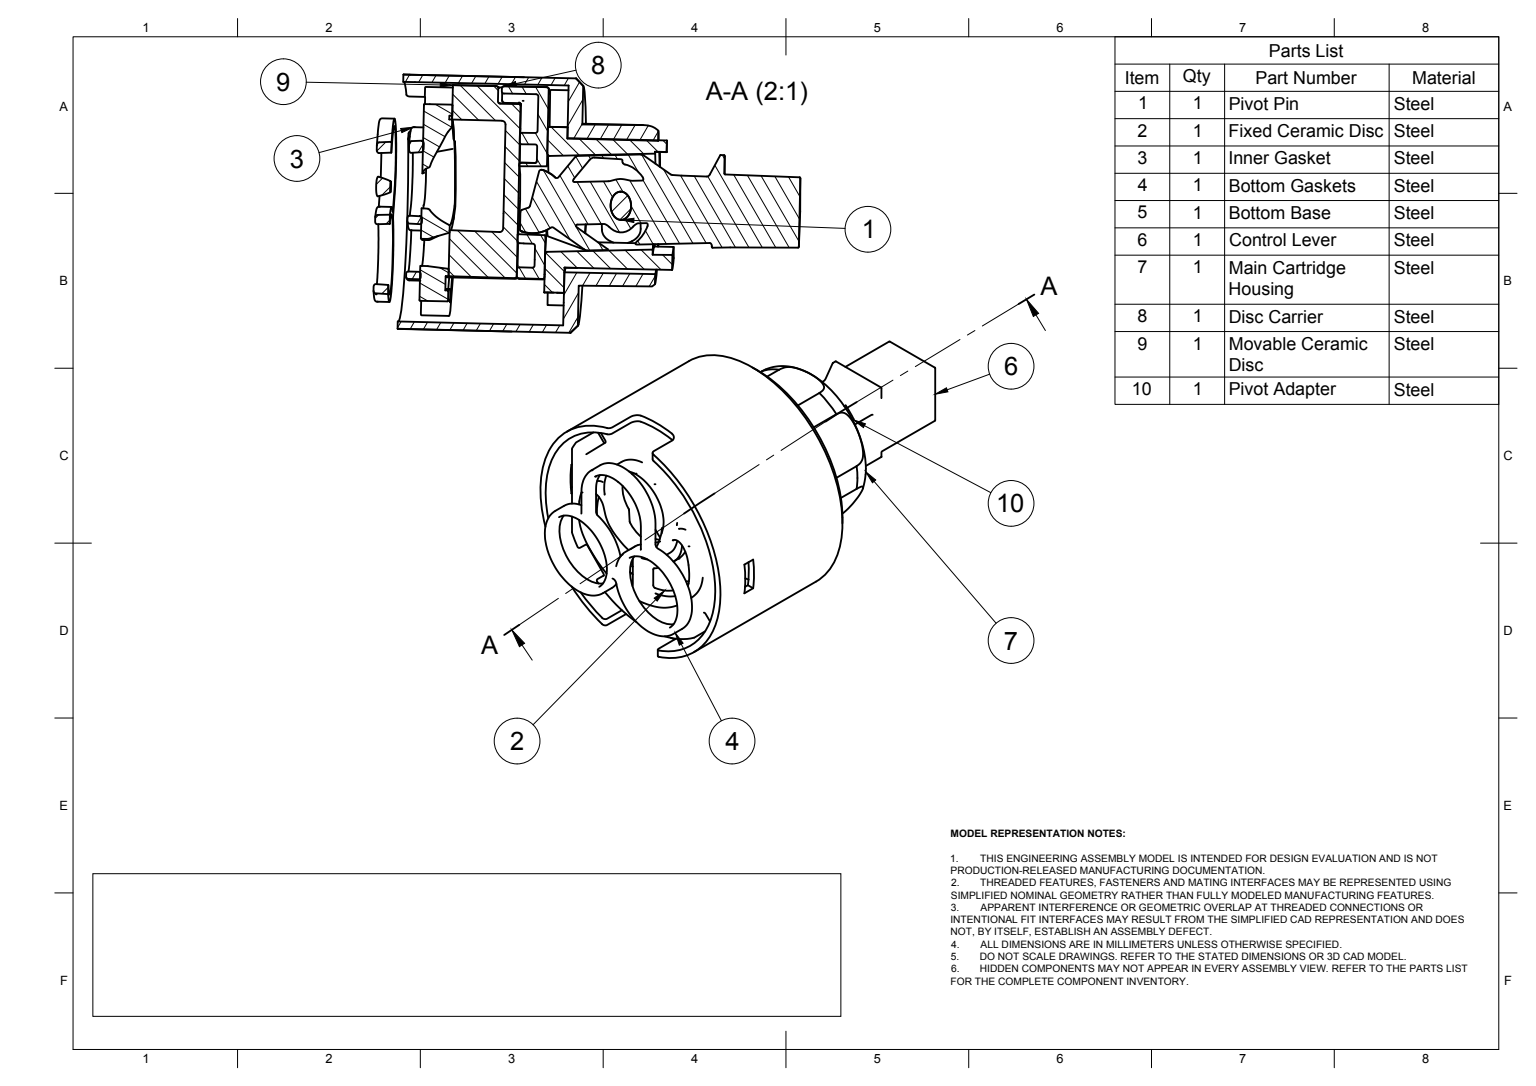
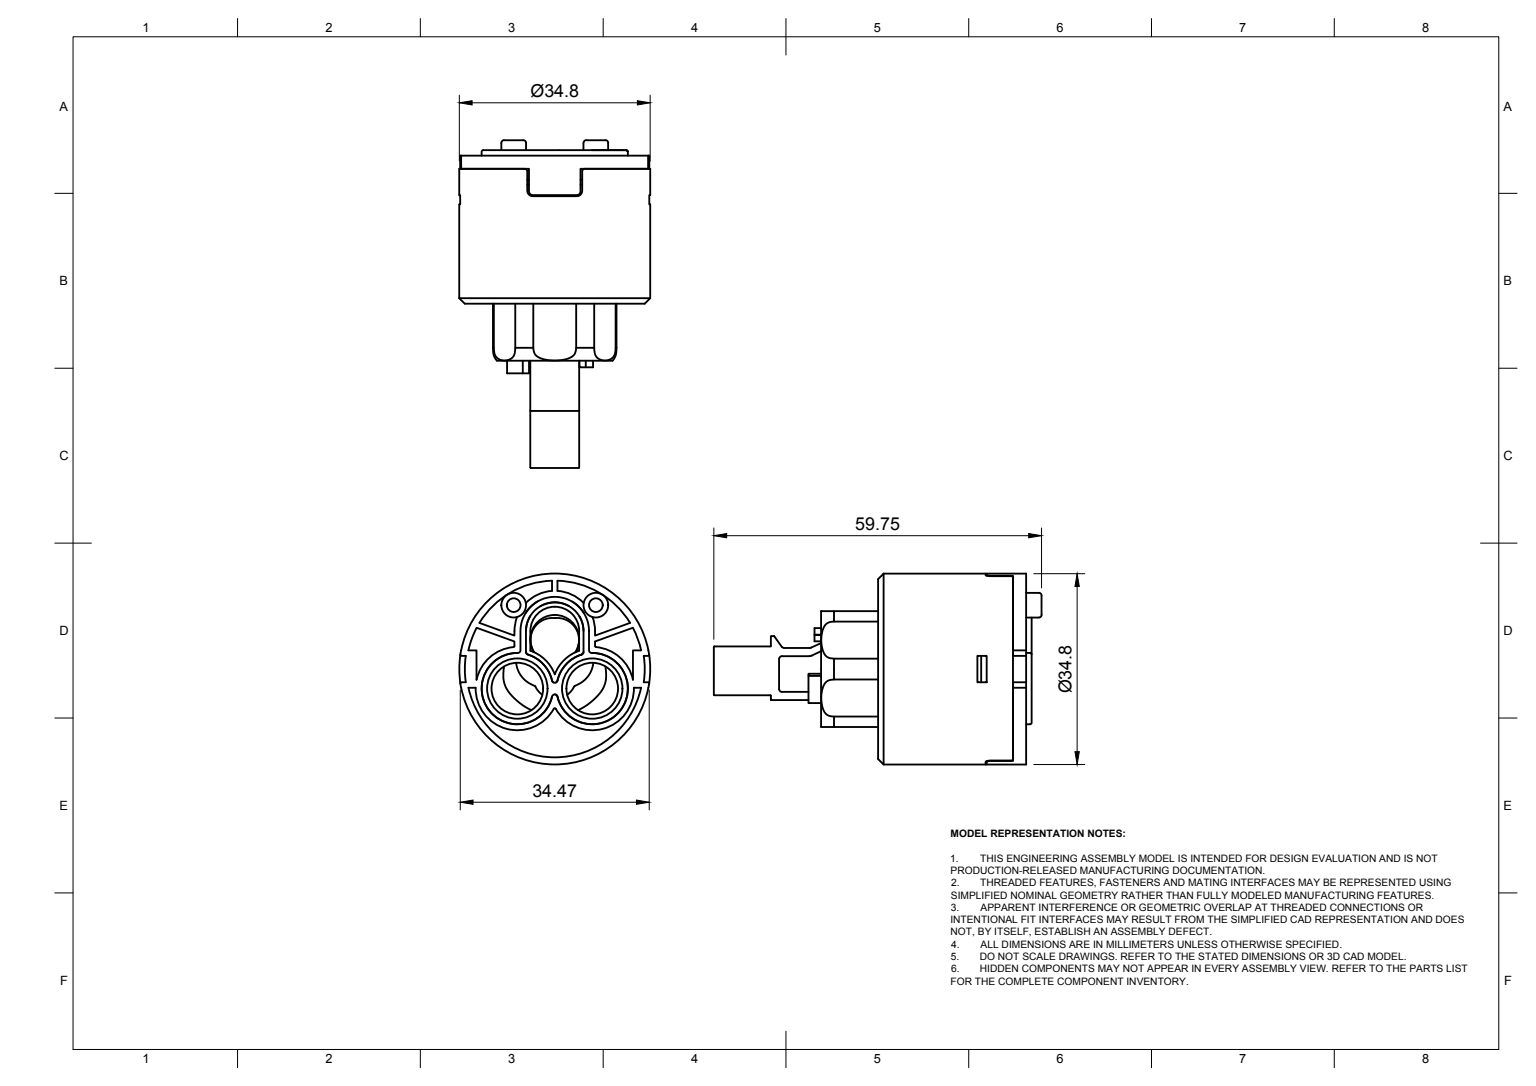
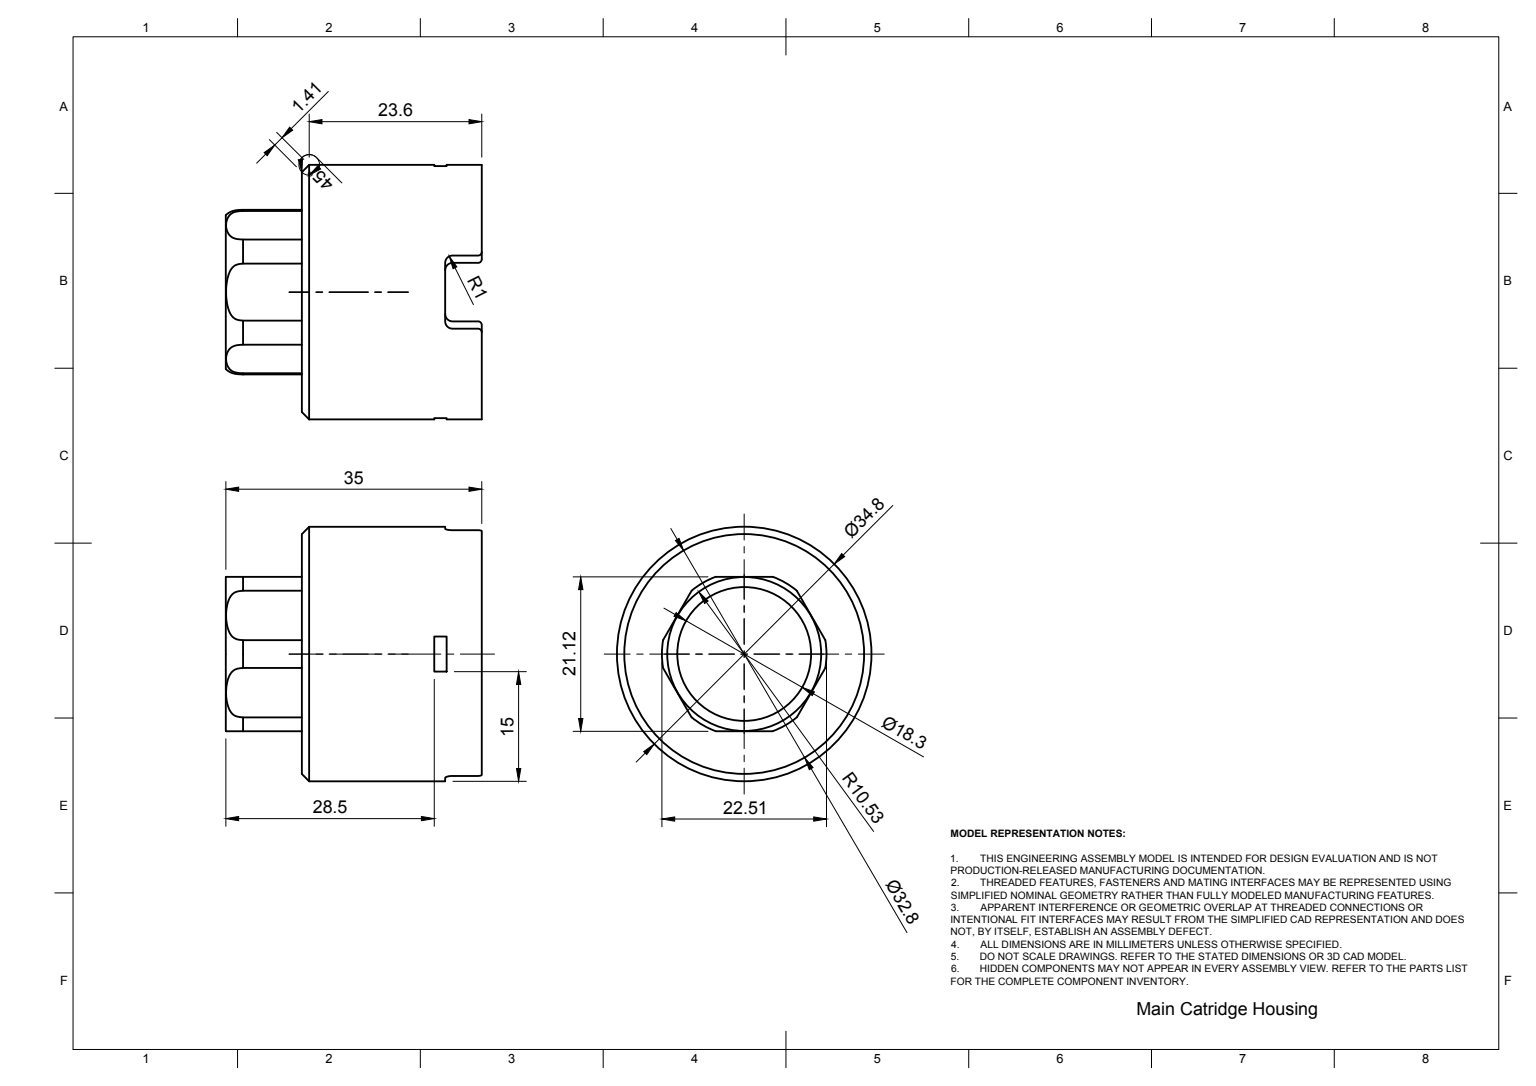
ISO-10303-21;
HEADER;
/* Generated by software containing ST-Developer
 * from STEP Tools, Inc. (www.steptools.com) 
 */

FILE_DESCRIPTION(
/* description */ ('STEP AP214'),
/* implementation_level */ '2;1');

FILE_NAME(
/* name */ 'MAS-608',
/* time_stamp */ '2026-10-06T00:19:40-07:00',
/* author */ (''),
/* organization */ (''),
/* preprocessor_version */ 'ST-DEVELOPER v20.2',
/* originating_system */ 'Autodesk Translation Framework v15.15.0.0',
/* authorisation */ '');

FILE_SCHEMA (('AUTOMOTIVE_DESIGN { 1 0 10303 214 3 1 1 }'));
ENDSEC;

DATA;
#10=MECHANICAL_DESIGN_GEOMETRIC_PRESENTATION_REPRESENTATION('',(#2063,#2064,
#2065,#2066,#2067,#2068,#2069,#2070,#2071,#2072),#98302);
#11=ITEM_DEFINED_TRANSFORMATION($,$,#34291,#38606);
#12=ITEM_DEFINED_TRANSFORMATION($,$,#34303,#38607);
#13=ITEM_DEFINED_TRANSFORMATION($,$,#34823,#38608);
#14=ITEM_DEFINED_TRANSFORMATION($,$,#34920,#38609);
#15=ITEM_DEFINED_TRANSFORMATION($,$,#34962,#38610);
#16=ITEM_DEFINED_TRANSFORMATION($,$,#35726,#38611);
#17=ITEM_DEFINED_TRANSFORMATION($,$,#36369,#38612);
#18=ITEM_DEFINED_TRANSFORMATION($,$,#36602,#38613);
#19=ITEM_DEFINED_TRANSFORMATION($,$,#38088,#38614);
#20=ITEM_DEFINED_TRANSFORMATION($,$,#38347,#38615);
#21=(
REPRESENTATION_RELATIONSHIP($,$,#98340,#98339)
REPRESENTATION_RELATIONSHIP_WITH_TRANSFORMATION(#11)
SHAPE_REPRESENTATION_RELATIONSHIP()
);
#22=(
REPRESENTATION_RELATIONSHIP($,$,#98341,#98339)
REPRESENTATION_RELATIONSHIP_WITH_TRANSFORMATION(#12)
SHAPE_REPRESENTATION_RELATIONSHIP()
);
#23=(
REPRESENTATION_RELATIONSHIP($,$,#98342,#98339)
REPRESENTATION_RELATIONSHIP_WITH_TRANSFORMATION(#13)
SHAPE_REPRESENTATION_RELATIONSHIP()
);
#24=(
REPRESENTATION_RELATIONSHIP($,$,#98343,#98339)
REPRESENTATION_RELATIONSHIP_WITH_TRANSFORMATION(#14)
SHAPE_REPRESENTATION_RELATIONSHIP()
);
#25=(
REPRESENTATION_RELATIONSHIP($,$,#98344,#98339)
REPRESENTATION_RELATIONSHIP_WITH_TRANSFORMATION(#15)
SHAPE_REPRESENTATION_RELATIONSHIP()
);
#26=(
REPRESENTATION_RELATIONSHIP($,$,#98345,#98339)
REPRESENTATION_RELATIONSHIP_WITH_TRANSFORMATION(#16)
SHAPE_REPRESENTATION_RELATIONSHIP()
);
#27=(
REPRESENTATION_RELATIONSHIP($,$,#98346,#98339)
REPRESENTATION_RELATIONSHIP_WITH_TRANSFORMATION(#17)
SHAPE_REPRESENTATION_RELATIONSHIP()
);
#28=(
REPRESENTATION_RELATIONSHIP($,$,#98347,#98339)
REPRESENTATION_RELATIONSHIP_WITH_TRANSFORMATION(#18)
SHAPE_REPRESENTATION_RELATIONSHIP()
);
#29=(
REPRESENTATION_RELATIONSHIP($,$,#98348,#98339)
REPRESENTATION_RELATIONSHIP_WITH_TRANSFORMATION(#19)
SHAPE_REPRESENTATION_RELATIONSHIP()
);
#30=(
REPRESENTATION_RELATIONSHIP($,$,#98349,#98339)
REPRESENTATION_RELATIONSHIP_WITH_TRANSFORMATION(#20)
SHAPE_REPRESENTATION_RELATIONSHIP()
);
#31=CONTEXT_DEPENDENT_SHAPE_REPRESENTATION(#21,#98329);
#32=CONTEXT_DEPENDENT_SHAPE_REPRESENTATION(#22,#98330);
#33=CONTEXT_DEPENDENT_SHAPE_REPRESENTATION(#23,#98331);
#34=CONTEXT_DEPENDENT_SHAPE_REPRESENTATION(#24,#98332);
#35=CONTEXT_DEPENDENT_SHAPE_REPRESENTATION(#25,#98333);
#36=CONTEXT_DEPENDENT_SHAPE_REPRESENTATION(#26,#98334);
#37=CONTEXT_DEPENDENT_SHAPE_REPRESENTATION(#27,#98335);
#38=CONTEXT_DEPENDENT_SHAPE_REPRESENTATION(#28,#98336);
#39=CONTEXT_DEPENDENT_SHAPE_REPRESENTATION(#29,#98337);
#40=CONTEXT_DEPENDENT_SHAPE_REPRESENTATION(#30,#98338);
#41=NEXT_ASSEMBLY_USAGE_OCCURRENCE('Pivot Pin:1','Pivot Pin:1',
'Pivot Pin:1',#98351,#98352,'Pivot Pin:1');
#42=NEXT_ASSEMBLY_USAGE_OCCURRENCE('Fixed Ceramic Disc:1',
'Fixed Ceramic Disc:1','Fixed Ceramic Disc:1',#98351,#98353,
'Fixed Ceramic Disc:1');
#43=NEXT_ASSEMBLY_USAGE_OCCURRENCE('Inner Gasket:1','Inner Gasket:1',
'Inner Gasket:1',#98351,#98354,'Inner Gasket:1');
#44=NEXT_ASSEMBLY_USAGE_OCCURRENCE('Bottom Gaskets:1',
'Bottom Gaskets:1','Bottom Gaskets:1',#98351,#98355,'Bottom Gaskets:1');
#45=NEXT_ASSEMBLY_USAGE_OCCURRENCE('Bottom Base:1','Bottom Base:1',
'Bottom Base:1',#98351,#98356,'Bottom Base:1');
#46=NEXT_ASSEMBLY_USAGE_OCCURRENCE('Control Lever:1','Control Lever:1',
'Control Lever:1',#98351,#98357,'Control Lever:1');
#47=NEXT_ASSEMBLY_USAGE_OCCURRENCE('Main Cartridge Housing:1',
'Main Cartridge Housing:1','Main Cartridge Housing:1',#98351,#98358,
'Main Cartridge Housing:1');
#48=NEXT_ASSEMBLY_USAGE_OCCURRENCE('Disc Carrier:1','Disc Carrier:1',
'Disc Carrier:1',#98351,#98359,'Disc Carrier:1');
#49=NEXT_ASSEMBLY_USAGE_OCCURRENCE('Movable Ceramic Disc:1',
'Movable Ceramic Disc:1','Movable Ceramic Disc:1',#98351,#98360,
'Movable Ceramic Disc:1');
#50=NEXT_ASSEMBLY_USAGE_OCCURRENCE('Pivot Adapter:1','Pivot Adapter:1',
'Pivot Adapter:1',#98351,#98361,'Pivot Adapter:1');
#51=(
BOUNDED_SURFACE()
B_SPLINE_SURFACE(2,2,((#79789,#79790,#79791),(#79792,#79793,#79794),(#79795,
#79796,#79797)),.UNSPECIFIED.,.F.,.F.,.F.)
B_SPLINE_SURFACE_WITH_KNOTS((3,3),(3,3),(-1.5707963267949,0.),(2.16840434497101E-15,
1.5707963267949),.UNSPECIFIED.)
GEOMETRIC_REPRESENTATION_ITEM()
RATIONAL_B_SPLINE_SURFACE(((1.,0.707106781186548,1.),(0.707106781186552,
0.500000000000004,0.707106781186552),(1.,0.707106781186548,1.)))
REPRESENTATION_ITEM('')
SURFACE()
);
#52=(
BOUNDED_SURFACE()
B_SPLINE_SURFACE(2,2,((#79805,#79806,#79807),(#79808,#79809,#79810),(#79811,
#79812,#79813)),.UNSPECIFIED.,.F.,.F.,.F.)
B_SPLINE_SURFACE_WITH_KNOTS((3,3),(3,3),(-1.5707963267949,0.),(-2.60208521396521E-15,
1.57079632679489),.UNSPECIFIED.)
GEOMETRIC_REPRESENTATION_ITEM()
RATIONAL_B_SPLINE_SURFACE(((1.,0.707106781186547,1.),(0.707106781186549,
0.500000000000001,0.707106781186549),(1.,0.707106781186547,1.)))
REPRESENTATION_ITEM('')
SURFACE()
);
#53=(
BOUNDED_SURFACE()
B_SPLINE_SURFACE(2,2,((#80188,#80189,#80190),(#80191,#80192,#80193),(#80194,
#80195,#80196)),.UNSPECIFIED.,.F.,.F.,.F.)
B_SPLINE_SURFACE_WITH_KNOTS((3,3),(3,3),(0.,1.4106605988315),(0.376263560334167,
1.46306115470143),.UNSPECIFIED.)
GEOMETRIC_REPRESENTATION_ITEM()
RATIONAL_B_SPLINE_SURFACE(((1.,0.855956286723383,1.),(0.761397465025631,
0.651722946883935,0.761397465025631),(1.,0.855956286723383,1.)))
REPRESENTATION_ITEM('')
SURFACE()
);
#54=(
BOUNDED_SURFACE()
B_SPLINE_SURFACE(2,2,((#80214,#80215,#80216),(#80217,#80218,#80219),(#80220,
#80221,#80222)),.UNSPECIFIED.,.F.,.F.,.F.)
B_SPLINE_SURFACE_WITH_KNOTS((3,3),(3,3),(0.,1.4106586369982),(-1.77013213181166E-11,
1.08679759433717),.UNSPECIFIED.)
GEOMETRIC_REPRESENTATION_ITEM()
RATIONAL_B_SPLINE_SURFACE(((1.,0.855956286726587,1.),(0.761398100939168,
0.651723491200565,0.761398100939168),(1.,0.855956286726587,1.)))
REPRESENTATION_ITEM('')
SURFACE()
);
#55=(
BOUNDED_SURFACE()
B_SPLINE_SURFACE(2,2,((#82289,#82290,#82291),(#82292,#82293,#82294),(#82295,
#82296,#82297)),.UNSPECIFIED.,.F.,.F.,.F.)
B_SPLINE_SURFACE_WITH_KNOTS((3,3),(3,3),(-1.5707963267949,0.),(-1.5707963267949,
-2.16840434497101E-15),.UNSPECIFIED.)
GEOMETRIC_REPRESENTATION_ITEM()
RATIONAL_B_SPLINE_SURFACE(((1.,0.707106781186548,1.),(0.707106781186552,
0.500000000000004,0.707106781186552),(1.,0.707106781186548,1.)))
REPRESENTATION_ITEM('')
SURFACE()
);
#56=(
BOUNDED_SURFACE()
B_SPLINE_SURFACE(2,2,((#82717,#82718,#82719),(#82720,#82721,#82722),(#82723,
#82724,#82725)),.UNSPECIFIED.,.F.,.F.,.F.)
B_SPLINE_SURFACE_WITH_KNOTS((3,3),(3,3),(-1.5707963267949,0.),(-1.57079632679489,
2.60208521396521E-15),.UNSPECIFIED.)
GEOMETRIC_REPRESENTATION_ITEM()
RATIONAL_B_SPLINE_SURFACE(((1.,0.707106781186547,1.),(0.707106781186549,
0.500000000000001,0.707106781186549),(1.,0.707106781186547,1.)))
REPRESENTATION_ITEM('')
SURFACE()
);
#57=(
BOUNDED_SURFACE()
B_SPLINE_SURFACE(2,2,((#82902,#82903,#82904),(#82905,#82906,#82907),(#82908,
#82909,#82910)),.UNSPECIFIED.,.F.,.F.,.F.)
B_SPLINE_SURFACE_WITH_KNOTS((3,3),(3,3),(0.,1.41065863634176),(-1.08679758944487,
1.77019687584094E-11),.UNSPECIFIED.)
GEOMETRIC_REPRESENTATION_ITEM()
RATIONAL_B_SPLINE_SURFACE(((1.,0.855956287991364,1.),(0.761398101151941,
0.651723492345688,0.761398101151941),(1.,0.855956287991364,1.)))
REPRESENTATION_ITEM('')
SURFACE()
);
#58=(
BOUNDED_SURFACE()
B_SPLINE_SURFACE(2,2,((#83156,#83157,#83158),(#83159,#83160,#83161),(#83162,
#83163,#83164)),.UNSPECIFIED.,.F.,.F.,.F.)
B_SPLINE_SURFACE_WITH_KNOTS((3,3),(3,3),(0.,1.41066059181116),(-1.46306115470144,
-0.376263565240401),.UNSPECIFIED.)
GEOMETRIC_REPRESENTATION_ITEM()
RATIONAL_B_SPLINE_SURFACE(((1.,0.855956287991761,1.),(0.761397467301222,
0.651722949797482,0.761397467301222),(1.,0.855956287991761,1.)))
REPRESENTATION_ITEM('')
SURFACE()
);
#59=(
BOUNDED_SURFACE()
B_SPLINE_SURFACE(3,3,((#83282,#83283,#83284,#83285),(#83286,#83287,#83288,
#83289),(#83290,#83291,#83292,#83293),(#83294,#83295,#83296,#83297),(#83298,
#83299,#83300,#83301),(#83302,#83303,#83304,#83305),(#83306,#83307,#83308,
#83309)),.UNSPECIFIED.,.F.,.F.,.F.)
B_SPLINE_SURFACE_WITH_KNOTS((4,3,4),(4,4),(0.,1.,1.00725260737196),(0.,
1.),.UNSPECIFIED.)
GEOMETRIC_REPRESENTATION_ITEM()
RATIONAL_B_SPLINE_SURFACE(((1.,0.333333333333333,0.333333333333333,1.),
(1.,0.333333333333333,0.333333333333333,1.),(1.,0.333333333333333,0.333333333333333,
1.),(1.,0.333333333333333,0.333333333333333,1.),(1.,0.333333333333333,0.333333333333333,
1.),(1.,0.333333333333333,0.333333333333333,1.),(1.,0.333333333333333,0.333333333333333,
1.)))
REPRESENTATION_ITEM('')
SURFACE()
);
#60=(
BOUNDED_SURFACE()
B_SPLINE_SURFACE(2,2,((#83938,#83939,#83940,#83941,#83942),(#83943,#83944,
#83945,#83946,#83947),(#83948,#83949,#83950,#83951,#83952),(#83953,#83954,
#83955,#83956,#83957),(#83958,#83959,#83960,#83961,#83962)),
 .UNSPECIFIED.,.F.,.F.,.F.)
B_SPLINE_SURFACE_WITH_KNOTS((3,2,3),(3,2,3),(0.,0.785398163496265,1.57079632699253),
(-2.06718528792769,-1.03359264376751,3.92659169068388E-10),
 .UNSPECIFIED.)
GEOMETRIC_REPRESENTATION_ITEM()
RATIONAL_B_SPLINE_SURFACE(((1.,0.869406567431186,1.,0.869406567431186,1.),
(0.923879532492386,0.803226933064135,0.923879532492386,0.803226933064135,
0.923879532492386),(1.,0.869406567431186,1.,0.869406567431186,1.),(0.92387953249249,
0.803226933064225,0.92387953249249,0.803226933064225,0.92387953249249),
(1.,0.869406567431186,1.,0.869406567431186,1.)))
REPRESENTATION_ITEM('')
SURFACE()
);
#61=(
BOUNDED_SURFACE()
B_SPLINE_SURFACE(2,2,((#84445,#84446,#84447,#84448,#84449),(#84450,#84451,
#84452,#84453,#84454),(#84455,#84456,#84457,#84458,#84459),(#84460,#84461,
#84462,#84463,#84464),(#84465,#84466,#84467,#84468,#84469)),
 .UNSPECIFIED.,.F.,.F.,.F.)
B_SPLINE_SURFACE_WITH_KNOTS((3,2,3),(3,2,3),(0.,0.785398163496265,1.57079632699253),
(-3.92659169068388E-10,1.03359264376751,2.06718528792769),.UNSPECIFIED.)
GEOMETRIC_REPRESENTATION_ITEM()
RATIONAL_B_SPLINE_SURFACE(((1.,0.869406567431186,1.,0.869406567431186,1.),
(0.923879532492386,0.803226933064135,0.923879532492386,0.803226933064135,
0.923879532492386),(1.,0.869406567431186,1.,0.869406567431186,1.),(0.92387953249249,
0.803226933064225,0.92387953249249,0.803226933064225,0.92387953249249),
(1.,0.869406567431186,1.,0.869406567431186,1.)))
REPRESENTATION_ITEM('')
SURFACE()
);
#62=(
BOUNDED_SURFACE()
B_SPLINE_SURFACE(3,3,((#85159,#85160,#85161,#85162),(#85163,#85164,#85165,
#85166),(#85167,#85168,#85169,#85170),(#85171,#85172,#85173,#85174),(#85175,
#85176,#85177,#85178),(#85179,#85180,#85181,#85182),(#85183,#85184,#85185,
#85186)),.UNSPECIFIED.,.F.,.F.,.F.)
B_SPLINE_SURFACE_WITH_KNOTS((4,3,4),(4,4),(0.,1.,1.00725260737198),(0.,
1.),.UNSPECIFIED.)
GEOMETRIC_REPRESENTATION_ITEM()
RATIONAL_B_SPLINE_SURFACE(((1.,0.333333333333333,0.333333333333333,1.),
(1.,0.333333333333333,0.333333333333333,1.),(1.,0.333333333333333,0.333333333333333,
1.),(1.,0.333333333333333,0.333333333333333,1.),(1.,0.333333333333333,0.333333333333333,
1.),(1.,0.333333333333333,0.333333333333333,1.),(1.,0.333333333333333,0.333333333333333,
1.)))
REPRESENTATION_ITEM('')
SURFACE()
);
#63=ORIENTED_CLOSED_SHELL('',*,#34171,.F.);
#64=ORIENTED_CLOSED_SHELL('',*,#34172,.F.);
#65=BREP_WITH_VOIDS('Body1',#34173,(#63,#64));
#66=TOROIDAL_SURFACE('',#34375,15.8,0.1);
#67=TOROIDAL_SURFACE('',#34378,0.2,0.1);
#68=TOROIDAL_SURFACE('',#34386,0.4,0.1);
#69=TOROIDAL_SURFACE('',#34394,0.4,0.1);
#70=TOROIDAL_SURFACE('',#34402,0.2,0.1);
#71=TOROIDAL_SURFACE('',#34407,15.8,0.1);
#72=TOROIDAL_SURFACE('',#34412,0.4,0.1);
#73=TOROIDAL_SURFACE('',#34420,0.4,0.1);
#74=TOROIDAL_SURFACE('',#34425,15.8,0.1);
#75=TOROIDAL_SURFACE('',#34430,0.2,0.1);
#76=TOROIDAL_SURFACE('',#34438,0.4,0.1);
#77=TOROIDAL_SURFACE('',#34446,0.4,0.1);
#78=TOROIDAL_SURFACE('',#34454,0.2,0.1);
#79=TOROIDAL_SURFACE('',#34462,15.8,0.1);
#80=TOROIDAL_SURFACE('',#34464,0.2,0.1);
#81=TOROIDAL_SURFACE('',#34472,0.4,0.1);
#82=TOROIDAL_SURFACE('',#34480,0.4,0.1);
#83=TOROIDAL_SURFACE('',#34488,0.2,0.1);
#84=TOROIDAL_SURFACE('',#34493,15.8,0.1);
#85=TOROIDAL_SURFACE('',#34498,0.4,0.1);
#86=TOROIDAL_SURFACE('',#34506,0.4,0.1);
#87=TOROIDAL_SURFACE('',#34511,15.8,0.1);
#88=TOROIDAL_SURFACE('',#34516,0.2,0.1);
#89=TOROIDAL_SURFACE('',#34524,0.4,0.1);
#90=TOROIDAL_SURFACE('',#34532,0.2,0.1);
#91=TOROIDAL_SURFACE('',#34537,0.4,0.1);
#92=TOROIDAL_SURFACE('',#34602,15.8,0.1);
#93=TOROIDAL_SURFACE('',#34606,0.2,0.1);
#94=TOROIDAL_SURFACE('',#34611,0.4,0.1);
#95=TOROIDAL_SURFACE('',#34616,0.4,0.1);
#96=TOROIDAL_SURFACE('',#34621,0.2,0.1);
#97=TOROIDAL_SURFACE('',#34624,15.8,0.1);
#98=TOROIDAL_SURFACE('',#34627,0.4,0.1);
#99=TOROIDAL_SURFACE('',#34632,0.4,0.1);
#100=TOROIDAL_SURFACE('',#34635,15.8,0.1);
#101=TOROIDAL_SURFACE('',#34638,0.2,0.1);
#102=TOROIDAL_SURFACE('',#34643,0.4,0.1);
#103=TOROIDAL_SURFACE('',#34648,0.4,0.1);
#104=TOROIDAL_SURFACE('',#34653,0.2,0.1);
#105=TOROIDAL_SURFACE('',#34656,15.8,0.1);
#106=TOROIDAL_SURFACE('',#34659,0.2,0.1);
#107=TOROIDAL_SURFACE('',#34664,0.4,0.1);
#108=TOROIDAL_SURFACE('',#34669,0.4,0.1);
#109=TOROIDAL_SURFACE('',#34674,0.2,0.1);
#110=TOROIDAL_SURFACE('',#34677,15.8,0.1);
#111=TOROIDAL_SURFACE('',#34680,0.4,0.1);
#112=TOROIDAL_SURFACE('',#34685,0.4,0.1);
#113=TOROIDAL_SURFACE('',#34688,15.8,0.1);
#114=TOROIDAL_SURFACE('',#34691,0.2,0.1);
#115=TOROIDAL_SURFACE('',#34696,0.4,0.1);
#116=TOROIDAL_SURFACE('',#34701,0.2,0.1);
#117=TOROIDAL_SURFACE('',#34704,0.4,0.1);
#118=TOROIDAL_SURFACE('',#34927,5.8,0.3);
#119=TOROIDAL_SURFACE('',#34931,5.8,0.3);
#120=TOROIDAL_SURFACE('',#35179,1.75,0.5);
#121=TOROIDAL_SURFACE('',#35197,1.75,0.5);
#122=TOROIDAL_SURFACE('',#35509,16.1,0.3);
#123=TOROIDAL_SURFACE('',#35537,0.6,0.3);
#124=TOROIDAL_SURFACE('',#35540,15.7,0.3);
#125=TOROIDAL_SURFACE('',#35542,0.6,0.3);
#126=TOROIDAL_SURFACE('',#35565,16.1,0.3);
#127=TOROIDAL_SURFACE('',#35593,0.6,0.3);
#128=TOROIDAL_SURFACE('',#35596,15.7,0.3);
#129=TOROIDAL_SURFACE('',#35598,0.6,0.3);
#130=TOROIDAL_SURFACE('',#35623,16.1,0.3);
#131=TOROIDAL_SURFACE('',#35651,0.6,0.3);
#132=TOROIDAL_SURFACE('',#35654,15.7,0.3);
#133=TOROIDAL_SURFACE('',#35656,0.6,0.3);
#134=TOROIDAL_SURFACE('',#35689,16.1,0.3);
#135=TOROIDAL_SURFACE('',#35706,0.6,0.3);
#136=TOROIDAL_SURFACE('',#35709,15.7,0.3);
#137=TOROIDAL_SURFACE('',#35711,0.6,0.3);
#138=TOROIDAL_SURFACE('',#35727,4.25458972174,0.3);
#139=TOROIDAL_SURFACE('',#35732,4.40145759978,0.3);
#140=TOROIDAL_SURFACE('',#35739,4.72461821943,0.3);
#141=TOROIDAL_SURFACE('',#35746,4.40145759978,0.3);
#142=TOROIDAL_SURFACE('',#35752,4.25458972174,0.3);
#143=TOROIDAL_SURFACE('',#35757,4.1423251838,0.3);
#144=TOROIDAL_SURFACE('',#35772,4.00032353732,0.3);
#145=TOROIDAL_SURFACE('',#35791,4.00032353732,0.3);
#146=TOROIDAL_SURFACE('',#35793,3.93623398426,0.3);
#147=TOROIDAL_SURFACE('',#35806,1.3,0.3);
#148=TOROIDAL_SURFACE('',#35819,4.45,0.3);
#149=TOROIDAL_SURFACE('',#35846,0.9,0.1);
#150=TOROIDAL_SURFACE('',#35851,0.6,0.1);
#151=TOROIDAL_SURFACE('',#35856,0.6,0.1);
#152=TOROIDAL_SURFACE('',#35874,3.85,0.3);
#153=TOROIDAL_SURFACE('',#35880,1.1,0.1);
#154=TOROIDAL_SURFACE('',#35901,4.15601973046,0.3);
#155=TOROIDAL_SURFACE('',#35912,0.7,0.3);
#156=TOROIDAL_SURFACE('',#35915,1.1,0.1);
#157=TOROIDAL_SURFACE('',#35927,0.8,0.3);
#158=TOROIDAL_SURFACE('',#35929,0.8,0.3);
#159=TOROIDAL_SURFACE('',#35933,0.9,0.1);
#160=TOROIDAL_SURFACE('',#35938,0.2,0.1);
#161=TOROIDAL_SURFACE('',#35941,3.05,0.1);
#162=TOROIDAL_SURFACE('',#35947,0.4,0.1);
#163=TOROIDAL_SURFACE('',#35951,1.1,0.1);
#164=TOROIDAL_SURFACE('',#35955,0.4,0.1);
#165=TOROIDAL_SURFACE('',#35960,3.05,0.1);
#166=TOROIDAL_SURFACE('',#35964,0.2,0.1);
#167=TOROIDAL_SURFACE('',#35969,0.9,0.1);
#168=TOROIDAL_SURFACE('',#35974,0.4,0.1);
#169=TOROIDAL_SURFACE('',#35979,0.6,0.1);
#170=TOROIDAL_SURFACE('',#35984,0.6,0.1);
#171=TOROIDAL_SURFACE('',#35995,0.2,0.1);
#172=TOROIDAL_SURFACE('',#36006,0.2,0.1);
#173=TOROIDAL_SURFACE('',#36010,2.95,0.3);
#174=TOROIDAL_SURFACE('',#36014,0.7,0.3);
#175=TOROIDAL_SURFACE('',#36016,2.65,0.3);
#176=TOROIDAL_SURFACE('',#36021,2.65,0.3);
#177=TOROIDAL_SURFACE('',#36027,2.65,0.3);
#178=TOROIDAL_SURFACE('',#36031,2.65,0.3);
#179=TOROIDAL_SURFACE('',#36042,0.8,0.3);
#180=TOROIDAL_SURFACE('',#36048,3.98150447852,0.3);
#181=TOROIDAL_SURFACE('',#36055,4.46095497424,0.3);
#182=TOROIDAL_SURFACE('',#36106,3.05,0.1);
#183=TOROIDAL_SURFACE('',#36112,4.15601973046,0.3);
#184=TOROIDAL_SURFACE('',#36135,0.9,0.1);
#185=TOROIDAL_SURFACE('',#36140,0.2,0.1);
#186=TOROIDAL_SURFACE('',#36143,0.2,0.1);
#187=TOROIDAL_SURFACE('',#36148,0.9,0.1);
#188=TOROIDAL_SURFACE('',#36153,0.4,0.1);
#189=TOROIDAL_SURFACE('',#36158,0.6,0.1);
#190=TOROIDAL_SURFACE('',#36163,0.6,0.1);
#191=TOROIDAL_SURFACE('',#36178,0.2,0.1);
#192=TOROIDAL_SURFACE('',#36193,0.2,0.1);
#193=TOROIDAL_SURFACE('',#36206,2.95,0.3);
#194=TOROIDAL_SURFACE('',#36212,0.7,0.3);
#195=TOROIDAL_SURFACE('',#36215,0.7,0.3);
#196=TOROIDAL_SURFACE('',#36220,0.8,0.3);
#197=TOROIDAL_SURFACE('',#36229,0.8,0.3);
#198=TOROIDAL_SURFACE('',#36233,0.8,0.3);
#199=TOROIDAL_SURFACE('',#36237,3.85,0.3);
#200=TOROIDAL_SURFACE('',#36240,2.36684105319,0.1);
#201=TOROIDAL_SURFACE('',#36253,0.4,0.1);
#202=TOROIDAL_SURFACE('',#36259,1.1,0.1);
#203=TOROIDAL_SURFACE('',#36268,3.98150447852,0.3);
#204=TOROIDAL_SURFACE('',#36272,2.55,0.1);
#205=TOROIDAL_SURFACE('',#36276,1.3,0.3);
#206=TOROIDAL_SURFACE('',#36292,1.1,0.1);
#207=TOROIDAL_SURFACE('',#36306,3.05,0.1);
#208=TOROIDAL_SURFACE('',#36312,0.4,0.1);
#209=TOROIDAL_SURFACE('',#36320,0.6,0.1);
#210=TOROIDAL_SURFACE('',#36325,0.6,0.1);
#211=TOROIDAL_SURFACE('',#36330,0.9,0.1);
#212=TOROIDAL_SURFACE('',#36335,1.1,0.1);
#213=TOROIDAL_SURFACE('',#36363,4.45,0.3);
#214=TOROIDAL_SURFACE('',#36474,0.8,0.3);
#215=TOROIDAL_SURFACE('',#36514,11.3,0.3);
#216=TOROIDAL_SURFACE('',#36520,0.8,0.3);
#217=TOROIDAL_SURFACE('',#36633,13.816744254,0.3);
#218=TOROIDAL_SURFACE('',#36640,0.6,0.3);
#219=TOROIDAL_SURFACE('',#36644,14.9875296363,0.3);
#220=TOROIDAL_SURFACE('',#36648,0.6,0.3);
#221=TOROIDAL_SURFACE('',#36651,14.9875296363,0.3);
#222=TOROIDAL_SURFACE('',#36655,0.6,0.3);
#223=TOROIDAL_SURFACE('',#36662,13.816744254,0.3);
#224=TOROIDAL_SURFACE('',#36692,13.9462109523,0.3);
#225=TOROIDAL_SURFACE('',#36699,0.6,0.3);
#226=TOROIDAL_SURFACE('',#36702,14.9875296363,0.3);
#227=TOROIDAL_SURFACE('',#36707,15.8875296363,0.3);
#228=TOROIDAL_SURFACE('',#36711,8.14541841273,0.3);
#229=TOROIDAL_SURFACE('',#36717,14.3875296363,0.3);
#230=TOROIDAL_SURFACE('',#36742,7.54541841273,0.3);
#231=TOROIDAL_SURFACE('',#36753,14.9875296363,0.3);
#232=TOROIDAL_SURFACE('',#36757,0.6,0.3);
#233=TOROIDAL_SURFACE('',#36763,0.6,0.3);
#234=TOROIDAL_SURFACE('',#36765,0.6,0.3);
#235=TOROIDAL_SURFACE('',#36767,0.6,0.3);
#236=TOROIDAL_SURFACE('',#36769,12.2256279976,0.3);
#237=TOROIDAL_SURFACE('',#36775,14.9875296363,0.3);
#238=TOROIDAL_SURFACE('',#36803,15.3875296363,0.3);
#239=TOROIDAL_SURFACE('',#36831,4.89295371933,0.3);
#240=TOROIDAL_SURFACE('',#36836,0.6,0.3);
#241=TOROIDAL_SURFACE('',#36842,0.6,0.3);
#242=TOROIDAL_SURFACE('',#36846,6.64541841273,0.3);
#243=TOROIDAL_SURFACE('',#36850,0.6,0.3);
#244=TOROIDAL_SURFACE('',#36854,0.6,0.3);
#245=TOROIDAL_SURFACE('',#36859,6.64541841273,0.3);
#246=TOROIDAL_SURFACE('',#36866,0.6,0.3);
#247=TOROIDAL_SURFACE('',#36875,4.89295371933,0.3);
#248=TOROIDAL_SURFACE('',#36879,0.6,0.3);
#249=TOROIDAL_SURFACE('',#36883,0.6,0.3);
#250=TOROIDAL_SURFACE('',#36894,4.89295371933,0.3);
#251=TOROIDAL_SURFACE('',#36900,0.6,0.3);
#252=TOROIDAL_SURFACE('',#36906,0.6,0.3);
#253=TOROIDAL_SURFACE('',#36910,6.64541841273,0.3);
#254=TOROIDAL_SURFACE('',#36914,0.6,0.3);
#255=TOROIDAL_SURFACE('',#36918,0.6,0.3);
#256=TOROIDAL_SURFACE('',#36926,6.04541841273,0.3);
#257=TOROIDAL_SURFACE('',#36933,5.49295371933,0.3);
#258=TOROIDAL_SURFACE('',#36946,5.49295371933,0.3);
#259=TOROIDAL_SURFACE('',#36950,0.6,0.3);
#260=TOROIDAL_SURFACE('',#36954,7.54541841273,0.3);
#261=TOROIDAL_SURFACE('',#36958,0.6,0.3);
#262=TOROIDAL_SURFACE('',#36962,0.6,0.3);
#263=TOROIDAL_SURFACE('',#36973,12.8256279976,0.3);
#264=TOROIDAL_SURFACE('',#36978,5.49295371933,0.3);
#265=TOROIDAL_SURFACE('',#36984,15.8875296363,0.3);
#266=TOROIDAL_SURFACE('',#36988,15.3875296363,0.3);
#267=TOROIDAL_SURFACE('',#36993,15.8875296363,0.3);
#268=TOROIDAL_SURFACE('',#36996,0.985778366608,0.3);
#269=TOROIDAL_SURFACE('',#37005,2.7,0.3);
#270=TOROIDAL_SURFACE('',#37007,2.7,0.3);
#271=TOROIDAL_SURFACE('',#37013,15.8875296363,0.3);
#272=TOROIDAL_SURFACE('',#37039,8.14541841273,0.3);
#273=TOROIDAL_SURFACE('',#37053,14.3875296363,0.3);
#274=TOROIDAL_SURFACE('',#37091,6.04541841273,0.3);
#275=TOROIDAL_SURFACE('',#37112,6.04541841273,0.3);
#276=TOROIDAL_SURFACE('',#37118,0.385778366608,0.3);
#277=TOROIDAL_SURFACE('',#37119,0.6,0.3);
#278=TOROIDAL_SURFACE('',#37129,8.14541841273,0.3);
#279=TOROIDAL_SURFACE('',#37134,0.6,0.3);
#280=TOROIDAL_SURFACE('',#37137,13.3462109523,0.3);
#281=TOROIDAL_SURFACE('',#37140,0.6,0.3);
#282=TOROIDAL_SURFACE('',#37149,14.3875296363,0.3);
#283=TOROIDAL_SURFACE('',#37154,14.3875296363,0.3);
#284=TOROIDAL_SURFACE('',#37170,0.6,0.3);
#285=TOROIDAL_SURFACE('',#37173,7.54541841273,0.3);
#286=TOROIDAL_SURFACE('',#37176,0.6,0.3);
#287=TOROIDAL_SURFACE('',#37182,0.6,0.3);
#288=TOROIDAL_SURFACE('',#37185,0.6,0.3);
#289=TOROIDAL_SURFACE('',#37188,14.9875296363,0.3);
#290=TOROIDAL_SURFACE('',#37190,0.6,0.3);
#291=TOROIDAL_SURFACE('',#37193,13.216744254,0.3);
#292=TOROIDAL_SURFACE('',#37205,15.8875296363,0.3);
#293=TOROIDAL_SURFACE('',#37207,1.3,0.3);
#294=TOROIDAL_SURFACE('',#37211,14.9875296363,0.3);
#295=TOROIDAL_SURFACE('',#37215,0.6,0.3);
#296=TOROIDAL_SURFACE('',#37221,0.6,0.3);
#297=TOROIDAL_SURFACE('',#37225,7.54541841273,0.3);
#298=TOROIDAL_SURFACE('',#37229,0.6,0.3);
#299=TOROIDAL_SURFACE('',#37261,14.3875296363,0.3);
#300=TOROIDAL_SURFACE('',#37264,0.7,0.3);
#301=TOROIDAL_SURFACE('',#37270,14.3875296363,0.3);
#302=TOROIDAL_SURFACE('',#37275,14.3875296363,0.3);
#303=TOROIDAL_SURFACE('',#37282,8.14541841273,0.3);
#304=TOROIDAL_SURFACE('',#37289,0.6,0.3);
#305=TOROIDAL_SURFACE('',#37292,13.216744254,0.3);
#306=TOROIDAL_SURFACE('',#37295,0.6,0.3);
#307=TOROIDAL_SURFACE('',#37328,13.816744254,0.3);
#308=TOROIDAL_SURFACE('',#37335,0.6,0.3);
#309=TOROIDAL_SURFACE('',#37339,14.9875296363,0.3);
#310=TOROIDAL_SURFACE('',#37343,0.6,0.3);
#311=TOROIDAL_SURFACE('',#37346,14.9875296363,0.3);
#312=TOROIDAL_SURFACE('',#37350,0.6,0.3);
#313=TOROIDAL_SURFACE('',#37357,13.816744254,0.3);
#314=TOROIDAL_SURFACE('',#37389,13.9462109523,0.3);
#315=TOROIDAL_SURFACE('',#37396,0.6,0.3);
#316=TOROIDAL_SURFACE('',#37400,14.9875296363,0.3);
#317=TOROIDAL_SURFACE('',#37406,15.8875296363,0.3);
#318=TOROIDAL_SURFACE('',#37412,8.14541841273,0.3);
#319=TOROIDAL_SURFACE('',#37417,14.3875296363,0.3);
#320=TOROIDAL_SURFACE('',#37442,7.54541841273,0.3);
#321=TOROIDAL_SURFACE('',#37453,14.9875296363,0.3);
#322=TOROIDAL_SURFACE('',#37457,0.6,0.3);
#323=TOROIDAL_SURFACE('',#37463,0.6,0.3);
#324=TOROIDAL_SURFACE('',#37465,0.6,0.3);
#325=TOROIDAL_SURFACE('',#37467,0.6,0.3);
#326=TOROIDAL_SURFACE('',#37470,12.2256279976,0.3);
#327=TOROIDAL_SURFACE('',#37476,14.9875296363,0.3);
#328=TOROIDAL_SURFACE('',#37511,15.3875296363,0.3);
#329=TOROIDAL_SURFACE('',#37543,4.89295371933,0.3);
#330=TOROIDAL_SURFACE('',#37548,0.6,0.3);
#331=TOROIDAL_SURFACE('',#37554,0.6,0.3);
#332=TOROIDAL_SURFACE('',#37558,6.64541841273,0.3);
#333=TOROIDAL_SURFACE('',#37562,0.6,0.3);
#334=TOROIDAL_SURFACE('',#37566,0.6,0.3);
#335=TOROIDAL_SURFACE('',#37571,6.64541841273,0.3);
#336=TOROIDAL_SURFACE('',#37578,0.6,0.3);
#337=TOROIDAL_SURFACE('',#37586,4.89295371933,0.3);
#338=TOROIDAL_SURFACE('',#37590,0.6,0.3);
#339=TOROIDAL_SURFACE('',#37594,0.6,0.3);
#340=TOROIDAL_SURFACE('',#37605,4.89295371933,0.3);
#341=TOROIDAL_SURFACE('',#37611,0.6,0.3);
#342=TOROIDAL_SURFACE('',#37617,0.6,0.3);
#343=TOROIDAL_SURFACE('',#37621,6.64541841273,0.3);
#344=TOROIDAL_SURFACE('',#37625,0.6,0.3);
#345=TOROIDAL_SURFACE('',#37629,0.6,0.3);
#346=TOROIDAL_SURFACE('',#37637,6.04541841273,0.3);
#347=TOROIDAL_SURFACE('',#37643,5.49295371933,0.3);
#348=TOROIDAL_SURFACE('',#37656,5.49295371933,0.3);
#349=TOROIDAL_SURFACE('',#37659,0.6,0.3);
#350=TOROIDAL_SURFACE('',#37663,7.54541841273,0.3);
#351=TOROIDAL_SURFACE('',#37667,0.6,0.3);
#352=TOROIDAL_SURFACE('',#37671,0.6,0.3);
#353=TOROIDAL_SURFACE('',#37684,12.8256279976,0.3);
#354=TOROIDAL_SURFACE('',#37689,5.49295371933,0.3);
#355=TOROIDAL_SURFACE('',#37696,15.8875296363,0.3);
#356=TOROIDAL_SURFACE('',#37700,15.3875296363,0.3);
#357=TOROIDAL_SURFACE('',#37710,0.4,0.1);
#358=TOROIDAL_SURFACE('',#37715,0.4,0.1);
#359=TOROIDAL_SURFACE('',#37720,0.4,0.1);
#360=TOROIDAL_SURFACE('',#37722,0.4,0.1);
#361=TOROIDAL_SURFACE('',#37727,0.4,0.1);
#362=TOROIDAL_SURFACE('',#37732,0.4,0.1);
#363=TOROIDAL_SURFACE('',#37737,0.4,0.1);
#364=TOROIDAL_SURFACE('',#37742,0.4,0.1);
#365=TOROIDAL_SURFACE('',#37749,15.8875296363,0.3);
#366=TOROIDAL_SURFACE('',#37750,0.985778366608,0.3);
#367=TOROIDAL_SURFACE('',#37759,2.7,0.3);
#368=TOROIDAL_SURFACE('',#37761,2.7,0.3);
#369=TOROIDAL_SURFACE('',#37766,15.8875296363,0.3);
#370=TOROIDAL_SURFACE('',#37779,15.3875296363,0.3);
#371=TOROIDAL_SURFACE('',#37803,8.14541841273,0.3);
#372=TOROIDAL_SURFACE('',#37814,14.3875296363,0.3);
#373=TOROIDAL_SURFACE('',#37850,6.04541841273,0.3);
#374=TOROIDAL_SURFACE('',#37871,6.04541841273,0.3);
#375=TOROIDAL_SURFACE('',#37877,0.385778366608,0.3);
#376=TOROIDAL_SURFACE('',#37878,0.6,0.3);
#377=TOROIDAL_SURFACE('',#37886,8.14541841273,0.3);
#378=TOROIDAL_SURFACE('',#37891,0.6,0.3);
#379=TOROIDAL_SURFACE('',#37894,13.3462109523,0.3);
#380=TOROIDAL_SURFACE('',#37897,0.6,0.3);
#381=TOROIDAL_SURFACE('',#37909,14.3875296363,0.3);
#382=TOROIDAL_SURFACE('',#37914,14.3875296363,0.3);
#383=TOROIDAL_SURFACE('',#37930,0.6,0.3);
#384=TOROIDAL_SURFACE('',#37933,7.54541841273,0.3);
#385=TOROIDAL_SURFACE('',#37936,0.6,0.3);
#386=TOROIDAL_SURFACE('',#37942,0.6,0.3);
#387=TOROIDAL_SURFACE('',#37945,0.6,0.3);
#388=TOROIDAL_SURFACE('',#37948,14.9875296363,0.3);
#389=TOROIDAL_SURFACE('',#37950,0.6,0.3);
#390=TOROIDAL_SURFACE('',#37953,13.216744254,0.3);
#391=TOROIDAL_SURFACE('',#37965,15.8875296363,0.3);
#392=TOROIDAL_SURFACE('',#37967,15.3875296363,0.3);
#393=TOROIDAL_SURFACE('',#37977,0.4,0.1);
#394=TOROIDAL_SURFACE('',#37979,0.4,0.1);
#395=TOROIDAL_SURFACE('',#37984,0.4,0.1);
#396=TOROIDAL_SURFACE('',#37991,0.4,0.1);
#397=TOROIDAL_SURFACE('',#37999,1.3,0.3);
#398=TOROIDAL_SURFACE('',#38003,14.9875296363,0.3);
#399=TOROIDAL_SURFACE('',#38006,0.6,0.3);
#400=TOROIDAL_SURFACE('',#38011,0.6,0.3);
#401=TOROIDAL_SURFACE('',#38014,7.54541841273,0.3);
#402=TOROIDAL_SURFACE('',#38017,0.6,0.3);
#403=TOROIDAL_SURFACE('',#38048,14.3875296363,0.3);
#404=TOROIDAL_SURFACE('',#38051,0.7,0.3);
#405=TOROIDAL_SURFACE('',#38057,14.3875296363,0.3);
#406=TOROIDAL_SURFACE('',#38062,14.3875296363,0.3);
#407=TOROIDAL_SURFACE('',#38071,8.14541841273,0.3);
#408=TOROIDAL_SURFACE('',#38079,0.6,0.3);
#409=TOROIDAL_SURFACE('',#38082,13.216744254,0.3);
#410=TOROIDAL_SURFACE('',#38085,0.6,0.3);
#411=TOROIDAL_SURFACE('',#38089,13.016744254,0.3);
#412=TOROIDAL_SURFACE('',#38103,25.2066723663,0.5);
#413=TOROIDAL_SURFACE('',#38106,11.7773059952,0.5);
#414=TOROIDAL_SURFACE('',#38114,4.5,0.5);
#415=TOROIDAL_SURFACE('',#38119,25.2066723663,0.5);
#416=TOROIDAL_SURFACE('',#38123,4.5,0.5);
#417=TOROIDAL_SURFACE('',#38131,11.7773059952,0.5);
#418=TOROIDAL_SURFACE('',#38142,13.616744254,0.3);
#419=TOROIDAL_SURFACE('',#38173,13.616744254,0.3);
#420=TOROIDAL_SURFACE('',#38197,13.7462109523,0.3);
#421=TOROIDAL_SURFACE('',#38202,2.8,0.3);
#422=TOROIDAL_SURFACE('',#38207,13.7462109523,0.3);
#423=TOROIDAL_SURFACE('',#38229,0.6,0.3);
#424=TOROIDAL_SURFACE('',#38232,13.016744254,0.3);
#425=TOROIDAL_SURFACE('',#38235,0.6,0.3);
#426=TOROIDAL_SURFACE('',#38243,0.6,0.3);
#427=TOROIDAL_SURFACE('',#38245,0.6,0.3);
#428=TOROIDAL_SURFACE('',#38253,0.6,0.3);
#429=TOROIDAL_SURFACE('',#38256,13.1462109523,0.3);
#430=TOROIDAL_SURFACE('',#38259,2.2,0.3);
#431=TOROIDAL_SURFACE('',#38262,13.1462109523,0.3);
#432=TOROIDAL_SURFACE('',#38265,0.6,0.3);
#433=TOROIDAL_SURFACE('',#38283,15.8875296363,0.3);
#434=TOROIDAL_SURFACE('',#38290,15.8875296363,0.3);
#435=TOROIDAL_SURFACE('',#38294,2.7,0.3);
#436=TOROIDAL_SURFACE('',#38307,15.8875296363,0.3);
#437=TOROIDAL_SURFACE('',#38312,15.8875296363,0.3);
#438=TOROIDAL_SURFACE('',#38317,2.7,0.3);
#439=TOROIDAL_SURFACE('',#38322,2.7,0.3);
#440=TOROIDAL_SURFACE('',#38336,15.3875296363,0.3);
#441=TOROIDAL_SURFACE('',#38338,15.3875296363,0.3);
#442=TOROIDAL_SURFACE('',#38342,15.3875296363,0.3);
#443=TOROIDAL_SURFACE('',#38348,4.64715395326,0.3);
#444=TOROIDAL_SURFACE('',#38570,0.6,0.3);
#445=TOROIDAL_SURFACE('',#38577,0.6,0.3);
#446=TOROIDAL_SURFACE('',#38588,0.6,0.3);
#447=TOROIDAL_SURFACE('',#38591,4.47840533247,0.3);
#448=TOROIDAL_SURFACE('',#38598,0.6,0.3);
#449=ELLIPSE('',#34351,0.0975089533003066,0.0318233698452749);
#450=ELLIPSE('',#34354,0.210203962458616,0.0684164528781414);
#451=ELLIPSE('',#34355,4.51181641557726,0.330426027279306);
#452=ELLIPSE('',#34356,0.371777616681055,0.0636641381433054);
#453=ELLIPSE('',#34358,1.12077531771054,0.208207940858736);
#454=ELLIPSE('',#34360,7.044836022966,0.27423437971207);
#455=ELLIPSE('',#34362,0.0975089533003066,0.0318233698452749);
#456=ELLIPSE('',#34364,7.044836022966,0.27423437971207);
#457=ELLIPSE('',#34365,1.12077531771054,0.208207940858736);
#458=ELLIPSE('',#34367,0.371777616681055,0.0636641381433054);
#459=ELLIPSE('',#34369,4.51181641557726,0.330426027279306);
#460=ELLIPSE('',#34370,0.210203962458616,0.0684164528781414);
#461=ELLIPSE('',#34546,4.64326105948723,1.41336611178093);
#462=ELLIPSE('',#34562,4.51762701288,1.39428357264109);
#463=ELLIPSE('',#34573,0.257803751558044,0.175002130709107);
#464=ELLIPSE('',#34575,0.1975438935833,0.117585941695249);
#465=ELLIPSE('',#34583,0.249924507512202,0.163903784221422);
#466=ELLIPSE('',#34586,0.1975438935833,0.117585941695249);
#467=ELLIPSE('',#34754,0.0363695267596646,0.0157585247759226);
#468=ELLIPSE('',#34757,0.0363695267596646,0.0157585247759226);
#469=ELLIPSE('',#34761,0.0439364458692703,0.0199986358668788);
#470=ELLIPSE('',#34763,0.751422058778054,0.147149952825287);
#471=ELLIPSE('',#34765,20.1759483174618,1.96800786553162);
#472=ELLIPSE('',#34766,20.1759483174618,1.96800786553162);
#473=ELLIPSE('',#34768,0.751422058778054,0.147149952825287);
#474=ELLIPSE('',#34770,0.0439364458692703,0.0199986358668788);
#475=ELLIPSE('',#34772,0.299969315421473,0.299941755102118);
#476=ELLIPSE('',#34773,0.299972264763754,0.299945275725425);
#477=ELLIPSE('',#34774,0.0990009013291418,0.0878823615802462);
#478=ELLIPSE('',#34780,0.299972288094039,0.299945322652049);
#479=ELLIPSE('',#34781,0.299969314787288,0.299941753885528);
#480=ELLIPSE('',#34782,0.0990009013291418,0.0878823615802462);
#481=ELLIPSE('',#34793,0.7851617239929,0.0246669925758606);
#482=ELLIPSE('',#34796,0.7851617239929,0.0246669925758606);
#483=ELLIPSE('',#34825,8.3799208131191,7.21545183497513);
#484=ELLIPSE('',#34826,4.63750951971154,3.97939150633538);
#485=ELLIPSE('',#34827,0.279111750317682,0.0287889222318791);
#486=ELLIPSE('',#34828,0.279155849620574,0.0287979766923596);
#487=ELLIPSE('',#34829,4.63750644581462,3.97938959050038);
#488=ELLIPSE('',#34830,2.90419978119635,2.54008245675797);
#489=ELLIPSE('',#34832,8.37996203818539,7.2155054701837);
#490=ELLIPSE('',#34833,4.6362036535388,3.97712799641558);
#491=ELLIPSE('',#34834,4.63620357301174,3.97712785757339);
#492=ELLIPSE('',#34835,2.90476620332758,2.54108275826229);
#493=ELLIPSE('',#34836,0.298848921430035,0.296905429574988);
#494=ELLIPSE('',#34837,0.298848915091874,0.296905425010623);
#495=ELLIPSE('',#34838,2.60097379562585,2.25500631930886);
#496=ELLIPSE('',#34839,0.298848922240667,0.296905431566661);
#497=ELLIPSE('',#34840,2.60096854257791,2.25499721056391);
#498=ELLIPSE('',#34841,0.298849077415496,0.296905613510738);
#499=ELLIPSE('',#34843,0.298848945791595,0.296905486595381);
#500=ELLIPSE('',#34844,0.298848920821335,0.296905428111335);
#501=ELLIPSE('',#34845,0.298848930247292,0.29690545026939);
#502=ELLIPSE('',#34846,0.29884892225185,0.296905431603897);
#503=ELLIPSE('',#34847,0.298848926446922,0.296905441346893);
#504=ELLIPSE('',#34848,0.298848931059905,0.296905452258441);
#505=ELLIPSE('',#34849,0.298848921910928,0.296905430717524);
#506=ELLIPSE('',#34850,0.298848923110476,0.2969054336145);
#507=ELLIPSE('',#34851,0.298848920968869,0.296905428505602);
#508=ELLIPSE('',#34852,4.93548202851956,4.27020424069084);
#509=ELLIPSE('',#34853,4.93548202854622,4.27020424073721);
#510=ELLIPSE('',#34854,0.298848930560778,0.296905451093701);
#511=ELLIPSE('',#34855,0.298848867142046,0.29690533520481);
#512=ELLIPSE('',#34856,0.29884889306055,0.296905361405062);
#513=ELLIPSE('',#34860,0.298848921989232,0.296905430886302);
#514=ELLIPSE('',#34861,0.298848931849281,0.29690545410484);
#515=ELLIPSE('',#34862,0.298848907172553,0.296905413572369);
#516=ELLIPSE('',#34863,0.298848917642298,0.296905420688533);
#517=ELLIPSE('',#34864,0.298848921443323,0.296905430437503);
#518=ELLIPSE('',#34865,0.298848921699928,0.296905431123917);
#519=ELLIPSE('',#34866,0.298848934453035,0.296905460108951);
#520=ELLIPSE('',#34867,0.298848929099766,0.296905447642822);
#521=ELLIPSE('',#34868,0.298848923421217,0.296905434233442);
#522=ELLIPSE('',#34869,2.60895186279743,2.25339178646564);
#523=ELLIPSE('',#34870,2.60895186279368,2.25339178645907);
#524=ELLIPSE('',#34871,0.298848908378948,0.296905399041772);
#525=ELLIPSE('',#34872,0.298848920956384,0.296905429882047);
#526=ELLIPSE('',#34873,0.298848920542523,0.29690542750572);
#527=ELLIPSE('',#34874,0.298848922234712,0.296905431547994);
#528=ELLIPSE('',#34875,0.298848922247508,0.296905431596198);
#529=ELLIPSE('',#34876,0.298848920242847,0.296905428747462);
#530=ELLIPSE('',#34877,0.298848966327266,0.296905496668989);
#531=ELLIPSE('',#34878,0.298849039002102,0.296905705367311);
#532=ELLIPSE('',#34879,0.29884891584007,0.296905416549116);
#533=ELLIPSE('',#34880,0.29884892201266,0.296905430947192);
#534=ELLIPSE('',#34881,2.60146235146488,2.25585351865204);
#535=ELLIPSE('',#34882,2.60146235146488,2.25585351865204);
#536=ELLIPSE('',#34883,0.298848922283708,0.296905431682282);
#537=ELLIPSE('',#34886,0.298848921993761,0.296905430900167);
#538=ELLIPSE('',#34888,0.298848922246914,0.296905431583466);
#539=ELLIPSE('',#34890,0.298848844698996,0.29690524961801);
#540=ELLIPSE('',#34891,0.298848922270607,0.296905431629623);
#541=ELLIPSE('',#34892,0.298848920959998,0.296905428481053);
#542=ELLIPSE('',#34893,4.93548202854677,4.27020424073817);
#543=ELLIPSE('',#34894,4.93548202854677,4.27020424073817);
#544=ELLIPSE('',#34895,0.298848930553665,0.29690545107324);
#545=ELLIPSE('',#34896,0.298848903185399,0.296905386777569);
#546=ELLIPSE('',#34897,0.298848895686848,0.296905369235784);
#547=ELLIPSE('',#34898,0.298848888559201,0.296905352560715);
#548=ELLIPSE('',#34899,0.298848922192621,0.296905431506102);
#549=ELLIPSE('',#34900,0.298848921998645,0.296905430922456);
#550=ELLIPSE('',#34901,0.298848922257891,0.296905431618786);
#551=ELLIPSE('',#34902,0.298848922085066,0.296905431050029);
#552=ELLIPSE('',#34903,0.298848921299427,0.296905430686572);
#553=ELLIPSE('',#34904,0.298848903202731,0.296905386834583);
#554=ELLIPSE('',#34905,0.298848888580021,0.296905352625924);
#555=ELLIPSE('',#34906,0.298848921981868,0.296905430864804);
#556=ELLIPSE('',#34907,0.298848909286409,0.296905401179665);
#557=ELLIPSE('',#34908,0.298848920591055,0.296905427635518);
#558=ELLIPSE('',#34909,0.298848922344033,0.296905431832649);
#559=ELLIPSE('',#34910,0.298848921961888,0.296905430820688);
#560=ELLIPSE('',#34911,0.298848922215141,0.296905431504259);
#561=ELLIPSE('',#34912,0.298848922001989,0.296905430644444);
#562=ELLIPSE('',#34913,0.298848941683903,0.296905477135918);
#563=ELLIPSE('',#34914,0.29884892196829,0.296905430801925);
#564=ELLIPSE('',#34915,8.67731949920772,7.50537904899086);
#565=ELLIPSE('',#34916,0.298848909045585,0.29690540101209);
#566=ELLIPSE('',#34917,8.67731949917931,7.50537904894157);
#567=ELLIPSE('',#34918,0.298848902335981,0.296905383066002);
#568=ELLIPSE('',#34919,0.298848920767452,0.296905427460604);
#569=ELLIPSE('',#34935,0.298848919318477,0.296905424707719);
#570=ELLIPSE('',#34936,0.298848892580485,0.296905360939291);
#571=ELLIPSE('',#34940,0.298848920090728,0.296905426638253);
#572=ELLIPSE('',#34941,0.29884889341624,0.296905361759044);
#573=ELLIPSE('',#34943,0.298848922260772,0.296905431625149);
#574=ELLIPSE('',#34945,0.298848920759339,0.296905428089205);
#575=ELLIPSE('',#34946,0.29884891933117,0.296905424743563);
#576=ELLIPSE('',#34947,0.298848915871755,0.296905416638318);
#577=ELLIPSE('',#34948,0.298848919843559,0.296905425953451);
#578=ELLIPSE('',#34949,0.298848891288725,0.296905359078035);
#579=ELLIPSE('',#34950,0.298848918410882,0.296905426718576);
#580=ELLIPSE('',#34951,0.298848922900226,0.296905433124464);
#581=ELLIPSE('',#34952,0.298848913927389,0.296905412076352);
#582=ELLIPSE('',#34953,0.298848922234263,0.296905431565699);
#583=ELLIPSE('',#34954,0.298848922236084,0.296905431557407);
#584=ELLIPSE('',#34956,0.298848891608559,0.296905359578392);
#585=ELLIPSE('',#34958,0.298848942238611,0.296905478386828);
#586=ELLIPSE('',#34959,0.298848922236084,0.296905431557407);
#587=ELLIPSE('',#35016,13.361638124116,11.5578357668316);
#588=ELLIPSE('',#35018,0.952789221356583,0.825051280209737);
#589=ELLIPSE('',#35164,8.5034308409691,7.3551645679647);
#590=ELLIPSE('',#35170,0.95278921998829,0.825051277838727);
#591=ELLIPSE('',#35172,13.3616381240247,11.5578357666725);
#592=ELLIPSE('',#35175,13.3641581201969,11.5586227277888);
#593=ELLIPSE('',#35177,13.3735436793885,11.5615411739172);
#594=ELLIPSE('',#35193,13.3735436794947,11.5615411741025);
#595=ELLIPSE('',#35195,13.3641581202021,11.5586227277978);
#596=ELLIPSE('',#35373,5.47251735374185,5.45746583056251);
#597=ELLIPSE('',#35374,5.47484463449433,5.45859738058976);
#598=ELLIPSE('',#35383,1586.78234781094,77.5099567232996);
#599=ELLIPSE('',#35385,1.14101622851481,0.979516364167449);
#600=ELLIPSE('',#35388,3.21318791213204,0.733552647206039);
#601=ELLIPSE('',#35393,9.5906032530047,5.82945480771065);
#602=ELLIPSE('',#35396,9.59060325044611,5.82945480684165);
#603=ELLIPSE('',#35401,1586.78234781094,77.5099567232996);
#604=ELLIPSE('',#35402,1.14101622838842,0.979516363971379);
#605=ELLIPSE('',#35405,3.21319255571472,0.733554698090194);
#606=ELLIPSE('',#35728,0.35400824521659,0.325120639664921);
#607=ELLIPSE('',#35730,0.26079295230188,0.225428549013028);
#608=ELLIPSE('',#35733,0.298959427554072,0.296143919662364);
#609=ELLIPSE('',#35753,0.260785485861866,0.225415709617204);
#610=ELLIPSE('',#35755,0.354058541716697,0.325144371990916);
#611=ELLIPSE('',#35805,0.298848922732419,0.296905432652653);
#612=ELLIPSE('',#35824,0.298891660055286,0.297093982021653);
#613=ELLIPSE('',#35833,0.298979043963965,0.297433001748831);
#614=ELLIPSE('',#35835,0.298894659298114,0.297106043484314);
#615=ELLIPSE('',#35836,0.298977328382314,0.297429112568373);
#616=ELLIPSE('',#35932,0.14142135623731,0.1);
#617=ELLIPSE('',#36133,0.14142135623731,0.1);
#618=ELLIPSE('',#36348,0.298848922836507,0.296905432909967);
#619=ELLIPSE('',#36349,0.298979123737475,0.29743317011586);
#620=ELLIPSE('',#36360,0.298979307954305,0.297433587262778);
#621=ELLIPSE('',#36361,0.298894247034695,0.297105377501926);
#622=ELLIPSE('',#36365,0.298891932661897,0.29709461276469);
#623=ELLIPSE('',#36366,0.298848892860348,0.296905360884096);
#624=ELLIPSE('',#36463,0.633386697976725,0.600234218712226);
#625=ELLIPSE('',#36470,0.298848745481257,0.296905215937904);
#626=ELLIPSE('',#36481,0.298864249839058,0.2969781551131);
#627=ELLIPSE('',#36482,0.635896586711713,0.60270133395858);
#628=ELLIPSE('',#36483,0.298848747221063,0.29690521700943);
#629=ELLIPSE('',#36505,0.633386697976725,0.600234218712226);
#630=ELLIPSE('',#36515,0.361788189515145,0.300001798267345);
#631=ELLIPSE('',#36516,0.298848773865698,0.296905284176984);
#632=ELLIPSE('',#36519,12.0546709739503,2.90799426775398);
#633=ELLIPSE('',#36527,0.298864504195414,0.296977933551803);
#634=ELLIPSE('',#36528,0.298848775543376,0.296905285050702);
#635=ELLIPSE('',#36529,0.635896586711713,0.60270133395858);
#636=ELLIPSE('',#36609,0.616948377444998,0.596990574629877);
#637=ELLIPSE('',#36774,0.298848892782947,0.2969053606671);
#638=ELLIPSE('',#36784,0.723457342561266,0.612142527579512);
#639=ELLIPSE('',#36787,0.839901750727128,0.325201544662394);
#640=ELLIPSE('',#36791,0.839902765005034,0.32520200920329);
#641=ELLIPSE('',#36792,0.855720879944736,0.334538055133644);
#642=ELLIPSE('',#36796,0.978504400650312,0.43206650732588);
#643=ELLIPSE('',#36807,0.298987522088764,0.297463090341305);
#644=ELLIPSE('',#36864,0.0996163073938246,0.0989684771695573);
#645=ELLIPSE('',#36865,0.0996064607576122,0.098921046723739);
#646=ELLIPSE('',#36870,0.0996019636355457,0.0988979538729398);
#647=ELLIPSE('',#36871,0.83480328877623,0.449020774204173);
#648=ELLIPSE('',#36872,0.0996163010870433,0.0989684579736212);
#649=ELLIPSE('',#36873,0.0996019611035896,0.0988979479073979);
#650=ELLIPSE('',#36874,0.95881614661924,0.545128833125042);
#651=ELLIPSE('',#36888,0.0996019636635876,0.0988979539393061);
#652=ELLIPSE('',#36889,0.834793007766825,0.449012007377356);
#653=ELLIPSE('',#36890,0.0996163011297496,0.0989684580705834);
#654=ELLIPSE('',#36891,0.0996019612880109,0.0988979483606112);
#655=ELLIPSE('',#36892,0.0996163073978892,0.0989684771734698);
#656=ELLIPSE('',#36893,0.842981617008318,0.456043592675208);
#657=ELLIPSE('',#37011,0.298848927783278,0.296905444507015);
#658=ELLIPSE('',#37012,0.299091836143122,0.297812318683333);
#659=ELLIPSE('',#37015,0.299092017159912,0.297812365396506);
#660=ELLIPSE('',#37030,0.298848921977966,0.296905430756493);
#661=ELLIPSE('',#37033,0.358196202460482,0.312309449719818);
#662=ELLIPSE('',#37114,0.299085253265536,0.297791465794382);
#663=ELLIPSE('',#37167,0.298848922572082,0.296905433095193);
#664=ELLIPSE('',#37196,0.48575646188926,0.315209432805966);
#665=ELLIPSE('',#37197,0.298848922223572,0.296905431591445);
#666=ELLIPSE('',#37198,0.298976384440305,0.297423661821599);
#667=ELLIPSE('',#37201,0.298848893179516,0.296905361743558);
#668=ELLIPSE('',#37203,0.298849004322787,0.296905465668005);
#669=ELLIPSE('',#37209,0.299077289129448,0.297765861381808);
#670=ELLIPSE('',#37233,0.2988599234424,0.296955631862372);
#671=ELLIPSE('',#37234,0.311781310291398,0.301461130998388);
#672=ELLIPSE('',#37302,0.616948377444998,0.596990574629877);
#673=ELLIPSE('',#37475,0.298848921980292,0.296905430856554);
#674=ELLIPSE('',#37488,0.723457342561266,0.612142527579512);
#675=ELLIPSE('',#37496,0.855721443648946,0.334538377478706);
#676=ELLIPSE('',#37500,0.839900853126743,0.325201217495182);
#677=ELLIPSE('',#37501,0.855721622372424,0.334538483108095);
#678=ELLIPSE('',#37576,0.0996064588793403,0.0989210426276871);
#679=ELLIPSE('',#37577,0.0996163153029603,0.0989684770999027);
#680=ELLIPSE('',#37582,0.0996163073887366,0.0989684771505584);
#681=ELLIPSE('',#37583,0.842986353714893,0.456047441690848);
#682=ELLIPSE('',#37584,0.0996019612459525,0.0988979482541347);
#683=ELLIPSE('',#37585,0.0996019632515573,0.0988979536268878);
#684=ELLIPSE('',#37599,0.0996163073858426,0.0989684771452112);
#685=ELLIPSE('',#37600,0.84298514231536,0.456046449061635);
#686=ELLIPSE('',#37601,0.0996019612550026,0.0988979482814453);
#687=ELLIPSE('',#37602,0.0996019632510724,0.0988979536158697);
#688=ELLIPSE('',#37603,0.83479393416711,0.449012748427101);
#689=ELLIPSE('',#37604,0.0996163011297535,0.0989684580706061);
#690=ELLIPSE('',#37764,0.299091892234915,0.297812430528943);
#691=ELLIPSE('',#37765,0.298848892822638,0.296905360819338);
#692=ELLIPSE('',#37767,0.298848925852848,0.296905440053724);
#693=ELLIPSE('',#37768,0.299092010660396,0.29781235080905);
#694=ELLIPSE('',#37796,0.358196201537078,0.312309449169694);
#695=ELLIPSE('',#37927,0.298848900003069,0.29690537960284);
#696=ELLIPSE('',#37955,0.298848922307858,0.296905431614744);
#697=ELLIPSE('',#37956,0.298976199239788,0.29742370304314);
#698=ELLIPSE('',#37957,0.298848893194714,0.296905361846251);
#699=ELLIPSE('',#37958,0.48575646188926,0.315209432805966);
#700=ELLIPSE('',#37960,0.298848918312141,0.296905422207127);
#701=ELLIPSE('',#37961,0.298848927446579,0.29690544380809);
#702=ELLIPSE('',#37963,0.298849777080326,0.296906780571315);
#703=ELLIPSE('',#38001,0.299077129594657,0.297765592394515);
#704=ELLIPSE('',#38020,0.311781310291398,0.301461130998388);
#705=ELLIPSE('',#38021,0.2988599234424,0.296955631862372);
#706=ELLIPSE('',#38289,0.298848923957396,0.296905362261884);
#707=ELLIPSE('',#38314,0.2988489185537,0.296905422816142);
#708=ELLIPSE('',#38324,0.298848919017662,0.29690542389071);
#709=ELLIPSE('',#38343,0.298849404757611,0.296905780207238);
#710=SPHERICAL_SURFACE('',#34346,0.3);
#711=SPHERICAL_SURFACE('',#34785,0.3);
#712=SPHERICAL_SURFACE('',#35503,0.3);
#713=SPHERICAL_SURFACE('',#35507,0.3);
#714=SPHERICAL_SURFACE('',#35514,0.3);
#715=SPHERICAL_SURFACE('',#35522,0.3);
#716=SPHERICAL_SURFACE('',#35527,0.3);
#717=SPHERICAL_SURFACE('',#35532,0.3);
#718=SPHERICAL_SURFACE('',#35559,0.3);
#719=SPHERICAL_SURFACE('',#35563,0.3);
#720=SPHERICAL_SURFACE('',#35570,0.3);
#721=SPHERICAL_SURFACE('',#35578,0.3);
#722=SPHERICAL_SURFACE('',#35583,0.3);
#723=SPHERICAL_SURFACE('',#35588,0.3);
#724=SPHERICAL_SURFACE('',#35617,0.3);
#725=SPHERICAL_SURFACE('',#35621,0.3);
#726=SPHERICAL_SURFACE('',#35628,0.3);
#727=SPHERICAL_SURFACE('',#35636,0.3);
#728=SPHERICAL_SURFACE('',#35641,0.3);
#729=SPHERICAL_SURFACE('',#35646,0.3);
#730=SPHERICAL_SURFACE('',#35673,0.3);
#731=SPHERICAL_SURFACE('',#35677,0.3);
#732=SPHERICAL_SURFACE('',#35686,0.3);
#733=SPHERICAL_SURFACE('',#35691,0.3);
#734=SPHERICAL_SURFACE('',#35697,0.3);
#735=SPHERICAL_SURFACE('',#35700,0.3);
#736=SPHERICAL_SURFACE('',#35769,0.3);
#737=SPHERICAL_SURFACE('',#35775,4.45);
#738=SPHERICAL_SURFACE('',#35788,0.3);
#739=SPHERICAL_SURFACE('',#35899,0.3);
#740=SPHERICAL_SURFACE('',#36036,0.3);
#741=SPHERICAL_SURFACE('',#36040,0.3);
#742=SPHERICAL_SURFACE('',#36047,0.3);
#743=SPHERICAL_SURFACE('',#36063,0.1);
#744=SPHERICAL_SURFACE('',#36068,0.1);
#745=SPHERICAL_SURFACE('',#36086,0.1);
#746=SPHERICAL_SURFACE('',#36089,0.1);
#747=SPHERICAL_SURFACE('',#36095,0.1);
#748=SPHERICAL_SURFACE('',#36098,0.1);
#749=SPHERICAL_SURFACE('',#36126,0.3);
#750=SPHERICAL_SURFACE('',#36199,0.1);
#751=SPHERICAL_SURFACE('',#36223,0.3);
#752=SPHERICAL_SURFACE('',#36227,0.3);
#753=SPHERICAL_SURFACE('',#36245,0.1);
#754=SPHERICAL_SURFACE('',#36246,0.1);
#755=SPHERICAL_SURFACE('',#36247,0.1);
#756=SPHERICAL_SURFACE('',#36248,0.1);
#757=SPHERICAL_SURFACE('',#36265,0.3);
#758=SPHERICAL_SURFACE('',#36308,0.1);
#759=SPHERICAL_SURFACE('',#36631,0.3);
#760=SPHERICAL_SURFACE('',#36636,0.3);
#761=SPHERICAL_SURFACE('',#36660,0.3);
#762=SPHERICAL_SURFACE('',#36665,0.3);
#763=SPHERICAL_SURFACE('',#36690,0.3);
#764=SPHERICAL_SURFACE('',#36695,0.3);
#765=SPHERICAL_SURFACE('',#36705,0.3);
#766=SPHERICAL_SURFACE('',#36721,0.3);
#767=SPHERICAL_SURFACE('',#36724,0.3);
#768=SPHERICAL_SURFACE('',#36728,0.3);
#769=SPHERICAL_SURFACE('',#36731,0.3);
#770=SPHERICAL_SURFACE('',#36759,0.3);
#771=SPHERICAL_SURFACE('',#36800,0.3);
#772=SPHERICAL_SURFACE('',#36930,0.3);
#773=SPHERICAL_SURFACE('',#36936,0.3);
#774=SPHERICAL_SURFACE('',#36939,0.3);
#775=SPHERICAL_SURFACE('',#36942,0.3);
#776=SPHERICAL_SURFACE('',#36966,0.3);
#777=SPHERICAL_SURFACE('',#36971,0.3);
#778=SPHERICAL_SURFACE('',#37003,0.3);
#779=SPHERICAL_SURFACE('',#37016,0.3);
#780=SPHERICAL_SURFACE('',#37021,0.3);
#781=SPHERICAL_SURFACE('',#37037,0.3);
#782=SPHERICAL_SURFACE('',#37043,0.3);
#783=SPHERICAL_SURFACE('',#37048,0.3);
#784=SPHERICAL_SURFACE('',#37050,0.3);
#785=SPHERICAL_SURFACE('',#37057,0.3);
#786=SPHERICAL_SURFACE('',#37089,0.3);
#787=SPHERICAL_SURFACE('',#37093,0.3);
#788=SPHERICAL_SURFACE('',#37095,0.3);
#789=SPHERICAL_SURFACE('',#37100,0.3);
#790=SPHERICAL_SURFACE('',#37101,0.3);
#791=SPHERICAL_SURFACE('',#37110,0.3);
#792=SPHERICAL_SURFACE('',#37117,0.3);
#793=SPHERICAL_SURFACE('',#37122,0.3);
#794=SPHERICAL_SURFACE('',#37145,0.3);
#795=SPHERICAL_SURFACE('',#37152,0.3);
#796=SPHERICAL_SURFACE('',#37162,0.3);
#797=SPHERICAL_SURFACE('',#37258,0.3);
#798=SPHERICAL_SURFACE('',#37267,0.3);
#799=SPHERICAL_SURFACE('',#37272,0.3);
#800=SPHERICAL_SURFACE('',#37277,0.3);
#801=SPHERICAL_SURFACE('',#37280,0.3);
#802=SPHERICAL_SURFACE('',#37284,0.3);
#803=SPHERICAL_SURFACE('',#37326,0.3);
#804=SPHERICAL_SURFACE('',#37331,0.3);
#805=SPHERICAL_SURFACE('',#37355,0.3);
#806=SPHERICAL_SURFACE('',#37360,0.3);
#807=SPHERICAL_SURFACE('',#37387,0.3);
#808=SPHERICAL_SURFACE('',#37392,0.3);
#809=SPHERICAL_SURFACE('',#37403,0.3);
#810=SPHERICAL_SURFACE('',#37421,0.3);
#811=SPHERICAL_SURFACE('',#37424,0.3);
#812=SPHERICAL_SURFACE('',#37428,0.3);
#813=SPHERICAL_SURFACE('',#37431,0.3);
#814=SPHERICAL_SURFACE('',#37459,0.3);
#815=SPHERICAL_SURFACE('',#37508,0.3);
#816=SPHERICAL_SURFACE('',#37640,0.3);
#817=SPHERICAL_SURFACE('',#37646,0.3);
#818=SPHERICAL_SURFACE('',#37649,0.3);
#819=SPHERICAL_SURFACE('',#37652,0.3);
#820=SPHERICAL_SURFACE('',#37675,0.3);
#821=SPHERICAL_SURFACE('',#37682,0.3);
#822=SPHERICAL_SURFACE('',#37757,0.3);
#823=SPHERICAL_SURFACE('',#37769,0.3);
#824=SPHERICAL_SURFACE('',#37787,0.3);
#825=SPHERICAL_SURFACE('',#37801,0.3);
#826=SPHERICAL_SURFACE('',#37806,0.3);
#827=SPHERICAL_SURFACE('',#37810,0.3);
#828=SPHERICAL_SURFACE('',#37812,0.3);
#829=SPHERICAL_SURFACE('',#37817,0.3);
#830=SPHERICAL_SURFACE('',#37848,0.3);
#831=SPHERICAL_SURFACE('',#37852,0.3);
#832=SPHERICAL_SURFACE('',#37854,0.3);
#833=SPHERICAL_SURFACE('',#37859,0.3);
#834=SPHERICAL_SURFACE('',#37860,0.3);
#835=SPHERICAL_SURFACE('',#37869,0.3);
#836=SPHERICAL_SURFACE('',#37876,0.3);
#837=SPHERICAL_SURFACE('',#37879,0.3);
#838=SPHERICAL_SURFACE('',#37905,0.3);
#839=SPHERICAL_SURFACE('',#37911,0.3);
#840=SPHERICAL_SURFACE('',#37922,0.3);
#841=SPHERICAL_SURFACE('',#38045,0.3);
#842=SPHERICAL_SURFACE('',#38054,0.3);
#843=SPHERICAL_SURFACE('',#38059,0.3);
#844=SPHERICAL_SURFACE('',#38065,0.3);
#845=SPHERICAL_SURFACE('',#38069,0.3);
#846=SPHERICAL_SURFACE('',#38074,0.3);
#847=SPHERICAL_SURFACE('',#38146,0.3);
#848=SPHERICAL_SURFACE('',#38154,0.3);
#849=SPHERICAL_SURFACE('',#38166,0.3);
#850=SPHERICAL_SURFACE('',#38177,0.3);
#851=SPHERICAL_SURFACE('',#38195,0.3);
#852=SPHERICAL_SURFACE('',#38214,0.3);
#853=SPHERICAL_SURFACE('',#38274,0.3);
#854=SPHERICAL_SURFACE('',#38278,0.3);
#855=SPHERICAL_SURFACE('',#38298,0.3);
#856=SPHERICAL_SURFACE('',#38303,0.3);
#857=SPHERICAL_SURFACE('',#38327,0.3);
#858=SPHERICAL_SURFACE('',#38331,0.3);
#859=SPHERICAL_SURFACE('',#38392,4.49);
#860=SPHERICAL_SURFACE('',#38586,0.3);
#861=SPHERICAL_SURFACE('',#38596,0.3);
#862=B_SPLINE_SURFACE_WITH_KNOTS('',5,1,((#49366,#49367),(#49368,#49369),
(#49370,#49371),(#49372,#49373),(#49374,#49375),(#49376,#49377),(#49378,
#49379),(#49380,#49381),(#49382,#49383)),.UNSPECIFIED.,.F.,.F.,.F.,(6,3,
6),(2,2),(0.,2.10936312981,4.22279623369),(0.,3.10437234689),
 .UNSPECIFIED.);
#863=B_SPLINE_SURFACE_WITH_KNOTS('',5,1,((#49466,#49467),(#49468,#49469),
(#49470,#49471),(#49472,#49473),(#49474,#49475),(#49476,#49477),(#49478,
#49479),(#49480,#49481),(#49482,#49483)),.UNSPECIFIED.,.F.,.F.,.F.,(6,3,
6),(2,2),(0.11111371251,1.22636799075,2.75103476973),(0.,0.108300515181936),
 .UNSPECIFIED.);
#864=B_SPLINE_SURFACE_WITH_KNOTS('',5,1,((#49587,#49588),(#49589,#49590),
(#49591,#49592),(#49593,#49594),(#49595,#49596),(#49597,#49598),(#49599,
#49600),(#49601,#49602),(#49603,#49604),(#49605,#49606),(#49607,#49608),
(#49609,#49610),(#49611,#49612),(#49613,#49614),(#49615,#49616),(#49617,
#49618),(#49619,#49620),(#49621,#49622)),.UNSPECIFIED.,.F.,.F.,.F.,(6,3,
3,3,3,6),(2,2),(0.465128126763,3.42050470566,7.30063973795,10.0042092191,
12.4987596036,13.1731669678),(0.,0.115270049227219),.UNSPECIFIED.);
#865=B_SPLINE_SURFACE_WITH_KNOTS('',5,1,((#49746,#49747),(#49748,#49749),
(#49750,#49751),(#49752,#49753),(#49754,#49755),(#49756,#49757)),
 .UNSPECIFIED.,.F.,.F.,.F.,(6,6),(2,2),(0.,1.62525620495),(0.,0.103685293259447),
 .UNSPECIFIED.);
#866=B_SPLINE_SURFACE_WITH_KNOTS('',5,1,((#49791,#49792),(#49793,#49794),
(#49795,#49796),(#49797,#49798),(#49799,#49800),(#49801,#49802),(#49803,
#49804),(#49805,#49806),(#49807,#49808),(#49809,#49810),(#49811,#49812),
(#49813,#49814),(#49815,#49816),(#49817,#49818),(#49819,#49820)),
 .UNSPECIFIED.,.F.,.F.,.F.,(6,3,3,3,6),(2,2),(0.617889185003,0.915206541473,
1.58780472511,2.42003303229,2.57855093571),(0.,0.109749059692414),
 .UNSPECIFIED.);
#867=B_SPLINE_SURFACE_WITH_KNOTS('',5,1,((#49873,#49874),(#49875,#49876),
(#49877,#49878),(#49879,#49880),(#49881,#49882),(#49883,#49884)),
 .UNSPECIFIED.,.F.,.F.,.F.,(6,6),(2,2),(0.,0.788840280269),(0.,0.12),
 .UNSPECIFIED.);
#868=B_SPLINE_SURFACE_WITH_KNOTS('',5,1,((#49932,#49933),(#49934,#49935),
(#49936,#49937),(#49938,#49939),(#49940,#49941),(#49942,#49943),(#49944,
#49945),(#49946,#49947),(#49948,#49949)),.UNSPECIFIED.,.F.,.F.,.F.,(6,3,
6),(2,2),(0.248824060028,2.99459552346,6.14853595161),(0.,0.120001139724),
 .UNSPECIFIED.);
#869=B_SPLINE_SURFACE_WITH_KNOTS('',5,1,((#50067,#50068),(#50069,#50070),
(#50071,#50072),(#50073,#50074),(#50075,#50076),(#50077,#50078),(#50079,
#50080),(#50081,#50082),(#50083,#50084)),.UNSPECIFIED.,.F.,.F.,.F.,(6,3,
6),(2,2),(0.11111371251,1.22636799075,2.75103476973),(0.,0.108300515181936),
 .UNSPECIFIED.);
#870=B_SPLINE_SURFACE_WITH_KNOTS('',5,1,((#50165,#50166),(#50167,#50168),
(#50169,#50170),(#50171,#50172),(#50173,#50174),(#50175,#50176),(#50177,
#50178),(#50179,#50180),(#50181,#50182)),.UNSPECIFIED.,.F.,.F.,.F.,(6,3,
6),(2,2),(0.248824060028,2.99459552346,6.14853595161),(0.,0.120001139724),
 .UNSPECIFIED.);
#871=B_SPLINE_SURFACE_WITH_KNOTS('',5,1,((#50281,#50282),(#50283,#50284),
(#50285,#50286),(#50287,#50288),(#50289,#50290),(#50291,#50292)),
 .UNSPECIFIED.,.F.,.F.,.F.,(6,6),(2,2),(0.,0.788840280269),(0.,0.12),
 .UNSPECIFIED.);
#872=B_SPLINE_SURFACE_WITH_KNOTS('',5,1,((#50340,#50341),(#50342,#50343),
(#50344,#50345),(#50346,#50347),(#50348,#50349),(#50350,#50351),(#50352,
#50353),(#50354,#50355),(#50356,#50357),(#50358,#50359),(#50360,#50361),
(#50362,#50363),(#50364,#50365),(#50366,#50367),(#50368,#50369)),
 .UNSPECIFIED.,.F.,.F.,.F.,(6,3,3,3,6),(2,2),(0.617889185003,0.915206541473,
1.58780472511,2.42003303229,2.57855093571),(0.,0.109749059692414),
 .UNSPECIFIED.);
#873=B_SPLINE_SURFACE_WITH_KNOTS('',5,1,((#50555,#50556),(#50557,#50558),
(#50559,#50560),(#50561,#50562),(#50563,#50564),(#50565,#50566)),
 .UNSPECIFIED.,.F.,.F.,.F.,(6,6),(2,2),(0.,1.62525620495),(0.,0.103685293259447),
 .UNSPECIFIED.);
#874=B_SPLINE_SURFACE_WITH_KNOTS('',5,1,((#50600,#50601),(#50602,#50603),
(#50604,#50605),(#50606,#50607),(#50608,#50609),(#50610,#50611),(#50612,
#50613),(#50614,#50615),(#50616,#50617),(#50618,#50619),(#50620,#50621),
(#50622,#50623),(#50624,#50625),(#50626,#50627),(#50628,#50629),(#50630,
#50631),(#50632,#50633),(#50634,#50635)),.UNSPECIFIED.,.F.,.F.,.F.,(6,3,
3,3,3,6),(2,2),(0.465128126763,3.42050470566,7.30063973795,10.0042092191,
12.4987596036,13.1731669678),(0.,0.115270054056779),.UNSPECIFIED.);
#875=B_SPLINE_SURFACE_WITH_KNOTS('',5,1,((#51251,#51252),(#51253,#51254),
(#51255,#51256),(#51257,#51258),(#51259,#51260),(#51261,#51262)),
 .UNSPECIFIED.,.F.,.F.,.F.,(6,6),(2,2),(0.,0.600083611309),(0.,3.10437234689),
 .UNSPECIFIED.);
#876=B_SPLINE_SURFACE_WITH_KNOTS('',5,1,((#51336,#51337),(#51338,#51339),
(#51340,#51341),(#51342,#51343),(#51344,#51345),(#51346,#51347)),
 .UNSPECIFIED.,.F.,.F.,.F.,(6,6),(2,2),(0.,0.226010362356),(0.,3.10437234689),
 .UNSPECIFIED.);
#877=B_SPLINE_SURFACE_WITH_KNOTS('',5,1,((#51368,#51369),(#51370,#51371),
(#51372,#51373),(#51374,#51375),(#51376,#51377),(#51378,#51379),(#51380,
#51381),(#51382,#51383),(#51384,#51385),(#51386,#51387),(#51388,#51389),
(#51390,#51391)),.UNSPECIFIED.,.F.,.F.,.F.,(6,3,3,6),(2,2),(0.,2.83532528452,
6.09533201542,9.83397913335),(0.,3.10437234689),.UNSPECIFIED.);
#878=B_SPLINE_SURFACE_WITH_KNOTS('',5,1,((#51471,#51472),(#51473,#51474),
(#51475,#51476),(#51477,#51478),(#51479,#51480),(#51481,#51482)),
 .UNSPECIFIED.,.F.,.F.,.F.,(6,6),(2,2),(0.,0.224378834114),(0.,3.10437234689),
 .UNSPECIFIED.);
#879=B_SPLINE_SURFACE_WITH_KNOTS('',5,1,((#51514,#51515),(#51516,#51517),
(#51518,#51519),(#51520,#51521),(#51522,#51523),(#51524,#51525)),
 .UNSPECIFIED.,.F.,.F.,.F.,(6,6),(2,2),(0.,0.2489231439),(0.,3.10437234689),
 .UNSPECIFIED.);
#880=B_SPLINE_SURFACE_WITH_KNOTS('',5,1,((#51570,#51571),(#51572,#51573),
(#51574,#51575),(#51576,#51577),(#51578,#51579),(#51580,#51581),(#51582,
#51583),(#51584,#51585),(#51586,#51587),(#51588,#51589),(#51590,#51591),
(#51592,#51593)),.UNSPECIFIED.,.F.,.F.,.F.,(6,3,3,6),(2,2),(0.,0.629547398659,
1.2493532974,1.86132516749),(0.,3.10437234689),.UNSPECIFIED.);
#881=B_SPLINE_SURFACE_WITH_KNOTS('',5,1,((#51679,#51680),(#51681,#51682),
(#51683,#51684),(#51685,#51686),(#51687,#51688),(#51689,#51690)),
 .UNSPECIFIED.,.F.,.F.,.F.,(6,6),(2,2),(0.,0.482067685837),(0.,3.10437234689),
 .UNSPECIFIED.);
#882=B_SPLINE_SURFACE_WITH_KNOTS('',5,1,((#51717,#51718),(#51719,#51720),
(#51721,#51722),(#51723,#51724),(#51725,#51726),(#51727,#51728)),
 .UNSPECIFIED.,.F.,.F.,.F.,(6,6),(2,2),(0.,1.84813202664),(0.,3.10437234689),
 .UNSPECIFIED.);
#883=B_SPLINE_SURFACE_WITH_KNOTS('',5,5,((#51829,#51830,#51831,#51832,#51833,
#51834),(#51835,#51836,#51837,#51838,#51839,#51840),(#51841,#51842,#51843,
#51844,#51845,#51846),(#51847,#51848,#51849,#51850,#51851,#51852),(#51853,
#51854,#51855,#51856,#51857,#51858),(#51859,#51860,#51861,#51862,#51863,
#51864)),.UNSPECIFIED.,.F.,.F.,.F.,(6,6),(6,6),(0.840058180513,4.79280767082),
(0.,1.),.UNSPECIFIED.);
#884=B_SPLINE_SURFACE_WITH_KNOTS('',5,5,((#51900,#51901,#51902,#51903,#51904,
#51905),(#51906,#51907,#51908,#51909,#51910,#51911),(#51912,#51913,#51914,
#51915,#51916,#51917),(#51918,#51919,#51920,#51921,#51922,#51923),(#51924,
#51925,#51926,#51927,#51928,#51929),(#51930,#51931,#51932,#51933,#51934,
#51935),(#51936,#51937,#51938,#51939,#51940,#51941),(#51942,#51943,#51944,
#51945,#51946,#51947),(#51948,#51949,#51950,#51951,#51952,#51953)),
 .UNSPECIFIED.,.F.,.F.,.F.,(6,3,6),(6,6),(0.225815728085,0.523709124902,
0.747252061964),(0.,1.),.UNSPECIFIED.);
#885=B_SPLINE_SURFACE_WITH_KNOTS('',5,5,((#51995,#51996,#51997,#51998,#51999,
#52000),(#52001,#52002,#52003,#52004,#52005,#52006),(#52007,#52008,#52009,
#52010,#52011,#52012),(#52013,#52014,#52015,#52016,#52017,#52018),(#52019,
#52020,#52021,#52022,#52023,#52024),(#52025,#52026,#52027,#52028,#52029,
#52030)),.UNSPECIFIED.,.F.,.F.,.F.,(6,6),(6,6),(1.28339894164,1.34350433703),
(0.,1.),.UNSPECIFIED.);
#886=B_SPLINE_SURFACE_WITH_KNOTS('',5,5,((#52045,#52046,#52047,#52048,#52049,
#52050),(#52051,#52052,#52053,#52054,#52055,#52056),(#52057,#52058,#52059,
#52060,#52061,#52062),(#52063,#52064,#52065,#52066,#52067,#52068),(#52069,
#52070,#52071,#52072,#52073,#52074),(#52075,#52076,#52077,#52078,#52079,
#52080)),.UNSPECIFIED.,.F.,.F.,.F.,(6,6),(6,6),(1.036743613,1.10280574369),
(0.,1.),.UNSPECIFIED.);
#887=B_SPLINE_SURFACE_WITH_KNOTS('',5,5,((#52086,#52087,#52088,#52089,#52090,
#52091),(#52092,#52093,#52094,#52095,#52096,#52097),(#52098,#52099,#52100,
#52101,#52102,#52103),(#52104,#52105,#52106,#52107,#52108,#52109),(#52110,
#52111,#52112,#52113,#52114,#52115),(#52116,#52117,#52118,#52119,#52120,
#52121),(#52122,#52123,#52124,#52125,#52126,#52127),(#52128,#52129,#52130,
#52131,#52132,#52133),(#52134,#52135,#52136,#52137,#52138,#52139)),
 .UNSPECIFIED.,.F.,.F.,.F.,(6,3,6),(6,6),(0.342430056326,0.787545489389,
1.14838178471),(0.,1.),.UNSPECIFIED.);
#888=B_SPLINE_SURFACE_WITH_KNOTS('',5,5,((#52179,#52180,#52181,#52182,#52183,
#52184),(#52185,#52186,#52187,#52188,#52189,#52190),(#52191,#52192,#52193,
#52194,#52195,#52196),(#52197,#52198,#52199,#52200,#52201,#52202),(#52203,
#52204,#52205,#52206,#52207,#52208),(#52209,#52210,#52211,#52212,#52213,
#52214)),.UNSPECIFIED.,.F.,.F.,.F.,(6,6),(6,6),(1.40817420416,1.45205022904),
(0.,1.),.UNSPECIFIED.);
#889=B_SPLINE_SURFACE_WITH_KNOTS('',5,5,((#52216,#52217,#52218,#52219,#52220,
#52221),(#52222,#52223,#52224,#52225,#52226,#52227),(#52228,#52229,#52230,
#52231,#52232,#52233),(#52234,#52235,#52236,#52237,#52238,#52239),(#52240,
#52241,#52242,#52243,#52244,#52245),(#52246,#52247,#52248,#52249,#52250,
#52251),(#52252,#52253,#52254,#52255,#52256,#52257),(#52258,#52259,#52260,
#52261,#52262,#52263),(#52264,#52265,#52266,#52267,#52268,#52269),(#52270,
#52271,#52272,#52273,#52274,#52275),(#52276,#52277,#52278,#52279,#52280,
#52281),(#52282,#52283,#52284,#52285,#52286,#52287)),.UNSPECIFIED.,.F.,
 .F.,.F.,(6,3,3,6),(6,6),(4.46364567829,9.98301756848,13.6615164274,17.5757040899),
(0.,1.),.UNSPECIFIED.);
#890=B_SPLINE_SURFACE_WITH_KNOTS('',5,5,((#52425,#52426,#52427,#52428,#52429,
#52430),(#52431,#52432,#52433,#52434,#52435,#52436),(#52437,#52438,#52439,
#52440,#52441,#52442),(#52443,#52444,#52445,#52446,#52447,#52448),(#52449,
#52450,#52451,#52452,#52453,#52454),(#52455,#52456,#52457,#52458,#52459,
#52460),(#52461,#52462,#52463,#52464,#52465,#52466),(#52467,#52468,#52469,
#52470,#52471,#52472),(#52473,#52474,#52475,#52476,#52477,#52478)),
 .UNSPECIFIED.,.F.,.F.,.F.,(6,3,6),(6,6),(1.01054285509,1.23011259501,1.32384910338),
(0.,1.),.UNSPECIFIED.);
#891=B_SPLINE_SURFACE_WITH_KNOTS('',5,5,((#52506,#52507,#52508,#52509,#52510,
#52511),(#52512,#52513,#52514,#52515,#52516,#52517),(#52518,#52519,#52520,
#52521,#52522,#52523),(#52524,#52525,#52526,#52527,#52528,#52529),(#52530,
#52531,#52532,#52533,#52534,#52535),(#52536,#52537,#52538,#52539,#52540,
#52541),(#52542,#52543,#52544,#52545,#52546,#52547),(#52548,#52549,#52550,
#52551,#52552,#52553),(#52554,#52555,#52556,#52557,#52558,#52559)),
 .UNSPECIFIED.,.F.,.F.,.F.,(6,3,6),(6,6),(2.57539738198,5.72432320356,8.12037630607),
(0.,1.),.UNSPECIFIED.);
#892=B_SPLINE_SURFACE_WITH_KNOTS('',5,5,((#52650,#52651,#52652,#52653,#52654,
#52655),(#52656,#52657,#52658,#52659,#52660,#52661),(#52662,#52663,#52664,
#52665,#52666,#52667),(#52668,#52669,#52670,#52671,#52672,#52673),(#52674,
#52675,#52676,#52677,#52678,#52679),(#52680,#52681,#52682,#52683,#52684,
#52685)),.UNSPECIFIED.,.F.,.F.,.F.,(6,6),(6,6),(0.993700418328028,1.22287270565897),
(-0.00157928356897239,1.00011077696173),.UNSPECIFIED.);
#893=B_SPLINE_SURFACE_WITH_KNOTS('',5,5,((#52690,#52691,#52692,#52693,#52694,
#52695),(#52696,#52697,#52698,#52699,#52700,#52701),(#52702,#52703,#52704,
#52705,#52706,#52707),(#52708,#52709,#52710,#52711,#52712,#52713),(#52714,
#52715,#52716,#52717,#52718,#52719),(#52720,#52721,#52722,#52723,#52724,
#52725)),.UNSPECIFIED.,.F.,.F.,.F.,(6,6),(6,6),(2.37851323355,2.46410111513),
(0.,1.),.UNSPECIFIED.);
#894=B_SPLINE_SURFACE_WITH_KNOTS('',5,5,((#52738,#52739,#52740,#52741,#52742,
#52743),(#52744,#52745,#52746,#52747,#52748,#52749),(#52750,#52751,#52752,
#52753,#52754,#52755),(#52756,#52757,#52758,#52759,#52760,#52761),(#52762,
#52763,#52764,#52765,#52766,#52767),(#52768,#52769,#52770,#52771,#52772,
#52773),(#52774,#52775,#52776,#52777,#52778,#52779),(#52780,#52781,#52782,
#52783,#52784,#52785),(#52786,#52787,#52788,#52789,#52790,#52791)),
 .UNSPECIFIED.,.F.,.F.,.F.,(6,3,6),(6,6),(0.586327318555,1.59285457075,
2.96825275179),(0.,1.),.UNSPECIFIED.);
#895=B_SPLINE_SURFACE_WITH_KNOTS('',5,5,((#52906,#52907,#52908,#52909,#52910,
#52911),(#52912,#52913,#52914,#52915,#52916,#52917),(#52918,#52919,#52920,
#52921,#52922,#52923),(#52924,#52925,#52926,#52927,#52928,#52929),(#52930,
#52931,#52932,#52933,#52934,#52935),(#52936,#52937,#52938,#52939,#52940,
#52941)),.UNSPECIFIED.,.F.,.F.,.F.,(6,6),(6,6),(0.881014033286,0.963434555076),
(0.,1.),.UNSPECIFIED.);
#896=B_SPLINE_SURFACE_WITH_KNOTS('',5,5,((#52951,#52952,#52953,#52954,#52955,
#52956),(#52957,#52958,#52959,#52960,#52961,#52962),(#52963,#52964,#52965,
#52966,#52967,#52968),(#52969,#52970,#52971,#52972,#52973,#52974),(#52975,
#52976,#52977,#52978,#52979,#52980),(#52981,#52982,#52983,#52984,#52985,
#52986),(#52987,#52988,#52989,#52990,#52991,#52992),(#52993,#52994,#52995,
#52996,#52997,#52998),(#52999,#53000,#53001,#53002,#53003,#53004)),
 .UNSPECIFIED.,.F.,.F.,.F.,(6,3,6),(6,6),(0.734432475987,1.16119681048,
1.33983380059),(0.,1.),.UNSPECIFIED.);
#897=B_SPLINE_SURFACE_WITH_KNOTS('',5,5,((#53026,#53027,#53028,#53029,#53030,
#53031),(#53032,#53033,#53034,#53035,#53036,#53037),(#53038,#53039,#53040,
#53041,#53042,#53043),(#53044,#53045,#53046,#53047,#53048,#53049),(#53050,
#53051,#53052,#53053,#53054,#53055),(#53056,#53057,#53058,#53059,#53060,
#53061),(#53062,#53063,#53064,#53065,#53066,#53067),(#53068,#53069,#53070,
#53071,#53072,#53073),(#53074,#53075,#53076,#53077,#53078,#53079),(#53080,
#53081,#53082,#53083,#53084,#53085),(#53086,#53087,#53088,#53089,#53090,
#53091),(#53092,#53093,#53094,#53095,#53096,#53097)),.UNSPECIFIED.,.F.,
 .F.,.F.,(6,3,3,6),(6,6),(1.14300114544,1.64244110169,2.30706085766,3.58561463726),
(0.,1.),.UNSPECIFIED.);
#898=B_SPLINE_SURFACE_WITH_KNOTS('',5,5,((#53200,#53201,#53202,#53203,#53204,
#53205),(#53206,#53207,#53208,#53209,#53210,#53211),(#53212,#53213,#53214,
#53215,#53216,#53217),(#53218,#53219,#53220,#53221,#53222,#53223),(#53224,
#53225,#53226,#53227,#53228,#53229),(#53230,#53231,#53232,#53233,#53234,
#53235)),.UNSPECIFIED.,.F.,.F.,.F.,(6,6),(6,6),(1.26425849888,1.32115953697),
(0.,1.),.UNSPECIFIED.);
#899=B_SPLINE_SURFACE_WITH_KNOTS('',5,1,((#53242,#53243),(#53244,#53245),
(#53246,#53247),(#53248,#53249),(#53250,#53251),(#53252,#53253)),
 .UNSPECIFIED.,.F.,.F.,.F.,(6,6),(2,2),(0.,0.898161272296),(0.,3.10437234689),
 .UNSPECIFIED.);
#900=B_SPLINE_SURFACE_WITH_KNOTS('',3,5,((#53286,#53287,#53288,#53289,#53290,
#53291),(#53292,#53293,#53294,#53295,#53296,#53297),(#53298,#53299,#53300,
#53301,#53302,#53303),(#53304,#53305,#53306,#53307,#53308,#53309)),
 .UNSPECIFIED.,.F.,.F.,.F.,(4,4),(6,6),(0.338318706236,0.636935495757),
(0.,1.),.UNSPECIFIED.);
#901=B_SPLINE_SURFACE_WITH_KNOTS('',5,1,((#53310,#53311),(#53312,#53313),
(#53314,#53315),(#53316,#53317),(#53318,#53319),(#53320,#53321),(#53322,
#53323),(#53324,#53325),(#53326,#53327)),.UNSPECIFIED.,.F.,.F.,.F.,(6,3,
6),(2,2),(0.,3.38335932988,6.7689179912),(-4.93438140460603E-6,3.10437234689),
 .UNSPECIFIED.);
#902=B_SPLINE_SURFACE_WITH_KNOTS('',5,5,((#53466,#53467,#53468,#53469,#53470,
#53471),(#53472,#53473,#53474,#53475,#53476,#53477),(#53478,#53479,#53480,
#53481,#53482,#53483),(#53484,#53485,#53486,#53487,#53488,#53489),(#53490,
#53491,#53492,#53493,#53494,#53495),(#53496,#53497,#53498,#53499,#53500,
#53501),(#53502,#53503,#53504,#53505,#53506,#53507),(#53508,#53509,#53510,
#53511,#53512,#53513),(#53514,#53515,#53516,#53517,#53518,#53519),(#53520,
#53521,#53522,#53523,#53524,#53525),(#53526,#53527,#53528,#53529,#53530,
#53531),(#53532,#53533,#53534,#53535,#53536,#53537)),.UNSPECIFIED.,.F.,
 .F.,.F.,(6,3,3,6),(6,6),(0.,2.20713855153,4.85810064575,8.61717037377),
(0.,1.),.UNSPECIFIED.);
#903=B_SPLINE_SURFACE_WITH_KNOTS('',5,5,((#53539,#53540,#53541,#53542,#53543,
#53544),(#53545,#53546,#53547,#53548,#53549,#53550),(#53551,#53552,#53553,
#53554,#53555,#53556),(#53557,#53558,#53559,#53560,#53561,#53562),(#53563,
#53564,#53565,#53566,#53567,#53568),(#53569,#53570,#53571,#53572,#53573,
#53574)),.UNSPECIFIED.,.F.,.F.,.F.,(6,6),(6,6),(2.946262962,2.98811189909),
(0.,1.),.UNSPECIFIED.);
#904=B_SPLINE_SURFACE_WITH_KNOTS('',5,5,((#53578,#53579,#53580,#53581,#53582,
#53583),(#53584,#53585,#53586,#53587,#53588,#53589),(#53590,#53591,#53592,
#53593,#53594,#53595),(#53596,#53597,#53598,#53599,#53600,#53601),(#53602,
#53603,#53604,#53605,#53606,#53607),(#53608,#53609,#53610,#53611,#53612,
#53613),(#53614,#53615,#53616,#53617,#53618,#53619),(#53620,#53621,#53622,
#53623,#53624,#53625),(#53626,#53627,#53628,#53629,#53630,#53631)),
 .UNSPECIFIED.,.F.,.F.,.F.,(6,3,6),(6,6),(0.160705691504905,0.296334742315,
0.49268070055009),(-0.00285589455108982,1.),.UNSPECIFIED.);
#905=B_SPLINE_SURFACE_WITH_KNOTS('',5,5,((#53652,#53653,#53654,#53655,#53656,
#53657),(#53658,#53659,#53660,#53661,#53662,#53663),(#53664,#53665,#53666,
#53667,#53668,#53669),(#53670,#53671,#53672,#53673,#53674,#53675),(#53676,
#53677,#53678,#53679,#53680,#53681),(#53682,#53683,#53684,#53685,#53686,
#53687)),.UNSPECIFIED.,.F.,.F.,.F.,(6,6),(6,6),(1.51692742518,1.55221398826),
(0.,1.),.UNSPECIFIED.);
#906=B_SPLINE_SURFACE_WITH_KNOTS('',5,5,((#53688,#53689,#53690,#53691,#53692,
#53693),(#53694,#53695,#53696,#53697,#53698,#53699),(#53700,#53701,#53702,
#53703,#53704,#53705),(#53706,#53707,#53708,#53709,#53710,#53711),(#53712,
#53713,#53714,#53715,#53716,#53717),(#53718,#53719,#53720,#53721,#53722,
#53723)),.UNSPECIFIED.,.F.,.F.,.F.,(6,6),(6,6),(1.28339894164,1.34350433703),
(0.,1.),.UNSPECIFIED.);
#907=B_SPLINE_SURFACE_WITH_KNOTS('',5,5,((#53738,#53739,#53740,#53741,#53742,
#53743),(#53744,#53745,#53746,#53747,#53748,#53749),(#53750,#53751,#53752,
#53753,#53754,#53755),(#53756,#53757,#53758,#53759,#53760,#53761),(#53762,
#53763,#53764,#53765,#53766,#53767),(#53768,#53769,#53770,#53771,#53772,
#53773),(#53774,#53775,#53776,#53777,#53778,#53779),(#53780,#53781,#53782,
#53783,#53784,#53785),(#53786,#53787,#53788,#53789,#53790,#53791)),
 .UNSPECIFIED.,.F.,.F.,.F.,(6,3,6),(6,6),(0.225815728085,0.523709124902,
0.747252061964),(0.,1.),.UNSPECIFIED.);
#908=B_SPLINE_SURFACE_WITH_KNOTS('',5,5,((#53802,#53803,#53804,#53805,#53806,
#53807),(#53808,#53809,#53810,#53811,#53812,#53813),(#53814,#53815,#53816,
#53817,#53818,#53819),(#53820,#53821,#53822,#53823,#53824,#53825),(#53826,
#53827,#53828,#53829,#53830,#53831),(#53832,#53833,#53834,#53835,#53836,
#53837)),.UNSPECIFIED.,.F.,.F.,.F.,(6,6),(6,6),(0.840058180513,4.79280767082),
(0.,1.),.UNSPECIFIED.);
#909=B_SPLINE_SURFACE_WITH_KNOTS('',5,5,((#53846,#53847,#53848,#53849,#53850,
#53851),(#53852,#53853,#53854,#53855,#53856,#53857),(#53858,#53859,#53860,
#53861,#53862,#53863),(#53864,#53865,#53866,#53867,#53868,#53869),(#53870,
#53871,#53872,#53873,#53874,#53875),(#53876,#53877,#53878,#53879,#53880,
#53881)),.UNSPECIFIED.,.F.,.F.,.F.,(6,6),(6,6),(1.51692742518,1.55221398826),
(0.,1.),.UNSPECIFIED.);
#910=B_SPLINE_SURFACE_WITH_KNOTS('',5,5,((#53886,#53887,#53888,#53889,#53890,
#53891),(#53892,#53893,#53894,#53895,#53896,#53897),(#53898,#53899,#53900,
#53901,#53902,#53903),(#53904,#53905,#53906,#53907,#53908,#53909),(#53910,
#53911,#53912,#53913,#53914,#53915),(#53916,#53917,#53918,#53919,#53920,
#53921),(#53922,#53923,#53924,#53925,#53926,#53927),(#53928,#53929,#53930,
#53931,#53932,#53933),(#53934,#53935,#53936,#53937,#53938,#53939)),
 .UNSPECIFIED.,.F.,.F.,.F.,(6,3,6),(6,6),(0.163561586047,0.296334742315,
0.489824805999),(0.,1.),.UNSPECIFIED.);
#911=B_SPLINE_SURFACE_WITH_KNOTS('',5,5,((#53941,#53942,#53943,#53944,#53945,
#53946),(#53947,#53948,#53949,#53950,#53951,#53952),(#53953,#53954,#53955,
#53956,#53957,#53958),(#53959,#53960,#53961,#53962,#53963,#53964),(#53965,
#53966,#53967,#53968,#53969,#53970),(#53971,#53972,#53973,#53974,#53975,
#53976)),.UNSPECIFIED.,.F.,.F.,.F.,(6,6),(6,6),(2.946262962,2.98811189909),
(0.,1.),.UNSPECIFIED.);
#912=B_SPLINE_SURFACE_WITH_KNOTS('',5,5,((#53978,#53979,#53980,#53981,#53982,
#53983),(#53984,#53985,#53986,#53987,#53988,#53989),(#53990,#53991,#53992,
#53993,#53994,#53995),(#53996,#53997,#53998,#53999,#54000,#54001),(#54002,
#54003,#54004,#54005,#54006,#54007),(#54008,#54009,#54010,#54011,#54012,
#54013),(#54014,#54015,#54016,#54017,#54018,#54019),(#54020,#54021,#54022,
#54023,#54024,#54025),(#54026,#54027,#54028,#54029,#54030,#54031),(#54032,
#54033,#54034,#54035,#54036,#54037),(#54038,#54039,#54040,#54041,#54042,
#54043),(#54044,#54045,#54046,#54047,#54048,#54049)),.UNSPECIFIED.,.F.,
 .F.,.F.,(6,3,3,6),(6,6),(0.,2.20713855153,4.85810064575,8.61717037377),
(0.,1.),.UNSPECIFIED.);
#913=B_SPLINE_SURFACE_WITH_KNOTS('',5,1,((#54062,#54063),(#54064,#54065),
(#54066,#54067),(#54068,#54069),(#54070,#54071),(#54072,#54073),(#54074,
#54075),(#54076,#54077),(#54078,#54079)),.UNSPECIFIED.,.F.,.F.,.F.,(6,3,
6),(2,2),(0.,3.38335932988,6.7689179912),(-1.30243697672538E-5,3.10437234689),
 .UNSPECIFIED.);
#914=B_SPLINE_SURFACE_WITH_KNOTS('',5,1,((#54088,#54089),(#54090,#54091),
(#54092,#54093),(#54094,#54095),(#54096,#54097),(#54098,#54099)),
 .UNSPECIFIED.,.F.,.F.,.F.,(6,6),(2,2),(0.,0.898161272296),(0.,3.10437234689),
 .UNSPECIFIED.);
#915=B_SPLINE_SURFACE_WITH_KNOTS('',3,5,((#54135,#54136,#54137,#54138,#54139,
#54140),(#54141,#54142,#54143,#54144,#54145,#54146),(#54147,#54148,#54149,
#54150,#54151,#54152),(#54153,#54154,#54155,#54156,#54157,#54158)),
 .UNSPECIFIED.,.F.,.F.,.F.,(4,4),(6,6),(0.338318706236,0.636935495757),
(0.,1.),.UNSPECIFIED.);
#916=B_SPLINE_SURFACE_WITH_KNOTS('',5,5,((#54160,#54161,#54162,#54163,#54164,
#54165),(#54166,#54167,#54168,#54169,#54170,#54171),(#54172,#54173,#54174,
#54175,#54176,#54177),(#54178,#54179,#54180,#54181,#54182,#54183),(#54184,
#54185,#54186,#54187,#54188,#54189),(#54190,#54191,#54192,#54193,#54194,
#54195)),.UNSPECIFIED.,.F.,.F.,.F.,(6,6),(6,6),(1.26425849888,1.32115953697),
(0.,1.),.UNSPECIFIED.);
#917=B_SPLINE_SURFACE_WITH_KNOTS('',5,5,((#54197,#54198,#54199,#54200,#54201,
#54202),(#54203,#54204,#54205,#54206,#54207,#54208),(#54209,#54210,#54211,
#54212,#54213,#54214),(#54215,#54216,#54217,#54218,#54219,#54220),(#54221,
#54222,#54223,#54224,#54225,#54226),(#54227,#54228,#54229,#54230,#54231,
#54232),(#54233,#54234,#54235,#54236,#54237,#54238),(#54239,#54240,#54241,
#54242,#54243,#54244),(#54245,#54246,#54247,#54248,#54249,#54250),(#54251,
#54252,#54253,#54254,#54255,#54256),(#54257,#54258,#54259,#54260,#54261,
#54262),(#54263,#54264,#54265,#54266,#54267,#54268)),.UNSPECIFIED.,.F.,
 .F.,.F.,(6,3,3,6),(6,6),(1.14300114544,1.64244110169,2.30706085766,3.58561463726),
(0.,1.),.UNSPECIFIED.);
#918=B_SPLINE_SURFACE_WITH_KNOTS('',5,5,((#54270,#54271,#54272,#54273,#54274,
#54275),(#54276,#54277,#54278,#54279,#54280,#54281),(#54282,#54283,#54284,
#54285,#54286,#54287),(#54288,#54289,#54290,#54291,#54292,#54293),(#54294,
#54295,#54296,#54297,#54298,#54299),(#54300,#54301,#54302,#54303,#54304,
#54305),(#54306,#54307,#54308,#54309,#54310,#54311),(#54312,#54313,#54314,
#54315,#54316,#54317),(#54318,#54319,#54320,#54321,#54322,#54323)),
 .UNSPECIFIED.,.F.,.F.,.F.,(6,3,6),(6,6),(0.734432475987,1.16119681048,
1.33983380059),(0.,1.),.UNSPECIFIED.);
#919=B_SPLINE_SURFACE_WITH_KNOTS('',5,5,((#54325,#54326,#54327,#54328,#54329,
#54330),(#54331,#54332,#54333,#54334,#54335,#54336),(#54337,#54338,#54339,
#54340,#54341,#54342),(#54343,#54344,#54345,#54346,#54347,#54348),(#54349,
#54350,#54351,#54352,#54353,#54354),(#54355,#54356,#54357,#54358,#54359,
#54360)),.UNSPECIFIED.,.F.,.F.,.F.,(6,6),(6,6),(0.881014033286,0.963434555076),
(0.,1.),.UNSPECIFIED.);
#920=B_SPLINE_SURFACE_WITH_KNOTS('',5,5,((#54362,#54363,#54364,#54365,#54366,
#54367),(#54368,#54369,#54370,#54371,#54372,#54373),(#54374,#54375,#54376,
#54377,#54378,#54379),(#54380,#54381,#54382,#54383,#54384,#54385),(#54386,
#54387,#54388,#54389,#54390,#54391),(#54392,#54393,#54394,#54395,#54396,
#54397),(#54398,#54399,#54400,#54401,#54402,#54403),(#54404,#54405,#54406,
#54407,#54408,#54409),(#54410,#54411,#54412,#54413,#54414,#54415)),
 .UNSPECIFIED.,.F.,.F.,.F.,(6,3,6),(6,6),(0.586327318555,1.59285457075,
2.96825275179),(0.,1.),.UNSPECIFIED.);
#921=B_SPLINE_SURFACE_WITH_KNOTS('',5,5,((#54417,#54418,#54419,#54420,#54421,
#54422),(#54423,#54424,#54425,#54426,#54427,#54428),(#54429,#54430,#54431,
#54432,#54433,#54434),(#54435,#54436,#54437,#54438,#54439,#54440),(#54441,
#54442,#54443,#54444,#54445,#54446),(#54447,#54448,#54449,#54450,#54451,
#54452)),.UNSPECIFIED.,.F.,.F.,.F.,(6,6),(6,6),(2.37851323355,2.46410111513),
(0.,1.),.UNSPECIFIED.);
#922=B_SPLINE_SURFACE_WITH_KNOTS('',5,5,((#54454,#54455,#54456,#54457,#54458,
#54459),(#54460,#54461,#54462,#54463,#54464,#54465),(#54466,#54467,#54468,
#54469,#54470,#54471),(#54472,#54473,#54474,#54475,#54476,#54477),(#54478,
#54479,#54480,#54481,#54482,#54483),(#54484,#54485,#54486,#54487,#54488,
#54489),(#54490,#54491,#54492,#54493,#54494,#54495),(#54496,#54497,#54498,
#54499,#54500,#54501),(#54502,#54503,#54504,#54505,#54506,#54507)),
 .UNSPECIFIED.,.F.,.F.,.F.,(6,3,6),(6,6),(2.57539738198,5.72432320356,8.12037630607),
(0.,1.),.UNSPECIFIED.);
#923=B_SPLINE_SURFACE_WITH_KNOTS('',5,5,((#54509,#54510,#54511,#54512,#54513,
#54514),(#54515,#54516,#54517,#54518,#54519,#54520),(#54521,#54522,#54523,
#54524,#54525,#54526),(#54527,#54528,#54529,#54530,#54531,#54532),(#54533,
#54534,#54535,#54536,#54537,#54538),(#54539,#54540,#54541,#54542,#54543,
#54544),(#54545,#54546,#54547,#54548,#54549,#54550),(#54551,#54552,#54553,
#54554,#54555,#54556),(#54557,#54558,#54559,#54560,#54561,#54562)),
 .UNSPECIFIED.,.F.,.F.,.F.,(6,3,6),(6,6),(1.01054285509,1.23011259501,1.32384910338),
(0.,1.),.UNSPECIFIED.);
#924=B_SPLINE_SURFACE_WITH_KNOTS('',5,5,((#54564,#54565,#54566,#54567,#54568,
#54569),(#54570,#54571,#54572,#54573,#54574,#54575),(#54576,#54577,#54578,
#54579,#54580,#54581),(#54582,#54583,#54584,#54585,#54586,#54587),(#54588,
#54589,#54590,#54591,#54592,#54593),(#54594,#54595,#54596,#54597,#54598,
#54599),(#54600,#54601,#54602,#54603,#54604,#54605),(#54606,#54607,#54608,
#54609,#54610,#54611),(#54612,#54613,#54614,#54615,#54616,#54617),(#54618,
#54619,#54620,#54621,#54622,#54623),(#54624,#54625,#54626,#54627,#54628,
#54629),(#54630,#54631,#54632,#54633,#54634,#54635)),.UNSPECIFIED.,.F.,
 .F.,.F.,(6,3,3,6),(6,6),(4.46364567829,9.98301756848,13.6615164274,17.5757040899),
(0.,1.),.UNSPECIFIED.);
#925=B_SPLINE_SURFACE_WITH_KNOTS('',5,5,((#54637,#54638,#54639,#54640,#54641,
#54642),(#54643,#54644,#54645,#54646,#54647,#54648),(#54649,#54650,#54651,
#54652,#54653,#54654),(#54655,#54656,#54657,#54658,#54659,#54660),(#54661,
#54662,#54663,#54664,#54665,#54666),(#54667,#54668,#54669,#54670,#54671,
#54672)),.UNSPECIFIED.,.F.,.F.,.F.,(6,6),(6,6),(0.994217933968,1.222355190019),
(-0.00106176792899955,1.00011077696173),.UNSPECIFIED.);
#926=B_SPLINE_SURFACE_WITH_KNOTS('',5,5,((#54674,#54675,#54676,#54677,#54678,
#54679),(#54680,#54681,#54682,#54683,#54684,#54685),(#54686,#54687,#54688,
#54689,#54690,#54691),(#54692,#54693,#54694,#54695,#54696,#54697),(#54698,
#54699,#54700,#54701,#54702,#54703),(#54704,#54705,#54706,#54707,#54708,
#54709)),.UNSPECIFIED.,.F.,.F.,.F.,(6,6),(6,6),(1.40817420416,1.45205022904),
(0.,1.),.UNSPECIFIED.);
#927=B_SPLINE_SURFACE_WITH_KNOTS('',5,5,((#54712,#54713,#54714,#54715,#54716,
#54717),(#54718,#54719,#54720,#54721,#54722,#54723),(#54724,#54725,#54726,
#54727,#54728,#54729),(#54730,#54731,#54732,#54733,#54734,#54735),(#54736,
#54737,#54738,#54739,#54740,#54741),(#54742,#54743,#54744,#54745,#54746,
#54747),(#54748,#54749,#54750,#54751,#54752,#54753),(#54754,#54755,#54756,
#54757,#54758,#54759),(#54760,#54761,#54762,#54763,#54764,#54765)),
 .UNSPECIFIED.,.F.,.F.,.F.,(6,3,6),(6,6),(0.342430056326,0.787545489389,
1.14838178471),(0.,1.),.UNSPECIFIED.);
#928=B_SPLINE_SURFACE_WITH_KNOTS('',5,5,((#54767,#54768,#54769,#54770,#54771,
#54772),(#54773,#54774,#54775,#54776,#54777,#54778),(#54779,#54780,#54781,
#54782,#54783,#54784),(#54785,#54786,#54787,#54788,#54789,#54790),(#54791,
#54792,#54793,#54794,#54795,#54796),(#54797,#54798,#54799,#54800,#54801,
#54802)),.UNSPECIFIED.,.F.,.F.,.F.,(6,6),(6,6),(1.036743613,1.10280574369),
(0.,1.),.UNSPECIFIED.);
#929=B_SPLINE_SURFACE_WITH_KNOTS('',5,1,((#55071,#55072),(#55073,#55074),
(#55075,#55076),(#55077,#55078),(#55079,#55080),(#55081,#55082)),
 .UNSPECIFIED.,.F.,.F.,.F.,(6,6),(2,2),(0.,3.0373684949),(0.,3.10437234689),
 .UNSPECIFIED.);
#930=B_SPLINE_SURFACE_WITH_KNOTS('',5,1,((#55109,#55110),(#55111,#55112),
(#55113,#55114),(#55115,#55116),(#55117,#55118),(#55119,#55120)),
 .UNSPECIFIED.,.F.,.F.,.F.,(6,6),(2,2),(0.,0.392615054569),(0.,3.10437234689),
 .UNSPECIFIED.);
#931=B_SPLINE_SURFACE_WITH_KNOTS('',5,1,((#55137,#55138),(#55139,#55140),
(#55141,#55142),(#55143,#55144),(#55145,#55146),(#55147,#55148)),
 .UNSPECIFIED.,.F.,.F.,.F.,(6,6),(2,2),(0.,0.226010362356),(0.,3.10437234689),
 .UNSPECIFIED.);
#932=B_SPLINE_SURFACE_WITH_KNOTS('',5,1,((#55159,#55160),(#55161,#55162),
(#55163,#55164),(#55165,#55166),(#55167,#55168),(#55169,#55170)),
 .UNSPECIFIED.,.F.,.F.,.F.,(6,6),(2,2),(0.,0.600083611309),(0.,3.10437234689),
 .UNSPECIFIED.);
#933=B_SPLINE_SURFACE_WITH_KNOTS('',5,1,((#55181,#55182),(#55183,#55184),
(#55185,#55186),(#55187,#55188),(#55189,#55190),(#55191,#55192),(#55193,
#55194),(#55195,#55196),(#55197,#55198),(#55199,#55200),(#55201,#55202),
(#55203,#55204)),.UNSPECIFIED.,.F.,.F.,.F.,(6,3,3,6),(2,2),(0.,2.83532528452,
6.09533201542,9.83397913335),(0.,3.10437234689),.UNSPECIFIED.);
#934=B_SPLINE_SURFACE_WITH_KNOTS('',5,1,((#55271,#55272),(#55273,#55274),
(#55275,#55276),(#55277,#55278),(#55279,#55280),(#55281,#55282)),
 .UNSPECIFIED.,.F.,.F.,.F.,(6,6),(2,2),(0.,0.224378834114),(0.,3.10437234689),
 .UNSPECIFIED.);
#935=B_SPLINE_SURFACE_WITH_KNOTS('',5,1,((#55291,#55292),(#55293,#55294),
(#55295,#55296),(#55297,#55298),(#55299,#55300),(#55301,#55302),(#55303,
#55304),(#55305,#55306),(#55307,#55308)),.UNSPECIFIED.,.F.,.F.,.F.,(6,3,
6),(2,2),(0.,2.10936312981,4.22279623369),(0.,3.10437234689),
 .UNSPECIFIED.);
#936=B_SPLINE_SURFACE_WITH_KNOTS('',5,1,((#55351,#55352),(#55353,#55354),
(#55355,#55356),(#55357,#55358),(#55359,#55360),(#55361,#55362)),
 .UNSPECIFIED.,.F.,.F.,.F.,(6,6),(2,2),(0.,1.84821844080963),(0.,3.10437234689),
 .UNSPECIFIED.);
#937=B_SPLINE_SURFACE_WITH_KNOTS('',5,1,((#55396,#55397),(#55398,#55399),
(#55400,#55401),(#55402,#55403),(#55404,#55405),(#55406,#55407)),
 .UNSPECIFIED.,.F.,.F.,.F.,(6,6),(2,2),(0.,0.482067685837),(0.,3.10437234689),
 .UNSPECIFIED.);
#938=B_SPLINE_SURFACE_WITH_KNOTS('',5,1,((#55411,#55412),(#55413,#55414),
(#55415,#55416),(#55417,#55418),(#55419,#55420),(#55421,#55422),(#55423,
#55424),(#55425,#55426),(#55427,#55428),(#55429,#55430),(#55431,#55432),
(#55433,#55434)),.UNSPECIFIED.,.F.,.F.,.F.,(6,3,3,6),(2,2),(0.,0.629547398659,
1.2493532974,1.86132516749),(0.,3.10437234689),.UNSPECIFIED.);
#939=B_SPLINE_SURFACE_WITH_KNOTS('',5,1,((#55504,#55505),(#55506,#55507),
(#55508,#55509),(#55510,#55511),(#55512,#55513),(#55514,#55515)),
 .UNSPECIFIED.,.F.,.F.,.F.,(6,6),(2,2),(0.,0.2489231439),(0.,3.10437234689),
 .UNSPECIFIED.);
#940=B_SPLINE_SURFACE_WITH_KNOTS('',5,1,((#55517,#55518),(#55519,#55520),
(#55521,#55522),(#55523,#55524),(#55525,#55526),(#55527,#55528)),
 .UNSPECIFIED.,.F.,.F.,.F.,(6,6),(2,2),(0.,3.0373684949),(0.,3.10437234689),
 .UNSPECIFIED.);
#941=B_SPLINE_SURFACE_WITH_KNOTS('',5,1,((#55553,#55554),(#55555,#55556),
(#55557,#55558),(#55559,#55560),(#55561,#55562),(#55563,#55564)),
 .UNSPECIFIED.,.F.,.F.,.F.,(6,6),(2,2),(0.,0.392615054569),(0.,3.10437234689),
 .UNSPECIFIED.);
#942=B_SPLINE_SURFACE_WITH_KNOTS('',5,5,((#55575,#55576,#55577,#55578,#55579,
#55580),(#55581,#55582,#55583,#55584,#55585,#55586),(#55587,#55588,#55589,
#55590,#55591,#55592),(#55593,#55594,#55595,#55596,#55597,#55598),(#55599,
#55600,#55601,#55602,#55603,#55604),(#55605,#55606,#55607,#55608,#55609,
#55610),(#55611,#55612,#55613,#55614,#55615,#55616),(#55617,#55618,#55619,
#55620,#55621,#55622),(#55623,#55624,#55625,#55626,#55627,#55628)),
 .UNSPECIFIED.,.F.,.F.,.F.,(6,3,6),(6,6),(8.63627991204,12.3201261581,17.1386583361),
(0.,0.3),.UNSPECIFIED.);
#943=B_SPLINE_SURFACE_WITH_KNOTS('',5,5,((#55795,#55796,#55797,#55798,#55799,
#55800),(#55801,#55802,#55803,#55804,#55805,#55806),(#55807,#55808,#55809,
#55810,#55811,#55812),(#55813,#55814,#55815,#55816,#55817,#55818),(#55819,
#55820,#55821,#55822,#55823,#55824),(#55825,#55826,#55827,#55828,#55829,
#55830),(#55831,#55832,#55833,#55834,#55835,#55836),(#55837,#55838,#55839,
#55840,#55841,#55842),(#55843,#55844,#55845,#55846,#55847,#55848)),
 .UNSPECIFIED.,.F.,.F.,.F.,(6,3,6),(6,6),(1.56090158029,2.52299916049,2.93530749734),
(0.,0.3),.UNSPECIFIED.);
#944=B_SPLINE_SURFACE_WITH_KNOTS('',5,5,((#55877,#55878,#55879,#55880,#55881,
#55882),(#55883,#55884,#55885,#55886,#55887,#55888),(#55889,#55890,#55891,
#55892,#55893,#55894),(#55895,#55896,#55897,#55898,#55899,#55900),(#55901,
#55902,#55903,#55904,#55905,#55906),(#55907,#55908,#55909,#55910,#55911,
#55912),(#55913,#55914,#55915,#55916,#55917,#55918),(#55919,#55920,#55921,
#55922,#55923,#55924),(#55925,#55926,#55927,#55928,#55929,#55930)),
 .UNSPECIFIED.,.F.,.F.,.F.,(6,3,6),(6,6),(3.22008961045,5.63866638969,8.97249770267),
(0.,0.3),.UNSPECIFIED.);
#945=B_SPLINE_SURFACE_WITH_KNOTS('',5,5,((#55998,#55999,#56000,#56001,#56002,
#56003),(#56004,#56005,#56006,#56007,#56008,#56009),(#56010,#56011,#56012,
#56013,#56014,#56015),(#56016,#56017,#56018,#56019,#56020,#56021),(#56022,
#56023,#56024,#56025,#56026,#56027),(#56028,#56029,#56030,#56031,#56032,
#56033),(#56034,#56035,#56036,#56037,#56038,#56039),(#56040,#56041,#56042,
#56043,#56044,#56045),(#56046,#56047,#56048,#56049,#56050,#56051)),
 .UNSPECIFIED.,.F.,.F.,.F.,(6,3,6),(6,6),(1.72939840805139,1.80499037738,
1.87215083229958),(-2.7802799580615E-5,0.3),.UNSPECIFIED.);
#946=B_SPLINE_SURFACE_WITH_KNOTS('',5,5,((#56388,#56389,#56390,#56391,#56392,
#56393),(#56394,#56395,#56396,#56397,#56398,#56399),(#56400,#56401,#56402,
#56403,#56404,#56405),(#56406,#56407,#56408,#56409,#56410,#56411),(#56412,
#56413,#56414,#56415,#56416,#56417),(#56418,#56419,#56420,#56421,#56422,
#56423)),.UNSPECIFIED.,.F.,.F.,.F.,(6,6),(6,6),(1.03921348145,1.16363378049),
(0.,0.3),.UNSPECIFIED.);
#947=B_SPLINE_SURFACE_WITH_KNOTS('',5,5,((#56432,#56433,#56434,#56435,#56436,
#56437),(#56438,#56439,#56440,#56441,#56442,#56443),(#56444,#56445,#56446,
#56447,#56448,#56449),(#56450,#56451,#56452,#56453,#56454,#56455),(#56456,
#56457,#56458,#56459,#56460,#56461),(#56462,#56463,#56464,#56465,#56466,
#56467)),.UNSPECIFIED.,.F.,.F.,.F.,(6,6),(6,6),(0.594536305137334,3.46674155179467),
(-0.000626841014666089,0.3),.UNSPECIFIED.);
#948=B_SPLINE_SURFACE_WITH_KNOTS('',5,5,((#56486,#56487,#56488,#56489,#56490,
#56491),(#56492,#56493,#56494,#56495,#56496,#56497),(#56498,#56499,#56500,
#56501,#56502,#56503),(#56504,#56505,#56506,#56507,#56508,#56509),(#56510,
#56511,#56512,#56513,#56514,#56515),(#56516,#56517,#56518,#56519,#56520,
#56521)),.UNSPECIFIED.,.F.,.F.,.F.,(6,6),(6,6),(3.1034218264,3.1199806069),
(0.,0.3),.UNSPECIFIED.);
#949=B_SPLINE_SURFACE_WITH_KNOTS('',5,5,((#56525,#56526,#56527,#56528,#56529,
#56530),(#56531,#56532,#56533,#56534,#56535,#56536),(#56537,#56538,#56539,
#56540,#56541,#56542),(#56543,#56544,#56545,#56546,#56547,#56548),(#56549,
#56550,#56551,#56552,#56553,#56554),(#56555,#56556,#56557,#56558,#56559,
#56560),(#56561,#56562,#56563,#56564,#56565,#56566),(#56567,#56568,#56569,
#56570,#56571,#56572),(#56573,#56574,#56575,#56576,#56577,#56578)),
 .UNSPECIFIED.,.F.,.F.,.F.,(6,3,6),(6,6),(0.0737511682725,0.240560274088,
0.36600685554),(0.,0.3),.UNSPECIFIED.);
#950=B_SPLINE_SURFACE_WITH_KNOTS('',4,5,((#56590,#56591,#56592,#56593,#56594,
#56595),(#56596,#56597,#56598,#56599,#56600,#56601),(#56602,#56603,#56604,
#56605,#56606,#56607),(#56608,#56609,#56610,#56611,#56612,#56613),(#56614,
#56615,#56616,#56617,#56618,#56619)),.UNSPECIFIED.,.F.,.F.,.F.,(5,5),(6,
6),(1.03670984253,1.04687754685),(0.,0.3),.UNSPECIFIED.);
#951=B_SPLINE_SURFACE_WITH_KNOTS('',5,5,((#56626,#56627,#56628,#56629,#56630,
#56631),(#56632,#56633,#56634,#56635,#56636,#56637),(#56638,#56639,#56640,
#56641,#56642,#56643),(#56644,#56645,#56646,#56647,#56648,#56649),(#56650,
#56651,#56652,#56653,#56654,#56655),(#56656,#56657,#56658,#56659,#56660,
#56661),(#56662,#56663,#56664,#56665,#56666,#56667),(#56668,#56669,#56670,
#56671,#56672,#56673),(#56674,#56675,#56676,#56677,#56678,#56679)),
 .UNSPECIFIED.,.F.,.F.,.F.,(6,3,6),(6,6),(1.01756015018,3.02586880249,6.44209971341),
(0.,0.3),.UNSPECIFIED.);
#952=B_SPLINE_SURFACE_WITH_KNOTS('',5,5,((#56691,#56692,#56693,#56694,#56695,
#56696),(#56697,#56698,#56699,#56700,#56701,#56702),(#56703,#56704,#56705,
#56706,#56707,#56708),(#56709,#56710,#56711,#56712,#56713,#56714),(#56715,
#56716,#56717,#56718,#56719,#56720),(#56721,#56722,#56723,#56724,#56725,
#56726),(#56727,#56728,#56729,#56730,#56731,#56732),(#56733,#56734,#56735,
#56736,#56737,#56738),(#56739,#56740,#56741,#56742,#56743,#56744)),
 .UNSPECIFIED.,.F.,.F.,.F.,(6,3,6),(6,6),(1.01756015018,3.02586880249,6.44209971341),
(0.,0.3),.UNSPECIFIED.);
#953=B_SPLINE_SURFACE_WITH_KNOTS('',4,5,((#56844,#56845,#56846,#56847,#56848,
#56849),(#56850,#56851,#56852,#56853,#56854,#56855),(#56856,#56857,#56858,
#56859,#56860,#56861),(#56862,#56863,#56864,#56865,#56866,#56867),(#56868,
#56869,#56870,#56871,#56872,#56873)),.UNSPECIFIED.,.F.,.F.,.F.,(5,5),(6,
6),(1.03670984253,1.04687754685),(0.,0.3),.UNSPECIFIED.);
#954=B_SPLINE_SURFACE_WITH_KNOTS('',5,5,((#56880,#56881,#56882,#56883,#56884,
#56885),(#56886,#56887,#56888,#56889,#56890,#56891),(#56892,#56893,#56894,
#56895,#56896,#56897),(#56898,#56899,#56900,#56901,#56902,#56903),(#56904,
#56905,#56906,#56907,#56908,#56909),(#56910,#56911,#56912,#56913,#56914,
#56915),(#56916,#56917,#56918,#56919,#56920,#56921),(#56922,#56923,#56924,
#56925,#56926,#56927),(#56928,#56929,#56930,#56931,#56932,#56933)),
 .UNSPECIFIED.,.F.,.F.,.F.,(6,3,6),(6,6),(0.0737511682725,0.240560274088,
0.36600685554),(0.,0.3),.UNSPECIFIED.);
#955=B_SPLINE_SURFACE_WITH_KNOTS('',5,5,((#56958,#56959,#56960,#56961,#56962,
#56963),(#56964,#56965,#56966,#56967,#56968,#56969),(#56970,#56971,#56972,
#56973,#56974,#56975),(#56976,#56977,#56978,#56979,#56980,#56981),(#56982,
#56983,#56984,#56985,#56986,#56987),(#56988,#56989,#56990,#56991,#56992,
#56993)),.UNSPECIFIED.,.F.,.F.,.F.,(6,6),(6,6),(3.1034218264,3.1199806069),
(0.,0.3),.UNSPECIFIED.);
#956=B_SPLINE_SURFACE_WITH_KNOTS('',5,5,((#56997,#56998,#56999,#57000,#57001,
#57002),(#57003,#57004,#57005,#57006,#57007,#57008),(#57009,#57010,#57011,
#57012,#57013,#57014),(#57015,#57016,#57017,#57018,#57019,#57020),(#57021,
#57022,#57023,#57024,#57025,#57026),(#57027,#57028,#57029,#57030,#57031,
#57032)),.UNSPECIFIED.,.F.,.F.,.F.,(6,6),(6,6),(0.594419717825406,3.46685813910659),
(-0.000743428326593711,0.3),.UNSPECIFIED.);
#957=B_SPLINE_SURFACE_WITH_KNOTS('',5,5,((#57039,#57040,#57041,#57042,#57043,
#57044),(#57045,#57046,#57047,#57048,#57049,#57050),(#57051,#57052,#57053,
#57054,#57055,#57056),(#57057,#57058,#57059,#57060,#57061,#57062),(#57063,
#57064,#57065,#57066,#57067,#57068),(#57069,#57070,#57071,#57072,#57073,
#57074)),.UNSPECIFIED.,.F.,.F.,.F.,(6,6),(6,6),(1.03921348145,1.16363378049),
(0.,0.3),.UNSPECIFIED.);
#958=B_SPLINE_SURFACE_WITH_KNOTS('',5,5,((#57092,#57093,#57094,#57095,#57096,
#57097),(#57098,#57099,#57100,#57101,#57102,#57103),(#57104,#57105,#57106,
#57107,#57108,#57109),(#57110,#57111,#57112,#57113,#57114,#57115),(#57116,
#57117,#57118,#57119,#57120,#57121),(#57122,#57123,#57124,#57125,#57126,
#57127),(#57128,#57129,#57130,#57131,#57132,#57133),(#57134,#57135,#57136,
#57137,#57138,#57139),(#57140,#57141,#57142,#57143,#57144,#57145)),
 .UNSPECIFIED.,.F.,.F.,.F.,(6,3,6),(6,6),(1.72942608575,1.80499037738,1.8721230295),
(0.,0.3),.UNSPECIFIED.);
#959=B_SPLINE_SURFACE_WITH_KNOTS('',5,5,((#57164,#57165,#57166,#57167,#57168,
#57169),(#57170,#57171,#57172,#57173,#57174,#57175),(#57176,#57177,#57178,
#57179,#57180,#57181),(#57182,#57183,#57184,#57185,#57186,#57187),(#57188,
#57189,#57190,#57191,#57192,#57193),(#57194,#57195,#57196,#57197,#57198,
#57199),(#57200,#57201,#57202,#57203,#57204,#57205),(#57206,#57207,#57208,
#57209,#57210,#57211),(#57212,#57213,#57214,#57215,#57216,#57217)),
 .UNSPECIFIED.,.F.,.F.,.F.,(6,3,6),(6,6),(3.22008961045,5.63866638969,8.97249770267),
(0.,0.3),.UNSPECIFIED.);
#960=B_SPLINE_SURFACE_WITH_KNOTS('',5,5,((#57269,#57270,#57271,#57272,#57273,
#57274),(#57275,#57276,#57277,#57278,#57279,#57280),(#57281,#57282,#57283,
#57284,#57285,#57286),(#57287,#57288,#57289,#57290,#57291,#57292),(#57293,
#57294,#57295,#57296,#57297,#57298),(#57299,#57300,#57301,#57302,#57303,
#57304),(#57305,#57306,#57307,#57308,#57309,#57310),(#57311,#57312,#57313,
#57314,#57315,#57316),(#57317,#57318,#57319,#57320,#57321,#57322)),
 .UNSPECIFIED.,.F.,.F.,.F.,(6,3,6),(6,6),(1.56090158029,2.52299916049,2.93530749734),
(0.,0.3),.UNSPECIFIED.);
#961=B_SPLINE_SURFACE_WITH_KNOTS('',5,5,((#57341,#57342,#57343,#57344,#57345,
#57346),(#57347,#57348,#57349,#57350,#57351,#57352),(#57353,#57354,#57355,
#57356,#57357,#57358),(#57359,#57360,#57361,#57362,#57363,#57364),(#57365,
#57366,#57367,#57368,#57369,#57370),(#57371,#57372,#57373,#57374,#57375,
#57376),(#57377,#57378,#57379,#57380,#57381,#57382),(#57383,#57384,#57385,
#57386,#57387,#57388),(#57389,#57390,#57391,#57392,#57393,#57394)),
 .UNSPECIFIED.,.F.,.F.,.F.,(6,3,6),(6,6),(8.63480411392599,12.3201261581,
17.1386583361),(0.,0.301475798114014),.UNSPECIFIED.);
#962=B_SPLINE_SURFACE_WITH_KNOTS('',5,5,((#57528,#57529,#57530,#57531,#57532,
#57533),(#57534,#57535,#57536,#57537,#57538,#57539),(#57540,#57541,#57542,
#57543,#57544,#57545),(#57546,#57547,#57548,#57549,#57550,#57551),(#57552,
#57553,#57554,#57555,#57556,#57557),(#57558,#57559,#57560,#57561,#57562,
#57563),(#57564,#57565,#57566,#57567,#57568,#57569),(#57570,#57571,#57572,
#57573,#57574,#57575),(#57576,#57577,#57578,#57579,#57580,#57581)),
 .UNSPECIFIED.,.F.,.F.,.F.,(6,3,6),(6,6),(-3.25426975736,0.,6.50853951471),
(0.,3.45067933061),.UNSPECIFIED.);
#963=B_SPLINE_SURFACE_WITH_KNOTS('',5,5,((#57612,#57613,#57614,#57615,#57616,
#57617),(#57618,#57619,#57620,#57621,#57622,#57623),(#57624,#57625,#57626,
#57627,#57628,#57629),(#57630,#57631,#57632,#57633,#57634,#57635),(#57636,
#57637,#57638,#57639,#57640,#57641),(#57642,#57643,#57644,#57645,#57646,
#57647),(#57648,#57649,#57650,#57651,#57652,#57653),(#57654,#57655,#57656,
#57657,#57658,#57659),(#57660,#57661,#57662,#57663,#57664,#57665)),
 .UNSPECIFIED.,.F.,.F.,.F.,(6,3,6),(6,6),(-3.25426975736,0.,6.50853951471),
(0.,3.45067933061),.UNSPECIFIED.);
#964=B_SPLINE_SURFACE_WITH_KNOTS('',5,1,((#57674,#57675),(#57676,#57677),
(#57678,#57679),(#57680,#57681),(#57682,#57683),(#57684,#57685)),
 .UNSPECIFIED.,.F.,.F.,.F.,(6,6),(2,2),(0.,1.06471780544),(0.,3.45067933061),
 .UNSPECIFIED.);
#965=B_SPLINE_SURFACE_WITH_KNOTS('',5,1,((#57689,#57690),(#57691,#57692),
(#57693,#57694),(#57695,#57696),(#57697,#57698),(#57699,#57700)),
 .UNSPECIFIED.,.F.,.F.,.F.,(6,6),(2,2),(0.,4.45911142417),(0.,3.45067933061),
 .UNSPECIFIED.);
#966=B_SPLINE_SURFACE_WITH_KNOTS('',5,1,((#57704,#57705),(#57706,#57707),
(#57708,#57709),(#57710,#57711),(#57712,#57713),(#57714,#57715)),
 .UNSPECIFIED.,.F.,.F.,.F.,(6,6),(2,2),(0.,0.261676985017),(0.,3.45067933061),
 .UNSPECIFIED.);
#967=B_SPLINE_SURFACE_WITH_KNOTS('',5,1,((#57719,#57720),(#57721,#57722),
(#57723,#57724),(#57725,#57726),(#57727,#57728),(#57729,#57730)),
 .UNSPECIFIED.,.F.,.F.,.F.,(6,6),(2,2),(0.,2.2409741083),(0.,3.45067933061),
 .UNSPECIFIED.);
#968=B_SPLINE_SURFACE_WITH_KNOTS('',5,1,((#57739,#57740),(#57741,#57742),
(#57743,#57744),(#57745,#57746),(#57747,#57748),(#57749,#57750)),
 .UNSPECIFIED.,.F.,.F.,.F.,(6,6),(2,2),(0.,0.230635297438),(0.,3.45067933061),
 .UNSPECIFIED.);
#969=B_SPLINE_SURFACE_WITH_KNOTS('',5,1,((#57754,#57755),(#57756,#57757),
(#57758,#57759),(#57760,#57761),(#57762,#57763),(#57764,#57765)),
 .UNSPECIFIED.,.F.,.F.,.F.,(6,6),(2,2),(0.,4.13278827108),(0.,3.45067933061),
 .UNSPECIFIED.);
#970=B_SPLINE_SURFACE_WITH_KNOTS('',5,1,((#57769,#57770),(#57771,#57772),
(#57773,#57774),(#57775,#57776),(#57777,#57778),(#57779,#57780)),
 .UNSPECIFIED.,.F.,.F.,.F.,(6,6),(2,2),(0.,4.13278827108),(0.,3.45067933061),
 .UNSPECIFIED.);
#971=B_SPLINE_SURFACE_WITH_KNOTS('',5,1,((#57784,#57785),(#57786,#57787),
(#57788,#57789),(#57790,#57791),(#57792,#57793),(#57794,#57795)),
 .UNSPECIFIED.,.F.,.F.,.F.,(6,6),(2,2),(0.,0.230635297438),(0.,3.45067933061),
 .UNSPECIFIED.);
#972=B_SPLINE_SURFACE_WITH_KNOTS('',5,1,((#57799,#57800),(#57801,#57802),
(#57803,#57804),(#57805,#57806),(#57807,#57808),(#57809,#57810)),
 .UNSPECIFIED.,.F.,.F.,.F.,(6,6),(2,2),(0.,2.2409741083),(0.,3.45067933061),
 .UNSPECIFIED.);
#973=B_SPLINE_SURFACE_WITH_KNOTS('',5,1,((#57819,#57820),(#57821,#57822),
(#57823,#57824),(#57825,#57826),(#57827,#57828),(#57829,#57830)),
 .UNSPECIFIED.,.F.,.F.,.F.,(6,6),(2,2),(0.,0.261676985017),(0.,3.45067933061),
 .UNSPECIFIED.);
#974=B_SPLINE_SURFACE_WITH_KNOTS('',5,1,((#57834,#57835),(#57836,#57837),
(#57838,#57839),(#57840,#57841),(#57842,#57843),(#57844,#57845)),
 .UNSPECIFIED.,.F.,.F.,.F.,(6,6),(2,2),(0.,4.45911142417),(0.,3.45067933061),
 .UNSPECIFIED.);
#975=B_SPLINE_SURFACE_WITH_KNOTS('',5,1,((#57849,#57850),(#57851,#57852),
(#57853,#57854),(#57855,#57856),(#57857,#57858),(#57859,#57860)),
 .UNSPECIFIED.,.F.,.F.,.F.,(6,6),(2,2),(0.,1.06471780544),(0.,3.45067933061),
 .UNSPECIFIED.);
#976=B_SPLINE_SURFACE_WITH_KNOTS('',5,5,((#63396,#63397,#63398,#63399,#63400,
#63401),(#63402,#63403,#63404,#63405,#63406,#63407),(#63408,#63409,#63410,
#63411,#63412,#63413),(#63414,#63415,#63416,#63417,#63418,#63419),(#63420,
#63421,#63422,#63423,#63424,#63425),(#63426,#63427,#63428,#63429,#63430,
#63431),(#63432,#63433,#63434,#63435,#63436,#63437),(#63438,#63439,#63440,
#63441,#63442,#63443),(#63444,#63445,#63446,#63447,#63448,#63449)),
 .UNSPECIFIED.,.F.,.F.,.F.,(6,3,6),(6,6),(0.168109267782,0.19381333378,
0.219517399778),(0.,0.3),.UNSPECIFIED.);
#977=B_SPLINE_SURFACE_WITH_KNOTS('',5,5,((#63455,#63456,#63457,#63458,#63459,
#63460),(#63461,#63462,#63463,#63464,#63465,#63466),(#63467,#63468,#63469,
#63470,#63471,#63472),(#63473,#63474,#63475,#63476,#63477,#63478),(#63479,
#63480,#63481,#63482,#63483,#63484),(#63485,#63486,#63487,#63488,#63489,
#63490)),.UNSPECIFIED.,.F.,.F.,.F.,(6,6),(6,6),(0.167763693398,0.219167536347),
(0.,0.3),.UNSPECIFIED.);
#978=B_SPLINE_SURFACE_WITH_KNOTS('',5,5,((#63499,#63500,#63501,#63502,#63503,
#63504),(#63505,#63506,#63507,#63508,#63509,#63510),(#63511,#63512,#63513,
#63514,#63515,#63516),(#63517,#63518,#63519,#63520,#63521,#63522),(#63523,
#63524,#63525,#63526,#63527,#63528),(#63529,#63530,#63531,#63532,#63533,
#63534),(#63535,#63536,#63537,#63538,#63539,#63540),(#63541,#63542,#63543,
#63544,#63545,#63546),(#63547,#63548,#63549,#63550,#63551,#63552),(#63553,
#63554,#63555,#63556,#63557,#63558),(#63559,#63560,#63561,#63562,#63563,
#63564),(#63565,#63566,#63567,#63568,#63569,#63570),(#63571,#63572,#63573,
#63574,#63575,#63576),(#63577,#63578,#63579,#63580,#63581,#63582),(#63583,
#63584,#63585,#63586,#63587,#63588),(#63589,#63590,#63591,#63592,#63593,
#63594),(#63595,#63596,#63597,#63598,#63599,#63600),(#63601,#63602,#63603,
#63604,#63605,#63606)),.UNSPECIFIED.,.F.,.F.,.F.,(6,3,3,3,3,6),(6,6),(16.6199171728,
22.5384106111,30.5763256225,36.3852909182,40.8836102145,50.0065308028),
(0.,0.3),.UNSPECIFIED.);
#979=B_SPLINE_SURFACE_WITH_KNOTS('',5,5,((#63633,#63634,#63635,#63636,#63637,
#63638),(#63639,#63640,#63641,#63642,#63643,#63644),(#63645,#63646,#63647,
#63648,#63649,#63650),(#63651,#63652,#63653,#63654,#63655,#63656),(#63657,
#63658,#63659,#63660,#63661,#63662),(#63663,#63664,#63665,#63666,#63667,
#63668),(#63669,#63670,#63671,#63672,#63673,#63674),(#63675,#63676,#63677,
#63678,#63679,#63680),(#63681,#63682,#63683,#63684,#63685,#63686),(#63687,
#63688,#63689,#63690,#63691,#63692),(#63693,#63694,#63695,#63696,#63697,
#63698),(#63699,#63700,#63701,#63702,#63703,#63704),(#63705,#63706,#63707,
#63708,#63709,#63710),(#63711,#63712,#63713,#63714,#63715,#63716),(#63717,
#63718,#63719,#63720,#63721,#63722),(#63723,#63724,#63725,#63726,#63727,
#63728),(#63729,#63730,#63731,#63732,#63733,#63734),(#63735,#63736,#63737,
#63738,#63739,#63740)),.UNSPECIFIED.,.F.,.F.,.F.,(6,3,3,3,3,6),(6,6),(12.5665153309,
21.1100928391,29.3112279304,33.9967366188,38.6616814006,45.9550550567),
(0.,0.3),.UNSPECIFIED.);
#980=B_SPLINE_SURFACE_WITH_KNOTS('',5,1,((#63864,#63865),(#63866,#63867),
(#63868,#63869),(#63870,#63871),(#63872,#63873),(#63874,#63875),(#63876,
#63877),(#63878,#63879),(#63880,#63881),(#63882,#63883),(#63884,#63885),
(#63886,#63887),(#63888,#63889),(#63890,#63891),(#63892,#63893),(#63894,
#63895),(#63896,#63897),(#63898,#63899),(#63900,#63901),(#63902,#63903),
(#63904,#63905),(#63906,#63907),(#63908,#63909),(#63910,#63911)),
 .UNSPECIFIED.,.F.,.F.,.F.,(6,3,3,3,3,3,3,6),(2,2),(7.96998083279,14.7982954236,
17.0693303053,21.6304346192,24.5117412112,26.3698077055,28.2289298688,30.7490985197),
(0.,0.168000000000001),.UNSPECIFIED.);
#981=B_SPLINE_SURFACE_WITH_KNOTS('',5,5,((#63913,#63914,#63915,#63916,#63917,
#63918),(#63919,#63920,#63921,#63922,#63923,#63924),(#63925,#63926,#63927,
#63928,#63929,#63930),(#63931,#63932,#63933,#63934,#63935,#63936),(#63937,
#63938,#63939,#63940,#63941,#63942),(#63943,#63944,#63945,#63946,#63947,
#63948),(#63949,#63950,#63951,#63952,#63953,#63954),(#63955,#63956,#63957,
#63958,#63959,#63960),(#63961,#63962,#63963,#63964,#63965,#63966)),
 .UNSPECIFIED.,.F.,.F.,.F.,(6,3,6),(6,6),(2.81282962644,5.03686033438,7.40331879449),
(0.,0.3),.UNSPECIFIED.);
#982=B_SPLINE_SURFACE_WITH_KNOTS('',5,5,((#64024,#64025,#64026,#64027,#64028,
#64029),(#64030,#64031,#64032,#64033,#64034,#64035),(#64036,#64037,#64038,
#64039,#64040,#64041),(#64042,#64043,#64044,#64045,#64046,#64047),(#64048,
#64049,#64050,#64051,#64052,#64053),(#64054,#64055,#64056,#64057,#64058,
#64059),(#64060,#64061,#64062,#64063,#64064,#64065),(#64066,#64067,#64068,
#64069,#64070,#64071),(#64072,#64073,#64074,#64075,#64076,#64077)),
 .UNSPECIFIED.,.F.,.F.,.F.,(6,3,6),(6,6),(2.10740882,4.45303692778,6.6978412202),
(0.,0.3),.UNSPECIFIED.);
#983=B_SPLINE_SURFACE_WITH_KNOTS('',5,1,((#64089,#64090),(#64091,#64092),
(#64093,#64094),(#64095,#64096),(#64097,#64098),(#64099,#64100),(#64101,
#64102),(#64103,#64104),(#64105,#64106),(#64107,#64108),(#64109,#64110),
(#64111,#64112)),.UNSPECIFIED.,.F.,.F.,.F.,(6,3,3,6),(2,2),(1.44955812073,
3.05666068068,3.70866677692,4.6795923245),(0.,0.168000000000001),
 .UNSPECIFIED.);
#984=B_SPLINE_SURFACE_WITH_KNOTS('',5,5,((#64114,#64115,#64116,#64117,#64118,
#64119),(#64120,#64121,#64122,#64123,#64124,#64125),(#64126,#64127,#64128,
#64129,#64130,#64131),(#64132,#64133,#64134,#64135,#64136,#64137),(#64138,
#64139,#64140,#64141,#64142,#64143),(#64144,#64145,#64146,#64147,#64148,
#64149),(#64150,#64151,#64152,#64153,#64154,#64155),(#64156,#64157,#64158,
#64159,#64160,#64161),(#64162,#64163,#64164,#64165,#64166,#64167),(#64168,
#64169,#64170,#64171,#64172,#64173),(#64174,#64175,#64176,#64177,#64178,
#64179),(#64180,#64181,#64182,#64183,#64184,#64185),(#64186,#64187,#64188,
#64189,#64190,#64191),(#64192,#64193,#64194,#64195,#64196,#64197),(#64198,
#64199,#64200,#64201,#64202,#64203)),.UNSPECIFIED.,.F.,.F.,.F.,(6,3,3,3,
6),(6,6),(2.88912209896,5.1429678095,7.13061874999,9.13254225469,11.2103678193),
(0.,0.3),.UNSPECIFIED.);
#985=B_SPLINE_SURFACE_WITH_KNOTS('',5,5,((#64315,#64316,#64317,#64318,#64319,
#64320),(#64321,#64322,#64323,#64324,#64325,#64326),(#64327,#64328,#64329,
#64330,#64331,#64332),(#64333,#64334,#64335,#64336,#64337,#64338),(#64339,
#64340,#64341,#64342,#64343,#64344),(#64345,#64346,#64347,#64348,#64349,
#64350),(#64351,#64352,#64353,#64354,#64355,#64356),(#64357,#64358,#64359,
#64360,#64361,#64362),(#64363,#64364,#64365,#64366,#64367,#64368),(#64369,
#64370,#64371,#64372,#64373,#64374),(#64375,#64376,#64377,#64378,#64379,
#64380),(#64381,#64382,#64383,#64384,#64385,#64386),(#64387,#64388,#64389,
#64390,#64391,#64392),(#64393,#64394,#64395,#64396,#64397,#64398),(#64399,
#64400,#64401,#64402,#64403,#64404)),.UNSPECIFIED.,.F.,.F.,.F.,(6,3,3,3,
6),(6,6),(3.85983652914,5.49553262739,7.77935654812,9.92881869084,12.1812673196),
(0.,0.3),.UNSPECIFIED.);
#986=B_SPLINE_SURFACE_WITH_KNOTS('',5,1,((#64422,#64423),(#64424,#64425),
(#64426,#64427),(#64428,#64429),(#64430,#64431),(#64432,#64433),(#64434,
#64435),(#64436,#64437),(#64438,#64439),(#64440,#64441),(#64442,#64443),
(#64444,#64445),(#64446,#64447),(#64448,#64449),(#64450,#64451),(#64452,
#64453),(#64454,#64455),(#64456,#64457),(#64458,#64459),(#64460,#64461),
(#64462,#64463),(#64464,#64465),(#64466,#64467),(#64468,#64469)),
 .UNSPECIFIED.,.F.,.F.,.F.,(6,3,3,3,3,3,3,6),(2,2),(1.38821963106,1.92901664016,
2.47239764086,3.02881582981,3.59314912291,4.73969819441,5.30964375821,6.97732526363),
(0.,0.168000000000001),.UNSPECIFIED.);
#987=B_SPLINE_SURFACE_WITH_KNOTS('',5,5,((#64471,#64472,#64473,#64474,#64475,
#64476),(#64477,#64478,#64479,#64480,#64481,#64482),(#64483,#64484,#64485,
#64486,#64487,#64488),(#64489,#64490,#64491,#64492,#64493,#64494),(#64495,
#64496,#64497,#64498,#64499,#64500),(#64501,#64502,#64503,#64504,#64505,
#64506),(#64507,#64508,#64509,#64510,#64511,#64512),(#64513,#64514,#64515,
#64516,#64517,#64518),(#64519,#64520,#64521,#64522,#64523,#64524),(#64525,
#64526,#64527,#64528,#64529,#64530),(#64531,#64532,#64533,#64534,#64535,
#64536),(#64537,#64538,#64539,#64540,#64541,#64542),(#64543,#64544,#64545,
#64546,#64547,#64548),(#64549,#64550,#64551,#64552,#64553,#64554),(#64555,
#64556,#64557,#64558,#64559,#64560),(#64561,#64562,#64563,#64564,#64565,
#64566),(#64567,#64568,#64569,#64570,#64571,#64572),(#64573,#64574,#64575,
#64576,#64577,#64578),(#64579,#64580,#64581,#64582,#64583,#64584),(#64585,
#64586,#64587,#64588,#64589,#64590),(#64591,#64592,#64593,#64594,#64595,
#64596),(#64597,#64598,#64599,#64600,#64601,#64602),(#64603,#64604,#64605,
#64606,#64607,#64608),(#64609,#64610,#64611,#64612,#64613,#64614)),
 .UNSPECIFIED.,.F.,.F.,.F.,(6,3,3,3,3,3,3,6),(6,6),(2.49496263694,3.75614411414,
4.32934465344,5.25874047989,6.18762608197,8.03803358836,9.88322107258,15.7678954384),
(0.,0.3),.UNSPECIFIED.);
#988=B_SPLINE_SURFACE_WITH_KNOTS('',5,5,((#64753,#64754,#64755,#64756,#64757,
#64758),(#64759,#64760,#64761,#64762,#64763,#64764),(#64765,#64766,#64767,
#64768,#64769,#64770),(#64771,#64772,#64773,#64774,#64775,#64776),(#64777,
#64778,#64779,#64780,#64781,#64782),(#64783,#64784,#64785,#64786,#64787,
#64788),(#64789,#64790,#64791,#64792,#64793,#64794),(#64795,#64796,#64797,
#64798,#64799,#64800),(#64801,#64802,#64803,#64804,#64805,#64806),(#64807,
#64808,#64809,#64810,#64811,#64812),(#64813,#64814,#64815,#64816,#64817,
#64818),(#64819,#64820,#64821,#64822,#64823,#64824),(#64825,#64826,#64827,
#64828,#64829,#64830),(#64831,#64832,#64833,#64834,#64835,#64836),(#64837,
#64838,#64839,#64840,#64841,#64842),(#64843,#64844,#64845,#64846,#64847,
#64848),(#64849,#64850,#64851,#64852,#64853,#64854),(#64855,#64856,#64857,
#64858,#64859,#64860)),.UNSPECIFIED.,.F.,.F.,.F.,(6,3,3,3,3,6),(6,6),(4.00115394842,
11.4721831186,13.451526058,14.4455167529,15.8981054324,17.2738332784),(0.,
0.3),.UNSPECIFIED.);
#989=B_SPLINE_SURFACE_WITH_KNOTS('',5,1,((#64881,#64882),(#64883,#64884),
(#64885,#64886),(#64887,#64888),(#64889,#64890),(#64891,#64892),(#64893,
#64894),(#64895,#64896),(#64897,#64898),(#64899,#64900),(#64901,#64902),
(#64903,#64904),(#64905,#64906),(#64907,#64908),(#64909,#64910),(#64911,
#64912),(#64913,#64914),(#64915,#64916)),.UNSPECIFIED.,.F.,.F.,.F.,(6,3,
3,3,3,6),(2,2),(2.30144058436,3.21523268549,4.17948834992,7.86941426972,
10.6293166988,11.5241632533),(0.,0.168000000000001),.UNSPECIFIED.);
#990=B_SPLINE_SURFACE_WITH_KNOTS('',5,5,((#64918,#64919,#64920,#64921,#64922,
#64923),(#64924,#64925,#64926,#64927,#64928,#64929),(#64930,#64931,#64932,
#64933,#64934,#64935),(#64936,#64937,#64938,#64939,#64940,#64941),(#64942,
#64943,#64944,#64945,#64946,#64947),(#64948,#64949,#64950,#64951,#64952,
#64953),(#64954,#64955,#64956,#64957,#64958,#64959),(#64960,#64961,#64962,
#64963,#64964,#64965),(#64966,#64967,#64968,#64969,#64970,#64971)),
 .UNSPECIFIED.,.F.,.F.,.F.,(6,3,6),(6,6),(1.35769229991,2.30681875984,3.25594521977),
(0.,0.3),.UNSPECIFIED.);
#991=B_SPLINE_SURFACE_WITH_KNOTS('',5,5,((#64975,#64976,#64977,#64978,#64979,
#64980),(#64981,#64982,#64983,#64984,#64985,#64986),(#64987,#64988,#64989,
#64990,#64991,#64992),(#64993,#64994,#64995,#64996,#64997,#64998),(#64999,
#65000,#65001,#65002,#65003,#65004),(#65005,#65006,#65007,#65008,#65009,
#65010),(#65011,#65012,#65013,#65014,#65015,#65016),(#65017,#65018,#65019,
#65020,#65021,#65022),(#65023,#65024,#65025,#65026,#65027,#65028)),
 .UNSPECIFIED.,.F.,.F.,.F.,(6,3,6),(6,6),(1.35799881012,2.30712712606,3.25625544201),
(0.,0.3),.UNSPECIFIED.);
#992=B_SPLINE_SURFACE_WITH_KNOTS('',5,1,((#65032,#65033),(#65034,#65035),
(#65036,#65037),(#65038,#65039),(#65040,#65041),(#65042,#65043)),
 .UNSPECIFIED.,.F.,.F.,.F.,(6,6),(2,2),(0.96552770951,2.34485300881),(0.,
0.168000000000001),.UNSPECIFIED.);
#993=B_SPLINE_SURFACE_WITH_KNOTS('',5,5,((#65045,#65046,#65047,#65048,#65049,
#65050),(#65051,#65052,#65053,#65054,#65055,#65056),(#65057,#65058,#65059,
#65060,#65061,#65062),(#65063,#65064,#65065,#65066,#65067,#65068),(#65069,
#65070,#65071,#65072,#65073,#65074),(#65075,#65076,#65077,#65078,#65079,
#65080),(#65081,#65082,#65083,#65084,#65085,#65086),(#65087,#65088,#65089,
#65090,#65091,#65092),(#65093,#65094,#65095,#65096,#65097,#65098)),
 .UNSPECIFIED.,.F.,.F.,.F.,(6,3,6),(6,6),(0.591273571839,1.32390886326,
1.88642093473),(0.,0.3),.UNSPECIFIED.);
#994=B_SPLINE_SURFACE_WITH_KNOTS('',5,5,((#65107,#65108,#65109,#65110,#65111,
#65112),(#65113,#65114,#65115,#65116,#65117,#65118),(#65119,#65120,#65121,
#65122,#65123,#65124),(#65125,#65126,#65127,#65128,#65129,#65130),(#65131,
#65132,#65133,#65134,#65135,#65136),(#65137,#65138,#65139,#65140,#65141,
#65142),(#65143,#65144,#65145,#65146,#65147,#65148),(#65149,#65150,#65151,
#65152,#65153,#65154),(#65155,#65156,#65157,#65158,#65159,#65160)),
 .UNSPECIFIED.,.F.,.F.,.F.,(6,3,6),(6,6),(0.591154687012,1.24895024918,
1.88603455695),(0.,0.3),.UNSPECIFIED.);
#995=B_SPLINE_SURFACE_WITH_KNOTS('',5,1,((#65172,#65173),(#65174,#65175),
(#65176,#65177),(#65178,#65179),(#65180,#65181),(#65182,#65183)),
 .UNSPECIFIED.,.F.,.F.,.F.,(6,6),(2,2),(0.493788369863,1.19920032681),(0.,
0.168000000000001),.UNSPECIFIED.);
#996=B_SPLINE_SURFACE_WITH_KNOTS('',5,5,((#65255,#65256,#65257,#65258,#65259,
#65260),(#65261,#65262,#65263,#65264,#65265,#65266),(#65267,#65268,#65269,
#65270,#65271,#65272),(#65273,#65274,#65275,#65276,#65277,#65278),(#65279,
#65280,#65281,#65282,#65283,#65284),(#65285,#65286,#65287,#65288,#65289,
#65290),(#65291,#65292,#65293,#65294,#65295,#65296),(#65297,#65298,#65299,
#65300,#65301,#65302),(#65303,#65304,#65305,#65306,#65307,#65308)),
 .UNSPECIFIED.,.F.,.F.,.F.,(6,3,6),(6,6),(1.56059358548,2.9568323585,4.75555213266),
(0.,0.3),.UNSPECIFIED.);
#997=B_SPLINE_SURFACE_WITH_KNOTS('',5,5,((#65361,#65362,#65363,#65364,#65365,
#65366),(#65367,#65368,#65369,#65370,#65371,#65372),(#65373,#65374,#65375,
#65376,#65377,#65378),(#65379,#65380,#65381,#65382,#65383,#65384),(#65385,
#65386,#65387,#65388,#65389,#65390),(#65391,#65392,#65393,#65394,#65395,
#65396),(#65397,#65398,#65399,#65400,#65401,#65402),(#65403,#65404,#65405,
#65406,#65407,#65408),(#65409,#65410,#65411,#65412,#65413,#65414)),
 .UNSPECIFIED.,.F.,.F.,.F.,(6,3,6),(6,6),(1.62520881516,3.23201031665,4.82017891154),
(0.,0.3),.UNSPECIFIED.);
#998=B_SPLINE_SURFACE_WITH_KNOTS('',5,1,((#65421,#65422),(#65423,#65424),
(#65425,#65426),(#65427,#65428),(#65429,#65430),(#65431,#65432)),
 .UNSPECIFIED.,.F.,.F.,.F.,(6,6),(2,2),(1.41662542015,3.44037602036),(0.,
0.168000000000001),.UNSPECIFIED.);
#999=B_SPLINE_SURFACE_WITH_KNOTS('',5,5,((#65433,#65434,#65435,#65436,#65437,
#65438),(#65439,#65440,#65441,#65442,#65443,#65444),(#65445,#65446,#65447,
#65448,#65449,#65450),(#65451,#65452,#65453,#65454,#65455,#65456),(#65457,
#65458,#65459,#65460,#65461,#65462),(#65463,#65464,#65465,#65466,#65467,
#65468),(#65469,#65470,#65471,#65472,#65473,#65474),(#65475,#65476,#65477,
#65478,#65479,#65480),(#65481,#65482,#65483,#65484,#65485,#65486)),
 .UNSPECIFIED.,.F.,.F.,.F.,(6,3,6),(6,6),(3.6079177031,7.76832519582,12.1678629797),
(0.,0.3),.UNSPECIFIED.);
#1000=B_SPLINE_SURFACE_WITH_KNOTS('',5,5,((#65508,#65509,#65510,#65511,
#65512,#65513),(#65514,#65515,#65516,#65517,#65518,#65519),(#65520,#65521,
#65522,#65523,#65524,#65525),(#65526,#65527,#65528,#65529,#65530,#65531),
(#65532,#65533,#65534,#65535,#65536,#65537),(#65538,#65539,#65540,#65541,
#65542,#65543),(#65544,#65545,#65546,#65547,#65548,#65549),(#65550,#65551,
#65552,#65553,#65554,#65555),(#65556,#65557,#65558,#65559,#65560,#65561)),
 .UNSPECIFIED.,.F.,.F.,.F.,(6,3,6),(6,6),(5.26262328413,9.35737491835,13.8219121669),
(0.,0.3),.UNSPECIFIED.);
#1001=B_SPLINE_SURFACE_WITH_KNOTS('',5,1,((#65583,#65584),(#65585,#65586),
(#65587,#65588),(#65589,#65590),(#65591,#65592),(#65593,#65594),(#65595,
#65596),(#65597,#65598),(#65599,#65600),(#65601,#65602),(#65603,#65604),
(#65605,#65606),(#65607,#65608),(#65609,#65610),(#65611,#65612),(#65613,
#65614),(#65615,#65616)),.UNSPECIFIED.,.F.,.F.,.F.,(6,5,3,3,6),(2,2),(1.81082989417716,
1.81130449228,3.02278054545,4.81654635721,7.83913682071),(0.,0.168000000000001),
 .UNSPECIFIED.);
#1002=B_SPLINE_SURFACE_WITH_KNOTS('',5,5,((#65619,#65620,#65621,#65622,
#65623,#65624),(#65625,#65626,#65627,#65628,#65629,#65630),(#65631,#65632,
#65633,#65634,#65635,#65636),(#65637,#65638,#65639,#65640,#65641,#65642),
(#65643,#65644,#65645,#65646,#65647,#65648),(#65649,#65650,#65651,#65652,
#65653,#65654),(#65655,#65656,#65657,#65658,#65659,#65660),(#65661,#65662,
#65663,#65664,#65665,#65666),(#65667,#65668,#65669,#65670,#65671,#65672)),
 .UNSPECIFIED.,.F.,.F.,.F.,(6,3,6),(6,6),(6.65601718416,11.623259991,18.3853430669),
(0.,0.3),.UNSPECIFIED.);
#1003=B_SPLINE_SURFACE_WITH_KNOTS('',5,5,((#65681,#65682,#65683,#65684,
#65685,#65686),(#65687,#65688,#65689,#65690,#65691,#65692),(#65693,#65694,
#65695,#65696,#65697,#65698),(#65699,#65700,#65701,#65702,#65703,#65704),
(#65705,#65706,#65707,#65708,#65709,#65710),(#65711,#65712,#65713,#65714,
#65715,#65716),(#65717,#65718,#65719,#65720,#65721,#65722),(#65723,#65724,
#65725,#65726,#65727,#65728),(#65729,#65730,#65731,#65732,#65733,#65734)),
 .UNSPECIFIED.,.F.,.F.,.F.,(6,3,6),(6,6),(6.65635355468,12.3414051375,18.3857494183),
(0.,0.3),.UNSPECIFIED.);
#1004=B_SPLINE_SURFACE_WITH_KNOTS('',5,1,((#65748,#65749),(#65750,#65751),
(#65752,#65753),(#65754,#65755),(#65756,#65757),(#65758,#65759)),
 .UNSPECIFIED.,.F.,.F.,.F.,(6,6),(2,2),(5.84195403358,14.187602653),(0.,
0.168000000000001),.UNSPECIFIED.);
#1005=B_SPLINE_SURFACE_WITH_KNOTS('',5,5,((#65761,#65762,#65763,#65764,
#65765,#65766),(#65767,#65768,#65769,#65770,#65771,#65772),(#65773,#65774,
#65775,#65776,#65777,#65778),(#65779,#65780,#65781,#65782,#65783,#65784),
(#65785,#65786,#65787,#65788,#65789,#65790),(#65791,#65792,#65793,#65794,
#65795,#65796),(#65797,#65798,#65799,#65800,#65801,#65802),(#65803,#65804,
#65805,#65806,#65807,#65808),(#65809,#65810,#65811,#65812,#65813,#65814)),
 .UNSPECIFIED.,.F.,.F.,.F.,(6,3,6),(6,6),(6.656059514,12.5206580023,18.3855563608),
(0.,0.3),.UNSPECIFIED.);
#1006=B_SPLINE_SURFACE_WITH_KNOTS('',5,5,((#65872,#65873,#65874,#65875,
#65876,#65877),(#65878,#65879,#65880,#65881,#65882,#65883),(#65884,#65885,
#65886,#65887,#65888,#65889),(#65890,#65891,#65892,#65893,#65894,#65895),
(#65896,#65897,#65898,#65899,#65900,#65901),(#65902,#65903,#65904,#65905,
#65906,#65907),(#65908,#65909,#65910,#65911,#65912,#65913),(#65914,#65915,
#65916,#65917,#65918,#65919),(#65920,#65921,#65922,#65923,#65924,#65925)),
 .UNSPECIFIED.,.F.,.F.,.F.,(6,3,6),(6,6),(6.65611545055,12.5207139017,18.3856123466),
(0.,0.3),.UNSPECIFIED.);
#1007=B_SPLINE_SURFACE_WITH_KNOTS('',5,1,((#65983,#65984),(#65985,#65986),
(#65987,#65988),(#65989,#65990),(#65991,#65992),(#65993,#65994)),
 .UNSPECIFIED.,.F.,.F.,.F.,(6,6),(2,2),(5.84195403358,14.187602653),(0.,
0.168000000000001),.UNSPECIFIED.);
#1008=B_SPLINE_SURFACE_WITH_KNOTS('',5,5,((#65996,#65997,#65998,#65999,
#66000,#66001),(#66002,#66003,#66004,#66005,#66006,#66007),(#66008,#66009,
#66010,#66011,#66012,#66013),(#66014,#66015,#66016,#66017,#66018,#66019),
(#66020,#66021,#66022,#66023,#66024,#66025),(#66026,#66027,#66028,#66029,
#66030,#66031),(#66032,#66033,#66034,#66035,#66036,#66037),(#66038,#66039,
#66040,#66041,#66042,#66043),(#66044,#66045,#66046,#66047,#66048,#66049),
(#66050,#66051,#66052,#66053,#66054,#66055),(#66056,#66057,#66058,#66059,
#66060,#66061),(#66062,#66063,#66064,#66065,#66066,#66067),(#66068,#66069,
#66070,#66071,#66072,#66073),(#66074,#66075,#66076,#66077,#66078,#66079)),
 .UNSPECIFIED.,.F.,.F.,.F.,(6,3,5,6),(6,6),(5.26516274934,9.50401785273,
13.8254388584,13.9110416194906),(0.,0.3),.UNSPECIFIED.);
#1009=B_SPLINE_SURFACE_WITH_KNOTS('',5,5,((#66094,#66095,#66096,#66097,
#66098,#66099),(#66100,#66101,#66102,#66103,#66104,#66105),(#66106,#66107,
#66108,#66109,#66110,#66111),(#66112,#66113,#66114,#66115,#66116,#66117),
(#66118,#66119,#66120,#66121,#66122,#66123),(#66124,#66125,#66126,#66127,
#66128,#66129),(#66130,#66131,#66132,#66133,#66134,#66135),(#66136,#66137,
#66138,#66139,#66140,#66141),(#66142,#66143,#66144,#66145,#66146,#66147)),
 .UNSPECIFIED.,.F.,.F.,.F.,(6,3,6),(6,6),(3.60712399577,7.99998279071,12.1666998724),
(0.,0.3),.UNSPECIFIED.);
#1010=B_SPLINE_SURFACE_WITH_KNOTS('',5,1,((#66225,#66226),(#66227,#66228),
(#66229,#66230),(#66231,#66232),(#66233,#66234),(#66235,#66236),(#66237,
#66238),(#66239,#66240),(#66241,#66242),(#66243,#66244),(#66245,#66246),
(#66247,#66248)),.UNSPECIFIED.,.F.,.F.,.F.,(6,3,3,6),(2,2),(2.71670313018,
5.73911718302,7.53277830329,8.74418364899),(0.,0.168000000000001),
 .UNSPECIFIED.);
#1011=B_SPLINE_SURFACE_WITH_KNOTS('',5,5,((#66250,#66251,#66252,#66253,
#66254,#66255),(#66256,#66257,#66258,#66259,#66260,#66261),(#66262,#66263,
#66264,#66265,#66266,#66267),(#66268,#66269,#66270,#66271,#66272,#66273),
(#66274,#66275,#66276,#66277,#66278,#66279),(#66280,#66281,#66282,#66283,
#66284,#66285),(#66286,#66287,#66288,#66289,#66290,#66291),(#66292,#66293,
#66294,#66295,#66296,#66297),(#66298,#66299,#66300,#66301,#66302,#66303),
(#66304,#66305,#66306,#66307,#66308,#66309),(#66310,#66311,#66312,#66313,
#66314,#66315),(#66316,#66317,#66318,#66319,#66320,#66321),(#66322,#66323,
#66324,#66325,#66326,#66327),(#66328,#66329,#66330,#66331,#66332,#66333),
(#66334,#66335,#66336,#66337,#66338,#66339)),.UNSPECIFIED.,.F.,.F.,.F.,
(6,3,3,3,6),(6,6),(5.22957298235,8.73373254507,11.36693316,14.9187174958,
17.8070761317),(0.,0.3),.UNSPECIFIED.);
#1012=B_SPLINE_SURFACE_WITH_KNOTS('',5,5,((#66427,#66428,#66429,#66430,
#66431,#66432),(#66433,#66434,#66435,#66436,#66437,#66438),(#66439,#66440,
#66441,#66442,#66443,#66444),(#66445,#66446,#66447,#66448,#66449,#66450),
(#66451,#66452,#66453,#66454,#66455,#66456),(#66457,#66458,#66459,#66460,
#66461,#66462),(#66463,#66464,#66465,#66466,#66467,#66468),(#66469,#66470,
#66471,#66472,#66473,#66474),(#66475,#66476,#66477,#66478,#66479,#66480),
(#66481,#66482,#66483,#66484,#66485,#66486),(#66487,#66488,#66489,#66490,
#66491,#66492),(#66493,#66494,#66495,#66496,#66497,#66498),(#66499,#66500,
#66501,#66502,#66503,#66504),(#66505,#66506,#66507,#66508,#66509,#66510),
(#66511,#66512,#66513,#66514,#66515,#66516)),.UNSPECIFIED.,.F.,.F.,.F.,
(6,3,3,3,6),(6,6),(5.19541482867,8.7224443269,11.7666783733,14.769293572,
17.772416875),(0.,0.3),.UNSPECIFIED.);
#1013=B_SPLINE_SURFACE_WITH_KNOTS('',5,1,((#66537,#66538),(#66539,#66540),
(#66541,#66542),(#66543,#66544),(#66545,#66546),(#66547,#66548),(#66549,
#66550),(#66551,#66552),(#66553,#66554),(#66555,#66556),(#66557,#66558),
(#66559,#66560),(#66561,#66562),(#66563,#66564),(#66565,#66566),(#66567,
#66568),(#66569,#66570),(#66571,#66572)),.UNSPECIFIED.,.F.,.F.,.F.,(6,3,
3,3,3,6),(2,2),(2.56814442563,4.26587753681,5.98143772792,6.84529958826,
9.44079904688,11.1645337758),(0.,0.168000000000001),.UNSPECIFIED.);
#1014=B_SPLINE_SURFACE_WITH_KNOTS('',5,5,((#66574,#66575,#66576,#66577,
#66578,#66579),(#66580,#66581,#66582,#66583,#66584,#66585),(#66586,#66587,
#66588,#66589,#66590,#66591),(#66592,#66593,#66594,#66595,#66596,#66597),
(#66598,#66599,#66600,#66601,#66602,#66603),(#66604,#66605,#66606,#66607,
#66608,#66609),(#66610,#66611,#66612,#66613,#66614,#66615),(#66616,#66617,
#66618,#66619,#66620,#66621),(#66622,#66623,#66624,#66625,#66626,#66627)),
 .UNSPECIFIED.,.F.,.F.,.F.,(6,3,6),(6,6),(1.00648613473,1.91246268912,2.81843924351),
(0.,0.3),.UNSPECIFIED.);
#1015=B_SPLINE_SURFACE_WITH_KNOTS('',5,5,((#66631,#66632,#66633,#66634,
#66635,#66636),(#66637,#66638,#66639,#66640,#66641,#66642),(#66643,#66644,
#66645,#66646,#66647,#66648),(#66649,#66650,#66651,#66652,#66653,#66654),
(#66655,#66656,#66657,#66658,#66659,#66660),(#66661,#66662,#66663,#66664,
#66665,#66666),(#66667,#66668,#66669,#66670,#66671,#66672),(#66673,#66674,
#66675,#66676,#66677,#66678),(#66679,#66680,#66681,#66682,#66683,#66684)),
 .UNSPECIFIED.,.F.,.F.,.F.,(6,3,6),(6,6),(1.00636935115,1.91235557727,2.81834180338),
(0.,0.3),.UNSPECIFIED.);
#1016=B_SPLINE_SURFACE_WITH_KNOTS('',5,1,((#66688,#66689),(#66690,#66691),
(#66692,#66693),(#66694,#66695),(#66696,#66697),(#66698,#66699)),
 .UNSPECIFIED.,.F.,.F.,.F.,(6,6),(2,2),(0.855391128886,2.07737845587),(0.,
0.168000000000001),.UNSPECIFIED.);
#1017=B_SPLINE_SURFACE_WITH_KNOTS('',5,5,((#66701,#66702,#66703,#66704,
#66705,#66706),(#66707,#66708,#66709,#66710,#66711,#66712),(#66713,#66714,
#66715,#66716,#66717,#66718),(#66719,#66720,#66721,#66722,#66723,#66724),
(#66725,#66726,#66727,#66728,#66729,#66730),(#66731,#66732,#66733,#66734,
#66735,#66736),(#66737,#66738,#66739,#66740,#66741,#66742),(#66743,#66744,
#66745,#66746,#66747,#66748),(#66749,#66750,#66751,#66752,#66753,#66754),
(#66755,#66756,#66757,#66758,#66759,#66760),(#66761,#66762,#66763,#66764,
#66765,#66766),(#66767,#66768,#66769,#66770,#66771,#66772),(#66773,#66774,
#66775,#66776,#66777,#66778),(#66779,#66780,#66781,#66782,#66783,#66784),
(#66785,#66786,#66787,#66788,#66789,#66790)),.UNSPECIFIED.,.F.,.F.,.F.,
(6,3,3,3,6),(6,6),(5.25334327713,8.78087326212,11.4506730327,14.9857329729,
17.830940375),(0.,0.3),.UNSPECIFIED.);
#1018=B_SPLINE_SURFACE_WITH_KNOTS('',5,5,((#66809,#66810,#66811,#66812,
#66813,#66814),(#66815,#66816,#66817,#66818,#66819,#66820),(#66821,#66822,
#66823,#66824,#66825,#66826),(#66827,#66828,#66829,#66830,#66831,#66832),
(#66833,#66834,#66835,#66836,#66837,#66838),(#66839,#66840,#66841,#66842,
#66843,#66844),(#66845,#66846,#66847,#66848,#66849,#66850),(#66851,#66852,
#66853,#66854,#66855,#66856),(#66857,#66858,#66859,#66860,#66861,#66862),
(#66863,#66864,#66865,#66866,#66867,#66868),(#66869,#66870,#66871,#66872,
#66873,#66874),(#66875,#66876,#66877,#66878,#66879,#66880),(#66881,#66882,
#66883,#66884,#66885,#66886),(#66887,#66888,#66889,#66890,#66891,#66892),
(#66893,#66894,#66895,#66896,#66897,#66898)),.UNSPECIFIED.,.F.,.F.,.F.,
(6,3,3,3,6),(6,6),(5.18156607379,7.64878179687,11.6904556298,14.7384492068,
17.7593366521),(0.,0.3),.UNSPECIFIED.);
#1019=B_SPLINE_SURFACE_WITH_KNOTS('',5,1,((#66917,#66918),(#66919,#66920),
(#66921,#66922),(#66923,#66924),(#66925,#66926),(#66927,#66928),(#66929,
#66930),(#66931,#66932),(#66933,#66934),(#66935,#66936),(#66937,#66938),
(#66939,#66940),(#66941,#66942),(#66943,#66944),(#66945,#66946),(#66947,
#66948),(#66949,#66950),(#66951,#66952)),.UNSPECIFIED.,.F.,.F.,.F.,(6,3,
3,3,3,6),(2,2),(2.58143959,4.30538111878,6.90119302094,7.76515862896,9.48090785315,
11.1787837181),(0.,0.168000000000001),.UNSPECIFIED.);
#1020=B_SPLINE_SURFACE_WITH_KNOTS('',5,5,((#66953,#66954,#66955,#66956,
#66957,#66958),(#66959,#66960,#66961,#66962,#66963,#66964),(#66965,#66966,
#66967,#66968,#66969,#66970),(#66971,#66972,#66973,#66974,#66975,#66976),
(#66977,#66978,#66979,#66980,#66981,#66982),(#66983,#66984,#66985,#66986,
#66987,#66988),(#66989,#66990,#66991,#66992,#66993,#66994),(#66995,#66996,
#66997,#66998,#66999,#67000),(#67001,#67002,#67003,#67004,#67005,#67006),
(#67007,#67008,#67009,#67010,#67011,#67012),(#67013,#67014,#67015,#67016,
#67017,#67018),(#67019,#67020,#67021,#67022,#67023,#67024),(#67025,#67026,
#67027,#67028,#67029,#67030),(#67031,#67032,#67033,#67034,#67035,#67036),
(#67037,#67038,#67039,#67040,#67041,#67042)),.UNSPECIFIED.,.F.,.F.,.F.,
(6,3,3,3,6),(6,6),(3.85962234114,6.1874356314,8.16908321302,10.1785749125,
12.1808522654),(0.,0.3),.UNSPECIFIED.);
#1021=B_SPLINE_SURFACE_WITH_KNOTS('',5,5,((#67071,#67072,#67073,#67074,
#67075,#67076),(#67077,#67078,#67079,#67080,#67081,#67082),(#67083,#67084,
#67085,#67086,#67087,#67088),(#67089,#67090,#67091,#67092,#67093,#67094),
(#67095,#67096,#67097,#67098,#67099,#67100),(#67101,#67102,#67103,#67104,
#67105,#67106),(#67107,#67108,#67109,#67110,#67111,#67112),(#67113,#67114,
#67115,#67116,#67117,#67118),(#67119,#67120,#67121,#67122,#67123,#67124),
(#67125,#67126,#67127,#67128,#67129,#67130),(#67131,#67132,#67133,#67134,
#67135,#67136),(#67137,#67138,#67139,#67140,#67141,#67142)),
 .UNSPECIFIED.,.F.,.F.,.F.,(6,3,3,6),(6,6),(2.76827068394,6.61192064383,
8.76054366777,11.0890194561),(0.,0.3),.UNSPECIFIED.);
#1022=B_SPLINE_SURFACE_WITH_KNOTS('',5,1,((#67159,#67160),(#67161,#67162),
(#67163,#67164),(#67165,#67166),(#67167,#67168),(#67169,#67170),(#67171,
#67172),(#67173,#67174),(#67175,#67176),(#67177,#67178),(#67179,#67180),
(#67181,#67182),(#67183,#67184),(#67185,#67186),(#67187,#67188),(#67189,
#67190),(#67191,#67192),(#67193,#67194),(#67195,#67196),(#67197,#67198),
(#67199,#67200),(#67201,#67202),(#67203,#67204),(#67205,#67206)),
 .UNSPECIFIED.,.F.,.F.,.F.,(6,3,3,3,3,3,3,6),(2,2),(1.95166187923,3.61934338467,
4.18928894847,5.33583801997,5.90017131307,6.45658950203,6.99997050268,7.54076751178),
(0.,0.168000000000001),.UNSPECIFIED.);
#1023=B_SPLINE_SURFACE_WITH_KNOTS('',5,5,((#67209,#67210,#67211,#67212,
#67213,#67214),(#67215,#67216,#67217,#67218,#67219,#67220),(#67221,#67222,
#67223,#67224,#67225,#67226),(#67227,#67228,#67229,#67230,#67231,#67232),
(#67233,#67234,#67235,#67236,#67237,#67238),(#67239,#67240,#67241,#67242,
#67243,#67244),(#67245,#67246,#67247,#67248,#67249,#67250),(#67251,#67252,
#67253,#67254,#67255,#67256),(#67257,#67258,#67259,#67260,#67261,#67262)),
 .UNSPECIFIED.,.F.,.F.,.F.,(6,3,6),(6,6),(2.24719882413,4.51381221186,6.83969663211),
(0.,0.3),.UNSPECIFIED.);
#1024=B_SPLINE_SURFACE_WITH_KNOTS('',5,5,((#67317,#67318,#67319,#67320,
#67321,#67322),(#67323,#67324,#67325,#67326,#67327,#67328),(#67329,#67330,
#67331,#67332,#67333,#67334),(#67335,#67336,#67337,#67338,#67339,#67340),
(#67341,#67342,#67343,#67344,#67345,#67346),(#67347,#67348,#67349,#67350,
#67351,#67352),(#67353,#67354,#67355,#67356,#67357,#67358),(#67359,#67360,
#67361,#67362,#67363,#67364),(#67365,#67366,#67367,#67368,#67369,#67370)),
 .UNSPECIFIED.,.F.,.F.,.F.,(6,3,6),(6,6),(2.81287993679,5.11582036754,7.40337618611),
(0.,0.3),.UNSPECIFIED.);
#1025=B_SPLINE_SURFACE_WITH_KNOTS('',5,1,((#67382,#67383),(#67384,#67385),
(#67386,#67387),(#67388,#67389),(#67390,#67391),(#67392,#67393),(#67394,
#67395),(#67396,#67397),(#67398,#67399),(#67400,#67401),(#67402,#67403),
(#67404,#67405)),.UNSPECIFIED.,.F.,.F.,.F.,(6,3,3,6),(2,2),(1.13146961455,
2.10239516213,2.75440125835,4.36150381835),(0.,0.168000000000001),
 .UNSPECIFIED.);
#1026=B_SPLINE_SURFACE_WITH_KNOTS('',5,5,((#67407,#67408,#67409,#67410,
#67411,#67412),(#67413,#67414,#67415,#67416,#67417,#67418),(#67419,#67420,
#67421,#67422,#67423,#67424),(#67425,#67426,#67427,#67428,#67429,#67430),
(#67431,#67432,#67433,#67434,#67435,#67436),(#67437,#67438,#67439,#67440,
#67441,#67442),(#67443,#67444,#67445,#67446,#67447,#67448),(#67449,#67450,
#67451,#67452,#67453,#67454),(#67455,#67456,#67457,#67458,#67459,#67460),
(#67461,#67462,#67463,#67464,#67465,#67466),(#67467,#67468,#67469,#67470,
#67471,#67472),(#67473,#67474,#67475,#67476,#67477,#67478),(#67479,#67480,
#67481,#67482,#67483,#67484),(#67485,#67486,#67487,#67488,#67489,#67490),
(#67491,#67492,#67493,#67494,#67495,#67496),(#67497,#67498,#67499,#67500,
#67501,#67502),(#67503,#67504,#67505,#67506,#67507,#67508),(#67509,#67510,
#67511,#67512,#67513,#67514)),.UNSPECIFIED.,.F.,.F.,.F.,(6,3,3,3,3,6),(6,
6),(12.5665153092,21.1100928175,29.3112276523,33.9967363407,38.6616811225,
45.9550547113),(0.,0.3),.UNSPECIFIED.);
#1027=B_SPLINE_SURFACE_WITH_KNOTS('',5,5,((#67647,#67648,#67649,#67650,
#67651,#67652),(#67653,#67654,#67655,#67656,#67657,#67658),(#67659,#67660,
#67661,#67662,#67663,#67664),(#67665,#67666,#67667,#67668,#67669,#67670),
(#67671,#67672,#67673,#67674,#67675,#67676),(#67677,#67678,#67679,#67680,
#67681,#67682),(#67683,#67684,#67685,#67686,#67687,#67688),(#67689,#67690,
#67691,#67692,#67693,#67694),(#67695,#67696,#67697,#67698,#67699,#67700),
(#67701,#67702,#67703,#67704,#67705,#67706),(#67707,#67708,#67709,#67710,
#67711,#67712),(#67713,#67714,#67715,#67716,#67717,#67718),(#67719,#67720,
#67721,#67722,#67723,#67724),(#67725,#67726,#67727,#67728,#67729,#67730),
(#67731,#67732,#67733,#67734,#67735,#67736),(#67737,#67738,#67739,#67740,
#67741,#67742),(#67743,#67744,#67745,#67746,#67747,#67748),(#67749,#67750,
#67751,#67752,#67753,#67754)),.UNSPECIFIED.,.F.,.F.,.F.,(6,3,3,3,3,6),(6,
6),(16.6199171729,22.5384104949,30.5763255063,36.3852905632,40.8836098595,
50.0065304478),(0.,0.3),.UNSPECIFIED.);
#1028=B_SPLINE_SURFACE_WITH_KNOTS('',5,1,((#67775,#67776),(#67777,#67778),
(#67779,#67780),(#67781,#67782),(#67783,#67784),(#67785,#67786),(#67787,
#67788),(#67789,#67790),(#67791,#67792),(#67793,#67794),(#67795,#67796),
(#67797,#67798),(#67799,#67800),(#67801,#67802),(#67803,#67804),(#67805,
#67806),(#67807,#67808),(#67809,#67810),(#67811,#67812),(#67813,#67814),
(#67815,#67816),(#67817,#67818),(#67819,#67820),(#67821,#67822)),
 .UNSPECIFIED.,.F.,.F.,.F.,(6,3,3,3,3,3,3,6),(2,2),(5.81590786279,8.33607651362,
10.1951986769,12.0532651712,14.9345717632,19.4956760771,21.7667109588,28.5950255496),
(0.,0.168000000000001),.UNSPECIFIED.);
#1029=B_SPLINE_SURFACE_WITH_KNOTS('',5,5,((#67824,#67825,#67826,#67827,
#67828,#67829),(#67830,#67831,#67832,#67833,#67834,#67835),(#67836,#67837,
#67838,#67839,#67840,#67841),(#67842,#67843,#67844,#67845,#67846,#67847),
(#67848,#67849,#67850,#67851,#67852,#67853),(#67854,#67855,#67856,#67857,
#67858,#67859),(#67860,#67861,#67862,#67863,#67864,#67865),(#67866,#67867,
#67868,#67869,#67870,#67871),(#67872,#67873,#67874,#67875,#67876,#67877)),
 .UNSPECIFIED.,.F.,.F.,.F.,(6,3,6),(6,6),(0.168109267782,0.193813333781,
0.219517399779),(0.,0.3),.UNSPECIFIED.);
#1030=B_SPLINE_SURFACE_WITH_KNOTS('',5,5,((#67881,#67882,#67883,#67884,
#67885,#67886),(#67887,#67888,#67889,#67890,#67891,#67892),(#67893,#67894,
#67895,#67896,#67897,#67898),(#67899,#67900,#67901,#67902,#67903,#67904),
(#67905,#67906,#67907,#67908,#67909,#67910),(#67911,#67912,#67913,#67914,
#67915,#67916)),.UNSPECIFIED.,.F.,.F.,.F.,(6,6),(6,6),(0.167763693388,0.219167536337),
(0.,0.3),.UNSPECIFIED.);
#1031=B_SPLINE_SURFACE_WITH_KNOTS('',5,5,((#67922,#67923,#67924,#67925,
#67926,#67927),(#67928,#67929,#67930,#67931,#67932,#67933),(#67934,#67935,
#67936,#67937,#67938,#67939),(#67940,#67941,#67942,#67943,#67944,#67945),
(#67946,#67947,#67948,#67949,#67950,#67951),(#67952,#67953,#67954,#67955,
#67956,#67957),(#67958,#67959,#67960,#67961,#67962,#67963),(#67964,#67965,
#67966,#67967,#67968,#67969),(#67970,#67971,#67972,#67973,#67974,#67975)),
 .UNSPECIFIED.,.F.,.F.,.F.,(6,3,6),(6,6),(1.62532205434,2.95680207855,4.76574024567),
(0.,0.3),.UNSPECIFIED.);
#1032=B_SPLINE_SURFACE_WITH_KNOTS('',5,5,((#68014,#68015,#68016,#68017,
#68018,#68019),(#68020,#68021,#68022,#68023,#68024,#68025),(#68026,#68027,
#68028,#68029,#68030,#68031),(#68032,#68033,#68034,#68035,#68036,#68037),
(#68038,#68039,#68040,#68041,#68042,#68043),(#68044,#68045,#68046,#68047,
#68048,#68049),(#68050,#68051,#68052,#68053,#68054,#68055),(#68056,#68057,
#68058,#68059,#68060,#68061),(#68062,#68063,#68064,#68065,#68066,#68067)),
 .UNSPECIFIED.,.F.,.F.,.F.,(6,3,6),(6,6),(1.62047643556,3.23201205664,4.75541642643),
(0.,0.3),.UNSPECIFIED.);
#1033=B_SPLINE_SURFACE_WITH_KNOTS('',5,1,((#68106,#68107),(#68108,#68109),
(#68110,#68111),(#68112,#68113),(#68114,#68115),(#68116,#68117)),
 .UNSPECIFIED.,.F.,.F.,.F.,(6,6),(2,2),(1.41662542015,3.44037602036),(0.,
0.168000000000001),.UNSPECIFIED.);
#1034=B_SPLINE_SURFACE_WITH_KNOTS('',5,5,((#68129,#68130,#68131,#68132,
#68133,#68134),(#68135,#68136,#68137,#68138,#68139,#68140),(#68141,#68142,
#68143,#68144,#68145,#68146),(#68147,#68148,#68149,#68150,#68151,#68152),
(#68153,#68154,#68155,#68156,#68157,#68158),(#68159,#68160,#68161,#68162,
#68163,#68164),(#68165,#68166,#68167,#68168,#68169,#68170),(#68171,#68172,
#68173,#68174,#68175,#68176),(#68177,#68178,#68179,#68180,#68181,#68182)),
 .UNSPECIFIED.,.F.,.F.,.F.,(6,3,6),(6,6),(0.591274134056,1.32390942548,
1.88642149695),(0.,0.3),.UNSPECIFIED.);
#1035=B_SPLINE_SURFACE_WITH_KNOTS('',5,5,((#68191,#68192,#68193,#68194,
#68195,#68196),(#68197,#68198,#68199,#68200,#68201,#68202),(#68203,#68204,
#68205,#68206,#68207,#68208),(#68209,#68210,#68211,#68212,#68213,#68214),
(#68215,#68216,#68217,#68218,#68219,#68220),(#68221,#68222,#68223,#68224,
#68225,#68226),(#68227,#68228,#68229,#68230,#68231,#68232),(#68233,#68234,
#68235,#68236,#68237,#68238),(#68239,#68240,#68241,#68242,#68243,#68244)),
 .UNSPECIFIED.,.F.,.F.,.F.,(6,3,6),(6,6),(0.591155709264,1.24895127143,
1.8860355782),(0.,0.3),.UNSPECIFIED.);
#1036=B_SPLINE_SURFACE_WITH_KNOTS('',5,1,((#68256,#68257),(#68258,#68259),
(#68260,#68261),(#68262,#68263),(#68264,#68265),(#68266,#68267)),
 .UNSPECIFIED.,.F.,.F.,.F.,(6,6),(2,2),(0.493788369863,1.19920032681),(0.,
0.168000000000001),.UNSPECIFIED.);
#1037=B_SPLINE_SURFACE_WITH_KNOTS('',5,5,((#68269,#68270,#68271,#68272,
#68273,#68274),(#68275,#68276,#68277,#68278,#68279,#68280),(#68281,#68282,
#68283,#68284,#68285,#68286),(#68287,#68288,#68289,#68290,#68291,#68292),
(#68293,#68294,#68295,#68296,#68297,#68298),(#68299,#68300,#68301,#68302,
#68303,#68304),(#68305,#68306,#68307,#68308,#68309,#68310),(#68311,#68312,
#68313,#68314,#68315,#68316),(#68317,#68318,#68319,#68320,#68321,#68322)),
 .UNSPECIFIED.,.F.,.F.,.F.,(6,3,6),(6,6),(1.35769229991,2.30681875985,3.25594521979),
(0.,0.3),.UNSPECIFIED.);
#1038=B_SPLINE_SURFACE_WITH_KNOTS('',5,5,((#68326,#68327,#68328,#68329,
#68330,#68331),(#68332,#68333,#68334,#68335,#68336,#68337),(#68338,#68339,
#68340,#68341,#68342,#68343),(#68344,#68345,#68346,#68347,#68348,#68349),
(#68350,#68351,#68352,#68353,#68354,#68355),(#68356,#68357,#68358,#68359,
#68360,#68361),(#68362,#68363,#68364,#68365,#68366,#68367),(#68368,#68369,
#68370,#68371,#68372,#68373),(#68374,#68375,#68376,#68377,#68378,#68379)),
 .UNSPECIFIED.,.F.,.F.,.F.,(6,3,6),(6,6),(1.35799881012,2.30712712606,3.25625544201),
(0.,0.3),.UNSPECIFIED.);
#1039=B_SPLINE_SURFACE_WITH_KNOTS('',5,1,((#68383,#68384),(#68385,#68386),
(#68387,#68388),(#68389,#68390),(#68391,#68392),(#68393,#68394)),
 .UNSPECIFIED.,.F.,.F.,.F.,(6,6),(2,2),(0.96552770951,2.34485300881),(0.,
0.168000000000001),.UNSPECIFIED.);
#1040=B_SPLINE_SURFACE_WITH_KNOTS('',5,5,((#68396,#68397,#68398,#68399,
#68400,#68401),(#68402,#68403,#68404,#68405,#68406,#68407),(#68408,#68409,
#68410,#68411,#68412,#68413),(#68414,#68415,#68416,#68417,#68418,#68419),
(#68420,#68421,#68422,#68423,#68424,#68425),(#68426,#68427,#68428,#68429,
#68430,#68431),(#68432,#68433,#68434,#68435,#68436,#68437),(#68438,#68439,
#68440,#68441,#68442,#68443),(#68444,#68445,#68446,#68447,#68448,#68449),
(#68450,#68451,#68452,#68453,#68454,#68455),(#68456,#68457,#68458,#68459,
#68460,#68461),(#68462,#68463,#68464,#68465,#68466,#68467),(#68468,#68469,
#68470,#68471,#68472,#68473),(#68474,#68475,#68476,#68477,#68478,#68479),
(#68480,#68481,#68482,#68483,#68484,#68485),(#68486,#68487,#68488,#68489,
#68490,#68491),(#68492,#68493,#68494,#68495,#68496,#68497),(#68498,#68499,
#68500,#68501,#68502,#68503),(#68504,#68505,#68506,#68507,#68508,#68509),
(#68510,#68511,#68512,#68513,#68514,#68515),(#68516,#68517,#68518,#68519,
#68520,#68521)),.UNSPECIFIED.,.F.,.F.,.F.,(6,3,3,3,3,3,6),(6,6),(4.50366397293,
11.9396101613,13.7854271296,14.9414943029,15.6351526747,16.3253424406,17.7760995894),
(0.,0.3),.UNSPECIFIED.);
#1041=B_SPLINE_SURFACE_WITH_KNOTS('',5,5,((#68540,#68541,#68542,#68543,
#68544,#68545),(#68546,#68547,#68548,#68549,#68550,#68551),(#68552,#68553,
#68554,#68555,#68556,#68557),(#68558,#68559,#68560,#68561,#68562,#68563),
(#68564,#68565,#68566,#68567,#68568,#68569),(#68570,#68571,#68572,#68573,
#68574,#68575),(#68576,#68577,#68578,#68579,#68580,#68581),(#68582,#68583,
#68584,#68585,#68586,#68587),(#68588,#68589,#68590,#68591,#68592,#68593),
(#68594,#68595,#68596,#68597,#68598,#68599),(#68600,#68601,#68602,#68603,
#68604,#68605),(#68606,#68607,#68608,#68609,#68610,#68611),(#68612,#68613,
#68614,#68615,#68616,#68617),(#68618,#68619,#68620,#68621,#68622,#68623),
(#68624,#68625,#68626,#68627,#68628,#68629),(#68630,#68631,#68632,#68633,
#68634,#68635),(#68636,#68637,#68638,#68639,#68640,#68641),(#68642,#68643,
#68644,#68645,#68646,#68647),(#68648,#68649,#68650,#68651,#68652,#68653),
(#68654,#68655,#68656,#68657,#68658,#68659),(#68660,#68661,#68662,#68663,
#68664,#68665)),.UNSPECIFIED.,.F.,.F.,.F.,(6,3,3,3,3,3,6),(6,6),(4.57396017214,
5.92885717573,7.41888220249,8.65504128479,9.89120036709,11.8754981945,17.8472140382),
(0.,0.3),.UNSPECIFIED.);
#1042=B_SPLINE_SURFACE_WITH_KNOTS('',5,1,((#68687,#68688),(#68689,#68690),
(#68691,#68692),(#68693,#68694),(#68695,#68696),(#68697,#68698),(#68699,
#68700),(#68701,#68702),(#68703,#68704),(#68705,#68706),(#68707,#68708),
(#68709,#68710),(#68711,#68712),(#68713,#68714),(#68715,#68716),(#68717,
#68718),(#68719,#68720),(#68721,#68722)),.UNSPECIFIED.,.F.,.F.,.F.,(6,3,
3,3,3,6),(2,2),(2.29196781189,3.18681436572,5.94671679294,9.63664271035,
10.6008983863,11.5146904868),(0.,0.168000000000001),.UNSPECIFIED.);
#1043=B_SPLINE_SURFACE_WITH_KNOTS('',5,5,((#68723,#68724,#68725,#68726,
#68727,#68728),(#68729,#68730,#68731,#68732,#68733,#68734),(#68735,#68736,
#68737,#68738,#68739,#68740),(#68741,#68742,#68743,#68744,#68745,#68746),
(#68747,#68748,#68749,#68750,#68751,#68752),(#68753,#68754,#68755,#68756,
#68757,#68758),(#68759,#68760,#68761,#68762,#68763,#68764),(#68765,#68766,
#68767,#68768,#68769,#68770),(#68771,#68772,#68773,#68774,#68775,#68776),
(#68777,#68778,#68779,#68780,#68781,#68782),(#68783,#68784,#68785,#68786,
#68787,#68788),(#68789,#68790,#68791,#68792,#68793,#68794)),
 .UNSPECIFIED.,.F.,.F.,.F.,(6,3,3,6),(6,6),(3.96957835788,8.52280966994,
10.8013830785,13.2112648606),(0.,0.3),.UNSPECIFIED.);
#1044=B_SPLINE_SURFACE_WITH_KNOTS('',5,5,((#68811,#68812,#68813,#68814,
#68815,#68816),(#68817,#68818,#68819,#68820,#68821,#68822),(#68823,#68824,
#68825,#68826,#68827,#68828),(#68829,#68830,#68831,#68832,#68833,#68834),
(#68835,#68836,#68837,#68838,#68839,#68840),(#68841,#68842,#68843,#68844,
#68845,#68846),(#68847,#68848,#68849,#68850,#68851,#68852),(#68853,#68854,
#68855,#68856,#68857,#68858),(#68859,#68860,#68861,#68862,#68863,#68864),
(#68865,#68866,#68867,#68868,#68869,#68870),(#68871,#68872,#68873,#68874,
#68875,#68876),(#68877,#68878,#68879,#68880,#68881,#68882)),
 .UNSPECIFIED.,.F.,.F.,.F.,(6,3,3,6),(6,6),(3.98723768815,6.53884477084,
8.77115009928,13.2289036984),(0.,0.3),.UNSPECIFIED.);
#1045=B_SPLINE_SURFACE_WITH_KNOTS('',5,1,((#68908,#68909),(#68910,#68911),
(#68912,#68913),(#68914,#68915),(#68916,#68917),(#68918,#68919),(#68920,
#68921),(#68922,#68923),(#68924,#68925),(#68926,#68927),(#68928,#68929),
(#68930,#68931),(#68932,#68933),(#68934,#68935),(#68936,#68937),(#68938,
#68939),(#68940,#68941),(#68942,#68943),(#68944,#68945),(#68946,#68947),
(#68948,#68949)),.UNSPECIFIED.,.F.,.F.,.F.,(6,3,3,3,3,3,6),(2,2),(1.95811472427,
3.23566574513,3.88589710876,5.21424414623,6.55599923652,7.22663415565,8.5548107935),
(0.,0.168000000000001),.UNSPECIFIED.);
#1046=B_SPLINE_SURFACE_WITH_KNOTS('',5,5,((#68952,#68953,#68954,#68955,
#68956,#68957),(#68958,#68959,#68960,#68961,#68962,#68963),(#68964,#68965,
#68966,#68967,#68968,#68969),(#68970,#68971,#68972,#68973,#68974,#68975),
(#68976,#68977,#68978,#68979,#68980,#68981),(#68982,#68983,#68984,#68985,
#68986,#68987),(#68988,#68989,#68990,#68991,#68992,#68993),(#68994,#68995,
#68996,#68997,#68998,#68999),(#69000,#69001,#69002,#69003,#69004,#69005)),
 .UNSPECIFIED.,.F.,.F.,.F.,(6,3,6),(6,6),(0.620886007027,1.29421436741,
2.17771162296),(0.,0.3),.UNSPECIFIED.);
#1047=B_SPLINE_SURFACE_WITH_KNOTS('',5,5,((#69014,#69015,#69016,#69017,
#69018,#69019),(#69020,#69021,#69022,#69023,#69024,#69025),(#69026,#69027,
#69028,#69029,#69030,#69031),(#69032,#69033,#69034,#69035,#69036,#69037),
(#69038,#69039,#69040,#69041,#69042,#69043),(#69044,#69045,#69046,#69047,
#69048,#69049),(#69050,#69051,#69052,#69053,#69054,#69055),(#69056,#69057,
#69058,#69059,#69060,#69061),(#69062,#69063,#69064,#69065,#69066,#69067)),
 .UNSPECIFIED.,.F.,.F.,.F.,(6,3,6),(6,6),(0.620875478398,1.40616268126,
2.17764450768),(0.,0.3),.UNSPECIFIED.);
#1048=B_SPLINE_SURFACE_WITH_KNOTS('',5,1,((#69113,#69114),(#69115,#69116),
(#69117,#69118),(#69119,#69120),(#69121,#69122),(#69123,#69124)),
 .UNSPECIFIED.,.F.,.F.,.F.,(6,6),(2,2),(0.52702168644,1.27990980993),(0.,
0.168000000000001),.UNSPECIFIED.);
#1049=B_SPLINE_SURFACE_WITH_KNOTS('',5,5,((#69126,#69127,#69128,#69129,
#69130,#69131),(#69132,#69133,#69134,#69135,#69136,#69137),(#69138,#69139,
#69140,#69141,#69142,#69143),(#69144,#69145,#69146,#69147,#69148,#69149),
(#69150,#69151,#69152,#69153,#69154,#69155),(#69156,#69157,#69158,#69159,
#69160,#69161),(#69162,#69163,#69164,#69165,#69166,#69167),(#69168,#69169,
#69170,#69171,#69172,#69173),(#69174,#69175,#69176,#69177,#69178,#69179)),
 .UNSPECIFIED.,.F.,.F.,.F.,(6,3,6),(6,6),(8.8689446919,17.3139944292,23.7989023215),
(0.,0.3),.UNSPECIFIED.);
#1050=B_SPLINE_SURFACE_WITH_KNOTS('',5,5,((#69191,#69192,#69193,#69194,
#69195,#69196),(#69197,#69198,#69199,#69200,#69201,#69202),(#69203,#69204,
#69205,#69206,#69207,#69208),(#69209,#69210,#69211,#69212,#69213,#69214),
(#69215,#69216,#69217,#69218,#69219,#69220),(#69221,#69222,#69223,#69224,
#69225,#69226),(#69227,#69228,#69229,#69230,#69231,#69232),(#69233,#69234,
#69235,#69236,#69237,#69238),(#69239,#69240,#69241,#69242,#69243,#69244)),
 .UNSPECIFIED.,.F.,.F.,.F.,(6,3,6),(6,6),(8.86843301073,15.565351162,23.7990765439),
(0.,0.3),.UNSPECIFIED.);
#1051=B_SPLINE_SURFACE_WITH_KNOTS('',5,1,((#69253,#69254),(#69255,#69256),
(#69257,#69258),(#69259,#69260),(#69261,#69262),(#69263,#69264)),
 .UNSPECIFIED.,.F.,.F.,.F.,(6,6),(2,2),(7.91037074022,19.2109003691),(0.,
0.168000000000001),.UNSPECIFIED.);
#1052=B_SPLINE_SURFACE_WITH_KNOTS('',5,5,((#69266,#69267,#69268,#69269,
#69270,#69271),(#69272,#69273,#69274,#69275,#69276,#69277),(#69278,#69279,
#69280,#69281,#69282,#69283),(#69284,#69285,#69286,#69287,#69288,#69289),
(#69290,#69291,#69292,#69293,#69294,#69295),(#69296,#69297,#69298,#69299,
#69300,#69301),(#69302,#69303,#69304,#69305,#69306,#69307),(#69308,#69309,
#69310,#69311,#69312,#69313),(#69314,#69315,#69316,#69317,#69318,#69319)),
 .UNSPECIFIED.,.F.,.F.,.F.,(6,3,6),(6,6),(8.86873667877,17.3137864161,23.7986943084),
(0.,0.3),.UNSPECIFIED.);
#1053=B_SPLINE_SURFACE_WITH_KNOTS('',5,5,((#69331,#69332,#69333,#69334,
#69335,#69336),(#69337,#69338,#69339,#69340,#69341,#69342),(#69343,#69344,
#69345,#69346,#69347,#69348),(#69349,#69350,#69351,#69352,#69353,#69354),
(#69355,#69356,#69357,#69358,#69359,#69360),(#69361,#69362,#69363,#69364,
#69365,#69366),(#69367,#69368,#69369,#69370,#69371,#69372),(#69373,#69374,
#69375,#69376,#69377,#69378),(#69379,#69380,#69381,#69382,#69383,#69384)),
 .UNSPECIFIED.,.F.,.F.,.F.,(6,3,6),(6,6),(8.86829015303,15.5652083044,23.7989336863),
(0.,0.3),.UNSPECIFIED.);
#1054=B_SPLINE_SURFACE_WITH_KNOTS('',5,1,((#69393,#69394),(#69395,#69396),
(#69397,#69398),(#69399,#69400),(#69401,#69402),(#69403,#69404)),
 .UNSPECIFIED.,.F.,.F.,.F.,(6,6),(2,2),(7.91037074022,19.2109003691),(0.,
0.168000000000001),.UNSPECIFIED.);
#1055=B_SPLINE_SURFACE_WITH_KNOTS('',5,5,((#69406,#69407,#69408,#69409,
#69410,#69411),(#69412,#69413,#69414,#69415,#69416,#69417),(#69418,#69419,
#69420,#69421,#69422,#69423),(#69424,#69425,#69426,#69427,#69428,#69429),
(#69430,#69431,#69432,#69433,#69434,#69435),(#69436,#69437,#69438,#69439,
#69440,#69441),(#69442,#69443,#69444,#69445,#69446,#69447),(#69448,#69449,
#69450,#69451,#69452,#69453),(#69454,#69455,#69456,#69457,#69458,#69459)),
 .UNSPECIFIED.,.F.,.F.,.F.,(6,3,6),(6,6),(0.620884089829,1.29421245021,
2.17770970576),(0.,0.3),.UNSPECIFIED.);
#1056=B_SPLINE_SURFACE_WITH_KNOTS('',5,5,((#69468,#69469,#69470,#69471,
#69472,#69473),(#69474,#69475,#69476,#69477,#69478,#69479),(#69480,#69481,
#69482,#69483,#69484,#69485),(#69486,#69487,#69488,#69489,#69490,#69491),
(#69492,#69493,#69494,#69495,#69496,#69497),(#69498,#69499,#69500,#69501,
#69502,#69503),(#69504,#69505,#69506,#69507,#69508,#69509),(#69510,#69511,
#69512,#69513,#69514,#69515),(#69516,#69517,#69518,#69519,#69520,#69521)),
 .UNSPECIFIED.,.F.,.F.,.F.,(6,3,6),(6,6),(0.620866600281,1.40615380315,
2.1776356295),(0.,0.3),.UNSPECIFIED.);
#1057=B_SPLINE_SURFACE_WITH_KNOTS('',5,1,((#69567,#69568),(#69569,#69570),
(#69571,#69572),(#69573,#69574),(#69575,#69576),(#69577,#69578)),
 .UNSPECIFIED.,.F.,.F.,.F.,(6,6),(2,2),(0.52702168644,1.27990980993),(0.,
0.168000000000001),.UNSPECIFIED.);
#1058=B_SPLINE_SURFACE_WITH_KNOTS('',5,5,((#69580,#69581,#69582,#69583,
#69584,#69585),(#69586,#69587,#69588,#69589,#69590,#69591),(#69592,#69593,
#69594,#69595,#69596,#69597),(#69598,#69599,#69600,#69601,#69602,#69603),
(#69604,#69605,#69606,#69607,#69608,#69609),(#69610,#69611,#69612,#69613,
#69614,#69615),(#69616,#69617,#69618,#69619,#69620,#69621),(#69622,#69623,
#69624,#69625,#69626,#69627),(#69628,#69629,#69630,#69631,#69632,#69633),
(#69634,#69635,#69636,#69637,#69638,#69639),(#69640,#69641,#69642,#69643,
#69644,#69645),(#69646,#69647,#69648,#69649,#69650,#69651)),
 .UNSPECIFIED.,.F.,.F.,.F.,(6,3,3,6),(6,6),(3.98757792105,6.5613910649,
8.51083290938,13.2292989355),(0.,0.3),.UNSPECIFIED.);
#1059=B_SPLINE_SURFACE_WITH_KNOTS('',5,5,((#69675,#69676,#69677,#69678,
#69679,#69680),(#69681,#69682,#69683,#69684,#69685,#69686),(#69687,#69688,
#69689,#69690,#69691,#69692),(#69693,#69694,#69695,#69696,#69697,#69698),
(#69699,#69700,#69701,#69702,#69703,#69704),(#69705,#69706,#69707,#69708,
#69709,#69710),(#69711,#69712,#69713,#69714,#69715,#69716),(#69717,#69718,
#69719,#69720,#69721,#69722),(#69723,#69724,#69725,#69726,#69727,#69728),
(#69729,#69730,#69731,#69732,#69733,#69734),(#69735,#69736,#69737,#69738,
#69739,#69740),(#69741,#69742,#69743,#69744,#69745,#69746)),
 .UNSPECIFIED.,.F.,.F.,.F.,(6,3,3,6),(6,6),(3.96959709723,8.41545051994,
10.641451928,13.2113291298),(0.,0.3),.UNSPECIFIED.);
#1060=B_SPLINE_SURFACE_WITH_KNOTS('',5,1,((#69770,#69771),(#69772,#69773),
(#69774,#69775),(#69776,#69777),(#69778,#69779),(#69780,#69781),(#69782,
#69783),(#69784,#69785),(#69786,#69787),(#69788,#69789),(#69790,#69791),
(#69792,#69793),(#69794,#69795),(#69796,#69797),(#69798,#69799),(#69800,
#69801),(#69802,#69803),(#69804,#69805),(#69806,#69807),(#69808,#69809),
(#69810,#69811)),.UNSPECIFIED.,.F.,.F.,.F.,(6,3,3,3,3,3,6),(2,2),(1.98342753277,
3.31160417062,3.98223908975,5.32399418003,6.6523412175,7.30257258114,8.58012360199),
(0.,0.168000000000001),.UNSPECIFIED.);
#1061=B_SPLINE_SURFACE_WITH_KNOTS('',5,5,((#69813,#69814,#69815,#69816,
#69817,#69818),(#69819,#69820,#69821,#69822,#69823,#69824),(#69825,#69826,
#69827,#69828,#69829,#69830),(#69831,#69832,#69833,#69834,#69835,#69836),
(#69837,#69838,#69839,#69840,#69841,#69842),(#69843,#69844,#69845,#69846,
#69847,#69848),(#69849,#69850,#69851,#69852,#69853,#69854),(#69855,#69856,
#69857,#69858,#69859,#69860),(#69861,#69862,#69863,#69864,#69865,#69866),
(#69867,#69868,#69869,#69870,#69871,#69872),(#69873,#69874,#69875,#69876,
#69877,#69878),(#69879,#69880,#69881,#69882,#69883,#69884),(#69885,#69886,
#69887,#69888,#69889,#69890),(#69891,#69892,#69893,#69894,#69895,#69896),
(#69897,#69898,#69899,#69900,#69901,#69902)),.UNSPECIFIED.,.F.,.F.,.F.,
(6,3,3,3,6),(6,6),(1.97579103232,2.74141165766,3.51110670868,5.05016737922,
7.48619339243),(0.,0.3),.UNSPECIFIED.);
#1062=B_SPLINE_SURFACE_WITH_KNOTS('',5,5,((#69920,#69921,#69922,#69923,
#69924,#69925),(#69926,#69927,#69928,#69929,#69930,#69931),(#69932,#69933,
#69934,#69935,#69936,#69937),(#69938,#69939,#69940,#69941,#69942,#69943),
(#69944,#69945,#69946,#69947,#69948,#69949),(#69950,#69951,#69952,#69953,
#69954,#69955),(#69956,#69957,#69958,#69959,#69960,#69961),(#69962,#69963,
#69964,#69965,#69966,#69967),(#69968,#69969,#69970,#69971,#69972,#69973),
(#69974,#69975,#69976,#69977,#69978,#69979),(#69980,#69981,#69982,#69983,
#69984,#69985),(#69986,#69987,#69988,#69989,#69990,#69991),(#69992,#69993,
#69994,#69995,#69996,#69997),(#69998,#69999,#70000,#70001,#70002,#70003),
(#70004,#70005,#70006,#70007,#70008,#70009)),.UNSPECIFIED.,.F.,.F.,.F.,
(6,3,3,3,6),(6,6),(2.79838908821,5.60075527683,6.50571033408,7.18248685409,
8.30480917216),(0.,0.3),.UNSPECIFIED.);
#1063=B_SPLINE_SURFACE_WITH_KNOTS('',5,1,((#70103,#70104),(#70105,#70106),
(#70107,#70108),(#70109,#70110),(#70111,#70112),(#70113,#70114),(#70115,
#70116),(#70117,#70118),(#70119,#70120),(#70121,#70122),(#70123,#70124),
(#70125,#70126),(#70127,#70128),(#70129,#70130),(#70131,#70132)),
 .UNSPECIFIED.,.F.,.F.,.F.,(6,3,3,3,6),(2,2),(1.35736905211,2.5282953222,
3.70557211292,4.48067762876,5.21689863741),(0.,0.168000000000001),
 .UNSPECIFIED.);
#1064=B_SPLINE_SURFACE_WITH_KNOTS('',5,5,((#70134,#70135,#70136,#70137,
#70138,#70139),(#70140,#70141,#70142,#70143,#70144,#70145),(#70146,#70147,
#70148,#70149,#70150,#70151),(#70152,#70153,#70154,#70155,#70156,#70157),
(#70158,#70159,#70160,#70161,#70162,#70163),(#70164,#70165,#70166,#70167,
#70168,#70169),(#70170,#70171,#70172,#70173,#70174,#70175),(#70176,#70177,
#70178,#70179,#70180,#70181),(#70182,#70183,#70184,#70185,#70186,#70187),
(#70188,#70189,#70190,#70191,#70192,#70193),(#70194,#70195,#70196,#70197,
#70198,#70199),(#70200,#70201,#70202,#70203,#70204,#70205),(#70206,#70207,
#70208,#70209,#70210,#70211),(#70212,#70213,#70214,#70215,#70216,#70217),
(#70218,#70219,#70220,#70221,#70222,#70223),(#70224,#70225,#70226,#70227,
#70228,#70229),(#70230,#70231,#70232,#70233,#70234,#70235),(#70236,#70237,
#70238,#70239,#70240,#70241),(#70242,#70243,#70244,#70245,#70246,#70247),
(#70248,#70249,#70250,#70251,#70252,#70253),(#70254,#70255,#70256,#70257,
#70258,#70259),(#70260,#70261,#70262,#70263,#70264,#70265),(#70266,#70267,
#70268,#70269,#70270,#70271),(#70272,#70273,#70274,#70275,#70276,#70277),
(#70278,#70279,#70280,#70281,#70282,#70283),(#70284,#70285,#70286,#70287,
#70288,#70289),(#70290,#70291,#70292,#70293,#70294,#70295),(#70296,#70297,
#70298,#70299,#70300,#70301),(#70302,#70303,#70304,#70305,#70306,#70307),
(#70308,#70309,#70310,#70311,#70312,#70313)),.UNSPECIFIED.,.F.,.F.,.F.,
(6,3,3,3,3,3,3,3,3,6),(6,6),(13.0484209298,14.3771824271,15.7058202332,
19.4329797586,22.2257607493,27.8279202183,33.4574539385,41.6679674559,47.6452295392,
53.2420797137),(0.,0.3),.UNSPECIFIED.);
#1065=B_SPLINE_SURFACE_WITH_KNOTS('',5,5,((#70355,#70356,#70357,#70358,
#70359,#70360),(#70361,#70362,#70363,#70364,#70365,#70366),(#70367,#70368,
#70369,#70370,#70371,#70372),(#70373,#70374,#70375,#70376,#70377,#70378),
(#70379,#70380,#70381,#70382,#70383,#70384),(#70385,#70386,#70387,#70388,
#70389,#70390),(#70391,#70392,#70393,#70394,#70395,#70396),(#70397,#70398,
#70399,#70400,#70401,#70402),(#70403,#70404,#70405,#70406,#70407,#70408),
(#70409,#70410,#70411,#70412,#70413,#70414),(#70415,#70416,#70417,#70418,
#70419,#70420),(#70421,#70422,#70423,#70424,#70425,#70426),(#70427,#70428,
#70429,#70430,#70431,#70432),(#70433,#70434,#70435,#70436,#70437,#70438),
(#70439,#70440,#70441,#70442,#70443,#70444),(#70445,#70446,#70447,#70448,
#70449,#70450),(#70451,#70452,#70453,#70454,#70455,#70456),(#70457,#70458,
#70459,#70460,#70461,#70462),(#70463,#70464,#70465,#70466,#70467,#70468),
(#70469,#70470,#70471,#70472,#70473,#70474),(#70475,#70476,#70477,#70478,
#70479,#70480),(#70481,#70482,#70483,#70484,#70485,#70486),(#70487,#70488,
#70489,#70490,#70491,#70492),(#70493,#70494,#70495,#70496,#70497,#70498),
(#70499,#70500,#70501,#70502,#70503,#70504),(#70505,#70506,#70507,#70508,
#70509,#70510),(#70511,#70512,#70513,#70514,#70515,#70516),(#70517,#70518,
#70519,#70520,#70521,#70522),(#70523,#70524,#70525,#70526,#70527,#70528),
(#70529,#70530,#70531,#70532,#70533,#70534)),.UNSPECIFIED.,.F.,.F.,.F.,
(6,3,3,3,3,3,3,3,3,6),(6,6),(13.30850513,22.9473682995,26.1445609307,32.8906058289,
38.6549810462,44.3241190945,47.1169000853,50.8440596107,52.1726974168,53.5008998895),
(0.,0.3),.UNSPECIFIED.);
#1066=B_SPLINE_SURFACE_WITH_KNOTS('',5,1,((#70576,#70577),(#70578,#70579),
(#70580,#70581),(#70582,#70583),(#70584,#70585),(#70586,#70587),(#70588,
#70589),(#70590,#70591),(#70592,#70593),(#70594,#70595),(#70596,#70597),
(#70598,#70599),(#70600,#70601),(#70602,#70603),(#70604,#70605),(#70606,
#70607),(#70608,#70609),(#70610,#70611),(#70612,#70613),(#70614,#70615),
(#70616,#70617),(#70618,#70619),(#70620,#70621),(#70622,#70623),(#70624,
#70625),(#70626,#70627),(#70628,#70629),(#70630,#70631),(#70632,#70633),
(#70634,#70635),(#70636,#70637),(#70638,#70639),(#70640,#70641),(#70642,
#70643),(#70644,#70645),(#70646,#70647),(#70648,#70649),(#70650,#70651),
(#70652,#70653)),.UNSPECIFIED.,.F.,.F.,.F.,(6,3,3,3,3,3,3,3,3,3,3,3,6),
(2,2),(5.58814360433,6.30725257391,8.49590865562,13.7853920845,17.0993514659,
21.0213468886,22.3238009285,24.9287160587,27.5338438134,29.43694187,30.0730233774,
30.7075742798,31.7310892021),(0.,0.168000000000001),.UNSPECIFIED.);
#1067=B_SPLINE_SURFACE_WITH_KNOTS('',5,5,((#70655,#70656,#70657,#70658,
#70659,#70660),(#70661,#70662,#70663,#70664,#70665,#70666),(#70667,#70668,
#70669,#70670,#70671,#70672),(#70673,#70674,#70675,#70676,#70677,#70678),
(#70679,#70680,#70681,#70682,#70683,#70684),(#70685,#70686,#70687,#70688,
#70689,#70690),(#70691,#70692,#70693,#70694,#70695,#70696),(#70697,#70698,
#70699,#70700,#70701,#70702),(#70703,#70704,#70705,#70706,#70707,#70708)),
 .UNSPECIFIED.,.F.,.F.,.F.,(6,3,6),(6,6),(2.27369288769,4.21221438122,6.15073587476),
(0.,0.3),.UNSPECIFIED.);
#1068=B_SPLINE_SURFACE_WITH_KNOTS('',5,5,((#70712,#70713,#70714,#70715,
#70716,#70717),(#70718,#70719,#70720,#70721,#70722,#70723),(#70724,#70725,
#70726,#70727,#70728,#70729),(#70730,#70731,#70732,#70733,#70734,#70735),
(#70736,#70737,#70738,#70739,#70740,#70741),(#70742,#70743,#70744,#70745,
#70746,#70747),(#70748,#70749,#70750,#70751,#70752,#70753),(#70754,#70755,
#70756,#70757,#70758,#70759),(#70760,#70761,#70762,#70763,#70764,#70765)),
 .UNSPECIFIED.,.F.,.F.,.F.,(6,3,6),(6,6),(2.27401419165,4.2125468931,6.15107959455),
(0.,0.3),.UNSPECIFIED.);
#1069=B_SPLINE_SURFACE_WITH_KNOTS('',5,1,((#70769,#70770),(#70771,#70772),
(#70773,#70774),(#70775,#70776),(#70777,#70778),(#70779,#70780)),
 .UNSPECIFIED.,.F.,.F.,.F.,(6,6),(2,2),(1.9503302649,4.73651635762),(0.,
0.168000000000001),.UNSPECIFIED.);
#1070=B_SPLINE_SURFACE_WITH_KNOTS('',5,5,((#70782,#70783,#70784,#70785,
#70786,#70787),(#70788,#70789,#70790,#70791,#70792,#70793),(#70794,#70795,
#70796,#70797,#70798,#70799),(#70800,#70801,#70802,#70803,#70804,#70805),
(#70806,#70807,#70808,#70809,#70810,#70811),(#70812,#70813,#70814,#70815,
#70816,#70817),(#70818,#70819,#70820,#70821,#70822,#70823),(#70824,#70825,
#70826,#70827,#70828,#70829),(#70830,#70831,#70832,#70833,#70834,#70835),
(#70836,#70837,#70838,#70839,#70840,#70841),(#70842,#70843,#70844,#70845,
#70846,#70847),(#70848,#70849,#70850,#70851,#70852,#70853),(#70854,#70855,
#70856,#70857,#70858,#70859),(#70860,#70861,#70862,#70863,#70864,#70865),
(#70866,#70867,#70868,#70869,#70870,#70871),(#70872,#70873,#70874,#70875,
#70876,#70877),(#70878,#70879,#70880,#70881,#70882,#70883),(#70884,#70885,
#70886,#70887,#70888,#70889),(#70890,#70891,#70892,#70893,#70894,#70895),
(#70896,#70897,#70898,#70899,#70900,#70901),(#70902,#70903,#70904,#70905,
#70906,#70907),(#70908,#70909,#70910,#70911,#70912,#70913),(#70914,#70915,
#70916,#70917,#70918,#70919),(#70920,#70921,#70922,#70923,#70924,#70925),
(#70926,#70927,#70928,#70929,#70930,#70931),(#70932,#70933,#70934,#70935,
#70936,#70937),(#70938,#70939,#70940,#70941,#70942,#70943),(#70944,#70945,
#70946,#70947,#70948,#70949),(#70950,#70951,#70952,#70953,#70954,#70955),
(#70956,#70957,#70958,#70959,#70960,#70961)),.UNSPECIFIED.,.F.,.F.,.F.,
(6,3,3,3,3,3,3,3,3,6),(6,6),(13.309352184,22.6115369711,27.6548280379,33.4130337529,
39.0575237739,44.6786014526,47.4881463874,50.2976913221,51.8585343078,53.4991626515),
(0.,0.3),.UNSPECIFIED.);
#1071=B_SPLINE_SURFACE_WITH_KNOTS('',5,5,((#71003,#71004,#71005,#71006,
#71007,#71008),(#71009,#71010,#71011,#71012,#71013,#71014),(#71015,#71016,
#71017,#71018,#71019,#71020),(#71021,#71022,#71023,#71024,#71025,#71026),
(#71027,#71028,#71029,#71030,#71031,#71032),(#71033,#71034,#71035,#71036,
#71037,#71038),(#71039,#71040,#71041,#71042,#71043,#71044),(#71045,#71046,
#71047,#71048,#71049,#71050),(#71051,#71052,#71053,#71054,#71055,#71056),
(#71057,#71058,#71059,#71060,#71061,#71062),(#71063,#71064,#71065,#71066,
#71067,#71068),(#71069,#71070,#71071,#71072,#71073,#71074),(#71075,#71076,
#71077,#71078,#71079,#71080),(#71081,#71082,#71083,#71084,#71085,#71086),
(#71087,#71088,#71089,#71090,#71091,#71092),(#71093,#71094,#71095,#71096,
#71097,#71098),(#71099,#71100,#71101,#71102,#71103,#71104),(#71105,#71106,
#71107,#71108,#71109,#71110),(#71111,#71112,#71113,#71114,#71115,#71116),
(#71117,#71118,#71119,#71120,#71121,#71122),(#71123,#71124,#71125,#71126,
#71127,#71128),(#71129,#71130,#71131,#71132,#71133,#71134),(#71135,#71136,
#71137,#71138,#71139,#71140),(#71141,#71142,#71143,#71144,#71145,#71146),
(#71147,#71148,#71149,#71150,#71151,#71152),(#71153,#71154,#71155,#71156,
#71157,#71158),(#71159,#71160,#71161,#71162,#71163,#71164)),
 .UNSPECIFIED.,.F.,.F.,.F.,(6,3,3,3,3,3,3,3,6),(6,6),(13.1529830415,14.6756170516,
15.9546703779,18.8316459182,24.5861173859,33.242662653,37.0047521746,43.9231881457,
53.3460404053),(0.,0.3),.UNSPECIFIED.);
#1072=B_SPLINE_SURFACE_WITH_KNOTS('',5,1,((#71372,#71373),(#71374,#71375),
(#71376,#71377),(#71378,#71379),(#71380,#71381),(#71382,#71383),(#71384,
#71385),(#71386,#71387),(#71388,#71389),(#71390,#71391),(#71392,#71393),
(#71394,#71395),(#71396,#71397),(#71398,#71399),(#71400,#71401),(#71402,
#71403),(#71404,#71405),(#71406,#71407),(#71408,#71409),(#71410,#71411),
(#71412,#71413),(#71414,#71415),(#71416,#71417),(#71418,#71419),(#71420,
#71421),(#71422,#71423),(#71424,#71425),(#71426,#71427),(#71428,#71429),
(#71430,#71431),(#71432,#71433),(#71434,#71435),(#71436,#71437),(#71438,
#71439),(#71440,#71441),(#71442,#71443),(#71444,#71445),(#71446,#71447),
(#71448,#71449)),.UNSPECIFIED.,.F.,.F.,.F.,(6,3,3,3,3,3,3,3,3,3,3,3,6),
(2,2),(5.7403465807,6.76386150304,7.39841240531,8.03449391269,9.9375919693,
12.5427197241,15.1476348542,16.4500888941,20.3720843168,23.6860436982,28.9755271271,
31.1641832088,31.8832921784),(0.,0.168000000000001),.UNSPECIFIED.);
#1073=B_SPLINE_SURFACE_WITH_KNOTS('',5,5,((#71451,#71452,#71453,#71454,
#71455,#71456),(#71457,#71458,#71459,#71460,#71461,#71462),(#71463,#71464,
#71465,#71466,#71467,#71468),(#71469,#71470,#71471,#71472,#71473,#71474),
(#71475,#71476,#71477,#71478,#71479,#71480),(#71481,#71482,#71483,#71484,
#71485,#71486),(#71487,#71488,#71489,#71490,#71491,#71492),(#71493,#71494,
#71495,#71496,#71497,#71498),(#71499,#71500,#71501,#71502,#71503,#71504),
(#71505,#71506,#71507,#71508,#71509,#71510),(#71511,#71512,#71513,#71514,
#71515,#71516),(#71517,#71518,#71519,#71520,#71521,#71522),(#71523,#71524,
#71525,#71526,#71527,#71528),(#71529,#71530,#71531,#71532,#71533,#71534),
(#71535,#71536,#71537,#71538,#71539,#71540)),.UNSPECIFIED.,.F.,.F.,.F.,
(6,3,3,3,6),(6,6),(2.79870510475,4.34415602331,5.89253492006,7.24045509522,
8.30631830913),(0.,0.3),.UNSPECIFIED.);
#1074=B_SPLINE_SURFACE_WITH_KNOTS('',5,5,((#71556,#71557,#71558,#71559,
#71560,#71561),(#71562,#71563,#71564,#71565,#71566,#71567),(#71568,#71569,
#71570,#71571,#71572,#71573),(#71574,#71575,#71576,#71577,#71578,#71579),
(#71580,#71581,#71582,#71583,#71584,#71585),(#71586,#71587,#71588,#71589,
#71590,#71591),(#71592,#71593,#71594,#71595,#71596,#71597),(#71598,#71599,
#71600,#71601,#71602,#71603),(#71604,#71605,#71606,#71607,#71608,#71609),
(#71610,#71611,#71612,#71613,#71614,#71615),(#71616,#71617,#71618,#71619,
#71620,#71621),(#71622,#71623,#71624,#71625,#71626,#71627)),
 .UNSPECIFIED.,.F.,.F.,.F.,(6,3,3,6),(6,6),(2.28525111063,3.36176031805,
5.06337143522,7.79281869645),(0.,0.3),.UNSPECIFIED.);
#1075=B_SPLINE_SURFACE_WITH_KNOTS('',5,1,((#71710,#71711),(#71712,#71713),
(#71714,#71715),(#71716,#71717),(#71718,#71719),(#71720,#71721),(#71722,
#71723),(#71724,#71725),(#71726,#71727),(#71728,#71729),(#71730,#71731),
(#71732,#71733),(#71734,#71735),(#71736,#71737),(#71738,#71739)),
 .UNSPECIFIED.,.F.,.F.,.F.,(6,3,3,3,6),(2,2),(1.14001641713,1.87623741919,
2.65134293549,3.82861972691,4.99954599766),(0.,0.168000000000001),
 .UNSPECIFIED.);
#1076=B_SPLINE_SURFACE_WITH_KNOTS('',5,5,((#72928,#72929,#72930,#72931,
#72932,#72933),(#72934,#72935,#72936,#72937,#72938,#72939),(#72940,#72941,
#72942,#72943,#72944,#72945),(#72946,#72947,#72948,#72949,#72950,#72951),
(#72952,#72953,#72954,#72955,#72956,#72957),(#72958,#72959,#72960,#72961,
#72962,#72963),(#72964,#72965,#72966,#72967,#72968,#72969),(#72970,#72971,
#72972,#72973,#72974,#72975),(#72976,#72977,#72978,#72979,#72980,#72981)),
 .UNSPECIFIED.,.F.,.F.,.F.,(6,3,6),(6,6),(0.546404786097,1.22269549144,
1.74380556781),(0.,0.3),.UNSPECIFIED.);
#1077=B_SPLINE_SURFACE_WITH_KNOTS('',5,1,((#72992,#72993),(#72994,#72995),
(#72996,#72997),(#72998,#72999),(#73000,#73001),(#73002,#73003)),
 .UNSPECIFIED.,.F.,.F.,.F.,(6,6),(2,2),(0.454732309483,1.10434989446),(0.,
0.204),.UNSPECIFIED.);
#1078=B_SPLINE_SURFACE_WITH_KNOTS('',5,5,((#73012,#73013,#73014,#73015,
#73016,#73017),(#73018,#73019,#73020,#73021,#73022,#73023),(#73024,#73025,
#73026,#73027,#73028,#73029),(#73030,#73031,#73032,#73033,#73034,#73035),
(#73036,#73037,#73038,#73039,#73040,#73041),(#73042,#73043,#73044,#73045,
#73046,#73047),(#73048,#73049,#73050,#73051,#73052,#73053),(#73054,#73055,
#73056,#73057,#73058,#73059),(#73060,#73061,#73062,#73063,#73064,#73065)),
 .UNSPECIFIED.,.F.,.F.,.F.,(6,3,6),(6,6),(6.80309055586,12.796423133,18.7900427979),
(0.,0.3),.UNSPECIFIED.);
#1079=B_SPLINE_SURFACE_WITH_KNOTS('',5,1,((#73074,#73075),(#73076,#73077),
(#73078,#73079),(#73080,#73081),(#73082,#73083),(#73084,#73085)),
 .UNSPECIFIED.,.F.,.F.,.F.,(6,6),(2,2),(5.9795921157,14.5218665667),(0.,
0.203999999999999),.UNSPECIFIED.);
#1080=B_SPLINE_SURFACE_WITH_KNOTS('',5,5,((#73087,#73088,#73089,#73090,
#73091,#73092),(#73093,#73094,#73095,#73096,#73097,#73098),(#73099,#73100,
#73101,#73102,#73103,#73104),(#73105,#73106,#73107,#73108,#73109,#73110),
(#73111,#73112,#73113,#73114,#73115,#73116),(#73117,#73118,#73119,#73120,
#73121,#73122),(#73123,#73124,#73125,#73126,#73127,#73128),(#73129,#73130,
#73131,#73132,#73133,#73134),(#73135,#73136,#73137,#73138,#73139,#73140)),
 .UNSPECIFIED.,.F.,.F.,.F.,(6,3,6),(6,6),(6.80400424079,13.5782854139,18.7904488943),
(0.,0.3),.UNSPECIFIED.);
#1081=B_SPLINE_SURFACE_WITH_KNOTS('',5,1,((#73201,#73202),(#73203,#73204),
(#73205,#73206),(#73207,#73208),(#73209,#73210),(#73211,#73212)),
 .UNSPECIFIED.,.F.,.F.,.F.,(6,6),(2,2),(5.9795921157,14.5218665667),(0.,
0.204),.UNSPECIFIED.);
#1082=B_SPLINE_SURFACE_WITH_KNOTS('',5,5,((#73220,#73221,#73222,#73223,
#73224,#73225),(#73226,#73227,#73228,#73229,#73230,#73231),(#73232,#73233,
#73234,#73235,#73236,#73237),(#73238,#73239,#73240,#73241,#73242,#73243),
(#73244,#73245,#73246,#73247,#73248,#73249),(#73250,#73251,#73252,#73253,
#73254,#73255),(#73256,#73257,#73258,#73259,#73260,#73261),(#73262,#73263,
#73264,#73265,#73266,#73267),(#73268,#73269,#73270,#73271,#73272,#73273)),
 .UNSPECIFIED.,.F.,.F.,.F.,(6,3,6),(6,6),(0.54640511867,1.22269582402,1.74380590038),
(0.,0.3),.UNSPECIFIED.);
#1083=B_SPLINE_SURFACE_WITH_KNOTS('',5,1,((#73282,#73283),(#73284,#73285),
(#73286,#73287),(#73288,#73289),(#73290,#73291),(#73292,#73293)),
 .UNSPECIFIED.,.F.,.F.,.F.,(6,6),(2,2),(0.454732309483,1.10434989446),(0.,
0.203999999999999),.UNSPECIFIED.);
#1084=B_SPLINE_SURFACE_WITH_KNOTS('',5,5,((#73295,#73296,#73297,#73298,
#73299,#73300),(#73301,#73302,#73303,#73304,#73305,#73306),(#73307,#73308,
#73309,#73310,#73311,#73312),(#73313,#73314,#73315,#73316,#73317,#73318),
(#73319,#73320,#73321,#73322,#73323,#73324),(#73325,#73326,#73327,#73328,
#73329,#73330),(#73331,#73332,#73333,#73334,#73335,#73336),(#73337,#73338,
#73339,#73340,#73341,#73342),(#73343,#73344,#73345,#73346,#73347,#73348)),
 .UNSPECIFIED.,.F.,.F.,.F.,(6,3,6),(6,6),(5.54615686267,10.8163068596,14.9229845471),
(0.,0.3),.UNSPECIFIED.);
#1085=B_SPLINE_SURFACE_WITH_KNOTS('',5,1,((#73357,#73358),(#73359,#73360),
(#73361,#73362),(#73363,#73364),(#73365,#73366),(#73367,#73368)),
 .UNSPECIFIED.,.F.,.F.,.F.,(6,6),(2,2),(4.82544286935,11.7189326827),(0.,
0.203999999999999),.UNSPECIFIED.);
#1086=B_SPLINE_SURFACE_WITH_KNOTS('',5,5,((#73370,#73371,#73372,#73373,
#73374,#73375),(#73376,#73377,#73378,#73379,#73380,#73381),(#73382,#73383,
#73384,#73385,#73386,#73387),(#73388,#73389,#73390,#73391,#73392,#73393),
(#73394,#73395,#73396,#73397,#73398,#73399),(#73400,#73401,#73402,#73403,
#73404,#73405),(#73406,#73407,#73408,#73409,#73410,#73411),(#73412,#73413,
#73414,#73415,#73416,#73417),(#73418,#73419,#73420,#73421,#73422,#73423)),
 .UNSPECIFIED.,.F.,.F.,.F.,(6,3,6),(6,6),(1.16471317114,2.5069575699,3.70327394785),
(0.,0.3),.UNSPECIFIED.);
#1087=B_SPLINE_SURFACE_WITH_KNOTS('',5,1,((#73478,#73479),(#73480,#73481),
(#73482,#73483),(#73484,#73485),(#73486,#73487),(#73488,#73489)),
 .UNSPECIFIED.,.F.,.F.,.F.,(6,6),(2,2),(1.04539060089,2.53880574503),(0.,
0.204),.UNSPECIFIED.);
#1088=B_SPLINE_SURFACE_WITH_KNOTS('',5,5,((#73491,#73492,#73493,#73494,
#73495,#73496),(#73497,#73498,#73499,#73500,#73501,#73502),(#73503,#73504,
#73505,#73506,#73507,#73508),(#73509,#73510,#73511,#73512,#73513,#73514),
(#73515,#73516,#73517,#73518,#73519,#73520),(#73521,#73522,#73523,#73524,
#73525,#73526),(#73527,#73528,#73529,#73530,#73531,#73532),(#73533,#73534,
#73535,#73536,#73537,#73538),(#73539,#73540,#73541,#73542,#73543,#73544)),
 .UNSPECIFIED.,.F.,.F.,.F.,(6,3,6),(6,6),(5.54628902772,10.8164390246,14.9231167121),
(0.,0.3),.UNSPECIFIED.);
#1089=B_SPLINE_SURFACE_WITH_KNOTS('',5,1,((#73551,#73552),(#73553,#73554),
(#73555,#73556),(#73557,#73558),(#73559,#73560),(#73561,#73562)),
 .UNSPECIFIED.,.F.,.F.,.F.,(6,6),(2,2),(4.82544286935,11.7189326827),(0.,
0.204),.UNSPECIFIED.);
#1090=B_SPLINE_SURFACE_WITH_KNOTS('',5,5,((#73563,#73564,#73565,#73566,
#73567,#73568),(#73569,#73570,#73571,#73572,#73573,#73574),(#73575,#73576,
#73577,#73578,#73579,#73580),(#73581,#73582,#73583,#73584,#73585,#73586),
(#73587,#73588,#73589,#73590,#73591,#73592),(#73593,#73594,#73595,#73596,
#73597,#73598),(#73599,#73600,#73601,#73602,#73603,#73604),(#73605,#73606,
#73607,#73608,#73609,#73610),(#73611,#73612,#73613,#73614,#73615,#73616)),
 .UNSPECIFIED.,.F.,.F.,.F.,(6,3,6),(6,6),(0.68208121853,1.52935115459,2.17454139046),
(0.,0.3),.UNSPECIFIED.);
#1091=B_SPLINE_SURFACE_WITH_KNOTS('',5,1,((#73627,#73628),(#73629,#73630),
(#73631,#73632),(#73633,#73634),(#73635,#73636),(#73637,#73638)),
 .UNSPECIFIED.,.F.,.F.,.F.,(6,6),(2,2),(0.574089330078,1.39421694447),(0.,
0.203999999999999),.UNSPECIFIED.);
#1092=B_SPLINE_SURFACE_WITH_KNOTS('',5,5,((#73641,#73642,#73643,#73644,
#73645,#73646),(#73647,#73648,#73649,#73650,#73651,#73652),(#73653,#73654,
#73655,#73656,#73657,#73658),(#73659,#73660,#73661,#73662,#73663,#73664),
(#73665,#73666,#73667,#73668,#73669,#73670),(#73671,#73672,#73673,#73674,
#73675,#73676),(#73677,#73678,#73679,#73680,#73681,#73682),(#73683,#73684,
#73685,#73686,#73687,#73688),(#73689,#73690,#73691,#73692,#73693,#73694),
(#73695,#73696,#73697,#73698,#73699,#73700),(#73701,#73702,#73703,#73704,
#73705,#73706),(#73707,#73708,#73709,#73710,#73711,#73712),(#73713,#73714,
#73715,#73716,#73717,#73718),(#73719,#73720,#73721,#73722,#73723,#73724),
(#73725,#73726,#73727,#73728,#73729,#73730)),.UNSPECIFIED.,.F.,.F.,.F.,
(6,3,3,3,6),(6,6),(13.4402611449,23.5689081291,33.6443676545,43.7196576595,
53.84849829),(0.,0.3),.UNSPECIFIED.);
#1093=B_SPLINE_SURFACE_WITH_KNOTS('',5,1,((#73748,#73749),(#73750,#73751),
(#73752,#73753),(#73754,#73755),(#73756,#73757),(#73758,#73759),(#73760,
#73761),(#73762,#73763),(#73764,#73765),(#73766,#73767),(#73768,#73769),
(#73770,#73771),(#73772,#73773),(#73774,#73775),(#73776,#73777)),
 .UNSPECIFIED.,.F.,.F.,.F.,(6,3,3,3,6),(2,2),(9.75975111992,17.2672519814,
24.7747528429,32.2822537043,39.7897545658),(0.,0.203999999999999),
 .UNSPECIFIED.);
#1094=B_SPLINE_SURFACE_WITH_KNOTS('',5,5,((#73779,#73780,#73781,#73782,
#73783,#73784),(#73785,#73786,#73787,#73788,#73789,#73790),(#73791,#73792,
#73793,#73794,#73795,#73796),(#73797,#73798,#73799,#73800,#73801,#73802),
(#73803,#73804,#73805,#73806,#73807,#73808),(#73809,#73810,#73811,#73812,
#73813,#73814),(#73815,#73816,#73817,#73818,#73819,#73820),(#73821,#73822,
#73823,#73824,#73825,#73826),(#73827,#73828,#73829,#73830,#73831,#73832)),
 .UNSPECIFIED.,.F.,.F.,.F.,(6,3,6),(6,6),(0.578957415869,1.29652194364,
1.84813902128),(0.,0.3),.UNSPECIFIED.);
#1095=B_SPLINE_SURFACE_WITH_KNOTS('',5,1,((#73841,#73842),(#73843,#73844),
(#73845,#73846),(#73847,#73848),(#73849,#73850),(#73851,#73852)),
 .UNSPECIFIED.,.F.,.F.,.F.,(6,6),(2,2),(0.48312294093,1.17329857083),(0.,
0.203999999999999),.UNSPECIFIED.);
#1096=B_SPLINE_SURFACE_WITH_KNOTS('',5,5,((#73854,#73855,#73856,#73857,
#73858,#73859),(#73860,#73861,#73862,#73863,#73864,#73865),(#73866,#73867,
#73868,#73869,#73870,#73871),(#73872,#73873,#73874,#73875,#73876,#73877),
(#73878,#73879,#73880,#73881,#73882,#73883),(#73884,#73885,#73886,#73887,
#73888,#73889),(#73890,#73891,#73892,#73893,#73894,#73895),(#73896,#73897,
#73898,#73899,#73900,#73901),(#73902,#73903,#73904,#73905,#73906,#73907)),
 .UNSPECIFIED.,.F.,.F.,.F.,(6,3,6),(6,6),(0.579418789984,1.29713059772,
1.84860050261),(0.,0.3),.UNSPECIFIED.);
#1097=B_SPLINE_SURFACE_WITH_KNOTS('',5,1,((#73916,#73917),(#73918,#73919),
(#73920,#73921),(#73922,#73923),(#73924,#73925),(#73926,#73927)),
 .UNSPECIFIED.,.F.,.F.,.F.,(6,6),(2,2),(0.48312294093,1.17329857083),(0.,
0.204),.UNSPECIFIED.);
#1098=B_SPLINE_SURFACE_WITH_KNOTS('',5,5,((#73929,#73930,#73931,#73932,
#73933,#73934),(#73935,#73936,#73937,#73938,#73939,#73940),(#73941,#73942,
#73943,#73944,#73945,#73946),(#73947,#73948,#73949,#73950,#73951,#73952),
(#73953,#73954,#73955,#73956,#73957,#73958),(#73959,#73960,#73961,#73962,
#73963,#73964),(#73965,#73966,#73967,#73968,#73969,#73970),(#73971,#73972,
#73973,#73974,#73975,#73976),(#73977,#73978,#73979,#73980,#73981,#73982),
(#73983,#73984,#73985,#73986,#73987,#73988),(#73989,#73990,#73991,#73992,
#73993,#73994),(#73995,#73996,#73997,#73998,#73999,#74000),(#74001,#74002,
#74003,#74004,#74005,#74006),(#74007,#74008,#74009,#74010,#74011,#74012),
(#74013,#74014,#74015,#74016,#74017,#74018)),.UNSPECIFIED.,.F.,.F.,.F.,
(6,3,3,3,6),(6,6),(13.4404181035,23.5157081046,33.5961540362,43.6766373031,
53.8487877185),(0.,0.3),.UNSPECIFIED.);
#1099=B_SPLINE_SURFACE_WITH_KNOTS('',5,1,((#74036,#74037),(#74038,#74039),
(#74040,#74041),(#74042,#74043),(#74044,#74045),(#74046,#74047),(#74048,
#74049),(#74050,#74051),(#74052,#74053),(#74054,#74055),(#74056,#74057),
(#74058,#74059),(#74060,#74061),(#74062,#74063),(#74064,#74065)),
 .UNSPECIFIED.,.F.,.F.,.F.,(6,3,3,3,6),(2,2),(9.75975111992,17.2672519814,
24.7747528429,32.2822537043,39.7897545658),(0.,0.203999999999999),
 .UNSPECIFIED.);
#1100=B_SPLINE_SURFACE_WITH_KNOTS('',5,5,((#74067,#74068,#74069,#74070,
#74071,#74072),(#74073,#74074,#74075,#74076,#74077,#74078),(#74079,#74080,
#74081,#74082,#74083,#74084),(#74085,#74086,#74087,#74088,#74089,#74090),
(#74091,#74092,#74093,#74094,#74095,#74096),(#74097,#74098,#74099,#74100,
#74101,#74102),(#74103,#74104,#74105,#74106,#74107,#74108),(#74109,#74110,
#74111,#74112,#74113,#74114),(#74115,#74116,#74117,#74118,#74119,#74120)),
 .UNSPECIFIED.,.F.,.F.,.F.,(6,3,6),(6,6),(0.682080632107,1.52935056816,
2.17454080403),(0.,0.3),.UNSPECIFIED.);
#1101=B_SPLINE_SURFACE_WITH_KNOTS('',5,1,((#74129,#74130),(#74131,#74132),
(#74133,#74134),(#74135,#74136),(#74137,#74138),(#74139,#74140)),
 .UNSPECIFIED.,.F.,.F.,.F.,(6,6),(2,2),(0.574089330078,1.39421694447),(0.,
0.203999999999999),.UNSPECIFIED.);
#1102=B_SPLINE_SURFACE_WITH_KNOTS('',5,5,((#74148,#74149,#74150,#74151,
#74152,#74153),(#74154,#74155,#74156,#74157,#74158,#74159),(#74160,#74161,
#74162,#74163,#74164,#74165),(#74166,#74167,#74168,#74169,#74170,#74171),
(#74172,#74173,#74174,#74175,#74176,#74177),(#74178,#74179,#74180,#74181,
#74182,#74183),(#74184,#74185,#74186,#74187,#74188,#74189),(#74190,#74191,
#74192,#74193,#74194,#74195),(#74196,#74197,#74198,#74199,#74200,#74201)),
 .UNSPECIFIED.,.F.,.F.,.F.,(6,3,6),(6,6),(8.03777014773,13.7697600959,21.5792812917),
(0.,0.3),.UNSPECIFIED.);
#1103=B_SPLINE_SURFACE_WITH_KNOTS('',5,1,((#74210,#74211),(#74212,#74213),
(#74214,#74215),(#74216,#74217),(#74218,#74219),(#74220,#74221)),
 .UNSPECIFIED.,.F.,.F.,.F.,(6,6),(2,2),(7.11986732816,17.2911063684),(0.,
0.204),.UNSPECIFIED.);
#1104=B_SPLINE_SURFACE_WITH_KNOTS('',5,5,((#74223,#74224,#74225,#74226,
#74227,#74228),(#74229,#74230,#74231,#74232,#74233,#74234),(#74235,#74236,
#74237,#74238,#74239,#74240),(#74241,#74242,#74243,#74244,#74245,#74246),
(#74247,#74248,#74249,#74250,#74251,#74252),(#74253,#74254,#74255,#74256,
#74257,#74258),(#74259,#74260,#74261,#74262,#74263,#74264),(#74265,#74266,
#74267,#74268,#74269,#74270),(#74271,#74272,#74273,#74274,#74275,#74276)),
 .UNSPECIFIED.,.F.,.F.,.F.,(6,3,6),(6,6),(8.03689290773,13.768506892,21.5784150656),
(0.,0.3),.UNSPECIFIED.);
#1105=B_SPLINE_SURFACE_WITH_KNOTS('',5,1,((#74285,#74286),(#74287,#74288),
(#74289,#74290),(#74291,#74292),(#74293,#74294),(#74295,#74296)),
 .UNSPECIFIED.,.F.,.F.,.F.,(6,6),(2,2),(7.11986732816,17.2911063684),(0.,
0.204000000000001),.UNSPECIFIED.);
#1106=B_SPLINE_SURFACE_WITH_KNOTS('',3,1,((#74322,#74323),(#74324,#74325),
(#74326,#74327),(#74328,#74329)),.UNSPECIFIED.,.F.,.F.,.F.,(4,4),(2,2),
(1.93787056397,2.72108189072),(0.,0.18),.UNSPECIFIED.);
#1107=B_SPLINE_SURFACE_WITH_KNOTS('',3,1,((#74355,#74356),(#74357,#74358),
(#74359,#74360),(#74361,#74362)),.UNSPECIFIED.,.F.,.F.,.F.,(4,4),(2,2),
(1.93787056397,2.72108189072),(0.,0.18),.UNSPECIFIED.);
#1108=B_SPLINE_SURFACE_WITH_KNOTS('',4,1,((#74601,#74602),(#74603,#74604),
(#74605,#74606),(#74607,#74608),(#74609,#74610)),.UNSPECIFIED.,.F.,.F.,
 .F.,(5,5),(2,2),(13.4220086236,14.3963748612),(0.,0.288),.UNSPECIFIED.);
#1109=B_SPLINE_SURFACE_WITH_KNOTS('',4,1,((#74660,#74661),(#74662,#74663),
(#74664,#74665),(#74666,#74667),(#74668,#74669)),.UNSPECIFIED.,.F.,.F.,
 .F.,(5,5),(2,2),(13.4220086236,14.3963748612),(0.,0.288),.UNSPECIFIED.);
#1110=B_SPLINE_SURFACE_WITH_KNOTS('',4,1,((#74721,#74722),(#74723,#74724),
(#74725,#74726),(#74727,#74728),(#74729,#74730)),.UNSPECIFIED.,.F.,.F.,
 .F.,(5,5),(2,2),(7.90893025972,8.88329649724),(0.,0.288),.UNSPECIFIED.);
#1111=B_SPLINE_SURFACE_WITH_KNOTS('',4,1,((#74780,#74781),(#74782,#74783),
(#74784,#74785),(#74786,#74787),(#74788,#74789)),.UNSPECIFIED.,.F.,.F.,
 .F.,(5,5),(2,2),(7.90893025972,8.88329649724),(0.,0.288),.UNSPECIFIED.);
#1112=B_SPLINE_SURFACE_WITH_KNOTS('',5,1,((#75672,#75673),(#75674,#75675),
(#75676,#75677),(#75678,#75679),(#75680,#75681),(#75682,#75683),(#75684,
#75685),(#75686,#75687),(#75688,#75689),(#75690,#75691),(#75692,#75693),
(#75694,#75695)),.UNSPECIFIED.,.F.,.F.,.F.,(6,3,3,6),(2,2),(0.,3.06410506181,
5.01303018899,6.53082821197),(0.,0.180000000000001),.UNSPECIFIED.);
#1113=B_SPLINE_SURFACE_WITH_KNOTS('',5,1,((#75710,#75711),(#75712,#75713),
(#75714,#75715),(#75716,#75717),(#75718,#75719),(#75720,#75721),(#75722,
#75723),(#75724,#75725),(#75726,#75727),(#75728,#75729),(#75730,#75731),
(#75732,#75733)),.UNSPECIFIED.,.F.,.F.,.F.,(6,3,3,6),(2,2),(0.,1.23981126536,
4.14117682427,4.7101423031),(0.,0.180000000000001),.UNSPECIFIED.);
#1114=B_SPLINE_SURFACE_WITH_KNOTS('',5,1,((#75748,#75749),(#75750,#75751),
(#75752,#75753),(#75754,#75755),(#75756,#75757),(#75758,#75759),(#75760,
#75761),(#75762,#75763),(#75764,#75765),(#75766,#75767),(#75768,#75769),
(#75770,#75771)),.UNSPECIFIED.,.F.,.F.,.F.,(6,3,3,6),(2,2),(17.5092154859,
21.7374875265,29.3008927769,31.9433833551),(0.,0.180000000000001),
 .UNSPECIFIED.);
#1115=B_SPLINE_SURFACE_WITH_KNOTS('',5,1,((#75786,#75787),(#75788,#75789),
(#75790,#75791),(#75792,#75793),(#75794,#75795),(#75796,#75797),(#75798,
#75799),(#75800,#75801),(#75802,#75803)),.UNSPECIFIED.,.F.,.F.,.F.,(6,3,
6),(2,2),(10.4583103224,10.8525207074,15.6953714763),(0.,0.180000000000001),
 .UNSPECIFIED.);
#1116=B_SPLINE_SURFACE_WITH_KNOTS('',5,1,((#75836,#75837),(#75838,#75839),
(#75840,#75841),(#75842,#75843),(#75844,#75845),(#75846,#75847),(#75848,
#75849),(#75850,#75851),(#75852,#75853)),.UNSPECIFIED.,.F.,.F.,.F.,(6,3,
6),(2,2),(-1.52206773895,0.,8.40229743882),(0.,0.180000000000003),
 .UNSPECIFIED.);
#1117=B_SPLINE_SURFACE_WITH_KNOTS('',5,1,((#75877,#75878),(#75879,#75880),
(#75881,#75882),(#75883,#75884),(#75885,#75886),(#75887,#75888),(#75889,
#75890),(#75891,#75892),(#75893,#75894)),.UNSPECIFIED.,.F.,.F.,.F.,(6,3,
6),(2,2),(-1.52206773895,0.,8.40229791516),(0.,0.180000000000001),
 .UNSPECIFIED.);
#1118=B_SPLINE_SURFACE_WITH_KNOTS('',5,1,((#75906,#75907),(#75908,#75909),
(#75910,#75911),(#75912,#75913),(#75914,#75915),(#75916,#75917),(#75918,
#75919),(#75920,#75921),(#75922,#75923)),.UNSPECIFIED.,.F.,.F.,.F.,(6,3,
6),(2,2),(10.4583103224,10.8525207074,15.6953714763),(0.,0.180000000000001),
 .UNSPECIFIED.);
#1119=B_SPLINE_SURFACE_WITH_KNOTS('',5,1,((#75956,#75957),(#75958,#75959),
(#75960,#75961),(#75962,#75963),(#75964,#75965),(#75966,#75967),(#75968,
#75969),(#75970,#75971),(#75972,#75973),(#75974,#75975),(#75976,#75977),
(#75978,#75979)),.UNSPECIFIED.,.F.,.F.,.F.,(6,3,3,6),(2,2),(17.5092154859,
21.7374875265,29.3008927769,31.9433833551),(0.,0.180000000000001),
 .UNSPECIFIED.);
#1120=B_SPLINE_SURFACE_WITH_KNOTS('',5,1,((#75996,#75997),(#75998,#75999),
(#76000,#76001),(#76002,#76003),(#76004,#76005),(#76006,#76007),(#76008,
#76009),(#76010,#76011),(#76012,#76013),(#76014,#76015),(#76016,#76017),
(#76018,#76019)),.UNSPECIFIED.,.F.,.F.,.F.,(6,3,3,6),(2,2),(0.,1.23981126536,
4.14117682427,4.7101423031),(0.,0.180000000000001),.UNSPECIFIED.);
#1121=B_SPLINE_SURFACE_WITH_KNOTS('',5,1,((#76034,#76035),(#76036,#76037),
(#76038,#76039),(#76040,#76041),(#76042,#76043),(#76044,#76045),(#76046,
#76047),(#76048,#76049),(#76050,#76051),(#76052,#76053),(#76054,#76055),
(#76056,#76057)),.UNSPECIFIED.,.F.,.F.,.F.,(6,3,3,6),(2,2),(0.,3.06410506181,
5.01303018899,6.53082821197),(0.,0.180000000000001),.UNSPECIFIED.);
#1122=B_SPLINE_SURFACE_WITH_KNOTS('',5,1,((#76190,#76191),(#76192,#76193),
(#76194,#76195),(#76196,#76197),(#76198,#76199),(#76200,#76201),(#76202,
#76203),(#76204,#76205),(#76206,#76207),(#76208,#76209),(#76210,#76211),
(#76212,#76213),(#76214,#76215),(#76216,#76217),(#76218,#76219)),
 .UNSPECIFIED.,.F.,.F.,.F.,(6,3,3,3,6),(2,2),(0.,2.13949651284,3.65547289001,
4.94562974894,5.62440522293),(0.,0.120000000000001),.UNSPECIFIED.);
#1123=B_SPLINE_SURFACE_WITH_KNOTS('',5,1,((#76253,#76254),(#76255,#76256),
(#76257,#76258),(#76259,#76260),(#76261,#76262),(#76263,#76264),(#76265,
#76266),(#76267,#76268),(#76269,#76270)),.UNSPECIFIED.,.F.,.F.,.F.,(6,3,
6),(2,2),(0.,1.07297825382,3.85154891337),(0.,0.120000000000002),
 .UNSPECIFIED.);
#1124=B_SPLINE_SURFACE_WITH_KNOTS('',5,1,((#76292,#76293),(#76294,#76295),
(#76296,#76297),(#76298,#76299),(#76300,#76301),(#76302,#76303),(#76304,
#76305),(#76306,#76307),(#76308,#76309),(#76310,#76311),(#76312,#76313),
(#76314,#76315),(#76316,#76317),(#76318,#76319),(#76320,#76321),(#76322,
#76323),(#76324,#76325),(#76326,#76327)),.UNSPECIFIED.,.F.,.F.,.F.,(6,3,
3,3,3,6),(2,2),(-1.28529178055,0.,8.34825709363,17.7305069581,25.102843518,
27.4630296434),(0.,0.120000000000001),.UNSPECIFIED.);
#1125=B_SPLINE_SURFACE_WITH_KNOTS('',5,1,((#76373,#76374),(#76375,#76376),
(#76377,#76378),(#76379,#76380),(#76381,#76382),(#76383,#76384),(#76385,
#76386),(#76387,#76388),(#76389,#76390),(#76391,#76392),(#76393,#76394),
(#76395,#76396),(#76397,#76398),(#76399,#76400),(#76401,#76402),(#76403,
#76404),(#76405,#76406),(#76407,#76408)),.UNSPECIFIED.,.F.,.F.,.F.,(6,3,
3,3,3,6),(2,2),(-1.28529178055,0.,8.34825709363,17.7305069581,25.102843518,
27.4630296434),(0.,0.120000000000001),.UNSPECIFIED.);
#1126=B_SPLINE_SURFACE_WITH_KNOTS('',5,1,((#76448,#76449),(#76450,#76451),
(#76452,#76453),(#76454,#76455),(#76456,#76457),(#76458,#76459),(#76460,
#76461),(#76462,#76463),(#76464,#76465)),.UNSPECIFIED.,.F.,.F.,.F.,(6,3,
6),(2,2),(0.,1.07297825382,3.85154891337),(0.,0.120000000000001),
 .UNSPECIFIED.);
#1127=B_SPLINE_SURFACE_WITH_KNOTS('',5,1,((#76487,#76488),(#76489,#76490),
(#76491,#76492),(#76493,#76494),(#76495,#76496),(#76497,#76498),(#76499,
#76500),(#76501,#76502),(#76503,#76504),(#76505,#76506),(#76507,#76508),
(#76509,#76510),(#76511,#76512),(#76513,#76514),(#76515,#76516)),
 .UNSPECIFIED.,.F.,.F.,.F.,(6,3,3,3,6),(2,2),(0.,2.13949651284,3.65547289001,
4.94562974894,5.62440522293),(0.,0.120000000000001),.UNSPECIFIED.);
#1128=B_SPLINE_SURFACE_WITH_KNOTS('',5,1,((#76588,#76589),(#76590,#76591),
(#76592,#76593),(#76594,#76595),(#76596,#76597),(#76598,#76599)),
 .UNSPECIFIED.,.F.,.F.,.F.,(6,6),(2,2),(0.,3.5713550833),(0.,0.300000000000001),
 .UNSPECIFIED.);
#1129=B_SPLINE_SURFACE_WITH_KNOTS('',5,1,((#76666,#76667),(#76668,#76669),
(#76670,#76671),(#76672,#76673),(#76674,#76675),(#76676,#76677)),
 .UNSPECIFIED.,.F.,.F.,.F.,(6,6),(2,2),(0.,3.5713550833),(0.,0.300000000000001),
 .UNSPECIFIED.);
#1130=B_SPLINE_SURFACE_WITH_KNOTS('',5,1,((#77077,#77078),(#77079,#77080),
(#77081,#77082),(#77083,#77084),(#77085,#77086),(#77087,#77088),(#77089,
#77090),(#77091,#77092),(#77093,#77094),(#77095,#77096),(#77097,#77098),
(#77099,#77100),(#77101,#77102),(#77103,#77104),(#77105,#77106),(#77107,
#77108),(#77109,#77110),(#77111,#77112)),.UNSPECIFIED.,.F.,.F.,.F.,(6,3,
3,3,3,6),(2,2),(2.04066423734,2.62011481805,3.50908168923,4.52495007124,
5.25002578886,6.51367347233),(0.,0.300000000000002),.UNSPECIFIED.);
#1131=B_SPLINE_SURFACE_WITH_KNOTS('',5,1,((#77218,#77219),(#77220,#77221),
(#77222,#77223),(#77224,#77225),(#77226,#77227),(#77228,#77229),(#77230,
#77231),(#77232,#77233),(#77234,#77235),(#77236,#77237),(#77238,#77239),
(#77240,#77241),(#77242,#77243),(#77244,#77245),(#77246,#77247),(#77248,
#77249),(#77250,#77251),(#77252,#77253)),.UNSPECIFIED.,.F.,.F.,.F.,(6,3,
3,3,3,6),(2,2),(2.04066423734,2.62011481805,3.50908168923,4.52495007124,
5.25002578886,6.51367347233),(0.,0.300000000000002),.UNSPECIFIED.);
#1132=B_SPLINE_SURFACE_WITH_KNOTS('',5,1,((#77254,#77255),(#77256,#77257),
(#77258,#77259),(#77260,#77261),(#77262,#77263),(#77264,#77265),(#77266,
#77267),(#77268,#77269),(#77270,#77271),(#77272,#77273),(#77274,#77275),
(#77276,#77277)),.UNSPECIFIED.,.F.,.F.,.F.,(6,3,3,6),(2,2),(0.,3.39713474113,
6.68643994484,8.37826425912),(0.,0.300000000000001),.UNSPECIFIED.);
#1133=B_SPLINE_SURFACE_WITH_KNOTS('',5,1,((#77298,#77299),(#77300,#77301),
(#77302,#77303),(#77304,#77305),(#77306,#77307),(#77308,#77309),(#77310,
#77311),(#77312,#77313),(#77314,#77315)),.UNSPECIFIED.,.F.,.F.,.F.,(6,3,
6),(2,2),(0.,2.6134611976,3.73613338933),(0.,0.300000000000001),
 .UNSPECIFIED.);
#1134=B_SPLINE_SURFACE_WITH_KNOTS('',5,1,((#77327,#77328),(#77329,#77330),
(#77331,#77332),(#77333,#77334),(#77335,#77336),(#77337,#77338)),
 .UNSPECIFIED.,.F.,.F.,.F.,(6,6),(2,2),(0.,1.1155886229),(0.,0.300000000000001),
 .UNSPECIFIED.);
#1135=B_SPLINE_SURFACE_WITH_KNOTS('',5,1,((#77347,#77348),(#77349,#77350),
(#77351,#77352),(#77353,#77354),(#77355,#77356),(#77357,#77358),(#77359,
#77360),(#77361,#77362),(#77363,#77364),(#77365,#77366),(#77367,#77368),
(#77369,#77370),(#77371,#77372),(#77373,#77374),(#77375,#77376)),
 .UNSPECIFIED.,.F.,.F.,.F.,(6,3,3,3,6),(2,2),(0.,1.14196741734,1.69664449439,
2.26600465298,2.82383165251),(0.,0.300000000000001),.UNSPECIFIED.);
#1136=B_SPLINE_SURFACE_WITH_KNOTS('',5,1,((#77394,#77395),(#77396,#77397),
(#77398,#77399),(#77400,#77401),(#77402,#77403),(#77404,#77405)),
 .UNSPECIFIED.,.F.,.F.,.F.,(6,6),(2,2),(0.,2.29845936737),(0.,0.300000000000001),
 .UNSPECIFIED.);
#1137=B_SPLINE_SURFACE_WITH_KNOTS('',5,1,((#77414,#77415),(#77416,#77417),
(#77418,#77419),(#77420,#77421),(#77422,#77423),(#77424,#77425),(#77426,
#77427),(#77428,#77429),(#77430,#77431),(#77432,#77433),(#77434,#77435),
(#77436,#77437),(#77438,#77439),(#77440,#77441),(#77442,#77443)),
 .UNSPECIFIED.,.F.,.F.,.F.,(6,3,3,3,6),(2,2),(0.,6.696077534,12.6191089245,
16.7682744334,17.9215041098),(0.,0.300000000000001),.UNSPECIFIED.);
#1138=B_SPLINE_SURFACE_WITH_KNOTS('',5,1,((#77471,#77472),(#77473,#77474),
(#77475,#77476),(#77477,#77478),(#77479,#77480),(#77481,#77482),(#77483,
#77484),(#77485,#77486),(#77487,#77488),(#77489,#77490),(#77491,#77492),
(#77493,#77494),(#77495,#77496),(#77497,#77498),(#77499,#77500)),
 .UNSPECIFIED.,.F.,.F.,.F.,(6,3,3,3,6),(2,2),(0.,6.696077534,12.6191089245,
16.7682744334,17.9215041098),(0.,0.300000000000001),.UNSPECIFIED.);
#1139=B_SPLINE_SURFACE_WITH_KNOTS('',5,1,((#77520,#77521),(#77522,#77523),
(#77524,#77525),(#77526,#77527),(#77528,#77529),(#77530,#77531),(#77532,
#77533),(#77534,#77535),(#77536,#77537)),.UNSPECIFIED.,.F.,.F.,.F.,(6,3,
6),(2,2),(0.,2.6134611976,3.73613338933),(0.,0.300000000000001),
 .UNSPECIFIED.);
#1140=B_SPLINE_SURFACE_WITH_KNOTS('',5,1,((#77565,#77566),(#77567,#77568),
(#77569,#77570),(#77571,#77572),(#77573,#77574),(#77575,#77576),(#77577,
#77578),(#77579,#77580),(#77581,#77582),(#77583,#77584),(#77585,#77586),
(#77587,#77588)),.UNSPECIFIED.,.F.,.F.,.F.,(6,3,3,6),(2,2),(0.,3.39713474113,
6.68643994484,8.37826425912),(0.,0.300000000000001),.UNSPECIFIED.);
#1141=B_SPLINE_SURFACE_WITH_KNOTS('',5,1,((#77603,#77604),(#77605,#77606),
(#77607,#77608),(#77609,#77610),(#77611,#77612),(#77613,#77614)),
 .UNSPECIFIED.,.F.,.F.,.F.,(6,6),(2,2),(0.,2.29845936737),(0.,0.300000000000001),
 .UNSPECIFIED.);
#1142=B_SPLINE_SURFACE_WITH_KNOTS('',5,1,((#77623,#77624),(#77625,#77626),
(#77627,#77628),(#77629,#77630),(#77631,#77632),(#77633,#77634),(#77635,
#77636),(#77637,#77638),(#77639,#77640),(#77641,#77642),(#77643,#77644),
(#77645,#77646),(#77647,#77648),(#77649,#77650),(#77651,#77652)),
 .UNSPECIFIED.,.F.,.F.,.F.,(6,3,3,3,6),(2,2),(0.,1.14196741734,1.69664449439,
2.26600465298,2.82383165251),(0.,0.300000000000001),.UNSPECIFIED.);
#1143=B_SPLINE_SURFACE_WITH_KNOTS('',5,1,((#77670,#77671),(#77672,#77673),
(#77674,#77675),(#77676,#77677),(#77678,#77679),(#77680,#77681)),
 .UNSPECIFIED.,.F.,.F.,.F.,(6,6),(2,2),(0.,1.1155886229),(0.,0.300000000000001),
 .UNSPECIFIED.);
#1144=B_SPLINE_SURFACE_WITH_KNOTS('',5,1,((#77688,#77689),(#77690,#77691),
(#77692,#77693),(#77694,#77695),(#77696,#77697),(#77698,#77699),(#77700,
#77701),(#77702,#77703),(#77704,#77705),(#77706,#77707),(#77708,#77709),
(#77710,#77711),(#77712,#77713),(#77714,#77715),(#77716,#77717)),
 .UNSPECIFIED.,.F.,.F.,.F.,(6,3,3,3,6),(2,2),(0.,1.06902836413,2.19771269917,
3.2241260379,4.7004853448),(0.,0.120000000000001),.UNSPECIFIED.);
#1145=B_SPLINE_SURFACE_WITH_KNOTS('',5,1,((#77737,#77738),(#77739,#77740),
(#77741,#77742),(#77743,#77744),(#77745,#77746),(#77747,#77748)),
 .UNSPECIFIED.,.F.,.F.,.F.,(6,6),(2,2),(0.,6.43612007405),(0.,0.120000000000001),
 .UNSPECIFIED.);
#1146=B_SPLINE_SURFACE_WITH_KNOTS('',5,1,((#77777,#77778),(#77779,#77780),
(#77781,#77782),(#77783,#77784),(#77785,#77786),(#77787,#77788),(#77789,
#77790),(#77791,#77792),(#77793,#77794),(#77795,#77796),(#77797,#77798),
(#77799,#77800),(#77801,#77802),(#77803,#77804),(#77805,#77806)),
 .UNSPECIFIED.,.F.,.F.,.F.,(6,3,3,3,6),(2,2),(0.039515807079,7.53253625942,
14.2747183071,18.8083875826,22.71906151),(0.,0.120000000000001),
 .UNSPECIFIED.);
#1147=B_SPLINE_SURFACE_WITH_KNOTS('',5,1,((#77824,#77825),(#77826,#77827),
(#77828,#77829),(#77830,#77831),(#77832,#77833),(#77834,#77835),(#77836,
#77837),(#77838,#77839),(#77840,#77841)),.UNSPECIFIED.,.F.,.F.,.F.,(6,3,
6),(2,2),(1.18944404077E-12,1.10170421198,3.01229896543),(0.,0.120000000000001),
 .UNSPECIFIED.);
#1148=B_SPLINE_SURFACE_WITH_KNOTS('',5,1,((#77851,#77852),(#77853,#77854),
(#77855,#77856),(#77857,#77858),(#77859,#77860),(#77861,#77862),(#77863,
#77864),(#77865,#77866),(#77867,#77868)),.UNSPECIFIED.,.F.,.F.,.F.,(6,3,
6),(2,2),(0.,2.92723336323,3.88093368919),(0.,0.120000000000002),
 .UNSPECIFIED.);
#1149=B_SPLINE_SURFACE_WITH_KNOTS('',5,1,((#77871,#77872),(#77873,#77874),
(#77875,#77876),(#77877,#77878),(#77879,#77880),(#77881,#77882),(#77883,
#77884),(#77885,#77886),(#77887,#77888),(#77889,#77890),(#77891,#77892),
(#77893,#77894),(#77895,#77896),(#77897,#77898),(#77899,#77900),(#77901,
#77902),(#77903,#77904)),.UNSPECIFIED.,.F.,.F.,.F.,(6,3,3,5,6),(2,2),(3.11522256756,
4.13897763214,6.99130562041,9.89933117719,9.89969814681689),(0.,0.120000000000001),
 .UNSPECIFIED.);
#1150=B_SPLINE_SURFACE_WITH_KNOTS('',5,1,((#77908,#77909),(#77910,#77911),
(#77912,#77913),(#77914,#77915),(#77916,#77917),(#77918,#77919),(#77920,
#77921),(#77922,#77923),(#77924,#77925),(#77926,#77927),(#77928,#77929),
(#77930,#77931)),.UNSPECIFIED.,.F.,.F.,.F.,(6,3,3,6),(2,2),(3.11522256756,
4.13897763214,6.99130562041,9.89912618426),(0.,0.120000000000001),
 .UNSPECIFIED.);
#1151=B_SPLINE_SURFACE_WITH_KNOTS('',5,1,((#77933,#77934),(#77935,#77936),
(#77937,#77938),(#77939,#77940),(#77941,#77942),(#77943,#77944),(#77945,
#77946),(#77947,#77948),(#77949,#77950),(#77951,#77952),(#77953,#77954),
(#77955,#77956),(#77957,#77958),(#77959,#77960)),.UNSPECIFIED.,.F.,.F.,
 .F.,(6,3,5,6),(2,2),(0.,2.92723336323,3.88093368919,3.88140412218319),
(0.,0.120000000000005),.UNSPECIFIED.);
#1152=B_SPLINE_SURFACE_WITH_KNOTS('',5,1,((#77987,#77988),(#77989,#77990),
(#77991,#77992),(#77993,#77994),(#77995,#77996),(#77997,#77998)),
 .UNSPECIFIED.,.F.,.F.,.F.,(6,6),(2,2),(0.,6.43612007405),(0.,0.120000000000003),
 .UNSPECIFIED.);
#1153=B_SPLINE_SURFACE_WITH_KNOTS('',5,1,((#78007,#78008),(#78009,#78010),
(#78011,#78012),(#78013,#78014),(#78015,#78016),(#78017,#78018),(#78019,
#78020),(#78021,#78022),(#78023,#78024),(#78025,#78026),(#78027,#78028),
(#78029,#78030),(#78031,#78032),(#78033,#78034),(#78035,#78036)),
 .UNSPECIFIED.,.F.,.F.,.F.,(6,3,3,3,6),(2,2),(0.,1.06902836413,2.19771269917,
3.2241260379,4.7004853448),(0.,0.120000000000001),.UNSPECIFIED.);
#1154=B_SPLINE_SURFACE_WITH_KNOTS('',5,1,((#78054,#78055),(#78056,#78057),
(#78058,#78059),(#78060,#78061),(#78062,#78063),(#78064,#78065),(#78066,
#78067),(#78068,#78069),(#78070,#78071)),.UNSPECIFIED.,.F.,.F.,.F.,(6,3,
6),(2,2),(1.18944404077E-12,1.10170421198,3.01229896543),(0.,0.120000000000001),
 .UNSPECIFIED.);
#1155=B_SPLINE_SURFACE_WITH_KNOTS('',5,1,((#78083,#78084),(#78085,#78086),
(#78087,#78088),(#78089,#78090),(#78091,#78092),(#78093,#78094),(#78095,
#78096),(#78097,#78098),(#78099,#78100),(#78101,#78102),(#78103,#78104),
(#78105,#78106),(#78107,#78108),(#78109,#78110),(#78111,#78112)),
 .UNSPECIFIED.,.F.,.F.,.F.,(6,3,3,3,6),(2,2),(0.0395158070789,7.53253625942,
14.2747183071,18.8083875826,22.71906151),(0.,0.120000000000001),
 .UNSPECIFIED.);
#1156=B_SPLINE_SURFACE_WITH_KNOTS('',5,5,((#79194,#79195,#79196,#79197,
#79198,#79199),(#79200,#79201,#79202,#79203,#79204,#79205),(#79206,#79207,
#79208,#79209,#79210,#79211),(#79212,#79213,#79214,#79215,#79216,#79217),
(#79218,#79219,#79220,#79221,#79222,#79223),(#79224,#79225,#79226,#79227,
#79228,#79229)),.UNSPECIFIED.,.F.,.F.,.F.,(6,6),(6,6),(1.91917304179,2.64214133457),
(0.,0.3),.UNSPECIFIED.);
#1157=B_SPLINE_SURFACE_WITH_KNOTS('',5,5,((#79714,#79715,#79716,#79717,
#79718,#79719),(#79720,#79721,#79722,#79723,#79724,#79725),(#79726,#79727,
#79728,#79729,#79730,#79731),(#79732,#79733,#79734,#79735,#79736,#79737),
(#79738,#79739,#79740,#79741,#79742,#79743),(#79744,#79745,#79746,#79747,
#79748,#79749)),.UNSPECIFIED.,.F.,.F.,.F.,(6,6),(6,6),(1.95117092983,2.67415250918),
(0.,0.3),.UNSPECIFIED.);
#1158=B_SPLINE_SURFACE_WITH_KNOTS('',5,5,((#79924,#79925,#79926,#79927,
#79928,#79929),(#79930,#79931,#79932,#79933,#79934,#79935),(#79936,#79937,
#79938,#79939,#79940,#79941),(#79942,#79943,#79944,#79945,#79946,#79947),
(#79948,#79949,#79950,#79951,#79952,#79953),(#79954,#79955,#79956,#79957,
#79958,#79959)),.UNSPECIFIED.,.F.,.F.,.F.,(6,6),(6,6),(1.62679171178,4.14575432942),
(0.,0.3),.UNSPECIFIED.);
#1159=B_SPLINE_SURFACE_WITH_KNOTS('',5,5,((#79981,#79982,#79983,#79984,
#79985,#79986),(#79987,#79988,#79989,#79990,#79991,#79992),(#79993,#79994,
#79995,#79996,#79997,#79998),(#79999,#80000,#80001,#80002,#80003,#80004),
(#80005,#80006,#80007,#80008,#80009,#80010),(#80011,#80012,#80013,#80014,
#80015,#80016)),.UNSPECIFIED.,.F.,.F.,.F.,(6,6),(6,6),(5.20521075808,6.00042817873),
(0.,0.3),.UNSPECIFIED.);
#1160=B_SPLINE_SURFACE_WITH_KNOTS('',5,5,((#80093,#80094,#80095,#80096,
#80097,#80098),(#80099,#80100,#80101,#80102,#80103,#80104),(#80105,#80106,
#80107,#80108,#80109,#80110),(#80111,#80112,#80113,#80114,#80115,#80116),
(#80117,#80118,#80119,#80120,#80121,#80122),(#80123,#80124,#80125,#80126,
#80127,#80128)),.UNSPECIFIED.,.F.,.F.,.F.,(6,6),(6,6),(5.20484021909,5.76063633602),
(0.,0.3),.UNSPECIFIED.);
#1161=B_SPLINE_SURFACE_WITH_KNOTS('',5,5,((#80139,#80140,#80141,#80142,
#80143,#80144),(#80145,#80146,#80147,#80148,#80149,#80150),(#80151,#80152,
#80153,#80154,#80155,#80156),(#80157,#80158,#80159,#80160,#80161,#80162),
(#80163,#80164,#80165,#80166,#80167,#80168),(#80169,#80170,#80171,#80172,
#80173,#80174)),.UNSPECIFIED.,.F.,.F.,.F.,(6,6),(6,6),(1.9878298196,2.53578324996),
(0.,0.3),.UNSPECIFIED.);
#1162=B_SPLINE_SURFACE_WITH_KNOTS('',5,5,((#80264,#80265,#80266,#80267,
#80268,#80269),(#80270,#80271,#80272,#80273,#80274,#80275),(#80276,#80277,
#80278,#80279,#80280,#80281),(#80282,#80283,#80284,#80285,#80286,#80287),
(#80288,#80289,#80290,#80291,#80292,#80293),(#80294,#80295,#80296,#80297,
#80298,#80299),(#80300,#80301,#80302,#80303,#80304,#80305),(#80306,#80307,
#80308,#80309,#80310,#80311),(#80312,#80313,#80314,#80315,#80316,#80317)),
 .UNSPECIFIED.,.F.,.F.,.F.,(6,3,6),(6,6),(3.54900880514,4.18701109461,4.71575303852),
(0.,0.3),.UNSPECIFIED.);
#1163=B_SPLINE_SURFACE_WITH_KNOTS('',5,5,((#80403,#80404,#80405,#80406,
#80407,#80408),(#80409,#80410,#80411,#80412,#80413,#80414),(#80415,#80416,
#80417,#80418,#80419,#80420),(#80421,#80422,#80423,#80424,#80425,#80426),
(#80427,#80428,#80429,#80430,#80431,#80432),(#80433,#80434,#80435,#80436,
#80437,#80438),(#80439,#80440,#80441,#80442,#80443,#80444),(#80445,#80446,
#80447,#80448,#80449,#80450),(#80451,#80452,#80453,#80454,#80455,#80456)),
 .UNSPECIFIED.,.F.,.F.,.F.,(6,3,6),(6,6),(3.54900880515,4.18701109461,4.71575303852),
(0.,0.3),.UNSPECIFIED.);
#1164=B_SPLINE_SURFACE_WITH_KNOTS('',5,5,((#80828,#80829,#80830,#80831,
#80832,#80833),(#80834,#80835,#80836,#80837,#80838,#80839),(#80840,#80841,
#80842,#80843,#80844,#80845),(#80846,#80847,#80848,#80849,#80850,#80851),
(#80852,#80853,#80854,#80855,#80856,#80857),(#80858,#80859,#80860,#80861,
#80862,#80863)),.UNSPECIFIED.,.F.,.F.,.F.,(6,6),(6,6),(3.53583307557,4.36798756241),
(0.,0.3),.UNSPECIFIED.);
#1165=B_SPLINE_SURFACE_WITH_KNOTS('',5,5,((#80907,#80908,#80909,#80910,
#80911,#80912,#80913,#80914,#80915),(#80916,#80917,#80918,#80919,#80920,
#80921,#80922,#80923,#80924),(#80925,#80926,#80927,#80928,#80929,#80930,
#80931,#80932,#80933),(#80934,#80935,#80936,#80937,#80938,#80939,#80940,
#80941,#80942),(#80943,#80944,#80945,#80946,#80947,#80948,#80949,#80950,
#80951),(#80952,#80953,#80954,#80955,#80956,#80957,#80958,#80959,#80960),
(#80961,#80962,#80963,#80964,#80965,#80966,#80967,#80968,#80969),(#80970,
#80971,#80972,#80973,#80974,#80975,#80976,#80977,#80978),(#80979,#80980,
#80981,#80982,#80983,#80984,#80985,#80986,#80987)),.UNSPECIFIED.,.F.,.F.,
 .F.,(6,3,6),(6,3,6),(1.97024157714,2.85861157082,3.64197819698),(0.,0.15,
0.3),.UNSPECIFIED.);
#1166=B_SPLINE_SURFACE_WITH_KNOTS('',5,5,((#81069,#81070,#81071,#81072,
#81073,#81074,#81075,#81076,#81077),(#81078,#81079,#81080,#81081,#81082,
#81083,#81084,#81085,#81086),(#81087,#81088,#81089,#81090,#81091,#81092,
#81093,#81094,#81095),(#81096,#81097,#81098,#81099,#81100,#81101,#81102,
#81103,#81104),(#81105,#81106,#81107,#81108,#81109,#81110,#81111,#81112,
#81113),(#81114,#81115,#81116,#81117,#81118,#81119,#81120,#81121,#81122),
(#81123,#81124,#81125,#81126,#81127,#81128,#81129,#81130,#81131),(#81132,
#81133,#81134,#81135,#81136,#81137,#81138,#81139,#81140),(#81141,#81142,
#81143,#81144,#81145,#81146,#81147,#81148,#81149)),.UNSPECIFIED.,.F.,.F.,
 .F.,(6,3,6),(6,3,6),(1.91124469448,2.8398573808,3.58302582769),(0.,0.15,
0.3),.UNSPECIFIED.);
#1167=B_SPLINE_SURFACE_WITH_KNOTS('',5,5,((#81243,#81244,#81245,#81246,
#81247,#81248),(#81249,#81250,#81251,#81252,#81253,#81254),(#81255,#81256,
#81257,#81258,#81259,#81260),(#81261,#81262,#81263,#81264,#81265,#81266),
(#81267,#81268,#81269,#81270,#81271,#81272),(#81273,#81274,#81275,#81276,
#81277,#81278),(#81279,#81280,#81281,#81282,#81283,#81284),(#81285,#81286,
#81287,#81288,#81289,#81290),(#81291,#81292,#81293,#81294,#81295,#81296)),
 .UNSPECIFIED.,.F.,.F.,.F.,(6,3,6),(6,6),(0.109166698395,1.13023412606,
2.1197288877),(0.,0.3),.UNSPECIFIED.);
#1168=B_SPLINE_SURFACE_WITH_KNOTS('',5,5,((#81385,#81386,#81387,#81388,
#81389,#81390,#81391,#81392,#81393),(#81394,#81395,#81396,#81397,#81398,
#81399,#81400,#81401,#81402),(#81403,#81404,#81405,#81406,#81407,#81408,
#81409,#81410,#81411),(#81412,#81413,#81414,#81415,#81416,#81417,#81418,
#81419,#81420),(#81421,#81422,#81423,#81424,#81425,#81426,#81427,#81428,
#81429),(#81430,#81431,#81432,#81433,#81434,#81435,#81436,#81437,#81438),
(#81439,#81440,#81441,#81442,#81443,#81444,#81445,#81446,#81447),(#81448,
#81449,#81450,#81451,#81452,#81453,#81454,#81455,#81456),(#81457,#81458,
#81459,#81460,#81461,#81462,#81463,#81464,#81465)),.UNSPECIFIED.,.F.,.F.,
 .F.,(6,3,6),(6,3,6),(2.21471914028,2.64235434316,3.16496476901),(0.,0.15,
0.3),.UNSPECIFIED.);
#1169=B_SPLINE_SURFACE_WITH_KNOTS('',5,5,((#81523,#81524,#81525,#81526,
#81527,#81528,#81529,#81530,#81531),(#81532,#81533,#81534,#81535,#81536,
#81537,#81538,#81539,#81540),(#81541,#81542,#81543,#81544,#81545,#81546,
#81547,#81548,#81549),(#81550,#81551,#81552,#81553,#81554,#81555,#81556,
#81557,#81558),(#81559,#81560,#81561,#81562,#81563,#81564,#81565,#81566,
#81567),(#81568,#81569,#81570,#81571,#81572,#81573,#81574,#81575,#81576),
(#81577,#81578,#81579,#81580,#81581,#81582,#81583,#81584,#81585),(#81586,
#81587,#81588,#81589,#81590,#81591,#81592,#81593,#81594),(#81595,#81596,
#81597,#81598,#81599,#81600,#81601,#81602,#81603)),.UNSPECIFIED.,.F.,.F.,
 .F.,(6,3,6),(6,3,6),(2.20468600976,2.64437519712,3.15494946669),(0.,0.15,
0.3),.UNSPECIFIED.);
#1170=B_SPLINE_SURFACE_WITH_KNOTS('',5,5,((#81743,#81744,#81745,#81746,
#81747,#81748,#81749,#81750,#81751),(#81752,#81753,#81754,#81755,#81756,
#81757,#81758,#81759,#81760),(#81761,#81762,#81763,#81764,#81765,#81766,
#81767,#81768,#81769),(#81770,#81771,#81772,#81773,#81774,#81775,#81776,
#81777,#81778),(#81779,#81780,#81781,#81782,#81783,#81784,#81785,#81786,
#81787),(#81788,#81789,#81790,#81791,#81792,#81793,#81794,#81795,#81796)),
 .UNSPECIFIED.,.F.,.F.,.F.,(6,6),(6,3,6),(1.4421658125425,1.77233951315641),
(-0.000123951336412412,0.15,0.3),.UNSPECIFIED.);
#1171=B_SPLINE_SURFACE_WITH_KNOTS('',5,5,((#81842,#81843,#81844,#81845,
#81846,#81847),(#81848,#81849,#81850,#81851,#81852,#81853),(#81854,#81855,
#81856,#81857,#81858,#81859),(#81860,#81861,#81862,#81863,#81864,#81865),
(#81866,#81867,#81868,#81869,#81870,#81871),(#81872,#81873,#81874,#81875,
#81876,#81877)),.UNSPECIFIED.,.F.,.F.,.F.,(6,6),(6,6),(1.49467475321184,
1.75483909752735),(-4.40481773546895E-5,0.3),.UNSPECIFIED.);
#1172=B_SPLINE_SURFACE_WITH_KNOTS('',5,5,((#81898,#81899,#81900,#81901,
#81902,#81903,#81904,#81905,#81906),(#81907,#81908,#81909,#81910,#81911,
#81912,#81913,#81914,#81915),(#81916,#81917,#81918,#81919,#81920,#81921,
#81922,#81923,#81924),(#81925,#81926,#81927,#81928,#81929,#81930,#81931,
#81932,#81933),(#81934,#81935,#81936,#81937,#81938,#81939,#81940,#81941,
#81942),(#81943,#81944,#81945,#81946,#81947,#81948,#81949,#81950,#81951)),
 .UNSPECIFIED.,.F.,.F.,.F.,(6,6),(6,3,6),(1.40783636987619,1.73804585327402),
(-0.000127187184019683,0.15,0.3),.UNSPECIFIED.);
#1173=B_SPLINE_SURFACE_WITH_KNOTS('',5,5,((#81966,#81967,#81968,#81969,
#81970,#81971),(#81972,#81973,#81974,#81975,#81976,#81977),(#81978,#81979,
#81980,#81981,#81982,#81983),(#81984,#81985,#81986,#81987,#81988,#81989),
(#81990,#81991,#81992,#81993,#81994,#81995),(#81996,#81997,#81998,#81999,
#82000,#82001)),.UNSPECIFIED.,.F.,.F.,.F.,(6,6),(6,6),(1.54690812238987,
1.80703488607013),(-4.43625301270991E-5,0.3),.UNSPECIFIED.);
#1174=B_SPLINE_SURFACE_WITH_KNOTS('',5,5,((#82309,#82310,#82311,#82312,
#82313,#82314),(#82315,#82316,#82317,#82318,#82319,#82320),(#82321,#82322,
#82323,#82324,#82325,#82326),(#82327,#82328,#82329,#82330,#82331,#82332),
(#82333,#82334,#82335,#82336,#82337,#82338),(#82339,#82340,#82341,#82342,
#82343,#82344),(#82345,#82346,#82347,#82348,#82349,#82350),(#82351,#82352,
#82353,#82354,#82355,#82356),(#82357,#82358,#82359,#82360,#82361,#82362)),
 .UNSPECIFIED.,.F.,.F.,.F.,(6,3,6),(6,6),(3.01269951131,3.90600477275,5.02326603963),
(0.,0.3),.UNSPECIFIED.);
#1175=B_SPLINE_SURFACE_WITH_KNOTS('',5,5,((#82489,#82490,#82491,#82492,
#82493,#82494),(#82495,#82496,#82497,#82498,#82499,#82500),(#82501,#82502,
#82503,#82504,#82505,#82506),(#82507,#82508,#82509,#82510,#82511,#82512),
(#82513,#82514,#82515,#82516,#82517,#82518),(#82519,#82520,#82521,#82522,
#82523,#82524)),.UNSPECIFIED.,.F.,.F.,.F.,(6,6),(6,6),(6.50394744106137,
7.33762762903),(-0.00162956260388768,0.301629563228629),.UNSPECIFIED.);
#1176=B_SPLINE_SURFACE_WITH_KNOTS('',5,5,((#82733,#82734,#82735,#82736,
#82737,#82738),(#82739,#82740,#82741,#82742,#82743,#82744),(#82745,#82746,
#82747,#82748,#82749,#82750),(#82751,#82752,#82753,#82754,#82755,#82756),
(#82757,#82758,#82759,#82760,#82761,#82762),(#82763,#82764,#82765,#82766,
#82767,#82768)),.UNSPECIFIED.,.F.,.F.,.F.,(6,6),(6,6),(5.20521075808,6.00042817873),
(0.,0.3),.UNSPECIFIED.);
#1177=B_SPLINE_SURFACE_WITH_KNOTS('',5,5,((#82781,#82782,#82783,#82784,
#82785,#82786),(#82787,#82788,#82789,#82790,#82791,#82792),(#82793,#82794,
#82795,#82796,#82797,#82798),(#82799,#82800,#82801,#82802,#82803,#82804),
(#82805,#82806,#82807,#82808,#82809,#82810),(#82811,#82812,#82813,#82814,
#82815,#82816),(#82817,#82818,#82819,#82820,#82821,#82822),(#82823,#82824,
#82825,#82826,#82827,#82828),(#82829,#82830,#82831,#82832,#82833,#82834)),
 .UNSPECIFIED.,.F.,.F.,.F.,(6,3,6),(6,6),(3.54900880514,4.18701109461,4.71575303852),
(0.,0.3),.UNSPECIFIED.);
#1178=B_SPLINE_SURFACE_WITH_KNOTS('',5,5,((#82991,#82992,#82993,#82994,
#82995,#82996),(#82997,#82998,#82999,#83000,#83001,#83002),(#83003,#83004,
#83005,#83006,#83007,#83008),(#83009,#83010,#83011,#83012,#83013,#83014),
(#83015,#83016,#83017,#83018,#83019,#83020),(#83021,#83022,#83023,#83024,
#83025,#83026)),.UNSPECIFIED.,.F.,.F.,.F.,(6,6),(6,6),(5.20484021909,5.76063633602),
(0.,0.3),.UNSPECIFIED.);
#1179=B_SPLINE_SURFACE_WITH_KNOTS('',5,5,((#83038,#83039,#83040,#83041,
#83042,#83043),(#83044,#83045,#83046,#83047,#83048,#83049),(#83050,#83051,
#83052,#83053,#83054,#83055),(#83056,#83057,#83058,#83059,#83060,#83061),
(#83062,#83063,#83064,#83065,#83066,#83067),(#83068,#83069,#83070,#83071,
#83072,#83073),(#83074,#83075,#83076,#83077,#83078,#83079),(#83080,#83081,
#83082,#83083,#83084,#83085),(#83086,#83087,#83088,#83089,#83090,#83091)),
 .UNSPECIFIED.,.F.,.F.,.F.,(6,3,6),(6,6),(3.54900880515,4.18701109461,4.71575303852),
(0.,0.3),.UNSPECIFIED.);
#1180=B_SPLINE_SURFACE_WITH_KNOTS('',5,5,((#83204,#83205,#83206,#83207,
#83208,#83209),(#83210,#83211,#83212,#83213,#83214,#83215),(#83216,#83217,
#83218,#83219,#83220,#83221),(#83222,#83223,#83224,#83225,#83226,#83227),
(#83228,#83229,#83230,#83231,#83232,#83233),(#83234,#83235,#83236,#83237,
#83238,#83239)),.UNSPECIFIED.,.F.,.F.,.F.,(6,6),(6,6),(1.9878298196,2.53578324996),
(0.,0.3),.UNSPECIFIED.);
#1181=B_SPLINE_SURFACE_WITH_KNOTS('',5,5,((#83241,#83242,#83243,#83244,
#83245,#83246),(#83247,#83248,#83249,#83250,#83251,#83252),(#83253,#83254,
#83255,#83256,#83257,#83258),(#83259,#83260,#83261,#83262,#83263,#83264),
(#83265,#83266,#83267,#83268,#83269,#83270),(#83271,#83272,#83273,#83274,
#83275,#83276)),.UNSPECIFIED.,.F.,.F.,.F.,(6,6),(6,6),(1.62679171178,4.14575432942),
(0.,0.3),.UNSPECIFIED.);
#1182=B_SPLINE_SURFACE_WITH_KNOTS('',5,5,((#83999,#84000,#84001,#84002,
#84003,#84004),(#84005,#84006,#84007,#84008,#84009,#84010),(#84011,#84012,
#84013,#84014,#84015,#84016),(#84017,#84018,#84019,#84020,#84021,#84022),
(#84023,#84024,#84025,#84026,#84027,#84028),(#84029,#84030,#84031,#84032,
#84033,#84034),(#84035,#84036,#84037,#84038,#84039,#84040),(#84041,#84042,
#84043,#84044,#84045,#84046),(#84047,#84048,#84049,#84050,#84051,#84052)),
 .UNSPECIFIED.,.F.,.F.,.F.,(6,3,6),(6,6),(1.66473273091,2.15120270837,2.76480988669),
(0.,0.3),.UNSPECIFIED.);
#1183=B_SPLINE_SURFACE_WITH_KNOTS('',2,5,((#84112,#84113,#84114,#84115,
#84116,#84117),(#84118,#84119,#84120,#84121,#84122,#84123),(#84124,#84125,
#84126,#84127,#84128,#84129)),.UNSPECIFIED.,.F.,.F.,.F.,(3,3),(6,6),(0.,
0.253192357174),(0.,0.3),.UNSPECIFIED.);
#1184=B_SPLINE_SURFACE_WITH_KNOTS('',5,5,((#84188,#84189,#84190,#84191,
#84192,#84193),(#84194,#84195,#84196,#84197,#84198,#84199),(#84200,#84201,
#84202,#84203,#84204,#84205),(#84206,#84207,#84208,#84209,#84210,#84211),
(#84212,#84213,#84214,#84215,#84216,#84217),(#84218,#84219,#84220,#84221,
#84222,#84223),(#84224,#84225,#84226,#84227,#84228,#84229),(#84230,#84231,
#84232,#84233,#84234,#84235),(#84236,#84237,#84238,#84239,#84240,#84241)),
 .UNSPECIFIED.,.F.,.F.,.F.,(6,3,6),(6,6),(1.53218389395,1.91811675676,2.24943434875),
(0.,0.3),.UNSPECIFIED.);
#1185=B_SPLINE_SURFACE_WITH_KNOTS('',5,5,((#84279,#84280,#84281,#84282,
#84283,#84284),(#84285,#84286,#84287,#84288,#84289,#84290),(#84291,#84292,
#84293,#84294,#84295,#84296),(#84297,#84298,#84299,#84300,#84301,#84302),
(#84303,#84304,#84305,#84306,#84307,#84308),(#84309,#84310,#84311,#84312,
#84313,#84314),(#84315,#84316,#84317,#84318,#84319,#84320),(#84321,#84322,
#84323,#84324,#84325,#84326),(#84327,#84328,#84329,#84330,#84331,#84332)),
 .UNSPECIFIED.,.F.,.F.,.F.,(6,3,6),(6,6),(2.14863240656,2.81847755741,3.42099781868),
(0.,0.3),.UNSPECIFIED.);
#1186=B_SPLINE_SURFACE_WITH_KNOTS('',4,5,((#84384,#84385,#84386,#84387,
#84388,#84389),(#84390,#84391,#84392,#84393,#84394,#84395),(#84396,#84397,
#84398,#84399,#84400,#84401),(#84402,#84403,#84404,#84405,#84406,#84407),
(#84408,#84409,#84410,#84411,#84412,#84413)),.UNSPECIFIED.,.F.,.F.,.F.,
(5,5),(6,6),(1.5664121072,1.61647585835),(0.,0.3),.UNSPECIFIED.);
#1187=B_SPLINE_SURFACE_WITH_KNOTS('',5,5,((#84507,#84508,#84509,#84510,
#84511,#84512),(#84513,#84514,#84515,#84516,#84517,#84518),(#84519,#84520,
#84521,#84522,#84523,#84524),(#84525,#84526,#84527,#84528,#84529,#84530),
(#84531,#84532,#84533,#84534,#84535,#84536),(#84537,#84538,#84539,#84540,
#84541,#84542),(#84543,#84544,#84545,#84546,#84547,#84548),(#84549,#84550,
#84551,#84552,#84553,#84554),(#84555,#84556,#84557,#84558,#84559,#84560)),
 .UNSPECIFIED.,.F.,.F.,.F.,(6,3,6),(6,6),(1.66473273091,2.15120270837,2.76480988669),
(0.,0.3),.UNSPECIFIED.);
#1188=B_SPLINE_SURFACE_WITH_KNOTS('',2,5,((#84566,#84567,#84568,#84569,
#84570,#84571),(#84572,#84573,#84574,#84575,#84576,#84577),(#84578,#84579,
#84580,#84581,#84582,#84583)),.UNSPECIFIED.,.F.,.F.,.F.,(3,3),(6,6),(0.,
0.253192357174),(0.,0.3),.UNSPECIFIED.);
#1189=B_SPLINE_SURFACE_WITH_KNOTS('',5,5,((#84679,#84680,#84681,#84682,
#84683,#84684),(#84685,#84686,#84687,#84688,#84689,#84690),(#84691,#84692,
#84693,#84694,#84695,#84696),(#84697,#84698,#84699,#84700,#84701,#84702),
(#84703,#84704,#84705,#84706,#84707,#84708),(#84709,#84710,#84711,#84712,
#84713,#84714),(#84715,#84716,#84717,#84718,#84719,#84720),(#84721,#84722,
#84723,#84724,#84725,#84726),(#84727,#84728,#84729,#84730,#84731,#84732)),
 .UNSPECIFIED.,.F.,.F.,.F.,(6,3,6),(6,6),(1.53218389395,1.91811675676,2.24943434875),
(0.,0.3),.UNSPECIFIED.);
#1190=B_SPLINE_SURFACE_WITH_KNOTS('',5,5,((#84767,#84768,#84769,#84770,
#84771,#84772),(#84773,#84774,#84775,#84776,#84777,#84778),(#84779,#84780,
#84781,#84782,#84783,#84784),(#84785,#84786,#84787,#84788,#84789,#84790),
(#84791,#84792,#84793,#84794,#84795,#84796),(#84797,#84798,#84799,#84800,
#84801,#84802),(#84803,#84804,#84805,#84806,#84807,#84808),(#84809,#84810,
#84811,#84812,#84813,#84814),(#84815,#84816,#84817,#84818,#84819,#84820)),
 .UNSPECIFIED.,.F.,.F.,.F.,(6,3,6),(6,6),(2.14863240656,2.81847755741,3.42099781868),
(0.,0.3),.UNSPECIFIED.);
#1191=B_SPLINE_SURFACE_WITH_KNOTS('',4,5,((#84872,#84873,#84874,#84875,
#84876,#84877),(#84878,#84879,#84880,#84881,#84882,#84883),(#84884,#84885,
#84886,#84887,#84888,#84889),(#84890,#84891,#84892,#84893,#84894,#84895),
(#84896,#84897,#84898,#84899,#84900,#84901)),.UNSPECIFIED.,.F.,.F.,.F.,
(5,5),(6,6),(1.5664121072,1.61647585835),(0.,0.3),.UNSPECIFIED.);
#1192=B_SPLINE_SURFACE_WITH_KNOTS('',5,5,((#86287,#86288,#86289,#86290,
#86291,#86292),(#86293,#86294,#86295,#86296,#86297,#86298),(#86299,#86300,
#86301,#86302,#86303,#86304),(#86305,#86306,#86307,#86308,#86309,#86310),
(#86311,#86312,#86313,#86314,#86315,#86316),(#86317,#86318,#86319,#86320,
#86321,#86322),(#86323,#86324,#86325,#86326,#86327,#86328),(#86329,#86330,
#86331,#86332,#86333,#86334),(#86335,#86336,#86337,#86338,#86339,#86340)),
 .UNSPECIFIED.,.F.,.F.,.F.,(6,3,6),(6,6),(1.75158458902,2.2812742412,2.90384942405),
(0.,0.3),.UNSPECIFIED.);
#1193=B_SPLINE_SURFACE_WITH_KNOTS('',5,5,((#86882,#86883,#86884,#86885,
#86886,#86887),(#86888,#86889,#86890,#86891,#86892,#86893),(#86894,#86895,
#86896,#86897,#86898,#86899),(#86900,#86901,#86902,#86903,#86904,#86905),
(#86906,#86907,#86908,#86909,#86910,#86911),(#86912,#86913,#86914,#86915,
#86916,#86917)),.UNSPECIFIED.,.F.,.F.,.F.,(6,6),(6,6),(1.0735101225,1.1089775272),
(0.,0.1),.UNSPECIFIED.);
#1194=B_SPLINE_SURFACE_WITH_KNOTS('',5,5,((#86931,#86932,#86933,#86934,
#86935,#86936),(#86937,#86938,#86939,#86940,#86941,#86942),(#86943,#86944,
#86945,#86946,#86947,#86948),(#86949,#86950,#86951,#86952,#86953,#86954),
(#86955,#86956,#86957,#86958,#86959,#86960),(#86961,#86962,#86963,#86964,
#86965,#86966)),.UNSPECIFIED.,.F.,.F.,.F.,(6,6),(6,6),(1.62703155549,1.68203627825),
(0.,0.1),.UNSPECIFIED.);
#1195=B_SPLINE_SURFACE_WITH_KNOTS('',5,5,((#86972,#86973,#86974,#86975,
#86976,#86977),(#86978,#86979,#86980,#86981,#86982,#86983),(#86984,#86985,
#86986,#86987,#86988,#86989),(#86990,#86991,#86992,#86993,#86994,#86995),
(#86996,#86997,#86998,#86999,#87000,#87001),(#87002,#87003,#87004,#87005,
#87006,#87007)),.UNSPECIFIED.,.F.,.F.,.F.,(6,6),(6,6),(0.205332243373231,
0.603435556801337),(-5.32516463369809E-5,0.1),.UNSPECIFIED.);
#1196=B_SPLINE_SURFACE_WITH_KNOTS('',4,5,((#87038,#87039,#87040,#87041,
#87042,#87043),(#87044,#87045,#87046,#87047,#87048,#87049),(#87050,#87051,
#87052,#87053,#87054,#87055),(#87056,#87057,#87058,#87059,#87060,#87061),
(#87062,#87063,#87064,#87065,#87066,#87067)),.UNSPECIFIED.,.F.,.F.,.F.,
(5,5),(6,6),(2.44731088148,2.46511887948),(0.,0.1),.UNSPECIFIED.);
#1197=B_SPLINE_SURFACE_WITH_KNOTS('',5,5,((#87090,#87091,#87092,#87093,
#87094,#87095),(#87096,#87097,#87098,#87099,#87100,#87101),(#87102,#87103,
#87104,#87105,#87106,#87107),(#87108,#87109,#87110,#87111,#87112,#87113),
(#87114,#87115,#87116,#87117,#87118,#87119),(#87120,#87121,#87122,#87123,
#87124,#87125)),.UNSPECIFIED.,.F.,.F.,.F.,(6,6),(6,6),(1.62703155549,1.68203627825),
(0.,0.1),.UNSPECIFIED.);
#1198=B_SPLINE_SURFACE_WITH_KNOTS('',5,5,((#87131,#87132,#87133,#87134,
#87135,#87136),(#87137,#87138,#87139,#87140,#87141,#87142),(#87143,#87144,
#87145,#87146,#87147,#87148),(#87149,#87150,#87151,#87152,#87153,#87154),
(#87155,#87156,#87157,#87158,#87159,#87160),(#87161,#87162,#87163,#87164,
#87165,#87166)),.UNSPECIFIED.,.F.,.F.,.F.,(6,6),(6,6),(0.205332100976151,
0.60343837439054),(-5.32318455396895E-5,0.1),.UNSPECIFIED.);
#1199=B_SPLINE_SURFACE_WITH_KNOTS('',5,5,((#87197,#87198,#87199,#87200,
#87201,#87202),(#87203,#87204,#87205,#87206,#87207,#87208),(#87209,#87210,
#87211,#87212,#87213,#87214),(#87215,#87216,#87217,#87218,#87219,#87220),
(#87221,#87222,#87223,#87224,#87225,#87226),(#87227,#87228,#87229,#87230,
#87231,#87232)),.UNSPECIFIED.,.F.,.F.,.F.,(6,6),(6,6),(2.44531347319,2.50031756413),
(0.,0.1),.UNSPECIFIED.);
#1200=B_SPLINE_SURFACE_WITH_KNOTS('',5,5,((#88026,#88027,#88028,#88029,
#88030,#88031),(#88032,#88033,#88034,#88035,#88036,#88037),(#88038,#88039,
#88040,#88041,#88042,#88043),(#88044,#88045,#88046,#88047,#88048,#88049),
(#88050,#88051,#88052,#88053,#88054,#88055),(#88056,#88057,#88058,#88059,
#88060,#88061),(#88062,#88063,#88064,#88065,#88066,#88067),(#88068,#88069,
#88070,#88071,#88072,#88073),(#88074,#88075,#88076,#88077,#88078,#88079)),
 .UNSPECIFIED.,.F.,.F.,.F.,(6,3,6),(6,6),(2.86241645295004,3.3764526533,
4.04046842116996),(0.,0.300992369259961),.UNSPECIFIED.);
#1201=B_SPLINE_SURFACE_WITH_KNOTS('',5,5,((#88128,#88129,#88130,#88131,
#88132,#88133),(#88134,#88135,#88136,#88137,#88138,#88139),(#88140,#88141,
#88142,#88143,#88144,#88145),(#88146,#88147,#88148,#88149,#88150,#88151),
(#88152,#88153,#88154,#88155,#88156,#88157),(#88158,#88159,#88160,#88161,
#88162,#88163),(#88164,#88165,#88166,#88167,#88168,#88169),(#88170,#88171,
#88172,#88173,#88174,#88175),(#88176,#88177,#88178,#88179,#88180,#88181)),
 .UNSPECIFIED.,.F.,.F.,.F.,(6,3,6),(6,6),(4.76185240083,5.31344541544,5.93786871511),
(0.,0.3),.UNSPECIFIED.);
#1202=B_SPLINE_SURFACE_WITH_KNOTS('',5,5,((#88250,#88251,#88252,#88253,
#88254,#88255),(#88256,#88257,#88258,#88259,#88260,#88261),(#88262,#88263,
#88264,#88265,#88266,#88267),(#88268,#88269,#88270,#88271,#88272,#88273),
(#88274,#88275,#88276,#88277,#88278,#88279),(#88280,#88281,#88282,#88283,
#88284,#88285),(#88286,#88287,#88288,#88289,#88290,#88291),(#88292,#88293,
#88294,#88295,#88296,#88297),(#88298,#88299,#88300,#88301,#88302,#88303)),
 .UNSPECIFIED.,.F.,.F.,.F.,(6,3,6),(6,6),(1.64208556101,2.12883652195,2.73162696034),
(0.,0.3),.UNSPECIFIED.);
#1203=B_SPLINE_SURFACE_WITH_KNOTS('',5,5,((#88685,#88686,#88687,#88688,
#88689,#88690),(#88691,#88692,#88693,#88694,#88695,#88696),(#88697,#88698,
#88699,#88700,#88701,#88702),(#88703,#88704,#88705,#88706,#88707,#88708),
(#88709,#88710,#88711,#88712,#88713,#88714),(#88715,#88716,#88717,#88718,
#88719,#88720)),.UNSPECIFIED.,.F.,.F.,.F.,(6,6),(6,6),(0.138174465866154,
1.09237668281),(-0.000329517642285316,0.3),.UNSPECIFIED.);
#1204=B_SPLINE_SURFACE_WITH_KNOTS('',5,5,((#88985,#88986,#88987,#88988,
#88989,#88990),(#88991,#88992,#88993,#88994,#88995,#88996),(#88997,#88998,
#88999,#89000,#89001,#89002),(#89003,#89004,#89005,#89006,#89007,#89008),
(#89009,#89010,#89011,#89012,#89013,#89014),(#89015,#89016,#89017,#89018,
#89019,#89020),(#89021,#89022,#89023,#89024,#89025,#89026),(#89027,#89028,
#89029,#89030,#89031,#89032),(#89033,#89034,#89035,#89036,#89037,#89038),
(#89039,#89040,#89041,#89042,#89043,#89044),(#89045,#89046,#89047,#89048,
#89049,#89050),(#89051,#89052,#89053,#89054,#89055,#89056),(#89057,#89058,
#89059,#89060,#89061,#89062),(#89063,#89064,#89065,#89066,#89067,#89068),
(#89069,#89070,#89071,#89072,#89073,#89074),(#89075,#89076,#89077,#89078,
#89079,#89080),(#89081,#89082,#89083,#89084,#89085,#89086),(#89087,#89088,
#89089,#89090,#89091,#89092)),.UNSPECIFIED.,.F.,.F.,.F.,(6,3,3,3,3,6),(6,
6),(0.,0.630653457813,0.794370029612,0.931886828419,1.04715733204,1.10981746796917),
(0.,0.300159997979174),.UNSPECIFIED.);
#1205=B_SPLINE_SURFACE_WITH_KNOTS('',5,5,((#89179,#89180,#89181,#89182,
#89183,#89184),(#89185,#89186,#89187,#89188,#89189,#89190),(#89191,#89192,
#89193,#89194,#89195,#89196),(#89197,#89198,#89199,#89200,#89201,#89202),
(#89203,#89204,#89205,#89206,#89207,#89208),(#89209,#89210,#89211,#89212,
#89213,#89214),(#89215,#89216,#89217,#89218,#89219,#89220),(#89221,#89222,
#89223,#89224,#89225,#89226),(#89227,#89228,#89229,#89230,#89231,#89232)),
 .UNSPECIFIED.,.F.,.F.,.F.,(6,3,6),(6,6),(0.,0.323534265941,0.647068531882),
(0.,0.538062533561),.UNSPECIFIED.);
#1206=B_SPLINE_SURFACE_WITH_KNOTS('',5,5,((#89332,#89333,#89334,#89335,
#89336,#89337),(#89338,#89339,#89340,#89341,#89342,#89343),(#89344,#89345,
#89346,#89347,#89348,#89349),(#89350,#89351,#89352,#89353,#89354,#89355),
(#89356,#89357,#89358,#89359,#89360,#89361),(#89362,#89363,#89364,#89365,
#89366,#89367)),.UNSPECIFIED.,.F.,.F.,.F.,(6,6),(6,6),(2.77894816417,3.04318822375),
(0.,0.3),.UNSPECIFIED.);
#1207=B_SPLINE_SURFACE_WITH_KNOTS('',5,5,((#89373,#89374,#89375,#89376,
#89377,#89378),(#89379,#89380,#89381,#89382,#89383,#89384),(#89385,#89386,
#89387,#89388,#89389,#89390),(#89391,#89392,#89393,#89394,#89395,#89396),
(#89397,#89398,#89399,#89400,#89401,#89402),(#89403,#89404,#89405,#89406,
#89407,#89408),(#89409,#89410,#89411,#89412,#89413,#89414),(#89415,#89416,
#89417,#89418,#89419,#89420),(#89421,#89422,#89423,#89424,#89425,#89426)),
 .UNSPECIFIED.,.F.,.F.,.F.,(6,3,6),(6,6),(1.25405163269,1.6430233414,2.19239180857),
(0.,0.3),.UNSPECIFIED.);
#1208=B_SPLINE_SURFACE_WITH_KNOTS('',5,5,((#89440,#89441,#89442,#89443,
#89444,#89445),(#89446,#89447,#89448,#89449,#89450,#89451),(#89452,#89453,
#89454,#89455,#89456,#89457),(#89458,#89459,#89460,#89461,#89462,#89463),
(#89464,#89465,#89466,#89467,#89468,#89469),(#89470,#89471,#89472,#89473,
#89474,#89475),(#89476,#89477,#89478,#89479,#89480,#89481),(#89482,#89483,
#89484,#89485,#89486,#89487),(#89488,#89489,#89490,#89491,#89492,#89493)),
 .UNSPECIFIED.,.F.,.F.,.F.,(6,3,6),(6,6),(1.69812247662,2.37608580106,2.83469359842),
(0.,0.3),.UNSPECIFIED.);
#1209=B_SPLINE_SURFACE_WITH_KNOTS('',5,5,((#89507,#89508,#89509,#89510,
#89511,#89512),(#89513,#89514,#89515,#89516,#89517,#89518),(#89519,#89520,
#89521,#89522,#89523,#89524),(#89525,#89526,#89527,#89528,#89529,#89530),
(#89531,#89532,#89533,#89534,#89535,#89536),(#89537,#89538,#89539,#89540,
#89541,#89542)),.UNSPECIFIED.,.F.,.F.,.F.,(6,6),(6,6),(1.6338579571,2.7257140478),
(0.,0.3),.UNSPECIFIED.);
#1210=B_SPLINE_SURFACE_WITH_KNOTS('',5,5,((#89651,#89652,#89653,#89654,
#89655,#89656),(#89657,#89658,#89659,#89660,#89661,#89662),(#89663,#89664,
#89665,#89666,#89667,#89668),(#89669,#89670,#89671,#89672,#89673,#89674),
(#89675,#89676,#89677,#89678,#89679,#89680),(#89681,#89682,#89683,#89684,
#89685,#89686),(#89687,#89688,#89689,#89690,#89691,#89692),(#89693,#89694,
#89695,#89696,#89697,#89698),(#89699,#89700,#89701,#89702,#89703,#89704)),
 .UNSPECIFIED.,.F.,.F.,.F.,(6,3,6),(6,6),(1.37442826527,1.83079344184,2.19966814328),
(0.,0.3),.UNSPECIFIED.);
#1211=B_SPLINE_SURFACE_WITH_KNOTS('',5,5,((#89748,#89749,#89750,#89751,
#89752,#89753),(#89754,#89755,#89756,#89757,#89758,#89759),(#89760,#89761,
#89762,#89763,#89764,#89765),(#89766,#89767,#89768,#89769,#89770,#89771),
(#89772,#89773,#89774,#89775,#89776,#89777),(#89778,#89779,#89780,#89781,
#89782,#89783)),.UNSPECIFIED.,.F.,.F.,.F.,(6,6),(6,6),(1.66778051169,1.825176882),
(0.,0.3),.UNSPECIFIED.);
#1212=B_SPLINE_SURFACE_WITH_KNOTS('',5,5,((#89821,#89822,#89823,#89824,
#89825,#89826),(#89827,#89828,#89829,#89830,#89831,#89832),(#89833,#89834,
#89835,#89836,#89837,#89838),(#89839,#89840,#89841,#89842,#89843,#89844),
(#89845,#89846,#89847,#89848,#89849,#89850),(#89851,#89852,#89853,#89854,
#89855,#89856)),.UNSPECIFIED.,.F.,.F.,.F.,(6,6),(6,6),(1.19509008928,1.27929234824),
(0.,0.3),.UNSPECIFIED.);
#1213=B_SPLINE_SURFACE_WITH_KNOTS('',5,5,((#89860,#89861,#89862,#89863,
#89864,#89865),(#89866,#89867,#89868,#89869,#89870,#89871),(#89872,#89873,
#89874,#89875,#89876,#89877),(#89878,#89879,#89880,#89881,#89882,#89883),
(#89884,#89885,#89886,#89887,#89888,#89889),(#89890,#89891,#89892,#89893,
#89894,#89895)),.UNSPECIFIED.,.F.,.F.,.F.,(6,6),(6,6),(0.176101352323,1.24191828283),
(0.,0.3),.UNSPECIFIED.);
#1214=B_SPLINE_SURFACE_WITH_KNOTS('',5,5,((#90678,#90679,#90680,#90681,
#90682,#90683),(#90684,#90685,#90686,#90687,#90688,#90689),(#90690,#90691,
#90692,#90693,#90694,#90695),(#90696,#90697,#90698,#90699,#90700,#90701),
(#90702,#90703,#90704,#90705,#90706,#90707),(#90708,#90709,#90710,#90711,
#90712,#90713)),.UNSPECIFIED.,.F.,.F.,.F.,(6,6),(6,6),(0.,0.788174979856),
(0.,1.),.UNSPECIFIED.);
#1215=B_SPLINE_SURFACE_WITH_KNOTS('',5,5,((#90776,#90777,#90778,#90779,
#90780,#90781),(#90782,#90783,#90784,#90785,#90786,#90787),(#90788,#90789,
#90790,#90791,#90792,#90793),(#90794,#90795,#90796,#90797,#90798,#90799),
(#90800,#90801,#90802,#90803,#90804,#90805),(#90806,#90807,#90808,#90809,
#90810,#90811),(#90812,#90813,#90814,#90815,#90816,#90817),(#90818,#90819,
#90820,#90821,#90822,#90823),(#90824,#90825,#90826,#90827,#90828,#90829),
(#90830,#90831,#90832,#90833,#90834,#90835),(#90836,#90837,#90838,#90839,
#90840,#90841),(#90842,#90843,#90844,#90845,#90846,#90847)),
 .UNSPECIFIED.,.F.,.F.,.F.,(6,3,3,6),(6,6),(0.144241926362,0.436612428829,
0.752300010655,1.24832448076),(0.,3.),.UNSPECIFIED.);
#1216=B_SPLINE_SURFACE_WITH_KNOTS('',5,5,((#91395,#91396,#91397,#91398,
#91399,#91400),(#91401,#91402,#91403,#91404,#91405,#91406),(#91407,#91408,
#91409,#91410,#91411,#91412),(#91413,#91414,#91415,#91416,#91417,#91418),
(#91419,#91420,#91421,#91422,#91423,#91424),(#91425,#91426,#91427,#91428,
#91429,#91430)),.UNSPECIFIED.,.F.,.F.,.F.,(6,6),(6,6),(5.32377368294E-13,
0.720782737349),(0.,1.),.UNSPECIFIED.);
#1217=B_SPLINE_SURFACE_WITH_KNOTS('',5,5,((#91495,#91496,#91497,#91498,
#91499,#91500),(#91501,#91502,#91503,#91504,#91505,#91506),(#91507,#91508,
#91509,#91510,#91511,#91512),(#91513,#91514,#91515,#91516,#91517,#91518),
(#91519,#91520,#91521,#91522,#91523,#91524),(#91525,#91526,#91527,#91528,
#91529,#91530),(#91531,#91532,#91533,#91534,#91535,#91536),(#91537,#91538,
#91539,#91540,#91541,#91542),(#91543,#91544,#91545,#91546,#91547,#91548)),
 .UNSPECIFIED.,.F.,.F.,.F.,(6,3,6),(6,6),(1.75158458902,2.2812742412,2.90384942405),
(0.,0.3),.UNSPECIFIED.);
#1218=B_SPLINE_SURFACE_WITH_KNOTS('',4,5,((#92139,#92140,#92141,#92142,
#92143,#92144),(#92145,#92146,#92147,#92148,#92149,#92150),(#92151,#92152,
#92153,#92154,#92155,#92156),(#92157,#92158,#92159,#92160,#92161,#92162),
(#92163,#92164,#92165,#92166,#92167,#92168)),.UNSPECIFIED.,.F.,.F.,.F.,
(5,5),(6,6),(1.00826496187,1.04373195388),(0.,0.1),.UNSPECIFIED.);
#1219=B_SPLINE_SURFACE_WITH_KNOTS('',5,5,((#92182,#92183,#92184,#92185,
#92186,#92187),(#92188,#92189,#92190,#92191,#92192,#92193),(#92194,#92195,
#92196,#92197,#92198,#92199),(#92200,#92201,#92202,#92203,#92204,#92205),
(#92206,#92207,#92208,#92209,#92210,#92211),(#92212,#92213,#92214,#92215,
#92216,#92217)),.UNSPECIFIED.,.F.,.F.,.F.,(6,6),(6,6),(2.44531347353,2.50031756447),
(0.,0.1),.UNSPECIFIED.);
#1220=B_SPLINE_SURFACE_WITH_KNOTS('',5,5,((#92223,#92224,#92225,#92226,
#92227,#92228),(#92229,#92230,#92231,#92232,#92233,#92234),(#92235,#92236,
#92237,#92238,#92239,#92240),(#92241,#92242,#92243,#92244,#92245,#92246),
(#92247,#92248,#92249,#92250,#92251,#92252),(#92253,#92254,#92255,#92256,
#92257,#92258)),.UNSPECIFIED.,.F.,.F.,.F.,(6,6),(6,6),(0.205331513734207,
0.603439035907376),(-5.33254607926776E-5,0.1),.UNSPECIFIED.);
#1221=B_SPLINE_SURFACE_WITH_KNOTS('',3,5,((#92289,#92290,#92291,#92292,
#92293,#92294),(#92295,#92296,#92297,#92298,#92299,#92300),(#92301,#92302,
#92303,#92304,#92305,#92306),(#92307,#92308,#92309,#92310,#92311,#92312)),
 .UNSPECIFIED.,.F.,.F.,.F.,(4,4),(6,6),(1.66422823568,1.68203627824),(0.,
0.1),.UNSPECIFIED.);
#1222=B_SPLINE_SURFACE_WITH_KNOTS('',5,5,((#92338,#92339,#92340,#92341,
#92342,#92343),(#92344,#92345,#92346,#92347,#92348,#92349),(#92350,#92351,
#92352,#92353,#92354,#92355),(#92356,#92357,#92358,#92359,#92360,#92361),
(#92362,#92363,#92364,#92365,#92366,#92367),(#92368,#92369,#92370,#92371,
#92372,#92373)),.UNSPECIFIED.,.F.,.F.,.F.,(6,6),(6,6),(2.4453134732,2.50031756414),
(0.,0.1),.UNSPECIFIED.);
#1223=B_SPLINE_SURFACE_WITH_KNOTS('',5,5,((#92379,#92380,#92381,#92382,
#92383,#92384),(#92385,#92386,#92387,#92388,#92389,#92390),(#92391,#92392,
#92393,#92394,#92395,#92396),(#92397,#92398,#92399,#92400,#92401,#92402),
(#92403,#92404,#92405,#92406,#92407,#92408),(#92409,#92410,#92411,#92412,
#92413,#92414)),.UNSPECIFIED.,.F.,.F.,.F.,(6,6),(6,6),(0.205331513735948,
0.603439035886987),(-5.3325460052425E-5,0.1),.UNSPECIFIED.);
#1224=B_SPLINE_SURFACE_WITH_KNOTS('',5,5,((#92445,#92446,#92447,#92448,
#92449,#92450),(#92451,#92452,#92453,#92454,#92455,#92456),(#92457,#92458,
#92459,#92460,#92461,#92462),(#92463,#92464,#92465,#92466,#92467,#92468),
(#92469,#92470,#92471,#92472,#92473,#92474),(#92475,#92476,#92477,#92478,
#92479,#92480)),.UNSPECIFIED.,.F.,.F.,.F.,(6,6),(6,6),(1.6270315555,1.68203627826),
(0.,0.1),.UNSPECIFIED.);
#1225=B_SPLINE_SURFACE_WITH_KNOTS('',5,5,((#93064,#93065,#93066,#93067,
#93068,#93069),(#93070,#93071,#93072,#93073,#93074,#93075),(#93076,#93077,
#93078,#93079,#93080,#93081),(#93082,#93083,#93084,#93085,#93086,#93087),
(#93088,#93089,#93090,#93091,#93092,#93093),(#93094,#93095,#93096,#93097,
#93098,#93099)),.UNSPECIFIED.,.F.,.F.,.F.,(6,6),(6,6),(0.,0.833577451733),
(0.,1.),.UNSPECIFIED.);
#1226=B_SPLINE_SURFACE_WITH_KNOTS('',5,5,((#93322,#93323,#93324,#93325,
#93326,#93327),(#93328,#93329,#93330,#93331,#93332,#93333),(#93334,#93335,
#93336,#93337,#93338,#93339),(#93340,#93341,#93342,#93343,#93344,#93345),
(#93346,#93347,#93348,#93349,#93350,#93351),(#93352,#93353,#93354,#93355,
#93356,#93357),(#93358,#93359,#93360,#93361,#93362,#93363),(#93364,#93365,
#93366,#93367,#93368,#93369),(#93370,#93371,#93372,#93373,#93374,#93375),
(#93376,#93377,#93378,#93379,#93380,#93381),(#93382,#93383,#93384,#93385,
#93386,#93387),(#93388,#93389,#93390,#93391,#93392,#93393),(#93394,#93395,
#93396,#93397,#93398,#93399),(#93400,#93401,#93402,#93403,#93404,#93405),
(#93406,#93407,#93408,#93409,#93410,#93411)),.UNSPECIFIED.,.F.,.F.,.F.,
(6,3,3,3,6),(6,6),(0.,0.314441419907,0.663953725274,0.811338767061,1.10181448416),
(0.,3.),.UNSPECIFIED.);
#1227=B_SPLINE_SURFACE_WITH_KNOTS('',5,5,((#93576,#93577,#93578,#93579,
#93580,#93581),(#93582,#93583,#93584,#93585,#93586,#93587),(#93588,#93589,
#93590,#93591,#93592,#93593),(#93594,#93595,#93596,#93597,#93598,#93599),
(#93600,#93601,#93602,#93603,#93604,#93605),(#93606,#93607,#93608,#93609,
#93610,#93611),(#93612,#93613,#93614,#93615,#93616,#93617),(#93618,#93619,
#93620,#93621,#93622,#93623),(#93624,#93625,#93626,#93627,#93628,#93629)),
 .UNSPECIFIED.,.F.,.F.,.F.,(6,3,6),(6,6),(2.86340882221,3.3764526533,4.03947605191),
(0.,0.3),.UNSPECIFIED.);
#1228=B_SPLINE_SURFACE_WITH_KNOTS('',5,5,((#93696,#93697,#93698,#93699,
#93700,#93701),(#93702,#93703,#93704,#93705,#93706,#93707),(#93708,#93709,
#93710,#93711,#93712,#93713),(#93714,#93715,#93716,#93717,#93718,#93719),
(#93720,#93721,#93722,#93723,#93724,#93725),(#93726,#93727,#93728,#93729,
#93730,#93731),(#93732,#93733,#93734,#93735,#93736,#93737),(#93738,#93739,
#93740,#93741,#93742,#93743),(#93744,#93745,#93746,#93747,#93748,#93749)),
 .UNSPECIFIED.,.F.,.F.,.F.,(6,3,6),(6,6),(4.76185240083,5.31344541544,5.93786871511),
(0.,0.3),.UNSPECIFIED.);
#1229=B_SPLINE_SURFACE_WITH_KNOTS('',5,5,((#93875,#93876,#93877,#93878,
#93879,#93880),(#93881,#93882,#93883,#93884,#93885,#93886),(#93887,#93888,
#93889,#93890,#93891,#93892),(#93893,#93894,#93895,#93896,#93897,#93898),
(#93899,#93900,#93901,#93902,#93903,#93904),(#93905,#93906,#93907,#93908,
#93909,#93910),(#93911,#93912,#93913,#93914,#93915,#93916),(#93917,#93918,
#93919,#93920,#93921,#93922),(#93923,#93924,#93925,#93926,#93927,#93928)),
 .UNSPECIFIED.,.F.,.F.,.F.,(6,3,6),(6,6),(1.64208556101,2.12883652195,2.73162696034),
(0.,0.3),.UNSPECIFIED.);
#1230=B_SPLINE_SURFACE_WITH_KNOTS('',5,5,((#94274,#94275,#94276,#94277,
#94278,#94279),(#94280,#94281,#94282,#94283,#94284,#94285),(#94286,#94287,
#94288,#94289,#94290,#94291),(#94292,#94293,#94294,#94295,#94296,#94297),
(#94298,#94299,#94300,#94301,#94302,#94303),(#94304,#94305,#94306,#94307,
#94308,#94309)),.UNSPECIFIED.,.F.,.F.,.F.,(6,6),(6,6),(0.138284020234617,
1.09237668281),(0.,0.300010819481383),.UNSPECIFIED.);
#1231=B_SPLINE_SURFACE_WITH_KNOTS('',4,5,((#94593,#94594,#94595,#94596,
#94597,#94598),(#94599,#94600,#94601,#94602,#94603,#94604),(#94605,#94606,
#94607,#94608,#94609,#94610),(#94611,#94612,#94613,#94614,#94615,#94616),
(#94617,#94618,#94619,#94620,#94621,#94622)),.UNSPECIFIED.,.F.,.F.,.F.,
(5,5),(6,6),(8.31692747129E-16,0.70510501139),(0.,1.),.UNSPECIFIED.);
#1232=B_SPLINE_SURFACE_WITH_KNOTS('',5,5,((#94701,#94702,#94703,#94704,
#94705,#94706),(#94707,#94708,#94709,#94710,#94711,#94712),(#94713,#94714,
#94715,#94716,#94717,#94718),(#94719,#94720,#94721,#94722,#94723,#94724),
(#94725,#94726,#94727,#94728,#94729,#94730),(#94731,#94732,#94733,#94734,
#94735,#94736),(#94737,#94738,#94739,#94740,#94741,#94742),(#94743,#94744,
#94745,#94746,#94747,#94748),(#94749,#94750,#94751,#94752,#94753,#94754),
(#94755,#94756,#94757,#94758,#94759,#94760),(#94761,#94762,#94763,#94764,
#94765,#94766),(#94767,#94768,#94769,#94770,#94771,#94772),(#94773,#94774,
#94775,#94776,#94777,#94778),(#94779,#94780,#94781,#94782,#94783,#94784),
(#94785,#94786,#94787,#94788,#94789,#94790),(#94791,#94792,#94793,#94794,
#94795,#94796),(#94797,#94798,#94799,#94800,#94801,#94802),(#94803,#94804,
#94805,#94806,#94807,#94808)),.UNSPECIFIED.,.F.,.F.,.F.,(6,3,3,3,3,6),(6,
6),(0.,0.630653457813,0.794370029612,0.931886828419,1.04715733204,1.10965746999),
(0.,0.3),.UNSPECIFIED.);
#1233=B_SPLINE_SURFACE_WITH_KNOTS('',5,5,((#94849,#94850,#94851,#94852,
#94853,#94854),(#94855,#94856,#94857,#94858,#94859,#94860),(#94861,#94862,
#94863,#94864,#94865,#94866),(#94867,#94868,#94869,#94870,#94871,#94872),
(#94873,#94874,#94875,#94876,#94877,#94878),(#94879,#94880,#94881,#94882,
#94883,#94884),(#94885,#94886,#94887,#94888,#94889,#94890),(#94891,#94892,
#94893,#94894,#94895,#94896),(#94897,#94898,#94899,#94900,#94901,#94902)),
 .UNSPECIFIED.,.F.,.F.,.F.,(6,3,6),(6,6),(0.,0.323534265941,0.647068531882),
(0.,0.538062533561),.UNSPECIFIED.);
#1234=B_SPLINE_SURFACE_WITH_KNOTS('',5,5,((#94932,#94933,#94934,#94935,
#94936,#94937),(#94938,#94939,#94940,#94941,#94942,#94943),(#94944,#94945,
#94946,#94947,#94948,#94949),(#94950,#94951,#94952,#94953,#94954,#94955),
(#94956,#94957,#94958,#94959,#94960,#94961),(#94962,#94963,#94964,#94965,
#94966,#94967)),.UNSPECIFIED.,.F.,.F.,.F.,(6,6),(6,6),(2.77894816417,3.04318822375),
(0.,0.3),.UNSPECIFIED.);
#1235=B_SPLINE_SURFACE_WITH_KNOTS('',5,5,((#94973,#94974,#94975,#94976,
#94977,#94978),(#94979,#94980,#94981,#94982,#94983,#94984),(#94985,#94986,
#94987,#94988,#94989,#94990),(#94991,#94992,#94993,#94994,#94995,#94996),
(#94997,#94998,#94999,#95000,#95001,#95002),(#95003,#95004,#95005,#95006,
#95007,#95008),(#95009,#95010,#95011,#95012,#95013,#95014),(#95015,#95016,
#95017,#95018,#95019,#95020),(#95021,#95022,#95023,#95024,#95025,#95026)),
 .UNSPECIFIED.,.F.,.F.,.F.,(6,3,6),(6,6),(1.25405163269,1.6430233414,2.19239180857),
(0.,0.3),.UNSPECIFIED.);
#1236=B_SPLINE_SURFACE_WITH_KNOTS('',5,5,((#95059,#95060,#95061,#95062,
#95063,#95064),(#95065,#95066,#95067,#95068,#95069,#95070),(#95071,#95072,
#95073,#95074,#95075,#95076),(#95077,#95078,#95079,#95080,#95081,#95082),
(#95083,#95084,#95085,#95086,#95087,#95088),(#95089,#95090,#95091,#95092,
#95093,#95094),(#95095,#95096,#95097,#95098,#95099,#95100),(#95101,#95102,
#95103,#95104,#95105,#95106),(#95107,#95108,#95109,#95110,#95111,#95112)),
 .UNSPECIFIED.,.F.,.F.,.F.,(6,3,6),(6,6),(1.69812247662,2.37608580106,2.83469359842),
(0.,0.3),.UNSPECIFIED.);
#1237=B_SPLINE_SURFACE_WITH_KNOTS('',5,5,((#95160,#95161,#95162,#95163,
#95164,#95165),(#95166,#95167,#95168,#95169,#95170,#95171),(#95172,#95173,
#95174,#95175,#95176,#95177),(#95178,#95179,#95180,#95181,#95182,#95183),
(#95184,#95185,#95186,#95187,#95188,#95189),(#95190,#95191,#95192,#95193,
#95194,#95195)),.UNSPECIFIED.,.F.,.F.,.F.,(6,6),(6,6),(1.6338579571,2.7257140478),
(0.,0.3),.UNSPECIFIED.);
#1238=B_SPLINE_SURFACE_WITH_KNOTS('',5,5,((#95325,#95326,#95327,#95328,
#95329,#95330),(#95331,#95332,#95333,#95334,#95335,#95336),(#95337,#95338,
#95339,#95340,#95341,#95342),(#95343,#95344,#95345,#95346,#95347,#95348),
(#95349,#95350,#95351,#95352,#95353,#95354),(#95355,#95356,#95357,#95358,
#95359,#95360),(#95361,#95362,#95363,#95364,#95365,#95366),(#95367,#95368,
#95369,#95370,#95371,#95372),(#95373,#95374,#95375,#95376,#95377,#95378)),
 .UNSPECIFIED.,.F.,.F.,.F.,(6,3,6),(6,6),(1.37442826527,1.83079344184,2.19966814328),
(0.,0.3),.UNSPECIFIED.);
#1239=B_SPLINE_SURFACE_WITH_KNOTS('',5,5,((#95504,#95505,#95506,#95507,
#95508,#95509),(#95510,#95511,#95512,#95513,#95514,#95515),(#95516,#95517,
#95518,#95519,#95520,#95521),(#95522,#95523,#95524,#95525,#95526,#95527),
(#95528,#95529,#95530,#95531,#95532,#95533),(#95534,#95535,#95536,#95537,
#95538,#95539)),.UNSPECIFIED.,.F.,.F.,.F.,(6,6),(6,6),(1.66778051169,1.825176882),
(0.,0.3),.UNSPECIFIED.);
#1240=B_SPLINE_SURFACE_WITH_KNOTS('',5,5,((#95565,#95566,#95567,#95568,
#95569,#95570),(#95571,#95572,#95573,#95574,#95575,#95576),(#95577,#95578,
#95579,#95580,#95581,#95582),(#95583,#95584,#95585,#95586,#95587,#95588),
(#95589,#95590,#95591,#95592,#95593,#95594),(#95595,#95596,#95597,#95598,
#95599,#95600)),.UNSPECIFIED.,.F.,.F.,.F.,(6,6),(6,6),(1.19509008928,1.27929234824),
(0.,0.3),.UNSPECIFIED.);
#1241=B_SPLINE_SURFACE_WITH_KNOTS('',5,5,((#95604,#95605,#95606,#95607,
#95608,#95609),(#95610,#95611,#95612,#95613,#95614,#95615),(#95616,#95617,
#95618,#95619,#95620,#95621),(#95622,#95623,#95624,#95625,#95626,#95627),
(#95628,#95629,#95630,#95631,#95632,#95633),(#95634,#95635,#95636,#95637,
#95638,#95639)),.UNSPECIFIED.,.F.,.F.,.F.,(6,6),(6,6),(0.176101352323,1.24191828283),
(0.,0.3),.UNSPECIFIED.);
#1242=B_SPLINE_SURFACE_WITH_KNOTS('',4,5,((#95885,#95886,#95887,#95888,
#95889,#95890),(#95891,#95892,#95893,#95894,#95895,#95896),(#95897,#95898,
#95899,#95900,#95901,#95902),(#95903,#95904,#95905,#95906,#95907,#95908),
(#95909,#95910,#95911,#95912,#95913,#95914)),.UNSPECIFIED.,.F.,.F.,.F.,
(5,5),(6,6),(0.,1.12670233583),(0.,0.3),.UNSPECIFIED.);
#1243=B_SPLINE_SURFACE_WITH_KNOTS('',4,5,((#96049,#96050,#96051,#96052,
#96053,#96054),(#96055,#96056,#96057,#96058,#96059,#96060),(#96061,#96062,
#96063,#96064,#96065,#96066),(#96067,#96068,#96069,#96070,#96071,#96072),
(#96073,#96074,#96075,#96076,#96077,#96078)),.UNSPECIFIED.,.F.,.F.,.F.,
(5,5),(6,6),(0.,1.12670210859),(0.,0.3),.UNSPECIFIED.);
#1244=B_SPLINE_SURFACE_WITH_KNOTS('',5,5,((#96516,#96517,#96518,#96519,
#96520,#96521,#96522,#96523,#96524),(#96525,#96526,#96527,#96528,#96529,
#96530,#96531,#96532,#96533),(#96534,#96535,#96536,#96537,#96538,#96539,
#96540,#96541,#96542),(#96543,#96544,#96545,#96546,#96547,#96548,#96549,
#96550,#96551),(#96552,#96553,#96554,#96555,#96556,#96557,#96558,#96559,
#96560),(#96561,#96562,#96563,#96564,#96565,#96566,#96567,#96568,#96569),
(#96570,#96571,#96572,#96573,#96574,#96575,#96576,#96577,#96578),(#96579,
#96580,#96581,#96582,#96583,#96584,#96585,#96586,#96587),(#96588,#96589,
#96590,#96591,#96592,#96593,#96594,#96595,#96596)),.UNSPECIFIED.,.F.,.F.,
 .F.,(6,3,6),(6,3,6),(1.82800160081,2.29147741959,2.71936718506),(0.,0.15,
0.3),.UNSPECIFIED.);
#1245=B_SPLINE_SURFACE_WITH_KNOTS('',5,5,((#96621,#96622,#96623,#96624,
#96625,#96626),(#96627,#96628,#96629,#96630,#96631,#96632),(#96633,#96634,
#96635,#96636,#96637,#96638),(#96639,#96640,#96641,#96642,#96643,#96644),
(#96645,#96646,#96647,#96648,#96649,#96650),(#96651,#96652,#96653,#96654,
#96655,#96656),(#96657,#96658,#96659,#96660,#96661,#96662),(#96663,#96664,
#96665,#96666,#96667,#96668),(#96669,#96670,#96671,#96672,#96673,#96674)),
 .UNSPECIFIED.,.F.,.F.,.F.,(6,3,6),(6,6),(1.72679799842804,2.34453942473,
2.86671715236056),(0.,0.300030052101964),.UNSPECIFIED.);
#1246=B_SPLINE_SURFACE_WITH_KNOTS('',5,5,((#96715,#96716,#96717,#96718,
#96719,#96720,#96721,#96722,#96723),(#96724,#96725,#96726,#96727,#96728,
#96729,#96730,#96731,#96732),(#96733,#96734,#96735,#96736,#96737,#96738,
#96739,#96740,#96741),(#96742,#96743,#96744,#96745,#96746,#96747,#96748,
#96749,#96750),(#96751,#96752,#96753,#96754,#96755,#96756,#96757,#96758,
#96759),(#96760,#96761,#96762,#96763,#96764,#96765,#96766,#96767,#96768),
(#96769,#96770,#96771,#96772,#96773,#96774,#96775,#96776,#96777),(#96778,
#96779,#96780,#96781,#96782,#96783,#96784,#96785,#96786),(#96787,#96788,
#96789,#96790,#96791,#96792,#96793,#96794,#96795)),.UNSPECIFIED.,.F.,.F.,
 .F.,(6,3,6),(6,3,6),(2.03426195559,2.39548583384,2.92554757),(0.,0.15,
0.3),.UNSPECIFIED.);
#1247=B_SPLINE_SURFACE_WITH_KNOTS('',5,5,((#96840,#96841,#96842,#96843,
#96844,#96845),(#96846,#96847,#96848,#96849,#96850,#96851),(#96852,#96853,
#96854,#96855,#96856,#96857),(#96858,#96859,#96860,#96861,#96862,#96863),
(#96864,#96865,#96866,#96867,#96868,#96869),(#96870,#96871,#96872,#96873,
#96874,#96875),(#96876,#96877,#96878,#96879,#96880,#96881),(#96882,#96883,
#96884,#96885,#96886,#96887),(#96888,#96889,#96890,#96891,#96892,#96893)),
 .UNSPECIFIED.,.F.,.F.,.F.,(6,3,6),(6,6),(1.66562909398,2.17637755312,2.80548129619),
(0.,0.3),.UNSPECIFIED.);
#1248=B_SPLINE_SURFACE_WITH_KNOTS('',5,5,((#96951,#96952,#96953,#96954,
#96955,#96956),(#96957,#96958,#96959,#96960,#96961,#96962),(#96963,#96964,
#96965,#96966,#96967,#96968),(#96969,#96970,#96971,#96972,#96973,#96974),
(#96975,#96976,#96977,#96978,#96979,#96980),(#96981,#96982,#96983,#96984,
#96985,#96986)),.UNSPECIFIED.,.F.,.F.,.F.,(6,6),(6,6),(1.15863824043,1.47670435084),
(0.,0.3),.UNSPECIFIED.);
#1249=B_SPLINE_SURFACE_WITH_KNOTS('',5,5,((#97008,#97009,#97010,#97011,
#97012,#97013),(#97014,#97015,#97016,#97017,#97018,#97019),(#97020,#97021,
#97022,#97023,#97024,#97025),(#97026,#97027,#97028,#97029,#97030,#97031),
(#97032,#97033,#97034,#97035,#97036,#97037),(#97038,#97039,#97040,#97041,
#97042,#97043)),.UNSPECIFIED.,.F.,.F.,.F.,(6,6),(6,6),(1.69754904882,2.01561058189),
(0.,0.3),.UNSPECIFIED.);
#1250=B_SPLINE_SURFACE_WITH_KNOTS('',5,5,((#97079,#97080,#97081,#97082,
#97083,#97084),(#97085,#97086,#97087,#97088,#97089,#97090),(#97091,#97092,
#97093,#97094,#97095,#97096),(#97097,#97098,#97099,#97100,#97101,#97102),
(#97103,#97104,#97105,#97106,#97107,#97108),(#97109,#97110,#97111,#97112,
#97113,#97114),(#97115,#97116,#97117,#97118,#97119,#97120),(#97121,#97122,
#97123,#97124,#97125,#97126),(#97127,#97128,#97129,#97130,#97131,#97132)),
 .UNSPECIFIED.,.F.,.F.,.F.,(6,3,6),(6,6),(1.64809551428,2.25520583962,2.74124708106),
(0.,0.3),.UNSPECIFIED.);
#1251=B_SPLINE_SURFACE_WITH_KNOTS('',5,5,((#97186,#97187,#97188,#97189,
#97190,#97191),(#97192,#97193,#97194,#97195,#97196,#97197),(#97198,#97199,
#97200,#97201,#97202,#97203),(#97204,#97205,#97206,#97207,#97208,#97209),
(#97210,#97211,#97212,#97213,#97214,#97215),(#97216,#97217,#97218,#97219,
#97220,#97221),(#97222,#97223,#97224,#97225,#97226,#97227),(#97228,#97229,
#97230,#97231,#97232,#97233),(#97234,#97235,#97236,#97237,#97238,#97239)),
 .UNSPECIFIED.,.F.,.F.,.F.,(6,3,6),(6,6),(1.62043318117,2.09769319653,2.71358394784),
(0.,0.3),.UNSPECIFIED.);
#1252=B_SPLINE_SURFACE_WITH_KNOTS('',5,5,((#98145,#98146,#98147,#98148,
#98149,#98150),(#98151,#98152,#98153,#98154,#98155,#98156),(#98157,#98158,
#98159,#98160,#98161,#98162),(#98163,#98164,#98165,#98166,#98167,#98168),
(#98169,#98170,#98171,#98172,#98173,#98174),(#98175,#98176,#98177,#98178,
#98179,#98180)),.UNSPECIFIED.,.F.,.F.,.F.,(6,6),(6,6),(2.82953519577,3.40560970652),
(0.,0.3),.UNSPECIFIED.);
#1253=B_SPLINE_SURFACE_WITH_KNOTS('',5,5,((#98207,#98208,#98209,#98210,
#98211,#98212),(#98213,#98214,#98215,#98216,#98217,#98218),(#98219,#98220,
#98221,#98222,#98223,#98224),(#98225,#98226,#98227,#98228,#98229,#98230),
(#98231,#98232,#98233,#98234,#98235,#98236),(#98237,#98238,#98239,#98240,
#98241,#98242)),.UNSPECIFIED.,.F.,.F.,.F.,(6,6),(6,6),(4.13551351914,4.71167786523),
(0.,0.3),.UNSPECIFIED.);
#1254=FACE_BOUND('',#5426,.T.);
#1255=FACE_BOUND('',#5427,.T.);
#1256=FACE_BOUND('',#5428,.T.);
#1257=FACE_BOUND('',#5633,.T.);
#1258=FACE_BOUND('',#5711,.T.);
#1259=FACE_BOUND('',#5712,.T.);
#1260=FACE_BOUND('',#5713,.T.);
#1261=FACE_BOUND('',#5722,.T.);
#1262=FACE_BOUND('',#5724,.T.);
#1263=FACE_BOUND('',#5725,.T.);
#1264=FACE_BOUND('',#5726,.T.);
#1265=FACE_BOUND('',#5728,.T.);
#1266=FACE_BOUND('',#5729,.T.);
#1267=FACE_BOUND('',#5730,.T.);
#1268=FACE_BOUND('',#5840,.T.);
#1269=FACE_BOUND('',#5841,.T.);
#1270=FACE_BOUND('',#5842,.T.);
#1271=FACE_BOUND('',#5844,.T.);
#1272=FACE_BOUND('',#5845,.T.);
#1273=FACE_BOUND('',#5846,.T.);
#1274=FACE_BOUND('',#5903,.T.);
#1275=FACE_BOUND('',#5904,.T.);
#1276=FACE_BOUND('',#5905,.T.);
#1277=FACE_BOUND('',#5906,.T.);
#1278=FACE_BOUND('',#5907,.T.);
#1279=FACE_BOUND('',#5908,.T.);
#1280=FACE_BOUND('',#6001,.T.);
#1281=FACE_BOUND('',#6002,.T.);
#1282=FACE_BOUND('',#6003,.T.);
#1283=FACE_BOUND('',#6038,.T.);
#1284=FACE_BOUND('',#6051,.T.);
#1285=FACE_BOUND('',#6070,.T.);
#1286=FACE_BOUND('',#6072,.T.);
#1287=FACE_BOUND('',#6074,.T.);
#1288=FACE_BOUND('',#6114,.T.);
#1289=FACE_BOUND('',#6115,.T.);
#1290=FACE_BOUND('',#6116,.T.);
#1291=FACE_BOUND('',#6121,.T.);
#1292=FACE_BOUND('',#6170,.T.);
#1293=FACE_BOUND('',#6172,.T.);
#1294=FACE_BOUND('',#6188,.T.);
#1295=FACE_BOUND('',#6322,.T.);
#1296=FACE_BOUND('',#6330,.T.);
#1297=FACE_BOUND('',#6375,.T.);
#1298=FACE_BOUND('',#6481,.T.);
#1299=FACE_BOUND('',#6516,.T.);
#1300=FACE_BOUND('',#6551,.T.);
#1301=FACE_BOUND('',#6609,.T.);
#1302=FACE_BOUND('',#6619,.T.);
#1303=FACE_BOUND('',#6620,.T.);
#1304=FACE_BOUND('',#6622,.T.);
#1305=FACE_BOUND('',#6623,.T.);
#1306=FACE_BOUND('',#6662,.T.);
#1307=FACE_BOUND('',#6715,.T.);
#1308=FACE_BOUND('',#6718,.T.);
#1309=FACE_BOUND('',#7201,.T.);
#1310=FACE_BOUND('',#7339,.T.);
#1311=FACE_BOUND('',#7340,.T.);
#1312=FACE_BOUND('',#7341,.T.);
#1313=FACE_BOUND('',#7342,.T.);
#1314=FACE_BOUND('',#7343,.T.);
#1315=FACE_BOUND('',#7442,.T.);
#1316=FACE_BOUND('',#7509,.T.);
#1317=FACE_BOUND('',#7564,.T.);
#1318=FACE_BOUND('',#7565,.T.);
#1319=FACE_BOUND('',#7599,.T.);
#1320=FACE_BOUND('',#7600,.T.);
#1321=FACE_BOUND('',#7601,.T.);
#1322=FACE_BOUND('',#7602,.T.);
#1323=FACE_BOUND('',#7603,.T.);
#1324=FACE_BOUND('',#7604,.T.);
#1325=FACE_BOUND('',#7605,.T.);
#1326=FACE_BOUND('',#7606,.T.);
#1327=FACE_BOUND('',#7607,.T.);
#1328=FACE_BOUND('',#7608,.T.);
#1329=FACE_BOUND('',#7619,.T.);
#1330=FACE_BOUND('',#7631,.T.);
#1331=FACE_BOUND('',#7634,.T.);
#1332=B_SPLINE_CURVE_WITH_KNOTS('',5,(#49225,#49226,#49227,#49228,#49229,
#49230,#49231),.UNSPECIFIED.,.F.,.F.,(6,1,6),(0.,0.465407720561711,1.),
 .UNSPECIFIED.);
#1333=B_SPLINE_CURVE_WITH_KNOTS('',5,(#49233,#49234,#49235,#49236,#49237,
#49238),.UNSPECIFIED.,.F.,.F.,(6,6),(0.,0.788840280269),.UNSPECIFIED.);
#1334=B_SPLINE_CURVE_WITH_KNOTS('',5,(#49240,#49241,#49242,#49243,#49244,
#49245,#49246,#49247,#49248,#49249,#49250),.UNSPECIFIED.,.F.,.F.,(6,3,1,
1,6),(0.,0.151641330465487,0.494687846976795,0.919150815604558,1.),
 .UNSPECIFIED.);
#1335=B_SPLINE_CURVE_WITH_KNOTS('',5,(#49252,#49253,#49254,#49255,#49256,
#49257),.UNSPECIFIED.,.F.,.F.,(6,6),(0.,1.62525620495),.UNSPECIFIED.);
#1336=B_SPLINE_CURVE_WITH_KNOTS('',5,(#49259,#49260,#49261,#49262,#49263,
#49264,#49265,#49266,#49267,#49268,#49269),.UNSPECIFIED.,.F.,.F.,(6,2,1,
1,1,6),(0.,0.232559611743824,0.537888788088502,0.750633611657941,0.946930649753588,
1.),.UNSPECIFIED.);
#1337=B_SPLINE_CURVE_WITH_KNOTS('',5,(#49276,#49277,#49278,#49279,#49280,
#49281,#49282,#49283),.UNSPECIFIED.,.F.,.F.,(6,2,6),(0.,0.422457434925888,
1.),.UNSPECIFIED.);
#1338=B_SPLINE_CURVE_WITH_KNOTS('',5,(#49305,#49306,#49307,#49308,#49309,
#49310,#49311,#49312,#49313,#49314,#49315,#49316,#49317,#49318,#49319,#49320,
#49321,#49322),.UNSPECIFIED.,.F.,.F.,(6,3,3,3,3,6),(0.465128126763,3.42050470566,
7.30063973795,10.0042092191,12.4987596036,13.1731669678),.UNSPECIFIED.);
#1339=B_SPLINE_CURVE_WITH_KNOTS('',5,(#49324,#49325,#49326,#49327,#49328,
#49329),.UNSPECIFIED.,.F.,.F.,(6,6),(0.,1.62525620495),.UNSPECIFIED.);
#1340=B_SPLINE_CURVE_WITH_KNOTS('',5,(#49331,#49332,#49333,#49334,#49335,
#49336,#49337,#49338,#49339,#49340,#49341,#49342,#49343,#49344,#49345),
 .UNSPECIFIED.,.F.,.F.,(6,3,3,3,6),(0.617889185003,0.915206541473,1.58780472511,
2.42003303229,2.57855093571),.UNSPECIFIED.);
#1341=B_SPLINE_CURVE_WITH_KNOTS('',5,(#49347,#49348,#49349,#49350,#49351,
#49352),.UNSPECIFIED.,.F.,.F.,(6,6),(0.,0.788840280269),.UNSPECIFIED.);
#1342=B_SPLINE_CURVE_WITH_KNOTS('',3,(#49354,#49355,#49356,#49357),
 .UNSPECIFIED.,.F.,.F.,(4,4),(0.,1.),.UNSPECIFIED.);
#1343=B_SPLINE_CURVE_WITH_KNOTS('',3,(#49361,#49362,#49363,#49364),
 .UNSPECIFIED.,.F.,.F.,(4,4),(0.,1.),.UNSPECIFIED.);
#1344=B_SPLINE_CURVE_WITH_KNOTS('',5,(#49388,#49389,#49390,#49391,#49392,
#49393,#49394,#49395,#49396),.UNSPECIFIED.,.F.,.F.,(6,3,6),(0.,0.500481905098514,
1.),.UNSPECIFIED.);
#1345=B_SPLINE_CURVE_WITH_KNOTS('',3,(#49400,#49401,#49402,#49403,#49404,
#49405,#49406,#49407,#49408,#49409),.UNSPECIFIED.,.F.,.F.,(4,3,3,4),(-2.46410111513,
-2.43212843610953,-2.39098596142,-2.37851323355),.UNSPECIFIED.);
#1346=B_SPLINE_CURVE_WITH_KNOTS('',3,(#49410,#49411,#49412,#49413,#49414,
#49415,#49416,#49417,#49418,#49419,#49420,#49421,#49422,#49423,#49424,#49425,
#49426,#49427,#49428,#49429,#49430,#49431,#49432,#49433,#49434,#49435,#49436,
#49437,#49438,#49439,#49440,#49441,#49442,#49443,#49444,#49445,#49446,#49447,
#49448,#49449,#49450,#49451,#49452),.UNSPECIFIED.,.F.,.F.,(4,3,3,3,3,3,
3,3,3,3,3,3,3,3,4),(0.,0.0613221810056141,0.125866562481823,0.192962198900169,
0.263336451623022,0.341802092378546,0.427968116931692,0.536199508330899,
0.56788778905896,0.661002984718601,0.746254481470477,0.828376996970244,
0.907920904739906,0.984520534711008,1.),.UNSPECIFIED.);
#1347=B_SPLINE_CURVE_WITH_KNOTS('',3,(#49487,#49488,#49489,#49490,#49491,
#49492,#49493,#49494,#49495,#49496,#49497,#49498,#49499,#49500,#49501,#49502,
#49503,#49504,#49505,#49506,#49507,#49508,#49509,#49510,#49511,#49512,#49513,
#49514,#49515,#49516,#49517,#49518,#49519,#49520),.UNSPECIFIED.,.F.,.F.,
(4,3,3,3,3,3,3,3,3,3,3,4),(0.,0.0987514676261084,0.196101602166033,0.2928935924342,
0.389205363491127,0.421433182784012,0.517619219660985,0.613998257361256,
0.711154034512961,0.808967652077894,0.908370062273473,1.),.UNSPECIFIED.);
#1348=B_SPLINE_CURVE_WITH_KNOTS('',5,(#49526,#49527,#49528,#49529,#49530,
#49531,#49532,#49533,#49534),.UNSPECIFIED.,.F.,.F.,(6,3,6),(0.,0.571293900064368,
1.),.UNSPECIFIED.);
#1349=B_SPLINE_CURVE_WITH_KNOTS('',3,(#49546,#49547,#49548,#49549,#49550,
#49551,#49552,#49553,#49554,#49555,#49556,#49557,#49558,#49559,#49560,#49561,
#49562,#49563,#49564,#49565,#49566,#49567,#49568,#49569,#49570,#49571,#49572,
#49573,#49574,#49575,#49576,#49577,#49578,#49579,#49580,#49581,#49582,#49583,
#49584,#49585),.UNSPECIFIED.,.F.,.F.,(4,3,3,3,3,3,3,3,3,3,3,3,3,4),(0.342430056326,
0.416647889440572,0.493342454420148,0.569706842465,0.648977821089767,0.726755174830412,
0.787545489389,0.864698238944471,0.942373129697395,1.0113837312,1.09481342684991,
1.13043704811,1.14340426682165,1.14838178471),.UNSPECIFIED.);
#1350=B_SPLINE_CURVE_WITH_KNOTS('',3,(#49626,#49627,#49628,#49629,#49630,
#49631,#49632,#49633,#49634,#49635,#49636,#49637,#49638,#49639,#49640,#49641,
#49642,#49643,#49644,#49645,#49646,#49647,#49648,#49649,#49650,#49651,#49652,
#49653,#49654,#49655,#49656,#49657,#49658,#49659,#49660,#49661,#49662,#49663,
#49664,#49665,#49666,#49667,#49668),.UNSPECIFIED.,.F.,.F.,(4,3,3,3,3,3,
3,3,3,3,3,3,3,3,4),(0.,0.0615954828555703,0.126643630853992,0.19444062384319,
0.265752116217026,0.345130620933528,0.430362574402989,0.517900008063448,
0.56788778905896,0.648999236771598,0.731976639456588,0.810477923749653,
0.885206012171236,0.955092587390329,1.),.UNSPECIFIED.);
#1351=B_SPLINE_CURVE_WITH_KNOTS('',3,(#49672,#49673,#49674,#49675,#49676,
#49677,#49678,#49679,#49680,#49681,#49682,#49683,#49684,#49685,#49686,#49687,
#49688,#49689,#49690,#49691,#49692,#49693,#49694,#49695,#49696,#49697,#49698,
#49699,#49700,#49701,#49702,#49703,#49704,#49705,#49706,#49707,#49708,#49709,
#49710,#49711,#49712,#49713,#49714,#49715,#49716,#49717,#49718,#49719,#49720,
#49721,#49722,#49723,#49724,#49725,#49726,#49727,#49728,#49729,#49730,#49731,
#49732,#49733,#49734,#49735,#49736,#49737,#49738,#49739,#49740,#49741,#49742,
#49743,#49744),.UNSPECIFIED.,.F.,.F.,(4,3,3,3,3,3,3,3,3,3,3,3,3,3,3,3,3,
3,3,3,3,3,3,3,4),(0.,0.0579967491242001,0.114812082591792,0.170568659950085,
0.225368908089845,0.278879773402611,0.331734010550692,0.383645284356977,
0.420938628926706,0.491074429566194,0.5407475186248,0.583067918566761,0.62318719578254,
0.662334513633599,0.699082071276243,0.701481831484658,0.731160497591717,
0.762275003148169,0.796507016141887,0.833748546202765,0.875311409652074,
0.913808413863513,0.949129309301143,0.981275404426876,1.),.UNSPECIFIED.);
#1352=B_SPLINE_CURVE_WITH_KNOTS('',5,(#49761,#49762,#49763,#49764,#49765,
#49766,#49767,#49768,#49769,#49770,#49771,#49772,#49773,#49774,#49775,#49776,
#49777,#49778,#49779,#49780,#49781),.UNSPECIFIED.,.F.,.F.,(6,3,3,3,3,3,
6),(-2.96825275179,-2.92587181617,-2.2858594369,-1.59285457075,-0.896955996606,
-0.723663994252,-0.586327318555),.UNSPECIFIED.);
#1353=B_SPLINE_CURVE_WITH_KNOTS('',5,(#49782,#49783,#49784,#49785,#49786,
#49787,#49788,#49789,#49790),.UNSPECIFIED.,.F.,.F.,(6,3,6),(-2.46410111513,
-2.39098596142,-2.37851323355),.UNSPECIFIED.);
#1354=B_SPLINE_CURVE_WITH_KNOTS('',5,(#49824,#49825,#49826,#49827,#49828,
#49829),.UNSPECIFIED.,.F.,.F.,(6,6),(1.26425849888,1.32115953697),
 .UNSPECIFIED.);
#1355=B_SPLINE_CURVE_WITH_KNOTS('',5,(#49831,#49832,#49833,#49834,#49835,
#49836,#49837,#49838,#49839,#49840,#49841,#49842),.UNSPECIFIED.,.F.,.F.,
(6,3,3,6),(0.,0.204469498724444,0.476563204173844,1.),.UNSPECIFIED.);
#1356=B_SPLINE_CURVE_WITH_KNOTS('',3,(#49844,#49845,#49846,#49847,#49848,
#49849,#49850,#49851,#49852,#49853,#49854,#49855,#49856,#49857,#49858,#49859,
#49860,#49861,#49862,#49863,#49864,#49865,#49866,#49867,#49868,#49869,#49870,
#49871),.UNSPECIFIED.,.F.,.F.,(4,3,3,3,3,3,3,3,3,4),(0.734432475987,0.878942275291463,
1.02006954288573,1.13913894251985,1.16119681048,1.21800796315046,1.27362568942023,
1.32243285508689,1.32924341569,1.33983380059),.UNSPECIFIED.);
#1357=B_SPLINE_CURVE_WITH_KNOTS('',3,(#49888,#49889,#49890,#49891,#49892,
#49893,#49894,#49895,#49896,#49897,#49898,#49899,#49900,#49901,#49902,#49903,
#49904,#49905,#49906,#49907,#49908,#49909,#49910,#49911,#49912,#49913,#49914,
#49915),.UNSPECIFIED.,.F.,.F.,(4,3,3,3,3,3,3,3,3,4),(-0.449080636148,-0.386865408847563,
-0.322025197047738,-0.251338921065949,-0.174920549069412,-0.0882035124128814,
0.0321179319799293,0.11744275401646,0.190820231313568,0.223602276698668),
 .UNSPECIFIED.);
#1358=B_SPLINE_CURVE_WITH_KNOTS('',3,(#49916,#49917,#49918,#49919,#49920,
#49921,#49922,#49923,#49924,#49925,#49926,#49927,#49928,#49929,#49930,#49931),
 .UNSPECIFIED.,.F.,.F.,(4,3,3,3,3,4),(0.338318706278865,0.442835581668533,
0.499233337792,0.619722435757,0.632996657825859,0.636935495757),
 .UNSPECIFIED.);
#1359=B_SPLINE_CURVE_WITH_KNOTS('',5,(#49953,#49954,#49955,#49956,#49957,
#49958,#49959,#49960,#49961,#49962,#49963,#49964),.UNSPECIFIED.,.F.,.F.,
(6,3,3,6),(0.,0.256132634704352,0.563769826408177,1.),.UNSPECIFIED.);
#1360=B_SPLINE_CURVE_WITH_KNOTS('',3,(#49965,#49966,#49967,#49968,#49969,
#49970,#49971,#49972,#49973,#49974),.UNSPECIFIED.,.F.,.F.,(4,3,3,4),(-0.0251761006649752,
-0.0188988511851622,-0.0125941833993852,0.),.UNSPECIFIED.);
#1361=B_SPLINE_CURVE_WITH_KNOTS('',3,(#49979,#49980,#49981,#49982,#49983,
#49984,#49985,#49986,#49987,#49988,#49989,#49990,#49991,#49992,#49993,#49994,
#49995,#49996,#49997,#49998,#49999,#50000,#50001,#50002,#50003,#50004,#50005,
#50006,#50007,#50008,#50009,#50010,#50011,#50012,#50013,#50014,#50015),
 .UNSPECIFIED.,.F.,.F.,(4,3,3,3,3,3,3,3,3,3,3,3,4),(0.163561610997277,0.16915058569,
0.199330059882,0.239135552965268,0.288418810440543,0.296334742315,0.337325345442903,
0.387217551940764,0.393295704107,0.436743632052119,0.473947536009189,0.486796678315,
0.489824805999),.UNSPECIFIED.);
#1362=B_SPLINE_CURVE_WITH_KNOTS('',3,(#50016,#50017,#50018,#50019),
 .UNSPECIFIED.,.F.,.F.,(4,4),(1.51692742518,1.55218902186356),
 .UNSPECIFIED.);
#1363=B_SPLINE_CURVE_WITH_KNOTS('',3,(#50026,#50027,#50028,#50029,#50030,
#50031,#50032,#50033,#50034,#50035,#50036,#50037,#50038,#50039,#50040,#50041,
#50042,#50043,#50044,#50045,#50046,#50047,#50048,#50049,#50050,#50051,#50052,
#50053,#50054,#50055,#50056,#50057,#50058,#50059,#50060,#50061,#50062,#50063,
#50064,#50065),.UNSPECIFIED.,.F.,.F.,(4,3,3,3,3,3,3,3,3,3,3,3,3,4),(0.,
0.0857703502139699,0.202245136770962,0.249999999999987,0.374999999999982,
0.422227909912381,0.468749804048871,0.499999999999978,0.574024073550536,
0.678093006562412,0.80341871283679,0.901709356418395,0.986122227259525,
1.),.UNSPECIFIED.);
#1364=B_SPLINE_CURVE_WITH_KNOTS('',3,(#50087,#50088,#50089,#50090,#50091,
#50092,#50093,#50094,#50095,#50096,#50097,#50098,#50099,#50100,#50101,#50102,
#50103,#50104,#50105,#50106,#50107,#50108,#50109,#50110,#50111,#50112,#50113,
#50114,#50115,#50116,#50117),.UNSPECIFIED.,.F.,.F.,(4,3,3,3,3,3,3,3,3,3,
4),(0.,0.11725177973149,0.25,0.345012070684631,0.440412902381579,0.5,0.640595034330486,
0.770463094223691,0.885231547111846,0.984266783604693,1.),.UNSPECIFIED.);
#1365=B_SPLINE_CURVE_WITH_KNOTS('',3,(#50122,#50123,#50124,#50125),
 .UNSPECIFIED.,.F.,.F.,(4,4),(1.51692742518,1.55218902180838),
 .UNSPECIFIED.);
#1366=B_SPLINE_CURVE_WITH_KNOTS('',3,(#50127,#50128,#50129,#50130,#50131,
#50132,#50133,#50134,#50135,#50136,#50137,#50138,#50139,#50140,#50141,#50142,
#50143,#50144,#50145,#50146,#50147,#50148,#50149,#50150,#50151,#50152,#50153,
#50154,#50155,#50156,#50157,#50158,#50159,#50160,#50161,#50162,#50163),
 .UNSPECIFIED.,.F.,.F.,(4,3,3,3,3,3,3,3,3,3,3,3,4),(0.163561610982573,0.16915058569,
0.199330059882,0.239135552965207,0.288418810441504,0.296334742315,0.337325345442626,
0.387217551940201,0.393295704107,0.436743632052091,0.473947536009078,0.486796678315,
0.489824805999),.UNSPECIFIED.);
#1367=B_SPLINE_CURVE_WITH_KNOTS('',3,(#50186,#50187,#50188,#50189,#50190,
#50191,#50192,#50193,#50194,#50195),.UNSPECIFIED.,.F.,.F.,(4,3,3,4),(-0.00626621565194798,
0.,0.0062935857631533,0.0188656317516384),.UNSPECIFIED.);
#1368=B_SPLINE_CURVE_WITH_KNOTS('',3,(#50196,#50197,#50198,#50199,#50200,
#50201,#50202,#50203,#50204,#50205,#50206,#50207,#50208,#50209,#50210,#50211,
#50212,#50213,#50214,#50215,#50216,#50217,#50218,#50219,#50220,#50221,#50222,
#50223,#50224,#50225,#50226,#50227,#50228,#50229,#50230,#50231,#50232,#50233,
#50234,#50235,#50236,#50237,#50238,#50239,#50240,#50241,#50242,#50243,#50244,
#50245,#50246,#50247,#50248,#50249,#50250,#50251,#50252,#50253,#50254,#50255,
#50256,#50257,#50258,#50259,#50260,#50261,#50262,#50263,#50264,#50265,#50266,
#50267,#50268,#50269,#50270,#50271,#50272,#50273,#50274,#50275,#50276,#50277,
#50278,#50279,#50280),.UNSPECIFIED.,.F.,.F.,(4,3,3,3,3,3,3,3,3,3,3,3,3,
3,3,3,3,3,3,3,3,3,3,3,3,3,3,3,4),(0.,0.0261765866933127,0.0558812683481721,
0.0885809143277048,0.125000000000002,0.183303332963854,0.187500000000003,
0.218750000000004,0.234375000000004,0.242187500000004,0.248195335397347,
0.250000000000004,0.256143136739208,0.313732104674438,0.375000000000005,
0.459378985198149,0.468750000000005,0.484375000000005,0.500000000000005,
0.564457131029769,0.625000000000004,0.709768961389738,0.734375000000003,
0.744291071006186,0.750000000000003,0.840934014400701,0.920467007200351,
0.992154975959462,1.),.UNSPECIFIED.);
#1369=B_SPLINE_CURVE_WITH_KNOTS('',3,(#50296,#50297,#50298,#50299,#50300,
#50301,#50302,#50303,#50304,#50305,#50306,#50307,#50308,#50309,#50310,#50311),
 .UNSPECIFIED.,.F.,.F.,(4,3,3,3,3,4),(0.338318706280354,0.44283558131635,
0.499233337792,0.619722435757,0.63299665782586,0.636935495757),
 .UNSPECIFIED.);
#1370=B_SPLINE_CURVE_WITH_KNOTS('',3,(#50312,#50313,#50314,#50315,#50316,
#50317,#50318,#50319,#50320,#50321,#50322,#50323,#50324,#50325,#50326,#50327,
#50328,#50329,#50330,#50331,#50332,#50333,#50334,#50335,#50336,#50337,#50338,
#50339),.UNSPECIFIED.,.F.,.F.,(4,3,3,3,3,3,3,3,3,4),(-0.449080636148,-0.386865408847633,
-0.32202519704816,-0.251338921067123,-0.174920549071681,-0.0882035124172373,
0.0321179319856406,0.117442754022834,0.190820231321014,0.223602276698669),
 .UNSPECIFIED.);
#1371=B_SPLINE_CURVE_WITH_KNOTS('',3,(#50375,#50376,#50377,#50378,#50379,
#50380,#50381,#50382,#50383,#50384,#50385,#50386,#50387,#50388,#50389,#50390,
#50391,#50392,#50393,#50394,#50395,#50396,#50397,#50398,#50399,#50400,#50401,
#50402),.UNSPECIFIED.,.F.,.F.,(4,3,3,3,3,3,3,3,3,4),(0.734432475987,0.878942275291463,
1.02006954288573,1.13913894251985,1.16119681048,1.21800796315046,1.27362568942023,
1.32243285508689,1.32924341569,1.33983380059),.UNSPECIFIED.);
#1372=B_SPLINE_CURVE_WITH_KNOTS('',3,(#50404,#50405,#50406,#50407,#50408,
#50409,#50410,#50411,#50412,#50413,#50414,#50415,#50416,#50417,#50418,#50419,
#50420,#50421,#50422,#50423,#50424,#50425,#50426,#50427,#50428,#50429,#50430,
#50431,#50432,#50433,#50434,#50435,#50436,#50437,#50438,#50439,#50440,#50441,
#50442,#50443,#50444,#50445,#50446,#50447,#50448,#50449,#50450,#50451,#50452,
#50453,#50454,#50455,#50456,#50457,#50458,#50459,#50460,#50461,#50462,#50463,
#50464,#50465,#50466,#50467,#50468,#50469,#50470,#50471,#50472,#50473,#50474,
#50475,#50476,#50477,#50478,#50479,#50480,#50481,#50482,#50483,#50484,#50485,
#50486,#50487,#50488,#50489,#50490,#50491,#50492,#50493,#50494,#50495,#50496,
#50497,#50498,#50499,#50500,#50501,#50502,#50503,#50504,#50505,#50506,#50507,
#50508,#50509,#50510,#50511,#50512,#50513,#50514,#50515,#50516,#50517,#50518,
#50519,#50520,#50521,#50522,#50523,#50524,#50525,#50526,#50527,#50528,#50529,
#50530,#50531,#50532,#50533,#50534,#50535,#50536,#50537,#50538,#50539,#50540,
#50541,#50542,#50543,#50544,#50545,#50546,#50547,#50548),.UNSPECIFIED.,
 .F.,.F.,(4,3,3,3,3,3,3,3,3,3,3,3,3,3,3,3,3,3,3,3,3,3,3,3,3,3,3,3,3,3,3,
3,3,3,3,3,3,3,3,3,3,3,3,3,3,3,3,3,4),(0.,0.0231346004295628,0.0500178550406402,
0.0845397778945774,0.119463675079143,0.125000000000173,0.165311219448787,
0.185320585969123,0.187500000000259,0.218750000000302,0.234375000000321,
0.242187500000328,0.247147468670735,0.250000000000335,0.286201553004801,
0.312500000000395,0.343750000000423,0.357088132051338,0.370908028354747,
0.375000000000451,0.411074730266149,0.437500000000507,0.465051541454789,
0.468750000000537,0.479325552184636,0.484375000000548,0.492187500000553,
0.496093750000553,0.498918789229101,0.500000000000554,0.536570602248778,
0.57402753795025,0.613446187852256,0.625000000000409,0.661047947208312,
0.687500000000338,0.717129701733469,0.718750000000303,0.734375000000285,
0.742187500000277,0.747463775729895,0.750000000000268,0.788333005300937,
0.827104022079326,0.867124780858469,0.875000000000134,0.915207770758867,
0.958291812587217,1.),.UNSPECIFIED.);
#1373=B_SPLINE_CURVE_WITH_KNOTS('',5,(#50549,#50550,#50551,#50552,#50553,
#50554),.UNSPECIFIED.,.F.,.F.,(6,6),(1.26425849888,1.32115953697),
 .UNSPECIFIED.);
#1374=B_SPLINE_CURVE_WITH_KNOTS('',5,(#50570,#50571,#50572,#50573,#50574,
#50575,#50576,#50577,#50578),.UNSPECIFIED.,.F.,.F.,(6,3,6),(-2.46410111513,
-2.39098596142,-2.37851323355),.UNSPECIFIED.);
#1375=B_SPLINE_CURVE_WITH_KNOTS('',5,(#50579,#50580,#50581,#50582,#50583,
#50584,#50585,#50586,#50587,#50588,#50589,#50590,#50591,#50592,#50593,#50594,
#50595,#50596,#50597,#50598,#50599),.UNSPECIFIED.,.F.,.F.,(6,3,3,3,3,3,
6),(-2.96825275179,-2.92587181617,-2.2858594369,-1.59285457075,-0.896955996606,
-0.723663994252,-0.586327318555),.UNSPECIFIED.);
#1376=B_SPLINE_CURVE_WITH_KNOTS('',3,(#50641,#50642,#50643,#50644,#50645,
#50646,#50647,#50648,#50649,#50650,#50651,#50652,#50653,#50654,#50655,#50656,
#50657,#50658,#50659,#50660,#50661,#50662,#50663,#50664,#50665,#50666,#50667,
#50668,#50669,#50670,#50671,#50672,#50673,#50674,#50675,#50676,#50677,#50678,
#50679,#50680,#50681,#50682,#50683,#50684,#50685,#50686,#50687,#50688,#50689,
#50690,#50691,#50692,#50693,#50694,#50695,#50696,#50697,#50698,#50699,#50700,
#50701,#50702,#50703,#50704,#50705,#50706,#50707,#50708,#50709,#50710,#50711,
#50712,#50713,#50714,#50715,#50716,#50717,#50718,#50719,#50720,#50721,#50722,
#50723,#50724,#50725,#50726,#50727,#50728,#50729,#50730,#50731,#50732,#50733,
#50734,#50735,#50736,#50737,#50738,#50739,#50740,#50741,#50742,#50743,#50744,
#50745,#50746,#50747,#50748,#50749,#50750,#50751,#50752,#50753,#50754,#50755,
#50756,#50757,#50758,#50759,#50760,#50761,#50762,#50763,#50764,#50765,#50766,
#50767,#50768,#50769,#50770,#50771,#50772,#50773,#50774,#50775,#50776,#50777,
#50778,#50779,#50780,#50781,#50782),.UNSPECIFIED.,.F.,.F.,(4,3,3,3,3,3,
3,3,3,3,3,3,3,3,3,3,3,3,3,3,3,3,3,3,3,3,3,3,3,3,3,3,3,3,3,3,3,3,3,3,3,3,
3,3,3,3,3,4),(0.,0.0482800745763561,0.0999928168250673,0.124999999999995,
0.174135612129771,0.229896375932678,0.249999999999991,0.316269512578206,
0.374999999999986,0.422793611779239,0.428296583176361,0.478606275337593,
0.492187499999981,0.497939634911579,0.499999999999981,0.534178550728474,
0.569174422590688,0.606755351723731,0.624999999999974,0.668818159693521,
0.687499999999971,0.690040383775526,0.718749999999969,0.734374999999968,
0.742187499999968,0.746337890624969,0.748348236083954,0.748842969536751,
0.74896984420037,0.749080959617201,0.749572830868696,0.749817805808406,
0.749921584695242,0.749993974242736,0.750061734871237,0.783289856320991,
0.81080130211654,0.842900651058264,0.858950325529126,0.866975162764558,
0.870987581382273,0.872993790691131,0.873164733602404,0.874999999999989,
0.909721106998409,0.943020259505496,0.975183165959494,1.),.UNSPECIFIED.);
#1377=B_SPLINE_CURVE_WITH_KNOTS('',3,(#50785,#50786,#50787,#50788,#50789,
#50790,#50791,#50792,#50793,#50794,#50795,#50796,#50797,#50798,#50799,#50800,
#50801,#50802,#50803,#50804,#50805,#50806,#50807,#50808,#50809,#50810,#50811,
#50812,#50813,#50814,#50815,#50816,#50817,#50818,#50819,#50820,#50821,#50822,
#50823,#50824,#50825,#50826,#50827,#50828,#50829,#50830,#50831,#50832,#50833,
#50834,#50835,#50836,#50837,#50838,#50839,#50840,#50841,#50842,#50843,#50844,
#50845,#50846,#50847,#50848,#50849,#50850,#50851,#50852,#50853,#50854,#50855,
#50856,#50857,#50858,#50859,#50860,#50861,#50862,#50863,#50864,#50865,#50866,
#50867,#50868,#50869,#50870,#50871,#50872),.UNSPECIFIED.,.F.,.F.,(4,3,3,
3,3,3,3,3,3,3,3,3,3,3,3,3,3,3,3,3,3,3,3,3,3,3,3,3,3,4),(0.,0.0677279874926389,
0.125000000000004,0.187500000000006,0.234375000000007,0.238769531250007,
0.240898132324226,0.241827442804597,0.242623468185741,0.246760234804936,
0.24876398113611,0.249960312481452,0.250461958420372,0.319628467835613,
0.37500000000001,0.43750000000001,0.468750000000011,0.484375000000011,0.492187500000011,
0.496093750000011,0.500000000000011,0.581594064625126,0.590609029780262,
0.664723012700118,0.735690189997278,0.750000000000005,0.823627905476949,
0.911813952738474,0.970263966690367,1.),.UNSPECIFIED.);
#1378=B_SPLINE_CURVE_WITH_KNOTS('',3,(#50879,#50880,#50881,#50882,#50883,
#50884,#50885,#50886,#50887,#50888,#50889,#50890,#50891,#50892,#50893,#50894,
#50895,#50896,#50897,#50898,#50899,#50900,#50901,#50902,#50903,#50904,#50905,
#50906,#50907,#50908,#50909,#50910,#50911,#50912,#50913,#50914,#50915,#50916,
#50917,#50918),.UNSPECIFIED.,.F.,.F.,(4,3,3,3,3,3,3,3,3,3,3,3,3,4),(0.342430056326,
0.416647889440572,0.493342454420148,0.569706842465,0.648977821089767,0.726755174830412,
0.787545489389,0.864698238944471,0.942373129697395,1.0113837312,1.09481342684991,
1.13043704811,1.14340426682165,1.14838178471),.UNSPECIFIED.);
#1379=B_SPLINE_CURVE_WITH_KNOTS('',3,(#51267,#51268,#51269,#51270,#51271,
#51272,#51273,#51274,#51275,#51276),.UNSPECIFIED.,.F.,.F.,(4,2,2,2,4),(0.,
0.0166816603056456,0.0333322760364835,0.0499757597117433,0.0666639750956066),
 .UNSPECIFIED.);
#1380=B_SPLINE_CURVE_WITH_KNOTS('',3,(#51279,#51280,#51281,#51282,#51283,
#51284,#51285,#51286,#51287,#51288,#51289,#51290,#51291,#51292,#51293,#51294,
#51295,#51296,#51297,#51298,#51299,#51300,#51301,#51302,#51303,#51304,#51305,
#51306,#51307,#51308,#51309,#51310,#51311,#51312,#51313,#51314,#51315,#51316,
#51317,#51318,#51319,#51320,#51321,#51322,#51323,#51324,#51325,#51326,#51327),
 .UNSPECIFIED.,.F.,.F.,(4,3,3,3,3,3,3,3,3,3,3,3,3,3,3,3,4),(0.342430099983039,
0.406155276626072,0.471478495422541,0.538329105188344,0.569706842465,0.635135726209432,
0.678900017195,0.741518988230734,0.787545489389,0.852180995271464,0.919332213618591,
0.987762598983568,1.0113837312,1.07392703039314,1.13043704811,1.14591870241,
1.14838178471),.UNSPECIFIED.);
#1381=B_SPLINE_CURVE_WITH_KNOTS('',3,(#51349,#51350,#51351,#51352,#51353,
#51354),.UNSPECIFIED.,.F.,.F.,(4,2,4),(-0.025439056349247,-0.0127192586494339,
0.),.UNSPECIFIED.);
#1382=B_SPLINE_CURVE_WITH_KNOTS('',5,(#51358,#51359,#51360,#51361,#51362,
#51363,#51364,#51365,#51366),.UNSPECIFIED.,.F.,.F.,(6,3,6),(0.995280026640254,
1.21544696444,1.22129342209),.UNSPECIFIED.);
#1383=B_SPLINE_CURVE_WITH_KNOTS('',3,(#51393,#51394,#51395,#51396,#51397,
#51398,#51399,#51400,#51401,#51402,#51403,#51404,#51405,#51406,#51407,#51408,
#51409,#51410,#51411,#51412,#51413,#51414,#51415,#51416,#51417,#51418,#51419,
#51420,#51421,#51422,#51423,#51424,#51425,#51426,#51427,#51428,#51429,#51430,
#51431,#51432,#51433,#51434,#51435,#51436,#51437,#51438,#51439,#51440,#51441,
#51442,#51443,#51444,#51445,#51446,#51447,#51448,#51449,#51450,#51451,#51452,
#51453,#51454,#51455,#51456),.UNSPECIFIED.,.F.,.F.,(4,3,3,3,3,3,3,3,3,3,
3,3,3,3,3,3,3,3,3,3,3,4),(0.,0.948237676895928,2.04200576184201,3.37474848426459,
4.40850535538508,5.30596315772473,5.58045964467773,6.71900177794048,8.10021196688407,
9.27267325358068,10.1040285365416,10.4451345402773,10.8737182939327,11.3495434571161,
11.699840638544,11.8670612467535,12.5378975955484,13.1340007751306,13.642280142205,
14.1090493942805,14.5397893196166,14.6803195994),.UNSPECIFIED.);
#1384=B_SPLINE_CURVE_WITH_KNOTS('',5,(#51459,#51460,#51461,#51462,#51463,
#51464,#51465,#51466,#51467,#51468,#51469,#51470),.UNSPECIFIED.,.F.,.F.,
(6,3,3,6),(6.85951996631323E-8,0.420938628926706,0.701481831484658,0.999999989476295),
 .UNSPECIFIED.);
#1385=B_SPLINE_CURVE_WITH_KNOTS('',3,(#51483,#51484,#51485,#51486,#51487,
#51488),.UNSPECIFIED.,.F.,.F.,(4,2,4),(-0.0251203830680402,-0.0125600919312397,
0.),.UNSPECIFIED.);
#1386=B_SPLINE_CURVE_WITH_KNOTS('',3,(#51489,#51490,#51491,#51492,#51493,
#51494,#51495,#51496,#51497,#51498,#51499,#51500,#51501,#51502,#51503,#51504,
#51505,#51506,#51507,#51508,#51509,#51510,#51511,#51512,#51513),
 .UNSPECIFIED.,.F.,.F.,(4,3,3,3,3,3,3,3,4),(1.01054286647469,1.0614593193646,
1.11979310493141,1.18952357816526,1.23011259501,1.26531612164489,1.29489655211715,
1.31773496162,1.32384910338),.UNSPECIFIED.);
#1387=B_SPLINE_CURVE_WITH_KNOTS('',3,(#51533,#51534,#51535,#51536,#51537,
#51538,#51539,#51540,#51541,#51542,#51543,#51544,#51545,#51546,#51547,#51548,
#51549,#51550,#51551,#51552,#51553,#51554,#51555,#51556,#51557,#51558,#51559,
#51560,#51561,#51562,#51563,#51564,#51565,#51566,#51567,#51568,#51569),
 .UNSPECIFIED.,.F.,.F.,(4,3,3,3,3,3,3,3,3,3,3,3,4),(0.163561586048556,0.16915058569,
0.199330059882,0.239717424431074,0.289567767371195,0.296334742315,0.342221563674437,
0.389994474503767,0.393295704107,0.435638979152134,0.473912817661004,0.486796678315,
0.489824805999),.UNSPECIFIED.);
#1388=B_SPLINE_CURVE_WITH_KNOTS('',3,(#51598,#51599,#51600,#51601,#51602,
#51603,#51604,#51605,#51606,#51607,#51608,#51609,#51610,#51611,#51612,#51613,
#51614,#51615,#51616,#51617,#51618,#51619,#51620,#51621,#51622,#51623,#51624,
#51625,#51626,#51627,#51628,#51629,#51630,#51631,#51632,#51633,#51634,#51635,
#51636,#51637,#51638,#51639,#51640,#51641,#51642,#51643,#51644,#51645,#51646,
#51647,#51648,#51649,#51650,#51651,#51652,#51653,#51654,#51655,#51656,#51657,
#51658,#51659,#51660,#51661,#51662,#51663,#51664),.UNSPECIFIED.,.F.,.F.,
(4,3,3,3,3,3,3,3,3,3,3,3,3,3,3,3,3,3,3,3,3,3,4),(0.,0.150485130188399,0.30297850459967,
0.457031628712122,0.561567306255,0.709215379177615,0.854264253416426,0.913473553147556,
1.04884917352124,1.12559454297,1.28001930589065,1.43693558960681,1.58742667059295,
1.69044089606,1.82557173927566,1.8394563651115,1.98772408517656,2.13847260473739,
2.25475688458,2.40866618427487,2.56165891031834,2.71215471728285,2.77932659819),
 .UNSPECIFIED.);
#1389=B_SPLINE_CURVE_WITH_KNOTS('',5,(#51667,#51668,#51669,#51670,#51671,
#51672,#51673,#51674,#51675,#51676,#51677,#51678),.UNSPECIFIED.,.F.,.F.,
(6,3,3,6),(0.,0.204469498724444,0.476563204173844,1.),.UNSPECIFIED.);
#1390=B_SPLINE_CURVE_WITH_KNOTS('',3,(#51695,#51696,#51697,#51698,#51699,
#51700,#51701,#51702,#51703,#51704,#51705,#51706,#51707,#51708,#51709,#51710,
#51711,#51712,#51713,#51714,#51715,#51716),.UNSPECIFIED.,.F.,.F.,(4,3,3,
3,3,3,3,4),(0.734432475987,0.897425480061445,1.04019709468454,1.16119681048,
1.22610423484268,1.28628740602881,1.32924341569,1.33983379849382),
 .UNSPECIFIED.);
#1391=B_SPLINE_CURVE_WITH_KNOTS('',3,(#51729,#51730,#51731,#51732,#51733,
#51734,#51735,#51736,#51737,#51738,#51739,#51740,#51741,#51742,#51743,#51744,
#51745,#51746,#51747,#51748,#51749,#51750,#51751,#51752,#51753,#51754,#51755,
#51756,#51757,#51758,#51759),.UNSPECIFIED.,.F.,.F.,(4,3,3,3,3,3,3,3,3,3,
4),(0.,0.244795327918773,0.502847705033991,0.780409654548682,1.09688525358557,
1.52122108872678,1.83404989561054,2.11578718796133,2.37921313711228,2.62468126213379,
2.75757599775),.UNSPECIFIED.);
#1392=B_SPLINE_CURVE_WITH_KNOTS('',3,(#51761,#51762,#51763,#51764,#51765,
#51766,#51767),.UNSPECIFIED.,.F.,.F.,(4,3,4),(0.881014033286,0.948965831295187,
0.963434555076),.UNSPECIFIED.);
#1393=B_SPLINE_CURVE_WITH_KNOTS('',3,(#51768,#51769,#51770,#51771,#51772,
#51773,#51774,#51775,#51776,#51777,#51778,#51779,#51780,#51781,#51782,#51783,
#51784,#51785,#51786,#51787,#51788,#51789,#51790,#51791,#51792,#51793,#51794,
#51795,#51796,#51797,#51798,#51799,#51800,#51801,#51802,#51803,#51804,#51805,
#51806,#51807,#51808,#51809,#51810,#51811,#51812,#51813,#51814,#51815,#51816),
 .UNSPECIFIED.,.F.,.F.,(4,3,3,3,3,3,3,3,3,3,3,3,3,3,3,3,4),(-2.96825275179,
-2.92587181617,-2.75740998902055,-2.58343808727891,-2.39896382434401,-2.2858594369,
-2.08411702426915,-1.87893514117023,-1.67994580319545,-1.59285457075,-1.39361191417081,
-1.20541337865871,-1.0344021207881,-0.896955996606,-0.740414779189322,-0.723663994252,
-0.586327318555),.UNSPECIFIED.);
#1394=B_SPLINE_CURVE_WITH_KNOTS('',3,(#51868,#51869,#51870,#51871,#51872,
#51873,#51874,#51875,#51876,#51877,#51878,#51879,#51880,#51881,#51882,#51883,
#51884,#51885,#51886,#51887,#51888,#51889,#51890,#51891,#51892,#51893,#51894,
#51895,#51896,#51897,#51898),.UNSPECIFIED.,.F.,.F.,(4,3,3,3,3,3,3,3,3,3,
4),(0.,0.106507047524963,0.214193650328982,0.326022688788743,0.446688121212756,
0.5,0.610700523139681,0.71326332802124,0.814167331458963,0.917046982929181,
1.),.UNSPECIFIED.);
#1395=B_SPLINE_CURVE_WITH_KNOTS('',3,(#51957,#51958,#51959,#51960,#51961,
#51962,#51963,#51964,#51965,#51966,#51967,#51968,#51969,#51970,#51971,#51972,
#51973,#51974,#51975,#51976,#51977,#51978,#51979,#51980,#51981,#51982,#51983,
#51984,#51985,#51986,#51987,#51988,#51989,#51990,#51991,#51992,#51993),
 .UNSPECIFIED.,.F.,.F.,(4,3,3,3,3,3,3,3,3,3,3,3,4),(0.,0.109774660407206,
0.236893273816627,0.249999999999999,0.323861363638668,0.396238624772552,
0.463887957515316,0.499999999999997,0.565010634550699,0.71662408184464,
0.842148144824872,0.956539659898614,1.),.UNSPECIFIED.);
#1396=B_SPLINE_CURVE_WITH_KNOTS('',3,(#52031,#52032,#52033,#52034,#52035,
#52036,#52037,#52038,#52039,#52040),.UNSPECIFIED.,.F.,.F.,(4,3,3,4),(1.28339894164,
1.30680607386887,1.3328892219684,1.34350433703),.UNSPECIFIED.);
#1397=B_SPLINE_CURVE_WITH_KNOTS('',3,(#52141,#52142,#52143,#52144,#52145,
#52146,#52147,#52148,#52149,#52150,#52151,#52152,#52153,#52154,#52155,#52156,
#52157,#52158,#52159,#52160,#52161,#52162,#52163,#52164,#52165,#52166,#52167,
#52168,#52169,#52170,#52171,#52172,#52173,#52174,#52175,#52176,#52177),
 .UNSPECIFIED.,.F.,.F.,(4,3,3,3,3,3,3,3,3,3,3,3,4),(5.1954086812113E-8,
0.0881831468536577,0.192584408778802,0.301488460118701,0.404564094688347,
0.5,0.561992944439645,0.652033254324342,0.748248539918247,0.841547093326746,
0.920773546663373,0.993552974112633,1.),.UNSPECIFIED.);
#1398=B_SPLINE_CURVE_WITH_KNOTS('',3,(#52291,#52292,#52293,#52294,#52295,
#52296,#52297,#52298,#52299,#52300,#52301,#52302,#52303,#52304,#52305,#52306,
#52307,#52308,#52309,#52310,#52311,#52312,#52313,#52314,#52315,#52316,#52317,
#52318,#52319,#52320,#52321,#52322,#52323,#52324,#52325,#52326,#52327,#52328,
#52329,#52330,#52331,#52332,#52333,#52334,#52335,#52336,#52337,#52338,#52339,
#52340,#52341,#52342,#52343,#52344,#52345,#52346,#52347,#52348,#52349,#52350,
#52351,#52352,#52353,#52354,#52355,#52356,#52357,#52358,#52359,#52360,#52361,
#52362,#52363,#52364,#52365,#52366,#52367,#52368,#52369,#52370,#52371,#52372,
#52373,#52374,#52375,#52376,#52377,#52378,#52379,#52380,#52381,#52382,#52383,
#52384,#52385,#52386,#52387,#52388,#52389,#52390,#52391,#52392,#52393,#52394,
#52395,#52396,#52397,#52398,#52399,#52400,#52401,#52402,#52403,#52404,#52405,
#52406,#52407,#52408,#52409,#52410,#52411,#52412,#52413,#52414,#52415,#52416,
#52417,#52418,#52419,#52420,#52421,#52422,#52423),.UNSPECIFIED.,.F.,.F.,
(4,3,3,3,3,3,3,3,3,3,3,3,3,3,3,3,3,3,3,3,3,3,3,3,3,3,3,3,3,3,3,3,3,3,3,
3,3,3,3,3,3,3,3,3,4),(0.,0.0449839752208177,0.094648655991429,0.125000000000001,
0.180289664252898,0.187500000000002,0.218750000000002,0.234375000000002,
0.242187500000002,0.246093750000002,0.250000000000003,0.307559572351956,
0.356504949280997,0.375000000000005,0.417469288796414,0.426882497257103,
0.437500000000006,0.468750000000007,0.487024846094567,0.500000000000007,
0.539444949446193,0.579065581700542,0.619687961577662,0.62500000000001,
0.667322932809044,0.687500000000011,0.696132105409999,0.718750000000011,
0.734375000000012,0.742187500000012,0.746093750000011,0.748046875000011,
0.750000000000011,0.787230005409161,0.812500000000007,0.843750000000005,
0.859375000000004,0.867187500000004,0.871093750000003,0.874404103182036,
0.875000000000003,0.910890016908024,0.944438319456343,0.97591609698468,
0.999999989299826),.UNSPECIFIED.);
#1399=B_SPLINE_CURVE_WITH_KNOTS('',3,(#52481,#52482,#52483,#52484,#52485,
#52486,#52487,#52488,#52489,#52490,#52491,#52492,#52493,#52494,#52495,#52496,
#52497,#52498,#52499,#52500,#52501,#52502,#52503,#52504,#52505),
 .UNSPECIFIED.,.F.,.F.,(4,3,3,3,3,3,3,3,4),(1.01054286443581,1.06145887153934,
1.11979195427008,1.18952209299618,1.23011254057257,1.26581096316738,1.29483003327369,
1.3210114243818,1.32384910338),.UNSPECIFIED.);
#1400=B_SPLINE_CURVE_WITH_KNOTS('',3,(#52562,#52563,#52564,#52565,#52566,
#52567,#52568,#52569,#52570,#52571,#52572,#52573,#52574,#52575,#52576,#52577,
#52578,#52579,#52580,#52581,#52582,#52583,#52584,#52585,#52586,#52587,#52588,
#52589,#52590,#52591,#52592,#52593,#52594,#52595,#52596,#52597,#52598,#52599,
#52600,#52601,#52602,#52603,#52604,#52605,#52606,#52607,#52608,#52609,#52610,
#52611,#52612,#52613,#52614,#52615,#52616,#52617,#52618,#52619,#52620,#52621,
#52622,#52623,#52624,#52625,#52626,#52627,#52628,#52629,#52630,#52631,#52632,
#52633,#52634,#52635,#52636,#52637,#52638,#52639,#52640,#52641,#52642,#52643,
#52644,#52645,#52646,#52647,#52648,#52649),.UNSPECIFIED.,.F.,.F.,(4,3,3,
3,3,3,3,3,3,3,3,3,3,3,3,3,3,3,3,3,3,3,3,3,3,3,3,3,3,4),(0.,0.0642476278262248,
0.125,0.1875,0.234375000000001,0.238769531250001,0.240898132324219,0.24178163869067,
0.242599226648374,0.246736750815612,0.248740864084118,0.249891670367119,
0.25033373353469,0.318681145396987,0.375000000000002,0.437500000000002,
0.468750000000002,0.484375000000002,0.492187500000003,0.496093750000003,
0.498046875000003,0.500000000000003,0.582577073350837,0.601597297982624,
0.677425679242019,0.750000000000001,0.824704147685727,0.912352073842863,
0.976551486277736,1.),.UNSPECIFIED.);
#1401=B_SPLINE_CURVE_WITH_KNOTS('',3,(#52686,#52687,#52688,#52689),
 .UNSPECIFIED.,.F.,.F.,(4,4),(0.995280026642634,1.22129342209),
 .UNSPECIFIED.);
#1402=B_SPLINE_CURVE_WITH_KNOTS('',3,(#52728,#52729,#52730,#52731,#52732,
#52733,#52734,#52735,#52736,#52737),.UNSPECIFIED.,.F.,.F.,(4,3,3,4),(-2.46410111513,
-2.43156045184461,-2.3842002845234,-2.37851323355),.UNSPECIFIED.);
#1403=B_SPLINE_CURVE_WITH_KNOTS('',3,(#52794,#52795,#52796,#52797,#52798,
#52799,#52800,#52801,#52802,#52803,#52804,#52805,#52806,#52807,#52808,#52809,
#52810,#52811,#52812,#52813,#52814,#52815,#52816,#52817,#52818,#52819,#52820,
#52821,#52822,#52823,#52824,#52825,#52826,#52827,#52828,#52829,#52830,#52831,
#52832,#52833,#52834,#52835,#52836,#52837,#52838,#52839,#52840,#52841,#52842,
#52843,#52844,#52845,#52846,#52847,#52848,#52849,#52850,#52851,#52852,#52853,
#52854,#52855,#52856,#52857,#52858,#52859,#52860,#52861,#52862,#52863,#52864,
#52865,#52866,#52867,#52868,#52869,#52870,#52871,#52872,#52873,#52874,#52875,
#52876,#52877,#52878,#52879,#52880,#52881,#52882,#52883,#52884,#52885,#52886,
#52887,#52888,#52889,#52890,#52891,#52892,#52893,#52894,#52895,#52896,#52897,
#52898,#52899,#52900,#52901,#52902,#52903,#52904,#52905),.UNSPECIFIED.,
 .F.,.F.,(4,3,3,3,3,3,3,3,3,3,3,3,3,3,3,3,3,3,3,3,3,3,3,3,3,3,3,3,3,3,3,
3,3,3,3,3,3,4),(0.,0.0477135724161135,0.0625000000000017,0.0937500000000023,
0.109375000000002,0.117187500000002,0.125000000000003,0.181640986341184,
0.187500000000002,0.218750000000002,0.234375000000003,0.248990132814251,
0.250000000000003,0.329265328614751,0.375000000000004,0.46359821529961,
0.479221960529419,0.483322124721982,0.48530594038562,0.498216219979678,
0.499936854854124,0.500928588655433,0.566229497664171,0.588588177138087,
0.624999999999997,0.684372375983187,0.687499999999994,0.718749999999992,
0.734374999999992,0.742187499999992,0.749136996345081,0.749999999999992,
0.796469608533299,0.844400751682625,0.891704275157033,0.93900736088884,
0.987732013854371,1.),.UNSPECIFIED.);
#1404=B_SPLINE_CURVE_WITH_KNOTS('',3,(#52944,#52945,#52946,#52947,#52948,
#52949,#52950),.UNSPECIFIED.,.F.,.F.,(4,3,4),(0.881014033286,0.948706774547412,
0.963434555076),.UNSPECIFIED.);
#1405=B_SPLINE_CURVE_WITH_KNOTS('',3,(#53007,#53008,#53009,#53010,#53011,
#53012,#53013,#53014,#53015,#53016,#53017,#53018,#53019,#53020,#53021,#53022,
#53023,#53024,#53025),.UNSPECIFIED.,.F.,.F.,(4,3,3,3,3,3,4),(0.,0.324828279928709,
0.585140352773158,0.649656559857417,0.772280636003616,0.895427880757141,
0.999999948942922),.UNSPECIFIED.);
#1406=B_SPLINE_CURVE_WITH_KNOTS('',3,(#53100,#53101,#53102,#53103,#53104,
#53105,#53106,#53107,#53108,#53109,#53110,#53111,#53112,#53113,#53114,#53115,
#53116,#53117,#53118,#53119,#53120,#53121,#53122,#53123,#53124,#53125,#53126,
#53127,#53128,#53129,#53130,#53131,#53132,#53133,#53134,#53135,#53136,#53137,
#53138,#53139,#53140,#53141,#53142,#53143,#53144,#53145,#53146,#53147,#53148,
#53149,#53150,#53151,#53152,#53153,#53154,#53155,#53156,#53157,#53158,#53159,
#53160,#53161,#53162,#53163,#53164,#53165,#53166,#53167,#53168,#53169,#53170,
#53171,#53172,#53173,#53174,#53175,#53176,#53177,#53178,#53179,#53180,#53181,
#53182,#53183,#53184,#53185,#53186,#53187,#53188,#53189,#53190,#53191,#53192,
#53193,#53194,#53195,#53196,#53197,#53198,#53199),.UNSPECIFIED.,.F.,.F.,
(4,3,3,3,3,3,3,3,3,3,3,3,3,3,3,3,3,3,3,3,3,3,3,3,3,3,3,3,3,3,3,3,3,4),(2.31347827906944E-9,
0.0304523904386003,0.0667565854045198,0.111071614656439,0.125000000000009,
0.166228903356154,0.196195787703402,0.218750000000012,0.23437500000001,
0.242763564282923,0.250000000000009,0.286657323311203,0.322698560618276,
0.357210368699332,0.375000000000006,0.406250000000004,0.437500000000003,
0.465316625673246,0.468750000000002,0.478007170175177,0.490299230010994,
0.500000000000001,0.533658524008943,0.56889649930393,0.606784435493325,
0.625000000000001,0.667117677043821,0.713500024564271,0.750000000000001,
0.806522802216992,0.865633153944195,0.9249705316322,0.984382807636567,1.),
 .UNSPECIFIED.);
#1407=B_SPLINE_CURVE_WITH_KNOTS('',3,(#53238,#53239,#53240,#53241),
 .UNSPECIFIED.,.F.,.F.,(4,4),(1.26426572301,1.32115953697),
 .UNSPECIFIED.);
#1408=B_SPLINE_CURVE_WITH_KNOTS('',3,(#53254,#53255,#53256,#53257,#53258,
#53259,#53260,#53261,#53262,#53263,#53264,#53265,#53266,#53267,#53268,#53269,
#53270,#53271,#53272,#53273,#53274,#53275),.UNSPECIFIED.,.F.,.F.,(4,3,3,
3,3,3,3,4),(0.338318706236,0.438258273139173,0.499233337792,0.545290114175537,
0.592030438707663,0.619722435757,0.633910105997971,0.636934808527437),
 .UNSPECIFIED.);
#1409=B_SPLINE_CURVE_WITH_KNOTS('',3,(#53279,#53280,#53281,#53282,#53283,
#53284),.UNSPECIFIED.,.F.,.F.,(4,2,4),(-0.10130067680855,-0.0506503369484061,
0.),.UNSPECIFIED.);
#1410=B_SPLINE_CURVE_WITH_KNOTS('',3,(#53329,#53330,#53331,#53332,#53333,
#53334,#53335,#53336,#53337,#53338,#53339,#53340,#53341,#53342,#53343,#53344,
#53345,#53346,#53347,#53348,#53349,#53350,#53351,#53352,#53353,#53354,#53355,
#53356,#53357,#53358,#53359,#53360,#53361,#53362,#53363,#53364,#53365,#53366,
#53367,#53368,#53369,#53370,#53371,#53372,#53373,#53374,#53375,#53376,#53377,
#53378,#53379,#53380,#53381,#53382,#53383,#53384,#53385,#53386,#53387,#53388,
#53389,#53390,#53391,#53392,#53393,#53394,#53395,#53396,#53397,#53398,#53399,
#53400,#53401,#53402,#53403,#53404,#53405,#53406,#53407,#53408,#53409,#53410,
#53411,#53412,#53413,#53414,#53415,#53416,#53417,#53418,#53419,#53420,#53421,
#53422,#53423,#53424,#53425,#53426,#53427,#53428,#53429,#53430,#53431,#53432,
#53433,#53434,#53435,#53436,#53437,#53438,#53439,#53440,#53441,#53442,#53443,
#53444,#53445,#53446,#53447,#53448,#53449,#53450,#53451,#53452,#53453,#53454,
#53455),.UNSPECIFIED.,.F.,.F.,(4,3,3,3,3,3,3,3,3,3,3,3,3,3,3,3,3,3,3,3,
3,3,3,3,3,3,3,3,3,3,3,3,3,3,3,3,3,3,3,3,3,3,4),(0.,0.0327143155580901,0.0625000000000028,
0.0937500000000044,0.109578455637257,0.125000000000006,0.163523013959447,
0.18750000000001,0.218750000000012,0.234375000000013,0.242187500000013,
0.246093750000014,0.249607117920692,0.250000000000014,0.257249878340838,
0.310510045979528,0.365381093929824,0.375000000000014,0.437500000000014,
0.468750000000014,0.484375000000014,0.489260595055283,0.491884315109107,
0.492587087124586,0.496959426734569,0.499008960926749,0.499641842136478,
0.500058671728224,0.552911785914761,0.56254452088432,0.615548813869578,
0.676384667730263,0.687500000000005,0.718750000000004,0.734375000000003,
0.742187500000003,0.74809367806907,0.750000000000003,0.809173214063901,
0.86756885888069,0.925738391101094,0.984348401097454,1.),.UNSPECIFIED.);
#1411=B_SPLINE_CURVE_WITH_KNOTS('',3,(#53460,#53461,#53462,#53463,#53464,
#53465),.UNSPECIFIED.,.F.,.F.,(4,2,4),(-0.750622279262213,-0.375340681565196,
0.),.UNSPECIFIED.);
#1412=B_SPLINE_CURVE_WITH_KNOTS('',3,(#53632,#53633,#53634,#53635,#53636,
#53637,#53638,#53639,#53640,#53641,#53642,#53643,#53644,#53645,#53646,#53647,
#53648,#53649,#53650),.UNSPECIFIED.,.F.,.F.,(4,3,3,3,3,3,4),(0.,0.158500319086325,
0.31863860447099,0.487780059128932,0.719403646007813,0.865891955512973,
0.999999739264845),.UNSPECIFIED.);
#1413=B_SPLINE_CURVE_WITH_KNOTS('',3,(#53727,#53728,#53729,#53730,#53731,
#53732,#53733,#53734,#53735,#53736),.UNSPECIFIED.,.F.,.F.,(4,3,3,4),(1.28339894164,
1.30680607386887,1.3328892219684,1.34350433703),.UNSPECIFIED.);
#1414=B_SPLINE_CURVE_WITH_KNOTS('',5,(#53792,#53793,#53794,#53795,#53796,
#53797,#53798,#53799,#53800),.UNSPECIFIED.,.F.,.F.,(6,3,6),(0.,0.571293900064368,
1.),.UNSPECIFIED.);
#1415=B_SPLINE_CURVE_WITH_KNOTS('',5,(#53840,#53841,#53842,#53843,#53844,
#53845),.UNSPECIFIED.,.F.,.F.,(6,6),(0.,1.),.UNSPECIFIED.);
#1416=B_SPLINE_CURVE_WITH_KNOTS('',5,(#54050,#54051,#54052,#54053,#54054,
#54055,#54056,#54057,#54058,#54059,#54060,#54061),.UNSPECIFIED.,.F.,.F.,
(6,3,3,6),(1.3907936820211E-8,0.256132634704352,0.563769826408177,1.),
 .UNSPECIFIED.);
#1417=B_SPLINE_CURVE_WITH_KNOTS('',3,(#54082,#54083,#54084,#54085,#54086,
#54087),.UNSPECIFIED.,.F.,.F.,(4,2,4),(-0.750622269444262,-0.375342208613163,
0.),.UNSPECIFIED.);
#1418=B_SPLINE_CURVE_WITH_KNOTS('',3,(#54100,#54101,#54102,#54103,#54104,
#54105),.UNSPECIFIED.,.F.,.F.,(4,2,4),(-0.101300676824578,-0.0506503372063276,
0.),.UNSPECIFIED.);
#1419=B_SPLINE_CURVE_WITH_KNOTS('',3,(#54107,#54108,#54109,#54110,#54111,
#54112,#54113,#54114,#54115,#54116,#54117,#54118,#54119,#54120,#54121,#54122,
#54123,#54124,#54125,#54126,#54127,#54128),.UNSPECIFIED.,.F.,.F.,(4,3,3,
3,3,3,3,4),(0.338318706236,0.438258273139173,0.499233337792,0.545290114175537,
0.592030438707663,0.619722435757,0.633910105997956,0.636934808527438),
 .UNSPECIFIED.);
#1420=B_SPLINE_CURVE_WITH_KNOTS('',5,(#54129,#54130,#54131,#54132,#54133,
#54134),.UNSPECIFIED.,.F.,.F.,(6,6),(1.26425849888,1.32115953697),
 .UNSPECIFIED.);
#1421=B_SPLINE_CURVE_WITH_KNOTS('',3,(#55086,#55087,#55088,#55089,#55090,
#55091,#55092,#55093,#55094,#55095,#55096,#55097,#55098,#55099,#55100,#55101,
#55102,#55103,#55104,#55105,#55106,#55107),.UNSPECIFIED.,.F.,.F.,(4,3,3,
3,3,3,3,4),(0.,0.528382896990167,1.08470689628943,1.66556978220358,2.28030783605745,
2.98182977652019,3.78815962830722,4.53770086709),.UNSPECIFIED.);
#1422=B_SPLINE_CURVE_WITH_KNOTS('',3,(#55123,#55124,#55125,#55126,#55127,
#55128,#55129,#55130,#55131,#55132),.UNSPECIFIED.,.F.,.F.,(4,2,2,2,4),(0.,
0.0110292280070327,0.0220815628933708,0.0331350655826502,0.0441631624440209),
 .UNSPECIFIED.);
#1423=B_SPLINE_CURVE_WITH_KNOTS('',3,(#55152,#55153,#55154,#55155,#55156,
#55157),.UNSPECIFIED.,.F.,.F.,(4,2,4),(-0.0254390562091683,-0.0127192554937957,
0.),.UNSPECIFIED.);
#1424=B_SPLINE_CURVE_WITH_KNOTS('',3,(#55171,#55172,#55173,#55174,#55175,
#55176,#55177,#55178,#55179,#55180),.UNSPECIFIED.,.F.,.F.,(4,2,2,2,4),(0.,
0.0166816603056456,0.0333322760364837,0.0499757597117436,0.066663975095607),
 .UNSPECIFIED.);
#1425=B_SPLINE_CURVE_WITH_KNOTS('',3,(#55207,#55208,#55209,#55210,#55211,
#55212,#55213,#55214,#55215,#55216,#55217,#55218,#55219,#55220,#55221,#55222,
#55223,#55224,#55225,#55226,#55227,#55228,#55229,#55230,#55231,#55232,#55233,
#55234,#55235,#55236,#55237,#55238,#55239,#55240,#55241,#55242,#55243,#55244,
#55245,#55246,#55247,#55248,#55249,#55250,#55251,#55252,#55253,#55254,#55255,
#55256,#55257,#55258,#55259,#55260,#55261,#55262,#55263,#55264,#55265,#55266,
#55267,#55268,#55269,#55270),.UNSPECIFIED.,.F.,.F.,(4,3,3,3,3,3,3,3,3,3,
3,3,3,3,3,3,3,3,3,3,3,4),(0.,0.948237676895928,2.04200576184201,3.37474848426459,
4.40850535538508,5.30596315772473,5.58045964467773,6.71900177794048,8.10021196688407,
9.27267325358068,10.1040285365416,10.4451345402773,10.8737182939327,11.3495434571161,
11.699840638544,11.8670612467535,12.5378975955484,13.1340007751306,13.642280142205,
14.1090493942805,14.5397893196166,14.6803195994),.UNSPECIFIED.);
#1426=B_SPLINE_CURVE_WITH_KNOTS('',3,(#55285,#55286,#55287,#55288,#55289,
#55290),.UNSPECIFIED.,.F.,.F.,(4,2,4),(-0.0251203830131541,-0.0125600904510716,
0.),.UNSPECIFIED.);
#1427=B_SPLINE_CURVE_WITH_KNOTS('',3,(#55311,#55312,#55313,#55314,#55315,
#55316,#55317,#55318,#55319,#55320,#55321,#55322,#55323,#55324,#55325,#55326,
#55327,#55328,#55329,#55330,#55331,#55332,#55333,#55334,#55335,#55336,#55337,
#55338,#55339,#55340,#55341,#55342,#55343,#55344,#55345,#55346,#55347,#55348,
#55349,#55350),.UNSPECIFIED.,.F.,.F.,(4,3,3,3,3,3,3,3,3,3,3,3,3,4),(0.,
0.070670504624755,0.148932316631556,0.249833176006254,0.34320409673537,
0.421793259367904,0.490751031937973,0.500382422000438,0.579388004174185,
0.668243342711819,0.83412167135591,0.917060835677955,0.993028978346361,
1.),.UNSPECIFIED.);
#1428=B_SPLINE_CURVE_WITH_KNOTS('',3,(#55365,#55366,#55367,#55368,#55369,
#55370,#55371,#55372,#55373,#55374,#55375,#55376,#55377,#55378,#55379,#55380,
#55381,#55382,#55383,#55384,#55385,#55386,#55387,#55388,#55389,#55390,#55391,
#55392,#55393,#55394,#55395),.UNSPECIFIED.,.F.,.F.,(4,3,3,3,3,3,3,3,3,3,
4),(0.,0.244795327918776,0.502847705033982,0.780409654548611,1.09688525358519,
1.52122108872658,1.83404989561042,2.11578718796133,2.37921313711243,2.62468126213374,
2.75757599775),.UNSPECIFIED.);
#1429=B_SPLINE_CURVE_WITH_KNOTS('',3,(#55435,#55436,#55437,#55438,#55439,
#55440,#55441,#55442,#55443,#55444,#55445,#55446,#55447,#55448,#55449,#55450,
#55451,#55452,#55453,#55454,#55455,#55456,#55457,#55458,#55459,#55460,#55461,
#55462,#55463,#55464,#55465,#55466,#55467,#55468,#55469,#55470,#55471,#55472,
#55473,#55474,#55475,#55476,#55477,#55478,#55479,#55480,#55481,#55482,#55483,
#55484,#55485,#55486,#55487,#55488,#55489,#55490,#55491,#55492,#55493,#55494,
#55495,#55496,#55497,#55498,#55499,#55500,#55501),.UNSPECIFIED.,.F.,.F.,
(4,3,3,3,3,3,3,3,3,3,3,3,3,3,3,3,3,3,3,3,3,3,4),(0.,0.150485130188399,0.30297850459967,
0.457031628712122,0.561567306255,0.709215379177615,0.854264253416426,0.913473553147556,
1.04884917352124,1.12559454297,1.28001930589065,1.43693558960681,1.58742667059295,
1.69044089606,1.82557173927566,1.8394563651115,1.98772408517656,2.13847260473739,
2.25475688458,2.40866618427487,2.56165891031834,2.71215471728285,2.77932659819),
 .UNSPECIFIED.);
#1430=B_SPLINE_CURVE_WITH_KNOTS('',3,(#55530,#55531,#55532,#55533,#55534,
#55535,#55536,#55537,#55538,#55539,#55540,#55541,#55542,#55543,#55544,#55545,
#55546,#55547,#55548,#55549,#55550,#55551),.UNSPECIFIED.,.F.,.F.,(4,3,3,
3,3,3,3,4),(0.,0.528382896990167,1.08470689628943,1.66556978220358,2.28030783605745,
2.98182977652019,3.78815962830722,4.53770086709),.UNSPECIFIED.);
#1431=B_SPLINE_CURVE_WITH_KNOTS('',3,(#55565,#55566,#55567,#55568,#55569,
#55570,#55571,#55572,#55573,#55574),.UNSPECIFIED.,.F.,.F.,(4,2,2,2,4),(0.,
0.0110292280070327,0.0220815628933709,0.0331350655826503,0.0441631624440211),
 .UNSPECIFIED.);
#1432=B_SPLINE_CURVE_WITH_KNOTS('',3,(#55631,#55632,#55633,#55634,#55635,
#55636,#55637,#55638,#55639,#55640,#55641,#55642,#55643,#55644,#55645,#55646,
#55647,#55648,#55649,#55650,#55651,#55652,#55653,#55654,#55655,#55656,#55657,
#55658,#55659,#55660,#55661,#55662,#55663,#55664,#55665,#55666,#55667,#55668,
#55669,#55670,#55671,#55672,#55673,#55674,#55675,#55676,#55677,#55678,#55679,
#55680,#55681,#55682,#55683,#55684,#55685,#55686,#55687,#55688,#55689,#55690,
#55691,#55692,#55693,#55694,#55695,#55696,#55697,#55698,#55699,#55700,#55701,
#55702,#55703,#55704,#55705,#55706,#55707,#55708,#55709,#55710,#55711,#55712,
#55713,#55714,#55715,#55716,#55717,#55718,#55719,#55720,#55721,#55722,#55723,
#55724,#55725,#55726,#55727,#55728,#55729,#55730,#55731,#55732,#55733,#55734,
#55735,#55736),.UNSPECIFIED.,.F.,.F.,(4,3,3,3,3,3,3,3,3,3,3,3,3,3,3,3,3,
3,3,3,3,3,3,3,3,3,3,3,3,3,3,3,3,3,3,4),(0.,0.0384119876990658,0.0763318975960008,
0.113412177947531,0.124999999999992,0.160716651462973,0.187499999999989,
0.218749999999986,0.232928769092456,0.246751174516542,0.249999999999984,
0.282386237316996,0.31654907127058,0.350680938752922,0.386159172447775,
0.419037573131334,0.455347724810625,0.489388492009961,0.497366796822306,
0.497748630780966,0.497988260492532,0.498153598164076,0.499133766917662,
0.499622894098407,0.499829505667003,0.499975189523554,0.500092687390758,
0.554153889445409,0.611580585028303,0.671171736573759,0.727934368287542,
0.770051355331336,0.840365849439072,0.913615318512178,0.990483335368595,
1.),.UNSPECIFIED.);
#1433=B_SPLINE_CURVE_WITH_KNOTS('',3,(#55740,#55741,#55742,#55743,#55744,
#55745,#55746,#55747,#55748,#55749,#55750,#55751,#55752,#55753,#55754,#55755,
#55756,#55757,#55758,#55759,#55760,#55761,#55762,#55763,#55764,#55765,#55766,
#55767,#55768,#55769,#55770,#55771,#55772,#55773,#55774,#55775,#55776,#55777,
#55778,#55779,#55780,#55781,#55782,#55783,#55784,#55785,#55786,#55787,#55788),
 .UNSPECIFIED.,.F.,.F.,(4,3,3,3,3,3,3,3,3,3,3,3,3,3,3,3,4),(0.,0.0676604284666797,
0.135784861932871,0.20460798040263,0.25,0.319653372776603,0.389866426888844,
0.437436993869913,0.504795728664956,0.576501433821266,0.649794474217745,
0.722270051336813,0.75,0.817235207241609,0.882009314671392,0.943423886769645,
1.),.UNSPECIFIED.);
#1434=B_SPLINE_CURVE_WITH_KNOTS('',3,(#55789,#55790,#55791,#55792,#55793,
#55794),.UNSPECIFIED.,.F.,.F.,(4,2,4),(3.06785140422797E-6,0.00589378101525545,
0.00795361422578012),.UNSPECIFIED.);
#1435=B_SPLINE_CURVE_WITH_KNOTS('',5,(#55852,#55853,#55854,#55855,#55856,
#55857,#55858,#55859,#55860),.UNSPECIFIED.,.F.,.F.,(6,3,6),(0.,0.70000977750811,
1.),.UNSPECIFIED.);
#1436=B_SPLINE_CURVE_WITH_KNOTS('',3,(#55861,#55862,#55863,#55864,#55865,
#55866,#55867,#55868,#55869,#55870,#55871,#55872,#55873,#55874,#55875,#55876),
 .UNSPECIFIED.,.F.,.F.,(4,3,3,3,3,4),(0.,0.310429118799804,0.624797217736552,
0.699629793433942,0.877551619350703,1.),.UNSPECIFIED.);
#1437=B_SPLINE_CURVE_WITH_KNOTS('',5,(#55934,#55935,#55936,#55937,#55938,
#55939,#55940,#55941,#55942),.UNSPECIFIED.,.F.,.F.,(6,3,6),(0.,0.420445966361648,
1.),.UNSPECIFIED.);
#1438=B_SPLINE_CURVE_WITH_KNOTS('',3,(#55943,#55944,#55945,#55946,#55947,
#55948,#55949,#55950,#55951,#55952,#55953,#55954,#55955,#55956,#55957,#55958,
#55959,#55960,#55961,#55962,#55963,#55964,#55965,#55966,#55967,#55968,#55969,
#55970,#55971,#55972,#55973,#55974,#55975,#55976,#55977,#55978,#55979,#55980,
#55981,#55982,#55983,#55984,#55985,#55986,#55987,#55988,#55989,#55990,#55991,
#55992,#55993,#55994,#55995,#55996,#55997),.UNSPECIFIED.,.F.,.F.,(4,3,3,
3,3,3,3,3,3,3,3,3,3,3,3,3,3,3,4),(0.,0.0948842995124858,0.190085202830028,
0.285409913484093,0.378133360715178,0.423302343602271,0.49609374999998,
0.499550986594487,0.49999999999998,0.557470780273894,0.613908528426856,
0.669611200661826,0.724088620846792,0.74999999999999,0.802588612033394,
0.853469118232013,0.903394163463505,0.951763239695998,1.),.UNSPECIFIED.);
#1439=B_SPLINE_CURVE_WITH_KNOTS('',3,(#56052,#56053,#56054,#56055,#56056,
#56057,#56058,#56059,#56060,#56061,#56062,#56063,#56064),.UNSPECIFIED.,
 .F.,.F.,(4,3,3,3,4),(0.,0.394963839602928,0.529543868594593,0.809415847321762,
1.),.UNSPECIFIED.);
#1440=B_SPLINE_CURVE_WITH_KNOTS('',3,(#56070,#56071,#56072,#56073,#56074,
#56075,#56076,#56077,#56078,#56079,#56080,#56081,#56082,#56083,#56084,#56085,
#56086,#56087,#56088,#56089,#56090,#56091,#56092,#56093,#56094,#56095,#56096,
#56097,#56098,#56099,#56100,#56101,#56102,#56103,#56104,#56105,#56106,#56107,
#56108,#56109,#56110,#56111,#56112,#56113,#56114,#56115,#56116,#56117,#56118),
 .UNSPECIFIED.,.F.,.F.,(4,3,3,3,3,3,3,3,3,3,3,3,3,3,3,3,4),(1.85172896462502E-10,
0.0694020177073269,0.138700016353406,0.207902958120875,0.27699293171057,
0.346014007423806,0.414958141095058,0.437324236739737,0.50765870411793,
0.575665169523303,0.643655775825584,0.711642092460888,0.779635683547978,
0.847672155976127,0.915732654483638,0.983852595780531,0.999999975765285),
 .UNSPECIFIED.);
#1441=B_SPLINE_CURVE_WITH_KNOTS('',3,(#56120,#56121,#56122,#56123,#56124,
#56125,#56126,#56127,#56128,#56129,#56130,#56131,#56132,#56133,#56134,#56135,
#56136,#56137,#56138),.UNSPECIFIED.,.F.,.F.,(4,3,3,3,3,3,4),(1.56090158029,
1.97847928202979,2.40343448569499,2.52299916049,2.76927079046744,2.93187648001,
2.93530749734),.UNSPECIFIED.);
#1442=B_SPLINE_CURVE_WITH_KNOTS('',5,(#56140,#56141,#56142,#56143,#56144,
#56145,#56146,#56147,#56148,#56149,#56150,#56151,#56152,#56153,#56154),
 .UNSPECIFIED.,.F.,.F.,(6,3,3,3,6),(3.22008961045,5.63866638969,7.2508178231,
8.95983620486,8.97249770267),.UNSPECIFIED.);
#1443=B_SPLINE_CURVE_WITH_KNOTS('',3,(#56166,#56167,#56168,#56169,#56170,
#56171,#56172,#56173,#56174,#56175,#56176,#56177,#56178,#56179,#56180,#56181,
#56182,#56183,#56184,#56185,#56186,#56187),.UNSPECIFIED.,.F.,.F.,(4,3,3,
3,3,3,3,4),(0.595163146152,1.08064893071393,1.40157444353,1.97827761057397,
2.70225888679198,3.29249008213981,3.42624016301,3.46611471078),
 .UNSPECIFIED.);
#1444=B_SPLINE_CURVE_WITH_KNOTS('',3,(#56193,#56194,#56195,#56196,#56197,
#56198,#56199,#56200,#56201,#56202,#56203,#56204,#56205,#56206,#56207,#56208,
#56209,#56210,#56211,#56212,#56213,#56214,#56215,#56216,#56217,#56218,#56219,
#56220),.UNSPECIFIED.,.F.,.F.,(4,3,3,3,3,3,3,3,3,4),(0.0737511725012,0.120582377595235,
0.156939526058,0.213622987505703,0.240560274088,0.296963246825959,0.324594419288,
0.356043030607,0.361284468446,0.36600685554),.UNSPECIFIED.);
#1445=B_SPLINE_CURVE_WITH_KNOTS('',5,(#56226,#56227,#56228,#56229,#56230,
#56231,#56232,#56233,#56234),.UNSPECIFIED.,.F.,.F.,(6,3,6),(7.03940069458791E-8,
0.360882270523195,1.),.UNSPECIFIED.);
#1446=B_SPLINE_CURVE_WITH_KNOTS('',3,(#56236,#56237,#56238,#56239,#56240,
#56241,#56242,#56243,#56244,#56245,#56246,#56247,#56248,#56249,#56250,#56251,
#56252,#56253,#56254,#56255,#56256,#56257,#56258,#56259,#56260,#56261,#56262,
#56263,#56264,#56265,#56266,#56267,#56268,#56269,#56270,#56271,#56272,#56273,
#56274,#56275,#56276,#56277,#56278,#56279,#56280,#56281,#56282,#56283,#56284,
#56285,#56286,#56287,#56288,#56289,#56290,#56291,#56292,#56293,#56294,#56295,
#56296,#56297,#56298,#56299,#56300,#56301,#56302,#56303,#56304,#56305,#56306,
#56307,#56308,#56309,#56310,#56311,#56312,#56313,#56314,#56315,#56316,#56317,
#56318,#56319,#56320,#56321,#56322,#56323,#56324,#56325,#56326),
 .UNSPECIFIED.,.F.,.F.,(4,3,3,3,3,3,3,3,3,3,3,3,3,3,3,3,3,3,3,3,3,3,3,3,
3,3,3,3,3,3,4),(7.24577941808172E-8,0.0512940021506198,0.103630723688098,
0.125000000000011,0.179593986387468,0.187500000000017,0.218750000000019,
0.234375000000021,0.242187500000021,0.248234663203568,0.250000000000022,
0.290930951812491,0.331940468398339,0.337768593684404,0.375000000000028,
0.417102508489356,0.459628379401037,0.496093750000034,0.498046875000034,
0.499027252197299,0.499516483396325,0.499778569489927,0.49997746513499,
0.500101039385769,0.576525095455382,0.652447461005577,0.72856119175266,
0.811259005869195,0.889711323751863,0.970201629824757,1.),.UNSPECIFIED.);
#1447=B_SPLINE_CURVE_WITH_KNOTS('',3,(#56332,#56333,#56334,#56335,#56336,
#56337,#56338,#56339,#56340,#56341,#56342,#56343,#56344,#56345,#56346,#56347,
#56348,#56349,#56350,#56351,#56352,#56353,#56354,#56355,#56356,#56357,#56358,
#56359),.UNSPECIFIED.,.F.,.F.,(4,3,3,3,3,3,3,3,3,4),(0.0737511725012,0.120582377595233,
0.156939526058,0.213622987505703,0.240560274088,0.296963246825932,0.324594419288,
0.356043030607,0.361284468446,0.36600685554),.UNSPECIFIED.);
#1448=B_SPLINE_CURVE_WITH_KNOTS('',3,(#56365,#56366,#56367,#56368,#56369,
#56370,#56371,#56372,#56373,#56374,#56375,#56376,#56377,#56378,#56379,#56380,
#56381,#56382,#56383,#56384,#56385,#56386),.UNSPECIFIED.,.F.,.F.,(4,3,3,
3,3,3,3,4),(0.595163146152,1.080648930714,1.40157444353,1.97827761057532,
2.70225888679266,3.29249008214117,3.42624016301,3.46611471078),
 .UNSPECIFIED.);
#1449=B_SPLINE_CURVE_WITH_KNOTS('',5,(#56426,#56427,#56428,#56429,#56430,
#56431),.UNSPECIFIED.,.F.,.F.,(6,6),(0.,1.),.UNSPECIFIED.);
#1450=B_SPLINE_CURVE_WITH_KNOTS('',3,(#56470,#56471,#56472,#56473,#56474,
#56475,#56476,#56477,#56478,#56479,#56480,#56481,#56482,#56483,#56484,#56485),
 .UNSPECIFIED.,.F.,.F.,(4,3,3,3,3,4),(0.,0.207236770649871,0.449803912628789,
0.724901956314395,0.939507656121702,1.),.UNSPECIFIED.);
#1451=B_SPLINE_CURVE_WITH_KNOTS('',5,(#56581,#56582,#56583,#56584,#56585,
#56586,#56587,#56588,#56589),.UNSPECIFIED.,.F.,.F.,(6,3,6),(0.,0.570764276223718,
1.),.UNSPECIFIED.);
#1452=B_SPLINE_CURVE_WITH_KNOTS('',3,(#56622,#56623,#56624,#56625),
 .UNSPECIFIED.,.F.,.F.,(4,4),(1.03670984253,1.04687754685),
 .UNSPECIFIED.);
#1453=B_SPLINE_CURVE_WITH_KNOTS('',5,(#56681,#56682,#56683,#56684,#56685,
#56686,#56687,#56688,#56689),.UNSPECIFIED.,.F.,.F.,(6,3,6),(2.76258508985744E-8,
0.359893824506783,1.),.UNSPECIFIED.);
#1454=B_SPLINE_CURVE_WITH_KNOTS('',3,(#56747,#56748,#56749,#56750,#56751,
#56752,#56753,#56754,#56755,#56756,#56757,#56758,#56759,#56760,#56761,#56762,
#56763,#56764,#56765,#56766,#56767,#56768,#56769,#56770,#56771,#56772,#56773,
#56774,#56775,#56776,#56777,#56778,#56779,#56780,#56781,#56782,#56783,#56784,
#56785,#56786,#56787,#56788,#56789,#56790,#56791,#56792,#56793,#56794,#56795,
#56796,#56797,#56798,#56799,#56800,#56801,#56802,#56803,#56804,#56805,#56806,
#56807,#56808,#56809,#56810,#56811,#56812,#56813,#56814,#56815,#56816,#56817,
#56818,#56819,#56820,#56821,#56822,#56823,#56824,#56825,#56826,#56827,#56828,
#56829,#56830,#56831,#56832,#56833,#56834,#56835,#56836,#56837,#56838,#56839,
#56840,#56841,#56842,#56843),.UNSPECIFIED.,.F.,.F.,(4,3,3,3,3,3,3,3,3,3,
3,3,3,3,3,3,3,3,3,3,3,3,3,3,3,3,3,3,3,3,3,3,4),(3.38230551104713E-8,0.0661085210548239,
0.130590121983721,0.196883083653977,0.250000000000032,0.331618079659059,
0.375000000000048,0.377020948134889,0.437500000000056,0.46875000000006,
0.484375000000062,0.492187500000063,0.496093750000063,0.498046875000064,
0.500000000000064,0.528452399150718,0.557731830669541,0.587365305364137,
0.617341747325477,0.625000000000077,0.65576171875008,0.685986908865822,
0.717016891932956,0.732531883466523,0.740289379233306,0.744677047469246,
0.747820353842888,0.748046875000089,0.750000000000089,0.812529999338103,
0.876411794971792,0.942357563683105,1.),.UNSPECIFIED.);
#1455=B_SPLINE_CURVE_WITH_KNOTS('',3,(#56876,#56877,#56878,#56879),
 .UNSPECIFIED.,.F.,.F.,(4,4),(1.03670984253,1.04687754685),
 .UNSPECIFIED.);
#1456=B_SPLINE_CURVE_WITH_KNOTS('',3,(#56936,#56937,#56938,#56939,#56940,
#56941,#56942,#56943,#56944,#56945,#56946,#56947,#56948,#56949,#56950,#56951,
#56952,#56953,#56954,#56955,#56956,#56957),.UNSPECIFIED.,.F.,.F.,(4,3,3,
3,3,3,3,4),(0.,0.164952116135099,0.340839944519898,0.529302228005302,0.588843624721089,
0.765500311524726,0.902274076507374,1.),.UNSPECIFIED.);
#1457=B_SPLINE_CURVE_WITH_KNOTS('',3,(#57035,#57036,#57037,#57038),
 .UNSPECIFIED.,.F.,.F.,(4,4),(0.,1.),.UNSPECIFIED.);
#1458=B_SPLINE_CURVE_WITH_KNOTS('',3,(#57077,#57078,#57079,#57080,#57081,
#57082,#57083,#57084,#57085,#57086,#57087,#57088,#57089),.UNSPECIFIED.,
 .F.,.F.,(4,3,3,3,4),(0.,0.302812745334426,0.611175192673633,0.89306501651859,
0.999999645076241),.UNSPECIFIED.);
#1459=B_SPLINE_CURVE_WITH_KNOTS('',3,(#57148,#57149,#57150,#57151,#57152,
#57153,#57154,#57155,#57156,#57157,#57158,#57159,#57160,#57161,#57162,#57163),
 .UNSPECIFIED.,.F.,.F.,(4,3,3,3,3,4),(0.,0.265384459220342,0.530768918440684,
0.765384459220342,0.96786815318798,1.),.UNSPECIFIED.);
#1460=B_SPLINE_CURVE_WITH_KNOTS('',3,(#57220,#57221,#57222,#57223,#57224,
#57225,#57226,#57227,#57228,#57229,#57230,#57231,#57232,#57233,#57234,#57235,
#57236,#57237,#57238,#57239,#57240,#57241,#57242,#57243,#57244,#57245,#57246,
#57247,#57248,#57249,#57250,#57251,#57252,#57253,#57254,#57255,#57256,#57257,
#57258,#57259,#57260,#57261,#57262,#57263,#57264,#57265,#57266,#57267,#57268),
 .UNSPECIFIED.,.F.,.F.,(4,3,3,3,3,3,3,3,3,3,3,3,3,3,3,3,4),(0.,0.076900072948699,
0.152363307739898,0.225801136908131,0.250000000000011,0.321091761249945,
0.390059812546072,0.430282639543951,0.492187500000021,0.49823793040025,
0.500000000000021,0.588209486901966,0.676836259388543,0.75000000000001,
0.850717574299832,0.949663866823197,1.),.UNSPECIFIED.);
#1461=B_SPLINE_CURVE_WITH_KNOTS('',3,(#57325,#57326,#57327,#57328,#57329,
#57330,#57331,#57332,#57333,#57334,#57335,#57336,#57337,#57338,#57339,#57340),
 .UNSPECIFIED.,.F.,.F.,(4,3,3,3,3,4),(0.,0.225369815259222,0.483809499590606,
0.692086551442115,0.90274357771896,1.),.UNSPECIFIED.);
#1462=B_SPLINE_CURVE_WITH_KNOTS('',3,(#57395,#57396,#57397,#57398,#57399,
#57400,#57401,#57402,#57403,#57404,#57405,#57406,#57407,#57408,#57409,#57410,
#57411,#57412,#57413,#57414,#57415,#57416,#57417,#57418,#57419,#57420,#57421,
#57422,#57423,#57424,#57425,#57426,#57427,#57428,#57429,#57430,#57431,#57432,
#57433,#57434,#57435,#57436,#57437,#57438,#57439,#57440,#57441,#57442,#57443,
#57444,#57445,#57446,#57447,#57448,#57449,#57450,#57451,#57452,#57453,#57454,
#57455,#57456,#57457,#57458,#57459,#57460,#57461,#57462,#57463,#57464,#57465,
#57466,#57467,#57468,#57469,#57470,#57471,#57472,#57473,#57474,#57475,#57476,
#57477,#57478,#57479,#57480,#57481,#57482,#57483,#57484,#57485,#57486,#57487,
#57488,#57489,#57490,#57491,#57492,#57493,#57494,#57495,#57496,#57497,#57498,
#57499,#57500,#57501,#57502,#57503,#57504,#57505,#57506,#57507,#57508,#57509,
#57510,#57511,#57512,#57513,#57514,#57515,#57516,#57517,#57518,#57519,#57520,
#57521,#57522,#57523,#57524,#57525,#57526,#57527),.UNSPECIFIED.,.F.,.F.,
(4,3,3,3,3,3,3,3,3,3,3,3,3,3,3,3,3,3,3,3,3,3,3,3,3,3,3,3,3,3,3,3,3,3,3,
3,3,3,3,3,3,3,3,3,4),(0.,0.0693839705898158,0.125000000000017,0.187500000000025,
0.218750000000029,0.234375000000031,0.242187500000032,0.246093750000032,
0.248046875000033,0.250000000000033,0.284634412927758,0.318997381436396,
0.352787785209862,0.375000000000025,0.407562306964218,0.437500000000021,
0.452477592263182,0.468750000000019,0.484375000000018,0.488525390625018,
0.49056816101076,0.491821161209957,0.49257078993287,0.496593121340169,0.498572862579699,
0.499804266710987,0.500267006315948,0.537432084962121,0.575039819621256,
0.61324330769772,0.652808414709024,0.693105958577131,0.721552979288567,
0.735776489644284,0.742888244822143,0.744666183616608,0.745999637712457,
0.746288571798483,0.749674538265303,0.750000000000002,0.812500000000002,
0.873474261559203,0.933084762257831,0.990543844166144,1.),.UNSPECIFIED.);
#1463=B_SPLINE_CURVE_WITH_KNOTS('',3,(#57583,#57584,#57585,#57586,#57587,
#57588,#57589,#57590,#57591,#57592,#57593,#57594,#57595),.UNSPECIFIED.,
 .F.,.F.,(4,3,3,3,4),(0.,0.242939372158968,0.486368987740473,0.730792780934889,
0.91853342156656),.UNSPECIFIED.);
#1464=B_SPLINE_CURVE_WITH_KNOTS('',3,(#57597,#57598,#57599,#57600),
 .UNSPECIFIED.,.F.,.F.,(4,4),(0.91853342156656,1.),.UNSPECIFIED.);
#1465=B_SPLINE_CURVE_WITH_KNOTS('',5,(#57602,#57603,#57604,#57605,#57606,
#57607,#57608,#57609,#57610),.UNSPECIFIED.,.F.,.F.,(6,3,6),(0.,0.0437456503794834,
1.),.UNSPECIFIED.);
#1466=B_SPLINE_CURVE_WITH_KNOTS('',3,(#57668,#57669,#57670,#57671,#57672,
#57673),.UNSPECIFIED.,.F.,.F.,(4,2,4),(0.,0.216978430582008,0.361147653076782),
 .UNSPECIFIED.);
#1467=B_SPLINE_CURVE_WITH_KNOTS('',3,(#57733,#57734,#57735,#57736,#57737,
#57738),.UNSPECIFIED.,.F.,.F.,(4,2,4),(-0.258354222257529,-0.129177105593006,
0.),.UNSPECIFIED.);
#1468=B_SPLINE_CURVE_WITH_KNOTS('',3,(#57813,#57814,#57815,#57816,#57817,
#57818),.UNSPECIFIED.,.F.,.F.,(4,2,4),(-0.258354222257541,-0.129177105593007,
0.),.UNSPECIFIED.);
#1469=B_SPLINE_CURVE_WITH_KNOTS('',3,(#57910,#57911,#57912,#57913,#57914,
#57915,#57916,#57917,#57918,#57919,#57920,#57921,#57922,#57923,#57924,#57925,
#57926,#57927,#57928,#57929,#57930,#57931,#57932,#57933,#57934,#57935,#57936,
#57937,#57938,#57939,#57940,#57941,#57942,#57943,#57944,#57945,#57946,#57947,
#57948,#57949,#57950,#57951,#57952,#57953,#57954,#57955,#57956,#57957,#57958,
#57959,#57960,#57961,#57962,#57963,#57964,#57965,#57966,#57967,#57968,#57969,
#57970,#57971,#57972,#57973,#57974,#57975,#57976,#57977,#57978,#57979,#57980,
#57981,#57982,#57983,#57984,#57985,#57986,#57987,#57988,#57989,#57990,#57991,
#57992,#57993,#57994,#57995,#57996,#57997,#57998,#57999,#58000,#58001,#58002,
#58003,#58004,#58005,#58006,#58007,#58008,#58009,#58010,#58011,#58012,#58013,
#58014,#58015,#58016,#58017,#58018,#58019,#58020,#58021,#58022,#58023,#58024,
#58025,#58026,#58027,#58028,#58029,#58030,#58031,#58032,#58033,#58034,#58035,
#58036,#58037,#58038,#58039,#58040,#58041,#58042,#58043,#58044,#58045,#58046,
#58047,#58048,#58049,#58050,#58051,#58052,#58053,#58054,#58055,#58056,#58057,
#58058,#58059,#58060,#58061,#58062,#58063,#58064,#58065,#58066,#58067,#58068,
#58069,#58070,#58071,#58072,#58073,#58074,#58075,#58076,#58077,#58078,#58079,
#58080,#58081,#58082,#58083,#58084,#58085,#58086,#58087,#58088,#58089,#58090,
#58091,#58092,#58093,#58094,#58095,#58096,#58097,#58098,#58099,#58100,#58101,
#58102,#58103,#58104,#58105,#58106,#58107,#58108,#58109,#58110,#58111,#58112,
#58113,#58114),.UNSPECIFIED.,.F.,.F.,(4,3,3,3,3,3,3,3,3,3,3,3,3,3,3,3,3,
3,3,3,3,3,3,3,3,3,3,3,3,3,3,3,3,3,3,3,3,3,3,3,3,3,3,3,3,3,3,3,3,3,3,3,3,
3,3,3,3,3,3,3,3,3,3,3,3,3,3,3,4),(13.309352184,13.323137025,13.3863594433,
14.12420843155,14.8856731093313,15.6888539595427,15.9597639966,16.8873511174641,
17.1203737742,18.1372619540516,18.2809835519,19.3636219067,20.2587429271837,
21.0960175022786,21.871126775755,22.6115369711,23.3438450692561,24.1167746190937,
24.9325083938468,25.7482421686,26.5792532013888,26.7015351032,27.4472809428227,
27.6548280379,28.374603752275,29.127256650775,29.8622469410304,30.8120080950777,
31.5487524214573,32.4808930871787,33.2657987908602,33.4130337529,34.437297417812,
35.4455607682181,36.2352334697,37.0820276885765,37.6463786218,38.4082532030519,
39.0575237739,40.2132927109806,41.3296198963854,42.1466787398524,43.4466846508938,
44.6786014526,46.0833739199895,47.3981772916748,47.4881463873789,48.0675133951128,
49.1826023586064,49.7401468403532,50.2346525230349,50.2976913221,50.6043371871572,
50.9220054878,51.2478630104204,51.5463196535,51.8055359260692,51.8585343078,
51.9934642813463,52.1351368654365,52.1707489621,52.3315300267018,52.511597748187,
52.7592184635403,52.9463039716658,53.1109033767957,53.2581518689432,53.4032370372,
53.4991626515),.UNSPECIFIED.);
#1470=B_SPLINE_CURVE_WITH_KNOTS('',3,(#58118,#58119,#58120,#58121,#58122,
#58123,#58124,#58125,#58126,#58127,#58128,#58129,#58130,#58131,#58132,#58133,
#58134,#58135,#58136,#58137,#58138,#58139,#58140,#58141,#58142,#58143,#58144,
#58145,#58146,#58147,#58148,#58149,#58150,#58151,#58152,#58153,#58154,#58155,
#58156,#58157,#58158,#58159,#58160,#58161,#58162,#58163,#58164,#58165,#58166,
#58167,#58168,#58169,#58170,#58171,#58172,#58173,#58174,#58175,#58176,#58177,
#58178,#58179,#58180,#58181,#58182,#58183,#58184,#58185,#58186,#58187,#58188,
#58189,#58190,#58191,#58192,#58193,#58194,#58195,#58196,#58197,#58198,#58199,
#58200,#58201,#58202,#58203,#58204,#58205,#58206,#58207,#58208,#58209,#58210,
#58211,#58212,#58213,#58214,#58215,#58216,#58217,#58218,#58219,#58220,#58221,
#58222,#58223,#58224,#58225,#58226,#58227,#58228,#58229,#58230,#58231,#58232,
#58233,#58234,#58235,#58236,#58237,#58238,#58239,#58240,#58241,#58242,#58243,
#58244,#58245,#58246,#58247,#58248,#58249,#58250,#58251,#58252,#58253,#58254,
#58255,#58256,#58257,#58258,#58259,#58260,#58261,#58262,#58263,#58264,#58265,
#58266,#58267,#58268,#58269,#58270,#58271,#58272,#58273,#58274,#58275,#58276,
#58277,#58278,#58279,#58280,#58281,#58282,#58283,#58284,#58285,#58286,#58287,
#58288,#58289,#58290,#58291,#58292,#58293,#58294,#58295,#58296,#58297,#58298,
#58299,#58300,#58301,#58302,#58303,#58304,#58305,#58306,#58307),
 .UNSPECIFIED.,.F.,.F.,(4,3,3,3,3,3,3,3,3,3,3,3,3,3,3,3,3,3,3,3,3,3,3,3,
3,3,3,3,3,3,3,3,3,3,3,3,3,3,3,3,3,3,3,3,3,3,3,3,3,3,3,3,3,3,3,3,3,3,3,3,
3,3,3,4),(13.0484209298,13.1985929592139,13.3595276799308,13.5385979322865,
13.7128016785,13.9893591774131,14.1906327377194,14.3771824271,14.54326308795,
14.7093437488,14.8963499782689,15.0415050705,15.2816537737298,15.5279902136833,
15.7058202332,16.5863775357757,17.5955458670479,18.9061966866262,19.4329797586,
20.311266855424,21.4702806672064,22.2257607493,23.6221512447,24.8448189225224,
25.0185417401,26.1279357243721,26.4232309792,27.450845739338,27.8279202183,
28.6310179366367,29.2326020624,30.0907997879616,30.6372839066,31.5630151799466,
32.5503655253306,33.4574539385,34.2879035210213,35.1589507142178,36.1110388869914,
36.2776239705,37.3654001731742,38.3930371789532,39.2955654086294,40.0450320001,
40.856499728,41.6679674559,42.4694699238593,43.2917945237491,44.136915507971,
45.0204388110303,45.9236134063345,46.84816360524,47.6452295392,48.4005579590137,
48.7814448095,49.8245939850343,49.9176600797,50.7203463862896,51.4551652964948,
52.1093626235535,52.1899842067,52.795745757086,53.2289587759,53.2420797137),
 .UNSPECIFIED.);
#1471=B_SPLINE_CURVE_WITH_KNOTS('',3,(#58309,#58310,#58311,#58312,#58313,
#58314,#58315,#58316,#58317,#58318,#58319,#58320,#58321,#58322,#58323,#58324,
#58325,#58326,#58327,#58328,#58329,#58330,#58331,#58332,#58333,#58334,#58335,
#58336,#58337,#58338,#58339,#58340,#58341,#58342,#58343,#58344,#58345,#58346,
#58347,#58348,#58349,#58350,#58351,#58352,#58353,#58354,#58355,#58356,#58357,
#58358,#58359,#58360,#58361,#58362,#58363,#58364,#58365,#58366,#58367,#58368,
#58369,#58370,#58371,#58372,#58373,#58374,#58375,#58376,#58377,#58378,#58379,
#58380,#58381,#58382,#58383,#58384,#58385,#58386,#58387,#58388,#58389,#58390,
#58391,#58392,#58393,#58394,#58395,#58396,#58397,#58398,#58399),
 .UNSPECIFIED.,.F.,.F.,(4,3,3,3,3,3,3,3,3,3,3,3,3,3,3,3,3,3,3,3,3,3,3,3,
3,3,3,3,3,3,4),(1.97579103232,2.07828074772114,2.18503422566924,2.30151093703245,
2.35860134499,2.50402104555128,2.68267531807239,2.74141165766,2.9137457614164,
2.93383581469,3.09971901414853,3.12625997171,3.28520678839759,3.44068202460021,
3.51110670868,3.93194807809976,4.27919611191,4.63210924602733,4.95850770531841,
5.05016737922,5.36028985569995,5.73870525373494,5.82385208673,6.211020287495,
6.51428680619734,6.59818848826,6.86631471668985,7.1224741520835,7.36521342880379,
7.47414519692,7.48619339243),.UNSPECIFIED.);
#1472=B_SPLINE_CURVE_WITH_KNOTS('',3,(#58401,#58402,#58403,#58404,#58405,
#58406,#58407,#58408,#58409,#58410,#58411,#58412,#58413,#58414,#58415,#58416,
#58417,#58418,#58419,#58420,#58421,#58422,#58423,#58424,#58425,#58426,#58427,
#58428,#58429,#58430,#58431,#58432,#58433,#58434,#58435,#58436,#58437,#58438,
#58439,#58440,#58441,#58442,#58443,#58444,#58445,#58446,#58447,#58448,#58449,
#58450,#58451,#58452,#58453,#58454,#58455,#58456,#58457,#58458,#58459,#58460,
#58461,#58462,#58463,#58464,#58465,#58466,#58467,#58468,#58469,#58470,#58471,
#58472,#58473,#58474,#58475,#58476,#58477,#58478,#58479,#58480,#58481,#58482,
#58483,#58484,#58485,#58486,#58487,#58488),.UNSPECIFIED.,.F.,.F.,(4,3,3,
3,3,3,3,3,3,3,3,3,3,3,3,3,3,3,3,3,3,3,3,3,3,3,3,3,3,4),(3.98757792105,4.37296381107402,
4.83010470053207,5.42700834471868,5.7540471061,5.91552193819,6.24545979117289,
6.5613910649,6.72371295995,6.886034855,7.21067302107,7.63677556282134,8.032077392405,
8.37387398489675,8.51083290938,8.83623063238,9.16162835537,9.58330595607059,
9.81286749338,10.1385220868,10.4641766803,10.8560732769984,11.1157021879,
11.4414966369,11.7672910859,12.2101021764744,12.6468293861861,13.074381154517,
13.1814695027,13.2292989355),.UNSPECIFIED.);
#1473=B_SPLINE_CURVE_WITH_KNOTS('',3,(#58490,#58491,#58492,#58493,#58494,
#58495,#58496,#58497,#58498,#58499,#58500,#58501,#58502,#58503,#58504,#58505,
#58506,#58507,#58508,#58509,#58510,#58511,#58512,#58513,#58514,#58515,#58516,
#58517,#58518,#58519,#58520,#58521,#58522,#58523,#58524,#58525,#58526,#58527,
#58528,#58529,#58530,#58531,#58532,#58533,#58534,#58535,#58536,#58537,#58538,
#58539,#58540,#58541,#58542,#58543,#58544,#58545,#58546,#58547,#58548,#58549,
#58550,#58551,#58552,#58553,#58554,#58555,#58556),.UNSPECIFIED.,.F.,.F.,
(4,3,3,3,3,3,3,3,3,3,3,3,3,3,3,3,3,3,3,3,3,3,4),(0.620884089829,0.716822013874948,
0.814811640695407,0.84119531409,0.940509199950627,1.04043228231547,1.06766803527,
1.16714488691394,1.26514484762101,1.29421245021,1.39419772064502,1.49551599200885,
1.52004026842,1.62238868361275,1.72429183399409,1.7458581253,1.84548984945833,
1.94348709363021,1.972411509,2.0695360714935,2.14245735488,2.17079617383,
2.17770970576),.UNSPECIFIED.);
#1474=B_SPLINE_CURVE_WITH_KNOTS('',3,(#58558,#58559,#58560,#58561,#58562,
#58563,#58564,#58565,#58566,#58567,#58568,#58569,#58570,#58571,#58572,#58573,
#58574,#58575,#58576,#58577,#58578,#58579,#58580,#58581,#58582,#58583,#58584,
#58585,#58586,#58587,#58588,#58589,#58590,#58591,#58592,#58593,#58594,#58595,
#58596,#58597,#58598,#58599,#58600,#58601,#58602,#58603,#58604,#58605,#58606,
#58607,#58608,#58609,#58610,#58611,#58612,#58613,#58614,#58615,#58616,#58617,
#58618,#58619,#58620,#58621,#58622,#58623,#58624),.UNSPECIFIED.,.F.,.F.,
(4,3,3,3,3,3,3,3,3,3,3,3,3,3,3,3,3,3,3,3,3,3,4),(8.86873667877,9.56765456322511,
10.2729436861767,10.9878758752376,11.7077824777404,12.4350615145002,13.0838534898,
13.8192347398744,14.5574383601605,15.2977913928285,16.0381171761183,16.7766041138207,
17.3137864161,18.0504471780062,18.7845067021332,19.5160468171481,20.2444500253411,
20.9691816021643,21.6873308194927,22.4015170165044,23.1087844511325,23.7914150129,
23.7986943084),.UNSPECIFIED.);
#1475=B_SPLINE_CURVE_WITH_KNOTS('',3,(#58626,#58627,#58628,#58629,#58630,
#58631,#58632,#58633,#58634,#58635,#58636,#58637,#58638,#58639,#58640,#58641,
#58642,#58643,#58644,#58645,#58646,#58647,#58648,#58649,#58650,#58651,#58652,
#58653,#58654,#58655,#58656,#58657,#58658,#58659,#58660,#58661,#58662,#58663,
#58664,#58665,#58666,#58667,#58668,#58669,#58670,#58671,#58672,#58673,#58674,
#58675,#58676,#58677,#58678,#58679,#58680,#58681,#58682,#58683,#58684,#58685,
#58686,#58687,#58688,#58689,#58690,#58691,#58692),.UNSPECIFIED.,.F.,.F.,
(4,3,3,3,3,3,3,3,3,3,3,3,3,3,3,3,3,3,3,3,3,3,4),(8.86900274924736,9.56791953010357,
10.2732073750769,10.9881379920343,11.7080429074792,12.4353200096991,13.0840615029,
13.8194427527924,14.5576463730041,15.2979994057468,16.0383251891797,16.7768121271005,
17.3139944292,18.0506551916125,18.7847147159344,19.5162548309688,20.2446580390238,
20.9693896155684,21.6875388324433,22.401725028926,23.1089924629253,23.7916230261,
23.7989023215),.UNSPECIFIED.);
#1476=B_SPLINE_CURVE_WITH_KNOTS('',3,(#58694,#58695,#58696,#58697,#58698,
#58699,#58700,#58701,#58702,#58703,#58704,#58705,#58706,#58707,#58708,#58709,
#58710,#58711,#58712,#58713,#58714,#58715,#58716,#58717,#58718,#58719,#58720,
#58721,#58722,#58723,#58724,#58725,#58726,#58727,#58728,#58729,#58730,#58731,
#58732,#58733,#58734,#58735,#58736,#58737,#58738,#58739,#58740,#58741,#58742,
#58743,#58744,#58745,#58746,#58747,#58748,#58749,#58750,#58751,#58752,#58753,
#58754,#58755,#58756,#58757,#58758,#58759,#58760),.UNSPECIFIED.,.F.,.F.,
(4,3,3,3,3,3,3,3,3,3,3,3,3,3,3,3,3,3,3,3,3,3,4),(0.620886007027,0.716872155729975,
0.814917720645,0.84119723129,0.940511117480007,1.04043420022721,1.06766995247,
1.16714680417379,1.26514676496046,1.29421436741,1.39419963807593,1.49551790965784,
1.52004218562,1.62239060093022,1.72429375142684,1.7458600425,1.84549176711273,
1.94348901169251,1.97241342619,2.06953798933515,2.14245927208,2.17079809103,
2.17771162296),.UNSPECIFIED.);
#1477=B_SPLINE_CURVE_WITH_KNOTS('',3,(#58762,#58763,#58764,#58765,#58766,
#58767,#58768,#58769,#58770,#58771,#58772,#58773,#58774,#58775,#58776,#58777,
#58778,#58779,#58780,#58781,#58782,#58783,#58784,#58785,#58786,#58787,#58788,
#58789,#58790,#58791,#58792,#58793,#58794,#58795,#58796,#58797,#58798,#58799,
#58800,#58801,#58802,#58803,#58804,#58805,#58806,#58807,#58808,#58809,#58810,
#58811,#58812,#58813,#58814,#58815,#58816,#58817,#58818,#58819,#58820,#58821,
#58822,#58823,#58824,#58825,#58826,#58827,#58828,#58829,#58830,#58831,#58832,
#58833,#58834,#58835,#58836,#58837,#58838,#58839,#58840,#58841,#58842,#58843,
#58844,#58845,#58846,#58847,#58848,#58849,#58850,#58851,#58852,#58853,#58854,
#58855,#58856,#58857,#58858),.UNSPECIFIED.,.F.,.F.,(4,3,3,3,3,3,3,3,3,3,
3,3,3,3,3,3,3,3,3,3,3,3,3,3,3,3,3,3,3,3,3,3,4),(3.96957835788,4.39597160341197,
4.83142631025598,5.2668810171,5.57677617355175,5.86532271174004,6.02614087237832,
6.40225920003408,6.59503115748336,6.95548992077255,7.25795107039535,7.67923093688714,
7.87144621262,8.29346059413677,8.52280966994,8.93355714097029,9.17417312726,
9.58477382996718,9.97944876858222,10.3091559889411,10.4557118199803,10.571368793377,
10.6388632093,10.8013830785,11.1075435152645,11.126417564,11.3027365160323,
11.4514500011,11.9118977470061,12.4712067694839,12.8675106802888,13.1811526769,
13.2112648606),.UNSPECIFIED.);
#1478=B_SPLINE_CURVE_WITH_KNOTS('',3,(#58859,#58860,#58861,#58862,#58863,
#58864,#58865,#58866,#58867,#58868,#58869,#58870,#58871,#58872,#58873,#58874,
#58875,#58876,#58877,#58878,#58879,#58880,#58881,#58882,#58883,#58884,#58885,
#58886,#58887,#58888,#58889,#58890,#58891,#58892,#58893,#58894,#58895,#58896,
#58897,#58898,#58899,#58900,#58901,#58902,#58903,#58904,#58905,#58906,#58907,
#58908,#58909,#58910,#58911,#58912,#58913,#58914,#58915,#58916,#58917,#58918,
#58919,#58920,#58921,#58922,#58923,#58924,#58925,#58926,#58927,#58928,#58929,
#58930,#58931,#58932,#58933,#58934,#58935,#58936,#58937,#58938,#58939,#58940,
#58941,#58942,#58943,#58944,#58945,#58946,#58947,#58948,#58949),
 .UNSPECIFIED.,.F.,.F.,(4,3,3,3,3,3,3,3,3,3,3,3,3,3,3,3,3,3,3,3,3,3,3,3,
3,3,3,3,3,3,4),(2.79870510475,3.04393466036784,3.30656708431892,3.56919950827,
3.86702674427847,4.2250471626441,4.34415602331,4.63129409529021,4.73138788155,
5.07553416287892,5.11861973979,5.505577329925,5.82824217543653,5.89253492006,
6.12297607298855,6.2782762368,6.62203670021294,6.66401755354,6.8891214006705,
7.08746626879966,7.24045509522,7.33801757407394,7.43260181799,7.54635634529559,
7.67608056663181,7.84610920044259,7.96861479261622,8.07891483464399,8.17911016106332,
8.26392367279,8.30631830913),.UNSPECIFIED.);
#1479=B_SPLINE_CURVE_WITH_KNOTS('',3,(#58952,#58953,#58954,#58955,#58956,
#58957,#58958,#58959,#58960,#58961,#58962,#58963,#58964,#58965,#58966,#58967,
#58968,#58969,#58970,#58971,#58972,#58973,#58974,#58975,#58976,#58977,#58978,
#58979,#58980,#58981,#58982,#58983,#58984,#58985,#58986,#58987,#58988,#58989,
#58990,#58991,#58992,#58993,#58994,#58995,#58996,#58997,#58998,#58999,#59000,
#59001,#59002,#59003,#59004,#59005,#59006,#59007,#59008,#59009,#59010,#59011,
#59012,#59013,#59014,#59015),.UNSPECIFIED.,.F.,.F.,(4,3,3,3,3,3,3,3,3,3,
3,3,3,3,3,3,3,3,3,3,3,4),(2.24719882413,2.47950959664509,2.7181592241886,
2.88911799452,3.14833691195321,3.42802670540373,3.53895765179,3.70165384248,
3.86435003317,4.18973836725,4.51381221186,4.79860489658347,4.83788605646,
5.12465109548868,5.4094896631728,5.69059563897099,5.96386594048412,6.23240174493241,
6.4936877081412,6.75497367135,6.83535944365,6.83969663211),
 .UNSPECIFIED.);
#1480=B_SPLINE_CURVE_WITH_KNOTS('',3,(#59017,#59018,#59019,#59020,#59021,
#59022,#59023,#59024,#59025,#59026,#59027,#59028,#59029,#59030,#59031,#59032,
#59033,#59034,#59035,#59036,#59037,#59038,#59039,#59040,#59041,#59042,#59043,
#59044,#59045,#59046,#59047,#59048,#59049,#59050,#59051,#59052,#59053,#59054,
#59055,#59056,#59057,#59058,#59059,#59060,#59061,#59062,#59063,#59064,#59065,
#59066,#59067,#59068,#59069,#59070,#59071,#59072,#59073,#59074,#59075,#59076,
#59077,#59078,#59079,#59080,#59081,#59082,#59083,#59084,#59085,#59086,#59087,
#59088,#59089,#59090,#59091,#59092,#59093,#59094,#59095,#59096,#59097,#59098,
#59099,#59100,#59101,#59102,#59103,#59104,#59105,#59106,#59107,#59108,#59109,
#59110,#59111,#59112,#59113,#59114,#59115,#59116,#59117,#59118,#59119,#59120,
#59121,#59122,#59123,#59124,#59125,#59126,#59127,#59128,#59129,#59130,#59131,
#59132,#59133,#59134,#59135,#59136,#59137),.UNSPECIFIED.,.F.,.F.,(4,3,3,
3,3,3,3,3,3,3,3,3,3,3,3,3,3,3,3,3,3,3,3,3,3,3,3,3,3,3,3,3,3,3,3,3,3,3,3,
3,4),(3.85962234114,4.19972391890181,4.53697841171985,4.869784285439,5.02187433899,
5.35760123169367,5.6906544867354,6.02105657040899,6.1874356314,6.45638966870391,
6.48278728797,6.74353369413089,6.90031644081217,7.10197837175744,7.30053328201393,
7.48704833849445,7.75167375530052,8.00411859419973,8.16908321302,8.40987017981997,
8.57068233883,8.77146651417,8.9722506895,9.22816232252967,9.48818563062432,
9.76109275858924,9.87702506481,10.1302745068855,10.1785749125,10.4351702200345,
10.4731717655,10.6204752146,10.7677786637,11.0253091767098,11.2837011973151,
11.3568793877,11.4511218437,11.7091168167062,11.9603884154845,12.1758537261,
12.1808522654),.UNSPECIFIED.);
#1481=B_SPLINE_CURVE_WITH_KNOTS('',3,(#59139,#59140,#59141,#59142,#59143,
#59144,#59145,#59146,#59147,#59148,#59149,#59150,#59151,#59152,#59153,#59154,
#59155,#59156,#59157,#59158,#59159,#59160,#59161,#59162,#59163,#59164,#59165,
#59166,#59167,#59168,#59169,#59170,#59171,#59172,#59173,#59174,#59175,#59176,
#59177,#59178,#59179,#59180,#59181,#59182,#59183,#59184,#59185,#59186,#59187,
#59188,#59189,#59190,#59191,#59192,#59193,#59194,#59195,#59196,#59197,#59198,
#59199,#59200,#59201,#59202,#59203,#59204,#59205,#59206,#59207,#59208,#59209,
#59210,#59211,#59212,#59213,#59214,#59215,#59216,#59217,#59218,#59219,#59220,
#59221,#59222,#59223,#59224,#59225,#59226,#59227,#59228,#59229,#59230,#59231,
#59232,#59233,#59234,#59235,#59236,#59237,#59238,#59239,#59240,#59241,#59242,
#59243,#59244,#59245,#59246,#59247,#59248,#59249,#59250,#59251,#59252,#59253,
#59254,#59255,#59256,#59257,#59258,#59259,#59260,#59261,#59262,#59263,#59264,
#59265,#59266,#59267,#59268,#59269,#59270,#59271,#59272,#59273,#59274,#59275,
#59276,#59277,#59278,#59279,#59280),.UNSPECIFIED.,.F.,.F.,(4,3,3,3,3,3,
3,3,3,3,3,3,3,3,3,3,3,3,3,3,3,3,3,3,3,3,3,3,3,3,3,3,3,3,3,3,3,3,3,3,3,3,
3,3,3,3,3,4),(4.50366397293,4.99124165569177,5.43037471844,5.89373484028,
6.35709496212,6.90400455685533,7.47912691149025,8.11630634984611,8.22021331127,
9.00207087590175,9.73645569725131,10.0610358316502,10.3759242294803,10.9668836400114,
11.5102521272997,11.9396101613,12.4394822515178,12.8992348856666,13.3423310076333,
13.7422758054098,13.7854271296,14.0100730382075,14.3250384976331,14.562738268668,
14.7102740046,14.9084134032829,14.9414943029,15.0571045639,15.1727148249,
15.3067326045136,15.4308105599538,15.5448300326044,15.6351526747,15.8376558220379,
15.9751983688068,16.095274225,16.2103083328,16.3187818774064,16.3253424406,
16.4403769587,16.6325985794226,16.8436821336366,17.1067596509336,17.3700673761745,
17.5731317933866,17.7244288223,17.7659084738,17.7760995894),
 .UNSPECIFIED.);
#1482=B_SPLINE_CURVE_WITH_KNOTS('',3,(#59284,#59285,#59286,#59287,#59288,
#59289,#59290,#59291,#59292,#59293,#59294,#59295,#59296,#59297,#59298,#59299,
#59300,#59301,#59302,#59303,#59304,#59305,#59306,#59307,#59308,#59309,#59310,
#59311,#59312,#59313,#59314,#59315,#59316,#59317,#59318,#59319,#59320,#59321,
#59322,#59323),.UNSPECIFIED.,.F.,.F.,(4,3,3,3,3,3,3,3,3,3,3,3,3,4),(0.591274134056,
0.737771024646977,0.884305624855233,1.0207914158492,1.15221742139287,1.27912445533491,
1.32390942548,1.45709767839612,1.50719219233,1.64441133416022,1.6904452675,
1.83867829106087,1.87380304476,1.88642149695),.UNSPECIFIED.);
#1483=B_SPLINE_CURVE_WITH_KNOTS('',3,(#59327,#59328,#59329,#59330,#59331,
#59332,#59333,#59334,#59335,#59336,#59337,#59338,#59339,#59340,#59341,#59342,
#59343,#59344,#59345,#59346,#59347,#59348,#59349,#59350,#59351,#59352,#59353,
#59354,#59355,#59356,#59357,#59358,#59359,#59360,#59361,#59362,#59363,#59364,
#59365,#59366,#59367,#59368,#59369,#59370,#59371,#59372,#59373,#59374,#59375,
#59376,#59377,#59378,#59379,#59380,#59381),.UNSPECIFIED.,.F.,.F.,(4,3,3,
3,3,3,3,3,3,3,3,3,3,3,3,3,3,3,4),(1.62532205434,1.8292510625355,2.03769001760317,
2.06608094185,2.288761226025,2.50697787928773,2.73188997891886,2.95680207855,
3.18629283499015,3.41149746017445,3.63033389632304,3.84717522696,4.06984785891,
4.27735501742918,4.29252049086,4.52218882627,4.73290113316675,4.75185716168,
4.7566717002),.UNSPECIFIED.);
#1484=B_SPLINE_CURVE_WITH_KNOTS('',3,(#59384,#59385,#59386,#59387,#59388,
#59389,#59390,#59391,#59392,#59393,#59394,#59395,#59396,#59397,#59398,#59399,
#59400,#59401,#59402,#59403,#59404,#59405,#59406,#59407,#59408,#59409,#59410,
#59411,#59412,#59413,#59414,#59415,#59416,#59417,#59418,#59419,#59420,#59421,
#59422,#59423,#59424,#59425,#59426,#59427,#59428,#59429,#59430,#59431,#59432,
#59433,#59434,#59435,#59436,#59437,#59438,#59439,#59440,#59441,#59442,#59443,
#59444,#59445,#59446,#59447,#59448,#59449,#59450,#59451,#59452,#59453,#59454,
#59455,#59456,#59457,#59458,#59459,#59460,#59461,#59462,#59463,#59464,#59465,
#59466,#59467,#59468,#59469,#59470,#59471,#59472,#59473,#59474,#59475,#59476,
#59477,#59478,#59479,#59480,#59481,#59482,#59483,#59484,#59485,#59486,#59487,
#59488,#59489,#59490,#59491,#59492,#59493,#59494,#59495,#59496,#59497,#59498,
#59499,#59500,#59501,#59502,#59503,#59504,#59505,#59506,#59507,#59508,#59509,
#59510,#59511,#59512,#59513,#59514,#59515,#59516,#59517,#59518,#59519,#59520,
#59521,#59522,#59523,#59524,#59525,#59526,#59527,#59528,#59529,#59530,#59531,
#59532,#59533,#59534),.UNSPECIFIED.,.F.,.F.,(4,3,3,3,3,3,3,3,3,3,3,3,3,
3,3,3,3,3,3,3,3,3,3,3,3,3,3,3,3,3,3,3,3,3,3,3,3,3,3,3,3,3,3,3,3,3,3,3,3,
3,4),(12.5665153092,12.69009921,13.2174016095,13.8698869846695,14.5642289168119,
15.3151925132145,16.0388958,16.8581279061159,17.6625886056314,17.9101510626,
18.6238243777442,18.8458744215,19.5096373001485,19.7815977804,20.44584529895,
21.059648595772,21.1100928175,21.7276111632648,22.3653169829574,22.4385878545,
23.124225370433,23.8648590976465,24.6494567737865,25.5236748237381,25.7297732797,
26.6264022970681,27.4702545905334,27.520500466,28.2933349196177,29.0051511936574,
29.3112276523,30.1086473503047,30.901548854693,31.6539457983,32.4171630493237,
32.8253410695,33.5504490487425,33.9967363407,34.9585356035503,36.0043997832878,
37.2106334827439,38.3142574004481,38.6616811225,39.8017790454581,40.9619707819579,
42.1851664159684,43.362585886113,44.531567646397,45.6794320868491,45.854753318,
45.9550547113),.UNSPECIFIED.);
#1485=B_SPLINE_CURVE_WITH_KNOTS('',3,(#59539,#59540,#59541,#59542,#59543,
#59544,#59545,#59546,#59547,#59548,#59549,#59550,#59551,#59552,#59553,#59554,
#59555,#59556,#59557,#59558,#59559,#59560,#59561,#59562,#59563,#59564,#59565,
#59566,#59567,#59568,#59569,#59570,#59571,#59572,#59573,#59574,#59575,#59576,
#59577,#59578,#59579,#59580,#59581,#59582,#59583,#59584,#59585,#59586,#59587,
#59588,#59589,#59590),.UNSPECIFIED.,.F.,.F.,(4,3,3,3,3,3,3,3,3,3,3,3,3,
3,3,3,3,4),(1.6242031795,1.7641955129598,1.91480668054345,2.07466312403716,
2.24808422551421,2.44933142681594,2.68661595806518,2.86896453197481,2.95435751105114,
3.20515307109064,3.44947321600323,3.68472165312646,3.91086811604638,4.12470379479479,
4.33276956159462,4.54416084712731,4.74069692760198,4.75555213266),
 .UNSPECIFIED.);
#1486=B_SPLINE_CURVE_WITH_KNOTS('',3,(#59594,#59595,#59596,#59597,#59598,
#59599,#59600,#59601,#59602,#59603,#59604,#59605,#59606,#59607,#59608,#59609,
#59610,#59611,#59612,#59613,#59614,#59615,#59616,#59617,#59618,#59619,#59620,
#59621,#59622,#59623,#59624,#59625,#59626,#59627,#59628,#59629,#59630,#59631,
#59632,#59633),.UNSPECIFIED.,.F.,.F.,(4,3,3,3,3,3,3,3,3,3,3,3,3,4),(0.591273571839,
0.737752285807162,0.879766304409762,0.957377792997,1.09086433302759,1.21862527059374,
1.32390886326,1.4570971165661,1.50719163011,1.64441077088749,1.69044470528,
1.83867772392408,1.87380248254,1.88642093473),.UNSPECIFIED.);
#1487=B_SPLINE_CURVE_WITH_KNOTS('',3,(#59637,#59638,#59639,#59640,#59641,
#59642,#59643,#59644,#59645,#59646,#59647,#59648,#59649,#59650,#59651,#59652,
#59653,#59654,#59655,#59656,#59657,#59658,#59659,#59660,#59661,#59662,#59663,
#59664,#59665,#59666,#59667,#59668,#59669,#59670,#59671,#59672,#59673,#59674,
#59675,#59676,#59677,#59678,#59679,#59680,#59681,#59682,#59683,#59684,#59685,
#59686,#59687,#59688,#59689,#59690,#59691,#59692,#59693,#59694,#59695,#59696,
#59697,#59698,#59699,#59700,#59701,#59702,#59703,#59704,#59705,#59706,#59707,
#59708,#59709,#59710,#59711,#59712,#59713,#59714,#59715,#59716,#59717,#59718,
#59719,#59720,#59721,#59722,#59723,#59724,#59725,#59726,#59727,#59728,#59729,
#59730,#59731,#59732,#59733,#59734,#59735,#59736,#59737,#59738,#59739,#59740,
#59741,#59742,#59743,#59744,#59745,#59746,#59747,#59748,#59749,#59750,#59751,
#59752,#59753,#59754,#59755,#59756,#59757,#59758,#59759,#59760,#59761,#59762,
#59763,#59764,#59765,#59766,#59767,#59768,#59769,#59770,#59771,#59772,#59773,
#59774,#59775,#59776,#59777,#59778,#59779,#59780,#59781),.UNSPECIFIED.,
 .F.,.F.,(4,3,3,3,3,3,3,3,3,3,3,3,3,3,3,3,3,3,3,3,3,3,3,3,3,3,3,3,3,3,3,
3,3,3,3,3,3,3,3,3,3,3,3,3,3,3,3,3,4),(2.49496263694,2.84179514601607,3.12358351517951,
3.37468226753677,3.6010877740917,3.75614411414,3.87078619317,4.03758016375783,
4.16768516830925,4.28156554397569,4.32934465344,4.49463348465464,4.68595286679397,
4.83083072763417,4.95658124471608,5.02650835018,5.14262441503,5.25238358605751,
5.25874047989,5.43431138791523,5.63242977425596,5.91002792811298,6.11508550569381,
6.18762608197,6.60014373032483,7.02708053772435,7.46356052808173,7.91555826554562,
8.03803358836,8.52379534643387,9.02744534056375,9.56874664025437,9.88322107258,
10.5307262920464,11.2570348591899,11.7377621928,12.397963307906,12.999665458703,
13.561841112136,13.6013676095,14.0675025336,14.3117517759605,14.5073368468212,
14.6122016308443,15.1160041712998,15.4419498048499,15.6049226216249,15.712383115035,
15.7678954384),.UNSPECIFIED.);
#1488=B_SPLINE_CURVE_WITH_KNOTS('',3,(#59783,#59784,#59785,#59786,#59787,
#59788,#59789,#59790,#59791,#59792,#59793,#59794,#59795,#59796,#59797,#59798,
#59799,#59800,#59801,#59802,#59803,#59804,#59805,#59806,#59807,#59808,#59809,
#59810,#59811,#59812,#59813,#59814,#59815,#59816,#59817,#59818,#59819,#59820,
#59821,#59822,#59823,#59824,#59825,#59826,#59827,#59828,#59829,#59830,#59831,
#59832,#59833,#59834,#59835,#59836,#59837,#59838,#59839,#59840,#59841,#59842,
#59843,#59844,#59845,#59846,#59847,#59848,#59849,#59850,#59851,#59852,#59853,
#59854,#59855,#59856,#59857,#59858,#59859,#59860,#59861,#59862,#59863,#59864,
#59865,#59866,#59867,#59868,#59869,#59870,#59871,#59872,#59873,#59874,#59875,
#59876,#59877,#59878,#59879,#59880,#59881,#59882,#59883,#59884,#59885,#59886,
#59887,#59888,#59889,#59890,#59891,#59892,#59893,#59894,#59895,#59896,#59897,
#59898,#59899,#59900,#59901,#59902,#59903,#59904,#59905,#59906,#59907,#59908,
#59909),.UNSPECIFIED.,.F.,.F.,(4,3,3,3,3,3,3,3,3,3,3,3,3,3,3,3,3,3,3,3,
3,3,3,3,3,3,3,3,3,3,3,3,3,3,3,3,3,3,3,3,3,3,4),(2.88912209896,3.13700724824184,
3.39458825543722,3.58392021798,3.72289252211,3.98628880886521,4.24665707065334,
4.28631003767,4.42907507566,4.57184011365,4.83048284543661,5.08100409555486,
5.1429678095,5.36927285077939,5.43868431146,5.67536287733583,5.73440081343,
5.98070533974942,6.0301432909,6.26817267571413,6.32588576837,6.57212979076101,
6.81101010914043,7.0391502779825,7.13061874999,7.36901534116979,7.53178369956,
7.73235096583,7.93291823211,8.20849768691155,8.4752234065794,8.6827158645,
8.83266433909,9.06554834733526,9.13254225469,9.45814484322078,9.78753654370285,
10.1215100985116,10.3109706634,10.6593104900296,10.8934901241,11.1848266494,
11.2103678193),.UNSPECIFIED.);
#1489=B_SPLINE_CURVE_WITH_KNOTS('',3,(#59911,#59912,#59913,#59914,#59915,
#59916,#59917,#59918,#59919,#59920,#59921,#59922,#59923,#59924,#59925,#59926,
#59927,#59928,#59929,#59930,#59931,#59932,#59933,#59934,#59935,#59936,#59937,
#59938,#59939,#59940,#59941,#59942,#59943,#59944,#59945,#59946,#59947,#59948,
#59949,#59950,#59951,#59952,#59953,#59954,#59955,#59956,#59957,#59958,#59959,
#59960,#59961,#59962,#59963,#59964,#59965,#59966,#59967,#59968,#59969,#59970,
#59971,#59972,#59973,#59974),.UNSPECIFIED.,.F.,.F.,(4,3,3,3,3,3,3,3,3,3,
3,3,3,3,3,3,3,3,3,3,3,4),(2.81282962644,3.06266228398076,3.32119792530808,
3.58514609404833,3.85885745601186,4.07803759972,4.36500988289161,4.66065264609048,
4.7151922635,5.01780193227688,5.03686033438,5.35852840527,5.72349096169794,
6.00613333041,6.30142940367959,6.33150425152,6.59883338343208,6.65687517263,
6.90228693396595,7.14631107564298,7.39033521732,7.40331879449),
 .UNSPECIFIED.);
#1490=B_SPLINE_CURVE_WITH_KNOTS('',3,(#59975,#59976,#59977,#59978,#59979,
#59980,#59981,#59982,#59983,#59984,#59985,#59986,#59987,#59988,#59989,#59990,
#59991,#59992,#59993,#59994,#59995,#59996,#59997,#59998,#59999,#60000,#60001,
#60002,#60003,#60004,#60005,#60006,#60007,#60008,#60009,#60010,#60011,#60012,
#60013,#60014,#60015,#60016,#60017,#60018,#60019,#60020,#60021,#60022,#60023,
#60024,#60025,#60026,#60027,#60028,#60029,#60030,#60031,#60032,#60033,#60034,
#60035,#60036,#60037,#60038,#60039,#60040,#60041,#60042,#60043,#60044,#60045,
#60046,#60047,#60048,#60049,#60050,#60051,#60052,#60053,#60054,#60055,#60056,
#60057,#60058,#60059,#60060,#60061,#60062,#60063,#60064,#60065,#60066,#60067,
#60068,#60069,#60070,#60071,#60072,#60073,#60074,#60075,#60076,#60077,#60078,
#60079,#60080,#60081,#60082,#60083,#60084,#60085,#60086,#60087,#60088,#60089,
#60090,#60091,#60092,#60093,#60094,#60095,#60096,#60097,#60098,#60099,#60100,
#60101,#60102,#60103,#60104,#60105,#60106,#60107,#60108,#60109,#60110,#60111,
#60112,#60113,#60114,#60115,#60116,#60117,#60118,#60119,#60120,#60121,#60122,
#60123,#60124,#60125),.UNSPECIFIED.,.F.,.F.,(4,3,3,3,3,3,3,3,3,3,3,3,3,
3,3,3,3,3,3,3,3,3,3,3,3,3,3,3,3,3,3,3,3,3,3,3,3,3,3,3,3,3,3,3,3,3,3,3,3,
3,4),(16.6199171728,16.7882414123,17.9571804763784,19.1237946395419,20.2651542998124,
21.4017824554562,22.4644640733447,22.5384106111,23.4876282272095,24.5248259815948,
25.1714775997893,25.8107789701635,26.8801413971835,27.8895685818,28.7828705984889,
29.2329471021,30.0685598834645,30.5763256225,31.5241408975413,32.4512947133434,
33.3589016805661,34.2400216773601,35.1072373135586,35.9553836369951,36.3852909182,
37.285084787083,37.9200729430749,38.3484054249084,39.078033259152,39.5193311416,
40.20147067805,40.8380785346705,40.8836102145,41.4881989858837,42.1149173319422,
42.2478892874,42.8850357315601,43.1836089333,43.8722843016629,44.1193285792,
44.8873595773554,45.7031826219889,45.990554775,46.7786481307242,47.5045421777594,
48.0421465447,48.7044889746508,49.3350094515254,49.827696459021,49.9655299284,
50.0065308028),.UNSPECIFIED.);
#1491=B_SPLINE_CURVE_WITH_KNOTS('',3,(#60128,#60129,#60130,#60131,#60132,
#60133,#60134,#60135,#60136,#60137,#60138,#60139,#60140,#60141,#60142,#60143,
#60144,#60145,#60146,#60147,#60148,#60149,#60150,#60151,#60152,#60153,#60154,
#60155,#60156,#60157,#60158,#60159,#60160,#60161,#60162,#60163,#60164,#60165,
#60166,#60167,#60168,#60169,#60170,#60171,#60172,#60173,#60174,#60175,#60176,
#60177,#60178,#60179,#60180,#60181,#60182,#60183,#60184,#60185,#60186,#60187,
#60188,#60189,#60190,#60191),.UNSPECIFIED.,.F.,.F.,(4,3,3,3,3,3,3,3,3,3,
3,3,3,3,3,3,3,3,3,3,3,4),(6.65601718416,7.29477936796371,7.93844920877978,
8.58674540795705,9.23928499675784,9.89729202723321,10.5577342961346,11.2208265785063,
11.623259991,12.2918631750371,12.960230968718,13.6273528326774,14.2922731198514,
14.9523209482512,15.6088709464739,16.2594069408208,16.6006372936,17.24679790118,
17.8853748974463,18.259922956,18.3634528429,18.3853430669),
 .UNSPECIFIED.);
#1492=B_SPLINE_CURVE_WITH_KNOTS('',3,(#60193,#60194,#60195,#60196,#60197,
#60198,#60199,#60200,#60201,#60202,#60203,#60204,#60205,#60206,#60207,#60208,
#60209,#60210,#60211,#60212,#60213,#60214,#60215,#60216,#60217,#60218,#60219,
#60220,#60221,#60222,#60223,#60224,#60225,#60226,#60227,#60228,#60229,#60230,
#60231,#60232,#60233,#60234,#60235,#60236,#60237,#60238,#60239,#60240,#60241,
#60242,#60243,#60244,#60245,#60246,#60247,#60248,#60249,#60250,#60251,#60252,
#60253,#60254,#60255,#60256,#60257,#60258,#60259,#60260,#60261,#60262,#60263,
#60264,#60265,#60266,#60267,#60268),.UNSPECIFIED.,.F.,.F.,(4,3,3,3,3,3,
3,3,3,3,3,3,3,3,3,3,3,3,3,3,3,3,3,3,3,4),(3.6079177031,3.90883706865,4.21466906474432,
4.53218264638424,4.8115951653,5.14200129762366,5.40176883821,5.76740314128159,
5.99194251112,6.37896984113116,6.80962623934222,7.28488360963019,7.76832519582,
8.20182855033449,8.64750474936071,9.07591953069402,9.50277466474551,9.79279299676506,
10.1847968843461,10.5613308583687,10.7833400669,11.1389210219272,11.4877159965757,
11.8269767713241,12.1534997188,12.1678629797),.UNSPECIFIED.);
#1493=B_SPLINE_CURVE_WITH_KNOTS('',3,(#60270,#60271,#60272,#60273,#60274,
#60275,#60276,#60277,#60278,#60279,#60280,#60281,#60282,#60283,#60284,#60285,
#60286,#60287,#60288,#60289,#60290,#60291,#60292,#60293,#60294,#60295,#60296,
#60297,#60298,#60299,#60300,#60301,#60302,#60303,#60304,#60305,#60306,#60307,
#60308,#60309,#60310,#60311,#60312,#60313,#60314,#60315,#60316,#60317,#60318,
#60319,#60320,#60321,#60322,#60323,#60324,#60325,#60326,#60327,#60328,#60329,
#60330,#60331,#60332,#60333,#60334,#60335,#60336,#60337,#60338,#60339,#60340,
#60341,#60342,#60343,#60344,#60345,#60346,#60347,#60348,#60349,#60350,#60351,
#60352,#60353,#60354,#60355,#60356,#60357,#60358,#60359,#60360,#60361,#60362,
#60363,#60364,#60365,#60366),.UNSPECIFIED.,.F.,.F.,(4,3,3,3,3,3,3,3,3,3,
3,3,3,3,3,3,3,3,3,3,3,3,3,3,3,3,3,3,3,3,3,3,4),(5.25334327713,5.71507679395458,
6.20067037733485,6.72422646913588,7.01125321047,7.45366970704,7.8960862036,
8.34468053427586,8.78087326212,9.21151474626878,9.65013812963318,10.1010680583122,
10.4599364913492,10.755057501583,11.212799144378,11.4506730327,11.8475195591173,
11.8957944479,12.3017989620678,12.3409158631,12.7831419415,13.2253680199,
13.7009269985786,14.1782614342998,14.6404182712168,14.9857329729,15.4237818735,
15.8618307742,16.3975356683301,16.9873115419291,17.6950030579161,17.8072669002,
17.830940375),.UNSPECIFIED.);
#1494=B_SPLINE_CURVE_WITH_KNOTS('',3,(#60370,#60371,#60372,#60373,#60374,
#60375,#60376,#60377,#60378,#60379,#60380,#60381,#60382,#60383,#60384,#60385,
#60386,#60387,#60388,#60389,#60390,#60391,#60392,#60393,#60394,#60395,#60396,
#60397,#60398,#60399,#60400,#60401,#60402,#60403,#60404,#60405,#60406,#60407,
#60408,#60409,#60410,#60411,#60412,#60413,#60414,#60415,#60416,#60417,#60418,
#60419,#60420,#60421,#60422,#60423,#60424,#60425,#60426,#60427,#60428,#60429,
#60430,#60431,#60432,#60433,#60434,#60435,#60436,#60437,#60438,#60439,#60440,
#60441,#60442,#60443,#60444,#60445,#60446,#60447,#60448,#60449,#60450,#60451,
#60452,#60453,#60454,#60455,#60456,#60457,#60458,#60459,#60460),
 .UNSPECIFIED.,.F.,.F.,(4,3,3,3,3,3,3,3,3,3,3,3,3,3,3,3,3,3,3,3,3,3,3,3,
3,3,3,3,3,3,4),(5.22957298235,5.72515531497929,6.23811612505594,6.78426433626665,
6.98390629531,7.59690004151861,7.87279845484386,8.57124459862821,8.73373254507,
9.17984086957932,9.60907313777,10.0483123491195,10.4844137305,10.8891125019663,
11.2738365701279,11.36693316,11.8065612589934,12.2352202864761,12.6835308024571,
13.1303519739113,13.5794071621556,14.0284623504,14.4735899231,14.9187174958,
15.3638712358,15.8090249758,16.318456840143,16.8416236232704,17.3572087860811,
17.7780978485,17.8070761317),.UNSPECIFIED.);
#1495=B_SPLINE_CURVE_WITH_KNOTS('',3,(#60462,#60463,#60464,#60465,#60466,
#60467,#60468,#60469,#60470,#60471,#60472,#60473,#60474,#60475,#60476,#60477,
#60478,#60479,#60480,#60481,#60482,#60483,#60484,#60485,#60486,#60487,#60488,
#60489,#60490,#60491,#60492,#60493,#60494,#60495,#60496,#60497,#60498,#60499,
#60500,#60501,#60502,#60503,#60504,#60505,#60506,#60507,#60508,#60509,#60510,
#60511,#60512,#60513,#60514,#60515,#60516,#60517,#60518,#60519,#60520,#60521,
#60522,#60523,#60524,#60525,#60526,#60527,#60528,#60529,#60530,#60531,#60532,
#60533,#60534,#60535,#60536,#60537,#60538,#60539,#60540,#60541,#60542,#60543,
#60544,#60545,#60546),.UNSPECIFIED.,.F.,.F.,(4,3,3,3,3,3,3,3,3,3,3,3,3,
3,3,3,3,3,3,3,3,3,3,3,3,3,3,3,4),(5.26516274934,5.60364973919554,5.94750904982777,
6.30061194587198,6.4671523865,6.83676658301042,7.2169534022643,7.60947300431465,
7.95473224321737,8.38000340982057,8.8249037638961,8.9008095338,9.35682876881741,
9.50401785273,9.99646091269704,10.1072261717,10.5612371713347,10.9769823432144,
11.366874414912,11.7306211259203,11.8905697622,12.1860647407,12.4815597193,
12.80236962685,13.1137390597323,13.4165240093164,13.7077321481745,13.7647993495,
13.8254388584),.UNSPECIFIED.);
#1496=B_SPLINE_CURVE_WITH_KNOTS('',3,(#60547,#60548,#60549,#60550,#60551,
#60552,#60553,#60554,#60555,#60556,#60557,#60558,#60559,#60560,#60561,#60562,
#60563,#60564,#60565,#60566,#60567,#60568,#60569,#60570,#60571,#60572,#60573,
#60574,#60575,#60576,#60577,#60578,#60579,#60580,#60581,#60582,#60583,#60584,
#60585,#60586,#60587,#60588,#60589,#60590,#60591,#60592,#60593,#60594,#60595,
#60596,#60597,#60598,#60599,#60600,#60601,#60602,#60603,#60604,#60605,#60606,
#60607),.UNSPECIFIED.,.F.,.F.,(4,3,3,3,3,3,3,3,3,3,3,3,3,3,3,3,3,3,3,3,
4),(6.656059514,6.70649596618,7.34364816588736,7.99077439543894,8.63810938722171,
9.29046036787606,9.94739592104111,10.610290255729,11.2756916426706,11.9437504407556,
12.5206580023,13.1894036939474,13.8555510001994,14.5190534443237,15.1792220023782,
15.8354746046203,16.4847448187666,17.1298267171795,17.7676868626226,18.3692626169,
18.3855563608),.UNSPECIFIED.);
#1497=B_SPLINE_CURVE_WITH_KNOTS('',3,(#60611,#60612,#60613,#60614,#60615,
#60616,#60617,#60618,#60619,#60620,#60621,#60622,#60623,#60624,#60625,#60626,
#60627,#60628,#60629,#60630,#60631,#60632,#60633,#60634,#60635,#60636,#60637,
#60638,#60639,#60640,#60641,#60642,#60643,#60644,#60645,#60646,#60647,#60648,
#60649,#60650,#60651,#60652,#60653,#60654,#60655,#60656,#60657,#60658,#60659,
#60660,#60661,#60662,#60663,#60664,#60665,#60666,#60667,#60668,#60669,#60670,
#60671,#60672,#60673,#60674,#60675,#60676,#60677,#60678,#60679,#60680,#60681,
#60682,#60683,#60684,#60685,#60686,#60687,#60688,#60689,#60690,#60691,#60692,
#60693,#60694,#60695,#60696,#60697,#60698),.UNSPECIFIED.,.F.,.F.,(4,3,3,
3,3,3,3,3,3,3,3,3,3,3,3,3,3,3,3,3,3,3,3,3,3,3,3,3,3,4),(-7.79281869645,
-7.67949942044,-7.42549542156316,-7.15478941327225,-6.88629582273,-6.57314502819122,
-6.43034092471,-6.03663324296969,-5.97438602668,-5.62643815484914,-5.33062385230929,
-5.06337143522,-4.81015944391811,-4.60864824296,-4.1539250507,-3.90194437733201,
-3.67105600336059,-3.46082690077013,-3.36176031805,-3.26575359933744,-3.2485926084,
-3.14531382964268,-3.0286901766774,-2.89235615658345,-2.73090076855235,
-2.60795854221919,-2.49694182442213,-2.39545292073385,-2.35004338101,-2.28525111063),
 .UNSPECIFIED.);
#1498=B_SPLINE_CURVE_WITH_KNOTS('',3,(#60700,#60701,#60702,#60703,#60704,
#60705,#60706,#60707,#60708,#60709,#60710,#60711,#60712,#60713,#60714,#60715,
#60716,#60717,#60718,#60719,#60720,#60721,#60722,#60723,#60724,#60725,#60726,
#60727,#60728,#60729,#60730,#60731,#60732,#60733,#60734,#60735,#60736,#60737,
#60738,#60739,#60740,#60741,#60742,#60743,#60744,#60745,#60746,#60747,#60748,
#60749,#60750,#60751,#60752,#60753,#60754,#60755,#60756,#60757,#60758,#60759,
#60760,#60761,#60762,#60763,#60764,#60765,#60766,#60767,#60768,#60769,#60770,
#60771,#60772,#60773,#60774,#60775,#60776,#60777,#60778,#60779,#60780,#60781,
#60782,#60783,#60784,#60785,#60786,#60787,#60788,#60789,#60790,#60791,#60792,
#60793),.UNSPECIFIED.,.F.,.F.,(4,3,3,3,3,3,3,3,3,3,3,3,3,3,3,3,3,3,3,3,
3,3,3,3,3,3,3,3,3,3,3,4),(-13.2289036984,-13.1363363987,-12.7039146576445,
-12.2656445883932,-11.8203474449897,-11.7478128989,-11.3759683318,-11.0041237647,
-10.6322757438,-10.260427723,-9.81056916950994,-9.36831267876866,-8.93752756344516,
-8.77115009928,-8.38005931279316,-8.02693833198,-7.58627963281806,-7.28260520275,
-6.91072921484,-6.72545154345561,-6.57518451173468,-6.53884477084,-6.20766710310589,
-5.85259632044063,-5.7953515875,-5.61051183579,-5.42567208408,-4.86329344259355,
-4.42659519004677,-4.04870735943222,-3.9898969375,-3.98723768815),
 .UNSPECIFIED.);
#1499=B_SPLINE_CURVE_WITH_KNOTS('',3,(#60795,#60796,#60797,#60798,#60799,
#60800,#60801,#60802,#60803,#60804,#60805,#60806,#60807,#60808,#60809,#60810,
#60811,#60812,#60813,#60814,#60815,#60816,#60817,#60818,#60819,#60820,#60821,
#60822,#60823,#60824,#60825,#60826,#60827,#60828,#60829,#60830,#60831,#60832,
#60833,#60834,#60835,#60836,#60837,#60838,#60839,#60840,#60841,#60842,#60843,
#60844,#60845,#60846,#60847,#60848,#60849,#60850,#60851,#60852,#60853,#60854,
#60855,#60856,#60857,#60858,#60859,#60860,#60861),.UNSPECIFIED.,.F.,.F.,
(4,3,3,3,3,3,3,3,3,3,3,3,3,3,3,3,3,3,3,3,3,3,4),(-2.17764450768,-2.16188924925,
-2.14608131572,-2.04937608347787,-1.95055079824093,-1.92475641533,-1.82569378496154,
-1.72535541822825,-1.66529892429,-1.56394425497464,-1.46322035284832,-1.40616268126,
-1.30612763707831,-1.20512898324395,-1.14773462447,-1.04670145974409,-0.946860935027668,
-0.88869522514,-0.791307897591113,-0.758836137641,-0.661745856495318,-0.628978582368,
-0.620875478398),.UNSPECIFIED.);
#1500=B_SPLINE_CURVE_WITH_KNOTS('',3,(#60863,#60864,#60865,#60866,#60867,
#60868,#60869,#60870,#60871,#60872,#60873,#60874,#60875,#60876,#60877,#60878,
#60879,#60880,#60881,#60882,#60883,#60884,#60885,#60886,#60887,#60888,#60889,
#60890,#60891,#60892,#60893,#60894,#60895,#60896,#60897,#60898,#60899,#60900,
#60901,#60902,#60903,#60904,#60905,#60906,#60907,#60908,#60909,#60910,#60911,
#60912,#60913,#60914,#60915,#60916,#60917,#60918,#60919,#60920,#60921,#60922,
#60923,#60924,#60925,#60926,#60927,#60928,#60929,#60930,#60931,#60932,#60933,
#60934,#60935),.UNSPECIFIED.,.F.,.F.,(4,3,3,3,3,3,3,3,3,3,3,3,3,3,3,3,3,
3,3,3,3,3,3,3,4),(-23.7990191102984,-23.5934535831,-23.1431272519468,-22.4354965963186,
-21.7218289035809,-21.0023651816132,-20.2749223320983,-19.5431341039927,
-18.807619336268,-18.0691154283988,-17.327756682932,-16.5856934993422,-15.8439026841036,
-15.565351162,-14.8278577905087,-14.0888878688926,-13.3557858843766,-12.6257415244233,
-11.8993880235048,-11.1535656220236,-10.4384244024611,-9.72763955180798,
-9.02311822061675,-8.91609841758,-8.86843301073),.UNSPECIFIED.);
#1501=B_SPLINE_CURVE_WITH_KNOTS('',3,(#60937,#60938,#60939,#60940,#60941,
#60942,#60943,#60944,#60945,#60946,#60947,#60948,#60949,#60950,#60951,#60952,
#60953,#60954,#60955,#60956,#60957,#60958,#60959,#60960,#60961,#60962,#60963,
#60964,#60965,#60966,#60967,#60968,#60969,#60970,#60971,#60972,#60973,#60974,
#60975,#60976,#60977,#60978,#60979,#60980,#60981,#60982,#60983,#60984,#60985,
#60986,#60987,#60988,#60989,#60990,#60991,#60992,#60993,#60994,#60995,#60996,
#60997,#60998,#60999,#61000,#61001,#61002,#61003,#61004,#61005,#61006,#61007,
#61008,#61009),.UNSPECIFIED.,.F.,.F.,(4,3,3,3,3,3,3,3,3,3,3,3,3,3,3,3,3,
3,3,3,3,3,3,3,4),(-23.7989336863,-23.5933107254,-23.1429840945252,-22.4353534366108,
-21.7216857415819,-21.0022220173521,-20.2747791658714,-19.5429909359402,
-18.8074761665865,-18.0689722573345,-17.3276135110272,-16.5855503268534,
-15.8437595113402,-15.5652083044,-14.8277149322353,-14.0887450106984,-13.3556430258233,
-12.625598665673,-11.8992451647312,-11.1534227635334,-10.4382815443863,
-9.7274966942919,-9.02297536384898,-8.91595555994,-8.86829015303),
 .UNSPECIFIED.);
#1502=B_SPLINE_CURVE_WITH_KNOTS('',3,(#61011,#61012,#61013,#61014,#61015,
#61016,#61017,#61018,#61019,#61020,#61021,#61022,#61023,#61024,#61025,#61026,
#61027,#61028,#61029,#61030,#61031,#61032,#61033,#61034,#61035,#61036,#61037,
#61038,#61039,#61040,#61041,#61042,#61043,#61044,#61045,#61046,#61047,#61048,
#61049,#61050,#61051,#61052,#61053,#61054,#61055,#61056,#61057,#61058,#61059,
#61060,#61061,#61062,#61063,#61064,#61065,#61066,#61067,#61068,#61069,#61070,
#61071,#61072,#61073,#61074,#61075,#61076,#61077),.UNSPECIFIED.,.F.,.F.,
(4,3,3,3,3,3,3,3,3,3,3,3,3,3,3,3,3,3,3,3,3,3,4),(-2.1776356295,-2.16188037113,
-2.1460724376,-2.04936720453685,-1.95054191829975,-1.92474753722,-1.82568490742854,
-1.7253465411801,-1.66529004618,-1.56393537591893,-1.46321147198222,-1.40615380315,
-1.3061187585445,-1.20512010447212,-1.14772574635,-1.04669258116211,-0.946852056176822,
-0.888686347023,-0.791299019961067,-0.758827259524,-0.661736983769767,-0.628969704251,
-0.620866600281),.UNSPECIFIED.);
#1503=B_SPLINE_CURVE_WITH_KNOTS('',3,(#61079,#61080,#61081,#61082,#61083,
#61084,#61085,#61086,#61087,#61088,#61089,#61090,#61091,#61092,#61093,#61094,
#61095,#61096,#61097,#61098,#61099,#61100,#61101,#61102,#61103,#61104,#61105,
#61106,#61107,#61108,#61109,#61110,#61111,#61112,#61113,#61114,#61115,#61116,
#61117,#61118,#61119,#61120,#61121,#61122,#61123,#61124,#61125,#61126,#61127,
#61128,#61129,#61130,#61131,#61132,#61133,#61134,#61135,#61136,#61137,#61138,
#61139,#61140,#61141,#61142,#61143,#61144,#61145,#61146,#61147,#61148,#61149,
#61150,#61151,#61152,#61153,#61154,#61155,#61156,#61157,#61158,#61159,#61160,
#61161,#61162,#61163,#61164,#61165,#61166,#61167,#61168,#61169,#61170,#61171,
#61172),.UNSPECIFIED.,.F.,.F.,(4,3,3,3,3,3,3,3,3,3,3,3,3,3,3,3,3,3,3,3,
3,3,3,3,3,3,3,3,3,3,3,4),(-13.2113291298,-13.1198592829,-12.7138234948033,
-12.2491997146626,-11.7479634371,-11.5635068486,-11.3790502601,-11.01025109405,
-10.6818996115644,-10.641451928,-10.4569885283,-10.2725251287,-9.89017431483876,
-9.53000452626,-9.09201113677,-8.78735838024,-8.41545051994,-8.04354265963,
-7.6036358701249,-7.14938102351304,-6.84005706681584,-6.48124957061761,
-6.15762630428405,-5.81661960069471,-5.65886522087669,-5.19480454113099,
-4.73527397296271,-4.35243553509635,-4.16101631616318,-4.05459365329759,
-3.98056776548391,-3.96959709723),.UNSPECIFIED.);
#1504=B_SPLINE_CURVE_WITH_KNOTS('',3,(#61174,#61175,#61176,#61177,#61178,
#61179,#61180,#61181,#61182,#61183,#61184,#61185,#61186,#61187,#61188,#61189,
#61190,#61191,#61192,#61193,#61194,#61195,#61196,#61197,#61198,#61199,#61200,
#61201,#61202,#61203,#61204,#61205,#61206,#61207,#61208,#61209,#61210,#61211,
#61212,#61213,#61214,#61215,#61216,#61217,#61218,#61219,#61220,#61221,#61222,
#61223,#61224,#61225,#61226,#61227,#61228,#61229,#61230,#61231,#61232,#61233,
#61234,#61235,#61236,#61237,#61238,#61239,#61240,#61241,#61242,#61243,#61244,
#61245,#61246,#61247,#61248,#61249,#61250,#61251,#61252,#61253,#61254,#61255,
#61256,#61257,#61258,#61259,#61260,#61261,#61262,#61263,#61264,#61265,#61266,
#61267,#61268,#61269,#61270),.UNSPECIFIED.,.F.,.F.,(4,3,3,3,3,3,3,3,3,3,
3,3,3,3,3,3,3,3,3,3,3,3,3,3,3,3,3,3,3,3,3,3,4),(-8.30480917216,-8.20674902705309,
-8.19221653176,-8.0877738063407,-7.97005328754931,-7.83350146987149,-7.66302190217223,
-7.53706337711518,-7.42341581646934,-7.31906007234852,-7.29528378098,-7.19860124179192,
-7.18248685409,-7.06312896319687,-6.93102711737306,-6.7599627390844,-6.61338526833548,
-6.50571033408,-6.1750621993239,-6.05323280545,-5.64559470344954,-5.60075527683,
-5.3106129931726,-4.97998265541636,-4.62489839005107,-4.23622188997,-3.91547288076966,
-3.7807289703,-3.50257938254203,-3.23689747688513,-2.9855623444676,-2.82975945536,
-2.79838908821),.UNSPECIFIED.);
#1505=B_SPLINE_CURVE_WITH_KNOTS('',3,(#61272,#61273,#61274,#61275,#61276,
#61277,#61278,#61279,#61280,#61281,#61282,#61283,#61284,#61285,#61286,#61287,
#61288,#61289,#61290,#61291,#61292,#61293,#61294,#61295,#61296,#61297,#61298,
#61299,#61300,#61301,#61302,#61303,#61304,#61305,#61306,#61307,#61308,#61309,
#61310,#61311,#61312,#61313,#61314,#61315,#61316,#61317,#61318,#61319,#61320,
#61321,#61322,#61323,#61324,#61325,#61326,#61327,#61328,#61329,#61330,#61331,
#61332,#61333,#61334,#61335,#61336,#61337,#61338,#61339,#61340,#61341,#61342,
#61343,#61344,#61345,#61346,#61347,#61348,#61349,#61350,#61351,#61352,#61353,
#61354,#61355,#61356,#61357,#61358,#61359,#61360,#61361,#61362,#61363,#61364,
#61365,#61366,#61367,#61368,#61369,#61370,#61371,#61372,#61373,#61374,#61375,
#61376,#61377,#61378,#61379,#61380,#61381,#61382,#61383,#61384,#61385,#61386,
#61387,#61388,#61389,#61390,#61391,#61392,#61393,#61394,#61395,#61396,#61397,
#61398,#61399,#61400,#61401,#61402,#61403,#61404,#61405,#61406,#61407,#61408,
#61409,#61410,#61411,#61412,#61413,#61414,#61415,#61416,#61417,#61418,#61419,
#61420,#61421,#61422,#61423,#61424,#61425,#61426,#61427,#61428,#61429,#61430,
#61431,#61432,#61433,#61434,#61435,#61436,#61437,#61438,#61439,#61440,#61441,
#61442,#61443,#61444,#61445,#61446),.UNSPECIFIED.,.F.,.F.,(4,3,3,3,3,3,
3,3,3,3,3,3,3,3,3,3,3,3,3,3,3,3,3,3,3,3,3,3,3,3,3,3,3,3,3,3,3,3,3,3,3,3,
3,3,3,3,3,3,3,3,3,3,3,3,3,3,3,3,4),(-53.5008998895,-53.3451916901284,-53.176656319643,
-52.9955204032205,-52.791135379922,-52.481916398361,-52.2794726982479,-52.1726974168,
-52.0066176910375,-51.8359554148276,-51.6537586616127,-51.4519287511538,
-51.1702440627414,-50.9427338453991,-50.8440596107,-49.9636996596638,-48.9547071229077,
-47.643973374075,-47.1169000853,-46.2401091876284,-45.0864798214665,-44.3241190945,
-42.906834582425,-41.7215633027034,-40.6182822590178,-39.6011883397494,
-38.6549810462,-37.8607076357675,-37.036273639443,-36.1743165155458,-35.2335575681182,
-34.233341794715,-33.16058908859,-32.8906058289,-32.0241966713569,-31.1105158015195,
-30.1341511136148,-29.0384970733065,-27.9400127615476,-26.9521397421388,
-26.1445609307,-25.4081132498847,-24.5844671352085,-23.8329347162207,-23.1710589742443,
-22.9473682995,-22.1867384924654,-21.3935014433163,-20.5314587518937,-19.6081583210602,
-18.6075304975,-17.5358782925033,-16.5923577579566,-16.313163739,-15.4464807336901,
-15.1660032466,-14.4038444044393,-14.0188427542,-13.30850513),
 .UNSPECIFIED.);
#1506=B_SPLINE_CURVE_WITH_KNOTS('',3,(#61449,#61450,#61451,#61452,#61453,
#61454,#61455,#61456,#61457,#61458,#61459,#61460,#61461,#61462,#61463,#61464,
#61465,#61466,#61467,#61468,#61469,#61470,#61471,#61472,#61473,#61474,#61475,
#61476,#61477,#61478,#61479,#61480,#61481,#61482,#61483,#61484,#61485,#61486,
#61487,#61488,#61489,#61490,#61491,#61492,#61493,#61494,#61495,#61496,#61497,
#61498,#61499,#61500,#61501,#61502,#61503,#61504,#61505,#61506,#61507,#61508,
#61509,#61510,#61511,#61512,#61513,#61514,#61515,#61516,#61517,#61518,#61519,
#61520,#61521,#61522,#61523,#61524,#61525,#61526,#61527,#61528,#61529,#61530,
#61531,#61532,#61533,#61534,#61535,#61536,#61537,#61538,#61539,#61540,#61541,
#61542,#61543,#61544,#61545,#61546,#61547,#61548,#61549,#61550,#61551,#61552,
#61553,#61554,#61555,#61556,#61557,#61558,#61559,#61560,#61561,#61562,#61563,
#61564,#61565,#61566,#61567,#61568,#61569,#61570,#61571,#61572,#61573,#61574,
#61575,#61576,#61577,#61578,#61579,#61580,#61581,#61582,#61583,#61584,#61585,
#61586,#61587,#61588,#61589,#61590,#61591,#61592,#61593,#61594,#61595,#61596,
#61597,#61598,#61599,#61600,#61601,#61602,#61603,#61604,#61605,#61606,#61607,
#61608,#61609,#61610,#61611,#61612,#61613,#61614,#61615,#61616,#61617,#61618,
#61619,#61620,#61621,#61622,#61623,#61624,#61625,#61626,#61627,#61628,#61629,
#61630,#61631,#61632,#61633,#61634,#61635,#61636,#61637,#61638,#61639,#61640,
#61641,#61642,#61643,#61644,#61645,#61646,#61647,#61648,#61649,#61650),
 .UNSPECIFIED.,.F.,.F.,(4,3,3,3,3,3,3,3,3,3,3,3,3,3,3,3,3,3,3,3,3,3,3,3,
3,3,3,3,3,3,3,3,3,3,3,3,3,3,3,3,3,3,3,3,3,3,3,3,3,3,3,3,3,3,3,3,3,3,3,3,
3,3,3,3,3,3,3,4),(-53.3460404053,-53.3427865087,-52.60822116117,-51.8501309764489,
-51.0468521204321,-50.5673270881,-49.6384172387309,-49.4117332356,-48.370926532647,
-48.256139383,-47.172901573675,-46.290385123257,-45.4631852964085,-44.6931867210543,
-43.9231881457,-43.1910896700299,-42.4326163740021,-41.655386537904,-40.846702077429,
-40.7712546448,-39.9111719491253,-38.9706748712524,-37.9461038688566,-37.0047521746,
-36.1296894289149,-35.1237074138,-34.1831850334,-33.3515209320406,-33.242662653,
-32.4464253978397,-31.622887139341,-30.7177557477536,-29.9241878583544,
-28.9084000075,-27.769668299622,-27.4636133133,-26.1168248606185,-25.0917528993528,
-24.5861173859,-23.0994130651888,-21.7086214585,-20.3835250606754,-19.1543842389577,
-18.8316459182,-18.3404587841209,-17.7232621803309,-17.1542493787613,-16.6759696232846,
-16.2528560288109,-15.9546703779,-15.7653246905542,-15.5401850478735,-15.3151445916,
-15.1222566797647,-14.9953808216,-14.8336231269604,-14.6756170516,-14.5309640342055,
-14.3738737358606,-14.2041627848116,-14.0359901315,-13.7860214709346,-13.6035114623165,
-13.4444369202988,-13.3963632114,-13.2512150095039,-13.2018838044,-13.1529830415),
 .UNSPECIFIED.);
#1507=B_SPLINE_CURVE_WITH_KNOTS('',3,(#61653,#61654,#61655,#61656,#61657,
#61658,#61659,#61660,#61661,#61662,#61663,#61664,#61665,#61666,#61667,#61668,
#61669,#61670,#61671,#61672,#61673,#61674,#61675,#61676,#61677,#61678,#61679,
#61680,#61681,#61682,#61683,#61684,#61685,#61686,#61687,#61688,#61689,#61690,
#61691,#61692,#61693,#61694,#61695,#61696,#61697,#61698,#61699,#61700,#61701,
#61702,#61703,#61704,#61705,#61706,#61707,#61708,#61709,#61710,#61711,#61712,
#61713,#61714,#61715,#61716,#61717,#61718,#61719,#61720,#61721,#61722,#61723,
#61724,#61725,#61726,#61727,#61728,#61729,#61730,#61731,#61732,#61733,#61734,
#61735,#61736,#61737,#61738,#61739,#61740,#61741,#61742,#61743,#61744,#61745,
#61746,#61747,#61748,#61749,#61750,#61751,#61752,#61753,#61754,#61755,#61756,
#61757,#61758,#61759,#61760,#61761,#61762,#61763,#61764,#61765,#61766,#61767,
#61768,#61769,#61770,#61771,#61772,#61773,#61774,#61775,#61776,#61777,#61778,
#61779,#61780,#61781,#61782,#61783,#61784,#61785,#61786,#61787,#61788,#61789,
#61790,#61791,#61792,#61793,#61794,#61795,#61796,#61797,#61798,#61799,#61800),
 .UNSPECIFIED.,.F.,.F.,(4,3,3,3,3,3,3,3,3,3,3,3,3,3,3,3,3,3,3,3,3,3,3,3,
3,3,3,3,3,3,3,3,3,3,3,3,3,3,3,3,3,3,3,3,3,3,3,3,3,4),(-50.0065304478,-49.9655295734,
-49.5003776209995,-48.8647346605083,-48.1990477939634,-48.0421461897,-47.3239922394653,
-46.546059887321,-45.99055442,-45.1729075981979,-44.4006897530799,-44.1193282242,
-43.4306528365354,-43.1836085783,-42.5464621396718,-42.2478889325,-41.6197270866977,
-41.0142731913314,-40.8836098595,-40.2470020031306,-39.5870400266364,-39.5193307866,
-38.8016514026391,-38.0559900546954,-37.6541457182902,-36.7245836424735,
-36.3852905632,-35.535496168716,-34.6711156567913,-33.790939725517,-32.8843725746734,
-31.9615205628221,-31.0128671534724,-30.5763255063,-29.7407127311743,-29.2329469859,
-28.3396449754151,-27.8895684656,-26.8655970551007,-25.7162996271993,-25.1653444925737,
-24.064560055184,-23.1069531953081,-22.5384104949,-21.4697437660747,-20.3631909524721,
-19.2056561621257,-17.9969487872128,-16.7882414123,-16.6199171729),
 .UNSPECIFIED.);
#1508=B_SPLINE_CURVE_WITH_KNOTS('',3,(#61802,#61803,#61804,#61805,#61806,
#61807,#61808,#61809,#61810,#61811,#61812,#61813,#61814,#61815,#61816,#61817,
#61818,#61819,#61820,#61821,#61822,#61823,#61824,#61825,#61826),
 .UNSPECIFIED.,.F.,.F.,(4,3,3,3,3,3,3,3,4),(-0.219167536337,-0.212065411498659,
-0.209869986607,-0.20125552271857,-0.189187478531417,-0.181061523730626,
-0.174173405713463,-0.169607467001,-0.167763693388021),.UNSPECIFIED.);
#1509=B_SPLINE_CURVE_WITH_KNOTS('',3,(#61828,#61829,#61830,#61831,#61832,
#61833,#61834,#61835,#61836,#61837,#61838,#61839,#61840,#61841,#61842,#61843,
#61844,#61845,#61846,#61847,#61848,#61849,#61850,#61851,#61852,#61853,#61854,
#61855,#61856,#61857,#61858,#61859,#61860,#61861,#61862,#61863,#61864,#61865,
#61866,#61867,#61868,#61869,#61870,#61871,#61872,#61873,#61874,#61875,#61876,
#61877,#61878,#61879,#61880,#61881,#61882,#61883,#61884,#61885,#61886,#61887,
#61888,#61889,#61890,#61891),.UNSPECIFIED.,.F.,.F.,(4,3,3,3,3,3,3,3,3,3,
3,3,3,3,3,3,3,3,3,3,3,4),(-4.75541642643,-4.72387222305,-4.69232801967,
-4.62924113332,-4.42053745532439,-4.25070576676,-4.03675783621436,-3.81910899772752,
-3.60004242876329,-3.38004735105967,-3.23201205664,-3.0052780124093,-2.78271542041613,
-2.72286212815,-2.50719500943497,-2.29534783281628,-2.213598844,-1.99844479337847,
-1.78837851696703,-1.66230163141,-1.62673590825417,-1.62406174599),
 .UNSPECIFIED.);
#1510=B_SPLINE_CURVE_WITH_KNOTS('',3,(#61895,#61896,#61897,#61898,#61899,
#61900,#61901,#61902,#61903,#61904,#61905,#61906,#61907,#61908,#61909,#61910,
#61911,#61912,#61913,#61914,#61915,#61916,#61917,#61918,#61919,#61920,#61921,
#61922,#61923,#61924,#61925,#61926,#61927,#61928,#61929,#61930,#61931,#61932,
#61933,#61934,#61935,#61936,#61937,#61938,#61939,#61940,#61941,#61942,#61943,
#61944,#61945,#61946),.UNSPECIFIED.,.F.,.F.,(4,3,3,3,3,3,3,3,3,3,3,3,3,
3,3,3,3,4),(-1.8860355782,-1.876230501475,-1.86804904262136,-1.86361992583938,
-1.8468152713,-1.74222710009253,-1.61996621682398,-1.57026734258,-1.43603198366343,
-1.32099299495717,-1.24895127143,-1.11387865106139,-0.97513337134255,-0.927387660673,
-0.783897981610959,-0.645270772084385,-0.605876247363,-0.591155709264),
 .UNSPECIFIED.);
#1511=B_SPLINE_CURVE_WITH_KNOTS('',3,(#61950,#61951,#61952,#61953,#61954,
#61955,#61956,#61957,#61958,#61959,#61960,#61961,#61962,#61963,#61964,#61965,
#61966,#61967,#61968,#61969,#61970,#61971,#61972,#61973,#61974,#61975,#61976,
#61977,#61978,#61979,#61980,#61981,#61982,#61983,#61984,#61985,#61986,#61987,
#61988,#61989,#61990,#61991,#61992,#61993,#61994,#61995,#61996,#61997,#61998,
#61999,#62000,#62001,#62002,#62003,#62004,#62005,#62006,#62007,#62008,#62009,
#62010,#62011,#62012,#62013,#62014,#62015,#62016,#62017,#62018,#62019,#62020,
#62021,#62022,#62023,#62024,#62025,#62026,#62027,#62028,#62029,#62030,#62031,
#62032,#62033,#62034,#62035,#62036,#62037,#62038,#62039,#62040,#62041,#62042,
#62043,#62044,#62045,#62046,#62047,#62048,#62049,#62050,#62051,#62052,#62053,
#62054,#62055,#62056,#62057,#62058,#62059,#62060,#62061,#62062,#62063,#62064,
#62065,#62066,#62067,#62068,#62069,#62070,#62071,#62072,#62073,#62074,#62075,
#62076,#62077,#62078,#62079,#62080,#62081,#62082,#62083,#62084,#62085,#62086,
#62087,#62088),.UNSPECIFIED.,.F.,.F.,(4,3,3,3,3,3,3,3,3,3,3,3,3,3,3,3,3,
3,3,3,3,3,3,3,3,3,3,3,3,3,3,3,3,3,3,3,3,3,3,3,3,3,3,3,3,3,4),(-17.8472140382,
-17.4019122389937,-17.3512488436,-16.85541857445,-16.617833683475,-16.3595883053,
-15.8637586192,-15.3045462433964,-14.7145756425834,-14.0542923973833,-13.8694359552,
-13.1009730407947,-12.8724670748,-12.2295685253444,-11.8754981945,-11.3790035319467,
-10.8840856317586,-10.3876429994243,-9.89120036709,-9.44497083276126,-9.01864480463145,
-8.655041284792,-8.46312097464113,-8.23964753863528,-7.99371675369271,-7.79717014573183,
-7.61881001009051,-7.45488131018598,-7.41888220249,-7.30472285597012,-7.29472016445,
-7.17409590447506,-7.04405617254464,-6.92223811653,-6.75802974895856,-6.55073660565142,
-6.40541579054849,-6.27111933005145,-6.14490398563562,-6.02723969347144,
-5.92885717573,-5.6476534049758,-5.35705149846824,-5.06034757923729,-4.75273035291205,
-4.57652678804,-4.57396017214),.UNSPECIFIED.);
#1512=B_SPLINE_CURVE_WITH_KNOTS('',3,(#62090,#62091,#62092,#62093,#62094,
#62095,#62096,#62097,#62098,#62099,#62100,#62101,#62102,#62103,#62104,#62105,
#62106,#62107,#62108,#62109,#62110,#62111,#62112,#62113,#62114,#62115,#62116,
#62117,#62118,#62119,#62120,#62121,#62122,#62123,#62124,#62125,#62126,#62127,
#62128,#62129,#62130,#62131,#62132,#62133,#62134,#62135,#62136,#62137,#62138,
#62139,#62140,#62141,#62142,#62143,#62144,#62145,#62146,#62147,#62148,#62149,
#62150,#62151,#62152,#62153,#62154,#62155,#62156,#62157,#62158,#62159,#62160,
#62161,#62162,#62163,#62164,#62165,#62166,#62167,#62168,#62169,#62170,#62171,
#62172,#62173,#62174,#62175,#62176,#62177,#62178,#62179,#62180,#62181,#62182,
#62183,#62184,#62185,#62186,#62187,#62188,#62189,#62190,#62191,#62192,#62193,
#62194,#62195,#62196,#62197,#62198,#62199,#62200,#62201,#62202,#62203,#62204,
#62205,#62206,#62207,#62208,#62209,#62210),.UNSPECIFIED.,.F.,.F.,(4,3,3,
3,3,3,3,3,3,3,3,3,3,3,3,3,3,3,3,3,3,3,3,3,3,3,3,3,3,3,3,3,3,3,3,3,3,3,3,
3,4),(-11.0890194561,-11.0060465091,-10.7571297503,-10.4223140055137,-10.0919171230019,
-9.76152024049,-9.427862963425,-9.09420568636,-8.76054366777,-8.59369978828,
-8.31461399497201,-8.04536355520786,-7.74133423580622,-7.55484692789209,
-7.42492523466838,-7.15925778640574,-6.90041903467715,-6.65046230229727,
-6.61192064383,-6.37656580563646,-6.15243841672,-5.91416092316544,-5.71470268512104,
-5.50378059751066,-5.33165972275241,-5.05173215616808,-4.92630401996643,
-4.65681431069814,-4.42074635735337,-4.33579570846539,-4.28137345509732,
-4.01455173363582,-3.75409956920042,-3.61454292872757,-3.48132690504573,
-3.23632060463136,-3.00229564428568,-2.88528316411284,-2.82677692402642,
-2.78998865932871,-2.76827068394),.UNSPECIFIED.);
#1513=B_SPLINE_CURVE_WITH_KNOTS('',3,(#62211,#62212,#62213,#62214,#62215,
#62216,#62217,#62218,#62219,#62220,#62221,#62222,#62223,#62224,#62225,#62226,
#62227,#62228,#62229,#62230,#62231,#62232,#62233,#62234,#62235,#62236,#62237,
#62238,#62239,#62240,#62241,#62242,#62243,#62244,#62245,#62246,#62247,#62248,
#62249,#62250,#62251,#62252,#62253,#62254,#62255,#62256,#62257,#62258,#62259,
#62260,#62261,#62262,#62263,#62264,#62265,#62266,#62267,#62268,#62269,#62270,
#62271),.UNSPECIFIED.,.F.,.F.,(4,3,3,3,3,3,3,3,3,3,3,3,3,3,3,3,3,3,3,3,
4),(-7.40337618611,-7.30024117289,-7.06600961895104,-6.8209088492883,-6.57835249804,
-6.30332631195281,-6.16026200237,-5.95121247231,-5.74216294226,-5.32460317331,
-5.11582036754,-4.90703756176,-4.604432666243,-4.31203427436253,-4.07794185412,
-3.80052244048256,-3.53509974462071,-3.27566898601775,-3.02440731543462,
-2.85217897174,-2.81287993679),.UNSPECIFIED.);
#1514=B_SPLINE_CURVE_WITH_KNOTS('',3,(#62274,#62275,#62276,#62277,#62278,
#62279,#62280,#62281,#62282,#62283,#62284,#62285,#62286,#62287,#62288,#62289,
#62290,#62291,#62292,#62293,#62294,#62295,#62296,#62297,#62298,#62299,#62300,
#62301,#62302,#62303,#62304,#62305,#62306,#62307,#62308,#62309,#62310,#62311,
#62312,#62313,#62314,#62315,#62316,#62317,#62318,#62319,#62320,#62321,#62322,
#62323,#62324,#62325,#62326,#62327,#62328,#62329,#62330,#62331,#62332,#62333,
#62334,#62335,#62336,#62337,#62338,#62339,#62340,#62341,#62342,#62343,#62344,
#62345,#62346,#62347,#62348,#62349,#62350,#62351,#62352,#62353,#62354,#62355,
#62356,#62357,#62358,#62359,#62360,#62361,#62362,#62363,#62364,#62365,#62366,
#62367,#62368,#62369,#62370,#62371,#62372,#62373,#62374,#62375,#62376,#62377,
#62378,#62379,#62380,#62381,#62382,#62383,#62384,#62385,#62386,#62387,#62388,
#62389,#62390,#62391,#62392,#62393,#62394,#62395,#62396,#62397,#62398,#62399,
#62400,#62401,#62402,#62403,#62404,#62405,#62406,#62407,#62408,#62409,#62410,
#62411,#62412,#62413,#62414,#62415,#62416,#62417,#62418,#62419,#62420,#62421),
 .UNSPECIFIED.,.F.,.F.,(4,3,3,3,3,3,3,3,3,3,3,3,3,3,3,3,3,3,3,3,3,3,3,3,
3,3,3,3,3,3,3,3,3,3,3,3,3,3,3,3,3,3,3,3,3,3,3,3,3,4),(-45.9550550567,-45.8547536634,
-44.7020593272519,-43.5325678037029,-42.3148462029271,-41.1424810446725,
-39.9829249214987,-38.8482537160837,-38.6616814006,-37.5789809595078,-36.3892933779578,
-35.390340457305,-34.4176032593006,-33.9967366188,-33.2716301060854,-32.8656396299714,
-32.4709155643619,-31.6730674084549,-30.882094563278,-30.0838824149726,
-29.3112279304,-28.6030919404868,-27.8382957062825,-27.5205007441,-26.6765064815491,
-25.7297735578,-24.8877396119559,-24.1080276682368,-23.373256104667,-22.6847835942949,
-22.4385878762,-21.77434035765,-21.156822041211,-21.1100928391,-20.4962895824888,
-19.8596314448538,-19.7815978021,-19.117834960177,-18.8458744432,-18.1322011061612,
-17.9101510843,-17.10894748536,-16.2880919017683,-16.0388958217,-15.2857278860319,
-14.5701591557272,-13.8937803934636,-13.2174016312,-12.7652853193346,-12.5665153309),
 .UNSPECIFIED.);
#1515=B_SPLINE_CURVE_WITH_KNOTS('',3,(#62423,#62424,#62425,#62426,#62427,
#62428,#62429,#62430,#62431,#62432,#62433,#62434,#62435,#62436,#62437,#62438,
#62439,#62440,#62441,#62442,#62443,#62444,#62445,#62446,#62447,#62448,#62449,
#62450,#62451,#62452,#62453,#62454,#62455,#62456,#62457,#62458,#62459,#62460,
#62461,#62462,#62463,#62464,#62465,#62466,#62467,#62468,#62469,#62470,#62471,
#62472,#62473,#62474,#62475,#62476,#62477),.UNSPECIFIED.,.F.,.F.,(4,3,3,
3,3,3,3,3,3,3,3,3,3,3,3,3,3,3,4),(-6.6978412202,-6.44998928167263,-6.19272717356715,
-5.92880591063826,-5.65745311051901,-5.37791579855118,-5.08570414740713,
-4.78670366790336,-4.48187066288165,-4.45303700515737,-4.02197464488505,
-3.67567871029374,-3.3757846822016,-3.09960655669372,-2.84547660754957,
-2.5999707008135,-2.35368976040675,-2.12340855147386,-2.10740882),
 .UNSPECIFIED.);
#1516=B_SPLINE_CURVE_WITH_KNOTS('',3,(#62479,#62480,#62481,#62482,#62483,
#62484,#62485,#62486,#62487,#62488,#62489,#62490,#62491,#62492,#62493,#62494,
#62495,#62496,#62497,#62498,#62499,#62500,#62501,#62502,#62503,#62504,#62505,
#62506,#62507,#62508,#62509,#62510,#62511,#62512,#62513,#62514,#62515,#62516,
#62517,#62518,#62519,#62520,#62521,#62522,#62523,#62524,#62525,#62526,#62527,
#62528,#62529,#62530,#62531,#62532,#62533,#62534,#62535,#62536,#62537,#62538,
#62539,#62540,#62541,#62542,#62543,#62544,#62545,#62546,#62547,#62548,#62549,
#62550,#62551,#62552,#62553,#62554,#62555,#62556,#62557,#62558,#62559,#62560,
#62561,#62562,#62563,#62564,#62565,#62566,#62567,#62568,#62569,#62570,#62571,
#62572,#62573,#62574,#62575,#62576,#62577,#62578,#62579,#62580,#62581,#62582,
#62583,#62584,#62585,#62586,#62587,#62588,#62589,#62590,#62591,#62592,#62593,
#62594,#62595,#62596,#62597,#62598,#62599,#62600,#62601,#62602,#62603,#62604,
#62605,#62606,#62607,#62608),.UNSPECIFIED.,.F.,.F.,(4,3,3,3,3,3,3,3,3,3,
3,3,3,3,3,3,3,3,3,3,3,3,3,3,3,3,3,3,3,3,3,3,3,3,3,3,3,3,3,3,3,3,3,4),(-12.1812673196,
-12.1019545715,-11.8530258523618,-11.595215506703,-11.5467858158,-11.3881500798,
-11.2295143438,-10.9699907679588,-10.9122488687,-10.7483463587,-10.5844438487,
-10.3384514976169,-10.2566501431,-10.0043239978651,-9.92881869084,-9.70732206868687,
-9.60098723862,-9.35831838515441,-9.14889513515,-8.93472094875681,-8.77284717678668,
-8.52420937980639,-8.28078037155647,-8.0453638509211,-7.82018311353108,
-7.77935654812,-7.52877970908887,-7.32110317374,-7.09200006145,-6.86289694915,
-6.5945495418842,-6.5210581838,-6.3501250021,-6.17919182041,-5.92442927962418,
-5.68485033386412,-5.49553262739,-5.20623148246893,-4.89872891457204,-4.82510489389,
-4.47179454085463,-4.15468159222,-3.87676906882,-3.85983652914),
 .UNSPECIFIED.);
#1517=B_SPLINE_CURVE_WITH_KNOTS('',3,(#62610,#62611,#62612,#62613,#62614,
#62615,#62616,#62617,#62618,#62619,#62620,#62621,#62622,#62623,#62624,#62625,
#62626,#62627,#62628,#62629,#62630,#62631,#62632,#62633,#62634,#62635,#62636,
#62637,#62638,#62639,#62640,#62641,#62642,#62643,#62644,#62645,#62646,#62647,
#62648,#62649,#62650,#62651,#62652,#62653,#62654,#62655,#62656,#62657,#62658,
#62659,#62660,#62661,#62662,#62663,#62664,#62665,#62666,#62667,#62668,#62669,
#62670,#62671,#62672,#62673,#62674,#62675,#62676,#62677,#62678,#62679,#62680,
#62681,#62682,#62683,#62684,#62685,#62686,#62687,#62688,#62689,#62690,#62691,
#62692,#62693,#62694,#62695,#62696,#62697,#62698,#62699,#62700,#62701,#62702,
#62703,#62704,#62705,#62706,#62707,#62708,#62709,#62710,#62711,#62712,#62713,
#62714,#62715,#62716,#62717,#62718,#62719,#62720,#62721,#62722,#62723,#62724,
#62725,#62726,#62727,#62728,#62729,#62730,#62731,#62732,#62733,#62734,#62735,
#62736,#62737,#62738,#62739,#62740,#62741,#62742,#62743,#62744,#62745,#62746,
#62747,#62748,#62749,#62750,#62751,#62752,#62753,#62754,#62755,#62756,#62757,
#62758,#62759,#62760),.UNSPECIFIED.,.F.,.F.,(4,3,3,3,3,3,3,3,3,3,3,3,3,
3,3,3,3,3,3,3,3,3,3,3,3,3,3,3,3,3,3,3,3,3,3,3,3,3,3,3,3,3,3,3,3,3,3,3,3,
3,4),(-17.2738332784,-17.0284868112151,-16.8153093983,-16.5064930943126,
-16.356669586,-16.0797319308535,-16.0127475115,-15.8981054324,-15.7808445708218,
-15.6585553960829,-15.5249349056484,-15.4395469722,-15.2698932931606,-15.062957071932,
-14.9385147756961,-14.8086216270683,-14.6940263327,-14.5760460181375,-14.5697715428,
-14.4565193782305,-14.4455167529,-14.291815073997,-14.1246199657078,-13.9241091491007,
-13.6878176035504,-13.5130680616142,-13.451526058,-13.0514035156419,-12.6195129795619,
-12.1624081206357,-11.6511703139133,-11.4721831186,-10.9335785602832,-10.3632144505192,
-9.74590695598728,-9.46909727915927,-8.78704121090936,-8.42694683890191,
-7.82822785856962,-7.52764856036114,-7.21067457575859,-6.62584211706413,
-6.0788387154238,-5.56229121985785,-5.4010635343667,-5.05395983406502,-4.84584110817332,
-4.42924492066666,-4.19245652259199,-4.01264873316,-4.00115394842),
 .UNSPECIFIED.);
#1518=B_SPLINE_CURVE_WITH_KNOTS('',3,(#62764,#62765,#62766,#62767,#62768,
#62769,#62770,#62771,#62772,#62773,#62774,#62775,#62776,#62777,#62778,#62779,
#62780,#62781,#62782,#62783,#62784,#62785,#62786,#62787,#62788,#62789,#62790,
#62791,#62792,#62793,#62794,#62795,#62796,#62797,#62798,#62799,#62800,#62801,
#62802,#62803,#62804,#62805,#62806,#62807,#62808,#62809),.UNSPECIFIED.,
 .F.,.F.,(4,3,3,3,3,3,3,3,3,3,3,3,3,3,3,4),(-1.88603455695,-1.86656727617,
-1.84681424904,-1.74222598447339,-1.61996499915831,-1.57026632032,-1.43603095182559,
-1.32099188319155,-1.24895024918,-1.1138776438742,-0.975132380159264,-0.927386638419,
-0.783896961730633,-0.645269714782231,-0.605875225111,-0.591154687012),
 .UNSPECIFIED.);
#1519=B_SPLINE_CURVE_WITH_KNOTS('',3,(#62813,#62814,#62815,#62816,#62817,
#62818,#62819,#62820,#62821,#62822,#62823,#62824,#62825,#62826,#62827,#62828,
#62829,#62830,#62831,#62832,#62833,#62834,#62835,#62836,#62837,#62838,#62839,
#62840,#62841,#62842,#62843,#62844,#62845,#62846,#62847,#62848,#62849,#62850,
#62851,#62852,#62853,#62854,#62855,#62856,#62857,#62858,#62859,#62860,#62861),
 .UNSPECIFIED.,.F.,.F.,(4,3,3,3,3,3,3,3,3,3,3,3,3,3,3,3,4),(-4.75656395656,
-4.60537498785813,-4.44818787789036,-4.27889046442468,-4.09863038425973,
-3.90212119682302,-3.66090058334715,-3.44155265372639,-3.23422551625958,
-2.97612342370908,-2.73021565496724,-2.49737898001046,-2.27933643879784,
-2.07018074570911,-1.86716482720178,-1.67150310968067,-1.62520881516),
 .UNSPECIFIED.);
#1520=B_SPLINE_CURVE_WITH_KNOTS('',3,(#62862,#62863,#62864,#62865,#62866,
#62867,#62868,#62869,#62870,#62871,#62872,#62873,#62874,#62875,#62876,#62877,
#62878,#62879,#62880,#62881,#62882,#62883,#62884,#62885,#62886),
 .UNSPECIFIED.,.F.,.F.,(4,3,3,3,3,3,3,3,4),(-0.219167536347,-0.212059197014113,
-0.209869986617,-0.201255522705921,-0.189187478425977,-0.181061523597616,
-0.1741734055503,-0.169607467011,-0.167763693398),.UNSPECIFIED.);
#1521=B_SPLINE_CURVE_WITH_KNOTS('',3,(#62889,#62890,#62891,#62892,#62893,
#62894,#62895,#62896,#62897,#62898,#62899,#62900,#62901,#62902,#62903,#62904,
#62905,#62906,#62907,#62908,#62909,#62910,#62911,#62912,#62913,#62914,#62915,
#62916,#62917,#62918,#62919,#62920,#62921,#62922,#62923,#62924,#62925,#62926,
#62927,#62928,#62929,#62930,#62931,#62932,#62933,#62934,#62935,#62936,#62937,
#62938,#62939,#62940,#62941,#62942,#62943,#62944,#62945,#62946,#62947,#62948,
#62949),.UNSPECIFIED.,.F.,.F.,(4,3,3,3,3,3,3,3,3,3,3,3,3,3,3,3,3,3,3,3,
4),(-18.3856123466,-18.3693186027,-17.7338457042873,-17.0822042289639,-16.4332948516141,
-15.7797891975128,-15.1220801611204,-14.4588486872985,-13.7932558597198,
-13.1250205669124,-12.5207139017,-11.8522076648893,-11.186292378156,-10.5231984210845,
-9.86372444518384,-9.20853401660924,-8.56222676146939,-7.91873801115672,
-7.27898147126907,-6.70655190271,-6.65611545055),.UNSPECIFIED.);
#1522=B_SPLINE_CURVE_WITH_KNOTS('',3,(#62951,#62952,#62953,#62954,#62955,
#62956,#62957,#62958,#62959,#62960,#62961,#62962,#62963,#62964,#62965,#62966,
#62967,#62968,#62969,#62970,#62971,#62972,#62973,#62974,#62975,#62976,#62977,
#62978,#62979,#62980,#62981,#62982,#62983,#62984,#62985,#62986,#62987,#62988,
#62989,#62990,#62991,#62992,#62993,#62994,#62995,#62996,#62997,#62998,#62999,
#63000,#63001,#63002,#63003,#63004,#63005,#63006,#63007,#63008,#63009,#63010,
#63011,#63012,#63013,#63014,#63015,#63016,#63017,#63018,#63019,#63020,#63021,
#63022,#63023,#63024,#63025,#63026,#63027,#63028,#63029,#63030,#63031,#63032,
#63033,#63034,#63035),.UNSPECIFIED.,.F.,.F.,(4,3,3,3,3,3,3,3,3,3,3,3,3,
3,3,3,3,3,3,3,3,3,3,3,3,3,3,3,4),(-12.1666998724,-11.9786962562,-11.6376009588191,
-11.2884914068467,-10.9310276199667,-10.6143846100047,-10.2318786454351,
-9.83665601387961,-9.42660550414306,-9.04238206530011,-8.59483084924109,
-8.1272682464219,-7.99998279071,-7.62059092272,-7.09680652253779,-6.64956410247717,
-6.25094224690215,-6.12491227162,-5.755282141945,-5.38565201227,-5.05920014817189,
-5.01602130474,-4.68257909391951,-4.6463905972,-4.33332998029539,-4.02503376786804,
-3.72192456507751,-3.66177393989,-3.60712399577),.UNSPECIFIED.);
#1523=B_SPLINE_CURVE_WITH_KNOTS('',3,(#63037,#63038,#63039,#63040,#63041,
#63042,#63043,#63044,#63045,#63046,#63047,#63048,#63049,#63050,#63051,#63052,
#63053,#63054,#63055,#63056,#63057,#63058,#63059,#63060,#63061,#63062,#63063,
#63064,#63065,#63066,#63067,#63068,#63069,#63070,#63071,#63072,#63073,#63074,
#63075,#63076,#63077,#63078,#63079,#63080,#63081,#63082,#63083,#63084,#63085,
#63086,#63087,#63088,#63089,#63090,#63091,#63092,#63093,#63094,#63095,#63096,
#63097,#63098,#63099,#63100,#63101,#63102,#63103,#63104,#63105,#63106,#63107,
#63108,#63109,#63110,#63111,#63112,#63113,#63114,#63115,#63116,#63117,#63118,
#63119,#63120,#63121,#63122,#63123,#63124,#63125,#63126,#63127,#63128,#63129,
#63130,#63131,#63132,#63133,#63134,#63135,#63136),.UNSPECIFIED.,.F.,.F.,
(4,3,3,3,3,3,3,3,3,3,3,3,3,3,3,3,3,3,3,3,3,3,3,3,3,3,3,3,3,3,3,3,3,4),(-17.772416875,
-17.521901514,-16.9335100063655,-16.3509832344328,-15.8162251865757,-15.7684564625,
-15.2647792762872,-14.769293572,-14.2697121268,-13.7701306816,-13.3014442440585,
-12.8657319415181,-12.7684045275,-12.3622943776427,-11.9768947679633,-11.7666783733,
-11.3217875172379,-10.877298655069,-10.7536322473,-10.3070868714199,-9.86925366913895,
-9.57637209730375,-9.14940821210187,-8.7224443269,-8.27106751604139,-7.79254976980533,
-7.70430253262,-7.19083078178567,-6.67906896927376,-6.18723057296208,-5.70660978985604,
-5.26270778945018,-5.22598900675,-5.19541482867),.UNSPECIFIED.);
#1524=B_SPLINE_CURVE_WITH_KNOTS('',3,(#63140,#63141,#63142,#63143,#63144,
#63145,#63146,#63147,#63148,#63149,#63150,#63151,#63152,#63153,#63154,#63155,
#63156,#63157,#63158,#63159,#63160,#63161,#63162,#63163,#63164,#63165,#63166,
#63167,#63168,#63169,#63170,#63171,#63172,#63173,#63174,#63175,#63176,#63177,
#63178,#63179,#63180,#63181,#63182,#63183,#63184,#63185,#63186,#63187,#63188,
#63189,#63190,#63191,#63192,#63193,#63194,#63195,#63196,#63197,#63198,#63199,
#63200,#63201,#63202,#63203,#63204,#63205,#63206,#63207,#63208,#63209,#63210,
#63211,#63212,#63213,#63214,#63215,#63216,#63217,#63218,#63219,#63220,#63221,
#63222,#63223,#63224,#63225,#63226,#63227,#63228,#63229,#63230,#63231,#63232,
#63233,#63234,#63235,#63236,#63237,#63238,#63239,#63240,#63241,#63242,#63243,
#63244,#63245),.UNSPECIFIED.,.F.,.F.,(4,3,3,3,3,3,3,3,3,3,3,3,3,3,3,3,3,
3,3,3,3,3,3,3,3,3,3,3,3,3,3,3,3,3,3,4),(-17.7593366521,-17.5082731747,-16.9919472481348,
-16.4599835808025,-15.9500345616009,-15.750791364,-15.2946015506613,-15.2446202854,
-14.8078388781449,-14.7384492068,-14.3057136278889,-13.8694237050522,-13.5442762157924,
-13.0972971028135,-12.7083210147,-12.2538973274484,-11.7931711149994,-11.6904556298,
-11.2764473929467,-10.8492913402097,-10.6739061369,-10.2365832725764,-10.1657133659,
-9.70970896481276,-9.6575205949,-9.1553358953925,-8.66383335866873,-8.15630757776936,
-7.67795613911451,-7.64878179687,-7.201975613066,-6.72017928606396,-6.1376841854597,
-5.40983099502471,-5.2053512509,-5.18156607379),.UNSPECIFIED.);
#1525=B_SPLINE_CURVE_WITH_KNOTS('',3,(#63247,#63248,#63249,#63250,#63251,
#63252,#63253,#63254,#63255,#63256,#63257,#63258,#63259,#63260,#63261,#63262,
#63263,#63264,#63265,#63266,#63267,#63268,#63269,#63270,#63271,#63272,#63273,
#63274,#63275,#63276,#63277,#63278,#63279,#63280,#63281,#63282,#63283,#63284,
#63285,#63286,#63287,#63288,#63289,#63290,#63291,#63292,#63293,#63294,#63295,
#63296,#63297,#63298,#63299,#63300,#63301,#63302,#63303,#63304,#63305,#63306,
#63307,#63308,#63309,#63310,#63311,#63312,#63313,#63314,#63315,#63316,#63317,
#63318,#63319,#63320,#63321,#63322,#63323,#63324,#63325,#63326,#63327,#63328,
#63329,#63330,#63331),.UNSPECIFIED.,.F.,.F.,(4,3,3,3,3,3,3,3,3,3,3,3,3,
3,3,3,3,3,3,3,3,3,3,3,3,3,3,3,4),(-13.8219121669,-13.5096825236108,-13.1998941240071,
-13.0694393691,-12.7498970842646,-12.4138466225267,-12.3169687025,-11.9842110392268,
-11.947857022,-11.5876140439936,-11.1992238939162,-10.7885323398095,-10.3216400674985,
-10.0989759692,-9.74353972606138,-9.48049443113105,-9.35737491835,-8.89583258585393,
-8.44881248962697,-8.02059283816397,-7.65521955896336,-7.26572917138508,
-6.88685706126507,-6.52131822386237,-6.33411128744,-5.98413683665983,-5.63575530097992,
-5.2873737653,-5.26262328413),.UNSPECIFIED.);
#1526=B_SPLINE_CURVE_WITH_KNOTS('',3,(#63332,#63333,#63334,#63335,#63336,
#63337,#63338,#63339,#63340,#63341,#63342,#63343,#63344,#63345,#63346,#63347,
#63348,#63349,#63350,#63351,#63352,#63353,#63354,#63355,#63356,#63357,#63358,
#63359,#63360,#63361,#63362,#63363,#63364,#63365,#63366,#63367,#63368,#63369,
#63370,#63371,#63372,#63373,#63374,#63375,#63376,#63377,#63378,#63379,#63380,
#63381,#63382,#63383,#63384,#63385,#63386,#63387,#63388,#63389,#63390,#63391,
#63392,#63393,#63394,#63395),.UNSPECIFIED.,.F.,.F.,(4,3,3,3,3,3,3,3,3,3,
3,3,3,3,3,3,3,3,3,3,3,4),(-18.3857494183,-18.1972119365,-18.0086744547,
-17.3704664943546,-16.7238562601433,-16.0724620532357,-15.4166996629135,
-14.7571067950976,-14.0929948370157,-13.4271604823992,-12.759986367352,
-12.3414051375,-11.6749604882608,-11.0099790390611,-10.3474170882745,-9.69024646845821,
-9.0367567914914,-8.39006781004132,-7.80407100094,-7.16502682994695,-6.66450349292,
-6.65635355468),.UNSPECIFIED.);
#1527=B_SPLINE_CURVE_WITH_KNOTS('',5,(#63609,#63610,#63611,#63612,#63613,
#63614,#63615,#63616,#63617,#63618,#63619,#63620,#63621,#63622,#63623,#63624,
#63625,#63626,#63627,#63628,#63629,#63630,#63631,#63632),.UNSPECIFIED.,
 .F.,.F.,(6,3,3,3,3,3,3,6),(0.,0.299762031377268,0.399460137024488,0.599691962356381,
0.726180908574686,0.807749761233441,0.889364957609916,1.),.UNSPECIFIED.);
#1528=B_SPLINE_CURVE_WITH_KNOTS('',3,(#63742,#63743,#63744,#63745,#63746,
#63747,#63748,#63749,#63750,#63751,#63752,#63753,#63754,#63755,#63756,#63757,
#63758,#63759,#63760,#63761,#63762,#63763,#63764,#63765,#63766,#63767,#63768,
#63769,#63770,#63771,#63772,#63773,#63774,#63775,#63776,#63777,#63778,#63779,
#63780,#63781,#63782,#63783,#63784,#63785,#63786,#63787,#63788,#63789,#63790,
#63791,#63792,#63793,#63794,#63795,#63796,#63797,#63798,#63799,#63800,#63801,
#63802,#63803,#63804,#63805,#63806,#63807,#63808,#63809,#63810,#63811,#63812,
#63813,#63814,#63815,#63816,#63817,#63818,#63819,#63820,#63821,#63822,#63823,
#63824,#63825,#63826,#63827,#63828,#63829,#63830,#63831,#63832,#63833,#63834,
#63835,#63836,#63837,#63838,#63839,#63840,#63841,#63842,#63843,#63844,#63845,
#63846,#63847,#63848,#63849,#63850,#63851,#63852,#63853,#63854,#63855,#63856,
#63857,#63858,#63859,#63860,#63861,#63862),.UNSPECIFIED.,.F.,.F.,(4,3,3,
3,3,3,3,3,3,3,3,3,3,3,3,3,3,3,3,3,3,3,3,3,3,3,3,3,3,3,3,3,3,3,3,3,3,3,3,
3,4),(0.,0.0316491751799897,0.0644683257425834,0.0985610461306416,0.134311793025957,
0.170399730229745,0.205743665747598,0.218439432092452,0.251442448401237,
0.291135045136278,0.324645711313536,0.355072767560426,0.358156377490794,
0.379293093761737,0.401196822338476,0.423985190632843,0.448171791950287,
0.473330505996812,0.498489220043337,0.520893370580924,0.544960444527389,
0.572101005410302,0.607462237305133,0.635947079645968,0.660729829937284,
0.682872356055211,0.704075903055738,0.724132541297263,0.744116466956529,
0.763570020027455,0.783812927173851,0.805062568839786,0.827656963226342,
0.853256235792581,0.880748557974103,0.907061466221659,0.930296099666244,
0.951950159507354,0.972658108974692,0.992320363498428,1.),.UNSPECIFIED.);
#1529=B_SPLINE_CURVE_WITH_KNOTS('',3,(#63969,#63970,#63971,#63972,#63973,
#63974,#63975,#63976,#63977,#63978,#63979,#63980,#63981,#63982,#63983,#63984,
#63985,#63986,#63987,#63988,#63989,#63990,#63991,#63992,#63993,#63994,#63995,
#63996,#63997,#63998,#63999,#64000,#64001,#64002,#64003,#64004,#64005,#64006,
#64007,#64008,#64009,#64010,#64011,#64012,#64013,#64014,#64015,#64016,#64017,
#64018,#64019,#64020,#64021,#64022,#64023),.UNSPECIFIED.,.F.,.F.,(4,3,3,
3,3,3,3,3,3,3,3,3,3,3,3,3,3,3,4),(0.,0.0611230585579808,0.124208925935708,
0.189652312423783,0.257713177850023,0.329796007159683,0.403624985796396,
0.477235323463936,0.488984468463847,0.510783466323955,0.599511866779462,
0.649572883432029,0.68078334097055,0.70173765692144,0.766971446251283,0.826706349016451,
0.884578246708151,0.942289123354076,1.),.UNSPECIFIED.);
#1530=B_SPLINE_CURVE_WITH_KNOTS('',5,(#64079,#64080,#64081,#64082,#64083,
#64084,#64085,#64086,#64087),.UNSPECIFIED.,.F.,.F.,(6,3,6),(0.,0.489018048130324,
1.),.UNSPECIFIED.);
#1531=B_SPLINE_CURVE_WITH_KNOTS('',3,(#64206,#64207,#64208,#64209,#64210,
#64211,#64212,#64213,#64214,#64215,#64216,#64217,#64218,#64219,#64220,#64221,
#64222,#64223,#64224,#64225,#64226,#64227,#64228,#64229,#64230,#64231,#64232,
#64233,#64234,#64235,#64236,#64237,#64238,#64239,#64240,#64241,#64242,#64243,
#64244,#64245,#64246,#64247,#64248,#64249,#64250,#64251,#64252,#64253,#64254,
#64255,#64256,#64257,#64258,#64259,#64260,#64261,#64262,#64263,#64264,#64265,
#64266,#64267,#64268,#64269,#64270,#64271,#64272,#64273,#64274,#64275,#64276,
#64277,#64278,#64279,#64280,#64281,#64282,#64283,#64284,#64285,#64286,#64287,
#64288,#64289,#64290,#64291,#64292,#64293,#64294,#64295,#64296,#64297,#64298,
#64299,#64300,#64301,#64302,#64303,#64304,#64305,#64306,#64307,#64308,#64309,
#64310,#64311,#64312,#64313,#64314),.UNSPECIFIED.,.F.,.F.,(4,3,3,3,3,3,
3,3,3,3,3,3,3,3,3,3,3,3,3,3,3,3,3,3,3,3,3,3,3,3,3,3,3,3,3,3,4),(0.,0.0346594543148337,
0.0696322066276516,0.0841787945508995,0.0941200626265949,0.101073116311595,
0.137518372591484,0.17245768807328,0.187690795924043,0.194591671799185,
0.230121129603681,0.263342933978537,0.27727563451867,0.295578236300883,
0.326545626280591,0.358345791467322,0.38118335794188,0.396975714575019,
0.42810993272217,0.458556467545967,0.487764180987173,0.511542683647487,
0.542606600917642,0.575567103336426,0.595309845990461,0.607159733636498,
0.642553986747648,0.676581605738495,0.6997079850505,0.717658166536222,0.748736746081099,
0.790711506309299,0.833723477279877,0.877063043691384,0.919856548091253,
0.960986423575859,1.),.UNSPECIFIED.);
#1532=B_SPLINE_CURVE_WITH_KNOTS('',5,(#64406,#64407,#64408,#64409,#64410,
#64411,#64412,#64413,#64414,#64415,#64416,#64417,#64418,#64419,#64420),
 .UNSPECIFIED.,.F.,.F.,(6,3,3,3,6),(0.,0.270680449730146,0.52898484435231,
0.803435714429636,1.),.UNSPECIFIED.);
#1533=B_SPLINE_CURVE_WITH_KNOTS('',3,(#64617,#64618,#64619,#64620,#64621,
#64622,#64623,#64624,#64625,#64626,#64627,#64628,#64629,#64630,#64631,#64632,
#64633,#64634,#64635,#64636,#64637,#64638,#64639,#64640,#64641,#64642,#64643,
#64644,#64645,#64646,#64647,#64648,#64649,#64650,#64651,#64652,#64653,#64654,
#64655,#64656,#64657,#64658,#64659,#64660,#64661,#64662,#64663,#64664,#64665,
#64666,#64667,#64668,#64669,#64670,#64671,#64672,#64673,#64674,#64675,#64676,
#64677,#64678,#64679,#64680,#64681,#64682,#64683,#64684,#64685,#64686,#64687,
#64688,#64689,#64690,#64691,#64692,#64693,#64694,#64695,#64696,#64697,#64698,
#64699,#64700,#64701,#64702,#64703,#64704,#64705,#64706,#64707,#64708,#64709,
#64710,#64711,#64712,#64713,#64714,#64715,#64716,#64717,#64718,#64719,#64720,
#64721,#64722,#64723,#64724,#64725,#64726,#64727,#64728,#64729,#64730,#64731,
#64732,#64733,#64734,#64735,#64736,#64737,#64738,#64739,#64740,#64741,#64742,
#64743,#64744,#64745,#64746,#64747,#64748,#64749,#64750,#64751,#64752),
 .UNSPECIFIED.,.F.,.F.,(4,3,3,3,3,3,3,3,3,3,3,3,3,3,3,3,3,3,3,3,3,3,3,3,
3,3,3,3,3,3,3,3,3,3,3,3,3,3,3,3,3,3,3,3,3,4),(0.,0.0178818661276581,0.0420046277498154,
0.0619147571895479,0.0784556688955424,0.0921046276778006,0.0982358839915246,
0.101631663647595,0.113481879413641,0.122768694086075,0.130945093051513,
0.13492366361535,0.147692763578984,0.162110991450564,0.17292466235425,0.182570798254554,
0.191640000877476,0.198502837971391,0.203003685351385,0.205365675065305,
0.220227760265693,0.237717341084149,0.257888024044024,0.27554448846269,
0.305320512941014,0.336139545307548,0.367581148155728,0.399998147169167,
0.416261364863618,0.451793169604947,0.489270790032098,0.531608562069829,
0.556652585026387,0.593570264533481,0.62366547684941,0.672288902338737,
0.71878877048483,0.762442054669932,0.803766603189827,0.843326669035891,
0.882495001776919,0.902430471697919,0.911523499995539,0.948130494390717,
0.983903842618441,1.),.UNSPECIFIED.);
#1534=B_SPLINE_CURVE_WITH_KNOTS('',5,(#64862,#64863,#64864,#64865,#64866,
#64867,#64868,#64869,#64870,#64871,#64872,#64873,#64874,#64875,#64876,#64877,
#64878,#64879),.UNSPECIFIED.,.F.,.F.,(6,3,3,3,3,6),(2.30144058436,3.21523268549,
4.17948834992,7.86941426972,10.6293166988,11.5241632533),.UNSPECIFIED.);
#1535=B_SPLINE_CURVE_WITH_KNOTS('',5,(#65101,#65102,#65103,#65104,#65105,
#65106),.UNSPECIFIED.,.F.,.F.,(6,6),(0.,1.),.UNSPECIFIED.);
#1536=B_SPLINE_CURVE_WITH_KNOTS('',5,(#65162,#65163,#65164,#65165,#65166,
#65167,#65168,#65169,#65170),.UNSPECIFIED.,.F.,.F.,(6,3,6),(0.,0.492002634808513,
1.),.UNSPECIFIED.);
#1537=B_SPLINE_CURVE_WITH_KNOTS('',3,(#65187,#65188,#65189,#65190,#65191,
#65192,#65193,#65194,#65195,#65196,#65197,#65198,#65199,#65200,#65201,#65202,
#65203,#65204,#65205,#65206,#65207,#65208,#65209,#65210,#65211,#65212,#65213,
#65214,#65215,#65216,#65217),.UNSPECIFIED.,.F.,.F.,(4,3,3,3,3,3,3,3,3,3,
4),(1.01419307112823E-10,0.114803214366508,0.229652502492259,0.344466449061211,
0.459272421602756,0.5,0.614960144518346,0.72996764431242,0.844937159320942,
0.9598873123093,0.999953286395137),.UNSPECIFIED.);
#1538=B_SPLINE_CURVE_WITH_KNOTS('',3,(#65222,#65223,#65224,#65225,#65226,
#65227,#65228,#65229,#65230,#65231,#65232,#65233,#65234,#65235,#65236,#65237,
#65238,#65239,#65240,#65241,#65242,#65243,#65244,#65245,#65246,#65247,#65248,
#65249,#65250,#65251,#65252),.UNSPECIFIED.,.F.,.F.,(4,3,3,3,3,3,3,3,3,3,
4),(5.04394994972232E-5,0.114997722791671,0.230017633717882,0.345013835241517,
0.460010499449355,0.5,0.614795527323077,0.729648824467911,0.844473441242412,
0.959299484217645,0.999999999986445),.UNSPECIFIED.);
#1539=B_SPLINE_CURVE_WITH_KNOTS('',3,(#65309,#65310,#65311,#65312,#65313,
#65314,#65315,#65316,#65317,#65318,#65319,#65320,#65321,#65322,#65323,#65324,
#65325,#65326,#65327,#65328,#65329,#65330,#65331,#65332,#65333,#65334,#65335,
#65336,#65337,#65338,#65339,#65340,#65341,#65342,#65343,#65344,#65345,#65346,
#65347,#65348,#65349,#65350,#65351,#65352,#65353,#65354,#65355,#65356,#65357,
#65358,#65359,#65360),.UNSPECIFIED.,.F.,.F.,(4,3,3,3,3,3,3,3,3,3,3,3,3,
3,3,3,3,4),(0.,0.0437126558078608,0.0915681494956934,0.142416637980807,
0.199087137007962,0.271354736821453,0.329530402979306,0.37856785682181,
0.426556605310522,0.490747528430981,0.556806799843687,0.624244332149857,
0.693278978525398,0.764166499868672,0.838303763782746,0.914636896986591,
0.994157837628613,1.),.UNSPECIFIED.);
#1540=B_SPLINE_CURVE_WITH_KNOTS('',5,(#65415,#65416,#65417,#65418,#65419,
#65420),.UNSPECIFIED.,.F.,.F.,(6,6),(1.41662542015,3.44037602036),
 .UNSPECIFIED.);
#1541=B_SPLINE_CURVE_WITH_KNOTS('',5,(#65488,#65489,#65490,#65491,#65492,
#65493),.UNSPECIFIED.,.F.,.F.,(6,6),(0.,0.999998872761371),
 .UNSPECIFIED.);
#1542=B_SPLINE_CURVE_WITH_KNOTS('',5,(#65496,#65497,#65498,#65499,#65500,
#65501,#65502,#65503,#65504,#65505,#65506,#65507),.UNSPECIFIED.,.F.,.F.,
(6,3,3,6),(0.,0.200980383521308,0.498560958763885,1.),.UNSPECIFIED.);
#1543=B_SPLINE_CURVE_WITH_KNOTS('',5,(#65563,#65564,#65565,#65566,#65567,
#65568),.UNSPECIFIED.,.F.,.F.,(6,6),(1.12325834678787E-6,1.),
 .UNSPECIFIED.);
#1544=B_SPLINE_CURVE_WITH_KNOTS('',5,(#65570,#65571,#65572,#65573,#65574,
#65575,#65576,#65577,#65578,#65579,#65580,#65581),.UNSPECIFIED.,.F.,.F.,
(6,3,3,6),(1.81130449228,3.02278054545,4.81654635721,7.83913682071),
 .UNSPECIFIED.);
#1545=B_SPLINE_CURVE_WITH_KNOTS('',5,(#65675,#65676,#65677,#65678,#65679,
#65680),.UNSPECIFIED.,.F.,.F.,(6,6),(0.,1.),.UNSPECIFIED.);
#1546=B_SPLINE_CURVE_WITH_KNOTS('',5,(#65736,#65737,#65738,#65739,#65740,
#65741),.UNSPECIFIED.,.F.,.F.,(6,6),(-4.0299576811,4.0299576811),
 .UNSPECIFIED.);
#1547=B_SPLINE_CURVE_WITH_KNOTS('',5,(#65742,#65743,#65744,#65745,#65746,
#65747),.UNSPECIFIED.,.F.,.F.,(6,6),(2.67640720078839E-8,1.),
 .UNSPECIFIED.);
#1548=B_SPLINE_CURVE_WITH_KNOTS('',3,(#65817,#65818,#65819,#65820,#65821,
#65822,#65823,#65824,#65825,#65826,#65827,#65828,#65829,#65830,#65831,#65832,
#65833,#65834,#65835,#65836,#65837,#65838,#65839,#65840,#65841,#65842,#65843,
#65844,#65845,#65846,#65847,#65848,#65849,#65850,#65851,#65852,#65853,#65854,
#65855,#65856,#65857,#65858,#65859,#65860,#65861,#65862,#65863,#65864,#65865,
#65866,#65867,#65868,#65869,#65870,#65871),.UNSPECIFIED.,.F.,.F.,(4,3,3,
3,3,3,3,3,3,3,3,3,3,3,3,3,3,3,4),(15.6461121486,16.0896325713055,16.5393779921266,
16.9924984702736,17.4485466874474,17.9069575593301,18.3676660600592,18.8288389264601,
19.2894880382849,19.6759856009261,20.1371224824956,20.598572133874,21.0593729051655,
21.5189112036208,21.9766242126307,22.4305838505212,22.8820570133801,23.3290841703052,
23.7060275108),.UNSPECIFIED.);
#1549=B_SPLINE_CURVE_WITH_KNOTS('',3,(#65927,#65928,#65929,#65930,#65931,
#65932,#65933,#65934,#65935,#65936,#65937,#65938,#65939,#65940,#65941,#65942,
#65943,#65944,#65945,#65946,#65947,#65948,#65949,#65950,#65951,#65952,#65953,
#65954,#65955,#65956,#65957,#65958,#65959,#65960,#65961,#65962,#65963,#65964,
#65965,#65966,#65967,#65968,#65969,#65970,#65971,#65972,#65973,#65974,#65975,
#65976,#65977,#65978,#65979,#65980,#65981),.UNSPECIFIED.,.F.,.F.,(4,3,3,
3,3,3,3,3,3,3,3,3,3,3,3,3,3,3,4),(-4.0299576811,-3.58432646698948,-3.13333878308903,
-2.67943996443098,-2.22299149481985,-1.76443619200231,-1.30366467078965,
-0.842282930845045,-0.380902091971085,8.4271212237035E-5,0.460259241512958,
0.921454150718638,1.38219890167591,1.84169198412367,2.29919664572966,2.75241920254977,
3.20276098063367,3.6479231507545,4.0299576811),.UNSPECIFIED.);
#1550=B_SPLINE_CURVE_WITH_KNOTS('',5,(#66082,#66083,#66084,#66085,#66086,
#66087,#66088,#66089,#66090,#66091,#66092,#66093),.UNSPECIFIED.,.F.,.F.,
(6,3,3,6),(0.,0.501439041305556,0.799019616584482,1.),.UNSPECIFIED.);
#1551=B_SPLINE_CURVE_WITH_KNOTS('',3,(#66149,#66150,#66151,#66152,#66153,
#66154,#66155,#66156,#66157,#66158,#66159,#66160,#66161,#66162,#66163,#66164,
#66165,#66166,#66167,#66168,#66169,#66170,#66171,#66172,#66173,#66174,#66175,
#66176,#66177,#66178,#66179,#66180,#66181,#66182,#66183,#66184,#66185,#66186,
#66187,#66188,#66189,#66190,#66191,#66192,#66193,#66194,#66195,#66196,#66197,
#66198,#66199,#66200,#66201,#66202,#66203,#66204,#66205,#66206,#66207,#66208,
#66209,#66210,#66211,#66212,#66213,#66214,#66215,#66216,#66217,#66218),
 .UNSPECIFIED.,.F.,.F.,(4,3,3,3,3,3,3,3,3,3,3,3,3,3,3,3,3,3,3,3,3,3,3,4),
(0.,0.0416934585115111,0.0842984248119822,0.127942034658533,0.173513963804105,
0.220527053595778,0.269266295706531,0.320117104895673,0.374981888964963,
0.434659850856473,0.486787066144604,0.531102769430081,0.578465001280323,
0.631156876120282,0.679840052794278,0.725322356099277,0.768143786601305,
0.80890232311754,0.848031527918299,0.886023645938725,0.922292844683316,
0.957806742735771,0.992402997682604,1.),.UNSPECIFIED.);
#1552=B_SPLINE_CURVE_WITH_KNOTS('',5,(#66219,#66220,#66221,#66222,#66223,
#66224),.UNSPECIFIED.,.F.,.F.,(6,6),(0.,1.),.UNSPECIFIED.);
#1553=B_SPLINE_CURVE_WITH_KNOTS('',3,(#66342,#66343,#66344,#66345,#66346,
#66347,#66348,#66349,#66350,#66351,#66352,#66353,#66354,#66355,#66356,#66357,
#66358,#66359,#66360,#66361,#66362,#66363,#66364,#66365,#66366,#66367,#66368,
#66369,#66370,#66371,#66372,#66373,#66374,#66375,#66376,#66377,#66378,#66379,
#66380,#66381,#66382,#66383,#66384,#66385,#66386,#66387,#66388,#66389,#66390,
#66391,#66392,#66393,#66394,#66395,#66396,#66397,#66398,#66399,#66400,#66401,
#66402,#66403,#66404,#66405,#66406,#66407,#66408,#66409,#66410,#66411,#66412,
#66413,#66414,#66415,#66416,#66417,#66418,#66419,#66420,#66421,#66422,#66423,
#66424,#66425,#66426),.UNSPECIFIED.,.F.,.F.,(4,3,3,3,3,3,3,3,3,3,3,3,3,
3,3,3,3,3,3,3,3,3,3,3,3,3,3,3,4),(0.,0.0365197170986561,0.0750561518641488,
0.116481352134669,0.157480958781737,0.195741855213761,0.21819216147024,
0.267279631016782,0.28047977872294,0.314494034692517,0.349363219215245,
0.384561538339423,0.416779364169955,0.458265327941776,0.490156495711959,
0.518807853109117,0.555862643296138,0.593061189935473,0.630400857109214,
0.66794626872993,0.705592102349747,0.743377716091016,0.770781707666146,
0.799011186296452,0.822310369292715,0.866732776969536,0.9103813251214,0.9551906625607,
1.),.UNSPECIFIED.);
#1554=B_SPLINE_CURVE_WITH_KNOTS('',5,(#66518,#66519,#66520,#66521,#66522,
#66523,#66524,#66525,#66526,#66527,#66528,#66529,#66530,#66531,#66532,#66533,
#66534,#66535),.UNSPECIFIED.,.F.,.F.,(6,3,3,3,3,6),(2.56814442563,4.26587753681,
5.98143772792,6.84529958826,9.44079904688,11.1645337758),.UNSPECIFIED.);
#1555=B_SPLINE_CURVE_WITH_KNOTS('',5,(#66791,#66792,#66793,#66794,#66795,
#66796,#66797,#66798,#66799,#66800,#66801,#66802,#66803,#66804,#66805,#66806,
#66807,#66808),.UNSPECIFIED.,.F.,.F.,(6,3,3,3,3,6),(2.58143959,4.30538111878,
6.90119302094,7.76515862896,9.48090785315,11.1787837181),.UNSPECIFIED.);
#1556=B_SPLINE_CURVE_WITH_KNOTS('',5,(#66899,#66900,#66901,#66902,#66903,
#66904,#66905,#66906,#66907,#66908,#66909,#66910,#66911,#66912,#66913,#66914,
#66915,#66916),.UNSPECIFIED.,.F.,.F.,(6,3,3,3,3,6),(2.58143959,4.30538111878,
6.90119302094,7.76515862896,9.48090785315,11.1787837181),.UNSPECIFIED.);
#1557=B_SPLINE_CURVE_WITH_KNOTS('',5,(#67047,#67048,#67049,#67050,#67051,
#67052,#67053,#67054,#67055,#67056,#67057,#67058,#67059,#67060,#67061,#67062,
#67063,#67064,#67065,#67066,#67067,#67068,#67069,#67070),.UNSPECIFIED.,
 .F.,.F.,(6,3,3,3,3,3,3,6),(0.,0.298380745521735,0.400355122330922,0.605495111960514,
0.706465344087353,0.806019409718089,0.903240868100526,1.),.UNSPECIFIED.);
#1558=B_SPLINE_CURVE_WITH_KNOTS('',5,(#67146,#67147,#67148,#67149,#67150,
#67151,#67152,#67153,#67154,#67155,#67156,#67157),.UNSPECIFIED.,.F.,.F.,
(6,3,3,6),(0.,0.279839693768996,0.538064414016406,1.),.UNSPECIFIED.);
#1559=B_SPLINE_CURVE_WITH_KNOTS('',3,(#67265,#67266,#67267,#67268,#67269,
#67270,#67271,#67272,#67273,#67274,#67275,#67276,#67277,#67278,#67279,#67280,
#67281,#67282,#67283,#67284,#67285,#67286,#67287,#67288,#67289,#67290,#67291,
#67292,#67293,#67294,#67295,#67296,#67297,#67298,#67299,#67300,#67301,#67302,
#67303,#67304,#67305,#67306,#67307,#67308,#67309,#67310,#67311,#67312,#67313,
#67314,#67315,#67316),.UNSPECIFIED.,.F.,.F.,(4,3,3,3,3,3,3,3,3,3,3,3,3,
3,3,3,3,4),(0.,0.0556187312399707,0.112993438321228,0.172143724257659,0.23389539128623,
0.297764219459196,0.321436234888974,0.41536792214111,0.489370703978092,
0.518718286518054,0.586784525784047,0.656446595575187,0.726367781106817,
0.794775835830112,0.860858656629832,0.925135456699957,0.986994389830349,
1.),.UNSPECIFIED.);
#1560=B_SPLINE_CURVE_WITH_KNOTS('',5,(#67372,#67373,#67374,#67375,#67376,
#67377,#67378,#67379,#67380),.UNSPECIFIED.,.F.,.F.,(6,3,6),(0.,0.498324297489375,
1.),.UNSPECIFIED.);
#1561=B_SPLINE_CURVE_WITH_KNOTS('',3,(#67517,#67518,#67519,#67520,#67521,
#67522,#67523,#67524,#67525,#67526,#67527,#67528,#67529,#67530,#67531,#67532,
#67533,#67534,#67535,#67536,#67537,#67538,#67539,#67540,#67541,#67542,#67543,
#67544,#67545,#67546,#67547,#67548,#67549,#67550,#67551,#67552,#67553,#67554,
#67555,#67556,#67557,#67558,#67559,#67560,#67561,#67562,#67563,#67564,#67565,
#67566,#67567,#67568,#67569,#67570,#67571,#67572,#67573,#67574,#67575,#67576,
#67577,#67578,#67579,#67580,#67581,#67582,#67583,#67584,#67585,#67586,#67587,
#67588,#67589,#67590,#67591,#67592,#67593,#67594,#67595,#67596,#67597,#67598,
#67599,#67600,#67601,#67602,#67603,#67604,#67605,#67606,#67607,#67608,#67609,
#67610,#67611,#67612,#67613,#67614,#67615,#67616,#67617,#67618,#67619,#67620,
#67621,#67622,#67623,#67624,#67625,#67626,#67627,#67628,#67629,#67630,#67631,
#67632,#67633,#67634,#67635,#67636,#67637,#67638,#67639,#67640,#67641,#67642,
#67643,#67644,#67645,#67646),.UNSPECIFIED.,.F.,.F.,(4,3,3,3,3,3,3,3,3,3,
3,3,3,3,3,3,3,3,3,3,3,3,3,3,3,3,3,3,3,3,3,3,3,3,3,3,3,3,3,3,3,3,3,4),(0.,
0.0198013619717458,0.0404159238918976,0.0620723153674499,0.086247822024199,
0.10843867563033,0.125899721004124,0.152218301219973,0.176179069456496,
0.196035357920758,0.216490434219102,0.235983401420272,0.255476368621443,
0.271170775069074,0.282640095018162,0.303570033406706,0.32561749981579,
0.350282440909494,0.377972561891687,0.399923595232346,0.415662554971816,
0.443004349547964,0.467591673748802,0.489986113834325,0.499978765489982,
0.524945472319113,0.549687996167472,0.573101538289844,0.59297413237794,
0.616741323308855,0.637748727055981,0.64050851423977,0.671117738474467,
0.693353256839199,0.714783014437229,0.750668884649306,0.780812121073995,
0.816630656902144,0.853091747051759,0.889818810288819,0.92403816438968,
0.957052970761367,0.988505420883898,1.),.UNSPECIFIED.);
#1562=B_SPLINE_CURVE_WITH_KNOTS('',5,(#67756,#67757,#67758,#67759,#67760,
#67761,#67762,#67763,#67764,#67765,#67766,#67767,#67768,#67769,#67770,#67771,
#67772,#67773),.UNSPECIFIED.,.F.,.F.,(6,3,3,3,3,6),(0.,0.273250853963034,
0.407985073911058,0.581975918956344,0.822728550713782,1.),.UNSPECIFIED.);
#1563=B_SPLINE_CURVE_WITH_KNOTS('',3,(#67977,#67978,#67979,#67980,#67981,
#67982,#67983,#67984,#67985,#67986,#67987,#67988,#67989,#67990,#67991,#67992,
#67993,#67994,#67995,#67996,#67997,#67998,#67999,#68000,#68001,#68002,#68003,
#68004,#68005,#68006,#68007),.UNSPECIFIED.,.F.,.F.,(4,3,3,3,3,3,3,3,3,3,
4),(0.,0.110287887209419,0.223345183110051,0.337717962698899,0.45335852785974,
0.5,0.615745954604195,0.730067416796077,0.84303840753261,0.953657228919592,
1.),.UNSPECIFIED.);
#1564=B_SPLINE_CURVE_WITH_KNOTS('',5,(#68008,#68009,#68010,#68011,#68012,
#68013),.UNSPECIFIED.,.F.,.F.,(6,6),(0.,1.),.UNSPECIFIED.);
#1565=B_SPLINE_CURVE_WITH_KNOTS('',5,(#68069,#68070,#68071,#68072,#68073,
#68074),.UNSPECIFIED.,.F.,.F.,(6,6),(1.41662542015,3.44037602036),
 .UNSPECIFIED.);
#1566=B_SPLINE_CURVE_WITH_KNOTS('',3,(#68075,#68076,#68077,#68078,#68079,
#68080,#68081,#68082,#68083,#68084,#68085,#68086,#68087,#68088,#68089,#68090,
#68091,#68092,#68093,#68094,#68095,#68096,#68097,#68098,#68099,#68100,#68101,
#68102,#68103,#68104,#68105),.UNSPECIFIED.,.F.,.F.,(4,3,3,3,3,3,3,3,3,3,
4),(0.,0.110294928224807,0.223359835487429,0.337740411810181,0.453388630710344,
0.5,0.615739698165253,0.730054755953022,0.843019355200479,0.953631919301136,
1.),.UNSPECIFIED.);
#1567=B_SPLINE_CURVE_WITH_KNOTS('',5,(#68185,#68186,#68187,#68188,#68189,
#68190),.UNSPECIFIED.,.F.,.F.,(6,6),(0.,1.),.UNSPECIFIED.);
#1568=B_SPLINE_CURVE_WITH_KNOTS('',5,(#68246,#68247,#68248,#68249,#68250,
#68251,#68252,#68253,#68254),.UNSPECIFIED.,.F.,.F.,(6,3,6),(0.,0.49200263441696,
1.),.UNSPECIFIED.);
#1569=B_SPLINE_CURVE_WITH_KNOTS('',5,(#68522,#68523,#68524,#68525,#68526,
#68527,#68528,#68529,#68530,#68531,#68532,#68533,#68534,#68535,#68536,#68537,
#68538,#68539),.UNSPECIFIED.,.F.,.F.,(6,3,3,3,3,6),(0.,0.0970262888056245,
0.396276577955941,0.796367315526125,0.900919486282946,0.99999999472897),
 .UNSPECIFIED.);
#1570=B_SPLINE_CURVE_WITH_KNOTS('',5,(#68666,#68667,#68668,#68669,#68670,
#68671,#68672,#68673,#68674,#68675,#68676,#68677,#68678,#68679,#68680,#68681,
#68682,#68683,#68684,#68685,#68686),.UNSPECIFIED.,.F.,.F.,(6,3,3,3,3,3,
6),(0.,0.449905946496647,0.59940190637457,0.692533484718061,0.785665063061551,
0.897922768805432,1.),.UNSPECIFIED.);
#1571=B_SPLINE_CURVE_WITH_KNOTS('',5,(#68798,#68799,#68800,#68801,#68802,
#68803,#68804,#68805,#68806,#68807,#68808,#68809),.UNSPECIFIED.,.F.,.F.,
(6,3,3,6),(0.,0.492684025877734,0.739237878130715,1.),.UNSPECIFIED.);
#1572=B_SPLINE_CURVE_WITH_KNOTS('',5,(#68887,#68888,#68889,#68890,#68891,
#68892,#68893,#68894,#68895,#68896,#68897,#68898,#68899,#68900,#68901,#68902,
#68903,#68904,#68905,#68906,#68907),.UNSPECIFIED.,.F.,.F.,(6,3,3,3,3,3,
6),(0.,0.201339674271977,0.303001917323942,0.506399963286459,0.70776546861359,
0.806334715522354,1.),.UNSPECIFIED.);
#1573=B_SPLINE_CURVE_WITH_KNOTS('',5,(#69008,#69009,#69010,#69011,#69012,
#69013),.UNSPECIFIED.,.F.,.F.,(6,6),(-1.27990980993,-0.52702168644),
 .UNSPECIFIED.);
#1574=B_SPLINE_CURVE_WITH_KNOTS('',3,(#69070,#69071,#69072,#69073,#69074,
#69075,#69076,#69077,#69078,#69079,#69080,#69081,#69082,#69083,#69084,#69085,
#69086,#69087,#69088,#69089,#69090,#69091,#69092,#69093,#69094,#69095,#69096,
#69097,#69098,#69099,#69100,#69101,#69102,#69103,#69104,#69105,#69106,#69107,
#69108,#69109,#69110,#69111,#69112),.UNSPECIFIED.,.F.,.F.,(4,3,3,3,3,3,
3,3,3,3,3,3,3,3,4),(0.,0.0776083637283321,0.155118249326187,0.232531965013796,
0.30981031864142,0.387003342323335,0.46407865662313,0.495424428724466,0.571227612704095,
0.648031014951877,0.725644046554455,0.803923133483166,0.882212778464548,
0.960052978009603,1.),.UNSPECIFIED.);
#1575=B_SPLINE_CURVE_WITH_KNOTS('',5,(#69182,#69183,#69184,#69185,#69186,
#69187,#69188,#69189,#69190),.UNSPECIFIED.,.F.,.F.,(6,3,6),(0.,0.565644588338075,
1.),.UNSPECIFIED.);
#1576=B_SPLINE_CURVE_WITH_KNOTS('',5,(#69247,#69248,#69249,#69250,#69251,
#69252),.UNSPECIFIED.,.F.,.F.,(6,6),(-19.8869526656,-9.07387951837),
 .UNSPECIFIED.);
#1577=B_SPLINE_CURVE_WITH_KNOTS('',5,(#69322,#69323,#69324,#69325,#69326,
#69327,#69328,#69329,#69330),.UNSPECIFIED.,.F.,.F.,(6,3,6),(0.,0.565644588338948,
1.),.UNSPECIFIED.);
#1578=B_SPLINE_CURVE_WITH_KNOTS('',5,(#69387,#69388,#69389,#69390,#69391,
#69392),.UNSPECIFIED.,.F.,.F.,(6,6),(-30.7000258128,-19.8869526656),
 .UNSPECIFIED.);
#1579=B_SPLINE_CURVE_WITH_KNOTS('',5,(#69462,#69463,#69464,#69465,#69466,
#69467),.UNSPECIFIED.,.F.,.F.,(6,6),(-1.27990980993,-0.52702168644),
 .UNSPECIFIED.);
#1580=B_SPLINE_CURVE_WITH_KNOTS('',3,(#69524,#69525,#69526,#69527,#69528,
#69529,#69530,#69531,#69532,#69533,#69534,#69535,#69536,#69537,#69538,#69539,
#69540,#69541,#69542,#69543,#69544,#69545,#69546,#69547,#69548,#69549,#69550,
#69551,#69552,#69553,#69554,#69555,#69556,#69557,#69558,#69559,#69560,#69561,
#69562,#69563,#69564,#69565,#69566),.UNSPECIFIED.,.F.,.F.,(4,3,3,3,3,3,
3,3,3,3,3,3,3,3,4),(0.,0.0776083635899578,0.155118249004403,0.232531964542428,
0.309810318214625,0.38700334212762,0.464078657022176,0.495424428696483,
0.571227612929565,0.648031015392319,0.725644047151879,0.803923134122699,
0.882212779078427,0.960052978513656,1.),.UNSPECIFIED.);
#1581=B_SPLINE_CURVE_WITH_KNOTS('',5,(#69654,#69655,#69656,#69657,#69658,
#69659,#69660,#69661,#69662,#69663,#69664,#69665,#69666,#69667,#69668,#69669,
#69670,#69671,#69672,#69673,#69674),.UNSPECIFIED.,.F.,.F.,(6,3,3,3,3,3,
6),(-8.58012360199,-7.30257258114,-6.6523412175,-5.32399418003,-3.98223908975,
-3.31160417062,-1.98342753277),.UNSPECIFIED.);
#1582=B_SPLINE_CURVE_WITH_KNOTS('',5,(#69749,#69750,#69751,#69752,#69753,
#69754,#69755,#69756,#69757,#69758,#69759,#69760,#69761,#69762,#69763,#69764,
#69765,#69766,#69767,#69768,#69769),.UNSPECIFIED.,.F.,.F.,(6,3,3,3,3,3,
6),(0.,0.193665284476424,0.292234531386853,0.493600036714289,0.696998082675599,
0.798660325727718,1.),.UNSPECIFIED.);
#1583=B_SPLINE_CURVE_WITH_KNOTS('',5,(#69905,#69906,#69907,#69908,#69909,
#69910,#69911,#69912,#69913,#69914,#69915,#69916,#69917,#69918,#69919),
 .UNSPECIFIED.,.F.,.F.,(6,3,3,3,6),(-5.21689863741,-4.48067762876,-3.70557211292,
-2.5282953222,-1.35736905211),.UNSPECIFIED.);
#1584=B_SPLINE_CURVE_WITH_KNOTS('',3,(#70012,#70013,#70014,#70015,#70016,
#70017,#70018,#70019,#70020,#70021,#70022,#70023,#70024,#70025,#70026,#70027,
#70028,#70029,#70030,#70031,#70032,#70033,#70034,#70035,#70036,#70037,#70038,
#70039,#70040,#70041,#70042,#70043,#70044,#70045,#70046,#70047,#70048,#70049,
#70050,#70051,#70052,#70053,#70054,#70055,#70056,#70057,#70058,#70059,#70060,
#70061,#70062,#70063,#70064,#70065,#70066,#70067,#70068,#70069,#70070,#70071,
#70072,#70073,#70074,#70075,#70076,#70077,#70078,#70079,#70080,#70081,#70082,
#70083,#70084,#70085,#70086,#70087,#70088,#70089,#70090,#70091,#70092,#70093,
#70094,#70095,#70096,#70097,#70098,#70099,#70100,#70101,#70102),
 .UNSPECIFIED.,.F.,.F.,(4,3,3,3,3,3,3,3,3,3,3,3,3,3,3,3,3,3,3,3,3,3,3,3,
3,3,3,3,3,3,4),(0.,0.0182662446037865,0.0375259675978898,0.0582758529991181,
0.0820848215164342,0.112848248846866,0.135920819344689,0.156749193614456,
0.17626986474751,0.191579331315563,0.205138530838161,0.22773672177315,0.253447922437721,
0.291000249561992,0.317357678976258,0.328552576686263,0.383012581099915,
0.412561924344558,0.486591650696816,0.492903941799935,0.546128883342705,
0.605058868866327,0.655577068132116,0.688250424539024,0.715729075586451,
0.773576659496423,0.826211419859548,0.874471298494987,0.921087205821898,
0.965827553474194,1.),.UNSPECIFIED.);
#1585=B_SPLINE_CURVE_WITH_KNOTS('',5,(#70316,#70317,#70318,#70319,#70320,
#70321,#70322,#70323,#70324,#70325,#70326,#70327,#70328,#70329,#70330,#70331,
#70332,#70333,#70334,#70335,#70336,#70337,#70338,#70339,#70340,#70341,#70342,
#70343,#70344,#70345,#70346,#70347,#70348,#70349,#70350,#70351,#70352,#70353,
#70354),.UNSPECIFIED.,.F.,.F.,(6,3,3,3,3,3,3,3,3,3,3,3,6),(-31.7310892021,
-30.7075742798,-30.0730233774,-29.43694187,-27.5338438134,-24.9287160587,
-22.3238009285,-21.0213468886,-17.0993514659,-13.7853920845,-8.49590865562,
-6.30725257391,-5.58814360433),.UNSPECIFIED.);
#1586=B_SPLINE_CURVE_WITH_KNOTS('',5,(#70537,#70538,#70539,#70540,#70541,
#70542,#70543,#70544,#70545,#70546,#70547,#70548,#70549,#70550,#70551,#70552,
#70553,#70554,#70555,#70556,#70557,#70558,#70559,#70560,#70561,#70562,#70563,
#70564,#70565,#70566,#70567,#70568,#70569,#70570,#70571,#70572,#70573,#70574,
#70575),.UNSPECIFIED.,.F.,.F.,(6,3,3,3,3,3,3,3,3,3,3,3,6),(0.,0.0391507115551396,
0.063423068318722,0.0877539726164481,0.160549826835811,0.260199185205061,
0.359840410424235,0.409660888190562,0.559682063426246,0.686445108126254,
0.888774390765743,0.97249319259413,1.),.UNSPECIFIED.);
#1587=B_SPLINE_CURVE_WITH_KNOTS('',5,(#70964,#70965,#70966,#70967,#70968,
#70969,#70970,#70971,#70972,#70973,#70974,#70975,#70976,#70977,#70978,#70979,
#70980,#70981,#70982,#70983,#70984,#70985,#70986,#70987,#70988,#70989,#70990,
#70991,#70992,#70993,#70994,#70995,#70996,#70997,#70998,#70999,#71000,#71001,
#71002),.UNSPECIFIED.,.F.,.F.,(6,3,3,3,3,3,3,3,3,3,3,3,6),(-31.8832921784,
-31.1641832088,-28.9755271271,-23.6860436982,-20.3720843168,-16.4500888941,
-15.1476348542,-12.5427197241,-9.9375919693,-8.03449391269,-7.39841240531,
-6.76386150304,-5.7403465807),.UNSPECIFIED.);
#1588=B_SPLINE_CURVE_WITH_KNOTS('',3,(#71167,#71168,#71169,#71170,#71171,
#71172,#71173,#71174,#71175,#71176,#71177,#71178,#71179,#71180,#71181,#71182,
#71183,#71184,#71185,#71186,#71187,#71188,#71189,#71190,#71191,#71192,#71193,
#71194,#71195,#71196,#71197,#71198,#71199,#71200,#71201,#71202,#71203,#71204,
#71205,#71206,#71207,#71208,#71209,#71210,#71211,#71212,#71213,#71214,#71215,
#71216,#71217,#71218,#71219,#71220,#71221,#71222,#71223,#71224,#71225,#71226,
#71227,#71228,#71229,#71230,#71231,#71232,#71233,#71234,#71235,#71236,#71237,
#71238,#71239,#71240,#71241,#71242,#71243,#71244,#71245,#71246,#71247,#71248,
#71249,#71250,#71251,#71252,#71253,#71254,#71255,#71256,#71257,#71258,#71259,
#71260,#71261,#71262,#71263,#71264,#71265,#71266,#71267,#71268,#71269,#71270,
#71271,#71272,#71273,#71274,#71275,#71276,#71277,#71278,#71279,#71280,#71281,
#71282,#71283,#71284,#71285,#71286,#71287,#71288,#71289,#71290,#71291,#71292,
#71293,#71294,#71295,#71296,#71297,#71298,#71299,#71300,#71301,#71302,#71303,
#71304,#71305,#71306,#71307,#71308,#71309,#71310,#71311,#71312,#71313,#71314,
#71315,#71316,#71317,#71318,#71319,#71320,#71321,#71322,#71323,#71324,#71325,
#71326,#71327,#71328,#71329,#71330,#71331,#71332,#71333,#71334,#71335,#71336,
#71337,#71338,#71339,#71340,#71341,#71342,#71343,#71344,#71345,#71346,#71347,
#71348,#71349,#71350,#71351,#71352,#71353,#71354,#71355,#71356,#71357,#71358,
#71359,#71360,#71361,#71362,#71363,#71364,#71365,#71366,#71367,#71368,#71369,
#71370,#71371),.UNSPECIFIED.,.F.,.F.,(4,3,3,3,3,3,3,3,3,3,3,3,3,3,3,3,3,
3,3,3,3,3,3,3,3,3,3,3,3,3,3,3,3,3,3,3,3,3,3,3,3,3,3,3,3,3,3,3,3,3,3,3,3,
3,3,3,3,3,3,3,3,3,3,3,3,3,3,3,4),(0.,0.0154108833739815,0.024396260675666,
0.0322672376773886,0.0509867983195788,0.070655365291477,0.091955212111218,
0.105014263643365,0.118071336189016,0.143019468820527,0.16594610599059,
0.186734949763442,0.206432882601081,0.224937065226494,0.234726017500779,
0.252391337653417,0.270528133993635,0.28952273821895,0.308536692801582,
0.324241359276896,0.345863793558721,0.368477343842195,0.392380882102757,
0.406636273014148,0.429460363972643,0.441722866558087,0.466249444060802,
0.487012897201986,0.499998942837968,0.519585389504108,0.539965369435351,
0.562135064298468,0.585423106641615,0.595055043844164,0.621056567089681,
0.639186449720391,0.670100538908602,0.693969077346171,0.715642974917153,
0.751561803628593,0.78639517991619,0.819094250974915,0.834422620522875,
0.844868688329344,0.859318289762911,0.871664748244572,0.887334416156321,
0.901524270073433,0.911323754293252,0.916718949293115,0.92722086707506,
0.931097752998277,0.935699661236655,0.939658545918256,0.946503170030517,
0.951478794929174,0.955953947599919,0.959463525531288,0.962295311108283,
0.962973103462657,0.96667709714004,0.970584348317267,0.975061015415103,
0.980444468128151,0.985362564279898,0.989550180366893,0.993386213762534,
0.996885676959665,1.),.UNSPECIFIED.);
#1589=B_SPLINE_CURVE_WITH_KNOTS('',5,(#71541,#71542,#71543,#71544,#71545,
#71546,#71547,#71548,#71549,#71550,#71551,#71552,#71553,#71554,#71555),
 .UNSPECIFIED.,.F.,.F.,(6,3,3,3,6),(-4.99954599766,-3.82861972691,-2.65134293549,
-1.87623741919,-1.14001641713),.UNSPECIFIED.);
#1590=B_SPLINE_CURVE_WITH_KNOTS('',3,(#71628,#71629,#71630,#71631,#71632,
#71633,#71634,#71635,#71636,#71637,#71638,#71639,#71640,#71641,#71642,#71643,
#71644,#71645,#71646,#71647,#71648,#71649,#71650,#71651,#71652,#71653,#71654,
#71655,#71656,#71657,#71658,#71659,#71660,#71661,#71662,#71663,#71664,#71665,
#71666,#71667,#71668,#71669,#71670,#71671,#71672,#71673,#71674,#71675,#71676,
#71677,#71678,#71679,#71680,#71681,#71682,#71683,#71684,#71685,#71686,#71687,
#71688,#71689,#71690,#71691,#71692,#71693,#71694,#71695,#71696,#71697,#71698,
#71699,#71700,#71701,#71702,#71703,#71704,#71705,#71706,#71707,#71708,#71709),
 .UNSPECIFIED.,.F.,.F.,(4,3,3,3,3,3,3,3,3,3,3,3,3,3,3,3,3,3,3,3,3,3,3,3,
3,3,3,4),(0.,0.0439316094348881,0.0891820224051535,0.136202678319011,0.187279339885987,
0.24254633142745,0.28611550350907,0.326361772648343,0.391110344479467,0.44490716763704,
0.493862617423488,0.542497006607632,0.600081606137234,0.621499512521632,
0.678028299826536,0.7265832841389,0.769693226668195,0.803454089159351,0.819848941519525,
0.838676687278942,0.859941456517357,0.884377849295373,0.914307868095059,
0.936993329670823,0.957477728773413,0.976663422649514,0.994636879500515,
1.),.UNSPECIFIED.);
#1591=B_SPLINE_CURVE_WITH_KNOTS('',3,(#71744,#71745,#71746,#71747,#71748,
#71749,#71750,#71751,#71752,#71753,#71754,#71755,#71756,#71757,#71758,#71759,
#71760,#71761,#71762,#71763,#71764,#71765,#71766,#71767,#71768,#71769,#71770,
#71771,#71772,#71773,#71774,#71775,#71776,#71777,#71778,#71779,#71780,#71781,
#71782,#71783,#71784,#71785,#71786,#71787,#71788,#71789,#71790,#71791,#71792,
#71793,#71794,#71795,#71796,#71797,#71798,#71799,#71800,#71801,#71802,#71803,
#71804,#71805,#71806,#71807,#71808,#71809,#71810,#71811,#71812,#71813,#71814,
#71815,#71816,#71817,#71818,#71819,#71820,#71821,#71822,#71823,#71824,#71825,
#71826,#71827,#71828,#71829,#71830,#71831,#71832,#71833,#71834,#71835,#71836,
#71837,#71838,#71839,#71840,#71841,#71842,#71843,#71844,#71845,#71846,#71847,
#71848,#71849,#71850,#71851,#71852,#71853,#71854,#71855,#71856,#71857,#71858,
#71859,#71860,#71861,#71862,#71863,#71864,#71865,#71866,#71867,#71868,#71869,
#71870,#71871,#71872,#71873,#71874,#71875,#71876,#71877,#71878,#71879,#71880,
#71881,#71882,#71883,#71884,#71885,#71886,#71887,#71888,#71889,#71890,#71891,
#71892,#71893,#71894,#71895,#71896,#71897,#71898,#71899,#71900,#71901,#71902,
#71903,#71904,#71905,#71906,#71907,#71908,#71909,#71910,#71911,#71912,#71913,
#71914,#71915,#71916,#71917,#71918),.UNSPECIFIED.,.F.,.F.,(4,3,3,3,3,3,
3,3,3,3,3,3,3,3,3,3,3,3,3,3,3,3,3,3,3,3,3,3,3,3,3,3,3,3,3,3,3,3,3,3,3,3,
3,3,3,3,3,3,3,3,3,3,3,3,3,3,3,3,4),(13.4402611449,13.5070964098,14.2468335688477,
14.9953689393349,15.7485030377147,16.5054819020246,17.2654067660921,18.0278474779116,
18.7905126436479,19.5517539434494,20.2095273779,20.9687643902614,21.7217135386243,
22.4703077255754,23.2116440479358,23.5689081291,24.3109067601058,25.0584792099068,
25.8110233837674,26.567773191108,27.3278022892921,28.1173729599431,28.8763863467288,
29.6393660388709,30.4006119455066,31.159144897169,31.9121345408492,32.6611814951464,
33.4038368880882,33.6443676545,34.3873867942773,35.135806909375,35.888999131998,
36.6461739203357,37.4063879012094,38.1955466209957,38.955487589057,39.7175566740638,
40.477710487504,41.2350068233562,41.9866165086,42.7342388949353,43.4754422745138,
43.7196576595,44.4613265079885,45.2089180014669,45.9618189072157,46.719235518721,
47.4801950110937,48.2678785133445,49.0291748631258,49.7910234685431,50.5510731777613,
51.3083055012999,52.0598033404119,52.8072294015329,53.5481010611059,53.7816630291,
53.84849829),.UNSPECIFIED.);
#1592=B_SPLINE_CURVE_WITH_KNOTS('',3,(#71920,#71921,#71922,#71923,#71924,
#71925,#71926,#71927,#71928,#71929,#71930,#71931,#71932,#71933,#71934,#71935,
#71936,#71937,#71938,#71939,#71940,#71941,#71942,#71943,#71944,#71945,#71946,
#71947,#71948,#71949,#71950,#71951,#71952,#71953,#71954,#71955,#71956,#71957,
#71958,#71959,#71960,#71961,#71962,#71963,#71964,#71965),.UNSPECIFIED.,
 .F.,.F.,(4,3,3,3,3,3,3,3,3,3,3,3,3,3,3,4),(0.68208121853,0.833285110291927,
0.893438704333,1.03975468193142,1.10556304245,1.23772138518436,1.36639838409707,
1.49153340548065,1.52935115459,1.66108737747387,1.74128259681,1.88383305622587,
1.95314956045,2.12228973264587,2.16523839884,2.17454139046),
 .UNSPECIFIED.);
#1593=B_SPLINE_CURVE_WITH_KNOTS('',3,(#71969,#71970,#71971,#71972,#71973,
#71974,#71975,#71976,#71977,#71978,#71979,#71980,#71981,#71982,#71983,#71984,
#71985,#71986,#71987,#71988,#71989,#71990,#71991,#71992,#71993,#71994,#71995,
#71996,#71997,#71998,#71999,#72000,#72001,#72002,#72003,#72004,#72005,#72006,
#72007,#72008,#72009,#72010,#72011,#72012,#72013,#72014,#72015,#72016,#72017,
#72018,#72019,#72020,#72021,#72022,#72023,#72024,#72025,#72026,#72027,#72028,
#72029),.UNSPECIFIED.,.F.,.F.,(4,3,3,3,3,3,3,3,3,3,3,3,3,3,3,3,3,3,3,3,
4),(8.03689290773,8.75334465576375,9.46923125712186,10.1895756567313,10.9140328563649,
11.6440191235026,12.3764813091007,13.1119708062231,13.768506892,14.5052662832091,
15.243807631294,15.9828982697244,16.7204464834581,17.4556667504414,18.1876202191916,
18.9154953869,19.6359475654664,20.3517214078531,21.0597384561033,21.5454531764,
21.5784150656),.UNSPECIFIED.);
#1594=B_SPLINE_CURVE_WITH_KNOTS('',3,(#72031,#72032,#72033,#72034,#72035,
#72036,#72037,#72038,#72039,#72040,#72041,#72042,#72043,#72044,#72045,#72046,
#72047,#72048,#72049,#72050,#72051,#72052,#72053,#72054,#72055,#72056,#72057,
#72058,#72059,#72060,#72061,#72062,#72063,#72064,#72065,#72066,#72067,#72068,
#72069,#72070,#72071,#72072,#72073,#72074,#72075,#72076,#72077,#72078,#72079,
#72080,#72081,#72082,#72083,#72084,#72085,#72086,#72087,#72088,#72089,#72090,
#72091),.UNSPECIFIED.,.F.,.F.,(4,3,3,3,3,3,3,3,3,3,3,3,3,3,3,3,3,3,3,3,
4),(8.03777014773,8.75426889125125,9.47001359609466,10.1902177205057,10.9145366724205,
11.6443893801527,12.3767202822979,13.1120832966385,13.7697600959,14.5065337688577,
15.2451024323911,15.9842354518727,16.7218509387113,17.4571540774596,18.1892052935327,
18.9171918235122,19.6377739811748,20.3536859093427,21.0618537376259,21.5465332101,
21.5792812917),.UNSPECIFIED.);
#1595=B_SPLINE_CURVE_WITH_KNOTS('',3,(#72095,#72096,#72097,#72098,#72099,
#72100,#72101,#72102,#72103,#72104,#72105,#72106,#72107,#72108,#72109,#72110,
#72111,#72112,#72113,#72114,#72115,#72116,#72117,#72118,#72119,#72120,#72121,
#72122,#72123,#72124,#72125,#72126,#72127,#72128,#72129,#72130,#72131,#72132,
#72133,#72134,#72135,#72136,#72137,#72138,#72139,#72140),.UNSPECIFIED.,
 .F.,.F.,(4,3,3,3,3,3,3,3,3,3,3,3,3,3,3,4),(0.682080632107,0.833188271917978,
0.893438117902,1.03975409805662,1.10556245601,1.23772079875137,1.36639779750311,
1.49153281928841,1.52935056816,1.66108679248608,1.74128201038,1.88383247191979,
1.95314897402,2.12228914750544,2.16523781241,2.17454080403),
 .UNSPECIFIED.);
#1596=B_SPLINE_CURVE_WITH_KNOTS('',3,(#72142,#72143,#72144,#72145,#72146,
#72147,#72148,#72149,#72150,#72151,#72152,#72153,#72154,#72155,#72156,#72157,
#72158,#72159,#72160,#72161,#72162,#72163,#72164,#72165,#72166,#72167,#72168,
#72169,#72170,#72171,#72172,#72173,#72174,#72175,#72176,#72177,#72178,#72179,
#72180,#72181,#72182,#72183,#72184,#72185,#72186,#72187,#72188,#72189,#72190,
#72191,#72192,#72193,#72194,#72195,#72196,#72197,#72198,#72199,#72200,#72201,
#72202,#72203,#72204,#72205,#72206,#72207,#72208,#72209,#72210,#72211,#72212,
#72213,#72214,#72215,#72216,#72217,#72218,#72219,#72220,#72221,#72222,#72223,
#72224,#72225,#72226,#72227,#72228,#72229,#72230,#72231,#72232,#72233,#72234,
#72235,#72236,#72237,#72238,#72239,#72240,#72241,#72242,#72243,#72244,#72245,
#72246,#72247,#72248,#72249,#72250,#72251,#72252,#72253,#72254,#72255,#72256,
#72257,#72258,#72259,#72260,#72261,#72262,#72263,#72264,#72265,#72266,#72267,
#72268,#72269,#72270,#72271,#72272,#72273,#72274,#72275,#72276,#72277,#72278,
#72279,#72280,#72281,#72282,#72283,#72284,#72285,#72286,#72287,#72288,#72289,
#72290,#72291,#72292,#72293,#72294,#72295,#72296,#72297,#72298,#72299,#72300,
#72301,#72302,#72303,#72304,#72305,#72306,#72307,#72308,#72309,#72310,#72311,
#72312,#72313),.UNSPECIFIED.,.F.,.F.,(4,3,3,3,3,3,3,3,3,3,3,3,3,3,3,3,3,
3,3,3,3,3,3,3,3,3,3,3,3,3,3,3,3,3,3,3,3,3,3,3,3,3,3,3,3,3,3,3,3,3,3,3,3,
3,3,3,3,4),(13.4404181035,14.1832469713423,14.9311788451456,15.6836632577811,
16.4417307823792,17.202055740606,17.9644513437534,18.4746549323,19.2374710902407,
19.9985815368466,20.7569924140862,21.509630605407,22.2582851244697,22.9999062408337,
23.5157081046,24.2597621045338,25.0092545320489,25.7635337985687,26.521784600003,
27.2830357102544,28.0721755009976,28.8305221896519,29.5929229482329,30.3533096498532,
31.1107361457363,31.8623257075202,32.6098454986528,33.3508338437457,33.5961540362,
34.3408789768401,35.0909966454356,35.8458336275569,36.6045522537918,37.3661601097332,
38.154969758904,38.8368239887457,39.599089755228,40.3593159984205,41.116556848427,
41.8678616724636,42.6150717427155,43.3555578410029,43.6766373031,44.4154372840554,
45.1632743442511,45.9157419950385,46.6741354613049,47.0360646138,47.7955806316773,
48.5576994151819,49.3198406379445,50.0808007763051,50.839431318698,51.5923911750364,
52.3413609598882,53.0826832013661,53.8176639786,53.8487877185),
 .UNSPECIFIED.);
#1597=B_SPLINE_CURVE_WITH_KNOTS('',3,(#72315,#72316,#72317,#72318,#72319,
#72320,#72321,#72322,#72323,#72324,#72325,#72326,#72327,#72328,#72329,#72330,
#72331,#72332,#72333,#72334,#72335,#72336,#72337,#72338,#72339,#72340,#72341,
#72342,#72343,#72344,#72345,#72346,#72347,#72348,#72349,#72350,#72351,#72352,
#72353,#72354),.UNSPECIFIED.,.F.,.F.,(4,3,3,3,3,3,3,3,3,3,3,3,3,4),(0.579418789984,
0.725653581578792,0.867122312367032,0.938068556291,1.07176782281773,1.11759224819,
1.24463101759673,1.29713059772,1.42927287787526,1.47665930895,1.61898723804258,
1.77132177608973,1.83573111331,1.84860050261),.UNSPECIFIED.);
#1598=B_SPLINE_CURVE_WITH_KNOTS('',3,(#72355,#72356,#72357,#72358,#72359,
#72360,#72361,#72362,#72363,#72364,#72365,#72366,#72367,#72368,#72369,#72370,
#72371,#72372,#72373,#72374,#72375,#72376,#72377,#72378,#72379,#72380,#72381,
#72382,#72383,#72384,#72385,#72386,#72387,#72388,#72389,#72390,#72391,#72392,
#72393,#72394),.UNSPECIFIED.,.F.,.F.,(4,3,3,3,3,3,3,3,3,3,3,3,3,4),(0.578957415869,
0.726935642898053,0.869358464457875,0.937512229109,1.07080769681197,1.19853817927595,
1.29652194364,1.42846234265899,1.4760627343,1.61769834304174,1.76863899687797,
1.83522042146,1.84649047214,1.84813902128),.UNSPECIFIED.);
#1599=B_SPLINE_CURVE_WITH_KNOTS('',3,(#72399,#72400,#72401,#72402,#72403,
#72404,#72405,#72406,#72407,#72408,#72409,#72410,#72411,#72412,#72413,#72414,
#72415,#72416,#72417,#72418,#72419,#72420,#72421,#72422,#72423,#72424,#72425,
#72426,#72427,#72428,#72429,#72430,#72431,#72432,#72433,#72434,#72435,#72436,
#72437,#72438),.UNSPECIFIED.,.F.,.F.,(4,3,3,3,3,3,3,3,3,3,3,3,3,4),(0.546404786097,
0.691378490918164,0.831851442486203,0.884338413692,1.0179759898933,1.05350843186,
1.1812184524978,1.22269549144,1.35451436280229,1.49122152065914,1.56106898317,
1.71044921676803,1.74092276094,1.74380556781),.UNSPECIFIED.);
#1600=B_SPLINE_CURVE_WITH_KNOTS('',3,(#72440,#72441,#72442,#72443,#72444,
#72445,#72446,#72447,#72448,#72449,#72450,#72451,#72452,#72453,#72454,#72455,
#72456,#72457,#72458,#72459,#72460,#72461,#72462,#72463,#72464,#72465,#72466,
#72467,#72468,#72469,#72470,#72471,#72472,#72473,#72474,#72475,#72476,#72477,
#72478,#72479,#72480,#72481,#72482),.UNSPECIFIED.,.F.,.F.,(4,3,3,3,3,3,
3,3,3,3,3,3,3,3,4),(5.54628902772,6.33044435630308,7.10830578793151,7.87994882881436,
8.64217889818713,9.39932532520428,10.1484181785832,10.8164390246,11.563804771993,
12.3219342993112,13.0975455758633,13.8843705850609,14.6884227142447,14.8537077686,
14.9231167121),.UNSPECIFIED.);
#1601=B_SPLINE_CURVE_WITH_KNOTS('',3,(#72484,#72485,#72486,#72487,#72488,
#72489,#72490,#72491,#72492,#72493,#72494,#72495,#72496,#72497,#72498,#72499,
#72500,#72501,#72502,#72503,#72504,#72505,#72506,#72507,#72508,#72509,#72510,
#72511,#72512,#72513,#72514,#72515,#72516,#72517,#72518,#72519,#72520,#72521,
#72522,#72523,#72524,#72525,#72526,#72527,#72528,#72529,#72530,#72531,#72532,
#72533,#72534,#72535,#72536,#72537,#72538,#72539,#72540,#72541,#72542,#72543,
#72544,#72545,#72546,#72547,#72548,#72549,#72550,#72551,#72552,#72553,#72554,
#72555,#72556,#72557,#72558,#72559),.UNSPECIFIED.,.F.,.F.,(4,3,3,3,3,3,
3,3,3,3,3,3,3,3,3,3,3,3,3,3,3,3,3,3,3,4),(1.16471317114,1.28955678457906,
1.34495894511,1.4697639644744,1.52520817925,1.65292971547884,1.76872520496,
1.90134001405299,2.0346343138382,2.13573896786,2.26681625793335,2.39531374620892,
2.5069575699,2.6339538548235,2.76351336933892,2.87774629091,3.00835142684093,
3.12090556789,3.24957903139955,3.30443948601,3.43081011387895,3.48797183209,
3.613503668297,3.67393178216,3.69717524887,3.70327394785),.UNSPECIFIED.);
#1602=B_SPLINE_CURVE_WITH_KNOTS('',3,(#72561,#72562,#72563,#72564,#72565,
#72566,#72567,#72568,#72569,#72570,#72571,#72572,#72573,#72574,#72575,#72576,
#72577,#72578,#72579,#72580,#72581,#72582,#72583,#72584,#72585,#72586,#72587,
#72588,#72589,#72590,#72591,#72592,#72593,#72594,#72595,#72596,#72597,#72598,
#72599,#72600,#72601,#72602,#72603,#72604,#72605,#72606),.UNSPECIFIED.,
 .F.,.F.,(4,3,3,3,3,3,3,3,3,3,3,3,3,3,3,4),(5.54615686267,6.33030620256032,
7.10816058979279,7.87979597471841,8.64201814773229,9.39915688584315,10.1482427247414,
10.8163068596,11.5638110745412,12.3220901845671,13.098030834098,13.8852098339371,
14.4040971905186,14.6843128354211,14.8776367646747,14.9229845471),
 .UNSPECIFIED.);
#1603=B_SPLINE_CURVE_WITH_KNOTS('',3,(#72608,#72609,#72610,#72611,#72612,
#72613,#72614,#72615,#72616,#72617,#72618,#72619,#72620,#72621,#72622,#72623,
#72624,#72625,#72626,#72627,#72628,#72629,#72630,#72631,#72632,#72633,#72634,
#72635,#72636,#72637,#72638,#72639,#72640,#72641,#72642,#72643,#72644),
 .UNSPECIFIED.,.F.,.F.,(4,3,3,3,3,3,3,3,3,3,3,3,4),(0.54640511867,0.69038189628902,
0.831066058366692,0.965751341507189,1.05350876443,1.1812187883191,1.22269582402,
1.35451469641816,1.49122185483681,1.56106931574,1.71044954193083,1.74092309351,
1.74380590038),.UNSPECIFIED.);
#1604=B_SPLINE_CURVE_WITH_KNOTS('',3,(#72648,#72649,#72650,#72651,#72652,
#72653,#72654,#72655,#72656,#72657,#72658,#72659,#72660,#72661,#72662,#72663,
#72664,#72665,#72666,#72667,#72668,#72669,#72670,#72671,#72672,#72673,#72674,
#72675,#72676,#72677,#72678,#72679,#72680,#72681,#72682,#72683,#72684,#72685,
#72686,#72687,#72688,#72689,#72690,#72691,#72692,#72693,#72694,#72695,#72696,
#72697,#72698,#72699,#72700,#72701,#72702,#72703,#72704,#72705,#72706,#72707,
#72708),.UNSPECIFIED.,.F.,.F.,(4,3,3,3,3,3,3,3,3,3,3,3,3,3,3,3,3,3,3,3,
4),(6.80400424079,7.43551608490868,8.07296241255818,8.71878211416777,9.36915323230095,
10.0253311081077,10.185707897,10.847851527524,11.530459999118,12.1974538393883,
12.8878696266442,13.5782854139,14.2435799397826,14.905962344532,15.5649203367182,
16.2200258486319,16.8684640346437,17.5129910403709,18.1507928771493,18.7732643273,
18.7904488943),.UNSPECIFIED.);
#1605=B_SPLINE_CURVE_WITH_KNOTS('',3,(#72709,#72710,#72711,#72712,#72713,
#72714,#72715,#72716,#72717,#72718,#72719,#72720,#72721,#72722,#72723,#72724,
#72725,#72726,#72727,#72728,#72729,#72730,#72731,#72732,#72733,#72734,#72735,
#72736,#72737,#72738,#72739,#72740,#72741,#72742,#72743,#72744,#72745,#72746,
#72747,#72748,#72749,#72750,#72751,#72752,#72753,#72754,#72755,#72756,#72757,
#72758,#72759,#72760,#72761,#72762,#72763,#72764,#72765,#72766,#72767,#72768,
#72769,#72770,#72771,#72772,#72773,#72774,#72775),.UNSPECIFIED.,.F.,.F.,
(4,3,3,3,3,3,3,3,3,3,3,3,3,3,3,3,3,3,3,3,3,3,4),(6.80309055586,6.83920298432,
7.47379817923227,8.13912629845323,8.78763073366937,9.44086248718233,10.0984392541387,
10.7729352238541,11.4388498023207,12.1176364676603,12.796423133,13.4656868144225,
14.132263549812,14.7961195641698,15.4565492516297,16.112959614828,16.782230410596,
17.4269097691535,18.0671355216093,18.4285891597547,18.6334246721777,18.7701216625788,
18.7900427979),.UNSPECIFIED.);
#1606=B_SPLINE_CURVE_WITH_KNOTS('',5,(#72783,#72784,#72785,#72786,#72787,
#72788),.UNSPECIFIED.,.F.,.F.,(6,6),(-0.791045523784,0.),.UNSPECIFIED.);
#1607=B_SPLINE_CURVE_WITH_KNOTS('',5,(#72790,#72791,#72792,#72793,#72794,
#72795,#72796,#72797,#72798,#72799,#72800,#72801,#72802,#72803,#72804),
 .UNSPECIFIED.,.F.,.F.,(6,3,3,3,6),(-30.0305934991,-22.7207065053,-15.4108195114,
-8.10093251761,-0.791045523784),.UNSPECIFIED.);
#1608=B_SPLINE_CURVE_WITH_KNOTS('',5,(#72806,#72807,#72808,#72809,#72810,
#72811),.UNSPECIFIED.,.F.,.F.,(6,6),(-30.70334581,-30.0305934991),
 .UNSPECIFIED.);
#1609=B_SPLINE_CURVE_WITH_KNOTS('',5,(#72813,#72814,#72815,#72816,#72817,
#72818),.UNSPECIFIED.,.F.,.F.,(6,6),(-31.3760981209,-30.70334581),
 .UNSPECIFIED.);
#1610=B_SPLINE_CURVE_WITH_KNOTS('',5,(#72820,#72821,#72822,#72823,#72824,
#72825,#72826,#72827,#72828,#72829,#72830,#72831,#72832,#72833,#72834),
 .UNSPECIFIED.,.F.,.F.,(6,3,3,3,6),(-60.6156460962,-53.3057591024,-45.9958721086,
-38.6859851147,-31.3760981209),.UNSPECIFIED.);
#1611=B_SPLINE_CURVE_WITH_KNOTS('',5,(#72836,#72837,#72838,#72839,#72840,
#72841),.UNSPECIFIED.,.F.,.F.,(6,6),(-61.40669162,-60.6156460962),
 .UNSPECIFIED.);
#1612=B_SPLINE_CURVE_WITH_KNOTS('',5,(#72845,#72846,#72847,#72848,#72849,
#72850),.UNSPECIFIED.,.F.,.F.,(6,6),(-74.6958207115,-64.888669513),
 .UNSPECIFIED.);
#1613=B_SPLINE_CURVE_WITH_KNOTS('',5,(#72852,#72853,#72854,#72855,#72856,
#72857),.UNSPECIFIED.,.F.,.F.,(6,6),(-84.5029719101,-74.6958207115),
 .UNSPECIFIED.);
#1614=B_SPLINE_CURVE_WITH_KNOTS('',5,(#72865,#72866,#72867,#72868,#72869,
#72870),.UNSPECIFIED.,.F.,.F.,(6,6),(0.,0.634618899121),.UNSPECIFIED.);
#1615=B_SPLINE_CURVE_WITH_KNOTS('',5,(#72874,#72875,#72876,#72877,#72878,
#72879),.UNSPECIFIED.,.F.,.F.,(6,6),(4.43202703274,12.6683819045),
 .UNSPECIFIED.);
#1616=B_SPLINE_CURVE_WITH_KNOTS('',5,(#72881,#72882,#72883,#72884,#72885,
#72886),.UNSPECIFIED.,.F.,.F.,(6,6),(12.6683819045,20.9047367763),
 .UNSPECIFIED.);
#1617=B_SPLINE_CURVE_WITH_KNOTS('',5,(#72890,#72891,#72892,#72893,#72894,
#72895),.UNSPECIFIED.,.F.,.F.,(6,6),(24.7021449099,25.336763809),
 .UNSPECIFIED.);
#1618=B_SPLINE_CURVE_WITH_KNOTS('',5,(#72897,#72898,#72899,#72900,#72901,
#72902),.UNSPECIFIED.,.F.,.F.,(6,6),(25.336763809,32.1215862286),
 .UNSPECIFIED.);
#1619=B_SPLINE_CURVE_WITH_KNOTS('',5,(#72904,#72905,#72906,#72907,#72908,
#72909),.UNSPECIFIED.,.F.,.F.,(6,6),(32.1215862286,33.4669635909),
 .UNSPECIFIED.);
#1620=B_SPLINE_CURVE_WITH_KNOTS('',5,(#72910,#72911,#72912,#72913,#72914,
#72915),.UNSPECIFIED.,.F.,.F.,(6,6),(33.4669635909,40.2517860105),
 .UNSPECIFIED.);
#1621=B_SPLINE_CURVE_WITH_KNOTS('',5,(#72986,#72987,#72988,#72989,#72990,
#72991),.UNSPECIFIED.,.F.,.F.,(6,6),(0.,1.),.UNSPECIFIED.);
#1622=B_SPLINE_CURVE_WITH_KNOTS('',5,(#73068,#73069,#73070,#73071,#73072,
#73073),.UNSPECIFIED.,.F.,.F.,(6,6),(4.43202703274,12.6683819045),
 .UNSPECIFIED.);
#1623=B_SPLINE_CURVE_WITH_KNOTS('',3,(#73143,#73144,#73145,#73146,#73147,
#73148,#73149,#73150,#73151,#73152,#73153,#73154,#73155,#73156,#73157,#73158,
#73159,#73160,#73161,#73162,#73163,#73164,#73165,#73166,#73167,#73168,#73169,
#73170,#73171,#73172,#73173,#73174,#73175,#73176,#73177,#73178,#73179,#73180,
#73181,#73182,#73183,#73184,#73185,#73186,#73187,#73188,#73189,#73190,#73191,
#73192,#73193,#73194,#73195,#73196,#73197,#73198,#73199,#73200),
 .UNSPECIFIED.,.F.,.F.,(4,3,3,3,3,3,3,3,3,3,3,3,3,3,3,3,3,3,3,4),(12.6683819045,
13.1106199615824,13.5570304890591,14.0277809275642,14.4835378398279,14.9420145479918,
15.4026526010081,15.882747950031,16.3457775995096,16.8085437495859,17.2700435239617,
17.3230339970997,17.7823518959161,18.2417043637307,18.7003769570558,19.1576865479113,
19.6116903525143,20.0633375875012,20.5105511785383,20.9047367763),
 .UNSPECIFIED.);
#1624=B_SPLINE_CURVE_WITH_KNOTS('',5,(#73276,#73277,#73278,#73279,#73280,
#73281),.UNSPECIFIED.,.F.,.F.,(6,6),(0.,1.),.UNSPECIFIED.);
#1625=B_SPLINE_CURVE_WITH_KNOTS('',5,(#73351,#73352,#73353,#73354,#73355,
#73356),.UNSPECIFIED.,.F.,.F.,(6,6),(25.336763809,32.1215862286),
 .UNSPECIFIED.);
#1626=B_SPLINE_CURVE_WITH_KNOTS('',3,(#73426,#73427,#73428,#73429,#73430,
#73431,#73432,#73433,#73434,#73435,#73436,#73437,#73438,#73439,#73440,#73441,
#73442,#73443,#73444,#73445,#73446,#73447,#73448,#73449,#73450,#73451,#73452,
#73453,#73454,#73455,#73456,#73457,#73458,#73459,#73460,#73461,#73462,#73463,
#73464,#73465,#73466,#73467,#73468,#73469,#73470,#73471,#73472,#73473,#73474,
#73475,#73476,#73477),.UNSPECIFIED.,.F.,.F.,(4,3,3,3,3,3,3,3,3,3,3,3,3,
3,3,3,3,4),(0.,0.0568525693849193,0.115818688059534,0.173763369030792,0.232053865677185,
0.290632777510717,0.350119962828498,0.409067978904654,0.468824748843247,
0.528581518781839,0.587508828934109,0.646482285375474,0.705424215615768,
0.764242216553829,0.823181662415371,0.881380292059083,0.940690146029541,
1.),.UNSPECIFIED.);
#1627=B_SPLINE_CURVE_WITH_KNOTS('',5,(#73545,#73546,#73547,#73548,#73549,
#73550),.UNSPECIFIED.,.F.,.F.,(6,6),(33.4669635909,40.2517860105),
 .UNSPECIFIED.);
#1628=B_SPLINE_CURVE_WITH_KNOTS('',5,(#73620,#73621,#73622,#73623,#73624,
#73625),.UNSPECIFIED.,.F.,.F.,(6,6),(-1.39421694447,-0.574089330078),
 .UNSPECIFIED.);
#1629=B_SPLINE_CURVE_WITH_KNOTS('',5,(#73733,#73734,#73735,#73736,#73737,
#73738,#73739,#73740,#73741,#73742,#73743,#73744,#73745,#73746,#73747),
 .UNSPECIFIED.,.F.,.F.,(6,3,3,3,6),(-39.7897545658,-32.2822537043,-24.7747528429,
-17.2672519814,-9.75975111992),.UNSPECIFIED.);
#1630=B_SPLINE_CURVE_WITH_KNOTS('',5,(#73835,#73836,#73837,#73838,#73839,
#73840),.UNSPECIFIED.,.F.,.F.,(6,6),(-0.336376155459,0.336376155459),
 .UNSPECIFIED.);
#1631=B_SPLINE_CURVE_WITH_KNOTS('',5,(#73910,#73911,#73912,#73913,#73914,
#73915),.UNSPECIFIED.,.F.,.F.,(6,6),(-0.336376155459,0.336376155459),
 .UNSPECIFIED.);
#1632=B_SPLINE_CURVE_WITH_KNOTS('',5,(#74021,#74022,#74023,#74024,#74025,
#74026,#74027,#74028,#74029,#74030,#74031,#74032,#74033,#74034,#74035),
 .UNSPECIFIED.,.F.,.F.,(6,3,3,3,6),(-39.7897545658,-32.2822537043,-24.7747528429,
-17.2672519814,-9.75975111992),.UNSPECIFIED.);
#1633=B_SPLINE_CURVE_WITH_KNOTS('',5,(#74123,#74124,#74125,#74126,#74127,
#74128),.UNSPECIFIED.,.F.,.F.,(6,6),(-1.39421694447,-0.574089330078),
 .UNSPECIFIED.);
#1634=B_SPLINE_CURVE_WITH_KNOTS('',5,(#74204,#74205,#74206,#74207,#74208,
#74209),.UNSPECIFIED.,.F.,.F.,(6,6),(-4.90357559929,4.90357559929),
 .UNSPECIFIED.);
#1635=B_SPLINE_CURVE_WITH_KNOTS('',5,(#74279,#74280,#74281,#74282,#74283,
#74284),.UNSPECIFIED.,.F.,.F.,(6,6),(-4.90357559929,4.90357559929),
 .UNSPECIFIED.);
#1636=B_SPLINE_CURVE_WITH_KNOTS('',3,(#74305,#74306,#74307,#74308),
 .UNSPECIFIED.,.F.,.F.,(4,4),(1.93787056397,2.72108189072),
 .UNSPECIFIED.);
#1637=B_SPLINE_CURVE_WITH_KNOTS('',3,(#74330,#74331,#74332,#74333),
 .UNSPECIFIED.,.F.,.F.,(4,4),(1.93787056397,2.72108189072),
 .UNSPECIFIED.);
#1638=B_SPLINE_CURVE_WITH_KNOTS('',3,(#74338,#74339,#74340,#74341),
 .UNSPECIFIED.,.F.,.F.,(4,4),(1.93787056397,2.72108189072),
 .UNSPECIFIED.);
#1639=B_SPLINE_CURVE_WITH_KNOTS('',3,(#74363,#74364,#74365,#74366),
 .UNSPECIFIED.,.F.,.F.,(4,4),(1.93787056397,2.72108189072),
 .UNSPECIFIED.);
#1640=B_SPLINE_CURVE_WITH_KNOTS('',4,(#74404,#74405,#74406,#74407,#74408),
 .UNSPECIFIED.,.F.,.F.,(5,5),(0.,1.),.UNSPECIFIED.);
#1641=B_SPLINE_CURVE_WITH_KNOTS('',4,(#74416,#74417,#74418,#74419,#74420),
 .UNSPECIFIED.,.F.,.F.,(5,5),(7.90893025972,8.88329649724),
 .UNSPECIFIED.);
#1642=B_SPLINE_CURVE_WITH_KNOTS('',4,(#74428,#74429,#74430,#74431,#74432),
 .UNSPECIFIED.,.F.,.F.,(5,5),(13.4220086236,14.3963748612),
 .UNSPECIFIED.);
#1643=B_SPLINE_CURVE_WITH_KNOTS('',4,(#74440,#74441,#74442,#74443,#74444),
 .UNSPECIFIED.,.F.,.F.,(5,5),(13.4220086236,14.3963748612),
 .UNSPECIFIED.);
#1644=B_SPLINE_CURVE_WITH_KNOTS('',5,(#74544,#74545,#74546,#74547,#74548,
#74549),.UNSPECIFIED.,.F.,.F.,(6,6),(1.465995819,7.32028714189),
 .UNSPECIFIED.);
#1645=B_SPLINE_CURVE_WITH_KNOTS('',4,(#74613,#74614,#74615,#74616,#74617),
 .UNSPECIFIED.,.F.,.F.,(5,5),(13.4220086236,14.3963748612),
 .UNSPECIFIED.);
#1646=B_SPLINE_CURVE_WITH_KNOTS('',3,(#74630,#74631,#74632,#74633,#74634,
#74635,#74636,#74637,#74638,#74639),.UNSPECIFIED.,.F.,.F.,(4,2,2,2,4),(-0.319033797120111,
-0.292165211589356,-0.265296626058601,-0.238938061557758,-0.212579497056914),
 .UNSPECIFIED.);
#1647=B_SPLINE_CURVE_WITH_KNOTS('',3,(#74643,#74644,#74645,#74646,#74647,
#74648,#74649,#74650,#74651,#74652),.UNSPECIFIED.,.F.,.F.,(4,2,2,2,4),(-0.425158994113829,
-0.398800429612985,-0.372441865112142,-0.345573279581387,-0.318704694050632),
 .UNSPECIFIED.);
#1648=B_SPLINE_CURVE_WITH_KNOTS('',4,(#74672,#74673,#74674,#74675,#74676),
 .UNSPECIFIED.,.F.,.F.,(5,5),(13.4220086236,14.3963748612),
 .UNSPECIFIED.);
#1649=B_SPLINE_CURVE_WITH_KNOTS('',4,(#74733,#74734,#74735,#74736,#74737),
 .UNSPECIFIED.,.F.,.F.,(5,5),(7.90893025972,8.88329649724),
 .UNSPECIFIED.);
#1650=B_SPLINE_CURVE_WITH_KNOTS('',3,(#74750,#74751,#74752,#74753,#74754,
#74755,#74756,#74757,#74758,#74759),.UNSPECIFIED.,.F.,.F.,(4,2,2,2,4),(-0.107173137775093,
-0.0799325798318727,-0.0526920218886528,-0.0263460109443264,0.),
 .UNSPECIFIED.);
#1651=B_SPLINE_CURVE_WITH_KNOTS('',3,(#74763,#74764,#74765,#74766,#74767,
#74768,#74769,#74770,#74771,#74772),.UNSPECIFIED.,.F.,.F.,(4,2,2,2,4),(-0.213889101174212,
-0.187543090229885,-0.161197079285559,-0.133956521342339,-0.106715963399119),
 .UNSPECIFIED.);
#1652=B_SPLINE_CURVE_WITH_KNOTS('',4,(#74791,#74792,#74793,#74794,#74795),
 .UNSPECIFIED.,.F.,.F.,(5,5),(7.90893025972,8.88329649724),
 .UNSPECIFIED.);
#1653=B_SPLINE_CURVE_WITH_KNOTS('',3,(#75099,#75100,#75101,#75102,#75103,
#75104,#75105,#75106,#75107,#75108),.UNSPECIFIED.,.F.,.F.,(4,2,2,2,4),(-0.321679119149099,
-0.294322680562913,-0.266966241976726,-0.24062267379048,-0.214279105604234),
 .UNSPECIFIED.);
#1654=B_SPLINE_CURVE_WITH_KNOTS('',3,(#75110,#75111,#75112,#75113,#75114,
#75115,#75116,#75117,#75118,#75119),.UNSPECIFIED.,.F.,.F.,(4,2,2,2,4),(0.321158197663602,
0.348514636249788,0.375871074835975,0.402214643022221,0.428558211208467),
 .UNSPECIFIED.);
#1655=B_SPLINE_CURVE_WITH_KNOTS('',5,(#75123,#75124,#75125,#75126,#75127,
#75128),.UNSPECIFIED.,.F.,.F.,(6,6),(148.878135266,165.903598687),
 .UNSPECIFIED.);
#1656=B_SPLINE_CURVE_WITH_KNOTS('',5,(#75131,#75132,#75133,#75134,#75135,
#75136),.UNSPECIFIED.,.F.,.F.,(6,6),(0.,2.27905325485),.UNSPECIFIED.);
#1657=B_SPLINE_CURVE_WITH_KNOTS('',5,(#75139,#75140,#75141,#75142,#75143,
#75144),.UNSPECIFIED.,.F.,.F.,(6,6),(0.,2.27905325485),.UNSPECIFIED.);
#1658=B_SPLINE_CURVE_WITH_KNOTS('',5,(#75147,#75148,#75149,#75150,#75151,
#75152),.UNSPECIFIED.,.F.,.F.,(6,6),(124.379562504,141.405025925),
 .UNSPECIFIED.);
#1659=B_SPLINE_CURVE_WITH_KNOTS('',4,(#75156,#75157,#75158,#75159,#75160),
 .UNSPECIFIED.,.F.,.F.,(5,5),(4.11843680488,6.1261056745),.UNSPECIFIED.);
#1660=B_SPLINE_CURVE_WITH_KNOTS('',4,(#75164,#75165,#75166,#75167,#75168),
 .UNSPECIFIED.,.F.,.F.,(5,5),(2.04203522484,4.04970409445),
 .UNSPECIFIED.);
#1661=B_SPLINE_CURVE_WITH_KNOTS('',5,(#75173,#75174,#75175,#75176,#75177,
#75178),.UNSPECIFIED.,.F.,.F.,(6,6),(1.465995819,7.32028714189),
 .UNSPECIFIED.);
#1662=B_SPLINE_CURVE_WITH_KNOTS('',3,(#75231,#75232,#75233,#75234,#75235,
#75236,#75237,#75238,#75239,#75240),.UNSPECIFIED.,.F.,.F.,(4,2,2,2,4),(-0.106582101769708,
-0.0796485655513957,-0.0527150293330838,-0.0263575146665419,0.),
 .UNSPECIFIED.);
#1663=B_SPLINE_CURVE_WITH_KNOTS('',3,(#75244,#75245,#75246,#75247,#75248,
#75249,#75250,#75251,#75252,#75253),.UNSPECIFIED.,.F.,.F.,(4,2,2,2,4),(0.212791235802262,
0.239148750468804,0.265506265135346,0.292439801353658,0.31937333757197),
 .UNSPECIFIED.);
#1664=B_SPLINE_CURVE_WITH_KNOTS('',5,(#75314,#75315,#75316,#75317,#75318,
#75319,#75320,#75321,#75322),.UNSPECIFIED.,.F.,.F.,(6,3,6),(-1.52206773895,
0.,8.40229708781167),.UNSPECIFIED.);
#1665=B_SPLINE_CURVE_WITH_KNOTS('',3,(#75337,#75338,#75339,#75340,#75341,
#75342,#75343,#75344,#75345,#75346,#75347,#75348,#75349,#75350,#75351,#75352,
#75353,#75354,#75355,#75356,#75357,#75358,#75359,#75360,#75361,#75362,#75363,
#75364),.UNSPECIFIED.,.F.,.F.,(4,3,3,3,3,3,3,3,3,4),(-0.271480002345994,
-0.251044878779879,-0.221887843336835,-0.191803254069106,-0.161041040318657,
-0.129499206095465,-0.096441307247811,-0.0623399505509545,-0.0260590387577341,
-3.17944058136899E-7),.UNSPECIFIED.);
#1666=B_SPLINE_CURVE_WITH_KNOTS('',5,(#75402,#75403,#75404,#75405,#75406,
#75407,#75408,#75409,#75410,#75411,#75412,#75413),.UNSPECIFIED.,.F.,.F.,
(6,3,3,6),(0.,0.469175571973241,0.767594863359273,1.),.UNSPECIFIED.);
#1667=B_SPLINE_CURVE_WITH_KNOTS('',5,(#75415,#75416,#75417,#75418,#75419,
#75420,#75421,#75422,#75423,#75424,#75425,#75426),.UNSPECIFIED.,.F.,.F.,
(6,3,3,6),(0.,1.23981126536,4.14117682427,4.7101423031),.UNSPECIFIED.);
#1668=B_SPLINE_CURVE_WITH_KNOTS('',5,(#75427,#75428,#75429,#75430,#75431,
#75432,#75433,#75434,#75435,#75436,#75437,#75438),.UNSPECIFIED.,.F.,.F.,
(6,3,3,6),(0.,0.292934935973857,0.816928097127191,1.),.UNSPECIFIED.);
#1669=B_SPLINE_CURVE_WITH_KNOTS('',5,(#75496,#75497,#75498,#75499,#75500,
#75501,#75502,#75503,#75504),.UNSPECIFIED.,.F.,.F.,(6,3,6),(-1.52206773895,
0.,8.40229708780905),.UNSPECIFIED.);
#1670=B_SPLINE_CURVE_WITH_KNOTS('',3,(#75515,#75516,#75517,#75518,#75519,
#75520,#75521,#75522,#75523,#75524,#75525,#75526,#75527,#75528,#75529,#75530,
#75531,#75532,#75533,#75534,#75535,#75536,#75537,#75538,#75539,#75540,#75541,
#75542),.UNSPECIFIED.,.F.,.F.,(4,3,3,3,3,3,3,3,3,4),(-0.271480014742483,
-0.251044890243242,-0.221887853468803,-0.191803262827329,-0.161041047672182,
-0.129499212008716,-0.0964413116515472,-0.0623399533975151,-0.0260590399476091,
-3.17944058081387E-7),.UNSPECIFIED.);
#1671=B_SPLINE_CURVE_WITH_KNOTS('',5,(#75558,#75559,#75560,#75561,#75562,
#75563,#75564,#75565,#75566,#75567,#75568,#75569),.UNSPECIFIED.,.F.,.F.,
(6,3,3,6),(17.5092154859,21.7374875265,29.3008927769,31.9433833551),
 .UNSPECIFIED.);
#1672=B_SPLINE_CURVE_WITH_KNOTS('',5,(#75571,#75572,#75573,#75574,#75575,
#75576,#75577,#75578,#75579,#75580,#75581,#75582),.UNSPECIFIED.,.F.,.F.,
(6,3,3,6),(0.,0.263221615309587,0.879204184880883,1.),.UNSPECIFIED.);
#1673=B_SPLINE_CURVE_WITH_KNOTS('',5,(#75584,#75585,#75586,#75587,#75588,
#75589,#75590,#75591,#75592,#75593,#75594,#75595),.UNSPECIFIED.,.F.,.F.,
(6,3,3,6),(0.,3.06410506181,5.01303018899,6.53082821197),.UNSPECIFIED.);
#1674=B_SPLINE_CURVE_WITH_KNOTS('',5,(#75698,#75699,#75700,#75701,#75702,
#75703,#75704,#75705,#75706,#75707,#75708,#75709),.UNSPECIFIED.,.F.,.F.,
(6,3,3,6),(0.,3.06410506181,5.01303018899,6.53082821197),.UNSPECIFIED.);
#1675=B_SPLINE_CURVE_WITH_KNOTS('',5,(#75735,#75736,#75737,#75738,#75739,
#75740,#75741,#75742,#75743,#75744,#75745,#75746),.UNSPECIFIED.,.F.,.F.,
(6,3,3,6),(0.,0.263221615309587,0.879204184880883,1.),.UNSPECIFIED.);
#1676=B_SPLINE_CURVE_WITH_KNOTS('',5,(#75773,#75774,#75775,#75776,#75777,
#75778,#75779,#75780,#75781,#75782,#75783,#75784),.UNSPECIFIED.,.F.,.F.,
(6,3,3,6),(17.5092154859,21.7374875265,29.3008927769,31.9433833551),
 .UNSPECIFIED.);
#1677=B_SPLINE_CURVE_WITH_KNOTS('',3,(#75807,#75808,#75809,#75810,#75811,
#75812,#75813,#75814,#75815,#75816,#75817,#75818,#75819,#75820,#75821,#75822,
#75823,#75824,#75825,#75826,#75827,#75828,#75829,#75830,#75831,#75832,#75833,
#75834),.UNSPECIFIED.,.F.,.F.,(4,3,3,3,3,3,3,3,3,4),(-0.271480015020472,
-0.251044890500306,-0.221887853696004,-0.191803263023729,-0.161041047837091,
-0.129499212141309,-0.0964413117502902,-0.0623399534613448,-0.0260590399743052,
-3.17944058358943E-7),.UNSPECIFIED.);
#1678=B_SPLINE_CURVE_WITH_KNOTS('',5,(#75856,#75857,#75858,#75859,#75860,
#75861,#75862,#75863,#75864),.UNSPECIFIED.,.F.,.F.,(6,3,6),(-1.52206773895,
0.,8.40229708781167),.UNSPECIFIED.);
#1679=B_SPLINE_CURVE_WITH_KNOTS('',5,(#75897,#75898,#75899,#75900,#75901,
#75902,#75903,#75904,#75905),.UNSPECIFIED.,.F.,.F.,(6,3,6),(-1.52206773895,
0.,8.40229708780905),.UNSPECIFIED.);
#1680=B_SPLINE_CURVE_WITH_KNOTS('',3,(#75928,#75929,#75930,#75931,#75932,
#75933,#75934,#75935,#75936,#75937,#75938,#75939,#75940,#75941,#75942,#75943,
#75944,#75945,#75946,#75947,#75948,#75949,#75950,#75951,#75952,#75953,#75954,
#75955),.UNSPECIFIED.,.F.,.F.,(4,3,3,3,3,3,3,3,3,4),(-0.271480002344046,
-0.251044878778074,-0.221887843335248,-0.191803254067733,-0.161041040317497,
-0.129499206094535,-0.0964413072471161,-0.0623399505504905,-0.0260590387575272,
-3.17944058136899E-7),.UNSPECIFIED.);
#1681=B_SPLINE_CURVE_WITH_KNOTS('',5,(#75983,#75984,#75985,#75986,#75987,
#75988,#75989,#75990,#75991,#75992,#75993,#75994),.UNSPECIFIED.,.F.,.F.,
(6,3,3,6),(0.,0.292934935973857,0.816928097127191,1.),.UNSPECIFIED.);
#1682=B_SPLINE_CURVE_WITH_KNOTS('',5,(#76022,#76023,#76024,#76025,#76026,
#76027,#76028,#76029,#76030,#76031,#76032,#76033),.UNSPECIFIED.,.F.,.F.,
(6,3,3,6),(0.,1.23981126536,4.14117682427,4.7101423031),.UNSPECIFIED.);
#1683=B_SPLINE_CURVE_WITH_KNOTS('',5,(#76059,#76060,#76061,#76062,#76063,
#76064,#76065,#76066,#76067,#76068,#76069,#76070),.UNSPECIFIED.,.F.,.F.,
(6,3,3,6),(0.,3.06410506181,5.01303018899,6.53082821197),.UNSPECIFIED.);
#1684=B_SPLINE_CURVE_WITH_KNOTS('',5,(#76115,#76116,#76117,#76118,#76119,
#76120),.UNSPECIFIED.,.F.,.F.,(6,6),(0.,1.),.UNSPECIFIED.);
#1685=B_SPLINE_CURVE_WITH_KNOTS('',5,(#76221,#76222,#76223,#76224,#76225,
#76226,#76227,#76228,#76229,#76230,#76231,#76232,#76233,#76234,#76235),
 .UNSPECIFIED.,.F.,.F.,(6,3,3,3,6),(0.,2.13949651284,3.65547289001,4.94562974894,
5.62440522293),.UNSPECIFIED.);
#1686=B_SPLINE_CURVE_WITH_KNOTS('',5,(#76238,#76239,#76240,#76241,#76242,
#76243,#76244,#76245,#76246,#76247,#76248,#76249,#76250,#76251,#76252),
 .UNSPECIFIED.,.F.,.F.,(6,3,3,3,6),(0.,2.13949651284,3.65547289001,4.94562974894,
5.62440522293),.UNSPECIFIED.);
#1687=B_SPLINE_CURVE_WITH_KNOTS('',5,(#76274,#76275,#76276,#76277,#76278,
#76279,#76280,#76281,#76282),.UNSPECIFIED.,.F.,.F.,(6,3,6),(0.,1.07297825382,
3.85154891337),.UNSPECIFIED.);
#1688=B_SPLINE_CURVE_WITH_KNOTS('',5,(#76283,#76284,#76285,#76286,#76287,
#76288,#76289,#76290,#76291),.UNSPECIFIED.,.F.,.F.,(6,3,6),(0.,0.278583571948246,
1.),.UNSPECIFIED.);
#1689=B_SPLINE_CURVE_WITH_KNOTS('',5,(#76329,#76330,#76331,#76332,#76333,
#76334,#76335,#76336,#76337,#76338,#76339,#76340,#76341,#76342,#76343,#76344,
#76345,#76346),.UNSPECIFIED.,.F.,.F.,(6,3,3,3,3,6),(-1.28529177837993,0.,
8.34825709363,17.7305069581,25.102843518,27.4630296434),.UNSPECIFIED.);
#1690=B_SPLINE_CURVE_WITH_KNOTS('',5,(#76348,#76349,#76350,#76351,#76352,
#76353,#76354,#76355,#76356,#76357,#76358,#76359,#76360,#76361,#76362,#76363,
#76364,#76365),.UNSPECIFIED.,.F.,.F.,(6,3,3,3,3,6),(-1.28529178055,0.,8.34825709363,
17.7305069581,25.102843518,27.4630296434),.UNSPECIFIED.);
#1691=B_SPLINE_CURVE_WITH_KNOTS('',5,(#76412,#76413,#76414,#76415,#76416,
#76417,#76418,#76419,#76420,#76421,#76422,#76423,#76424,#76425,#76426,#76427,
#76428,#76429),.UNSPECIFIED.,.F.,.F.,(6,3,3,3,3,6),(-1.28529177837993,0.,
8.34825709363,17.7305069581,25.102843518,27.4630296434),.UNSPECIFIED.);
#1692=B_SPLINE_CURVE_WITH_KNOTS('',5,(#76430,#76431,#76432,#76433,#76434,
#76435,#76436,#76437,#76438,#76439,#76440,#76441,#76442,#76443,#76444,#76445,
#76446,#76447),.UNSPECIFIED.,.F.,.F.,(6,3,3,3,3,6),(0.,0.0447084113745589,
0.335099525711938,0.661457705937853,0.917901776225663,1.),.UNSPECIFIED.);
#1693=B_SPLINE_CURVE_WITH_KNOTS('',5,(#76467,#76468,#76469,#76470,#76471,
#76472,#76473,#76474,#76475),.UNSPECIFIED.,.F.,.F.,(6,3,6),(0.,0.278583571948246,
1.),.UNSPECIFIED.);
#1694=B_SPLINE_CURVE_WITH_KNOTS('',5,(#76477,#76478,#76479,#76480,#76481,
#76482,#76483,#76484,#76485),.UNSPECIFIED.,.F.,.F.,(6,3,6),(0.,1.07297825382,
3.85154891337),.UNSPECIFIED.);
#1695=B_SPLINE_CURVE_WITH_KNOTS('',5,(#76520,#76521,#76522,#76523,#76524,
#76525,#76526,#76527,#76528,#76529,#76530,#76531,#76532,#76533,#76534),
 .UNSPECIFIED.,.F.,.F.,(6,3,3,3,6),(0.,2.13949651284,3.65547289001,4.94562974894,
5.62440522293),.UNSPECIFIED.);
#1696=B_SPLINE_CURVE_WITH_KNOTS('',5,(#76535,#76536,#76537,#76538,#76539,
#76540,#76541,#76542,#76543,#76544,#76545,#76546,#76547,#76548,#76549),
 .UNSPECIFIED.,.F.,.F.,(6,3,3,3,6),(0.,0.380395157894659,0.649930569566199,
0.879316043726239,1.),.UNSPECIFIED.);
#1697=B_SPLINE_CURVE_WITH_KNOTS('',5,(#76565,#76566,#76567,#76568,#76569,
#76570),.UNSPECIFIED.,.F.,.F.,(6,6),(0.,0.144177579366703),
 .UNSPECIFIED.);
#1698=B_SPLINE_CURVE_WITH_KNOTS('',5,(#76575,#76576,#76577,#76578,#76579,
#76580),.UNSPECIFIED.,.F.,.F.,(6,6),(0.,0.144177579366703),
 .UNSPECIFIED.);
#1699=B_SPLINE_CURVE_WITH_KNOTS('',5,(#76582,#76583,#76584,#76585,#76586,
#76587),.UNSPECIFIED.,.F.,.F.,(6,6),(0.266540302038896,2.4758008952433),
 .UNSPECIFIED.);
#1700=B_SPLINE_CURVE_WITH_KNOTS('',5,(#76602,#76603,#76604,#76605,#76606,
#76607),.UNSPECIFIED.,.F.,.F.,(6,6),(0.,3.5713550833),.UNSPECIFIED.);
#1701=B_SPLINE_CURVE_WITH_KNOTS('',5,(#76610,#76611,#76612,#76613,#76614,
#76615),.UNSPECIFIED.,.F.,.F.,(6,6),(2.4758008952433,3.5713550833),
 .UNSPECIFIED.);
#1702=B_SPLINE_CURVE_WITH_KNOTS('',5,(#76619,#76620,#76621,#76622,#76623,
#76624,#76625,#76626,#76627,#76628,#76629,#76630,#76631),.UNSPECIFIED.,
 .F.,.F.,(6,2,2,1,2,6),(0.,0.129543792616671,0.328284019716155,0.555394747336254,
0.717494953154769,1.),.UNSPECIFIED.);
#1703=B_SPLINE_CURVE_WITH_KNOTS('',5,(#76635,#76636,#76637,#76638,#76639,
#76640,#76641,#76642,#76643,#76644,#76645,#76646,#76647,#76648,#76649,#76650,
#76651,#76652),.UNSPECIFIED.,.F.,.F.,(6,3,3,3,3,6),(2.04066423734,2.62011481805,
3.50908168923,4.52495007124,5.25002578886,6.51367347233),.UNSPECIFIED.);
#1704=B_SPLINE_CURVE_WITH_KNOTS('',5,(#76653,#76654,#76655,#76656,#76657,
#76658),.UNSPECIFIED.,.F.,.F.,(6,6),(2.47580089524329,3.5713550833),
 .UNSPECIFIED.);
#1705=B_SPLINE_CURVE_WITH_KNOTS('',5,(#76660,#76661,#76662,#76663,#76664,
#76665),.UNSPECIFIED.,.F.,.F.,(6,6),(0.266540302038896,2.47580089524329),
 .UNSPECIFIED.);
#1706=B_SPLINE_CURVE_WITH_KNOTS('',5,(#76682,#76683,#76684,#76685,#76686,
#76687),.UNSPECIFIED.,.F.,.F.,(6,6),(0.,3.5713550833),.UNSPECIFIED.);
#1707=B_SPLINE_CURVE_WITH_KNOTS('',5,(#76693,#76694,#76695,#76696,#76697,
#76698,#76699,#76700,#76701,#76702,#76703,#76704),.UNSPECIFIED.,.F.,.F.,
(6,3,3,6),(0.380642553355298,3.39713474113,6.68643994484,8.37826425912),
 .UNSPECIFIED.);
#1708=B_SPLINE_CURVE_WITH_KNOTS('',5,(#76706,#76707,#76708,#76709,#76710,
#76711),.UNSPECIFIED.,.F.,.F.,(6,6),(0.836079546685,9.68451754643),
 .UNSPECIFIED.);
#1709=B_SPLINE_CURVE_WITH_KNOTS('',3,(#76714,#76715,#76716,#76717),
 .UNSPECIFIED.,.F.,.F.,(4,4),(0.,1.89584162936),.UNSPECIFIED.);
#1710=B_SPLINE_CURVE_WITH_KNOTS('',3,(#76721,#76722,#76723,#76724,#76725,
#76726),.UNSPECIFIED.,.F.,.F.,(4,2,4),(-0.0280207886793255,-0.0140109256855064,
-1.00277206334723E-6),.UNSPECIFIED.);
#1711=B_SPLINE_CURVE_WITH_KNOTS('',5,(#76728,#76729,#76730,#76731,#76732,
#76733),.UNSPECIFIED.,.F.,.F.,(6,6),(0.,1.1155886229),.UNSPECIFIED.);
#1712=B_SPLINE_CURVE_WITH_KNOTS('',5,(#76735,#76736,#76737,#76738,#76739,
#76740,#76741,#76742,#76743,#76744,#76745,#76746,#76747,#76748,#76749),
 .UNSPECIFIED.,.F.,.F.,(6,3,3,3,6),(0.,0.404403504835335,0.600830610026598,
0.80245741666853,1.),.UNSPECIFIED.);
#1713=B_SPLINE_CURVE_WITH_KNOTS('',5,(#76751,#76752,#76753,#76754,#76755,
#76756),.UNSPECIFIED.,.F.,.F.,(6,6),(0.,2.29845936737),.UNSPECIFIED.);
#1714=B_SPLINE_CURVE_WITH_KNOTS('',5,(#76759,#76760,#76761,#76762,#76763,
#76764,#76765,#76766,#76767,#76768,#76769,#76770,#76771,#76772,#76773),
 .UNSPECIFIED.,.F.,.F.,(6,3,3,3,6),(3.5609211009699,6.696077534,12.6191089245,
16.7682744334,17.8619151354404),.UNSPECIFIED.);
#1715=B_SPLINE_CURVE_WITH_KNOTS('',5,(#76776,#76777,#76778,#76779,#76780,
#76781),.UNSPECIFIED.,.F.,.F.,(6,6),(1.73726460462955E-9,3.5609211009699),
 .UNSPECIFIED.);
#1716=B_SPLINE_CURVE_WITH_KNOTS('',5,(#76790,#76791,#76792,#76793,#76794,
#76795,#76796,#76797,#76798,#76799,#76800,#76801,#76802,#76803,#76804),
 .UNSPECIFIED.,.F.,.F.,(6,3,3,3,6),(3.56092110096989,6.696077534,12.6191089245,
16.7682744334,17.8619151354404),.UNSPECIFIED.);
#1717=B_SPLINE_CURVE_WITH_KNOTS('',5,(#76814,#76815,#76816,#76817,#76818,
#76819),.UNSPECIFIED.,.F.,.F.,(6,6),(1.73726460462955E-9,3.56092110096989),
 .UNSPECIFIED.);
#1718=B_SPLINE_CURVE_WITH_KNOTS('',5,(#76822,#76823,#76824,#76825,#76826,
#76827,#76828,#76829,#76830,#76831,#76832,#76833),.UNSPECIFIED.,.F.,.F.,
(6,3,3,6),(0.380642553355298,3.39713474113,6.68643994484,8.37826425912),
 .UNSPECIFIED.);
#1719=B_SPLINE_CURVE_WITH_KNOTS('',3,(#76838,#76839,#76840,#76841),
 .UNSPECIFIED.,.F.,.F.,(4,4),(0.,1.89584162936),.UNSPECIFIED.);
#1720=B_SPLINE_CURVE_WITH_KNOTS('',5,(#76844,#76845,#76846,#76847,#76848,
#76849),.UNSPECIFIED.,.F.,.F.,(6,6),(0.836079546685,9.68451754643),
 .UNSPECIFIED.);
#1721=B_SPLINE_CURVE_WITH_KNOTS('',5,(#76855,#76856,#76857,#76858,#76859,
#76860),.UNSPECIFIED.,.F.,.F.,(6,6),(0.,2.29845936737),.UNSPECIFIED.);
#1722=B_SPLINE_CURVE_WITH_KNOTS('',5,(#76862,#76863,#76864,#76865,#76866,
#76867,#76868,#76869,#76870,#76871,#76872,#76873,#76874,#76875,#76876),
 .UNSPECIFIED.,.F.,.F.,(6,3,3,3,6),(0.,1.14196741734,1.69664449439,2.26600465298,
2.82383165251),.UNSPECIFIED.);
#1723=B_SPLINE_CURVE_WITH_KNOTS('',5,(#76878,#76879,#76880,#76881,#76882,
#76883),.UNSPECIFIED.,.F.,.F.,(6,6),(0.,1.1155886229),.UNSPECIFIED.);
#1724=B_SPLINE_CURVE_WITH_KNOTS('',3,(#76884,#76885,#76886,#76887,#76888,
#76889),.UNSPECIFIED.,.F.,.F.,(4,2,4),(-0.0280207886793728,-0.0140109256855102,
-1.0027720631911E-6),.UNSPECIFIED.);
#1725=B_SPLINE_CURVE_WITH_KNOTS('',5,(#76893,#76894,#76895,#76896,#76897,
#76898,#76899,#76900,#76901,#76902,#76903,#76904,#76905,#76906,#76907),
 .UNSPECIFIED.,.F.,.F.,(6,3,3,3,6),(0.,1.06902836413,2.19771269917,3.2241260379,
4.7004853448),.UNSPECIFIED.);
#1726=B_SPLINE_CURVE_WITH_KNOTS('',5,(#76909,#76910,#76911,#76912,#76913,
#76914),.UNSPECIFIED.,.F.,.F.,(6,6),(0.,6.43612007405),.UNSPECIFIED.);
#1727=B_SPLINE_CURVE_WITH_KNOTS('',5,(#76926,#76927,#76928,#76929,#76930,
#76931,#76932,#76933,#76934,#76935,#76936,#76937,#76938,#76939,#76940),
 .UNSPECIFIED.,.F.,.F.,(6,3,3,3,6),(0.0395158293388482,7.53253625942,14.2747183071,
18.8083875826,22.71906151),.UNSPECIFIED.);
#1728=B_SPLINE_CURVE_WITH_KNOTS('',5,(#76941,#76942,#76943,#76944,#76945,
#76946,#76947,#76948,#76949),.UNSPECIFIED.,.F.,.F.,(6,3,6),(0.,0.365735348523741,
1.),.UNSPECIFIED.);
#1729=B_SPLINE_CURVE_WITH_KNOTS('',5,(#76952,#76953,#76954,#76955,#76956,
#76957,#76958,#76959,#76960),.UNSPECIFIED.,.F.,.F.,(6,3,6),(0.,2.92723336323,
3.88093368919),.UNSPECIFIED.);
#1730=B_SPLINE_CURVE_WITH_KNOTS('',5,(#76962,#76963,#76964,#76965,#76966,
#76967,#76968,#76969,#76970,#76971,#76972,#76973,#76974,#76975,#76976,#76977,
#76978),.UNSPECIFIED.,.F.,.F.,(6,3,3,5,6),(3.11522256756,4.13897763214,
6.99130562041,9.89933117719,9.89969814681689),.UNSPECIFIED.);
#1731=B_SPLINE_CURVE_WITH_KNOTS('',5,(#76982,#76983,#76984,#76985,#76986,
#76987,#76988,#76989,#76990,#76991,#76992,#76993),.UNSPECIFIED.,.F.,.F.,
(6,3,3,6),(3.11522256756,4.13897763214,6.99130562041,9.89912618426),
 .UNSPECIFIED.);
#1732=B_SPLINE_CURVE_WITH_KNOTS('',5,(#76995,#76996,#76997,#76998,#76999,
#77000,#77001,#77002,#77003,#77004,#77005,#77006,#77007,#77008),
 .UNSPECIFIED.,.F.,.F.,(6,3,5,6),(0.,2.92723336323,3.88093368919,3.88140412218319),
 .UNSPECIFIED.);
#1733=B_SPLINE_CURVE_WITH_KNOTS('',5,(#77024,#77025,#77026,#77027,#77028,
#77029),.UNSPECIFIED.,.F.,.F.,(6,6),(0.,1.),.UNSPECIFIED.);
#1734=B_SPLINE_CURVE_WITH_KNOTS('',5,(#77031,#77032,#77033,#77034,#77035,
#77036,#77037,#77038,#77039,#77040,#77041,#77042,#77043,#77044,#77045),
 .UNSPECIFIED.,.F.,.F.,(6,3,3,3,6),(0.,0.227429357973136,0.467550165133747,
0.685913432634515,1.),.UNSPECIFIED.);
#1735=B_SPLINE_CURVE_WITH_KNOTS('',5,(#77047,#77048,#77049,#77050,#77051,
#77052,#77053,#77054,#77055),.UNSPECIFIED.,.F.,.F.,(6,3,6),(1.18944404077E-12,
1.10170421198,3.01229896543),.UNSPECIFIED.);
#1736=B_SPLINE_CURVE_WITH_KNOTS('',5,(#77056,#77057,#77058,#77059,#77060,
#77061,#77062,#77063,#77064,#77065,#77066,#77067,#77068,#77069,#77070),
 .UNSPECIFIED.,.F.,.F.,(6,3,3,3,6),(0.0395158293387482,7.53253625942,14.2747183071,
18.8083875826,22.71906151),.UNSPECIFIED.);
#1737=B_SPLINE_CURVE_WITH_KNOTS('',5,(#77114,#77115,#77116,#77117,#77118,
#77119,#77120,#77121,#77122,#77123,#77124,#77125,#77126,#77127,#77128,#77129,
#77130,#77131),.UNSPECIFIED.,.F.,.F.,(6,3,3,3,3,6),(2.04066423734,2.62011481805,
3.50908168923,4.52495007124,5.25002578886,6.51367347233),.UNSPECIFIED.);
#1738=B_SPLINE_CURVE_WITH_KNOTS('',5,(#77136,#77137,#77138,#77139,#77140,
#77141,#77142,#77143,#77144,#77145,#77146,#77147,#77148,#77149,#77150,#77151,
#77152),.UNSPECIFIED.,.F.,.F.,(6,3,3,5,6),(3.11522256756,4.13897763214,
6.99130562041,9.89933117719,9.89969814681689),.UNSPECIFIED.);
#1739=B_SPLINE_CURVE_WITH_KNOTS('',5,(#77154,#77155,#77156,#77157,#77158,
#77159,#77160,#77161,#77162),.UNSPECIFIED.,.F.,.F.,(6,3,6),(0.,0.754260082150734,
1.),.UNSPECIFIED.);
#1740=B_SPLINE_CURVE_WITH_KNOTS('',5,(#77168,#77169,#77170,#77171,#77172,
#77173,#77174,#77175,#77176,#77177,#77178,#77179,#77180,#77181),
 .UNSPECIFIED.,.F.,.F.,(6,3,5,6),(0.,2.92723336323,3.88093368919,3.88140411694228),
 .UNSPECIFIED.);
#1741=B_SPLINE_CURVE_WITH_KNOTS('',5,(#77183,#77184,#77185,#77186,#77187,
#77188,#77189,#77190,#77191,#77192,#77193,#77194),.UNSPECIFIED.,.F.,.F.,
(6,3,3,6),(3.11522256756,4.13897763214,6.99130562041,9.89912618426),
 .UNSPECIFIED.);
#1742=B_SPLINE_CURVE_WITH_KNOTS('',5,(#77198,#77199,#77200,#77201,#77202,
#77203,#77204,#77205,#77206,#77207,#77208,#77209,#77210,#77211,#77212,#77213,
#77214,#77215),.UNSPECIFIED.,.F.,.F.,(6,3,3,3,3,6),(2.04066423734,2.62011481805,
3.50908168923,4.52495007124,5.25002578886,6.51367347233),.UNSPECIFIED.);
#1743=B_SPLINE_CURVE_WITH_KNOTS('',5,(#77281,#77282,#77283,#77284,#77285,
#77286,#77287,#77288,#77289,#77290,#77291,#77292),.UNSPECIFIED.,.F.,.F.,
(6,3,3,6),(0.,3.39713474113,6.68643994484,8.37826425912),.UNSPECIFIED.);
#1744=B_SPLINE_CURVE_WITH_KNOTS('',5,(#77318,#77319,#77320,#77321,#77322,
#77323,#77324,#77325,#77326),.UNSPECIFIED.,.F.,.F.,(6,3,6),(0.,2.6134611976,
3.73613338933),.UNSPECIFIED.);
#1745=B_SPLINE_CURVE_WITH_KNOTS('',5,(#77341,#77342,#77343,#77344,#77345,
#77346),.UNSPECIFIED.,.F.,.F.,(6,6),(0.,1.1155886229),.UNSPECIFIED.);
#1746=B_SPLINE_CURVE_WITH_KNOTS('',5,(#77379,#77380,#77381,#77382,#77383,
#77384,#77385,#77386,#77387,#77388,#77389,#77390,#77391,#77392,#77393),
 .UNSPECIFIED.,.F.,.F.,(6,3,3,3,6),(0.,1.14196741734,1.69664449439,2.26600465298,
2.82383165251),.UNSPECIFIED.);
#1747=B_SPLINE_CURVE_WITH_KNOTS('',5,(#77407,#77408,#77409,#77410,#77411,
#77412),.UNSPECIFIED.,.F.,.F.,(6,6),(0.,2.29845936737),.UNSPECIFIED.);
#1748=B_SPLINE_CURVE_WITH_KNOTS('',5,(#77445,#77446,#77447,#77448,#77449,
#77450,#77451,#77452,#77453,#77454,#77455,#77456,#77457,#77458,#77459),
 .UNSPECIFIED.,.F.,.F.,(6,3,3,3,6),(1.73726460462955E-9,6.696077534,12.6191089245,
16.7682744334,17.9215041098),.UNSPECIFIED.);
#1749=B_SPLINE_CURVE_WITH_KNOTS('',5,(#77503,#77504,#77505,#77506,#77507,
#77508,#77509,#77510,#77511,#77512,#77513,#77514,#77515,#77516,#77517),
 .UNSPECIFIED.,.F.,.F.,(6,3,3,3,6),(1.73726460462955E-9,6.696077534,12.6191089245,
16.7682744334,17.9215041098),.UNSPECIFIED.);
#1750=B_SPLINE_CURVE_WITH_KNOTS('',5,(#77540,#77541,#77542,#77543,#77544,
#77545,#77546,#77547,#77548),.UNSPECIFIED.,.F.,.F.,(6,3,6),(0.,0.699509606660128,
1.),.UNSPECIFIED.);
#1751=B_SPLINE_CURVE_WITH_KNOTS('',5,(#77590,#77591,#77592,#77593,#77594,
#77595,#77596,#77597,#77598,#77599,#77600,#77601),.UNSPECIFIED.,.F.,.F.,
(6,3,3,6),(0.,0.405469991881924,0.798069831416645,1.),.UNSPECIFIED.);
#1752=B_SPLINE_CURVE_WITH_KNOTS('',5,(#77616,#77617,#77618,#77619,#77620,
#77621),.UNSPECIFIED.,.F.,.F.,(6,6),(0.,2.29845936737),.UNSPECIFIED.);
#1753=B_SPLINE_CURVE_WITH_KNOTS('',5,(#77654,#77655,#77656,#77657,#77658,
#77659,#77660,#77661,#77662,#77663,#77664,#77665,#77666,#77667,#77668),
 .UNSPECIFIED.,.F.,.F.,(6,3,3,3,6),(0.,0.404403504835335,0.600830610026598,
0.80245741666853,1.),.UNSPECIFIED.);
#1754=B_SPLINE_CURVE_WITH_KNOTS('',5,(#77682,#77683,#77684,#77685,#77686,
#77687),.UNSPECIFIED.,.F.,.F.,(6,6),(0.,1.1155886229),.UNSPECIFIED.);
#1755=B_SPLINE_CURVE_WITH_KNOTS('',5,(#77721,#77722,#77723,#77724,#77725,
#77726,#77727,#77728,#77729,#77730,#77731,#77732,#77733,#77734,#77735),
 .UNSPECIFIED.,.F.,.F.,(6,3,3,3,6),(0.,0.227429357973136,0.467550165133747,
0.685913432634515,1.),.UNSPECIFIED.);
#1756=B_SPLINE_CURVE_WITH_KNOTS('',5,(#77750,#77751,#77752,#77753,#77754,
#77755),.UNSPECIFIED.,.F.,.F.,(6,6),(0.,1.),.UNSPECIFIED.);
#1757=B_SPLINE_CURVE_WITH_KNOTS('',5,(#77808,#77809,#77810,#77811,#77812,
#77813,#77814,#77815,#77816,#77817,#77818,#77819,#77820,#77821,#77822),
 .UNSPECIFIED.,.F.,.F.,(6,3,3,3,6),(0.0395158293388482,7.53253625942,14.2747183071,
18.8083875826,22.71906151),.UNSPECIFIED.);
#1758=B_SPLINE_CURVE_WITH_KNOTS('',5,(#77842,#77843,#77844,#77845,#77846,
#77847,#77848,#77849,#77850),.UNSPECIFIED.,.F.,.F.,(6,3,6),(1.18944404077E-12,
1.10170421198,3.01229896543),.UNSPECIFIED.);
#1759=B_SPLINE_CURVE_WITH_KNOTS('',5,(#78000,#78001,#78002,#78003,#78004,
#78005),.UNSPECIFIED.,.F.,.F.,(6,6),(0.,6.43612007405),.UNSPECIFIED.);
#1760=B_SPLINE_CURVE_WITH_KNOTS('',5,(#78038,#78039,#78040,#78041,#78042,
#78043,#78044,#78045,#78046,#78047,#78048,#78049,#78050,#78051,#78052),
 .UNSPECIFIED.,.F.,.F.,(6,3,3,3,6),(0.,1.06902836413,2.19771269917,3.2241260379,
4.7004853448),.UNSPECIFIED.);
#1761=B_SPLINE_CURVE_WITH_KNOTS('',5,(#78073,#78074,#78075,#78076,#78077,
#78078,#78079,#78080,#78081),.UNSPECIFIED.,.F.,.F.,(6,3,6),(0.,0.365735348523741,
1.),.UNSPECIFIED.);
#1762=B_SPLINE_CURVE_WITH_KNOTS('',5,(#78113,#78114,#78115,#78116,#78117,
#78118,#78119,#78120,#78121,#78122,#78123,#78124,#78125,#78126,#78127),
 .UNSPECIFIED.,.F.,.F.,(6,3,3,3,6),(0.0395158293387482,7.53253625942,14.2747183071,
18.8083875826,22.71906151),.UNSPECIFIED.);
#1763=B_SPLINE_CURVE_WITH_KNOTS('',5,(#78627,#78628,#78629,#78630,#78631,
#78632),.UNSPECIFIED.,.F.,.F.,(6,6),(0.226923016970762,1.),
 .UNSPECIFIED.);
#1764=B_SPLINE_CURVE_WITH_KNOTS('',3,(#78640,#78641,#78642,#78643,#78644,
#78645),.UNSPECIFIED.,.F.,.F.,(4,2,4),(0.226811293541348,0.613405646770674,
1.),.UNSPECIFIED.);
#1765=B_SPLINE_CURVE_WITH_KNOTS('',3,(#78678,#78679,#78680,#78681,#78682,
#78683),.UNSPECIFIED.,.F.,.F.,(4,2,4),(0.197042714657638,0.598521357328819,
1.),.UNSPECIFIED.);
#1766=B_SPLINE_CURVE_WITH_KNOTS('',3,(#78696,#78697,#78698,#78699,#78700,
#78701),.UNSPECIFIED.,.F.,.F.,(4,2,4),(0.226811293549919,0.61340564677496,
1.),.UNSPECIFIED.);
#1767=B_SPLINE_CURVE_WITH_KNOTS('',5,(#78705,#78706,#78707,#78708,#78709,
#78710),.UNSPECIFIED.,.F.,.F.,(6,6),(0.226923156363992,1.),
 .UNSPECIFIED.);
#1768=B_SPLINE_CURVE_WITH_KNOTS('',5,(#78719,#78720,#78721,#78722,#78723,
#78724),.UNSPECIFIED.,.F.,.F.,(6,6),(0.,1.),.UNSPECIFIED.);
#1769=B_SPLINE_CURVE_WITH_KNOTS('',3,(#78728,#78729,#78730,#78731,#78732,
#78733,#78734,#78735,#78736,#78737,#78738,#78739,#78740,#78741,#78742,#78743,
#78744,#78745,#78746,#78747,#78748,#78749,#78750,#78751,#78752,#78753,#78754,
#78755,#78756,#78757,#78758,#78759,#78760,#78761,#78762,#78763,#78764,#78765,
#78766,#78767,#78768,#78769,#78770,#78771,#78772,#78773,#78774,#78775,#78776,
#78777,#78778,#78779,#78780,#78781,#78782,#78783,#78784,#78785,#78786,#78787,
#78788,#78789,#78790,#78791,#78792,#78793,#78794,#78795,#78796,#78797,#78798,
#78799,#78800,#78801,#78802,#78803,#78804,#78805,#78806,#78807,#78808,#78809,
#78810,#78811,#78812,#78813,#78814,#78815,#78816,#78817,#78818,#78819,#78820,
#78821,#78822,#78823,#78824,#78825,#78826,#78827,#78828,#78829,#78830,#78831,
#78832,#78833,#78834,#78835,#78836,#78837,#78838,#78839,#78840,#78841,#78842,
#78843,#78844,#78845,#78846,#78847,#78848,#78849,#78850,#78851,#78852,#78853,
#78854,#78855,#78856,#78857,#78858,#78859,#78860,#78861,#78862,#78863,#78864,
#78865,#78866,#78867,#78868,#78869,#78870,#78871,#78872,#78873,#78874,#78875,
#78876,#78877,#78878,#78879,#78880,#78881,#78882,#78883,#78884,#78885,#78886,
#78887,#78888,#78889,#78890,#78891,#78892,#78893,#78894,#78895,#78896,#78897,
#78898,#78899,#78900,#78901,#78902,#78903,#78904,#78905,#78906,#78907,#78908,
#78909,#78910,#78911,#78912,#78913,#78914,#78915,#78916,#78917,#78918,#78919,
#78920,#78921,#78922,#78923,#78924,#78925,#78926,#78927,#78928,#78929,#78930,
#78931,#78932,#78933,#78934,#78935,#78936,#78937,#78938,#78939,#78940,#78941,
#78942,#78943,#78944,#78945,#78946,#78947),.UNSPECIFIED.,.F.,.F.,(4,3,3,
3,3,3,3,3,3,3,3,3,3,3,3,3,3,3,3,3,3,3,3,3,3,3,3,3,3,3,3,3,3,3,3,3,3,3,3,
3,3,3,3,3,3,3,3,3,3,3,3,3,3,3,3,3,3,3,3,3,3,3,3,3,3,3,3,3,3,3,3,3,3,4),
(0.0868385867057379,0.0937499999999956,0.109374999999995,0.117187499999994,
0.121093749999994,0.123046874999994,0.124023437499994,0.124999999999994,
0.145934913493643,0.167462598467453,0.187499999999996,0.209872497695248,
0.218749999999997,0.234374999999997,0.242187499999998,0.246093749999998,
0.248046874999998,0.249023437499998,0.249999999999998,0.272528330630081,
0.29564318505803,0.312499999999998,0.336432597942232,0.343749999999998,
0.359374999999998,0.367187499999998,0.371093749999998,0.373046874999998,
0.374851354279564,0.374999999999998,0.398493781362424,0.406249999999999,
0.421874999999999,0.429687499999999,0.433593749999999,0.436607414249363,
0.437499999999999,0.461739947182365,0.468749999999999,0.484374999999999,
0.492187499999999,0.497333394583601,0.499999999999998,0.525206949984025,
0.551256701035308,0.562499999999999,0.591346920143275,0.593749999999999,
0.609375,0.6171875,0.622302819166279,0.625,0.65625,0.6875,0.716247216753145,
0.71875,0.734375,0.7421875,0.747756676868899,0.75,0.778803250902111,0.78125,
0.798733322246778,0.8125,0.840832577832501,0.84375,0.859375,0.868597898855189,
0.875,0.903754289572031,0.93251341058128,0.961094429961356,0.989185606847336,
1.),.UNSPECIFIED.);
#1770=B_SPLINE_CURVE_WITH_KNOTS('',3,(#78949,#78950,#78951,#78952,#78953,
#78954,#78955,#78956,#78957,#78958,#78959,#78960,#78961,#78962,#78963,#78964,
#78965,#78966,#78967,#78968,#78969,#78970,#78971,#78972,#78973,#78974,#78975,
#78976,#78977,#78978,#78979,#78980,#78981,#78982,#78983,#78984,#78985,#78986,
#78987,#78988,#78989,#78990,#78991),.UNSPECIFIED.,.F.,.F.,(4,3,3,3,3,3,
3,3,3,3,3,3,3,3,4),(0.,0.00951856234533963,0.0190261223058877,0.0285057566012048,
0.0312499999999986,0.0406555969248241,0.0468749999999981,0.0546874999999978,
0.0585937499999976,0.0605468749999976,0.0615234374999975,0.0624213299799009,
0.0624999999999974,0.0778317290989469,0.0868385867057379),.UNSPECIFIED.);
#1771=B_SPLINE_CURVE_WITH_KNOTS('',3,(#79000,#79001,#79002,#79003,#79004,
#79005,#79006,#79007,#79008,#79009,#79010,#79011,#79012,#79013,#79014,#79015,
#79016,#79017,#79018,#79019,#79020,#79021,#79022,#79023,#79024,#79025,#79026,
#79027,#79028,#79029,#79030,#79031,#79032,#79033,#79034,#79035,#79036,#79037,
#79038,#79039,#79040,#79041,#79042,#79043,#79044,#79045,#79046,#79047,#79048,
#79049,#79050,#79051,#79052,#79053,#79054,#79055,#79056,#79057,#79058,#79059,
#79060,#79061,#79062,#79063,#79064,#79065,#79066),.UNSPECIFIED.,.F.,.F.,
(4,3,3,3,3,3,3,3,3,3,3,3,3,3,3,3,3,3,3,3,3,3,4),(0.,0.0967186461262831,
0.12500000000004,0.18750000000006,0.21875000000007,0.234375000000064,0.243656743286663,
0.250000000000058,0.304783310397428,0.358759691292195,0.375000000000016,
0.42752541592923,0.437500000000005,0.468750000000006,0.483401950931687,
0.498680111726324,0.500000000000007,0.585314944032889,0.673616873479213,
0.766999996706054,0.86351900109437,0.96497775590487,1.),.UNSPECIFIED.);
#1772=B_SPLINE_CURVE_WITH_KNOTS('',3,(#79069,#79070,#79071,#79072,#79073,
#79074,#79075,#79076,#79077,#79078,#79079,#79080,#79081,#79082,#79083,#79084,
#79085,#79086,#79087,#79088,#79089,#79090,#79091,#79092,#79093,#79094,#79095,
#79096,#79097,#79098,#79099,#79100,#79101,#79102,#79103,#79104,#79105,#79106,
#79107,#79108,#79109,#79110,#79111,#79112,#79113,#79114,#79115,#79116,#79117,
#79118,#79119,#79120,#79121,#79122,#79123,#79124,#79125,#79126,#79127,#79128,
#79129,#79130,#79131,#79132,#79133,#79134,#79135),.UNSPECIFIED.,.F.,.F.,
(4,3,3,3,3,3,3,3,3,3,3,3,3,3,3,3,3,3,3,3,3,3,4),(0.,0.100757444409959,0.196147984514473,
0.249999999999972,0.340191959854596,0.374999999999954,0.437499999999945,
0.468749999999941,0.484374999999938,0.498793165549547,0.499999999999936,
0.550373236664276,0.602950842746076,0.624999999999946,0.678928159561804,
0.687499999999961,0.718749999999969,0.734374999999973,0.742187499999975,
0.749999999999977,0.841743474586641,0.938196398372317,1.),.UNSPECIFIED.);
#1773=B_SPLINE_CURVE_WITH_KNOTS('',3,(#79143,#79144,#79145,#79146,#79147,
#79148,#79149,#79150,#79151,#79152,#79153,#79154,#79155,#79156,#79157,#79158,
#79159,#79160,#79161,#79162,#79163,#79164),.UNSPECIFIED.,.F.,.F.,(4,3,3,
3,3,3,3,4),(1.91917304179,2.05149792398005,2.18491877151797,2.22039294838,
2.3639360580223,2.50932327973008,2.52698484563,2.64214133457),
 .UNSPECIFIED.);
#1774=B_SPLINE_CURVE_WITH_KNOTS('',3,(#79166,#79167,#79168,#79169,#79170,
#79171,#79172,#79173,#79174,#79175,#79176,#79177,#79178,#79179,#79180,#79181,
#79182,#79183,#79184),.UNSPECIFIED.,.F.,.F.,(4,3,3,3,3,3,4),(1.95117092983,
2.10540845651,2.25964598319,2.39637208287195,2.53179243110294,2.56487158268,
2.67415250918),.UNSPECIFIED.);
#1775=B_SPLINE_CURVE_WITH_KNOTS('',3,(#79230,#79231,#79232,#79233,#79234,
#79235,#79236,#79237,#79238,#79239,#79240,#79241,#79242,#79243,#79244,#79245,
#79246,#79247,#79248,#79249,#79250,#79251),.UNSPECIFIED.,.F.,.F.,(4,3,3,
3,3,3,3,4),(1.91917304179,2.02579232441727,2.13535045929516,2.24802429461472,
2.36515236413743,2.48418559772032,2.60408580572557,2.64214133457),
 .UNSPECIFIED.);
#1776=B_SPLINE_CURVE_WITH_KNOTS('',3,(#79255,#79256,#79257,#79258,#79259,
#79260,#79261,#79262,#79263,#79264,#79265,#79266,#79267,#79268,#79269,#79270,
#79271,#79272,#79273,#79274,#79275,#79276,#79277,#79278,#79279,#79280,#79281,
#79282,#79283,#79284,#79285,#79286,#79287,#79288,#79289,#79290,#79291,#79292,
#79293,#79294,#79295,#79296,#79297,#79298,#79299,#79300,#79301,#79302,#79303,
#79304,#79305,#79306,#79307,#79308,#79309,#79310,#79311,#79312,#79313,#79314,
#79315,#79316,#79317,#79318,#79319,#79320,#79321,#79322,#79323,#79324,#79325,
#79326,#79327,#79328,#79329,#79330,#79331,#79332,#79333,#79334,#79335,#79336,
#79337,#79338,#79339,#79340,#79341,#79342,#79343,#79344,#79345,#79346,#79347,
#79348,#79349,#79350,#79351),.UNSPECIFIED.,.F.,.F.,(4,3,3,3,3,3,3,3,3,3,
3,3,3,3,3,3,3,3,3,3,3,3,3,3,3,3,3,3,3,3,3,3,4),(4.0025111321083E-13,0.0632489107248744,
0.125000000000003,0.187500000000005,0.218750000000006,0.235672573927374,
0.250000000000007,0.3073632326897,0.363175963289869,0.37500000000001,0.429360664035595,
0.437500000000012,0.468750000000012,0.484375000000012,0.492187500000013,
0.497903776612221,0.500000000000013,0.554907532207408,0.608404879582191,
0.625000000000013,0.676344675408734,0.687500000000013,0.718750000000014,
0.734375000000014,0.742187500000014,0.746093750000014,0.749653402950428,
0.750000000000014,0.808127914628195,0.864545740498736,0.920016589838173,
0.974147928007887,0.99999998552153),.UNSPECIFIED.);
#1777=B_SPLINE_CURVE_WITH_KNOTS('',3,(#79354,#79355,#79356,#79357,#79358,
#79359,#79360,#79361,#79362,#79363,#79364,#79365,#79366,#79367,#79368,#79369,
#79370,#79371,#79372,#79373,#79374,#79375),.UNSPECIFIED.,.F.,.F.,(4,3,3,
3,3,3,3,4),(1.95117092983,2.07121338925534,2.1903352130963,2.31128953711722,
2.42369300779211,2.53345239947667,2.6396571157376,2.67415250918),
 .UNSPECIFIED.);
#1778=B_SPLINE_CURVE_WITH_KNOTS('',5,(#79383,#79384,#79385,#79386,#79387,
#79388,#79389,#79390,#79391),.UNSPECIFIED.,.F.,.F.,(6,3,6),(0.,0.444536926591004,
1.),.UNSPECIFIED.);
#1779=B_SPLINE_CURVE_WITH_KNOTS('',5,(#79394,#79395,#79396,#79397,#79398,
#79399,#79400,#79401,#79402,#79403,#79404,#79405),.UNSPECIFIED.,.F.,.F.,
(6,3,3,6),(-1.80699050239119,-1.67012369382,-1.56537299057,-1.54695248492),
 .UNSPECIFIED.);
#1780=B_SPLINE_CURVE_WITH_KNOTS('',3,(#79407,#79408,#79409,#79410,#79411,
#79412,#79413,#79414,#79415,#79416,#79417,#79418,#79419,#79420,#79421,#79422,
#79423,#79424,#79425,#79426,#79427,#79428),.UNSPECIFIED.,.F.,.F.,(4,3,3,
3,3,3,3,4),(-4.36798756241,-4.169936044415,-3.99462490463767,-3.97188452642,
-3.81611914244834,-3.6712886258062,-3.62984805881,-3.53583307557),
 .UNSPECIFIED.);
#1781=B_SPLINE_CURVE_WITH_KNOTS('',3,(#79433,#79434,#79435,#79436,#79437,
#79438,#79439,#79440,#79441,#79442,#79443,#79444,#79445,#79446,#79447,#79448,
#79449,#79450,#79451,#79452,#79453,#79454,#79455,#79456,#79457,#79458,#79459,
#79460,#79461,#79462,#79463,#79464,#79465,#79466,#79467,#79468,#79469,#79470,
#79471,#79472,#79473,#79474,#79475),.UNSPECIFIED.,.F.,.F.,(4,3,3,3,3,3,
3,3,3,3,3,3,3,3,4),(-2.1197288877,-1.98841331521492,-1.86159678165,-1.7188993737364,
-1.60356346906,-1.44037681505088,-1.3668875221,-1.17788035732586,-1.13023412606,
-0.922050724180072,-0.709993980015713,-0.657118805891,-0.442216022332552,
-0.328557428358,-0.109166698395),.UNSPECIFIED.);
#1782=B_SPLINE_CURVE_WITH_KNOTS('',3,(#79477,#79478,#79479,#79480,#79481,
#79482,#79483,#79484,#79485,#79486,#79487,#79488,#79489,#79490,#79491,#79492,
#79493,#79494,#79495,#79496,#79497,#79498,#79499,#79500,#79501),
 .UNSPECIFIED.,.F.,.F.,(4,3,3,3,3,3,3,3,4),(-1.73791866609,-1.69805976489305,
-1.65573758388662,-1.61550378495,-1.56701234941871,-1.51549851525847,-1.49803365755,
-1.45023151716658,-1.40796354572),.UNSPECIFIED.);
#1783=B_SPLINE_CURVE_WITH_KNOTS('',3,(#79504,#79505,#79506,#79507,#79508,
#79509,#79510,#79511,#79512,#79513,#79514,#79515,#79516,#79517,#79518,#79519,
#79520,#79521,#79522,#79523,#79524,#79525,#79526,#79527,#79528,#79529,#79530,
#79531,#79532,#79533,#79534,#79535,#79536,#79537,#79538,#79539,#79540,#79541,
#79542,#79543,#79544,#79545,#79546),.UNSPECIFIED.,.F.,.F.,(4,3,3,3,3,3,
3,3,3,3,3,3,3,3,4),(-3.16496476901,-3.05739501013341,-2.95490927595688,
-2.89022619818,-2.80130651793357,-2.71899621993714,-2.64235434316,-2.57577600227824,
-2.53314284706,-2.46341560037499,-2.42388273879,-2.35998782232,-2.29609290585,
-2.23666406729655,-2.21471914028),.UNSPECIFIED.);
#1784=B_SPLINE_CURVE_WITH_KNOTS('',3,(#79548,#79549,#79550,#79551,#79552,
#79553,#79554,#79555,#79556,#79557,#79558,#79559,#79560,#79561,#79562,#79563,
#79564,#79565,#79566,#79567,#79568,#79569,#79570,#79571,#79572,#79573,#79574,
#79575,#79576,#79577,#79578,#79579,#79580,#79581,#79582,#79583,#79584,#79585,
#79586,#79587),.UNSPECIFIED.,.F.,.F.,(4,3,3,3,3,3,3,3,3,3,3,3,3,4),(-3.15494946668974,
-3.09429422325597,-3.03469546375,-2.97101336920453,-2.90283799032044,-2.84788436267,
-2.77508951699777,-2.70623933891542,-2.64437519712,-2.56234040630418,-2.47134155465,
-2.36779504868473,-2.29839214685,-2.20468603571421),.UNSPECIFIED.);
#1785=B_SPLINE_CURVE_WITH_KNOTS('',3,(#79590,#79591,#79592,#79593,#79594,
#79595,#79596,#79597,#79598,#79599,#79600,#79601,#79602,#79603,#79604,#79605,
#79606,#79607,#79608,#79609,#79610,#79611,#79612,#79613,#79614,#79615,#79616,
#79617),.UNSPECIFIED.,.F.,.F.,(4,3,3,3,3,3,3,3,3,4),(-1.77221556182,-1.72541256452829,
-1.67470799810622,-1.63241886503,-1.58516494184952,-1.55011502341,-1.50856575067229,
-1.49939588111,-1.45848471590269,-1.44228974252),.UNSPECIFIED.);
#1786=B_SPLINE_CURVE_WITH_KNOTS('',3,(#79619,#79620,#79621,#79622,#79623,
#79624,#79625,#79626,#79627,#79628,#79629,#79630,#79631,#79632,#79633,#79634,
#79635,#79636,#79637,#79638,#79639,#79640,#79641,#79642,#79643,#79644,#79645,
#79646,#79647,#79648,#79649,#79650,#79651,#79652,#79653,#79654,#79655,#79656,
#79657,#79658),.UNSPECIFIED.,.F.,.F.,(4,3,3,3,3,3,3,3,3,3,3,3,3,4),(-5.02326603963,
-4.80637580757057,-4.59184582783107,-4.46470265851,-4.25520068526698,-4.05094564988226,
-3.90600477275,-3.72858936815271,-3.56430826698,-3.41556843081671,-3.27772290795148,
-3.22245900472,-3.09341777853601,-3.01269951131),.UNSPECIFIED.);
#1787=B_SPLINE_CURVE_WITH_KNOTS('',3,(#79663,#79664,#79665,#79666,#79667,
#79668,#79669,#79670,#79671,#79672,#79673,#79674,#79675,#79676,#79677,#79678,
#79679,#79680,#79681,#79682,#79683,#79684),.UNSPECIFIED.,.F.,.F.,(4,3,3,
3,3,3,3,4),(-7.33762762903,-7.19451398421356,-7.08790984155,-6.92735535556756,
-6.82008855637394,-6.62897001935503,-6.58881135386,-6.50557700429),
 .UNSPECIFIED.);
#1788=B_SPLINE_CURVE_WITH_KNOTS('',5,(#79686,#79687,#79688,#79689,#79690,
#79691,#79692,#79693,#79694,#79695,#79696,#79697),.UNSPECIFIED.,.F.,.F.,
(6,3,3,6),(-1.75479504935,-1.62859651807,-1.50635582191,-1.4947188012),
 .UNSPECIFIED.);
#1789=B_SPLINE_CURVE_WITH_KNOTS('',5,(#79700,#79701,#79702,#79703,#79704,
#79705,#79706,#79707,#79708),.UNSPECIFIED.,.F.,.F.,(6,3,6),(3.35057951372198E-8,
0.468594524318655,1.),.UNSPECIFIED.);
#1790=B_SPLINE_CURVE_WITH_KNOTS('',5,(#79823,#79824,#79825,#79826,#79827,
#79828,#79829,#79830,#79831),.UNSPECIFIED.,.F.,.F.,(6,3,6),(-6.00042817873,
-5.42884095166,-5.20521075808),.UNSPECIFIED.);
#1791=B_SPLINE_CURVE_WITH_KNOTS('',3,(#79833,#79834,#79835,#79836,#79837,
#79838,#79839,#79840,#79841,#79842,#79843,#79844,#79845,#79846,#79847,#79848,
#79849,#79850,#79851,#79852,#79853,#79854,#79855,#79856,#79857),
 .UNSPECIFIED.,.F.,.F.,(4,3,3,3,3,3,3,3,4),(0.,0.125,0.249051326604059,
0.37312891753387,0.497226955279358,0.622920216459519,0.747043580627599,
0.873521790313799,1.),.UNSPECIFIED.);
#1792=B_SPLINE_CURVE_WITH_KNOTS('',5,(#79859,#79860,#79861,#79862,#79863,
#79864,#79865,#79866,#79867),.UNSPECIFIED.,.F.,.F.,(6,3,6),(1.9878298196,
2.20723764364,2.53578324996),.UNSPECIFIED.);
#1793=B_SPLINE_CURVE_WITH_KNOTS('',5,(#79869,#79870,#79871,#79872,#79873,
#79874),.UNSPECIFIED.,.F.,.F.,(6,6),(5.20484021909,5.76063633602),
 .UNSPECIFIED.);
#1794=B_SPLINE_CURVE_WITH_KNOTS('',3,(#79886,#79887,#79888,#79889,#79890,
#79891,#79892,#79893,#79894,#79895,#79896,#79897,#79898,#79899,#79900,#79901,
#79902,#79903,#79904,#79905,#79906,#79907,#79908,#79909,#79910,#79911,#79912,
#79913,#79914,#79915,#79916,#79917,#79918,#79919,#79920,#79921,#79922),
 .UNSPECIFIED.,.F.,.F.,(4,3,3,3,3,3,3,3,3,3,3,3,4),(1.62679171178,1.80119189921,
2.06549727040562,2.33022193180684,2.59511005010776,2.8601162004504,2.9864917,
3.25107716364615,3.51563595035349,3.56612301471,3.83086251970706,4.09597227277403,
4.14575432942),.UNSPECIFIED.);
#1795=B_SPLINE_CURVE_WITH_KNOTS('',3,(#80019,#80020,#80021,#80022,#80023,
#80024,#80025,#80026,#80027,#80028),.UNSPECIFIED.,.F.,.F.,(4,3,3,4),(-6.00042817873,
-5.73764962787167,-5.47143019297584,-5.20521075808),.UNSPECIFIED.);
#1796=B_SPLINE_CURVE_WITH_KNOTS('',3,(#80031,#80032,#80033,#80034,#80035,
#80036,#80037,#80038,#80039,#80040,#80041,#80042,#80043,#80044,#80045,#80046,
#80047,#80048,#80049,#80050,#80051,#80052,#80053,#80054,#80055,#80056,#80057,
#80058,#80059,#80060,#80061,#80062,#80063,#80064,#80065,#80066,#80067,#80068,
#80069,#80070,#80071,#80072,#80073,#80074,#80075,#80076,#80077,#80078,#80079,
#80080,#80081,#80082,#80083,#80084,#80085),.UNSPECIFIED.,.F.,.F.,(4,3,3,
3,3,3,3,3,3,3,3,3,3,3,3,3,3,3,4),(-4.71575303852,-4.65907697863314,-4.59837909975905,
-4.56620180037,-4.49782940088838,-4.45572366868,-4.37891278786157,-4.34130806771,
-4.27463577302459,-4.21375904184622,-4.18701109461,-4.10530819905221,-4.019523415627,
-3.96784558239,-3.87773712401142,-3.78337627560873,-3.75420974096,-3.65160927305,
-3.54900880514),.UNSPECIFIED.);
#1797=B_SPLINE_CURVE_WITH_KNOTS('',5,(#80132,#80133,#80134,#80135,#80136,
#80137),.UNSPECIFIED.,.F.,.F.,(6,6),(5.20484021909,5.76063633602),
 .UNSPECIFIED.);
#1798=B_SPLINE_CURVE_WITH_KNOTS('',3,(#80175,#80176,#80177,#80178,#80179,
#80180,#80181,#80182,#80183,#80184,#80185,#80186,#80187),.UNSPECIFIED.,
 .F.,.F.,(4,3,3,3,4),(0.,0.253975090744685,0.502216732464109,0.751108366232054,
1.),.UNSPECIFIED.);
#1799=B_SPLINE_CURVE_WITH_KNOTS('',5,(#80199,#80200,#80201,#80202,#80203,
#80204,#80205,#80206,#80207),.UNSPECIFIED.,.F.,.F.,(6,3,6),(0.,0.546822749333166,
1.),.UNSPECIFIED.);
#1800=B_SPLINE_CURVE_WITH_KNOTS('',5,(#80225,#80226,#80227,#80228,#80229,
#80230,#80231,#80232,#80233),.UNSPECIFIED.,.F.,.F.,(6,3,6),(0.,0.45317725066295,
1.),.UNSPECIFIED.);
#1801=B_SPLINE_CURVE_WITH_KNOTS('',3,(#80348,#80349,#80350,#80351,#80352,
#80353,#80354,#80355,#80356,#80357,#80358,#80359,#80360,#80361,#80362,#80363,
#80364,#80365,#80366,#80367,#80368,#80369,#80370,#80371,#80372,#80373,#80374,
#80375,#80376,#80377,#80378,#80379,#80380,#80381,#80382,#80383,#80384,#80385,
#80386,#80387,#80388,#80389,#80390,#80391,#80392,#80393,#80394,#80395,#80396,
#80397,#80398,#80399,#80400,#80401,#80402),.UNSPECIFIED.,.F.,.F.,(4,3,3,
3,3,3,3,3,3,3,3,3,3,3,3,3,3,3,4),(3.54900880515,3.651609273055,3.75420974096,
3.84893307386556,3.93929532064981,3.96784558239,4.05430391724671,4.13645477350633,
4.18701109461,4.24753706288369,4.31344142163189,4.34130806771,4.41811894852724,
4.45572366868,4.52409606816139,4.56620180037,4.62755792701915,4.68459440694729,
4.71575303852),.UNSPECIFIED.);
#1802=B_SPLINE_CURVE_WITH_KNOTS('',5,(#80754,#80755,#80756,#80757,#80758,
#80759),.UNSPECIFIED.,.F.,.F.,(6,6),(3.1859449136978E-8,1.),
 .UNSPECIFIED.);
#1803=B_SPLINE_CURVE_WITH_KNOTS('',3,(#80765,#80766,#80767,#80768,#80769,
#80770,#80771,#80772,#80773,#80774),.UNSPECIFIED.,.F.,.F.,(4,2,2,2,4),(0.,
0.25,0.5,0.75,1.),.UNSPECIFIED.);
#1804=B_SPLINE_CURVE_WITH_KNOTS('',3,(#80792,#80793,#80794,#80795,#80796,
#80797,#80798,#80799,#80800,#80801,#80802,#80803,#80804,#80805,#80806,#80807,
#80808,#80809,#80810,#80811,#80812,#80813,#80814,#80815,#80816,#80817,#80818,
#80819,#80820,#80821,#80822),.UNSPECIFIED.,.F.,.F.,(4,3,3,3,3,3,3,3,3,3,
4),(0.,0.103486941292664,0.209722140116913,0.317273808041208,0.426249484256839,
0.5,0.609150430624086,0.71686238797799,0.823269317845894,0.927288353897733,
1.),.UNSPECIFIED.);
#1805=B_SPLINE_CURVE_WITH_KNOTS('',3,(#80864,#80865,#80866,#80867,#80868,
#80869,#80870,#80871,#80872,#80873,#80874,#80875,#80876),.UNSPECIFIED.,
 .F.,.F.,(4,3,3,3,4),(0.,0.283655470482566,0.567100173465966,0.871696373072702,
1.),.UNSPECIFIED.);
#1806=B_SPLINE_CURVE_WITH_KNOTS('',3,(#80988,#80989,#80990,#80991,#80992,
#80993,#80994,#80995,#80996,#80997,#80998,#80999,#81000,#81001,#81002,#81003,
#81004,#81005,#81006,#81007,#81008,#81009,#81010,#81011,#81012,#81013,#81014,
#81015,#81016,#81017,#81018,#81019,#81020,#81021,#81022,#81023,#81024,#81025,
#81026,#81027,#81028,#81029,#81030,#81031,#81032,#81033,#81034,#81035,#81036,
#81037,#81038,#81039,#81040,#81041,#81042,#81043,#81044,#81045,#81046,#81047,
#81048,#81049,#81050,#81051,#81052,#81053,#81054,#81055,#81056,#81057,#81058,
#81059,#81060,#81061,#81062,#81063,#81064,#81065,#81066),.UNSPECIFIED.,
 .F.,.F.,(4,3,3,3,3,3,3,3,3,3,3,3,3,3,3,3,3,3,3,3,3,3,3,3,3,3,4),(0.,0.0787260457931564,
0.124999999999993,0.187499999999992,0.218749999999992,0.247757967308853,
0.249999999999991,0.331434298157057,0.37499999999999,0.449421300548547,
0.466731041768843,0.483365520884418,0.485303339327099,0.495778997034871,
0.499999999999993,0.548146868097096,0.624999999999991,0.687499999999989,
0.718749999999989,0.734374999999988,0.742936082500893,0.749999999999988,
0.816779350141409,0.883437797437894,0.937634632232333,0.984782267543852,
1.),.UNSPECIFIED.);
#1807=B_SPLINE_CURVE_WITH_KNOTS('',3,(#81150,#81151,#81152,#81153,#81154,
#81155,#81156,#81157,#81158,#81159,#81160,#81161,#81162,#81163,#81164,#81165,
#81166,#81167,#81168,#81169,#81170,#81171,#81172,#81173,#81174,#81175,#81176,
#81177,#81178,#81179,#81180,#81181,#81182,#81183,#81184,#81185,#81186,#81187,
#81188,#81189,#81190,#81191,#81192,#81193,#81194,#81195,#81196,#81197,#81198,
#81199,#81200,#81201,#81202,#81203,#81204,#81205,#81206,#81207,#81208,#81209,
#81210,#81211,#81212,#81213,#81214,#81215,#81216,#81217,#81218,#81219,#81220,
#81221,#81222,#81223,#81224,#81225,#81226,#81227,#81228,#81229,#81230,#81231,
#81232,#81233,#81234,#81235,#81236,#81237),.UNSPECIFIED.,.F.,.F.,(4,3,3,
3,3,3,3,3,3,3,3,3,3,3,3,3,3,3,3,3,3,3,3,3,3,3,3,3,3,4),(0.,0.0468087724836094,
0.100006845757394,0.135651264268524,0.192825632134262,0.221412816067131,
0.228559612050348,0.233919709037761,0.235289363314821,0.243650512143623,
0.25,0.31592266226525,0.374999999999993,0.425566231049382,0.43749999999999,
0.451681239474872,0.468749999999989,0.484374999999988,0.493507364861486,
0.499999999999987,0.578683814801776,0.624999999999991,0.687499999999992,
0.718749999999993,0.734374999999993,0.745475655325922,0.749999999999993,
0.861453741249095,0.944849601132576,1.),.UNSPECIFIED.);
#1808=B_SPLINE_CURVE_WITH_KNOTS('',3,(#81297,#81298,#81299,#81300,#81301,
#81302,#81303,#81304,#81305,#81306,#81307,#81308,#81309,#81310,#81311,#81312,
#81313,#81314,#81315,#81316,#81317,#81318,#81319,#81320,#81321,#81322,#81323,
#81324,#81325,#81326,#81327,#81328,#81329,#81330,#81331,#81332,#81333,#81334,
#81335,#81336,#81337,#81338,#81339,#81340,#81341,#81342,#81343,#81344,#81345,
#81346,#81347,#81348,#81349,#81350,#81351,#81352,#81353,#81354,#81355,#81356,
#81357,#81358,#81359,#81360,#81361,#81362,#81363,#81364,#81365,#81366,#81367,
#81368,#81369,#81370,#81371,#81372,#81373,#81374,#81375,#81376,#81377,#81378),
 .UNSPECIFIED.,.F.,.F.,(4,3,3,3,3,3,3,3,3,3,3,3,3,3,3,3,3,3,3,3,3,3,3,3,
3,3,3,4),(0.,0.101529500922143,0.222413752673,0.249999999999876,0.362127564372828,
0.374999999999812,0.437499999999778,0.46874999999976,0.484374999999751,
0.48892738670375,0.492135627913471,0.492858316487225,0.493479773407748,
0.499999999999745,0.601963594423371,0.624999999999756,0.687499999999762,
0.718749999999763,0.734374999999762,0.74218749999976,0.746093749999758,
0.749999999999756,0.795770799058943,0.841887284320127,0.887967824962089,
0.933349893659305,0.976313037422695,1.),.UNSPECIFIED.);
#1809=B_SPLINE_CURVE_WITH_KNOTS('',3,(#81466,#81467,#81468,#81469,#81470,
#81471,#81472,#81473,#81474,#81475,#81476,#81477,#81478,#81479,#81480,#81481,
#81482,#81483,#81484,#81485,#81486,#81487,#81488,#81489,#81490,#81491,#81492,
#81493,#81494,#81495,#81496,#81497,#81498,#81499,#81500,#81501,#81502,#81503,
#81504,#81505,#81506,#81507,#81508,#81509,#81510,#81511,#81512,#81513,#81514,
#81515,#81516,#81517,#81518,#81519,#81520),.UNSPECIFIED.,.F.,.F.,(4,3,3,
3,3,3,3,3,3,3,3,3,3,3,3,3,3,3,4),(0.,0.120637102514753,0.250000000000005,
0.375000000000008,0.437500000000011,0.46400815730569,0.468497525776301,
0.470967635615609,0.487729750531094,0.494705110367547,0.497908251856533,
0.499991186139283,0.501597039562557,0.543532629222724,0.626157938461672,
0.747341134508375,0.859198878060181,0.960140090645202,1.),.UNSPECIFIED.);
#1810=B_SPLINE_CURVE_WITH_KNOTS('',3,(#81604,#81605,#81606,#81607,#81608,
#81609,#81610,#81611,#81612,#81613,#81614,#81615,#81616,#81617,#81618,#81619,
#81620,#81621,#81622,#81623,#81624,#81625,#81626,#81627,#81628,#81629,#81630,
#81631,#81632,#81633,#81634,#81635,#81636,#81637,#81638,#81639,#81640,#81641,
#81642,#81643,#81644,#81645,#81646),.UNSPECIFIED.,.F.,.F.,(4,3,3,3,3,3,
3,3,3,3,3,3,3,3,4),(0.,0.0966694249688917,0.231867346864773,0.250000000000024,
0.352344865255222,0.375000000000035,0.437500000000042,0.468750000000045,
0.483362225881677,0.500000000000047,0.545177325600272,0.705546343994153,
0.856284891331945,0.975254970201329,1.),.UNSPECIFIED.);
#1811=B_SPLINE_CURVE_WITH_KNOTS('',3,(#81797,#81798,#81799,#81800,#81801,
#81802,#81803,#81804,#81805,#81806,#81807,#81808,#81809),.UNSPECIFIED.,
 .F.,.F.,(4,3,3,3,4),(0.,0.290643058527184,0.585647964061105,0.887654578917741,
1.),.UNSPECIFIED.);
#1812=B_SPLINE_CURVE_WITH_KNOTS('',3,(#81878,#81879,#81880,#81881,#81882,
#81883,#81884,#81885,#81886,#81887),.UNSPECIFIED.,.F.,.F.,(4,3,3,4),(0.,
0.388137409541929,0.768803426065497,1.),.UNSPECIFIED.);
#1813=B_SPLINE_CURVE_WITH_KNOTS('',3,(#81952,#81953,#81954,#81955,#81956,
#81957,#81958,#81959,#81960,#81961,#81962,#81963,#81964),.UNSPECIFIED.,
 .F.,.F.,(4,3,3,3,4),(0.,0.301170390997793,0.597353856341166,0.886897365258997,
1.),.UNSPECIFIED.);
#1814=B_SPLINE_CURVE_WITH_KNOTS('',3,(#82002,#82003,#82004,#82005,#82006,
#82007,#82008,#82009,#82010,#82011),.UNSPECIFIED.,.F.,.F.,(4,3,3,4),(0.,
0.379616953105207,0.766838018123526,0.999999998064869),.UNSPECIFIED.);
#1815=B_SPLINE_CURVE_WITH_KNOTS('',3,(#82165,#82166,#82167,#82168,#82169,
#82170,#82171,#82172,#82173,#82174,#82175,#82176,#82177,#82178,#82179,#82180,
#82181,#82182,#82183,#82184,#82185,#82186,#82187,#82188,#82189,#82190,#82191,
#82192,#82193,#82194,#82195),.UNSPECIFIED.,.F.,.F.,(4,3,3,3,3,3,3,3,3,3,
4),(0.,0.0997880523616104,0.200062662981434,0.301948937113961,0.405212424694865,
0.51037062471613,0.61810126360354,0.731592938427962,0.849728512114637,0.976002843446623,
1.),.UNSPECIFIED.);
#1816=B_SPLINE_CURVE_WITH_KNOTS('',3,(#82363,#82364,#82365,#82366,#82367,
#82368,#82369,#82370,#82371,#82372,#82373,#82374,#82375,#82376,#82377,#82378,
#82379,#82380,#82381,#82382,#82383,#82384,#82385,#82386,#82387,#82388,#82389,
#82390,#82391,#82392,#82393,#82394,#82395,#82396,#82397,#82398,#82399,#82400,
#82401,#82402,#82403,#82404,#82405,#82406,#82407,#82408,#82409,#82410,#82411,
#82412,#82413,#82414,#82415,#82416,#82417,#82418,#82419,#82420,#82421,#82422,
#82423,#82424,#82425,#82426,#82427,#82428,#82429,#82430,#82431,#82432,#82433,
#82434,#82435),.UNSPECIFIED.,.F.,.F.,(4,3,3,3,3,3,3,3,3,3,3,3,3,3,3,3,3,
3,3,3,3,3,3,3,4),(0.,0.0437264140634012,0.089989771863013,0.12499999999996,
0.170646942111976,0.187499999999941,0.218749999999933,0.234374999999931,
0.242187499999928,0.246093749999931,0.249999999999934,0.324140195987469,
0.374999999999962,0.437499999999977,0.468749999999983,0.484374999999987,
0.492187499999989,0.499419384271932,0.499999999999991,0.546155699914753,
0.638263904679061,0.757052346717483,0.864898370340035,0.957922231030437,
1.),.UNSPECIFIED.);
#1817=B_SPLINE_CURVE_WITH_KNOTS('',3,(#82525,#82526,#82527,#82528,#82529,
#82530,#82531,#82532,#82533,#82534,#82535,#82536,#82537),.UNSPECIFIED.,
 .F.,.F.,(4,3,3,3,4),(0.,0.32216108780556,0.609771124076306,0.905431279270806,
1.),.UNSPECIFIED.);
#1818=B_SPLINE_CURVE_WITH_KNOTS('',3,(#82548,#82549,#82550,#82551,#82552,
#82553,#82554,#82555,#82556,#82557,#82558,#82559,#82560,#82561,#82562,#82563,
#82564,#82565,#82566,#82567,#82568,#82569,#82570,#82571,#82572,#82573,#82574,
#82575,#82576,#82577,#82578,#82579,#82580,#82581,#82582,#82583,#82584,#82585,
#82586,#82587,#82588,#82589,#82590,#82591,#82592,#82593,#82594,#82595,#82596,
#82597,#82598,#82599,#82600,#82601,#82602),.UNSPECIFIED.,.F.,.F.,(4,3,3,
3,3,3,3,3,3,3,3,3,3,3,3,3,3,3,4),(-4.71575303852,-4.65907697863314,-4.59837909975905,
-4.56620180037,-4.49782940088838,-4.45572366868,-4.37891278786157,-4.34130806771,
-4.27463577302459,-4.21375904184622,-4.18701109461,-4.10530819905221,-4.019523415627,
-3.96784558239,-3.87773712401142,-3.78337627560873,-3.75420974096,-3.65160927305,
-3.54900880514),.UNSPECIFIED.);
#1819=B_SPLINE_CURVE_WITH_KNOTS('',3,(#82604,#82605,#82606,#82607,#82608,
#82609,#82610,#82611,#82612,#82613),.UNSPECIFIED.,.F.,.F.,(4,3,3,4),(-6.00042817873,
-5.73764962787167,-5.47143019297584,-5.20521075808),.UNSPECIFIED.);
#1820=B_SPLINE_CURVE_WITH_KNOTS('',3,(#82649,#82650,#82651,#82652,#82653,
#82654,#82655,#82656,#82657,#82658,#82659,#82660,#82661,#82662,#82663,#82664),
 .UNSPECIFIED.,.F.,.F.,(4,3,3,3,3,4),(1.9878298196,2.12810444562736,2.20723764364,
2.34744480889074,2.48762106236855,2.53578324996),.UNSPECIFIED.);
#1821=B_SPLINE_CURVE_WITH_KNOTS('',3,(#82670,#82671,#82672,#82673,#82674,
#82675,#82676,#82677,#82678,#82679,#82680,#82681,#82682,#82683,#82684,#82685,
#82686,#82687,#82688,#82689,#82690,#82691,#82692,#82693,#82694,#82695,#82696,
#82697,#82698,#82699,#82700,#82701,#82702,#82703,#82704,#82705,#82706),
 .UNSPECIFIED.,.F.,.F.,(4,3,3,3,3,3,3,3,3,3,3,3,4),(1.62679171178,1.80119189921,
2.06549727040562,2.33022193180684,2.59511005010776,2.8601162004504,2.9864917,
3.25107716364615,3.51563595035349,3.56612301471,3.83086251970706,4.09597227277403,
4.14575432942),.UNSPECIFIED.);
#1822=B_SPLINE_CURVE_WITH_KNOTS('',3,(#82771,#82772,#82773,#82774,#82775,
#82776,#82777,#82778,#82779,#82780),.UNSPECIFIED.,.F.,.F.,(4,3,3,4),(0.,
0.393559372360371,0.800977653566811,1.),.UNSPECIFIED.);
#1823=B_SPLINE_CURVE_WITH_KNOTS('',3,(#82835,#82836,#82837,#82838,#82839,
#82840,#82841,#82842,#82843,#82844,#82845,#82846,#82847,#82848,#82849,#82850,
#82851,#82852,#82853,#82854,#82855,#82856,#82857,#82858,#82859,#82860,#82861,
#82862,#82863,#82864,#82865,#82866,#82867,#82868,#82869,#82870,#82871,#82872,
#82873,#82874,#82875,#82876,#82877,#82878,#82879,#82880,#82881,#82882,#82883,
#82884,#82885,#82886,#82887,#82888,#82889,#82890,#82891,#82892,#82893,#82894,
#82895,#82896,#82897,#82898,#82899,#82900,#82901),.UNSPECIFIED.,.F.,.F.,
(4,3,3,3,3,3,3,3,3,3,3,3,3,3,3,3,3,3,3,3,3,3,4),(0.,0.0466542567303633,
0.100279857526539,0.162566268563517,0.222223321736243,0.250000000000032,
0.32224695109353,0.371748221688835,0.420281745240556,0.462936832422792,
0.481468416211426,0.484289083525892,0.485665060839194,0.493820456455645,
0.500000000000061,0.582690514763901,0.661722188633312,0.737674786625859,
0.75000000000003,0.825845181320885,0.900982137734557,0.97270193986251,1.),
 .UNSPECIFIED.);
#1824=B_SPLINE_CURVE_WITH_KNOTS('',5,(#82930,#82931,#82932,#82933,#82934,
#82935),.UNSPECIFIED.,.F.,.F.,(6,6),(5.20484021909,5.76063633602),
 .UNSPECIFIED.);
#1825=B_SPLINE_CURVE_WITH_KNOTS('',3,(#82936,#82937,#82938,#82939,#82940,
#82941,#82942,#82943,#82944,#82945,#82946,#82947,#82948,#82949,#82950,#82951,
#82952,#82953,#82954,#82955,#82956,#82957,#82958,#82959,#82960,#82961,#82962,
#82963,#82964,#82965,#82966,#82967,#82968,#82969,#82970,#82971,#82972,#82973,
#82974,#82975,#82976,#82977,#82978,#82979,#82980,#82981,#82982,#82983,#82984,
#82985,#82986,#82987,#82988,#82989,#82990),.UNSPECIFIED.,.F.,.F.,(4,3,3,
3,3,3,3,3,3,3,3,3,3,3,3,3,3,3,4),(3.54900880515,3.651609273055,3.75420974096,
3.84893307386556,3.93929532064981,3.96784558239,4.05430391724671,4.13645477350633,
4.18701109461,4.24753706288369,4.31344142163189,4.34130806771,4.41811894852724,
4.45572366868,4.52409606816139,4.56620180037,4.62755792701915,4.68459440694729,
4.71575303852),.UNSPECIFIED.);
#1826=B_SPLINE_CURVE_WITH_KNOTS('',3,(#83031,#83032,#83033,#83034,#83035,
#83036,#83037),.UNSPECIFIED.,.F.,.F.,(4,3,4),(5.20484021909,5.51152466079559,
5.76063633567283),.UNSPECIFIED.);
#1827=B_SPLINE_CURVE_WITH_KNOTS('',3,(#83092,#83093,#83094,#83095,#83096,
#83097,#83098,#83099,#83100,#83101,#83102,#83103,#83104,#83105,#83106,#83107,
#83108,#83109,#83110,#83111,#83112,#83113,#83114,#83115,#83116,#83117,#83118,
#83119,#83120,#83121,#83122,#83123,#83124,#83125,#83126,#83127,#83128,#83129,
#83130,#83131,#83132,#83133,#83134,#83135,#83136,#83137,#83138,#83139,#83140,
#83141,#83142,#83143,#83144,#83145,#83146,#83147,#83148,#83149,#83150,#83151,
#83152,#83153,#83154,#83155),.UNSPECIFIED.,.F.,.F.,(4,3,3,3,3,3,3,3,3,3,
3,3,3,3,3,3,3,3,3,3,3,4),(0.,0.0726878348096301,0.147617440689613,0.22357937320159,
0.250000000000044,0.325585219584544,0.375000000000065,0.437500000000074,
0.468750000000078,0.484375000000076,0.493410050348708,0.500000000000073,
0.537063812349334,0.579892736074948,0.63030009007674,0.696058572840903,
0.750000000000037,0.808743423167996,0.871226719986258,0.928440251933461,
0.975705935423915,1.),.UNSPECIFIED.);
#1828=B_SPLINE_CURVE_WITH_KNOTS('',5,(#83168,#83169,#83170,#83171,#83172,
#83173,#83174,#83175,#83176),.UNSPECIFIED.,.F.,.F.,(6,3,6),(1.9878298196,
2.20723764364,2.53578324996),.UNSPECIFIED.);
#1829=B_SPLINE_CURVE_WITH_KNOTS('',3,(#83178,#83179,#83180,#83181,#83182,
#83183,#83184,#83185,#83186,#83187,#83188,#83189,#83190,#83191,#83192,#83193,
#83194,#83195,#83196,#83197,#83198,#83199,#83200,#83201,#83202),
 .UNSPECIFIED.,.F.,.F.,(4,3,3,3,3,3,3,3,4),(0.,0.125,0.250543946517898,
0.377358570830386,0.5,0.626576440687726,0.752623525909811,0.876311762954906,
1.),.UNSPECIFIED.);
#1830=B_SPLINE_CURVE_WITH_KNOTS('',3,(#83314,#83315,#83316,#83317),
 .UNSPECIFIED.,.F.,.F.,(4,4),(0.,1.),.UNSPECIFIED.);
#1831=B_SPLINE_CURVE_WITH_KNOTS('',3,(#83321,#83322,#83323,#83324),
 .UNSPECIFIED.,.F.,.F.,(4,4),(0.,1.),.UNSPECIFIED.);
#1832=B_SPLINE_CURVE_WITH_KNOTS('',3,(#83328,#83329,#83330,#83331,#83332,
#83333,#83334,#83335,#83336,#83337,#83338,#83339,#83340,#83341,#83342,#83343,
#83344,#83345,#83346,#83347,#83348,#83349,#83350,#83351,#83352,#83353,#83354,
#83355,#83356,#83357),.UNSPECIFIED.,.F.,.F.,(4,2,2,2,2,2,2,2,2,2,2,2,2,
2,4),(-0.833290959100427,-0.719731949150803,-0.654120822724273,-0.577438704646923,
-0.501338594516947,-0.461398420908702,-0.440530284809963,-0.42516956916302,
-0.409392849496736,-0.386618223744604,-0.341743775261219,-0.248906272057569,
-0.173189557116592,-0.104522264822832,0.),.UNSPECIFIED.);
#1833=B_SPLINE_CURVE_WITH_KNOTS('',3,(#83361,#83362,#83363,#83364,#83365,
#83366,#83367,#83368,#83369,#83370,#83371,#83372,#83373,#83374,#83375,#83376,
#83377,#83378,#83379,#83380,#83381,#83382,#83383,#83384,#83385,#83386,#83387,
#83388,#83389,#83390,#83391,#83392,#83393,#83394),.UNSPECIFIED.,.F.,.F.,
(4,2,2,2,2,2,2,2,2,2,2,2,2,2,2,2,4),(-1.07487450803108,-1.01285655971456,
-0.949156086804949,-0.887082494974661,-0.773145859214011,-0.648162202604292,
-0.588558809942147,-0.558533895802779,-0.537355412523811,-0.51622241952717,
-0.486414822988416,-0.427362602801514,-0.303708789768619,-0.188644968303673,
-0.126436798617497,-0.0628185639370024,0.),.UNSPECIFIED.);
#1834=B_SPLINE_CURVE_WITH_KNOTS('',3,(#83397,#83398,#83399,#83400,#83401,
#83402,#83403,#83404,#83405,#83406,#83407,#83408,#83409,#83410,#83411,#83412,
#83413,#83414,#83415,#83416,#83417,#83418,#83419,#83420,#83421,#83422,#83423,
#83424,#83425,#83426),.UNSPECIFIED.,.F.,.F.,(4,2,2,2,2,2,2,2,2,2,2,2,2,
2,4),(-0.852996228072085,-0.748747176415804,-0.679888185472483,-0.60345940835717,
-0.506988533121608,-0.460271817616593,-0.436590151478536,-0.420246786301877,
-0.404384441460722,-0.382912427188685,-0.341869354576151,-0.263694658937176,
-0.184053280783239,-0.1167820739734,0.),.UNSPECIFIED.);
#1835=B_SPLINE_CURVE_WITH_KNOTS('',3,(#83442,#83443,#83444,#83445,#83446,
#83447,#83448,#83449,#83450,#83451),.UNSPECIFIED.,.F.,.F.,(4,3,3,4),(-0.253192357174,
-0.139449012417409,-0.0270751805148477,0.),.UNSPECIFIED.);
#1836=B_SPLINE_CURVE_WITH_KNOTS('',3,(#83459,#83460,#83461,#83462,#83463,
#83464,#83465,#83466,#83467,#83468),.UNSPECIFIED.,.F.,.F.,(4,3,3,4),(-0.253192357174,
-0.138730841190324,-0.0343582758464,0.),.UNSPECIFIED.);
#1837=B_SPLINE_CURVE_WITH_KNOTS('',3,(#83549,#83550,#83551,#83552,#83553,
#83554,#83555,#83556,#83557,#83558),.UNSPECIFIED.,.F.,.F.,(4,2,2,2,4),(-0.144315123192822,
-0.131533764343683,-0.118752405494545,-0.107522188711281,-0.0962919719280169),
 .UNSPECIFIED.);
#1838=B_SPLINE_CURVE_WITH_KNOTS('',3,(#83562,#83563,#83564,#83565,#83566,
#83567,#83568,#83569,#83570,#83571),.UNSPECIFIED.,.F.,.F.,(4,2,2,2,4),(-0.196399203297034,
-0.185168424394202,-0.17393764549137,-0.16054110108432,-0.14714455667727),
 .UNSPECIFIED.);
#1839=B_SPLINE_CURVE_WITH_KNOTS('',3,(#83579,#83580,#83581,#83582,#83583,
#83584,#83585,#83586,#83587,#83588),.UNSPECIFIED.,.F.,.F.,(4,2,2,2,4),(-0.0467821086425278,
-0.0346600950145953,-0.0225380813866629,-0.0112690406933315,0.),
 .UNSPECIFIED.);
#1840=B_SPLINE_CURVE_WITH_KNOTS('',3,(#83592,#83593,#83594,#83595,#83596,
#83597,#83598,#83599,#83600,#83601),.UNSPECIFIED.,.F.,.F.,(4,2,2,2,4),(0.140042886502516,
0.152164900130449,0.164286913758381,0.175555954451712,0.186824995145044),
 .UNSPECIFIED.);
#1841=B_SPLINE_CURVE_WITH_KNOTS('',3,(#83609,#83610,#83611,#83612,#83613,
#83614,#83615,#83616,#83617,#83618),.UNSPECIFIED.,.F.,.F.,(4,2,2,2,4),(0.,
0.0112307789028322,0.0224615578056644,0.0358581022127147,0.049254646619765),
 .UNSPECIFIED.);
#1842=B_SPLINE_CURVE_WITH_KNOTS('',3,(#83622,#83623,#83624,#83625,#83626,
#83627,#83628,#83629,#83630,#83631),.UNSPECIFIED.,.F.,.F.,(4,2,2,2,4),(0.0482688206632123,
0.0610501795123504,0.0738315383614886,0.0850617551447528,0.0962919719280169),
 .UNSPECIFIED.);
#1843=B_SPLINE_CURVE_WITH_KNOTS('',3,(#83654,#83655,#83656,#83657,#83658,
#83659,#83660,#83661,#83662,#83663),.UNSPECIFIED.,.F.,.F.,(4,2,2,2,4),(0.155359683062337,
0.174129548699776,0.192899414337214,0.212868752049424,0.232838089761635),
 .UNSPECIFIED.);
#1844=B_SPLINE_CURVE_WITH_KNOTS('',3,(#83667,#83668,#83669,#83670,#83671,
#83672,#83673,#83674,#83675,#83676),.UNSPECIFIED.,.F.,.F.,(4,2,2,2,4),(0.,
0.0376480157709213,0.0752960315418425,0.114456223316623,0.153616415091404),
 .UNSPECIFIED.);
#1845=B_SPLINE_CURVE_WITH_KNOTS('',3,(#83680,#83681,#83682,#83683,#83684,
#83685,#83686,#83687,#83688,#83689),.UNSPECIFIED.,.F.,.F.,(4,2,2,2,4),(0.152551363664982,
0.191711555439763,0.230871747214544,0.268519762985465,0.306167778756386),
 .UNSPECIFIED.);
#1846=B_SPLINE_CURVE_WITH_KNOTS('',3,(#83693,#83694,#83695,#83696,#83697,
#83698,#83699,#83700,#83701,#83702),.UNSPECIFIED.,.F.,.F.,(4,2,2,2,4),(0.233240959425377,
0.253210297137588,0.273179634849798,0.291949500487237,0.310719366124675),
 .UNSPECIFIED.);
#1847=B_SPLINE_CURVE_WITH_KNOTS('',3,(#83706,#83707,#83708,#83709,#83710,
#83711,#83712,#83713,#83714,#83715),.UNSPECIFIED.,.F.,.F.,(4,2,2,2,4),(0.,
0.0187909725801054,0.0375819451602107,0.057142029435283,0.0767021137103553),
 .UNSPECIFIED.);
#1848=B_SPLINE_CURVE_WITH_KNOTS('',3,(#83719,#83720,#83721,#83722,#83723,
#83724,#83725,#83726,#83727,#83728),.UNSPECIFIED.,.F.,.F.,(4,2,2,2,4),(0.304035731537011,
0.341700659844232,0.379365588151452,0.417900205299532,0.456434822447611),
 .UNSPECIFIED.);
#1849=B_SPLINE_CURVE_WITH_KNOTS('',3,(#83732,#83733,#83734,#83735,#83736,
#83737,#83738,#83739,#83740,#83741),.UNSPECIFIED.,.F.,.F.,(4,2,2,2,4),(0.455672372163422,
0.494206989311501,0.53274160645958,0.570406534766801,0.608071463074022),
 .UNSPECIFIED.);
#1850=B_SPLINE_CURVE_WITH_KNOTS('',3,(#83744,#83745,#83746,#83747,#83748,
#83749,#83750,#83751,#83752,#83753),.UNSPECIFIED.,.F.,.F.,(4,2,2,2,4),(0.0770095720919635,
0.0965696563670357,0.116129740642108,0.134920713222213,0.153711685802319),
 .UNSPECIFIED.);
#1851=B_SPLINE_CURVE_WITH_KNOTS('',3,(#83760,#83761,#83762,#83763,#83764,
#83765,#83766,#83767,#83768,#83769),.UNSPECIFIED.,.F.,.F.,(4,2,2,2,4),(-0.153352484887989,
-0.134556531278179,-0.115760577668369,-0.0962856459910287,-0.0768107143136885),
 .UNSPECIFIED.);
#1852=B_SPLINE_CURVE_WITH_KNOTS('',3,(#83773,#83774,#83775,#83776,#83777,
#83778,#83779,#83780,#83781,#83782),.UNSPECIFIED.,.F.,.F.,(4,2,2,2,4),(-0.607454139351607,
-0.569789123310172,-0.532124107268736,-0.493689195876788,-0.45525428448484),
 .UNSPECIFIED.);
#1853=B_SPLINE_CURVE_WITH_KNOTS('',3,(#83786,#83787,#83788,#83789,#83790,
#83791,#83792,#83793,#83794,#83795),.UNSPECIFIED.,.F.,.F.,(4,2,2,2,4),(-0.455926924542571,
-0.417492013150623,-0.379057101758675,-0.341392085717239,-0.303727069675804),
 .UNSPECIFIED.);
#1854=B_SPLINE_CURVE_WITH_KNOTS('',3,(#83799,#83800,#83801,#83802,#83803,
#83804,#83805,#83806,#83807,#83808),.UNSPECIFIED.,.F.,.F.,(4,2,2,2,4),(-0.0765417705743012,
-0.0570668388969609,-0.0375919072196206,-0.0187959536098103,0.),
 .UNSPECIFIED.);
#1855=B_SPLINE_CURVE_WITH_KNOTS('',3,(#83812,#83813,#83814,#83815,#83816,
#83817,#83818,#83819,#83820,#83821),.UNSPECIFIED.,.F.,.F.,(4,2,2,2,4),(-0.309577812617237,
-0.29080046183718,-0.272023111057122,-0.252190592955192,-0.232358074853261),
 .UNSPECIFIED.);
#1856=B_SPLINE_CURVE_WITH_KNOTS('',3,(#83825,#83826,#83827,#83828,#83829,
#83830,#83831,#83832,#83833,#83834),.UNSPECIFIED.,.F.,.F.,(4,2,2,2,4),(-0.30560294875119,
-0.267953353992129,-0.230303759233068,-0.191318992716313,-0.152334226199558),
 .UNSPECIFIED.);
#1857=B_SPLINE_CURVE_WITH_KNOTS('',3,(#83838,#83839,#83840,#83841,#83842,
#83843,#83844,#83845,#83846,#83847),.UNSPECIFIED.,.F.,.F.,(4,2,2,2,4),(-0.153268722551632,
-0.114283956034877,-0.0752991895181218,-0.0376495947590609,-2.77555756156289E-17),
 .UNSPECIFIED.);
#1858=B_SPLINE_CURVE_WITH_KNOTS('',3,(#83851,#83852,#83853,#83854,#83855,
#83856,#83857,#83858,#83859,#83860),.UNSPECIFIED.,.F.,.F.,(4,2,2,2,4),(-0.232008644072594,
-0.212176125970663,-0.192343607868733,-0.173566257088676,-0.154788906308618),
 .UNSPECIFIED.);
#1859=B_SPLINE_CURVE_WITH_KNOTS('',5,(#83981,#83982,#83983,#83984,#83985,
#83986),.UNSPECIFIED.,.F.,.F.,(6,6),(0.,1.),.UNSPECIFIED.);
#1860=B_SPLINE_CURVE_WITH_KNOTS('',3,(#84055,#84056,#84057,#84058,#84059,
#84060,#84061,#84062,#84063,#84064,#84065,#84066,#84067,#84068,#84069,#84070,
#84071,#84072,#84073,#84074,#84075,#84076,#84077,#84078,#84079,#84080,#84081,
#84082,#84083,#84084,#84085,#84086,#84087,#84088,#84089,#84090,#84091,#84092,
#84093,#84094,#84095,#84096,#84097,#84098,#84099,#84100,#84101,#84102,#84103,
#84104,#84105,#84106,#84107,#84108,#84109),.UNSPECIFIED.,.F.,.F.,(4,3,3,
3,3,3,3,3,3,3,3,3,3,3,3,3,3,3,4),(0.,0.105101150010298,0.211780208222473,
0.250000000000078,0.350769437864941,0.375000000000119,0.43750000000015,
0.446703937993579,0.468750000000166,0.48437500000017,0.494150913539028,
0.500000000000174,0.587354816489945,0.669329229379294,0.750000000000087,
0.823686773495111,0.895618722555497,0.965577824896743,1.),.UNSPECIFIED.);
#1861=B_SPLINE_CURVE_WITH_KNOTS('',3,(#84137,#84138,#84139,#84140,#84141,
#84142,#84143,#84144,#84145,#84146,#84147,#84148,#84149,#84150,#84151,#84152,
#84153,#84154,#84155,#84156,#84157,#84158,#84159,#84160,#84161,#84162,#84163,
#84164,#84165,#84166,#84167),.UNSPECIFIED.,.F.,.F.,(4,3,3,3,3,3,3,3,3,3,
4),(1.53218401448002,1.66838947160658,1.72279580036,1.86752328695562,1.91811675676,
2.019356098765,2.09643752541409,2.12059544077,2.17333959204,2.22608374331,
2.24943434875),.UNSPECIFIED.);
#1862=B_SPLINE_CURVE_WITH_KNOTS('',5,(#84168,#84169,#84170,#84171,#84172,
#84173,#84174,#84175,#84176),.UNSPECIFIED.,.F.,.F.,(6,3,6),(0.,0.473543414125104,
1.),.UNSPECIFIED.);
#1863=B_SPLINE_CURVE_WITH_KNOTS('',5,(#84180,#84181,#84182,#84183,#84184,
#84185),.UNSPECIFIED.,.F.,.F.,(6,6),(-1.61647556848,-1.5664121072),
 .UNSPECIFIED.);
#1864=B_SPLINE_CURVE_WITH_KNOTS('',3,(#84243,#84244,#84245,#84246,#84247,
#84248,#84249,#84250,#84251,#84252,#84253,#84254,#84255,#84256,#84257,#84258,
#84259,#84260,#84261,#84262,#84263,#84264,#84265,#84266,#84267,#84268,#84269,
#84270,#84271,#84272,#84273),.UNSPECIFIED.,.F.,.F.,(4,3,3,3,3,3,3,3,3,3,
4),(5.40059579705348E-8,0.108408281448171,0.220095081705907,0.333600124442993,
0.450483280546452,0.466393453636723,0.5,0.618967115497545,0.74413257000632,
0.879599145160207,1.),.UNSPECIFIED.);
#1865=B_SPLINE_CURVE_WITH_KNOTS('',3,(#84334,#84335,#84336,#84337,#84338,
#84339,#84340,#84341,#84342,#84343,#84344,#84345,#84346,#84347,#84348,#84349,
#84350,#84351,#84352,#84353,#84354,#84355,#84356,#84357,#84358,#84359,#84360,
#84361,#84362,#84363,#84364,#84365,#84366,#84367,#84368,#84369,#84370,#84371,
#84372,#84373,#84374,#84375,#84376,#84377,#84378,#84379,#84380,#84381,#84382),
 .UNSPECIFIED.,.F.,.F.,(4,3,3,3,3,3,3,3,3,3,3,3,3,3,3,3,4),(-3.42099781868,
-3.33892724177637,-3.26381939413,-3.17772035749469,-3.10665277284,-3.01841374448793,
-2.96248504801,-2.88144261558925,-2.81847755741,-2.71554484205924,-2.67456504578,
-2.53067648094,-2.39385786562,-2.28537736936454,-2.25703034102,-2.17618742334,
-2.14863240656),.UNSPECIFIED.);
#1866=B_SPLINE_CURVE_WITH_KNOTS('',3,(#84590,#84591,#84592,#84593,#84594,
#84595,#84596,#84597,#84598,#84599,#84600,#84601,#84602,#84603,#84604,#84605,
#84606,#84607,#84608,#84609,#84610,#84611,#84612,#84613,#84614,#84615,#84616,
#84617,#84618,#84619,#84620,#84621,#84622,#84623,#84624,#84625,#84626,#84627,
#84628,#84629,#84630,#84631,#84632,#84633,#84634,#84635),.UNSPECIFIED.,
 .F.,.F.,(4,3,3,3,3,3,3,3,3,3,3,3,3,3,3,4),(0.,0.0675680446171937,0.124999999999998,
0.170177845044704,0.219746219115553,0.249999999999996,0.32140342215739,
0.397256102134981,0.473108782112573,0.499999999999997,0.613366660168327,
0.686326334594986,0.749999999999999,0.837332896579508,0.925213195395331,
0.999999999999777),.UNSPECIFIED.);
#1867=B_SPLINE_CURVE_WITH_KNOTS('',3,(#84636,#84637,#84638,#84639,#84640,
#84641,#84642,#84643,#84644,#84645,#84646,#84647,#84648,#84649,#84650,#84651,
#84652,#84653,#84654,#84655,#84656,#84657,#84658,#84659,#84660,#84661,#84662,
#84663,#84664,#84665,#84666),.UNSPECIFIED.,.F.,.F.,(4,3,3,3,3,3,3,3,3,3,
4),(1.53218401448,1.66838947160656,1.72279580036,1.86752328695562,1.91811675676,
2.019356098765,2.09643752541409,2.12059544077,2.17333959204,2.22608374331,
2.24943434875),.UNSPECIFIED.);
#1868=B_SPLINE_CURVE_WITH_KNOTS('',5,(#84670,#84671,#84672,#84673,#84674,
#84675),.UNSPECIFIED.,.F.,.F.,(6,6),(-1.61647556848,-1.5664121072),
 .UNSPECIFIED.);
#1869=B_SPLINE_CURVE_WITH_KNOTS('',3,(#84735,#84736,#84737,#84738,#84739,
#84740,#84741,#84742,#84743,#84744,#84745,#84746,#84747,#84748,#84749,#84750,
#84751,#84752,#84753,#84754,#84755,#84756,#84757,#84758,#84759,#84760,#84761,
#84762),.UNSPECIFIED.,.F.,.F.,(4,3,3,3,3,3,3,3,3,4),(6.97389952659368E-8,
0.156232405135153,0.315775975767977,0.47610392685238,0.538072664088518,
0.67492807522622,0.766738756539317,0.849071536484418,0.924535768242209,
1.),.UNSPECIFIED.);
#1870=B_SPLINE_CURVE_WITH_KNOTS('',3,(#84823,#84824,#84825,#84826,#84827,
#84828,#84829,#84830,#84831,#84832,#84833,#84834,#84835,#84836,#84837,#84838,
#84839,#84840,#84841,#84842,#84843,#84844,#84845,#84846,#84847,#84848,#84849,
#84850,#84851,#84852,#84853,#84854,#84855,#84856,#84857,#84858,#84859,#84860,
#84861,#84862,#84863,#84864,#84865,#84866,#84867,#84868,#84869,#84870,#84871),
 .UNSPECIFIED.,.F.,.F.,(4,3,3,3,3,3,3,3,3,3,3,3,3,3,3,3,4),(-3.42099781868,
-3.33892724177637,-3.26381939413,-3.17772035749469,-3.10665277284,-3.01841374448793,
-2.96248504801,-2.88144261558925,-2.81847755741,-2.71554484205924,-2.67456504578,
-2.53067648094,-2.39385786562,-2.28537736936454,-2.25703034102,-2.17618742334,
-2.14863240656),.UNSPECIFIED.);
#1871=B_SPLINE_CURVE_WITH_KNOTS('',3,(#85045,#85046,#85047,#85048,#85049,
#85050,#85051,#85052,#85053,#85054,#85055,#85056,#85057,#85058,#85059,#85060,
#85061,#85062,#85063,#85064,#85065,#85066,#85067,#85068,#85069,#85070,#85071,
#85072,#85073,#85074),.UNSPECIFIED.,.F.,.F.,(4,2,2,2,2,2,2,2,2,2,2,2,2,
2,4),(-0.833290959113763,-0.71973194916232,-0.654120822734474,-0.577438704655354,
-0.501338594523518,-0.4613984209143,-0.440530284815032,-0.425169569167644,
-0.409392849500976,-0.38661822374839,-0.341743775264109,-0.248906272058694,
-0.173189557116784,-0.104522264822944,0.),.UNSPECIFIED.);
#1872=B_SPLINE_CURVE_WITH_KNOTS('',3,(#85082,#85083,#85084,#85085,#85086,
#85087,#85088,#85089,#85090,#85091,#85092,#85093,#85094,#85095,#85096,#85097,
#85098,#85099,#85100,#85101,#85102,#85103,#85104,#85105,#85106,#85107,#85108,
#85109,#85110,#85111,#85112,#85113,#85114,#85115),.UNSPECIFIED.,.F.,.F.,
(4,2,2,2,2,2,2,2,2,2,2,2,2,2,2,2,4),(-1.07487450803614,-1.0128565597187,
-0.949156086808256,-0.887082494977377,-0.773145859215987,-0.648162202605535,
-0.588558809943016,-0.558533895803447,-0.537355412524404,-0.516222419527731,
-0.486414822988885,-0.427362602801782,-0.303708789768471,-0.188644968303642,
-0.126436798617536,-0.0628185639369926,0.),.UNSPECIFIED.);
#1873=B_SPLINE_CURVE_WITH_KNOTS('',3,(#85123,#85124,#85125,#85126,#85127,
#85128,#85129,#85130,#85131,#85132,#85133,#85134,#85135,#85136,#85137,#85138,
#85139,#85140,#85141,#85142,#85143,#85144,#85145,#85146,#85147,#85148,#85149,
#85150,#85151,#85152),.UNSPECIFIED.,.F.,.F.,(4,2,2,2,2,2,2,2,2,2,2,2,2,
2,4),(-0.852996228067092,-0.748747176411645,-0.679888185468851,-0.603459408354018,
-0.506988533119108,-0.4602718176145,-0.436590151476641,-0.420246786300089,
-0.404384441459014,-0.38291242718713,-0.341869354574893,-0.263694658936475,
-0.184053280783088,-0.116782073973477,0.),.UNSPECIFIED.);
#1874=B_SPLINE_CURVE_WITH_KNOTS('',5,(#85191,#85192,#85193,#85194,#85195,
#85196,#85197,#85198,#85199,#85200,#85201,#85202,#85203,#85204,#85205,#85206,
#85207,#85208),.UNSPECIFIED.,.F.,.F.,(6,3,3,3,3,6),(0.,0.0563238113023862,
0.160203167534755,0.284130417633147,0.431668352740704,1.),.UNSPECIFIED.);
#1875=B_SPLINE_CURVE_WITH_KNOTS('',3,(#85226,#85227,#85228,#85229,#85230,
#85231,#85232,#85233,#85234,#85235,#85236,#85237,#85238,#85239,#85240,#85241,
#85242,#85243,#85244,#85245,#85246,#85247,#85248,#85249,#85250,#85251,#85252,
#85253,#85254,#85255,#85256,#85257,#85258,#85259,#85260,#85261,#85262,#85263,
#85264,#85265,#85266,#85267,#85268,#85269,#85270,#85271,#85272,#85273,#85274),
 .UNSPECIFIED.,.F.,.F.,(4,3,3,3,3,3,3,3,3,3,3,3,3,3,3,3,4),(0.,0.0625,0.127496488131178,
0.198782619245015,0.25,0.34219327047516,0.429444619020733,0.5,0.567975901527668,
0.632411690271494,0.692807754146875,0.75,0.806943714649852,0.861664292573192,
0.915319845265426,0.967555934138337,1.),.UNSPECIFIED.);
#1876=B_SPLINE_CURVE_WITH_KNOTS('',3,(#85286,#85287,#85288,#85289,#85290,
#85291,#85292,#85293,#85294,#85295,#85296,#85297,#85298,#85299,#85300),
 .UNSPECIFIED.,.F.,.F.,(4,2,2,3,2,2,4),(-0.00622622250198344,-0.00386052358474924,
-0.00164759382340911,0.,0.00161285720621331,0.00376992579683336,0.00622515821920392),
 .UNSPECIFIED.);
#1877=B_SPLINE_CURVE_WITH_KNOTS('',3,(#85334,#85335,#85336,#85337,#85338,
#85339,#85340,#85341,#85342,#85343,#85344,#85345,#85346,#85347,#85348,#85349,
#85350,#85351,#85352,#85353,#85354,#85355,#85356,#85357,#85358,#85359,#85360,
#85361,#85362,#85363,#85364,#85365,#85366,#85367,#85368,#85369,#85370,#85371,
#85372,#85373,#85374,#85375,#85376,#85377,#85378,#85379,#85380,#85381,#85382,
#85383,#85384,#85385,#85386,#85387,#85388),.UNSPECIFIED.,.F.,.F.,(4,3,3,
3,3,3,3,3,3,3,3,3,3,3,3,3,3,3,4),(2.67419613751012E-11,0.0720732721924963,
0.164826904591394,0.250000000000005,0.333767822910639,0.408022771354064,
0.444958736785786,0.468749999999991,0.486035361760652,0.499999999999984,
0.550902044618006,0.620498810264917,0.703215974839016,0.777411981129262,
0.842930292554886,0.899989318083444,0.949994659041722,0.991475269880567,
1.),.UNSPECIFIED.);
#1878=B_SPLINE_CURVE_WITH_KNOTS('',3,(#85403,#85404,#85405,#85406,#85407,
#85408,#85409,#85410,#85411,#85412,#85413,#85414,#85415,#85416,#85417,#85418,
#85419,#85420,#85421,#85422,#85423,#85424,#85425,#85426,#85427,#85428,#85429,
#85430,#85431,#85432,#85433,#85434,#85435,#85436,#85437,#85438,#85439,#85440,
#85441,#85442,#85443,#85444,#85445,#85446,#85447,#85448,#85449,#85450,#85451,
#85452,#85453,#85454),.UNSPECIFIED.,.F.,.F.,(4,3,3,3,3,3,3,3,3,3,3,3,3,
3,3,3,3,4),(0.,0.117683452141709,0.231772170622364,0.250000000000002,0.359974894834341,
0.37499999999999,0.437499999999986,0.468749999999984,0.48313769999903,0.499999999999981,
0.584430981722446,0.667215490861218,0.744913217773219,0.749999999999991,
0.823394141625011,0.894590151515514,0.962832104312354,1.),.UNSPECIFIED.);
#1879=B_SPLINE_CURVE_WITH_KNOTS('',3,(#85511,#85512,#85513,#85514,#85515,
#85516,#85517,#85518,#85519,#85520,#85521,#85522,#85523,#85524,#85525,#85526,
#85527,#85528,#85529,#85530,#85531,#85532,#85533,#85534,#85535,#85536,#85537,
#85538,#85539,#85540,#85541,#85542,#85543,#85544,#85545,#85546,#85547,#85548,
#85549,#85550,#85551,#85552,#85553),.UNSPECIFIED.,.F.,.F.,(4,3,3,3,3,3,
3,3,3,3,3,3,3,3,4),(0.,0.0665912841326879,0.134925436752382,0.20631186892184,
0.249999999999947,0.326272372957872,0.374999999999915,0.437499999999907,
0.468749999999907,0.484929812616762,0.499999999999907,0.610160130828769,
0.730077716451813,0.8574587793753,1.),.UNSPECIFIED.);
#1880=B_SPLINE_CURVE_WITH_KNOTS('',3,(#85570,#85571,#85572,#85573,#85574,
#85575,#85576,#85577,#85578,#85579,#85580,#85581,#85582,#85583,#85584,#85585,
#85586,#85587,#85588,#85589,#85590,#85591,#85592,#85593,#85594,#85595,#85596,
#85597,#85598,#85599,#85600,#85601,#85602,#85603,#85604,#85605,#85606,#85607,
#85608,#85609,#85610,#85611,#85612),.UNSPECIFIED.,.F.,.F.,(4,3,3,3,3,3,
3,3,3,3,3,3,3,3,4),(1.75158458902,1.82585854461461,1.90397349676335,1.93627831766,
2.01926759576981,2.10594778966711,2.14030218981,2.22559412880545,2.2812742412,
2.38564669191982,2.42220846454,2.53792768505673,2.67402562128176,2.83070830556877,
2.90384942405),.UNSPECIFIED.);
#1881=B_SPLINE_CURVE_WITH_KNOTS('',3,(#85645,#85646,#85647,#85648,#85649,
#85650,#85651,#85652,#85653,#85654,#85655,#85656,#85657,#85658,#85659,#85660,
#85661,#85662,#85663,#85664,#85665,#85666,#85667,#85668,#85669,#85670,#85671,
#85672,#85673,#85674,#85675,#85676,#85677,#85678,#85679,#85680,#85681),
 .UNSPECIFIED.,.F.,.F.,(4,3,3,3,3,3,3,3,3,3,3,3,4),(0.,0.0838435767709854,
0.171312435754512,0.25,0.323221763664416,0.398257191635949,0.478149991450796,
0.5,0.613728058543987,0.7328575589571,0.853783659825959,0.974765098059976,
1.),.UNSPECIFIED.);
#1882=B_SPLINE_CURVE_WITH_KNOTS('',5,(#85713,#85714,#85715,#85716,#85717,
#85718),.UNSPECIFIED.,.F.,.F.,(6,6),(0.,1.),.UNSPECIFIED.);
#1883=B_SPLINE_CURVE_WITH_KNOTS('',3,(#85726,#85727,#85728,#85729,#85730,
#85731,#85732,#85733,#85734,#85735,#85736,#85737,#85738,#85739,#85740,#85741,
#85742,#85743,#85744,#85745,#85746,#85747,#85748,#85749,#85750,#85751,#85752,
#85753,#85754,#85755,#85756,#85757,#85758,#85759,#85760,#85761,#85762,#85763,
#85764,#85765,#85766,#85767,#85768,#85769,#85770,#85771,#85772,#85773,#85774,
#85775,#85776,#85777,#85778,#85779,#85780,#85781,#85782,#85783,#85784,#85785,
#85786,#85787,#85788,#85789,#85790,#85791,#85792,#85793,#85794,#85795,#85796,
#85797,#85798,#85799,#85800,#85801,#85802,#85803,#85804,#85805,#85806,#85807,
#85808,#85809,#85810,#85811,#85812,#85813,#85814,#85815,#85816,#85817,#85818,
#85819),.UNSPECIFIED.,.F.,.F.,(4,3,3,3,3,3,3,3,3,3,3,3,3,3,3,3,3,3,3,3,
3,3,3,3,3,3,3,3,3,3,3,4),(0.,0.0748276374910851,0.125000000000074,0.187500000000111,
0.218750000000129,0.250000000000147,0.300925328069866,0.355808241698709,
0.37500000000022,0.429937897165098,0.437500000000255,0.46875000000027,0.484375000000277,
0.492187500000278,0.499376491125885,0.500000000000278,0.575416119571093,
0.625000000000229,0.687500000000202,0.718750000000192,0.731094508404207,
0.734375000000187,0.74218750000018,0.748059577436124,0.750000000000173,
0.777151942597279,0.820855228447611,0.860696859758832,0.905081076278559,
0.952540538139279,0.994179803577402,1.),.UNSPECIFIED.);
#1884=B_SPLINE_CURVE_WITH_KNOTS('',3,(#85827,#85828,#85829,#85830,#85831,
#85832,#85833,#85834,#85835,#85836,#85837,#85838,#85839,#85840,#85841,#85842,
#85843,#85844,#85845,#85846,#85847,#85848,#85849,#85850,#85851,#85852,#85853,
#85854,#85855,#85856,#85857,#85858,#85859,#85860,#85861,#85862,#85863,#85864,
#85865,#85866,#85867,#85868,#85869,#85870,#85871,#85872,#85873,#85874,#85875,
#85876,#85877,#85878,#85879,#85880,#85881,#85882,#85883,#85884,#85885,#85886,
#85887,#85888,#85889,#85890,#85891,#85892,#85893,#85894,#85895,#85896,#85897,
#85898,#85899,#85900,#85901,#85902),.UNSPECIFIED.,.F.,.F.,(4,3,3,3,3,3,
3,3,3,3,3,3,3,3,3,3,3,3,3,3,3,3,3,3,3,4),(0.,0.0240929222738366,0.0491054078753616,
0.0625000000000391,0.088020898963512,0.0937500000000545,0.109375000000062,
0.117187500000066,0.12500000000007,0.175258665507682,0.18750000000008,0.218750000000081,
0.2319234838028,0.245688962683513,0.250000000000082,0.326444716335682,0.375000000000072,
0.437500000000073,0.464386992567282,0.492751176174476,0.500000000000074,
0.592825659779259,0.68928762721816,0.789845932118812,0.894922966059406,
1.),.UNSPECIFIED.);
#1885=B_SPLINE_CURVE_WITH_KNOTS('',3,(#85905,#85906,#85907,#85908,#85909,
#85910,#85911,#85912,#85913,#85914,#85915,#85916,#85917,#85918,#85919,#85920,
#85921,#85922,#85923,#85924,#85925,#85926,#85927,#85928,#85929,#85930,#85931,
#85932,#85933,#85934,#85935,#85936,#85937,#85938,#85939,#85940,#85941,#85942,
#85943,#85944,#85945,#85946,#85947,#85948,#85949,#85950,#85951,#85952,#85953,
#85954,#85955,#85956,#85957,#85958,#85959),.UNSPECIFIED.,.F.,.F.,(4,3,3,
3,3,3,3,3,3,3,3,3,3,3,3,3,3,3,4),(0.,0.0980794130832024,0.195976664920974,
0.250000000000032,0.352035387886095,0.375000000000048,0.437500000000056,
0.465353490760474,0.494109597840485,0.500000000000065,0.57233409034639,
0.641941684786156,0.707653647662655,0.750000000000032,0.812500000000024,
0.87286251821144,0.931708475455832,0.98870050755195,1.),.UNSPECIFIED.);
#1886=B_SPLINE_CURVE_WITH_KNOTS('',3,(#85964,#85965,#85966,#85967,#85968,
#85969,#85970,#85971,#85972,#85973,#85974,#85975,#85976,#85977,#85978,#85979,
#85980,#85981,#85982,#85983,#85984,#85985,#85986,#85987,#85988,#85989,#85990,
#85991,#85992,#85993,#85994,#85995,#85996,#85997,#85998,#85999,#86000,#86001,
#86002,#86003,#86004,#86005,#86006,#86007,#86008,#86009,#86010,#86011,#86012,
#86013,#86014,#86015,#86016,#86017,#86018,#86019,#86020,#86021),
 .UNSPECIFIED.,.F.,.F.,(4,3,3,3,3,3,3,3,3,3,3,3,3,3,3,3,3,3,3,4),(0.,0.099452164972226,
0.198552648607838,0.249999999999997,0.320807489597197,0.390438911073157,
0.456941024049377,0.499999999999994,0.580883873456206,0.624999999999999,
0.687500000000001,0.718750000000002,0.73273662702563,0.747996545880403,
0.750000000000003,0.8052526318332,0.857501453743751,0.907936862272324,0.955604058949788,
1.),.UNSPECIFIED.);
#1887=B_SPLINE_CURVE_WITH_KNOTS('',3,(#86029,#86030,#86031,#86032,#86033,
#86034,#86035,#86036,#86037,#86038,#86039,#86040,#86041,#86042,#86043,#86044,
#86045,#86046,#86047,#86048,#86049,#86050,#86051,#86052,#86053,#86054,#86055,
#86056,#86057,#86058,#86059,#86060,#86061,#86062,#86063,#86064,#86065,#86066,
#86067,#86068,#86069,#86070,#86071,#86072,#86073,#86074),.UNSPECIFIED.,
 .F.,.F.,(4,3,3,3,3,3,3,3,3,3,3,3,3,3,3,4),(0.,0.12308642460795,0.217602621418341,
0.233320563260424,0.330691107811757,0.415188069702116,0.486802780982227,
0.545527895202698,0.591357388167948,0.624286558555176,0.644312028400629,
0.651431743486894,0.746696799313277,0.841963369757472,0.920978246085679,
1.),.UNSPECIFIED.);
#1888=B_SPLINE_CURVE_WITH_KNOTS('',3,(#86082,#86083,#86084,#86085,#86086,
#86087,#86088,#86089,#86090,#86091,#86092,#86093,#86094,#86095,#86096,#86097,
#86098,#86099,#86100,#86101,#86102,#86103,#86104,#86105,#86106,#86107,#86108,
#86109,#86110,#86111,#86112,#86113,#86114,#86115,#86116,#86117,#86118,#86119,
#86120,#86121,#86122,#86123,#86124,#86125,#86126,#86127,#86128,#86129,#86130,
#86131,#86132,#86133,#86134,#86135,#86136,#86137,#86138,#86139,#86140,#86141,
#86142,#86143,#86144,#86145,#86146,#86147,#86148,#86149,#86150,#86151,#86152,
#86153,#86154,#86155,#86156,#86157,#86158,#86159,#86160,#86161,#86162,#86163,
#86164,#86165,#86166,#86167,#86168,#86169,#86170,#86171,#86172,#86173,#86174,
#86175,#86176,#86177,#86178,#86179,#86180,#86181,#86182,#86183,#86184,#86185,
#86186,#86187,#86188,#86189,#86190),.UNSPECIFIED.,.F.,.F.,(4,3,3,3,3,3,
3,3,3,3,3,3,3,3,3,3,3,3,3,3,3,3,3,3,3,3,3,3,3,3,3,3,3,3,3,3,4),(0.,0.0355919704945219,
0.0625000000000467,0.0937500000000701,0.109375000000085,0.117187500000093,
0.124095624449358,0.125000000000101,0.147837211789802,0.179510913752234,
0.187500000000158,0.212407992374527,0.218750000000188,0.234375000000198,
0.242558143933212,0.250000000000209,0.29895865159147,0.312500000000223,
0.343750000000233,0.358265386399709,0.372173812649809,0.375000000000243,
0.396581328937065,0.421228179308561,0.43750000000025,0.468750000000241,
0.482453344550044,0.496856148402139,0.500000000000232,0.618014487413222,
0.625000000000166,0.667542699814932,0.711630271843116,0.750000000000099,
0.849282816651991,0.949069247991813,1.),.UNSPECIFIED.);
#1889=B_SPLINE_CURVE_WITH_KNOTS('',5,(#86275,#86276,#86277,#86278,#86279,
#86280),.UNSPECIFIED.,.F.,.F.,(6,6),(0.,1.),.UNSPECIFIED.);
#1890=B_SPLINE_CURVE_WITH_KNOTS('',5,(#86342,#86343,#86344,#86345,#86346,
#86347),.UNSPECIFIED.,.F.,.F.,(6,6),(0.,1.),.UNSPECIFIED.);
#1891=B_SPLINE_CURVE_WITH_KNOTS('',3,(#86350,#86351,#86352,#86353,#86354,
#86355,#86356,#86357,#86358,#86359,#86360,#86361,#86362,#86363,#86364,#86365,
#86366,#86367,#86368,#86369,#86370,#86371,#86372,#86373,#86374,#86375,#86376,
#86377,#86378,#86379,#86380,#86381,#86382,#86383,#86384,#86385,#86386,#86387,
#86388,#86389,#86390,#86391,#86392,#86393,#86394,#86395,#86396,#86397,#86398,
#86399,#86400,#86401,#86402,#86403,#86404,#86405,#86406,#86407,#86408,#86409,
#86410,#86411,#86412,#86413,#86414,#86415,#86416,#86417,#86418,#86419,#86420,
#86421,#86422,#86423,#86424,#86425),.UNSPECIFIED.,.F.,.F.,(4,3,3,3,3,3,
3,3,3,3,3,3,3,3,3,3,3,3,3,3,3,3,3,3,3,4),(0.,0.0979906433443701,0.199916167668728,
0.24999999999997,0.34212271718657,0.374999999999957,0.437499999999956,0.464543924780552,
0.468749999999952,0.483028853555349,0.498667542585192,0.499999999999948,
0.584290236907723,0.624999999999926,0.687499999999915,0.718749999999904,
0.734374999999899,0.742187499999895,0.748091694014882,0.749999999999891,
0.80006377933794,0.850047834503455,0.898722268222934,0.94559281701662,0.989236405049239,
1.),.UNSPECIFIED.);
#1892=B_SPLINE_CURVE_WITH_KNOTS('',3,(#86448,#86449,#86450,#86451,#86452,
#86453,#86454,#86455,#86456,#86457,#86458,#86459,#86460,#86461,#86462,#86463,
#86464,#86465,#86466,#86467,#86468,#86469,#86470,#86471,#86472,#86473,#86474,
#86475,#86476,#86477,#86478,#86479,#86480,#86481,#86482,#86483,#86484,#86485,
#86486,#86487,#86488,#86489,#86490,#86491,#86492,#86493,#86494,#86495,#86496,
#86497,#86498,#86499,#86500,#86501,#86502,#86503,#86504,#86505),
 .UNSPECIFIED.,.F.,.F.,(4,3,3,3,3,3,3,3,3,3,3,3,3,3,3,3,3,3,3,4),(2.86340882221,
2.96038236608017,2.9912183572,3.08700311846,3.18278787972,3.27460804500358,
3.3634673030912,3.3764526533,3.45865940729474,3.54085709160535,3.57484410128,
3.65773122998381,3.67917202515,3.75805208465002,3.78350088337,3.86115067208,
3.93423338613357,3.93880046079,4.01498217619638,4.03947605191),
 .UNSPECIFIED.);
#1893=B_SPLINE_CURVE_WITH_KNOTS('',3,(#86509,#86510,#86511,#86512,#86513,
#86514,#86515,#86516,#86517,#86518,#86519,#86520,#86521,#86522,#86523,#86524,
#86525,#86526,#86527,#86528,#86529,#86530,#86531,#86532,#86533,#86534,#86535,
#86536,#86537,#86538,#86539,#86540,#86541,#86542,#86543,#86544,#86545,#86546,
#86547,#86548,#86549,#86550,#86551,#86552,#86553,#86554,#86555,#86556,#86557,
#86558,#86559,#86560,#86561,#86562,#86563,#86564,#86565,#86566),
 .UNSPECIFIED.,.F.,.F.,(4,3,3,3,3,3,3,3,3,3,3,3,3,3,3,3,3,3,3,4),(4.76185240083,
4.83763310355387,4.8511070755,4.9237368026632,4.94035737066,5.01616912552097,
5.04125309343,5.11983939701062,5.14214350511,5.21975609722012,5.29603838282238,
5.31344541544,5.40219520324995,5.47351631749,5.56538841319371,5.65858597861109,
5.75320413758695,5.78071175361,5.87661154462981,5.93786871511),
 .UNSPECIFIED.);
#1894=B_SPLINE_CURVE_WITH_KNOTS('',3,(#86577,#86578,#86579,#86580,#86581,
#86582,#86583,#86584,#86585,#86586,#86587,#86588,#86589,#86590,#86591,#86592,
#86593,#86594,#86595,#86596,#86597,#86598,#86599,#86600,#86601,#86602,#86603,
#86604,#86605,#86606,#86607,#86608,#86609,#86610,#86611,#86612,#86613,#86614,
#86615,#86616),.UNSPECIFIED.,.F.,.F.,(4,3,3,3,3,3,3,3,3,3,3,3,3,4),(1.69812247662,
1.82517827643346,1.94835352449351,2.04354239572,2.1493981491557,2.2504202018726,
2.34618007075805,2.37608580106,2.46390218046495,2.55211800019734,2.6379844451379,
2.6897944832,2.77017696446133,2.83469359842),.UNSPECIFIED.);
#1895=B_SPLINE_CURVE_WITH_KNOTS('',3,(#86634,#86635,#86636,#86637,#86638,
#86639,#86640,#86641,#86642,#86643,#86644,#86645,#86646,#86647,#86648,#86649,
#86650,#86651,#86652,#86653,#86654,#86655,#86656,#86657,#86658,#86659,#86660,
#86661,#86662,#86663,#86664,#86665,#86666,#86667,#86668,#86669,#86670,#86671,
#86672,#86673),.UNSPECIFIED.,.F.,.F.,(4,3,3,3,3,3,3,3,3,3,3,3,3,4),(9.16642701788228E-11,
0.0777685045691623,0.155298490954937,0.235788513859965,0.249999999999996,
0.374999999999999,0.425782059261454,0.476666286858019,0.492264924606089,
0.500315380842036,0.647629842965568,0.788859013702841,0.917371668501292,
1.),.UNSPECIFIED.);
#1896=B_SPLINE_CURVE_WITH_KNOTS('',3,(#86689,#86690,#86691,#86692,#86693,
#86694,#86695,#86696,#86697,#86698,#86699,#86700,#86701,#86702,#86703,#86704,
#86705,#86706,#86707,#86708,#86709,#86710,#86711,#86712,#86713,#86714,#86715,
#86716,#86717,#86718,#86719,#86720,#86721,#86722,#86723,#86724,#86725,#86726,
#86727,#86728),.UNSPECIFIED.,.F.,.F.,(4,3,3,3,3,3,3,3,3,3,3,3,3,4),(0.,
0.0777737453085021,0.155308734732268,0.235802705737845,0.250000000000003,
0.375000000000003,0.425780378411465,0.476662994638966,0.49226568581941,
0.500315400257842,0.647633193305892,0.788863146805967,0.917372111358519,
1.),.UNSPECIFIED.);
#1897=B_SPLINE_CURVE_WITH_KNOTS('',5,(#86737,#86738,#86739,#86740,#86741,
#86742),.UNSPECIFIED.,.F.,.F.,(6,6),(-1.1089775272,-1.0735101225),
 .UNSPECIFIED.);
#1898=B_SPLINE_CURVE_WITH_KNOTS('',5,(#86802,#86803,#86804,#86805,#86806,
#86807),.UNSPECIFIED.,.F.,.F.,(6,6),(0.,1.),.UNSPECIFIED.);
#1899=B_SPLINE_CURVE_WITH_KNOTS('',3,(#86921,#86922,#86923,#86924),
 .UNSPECIFIED.,.F.,.F.,(4,4),(-1.1089775272,-1.07351012327562),
 .UNSPECIFIED.);
#1900=B_SPLINE_CURVE_WITH_KNOTS('',3,(#87010,#87011,#87012,#87013,#87014,
#87015,#87016,#87017,#87018,#87019,#87020,#87021,#87022,#87023,#87024,#87025,
#87026,#87027,#87028,#87029,#87030,#87031,#87032,#87033,#87034,#87035,#87036,
#87037),.UNSPECIFIED.,.F.,.F.,(4,3,3,3,3,3,3,3,3,4),(1.39576967731014E-10,
0.1505103555998,0.288268426485318,0.376933003975363,0.503523155116763,0.532699752981522,
0.664316984007422,0.802626544765739,0.950088550067854,1.),.UNSPECIFIED.);
#1901=B_SPLINE_CURVE_WITH_KNOTS('',3,(#87169,#87170,#87171,#87172,#87173,
#87174,#87175,#87176,#87177,#87178,#87179,#87180,#87181,#87182,#87183,#87184,
#87185,#87186,#87187,#87188,#87189,#87190,#87191,#87192,#87193,#87194,#87195,
#87196),.UNSPECIFIED.,.F.,.F.,(4,3,3,3,3,3,3,3,3,4),(3.99334178330209E-9,
0.150506684297317,0.288263057281987,0.376930108117779,0.503520614101364,
0.532697581088335,0.664314707972964,0.802621307209367,0.950075916205342,
1.),.UNSPECIFIED.);
#1902=B_SPLINE_CURVE_WITH_KNOTS('',3,(#87293,#87294,#87295,#87296,#87297,
#87298,#87299,#87300,#87301,#87302,#87303,#87304,#87305,#87306,#87307,#87308,
#87309,#87310,#87311,#87312,#87313,#87314,#87315,#87316,#87317,#87318,#87319,
#87320,#87321,#87322,#87323,#87324,#87325,#87326,#87327,#87328,#87329,#87330,
#87331,#87332,#87333,#87334,#87335,#87336,#87337,#87338,#87339,#87340,#87341,
#87342,#87343,#87344,#87345,#87346,#87347,#87348,#87349,#87350,#87351,#87352,
#87353,#87354,#87355,#87356,#87357,#87358,#87359,#87360,#87361,#87362,#87363,
#87364,#87365,#87366,#87367,#87368,#87369,#87370,#87371),.UNSPECIFIED.,
 .F.,.F.,(4,3,3,3,3,3,3,3,3,3,3,3,3,3,3,3,3,3,3,3,3,3,3,3,3,3,4),(0.,0.0355362144885678,
0.0624999999999996,0.0937499999999993,0.107276596424941,0.120331439252964,
0.124999999999999,0.163762141652132,0.203173805928779,0.244559237814547,
0.249999999999999,0.325460882975541,0.375,0.415174481039151,0.457587240519576,
0.497815749000596,0.5,0.552880648155298,0.608960672555796,0.625,0.675510724434953,
0.724578356810552,0.750000000000001,0.809241727425364,0.871851356636048,
0.935925678318024,1.),.UNSPECIFIED.);
#1903=B_SPLINE_CURVE_WITH_KNOTS('',3,(#87376,#87377,#87378,#87379,#87380,
#87381,#87382,#87383,#87384,#87385,#87386,#87387,#87388,#87389,#87390,#87391,
#87392,#87393,#87394,#87395,#87396,#87397,#87398,#87399,#87400,#87401,#87402,
#87403,#87404,#87405,#87406,#87407,#87408,#87409,#87410,#87411,#87412,#87413,
#87414,#87415,#87416,#87417,#87418,#87419,#87420,#87421,#87422,#87423,#87424,
#87425,#87426,#87427,#87428,#87429,#87430,#87431,#87432,#87433,#87434,#87435,
#87436),.UNSPECIFIED.,.F.,.F.,(4,3,3,3,3,3,3,3,3,3,3,3,3,3,3,3,3,3,3,3,
4),(0.,0.124999999999991,0.242509431927007,0.249999999999983,0.364359301276675,
0.374999999999985,0.422328004362009,0.469735704085969,0.499999999999987,
0.585785621366277,0.624999999999989,0.687499999999998,0.718749999999998,
0.732488337520169,0.74772746595688,0.749999999999999,0.812499999999999,
0.869532237334179,0.924605486450739,0.976916884333088,1.),.UNSPECIFIED.);
#1904=B_SPLINE_CURVE_WITH_KNOTS('',3,(#87443,#87444,#87445,#87446,#87447,
#87448,#87449,#87450,#87451,#87452,#87453,#87454,#87455,#87456,#87457,#87458,
#87459,#87460,#87461,#87462,#87463,#87464,#87465,#87466,#87467,#87468,#87469,
#87470,#87471,#87472,#87473,#87474,#87475,#87476,#87477,#87478,#87479,#87480,
#87481,#87482,#87483,#87484,#87485,#87486,#87487,#87488,#87489,#87490,#87491,
#87492,#87493,#87494,#87495,#87496,#87497,#87498,#87499,#87500,#87501,#87502,
#87503,#87504,#87505,#87506,#87507,#87508,#87509,#87510,#87511,#87512,#87513,
#87514,#87515,#87516,#87517,#87518,#87519,#87520,#87521,#87522,#87523,#87524,
#87525,#87526,#87527,#87528,#87529,#87530,#87531,#87532,#87533,#87534,#87535,
#87536,#87537,#87538,#87539,#87540,#87541,#87542),.UNSPECIFIED.,.F.,.F.,
(4,3,3,3,3,3,3,3,3,3,3,3,3,3,3,3,3,3,3,3,3,3,3,3,3,3,3,3,3,3,3,3,3,4),(0.,
0.0958472142403171,0.183853112222453,0.249999999999939,0.374999999999948,
0.437499999999953,0.469467566143704,0.49837783867004,0.499999999999958,
0.5841637537743,0.624999999999968,0.687499999999974,0.718749999999991,0.734374999999999,
0.744227145958902,0.750000000000008,0.78820713890752,0.812499999999997,
0.843749999999993,0.859374999999992,0.867187499999991,0.87441427028628,
0.87499999999999,0.896435606631704,0.906249999999993,0.921874999999993,
0.929687499999994,0.933825830539164,0.937499999999995,0.951631947114754,
0.965077849015114,0.978069978143163,0.990363804263242,1.),.UNSPECIFIED.);
#1905=B_SPLINE_CURVE_WITH_KNOTS('',3,(#87555,#87556,#87557,#87558,#87559,
#87560,#87561,#87562,#87563,#87564,#87565,#87566,#87567,#87568,#87569,#87570,
#87571,#87572,#87573,#87574,#87575,#87576,#87577,#87578,#87579,#87580,#87581,
#87582,#87583,#87584,#87585,#87586,#87587,#87588,#87589,#87590,#87591,#87592,
#87593,#87594,#87595,#87596,#87597,#87598,#87599,#87600,#87601,#87602,#87603,
#87604,#87605,#87606,#87607,#87608,#87609,#87610,#87611,#87612,#87613,#87614,
#87615,#87616,#87617,#87618,#87619,#87620,#87621,#87622,#87623,#87624,#87625,
#87626,#87627),.UNSPECIFIED.,.F.,.F.,(4,3,3,3,3,3,3,3,3,3,3,3,3,3,3,3,3,
3,3,3,3,3,3,3,4),(0.,0.0966099788589137,0.125000000000007,0.17130877196425,
0.215592241170992,0.250000000000015,0.361544036934436,0.375000000000022,
0.437500000000026,0.465511784233522,0.492096554438188,0.50000000000003,
0.57608153399594,0.62500000000002,0.687500000000008,0.718750000000006,0.733471387992378,
0.749161313096158,0.750000000000005,0.799727105623058,0.849795329217294,
0.894862691334285,0.93837411729665,0.979784735280439,1.),.UNSPECIFIED.);
#1906=B_SPLINE_CURVE_WITH_KNOTS('',3,(#87689,#87690,#87691,#87692,#87693,
#87694,#87695,#87696,#87697,#87698,#87699,#87700,#87701,#87702,#87703,#87704,
#87705,#87706,#87707,#87708,#87709,#87710,#87711,#87712,#87713,#87714,#87715,
#87716,#87717,#87718),.UNSPECIFIED.,.F.,.F.,(4,2,2,1,1,2,2,2,1,1,2,2,2,
1,1,2,2,4),(0.,0.124999999999985,0.187499999999977,0.218749999999974,0.234374999999974,
0.242187499999973,0.249999999999972,0.374999999999976,0.437499999999979,
0.468749999999981,0.484374999999981,0.499999999999982,0.624999999999999,
0.687500000000007,0.718750000000012,0.734375000000014,0.750000000000015,
1.),.UNSPECIFIED.);
#1907=B_SPLINE_CURVE_WITH_KNOTS('',5,(#87719,#87720,#87721,#87722,#87723,
#87724),.UNSPECIFIED.,.F.,.F.,(6,6),(0.,1.),.UNSPECIFIED.);
#1908=B_SPLINE_CURVE_WITH_KNOTS('',3,(#87738,#87739,#87740,#87741,#87742,
#87743,#87744,#87745,#87746,#87747,#87748,#87749,#87750,#87751,#87752,#87753,
#87754,#87755,#87756,#87757,#87758,#87759,#87760,#87761,#87762,#87763,#87764,
#87765,#87766,#87767,#87768,#87769,#87770,#87771,#87772,#87773,#87774,#87775,
#87776,#87777,#87778,#87779,#87780,#87781,#87782,#87783,#87784,#87785,#87786,
#87787,#87788,#87789,#87790,#87791,#87792,#87793,#87794,#87795),
 .UNSPECIFIED.,.F.,.F.,(4,3,3,3,3,3,3,3,3,3,3,3,3,3,3,3,3,3,3,4),(0.,0.100609639419896,
0.200720123081653,0.249999999999981,0.32470459539465,0.398051288913321,
0.468246679183588,0.499999999999963,0.581413825455905,0.624999999999953,
0.687499999999949,0.718749999999946,0.732699964043024,0.747947399939569,
0.749999999999944,0.805776737616528,0.858544229418813,0.909482024872923,
0.9576486572329,1.),.UNSPECIFIED.);
#1909=B_SPLINE_CURVE_WITH_KNOTS('',3,(#87819,#87820,#87821,#87822,#87823,
#87824,#87825,#87826,#87827,#87828,#87829,#87830,#87831,#87832,#87833,#87834,
#87835,#87836,#87837,#87838,#87839,#87840,#87841,#87842,#87843,#87844,#87845,
#87846,#87847,#87848,#87849,#87850,#87851,#87852,#87853,#87854,#87855,#87856,
#87857,#87858,#87859,#87860,#87861,#87862,#87863,#87864,#87865,#87866,#87867,
#87868,#87869,#87870,#87871,#87872,#87873,#87874,#87875,#87876,#87877,#87878,
#87879,#87880,#87881,#87882,#87883,#87884,#87885,#87886,#87887,#87888,#87889,
#87890,#87891,#87892,#87893,#87894,#87895,#87896,#87897,#87898,#87899,#87900,
#87901,#87902,#87903,#87904,#87905,#87906,#87907,#87908,#87909),
 .UNSPECIFIED.,.F.,.F.,(4,3,3,3,3,3,3,3,3,3,3,3,3,3,3,3,3,3,3,3,3,3,3,3,
3,3,3,3,3,3,4),(0.,0.0397814237123525,0.0877360660119328,0.124999999999976,
0.165730845336603,0.187499999999964,0.218749999999958,0.234374999999955,
0.242187499999953,0.247641935945892,0.249999999999951,0.267411966703376,
0.322992096802285,0.374999999999974,0.411075296464987,0.437499999999989,
0.468749999999994,0.484374999999995,0.492187499999993,0.498855130311395,
0.499999999999992,0.567142758786176,0.624999999999997,0.687499999999998,
0.718742348599412,0.723042232423563,0.749999999999999,0.817189597240934,
0.893554069690658,0.97480672873194,1.),.UNSPECIFIED.);
#1910=B_SPLINE_CURVE_WITH_KNOTS('',3,(#87915,#87916,#87917,#87918,#87919,
#87920,#87921,#87922,#87923,#87924,#87925,#87926,#87927,#87928,#87929,#87930,
#87931,#87932,#87933,#87934,#87935,#87936,#87937,#87938,#87939,#87940,#87941,
#87942,#87943,#87944,#87945,#87946,#87947,#87948,#87949,#87950,#87951,#87952,
#87953,#87954,#87955,#87956,#87957,#87958,#87959,#87960,#87961,#87962,#87963,
#87964,#87965,#87966,#87967,#87968,#87969,#87970,#87971,#87972),
 .UNSPECIFIED.,.F.,.F.,(4,3,3,3,3,3,3,3,3,3,3,3,3,3,3,3,3,3,3,4),(0.,0.0356451281179679,
0.0693279121910458,0.100412016848408,0.125000000000114,0.161875456310924,
0.187500000000171,0.2187500000002,0.234375000000204,0.243649194272616,0.250000000000208,
0.30872348200964,0.371020762472332,0.437204595886178,0.500000000000135,
0.5983757256371,0.703843588454204,0.81350499211572,0.93003274416397,1.),
 .UNSPECIFIED.);
#1911=B_SPLINE_CURVE_WITH_KNOTS('',3,(#87992,#87993,#87994,#87995,#87996,
#87997,#87998,#87999,#88000,#88001,#88002,#88003,#88004,#88005,#88006,#88007,
#88008,#88009,#88010,#88011,#88012,#88013,#88014,#88015,#88016,#88017,#88018,
#88019,#88020,#88021,#88022,#88023,#88024,#88025),.UNSPECIFIED.,.F.,.F.,
(4,3,3,3,3,3,3,3,3,3,3,4),(1.25405163269,1.32643264163,1.4055803165725,
1.48574465294545,1.56752327448427,1.6430233414,1.72858124378027,1.81406569145,
1.90733041601598,1.99715560017,2.09477370437,2.19239180857),
 .UNSPECIFIED.);
#1912=B_SPLINE_CURVE_WITH_KNOTS('',3,(#88081,#88082,#88083,#88084,#88085,
#88086,#88087,#88088,#88089,#88090,#88091,#88092,#88093,#88094,#88095,#88096,
#88097,#88098,#88099,#88100,#88101,#88102,#88103,#88104,#88105,#88106,#88107,
#88108,#88109,#88110,#88111,#88112,#88113,#88114,#88115,#88116,#88117,#88118,
#88119,#88120,#88121,#88122,#88123),.UNSPECIFIED.,.F.,.F.,(4,3,3,3,3,3,
3,3,3,3,3,3,3,3,4),(4.39679769916515E-10,0.0896494939985405,0.177741271167206,
0.265221869705284,0.352748440567542,0.43623682229533,0.506707219508413,
0.574976714664183,0.643034716691638,0.710667694098751,0.77742624196382,
0.842035244579551,0.905067000126942,0.965268347329118,1.),.UNSPECIFIED.);
#1913=B_SPLINE_CURVE_WITH_KNOTS('',3,(#88183,#88184,#88185,#88186,#88187,
#88188,#88189,#88190,#88191,#88192,#88193,#88194,#88195,#88196,#88197,#88198,
#88199,#88200,#88201,#88202,#88203,#88204,#88205,#88206,#88207,#88208,#88209,
#88210,#88211,#88212,#88213,#88214,#88215,#88216,#88217,#88218,#88219,#88220,
#88221,#88222),.UNSPECIFIED.,.F.,.F.,(4,3,3,3,3,3,3,3,3,3,3,3,3,4),(0.,
0.0586293965389953,0.118458772750461,0.181450715788032,0.248647653214792,
0.323992525315228,0.399761183556369,0.469035172311963,0.559603022429232,
0.654066796784159,0.752582807186012,0.8505413511493,0.944145001536187,1.),
 .UNSPECIFIED.);
#1914=B_SPLINE_CURVE_WITH_KNOTS('',5,(#88305,#88306,#88307,#88308,#88309,
#88310,#88311,#88312,#88313),.UNSPECIFIED.,.F.,.F.,(6,3,6),(0.,0.446748477147653,
1.),.UNSPECIFIED.);
#1915=B_SPLINE_CURVE_WITH_KNOTS('',3,(#88316,#88317,#88318,#88319,#88320,
#88321,#88322,#88323,#88324,#88325,#88326,#88327,#88328,#88329,#88330,#88331,
#88332,#88333,#88334,#88335,#88336,#88337,#88338,#88339,#88340,#88341,#88342,
#88343,#88344,#88345,#88346,#88347,#88348,#88349,#88350,#88351,#88352,#88353,
#88354,#88355),.UNSPECIFIED.,.F.,.F.,(4,3,3,3,3,3,3,3,3,3,3,3,3,4),(1.81673175559521E-10,
0.0836057555609339,0.174429967985735,0.268968220557755,0.366735443263493,
0.446902605260138,0.500000000000001,0.597735980402653,0.707686006743452,
0.75,0.824579319188729,0.899060478571651,0.971802328054873,1.),
 .UNSPECIFIED.);
#1916=B_SPLINE_CURVE_WITH_KNOTS('',3,(#88364,#88365,#88366,#88367,#88368,
#88369,#88370,#88371,#88372,#88373,#88374,#88375,#88376,#88377,#88378,#88379,
#88380,#88381,#88382,#88383,#88384,#88385,#88386),.UNSPECIFIED.,.F.,.F.,
(4,2,2,2,3,2,2,2,2,2,4),(0.223210461888191,0.223397147217863,0.223717290566587,
0.224391037089802,0.228125629041838,0.234943871134553,0.243585952736414,
0.25309083829967,0.263261316553702,0.27431000560614,0.277820240597038),
 .UNSPECIFIED.);
#1917=B_SPLINE_CURVE_WITH_KNOTS('',3,(#88401,#88402,#88403,#88404,#88405,
#88406,#88407,#88408,#88409,#88410,#88411,#88412,#88413,#88414,#88415,#88416),
 .UNSPECIFIED.,.F.,.F.,(4,2,2,2,2,2,2,4),(0.0329698156679733,0.0333695174810278,
0.0386982857933801,0.0439884179233323,0.0499284327972441,0.0577713467846448,
0.0633464558735427,0.0721131672795402),.UNSPECIFIED.);
#1918=B_SPLINE_CURVE_WITH_KNOTS('',3,(#88418,#88419,#88420,#88421,#88422,
#88423,#88424,#88425,#88426,#88427),.UNSPECIFIED.,.F.,.F.,(4,2,2,2,4),(0.271351380209749,
0.293031113526595,0.302969887271488,0.308596889767683,0.311849694512603),
 .UNSPECIFIED.);
#1919=B_SPLINE_CURVE_WITH_KNOTS('',3,(#88520,#88521,#88522,#88523,#88524,
#88525,#88526,#88527,#88528,#88529,#88530,#88531,#88532,#88533,#88534,#88535,
#88536,#88537,#88538,#88539,#88540,#88541,#88542,#88543,#88544,#88545,#88546,
#88547,#88548,#88549,#88550,#88551,#88552,#88553,#88554,#88555,#88556,#88557,
#88558,#88559,#88560,#88561,#88562,#88563,#88564,#88565,#88566,#88567,#88568,
#88569,#88570,#88571,#88572,#88573,#88574,#88575,#88576,#88577),
 .UNSPECIFIED.,.F.,.F.,(4,3,3,3,3,3,3,3,3,3,3,3,3,3,3,3,3,3,3,4),(0.,0.0897308056971427,
0.179444739745368,0.250000000000193,0.336421147132234,0.375000000000287,
0.437500000000334,0.468750000000357,0.484375000000361,0.493366966257959,
0.500000000000365,0.607568988871737,0.625000000000288,0.687500000000249,
0.714210713960481,0.742118754756523,0.750000000000211,0.864717251909047,
0.990112105797021,1.),.UNSPECIFIED.);
#1920=B_SPLINE_CURVE_WITH_KNOTS('',3,(#88604,#88605,#88606,#88607,#88608,
#88609,#88610,#88611,#88612,#88613,#88614,#88615,#88616,#88617,#88618,#88619,
#88620,#88621,#88622,#88623,#88624,#88625,#88626,#88627,#88628,#88629,#88630,
#88631,#88632,#88633,#88634,#88635,#88636,#88637,#88638,#88639,#88640,#88641,
#88642,#88643,#88644,#88645,#88646,#88647,#88648,#88649,#88650,#88651,#88652,
#88653,#88654,#88655,#88656,#88657,#88658,#88659,#88660,#88661,#88662,#88663,
#88664,#88665,#88666,#88667,#88668,#88669,#88670,#88671,#88672,#88673,#88674,
#88675,#88676,#88677,#88678,#88679,#88680,#88681,#88682),.UNSPECIFIED.,
 .F.,.F.,(4,3,3,3,3,3,3,3,3,3,3,3,3,3,3,3,3,3,3,3,3,3,3,3,3,3,4),(0.,0.0355771815476919,
0.0624999999999976,0.0937499999999986,0.10728274018591,0.120341032646476,
0.125,0.16393206809617,0.203518656130192,0.245075225467878,0.250000000000004,
0.32548942661256,0.375000000000008,0.415134282467528,0.45756714123377,0.497745693090781,
0.500000000000012,0.552904193134679,0.60901082343741,0.625000000000016,
0.675540464737087,0.72463970904679,0.75000000000002,0.809244134152876,0.871848389017905,
0.935924194508953,1.),.UNSPECIFIED.);
#1921=B_SPLINE_CURVE_WITH_KNOTS('',3,(#88721,#88722,#88723,#88724,#88725,
#88726,#88727,#88728,#88729,#88730,#88731,#88732,#88733,#88734,#88735,#88736,
#88737,#88738,#88739,#88740,#88741,#88742,#88743,#88744,#88745,#88746,#88747,
#88748,#88749,#88750,#88751,#88752,#88753,#88754,#88755,#88756,#88757,#88758,
#88759,#88760,#88761,#88762,#88763,#88764,#88765,#88766,#88767,#88768,#88769),
 .UNSPECIFIED.,.F.,.F.,(4,3,3,3,3,3,3,3,3,3,3,3,3,3,3,3,4),(0.,0.0648620446179728,
0.132474572992778,0.205862839558522,0.25,0.336375995977143,0.420555151483361,
0.5,0.569903495187839,0.636422109127358,0.69901012047123,0.75,0.80922275929286,
0.866139446326761,0.921929236615715,0.976271344364284,1.),.UNSPECIFIED.);
#1922=B_SPLINE_CURVE_WITH_KNOTS('',3,(#88771,#88772,#88773,#88774,#88775,
#88776,#88777,#88778,#88779,#88780,#88781,#88782,#88783,#88784,#88785,#88786,
#88787,#88788,#88789,#88790,#88791,#88792,#88793,#88794,#88795,#88796,#88797,
#88798,#88799,#88800,#88801,#88802,#88803,#88804,#88805,#88806,#88807,#88808,
#88809,#88810,#88811,#88812,#88813,#88814,#88815,#88816,#88817,#88818,#88819,
#88820,#88821,#88822),.UNSPECIFIED.,.F.,.F.,(4,3,3,3,3,3,3,3,3,3,3,3,3,
3,3,3,3,4),(0.,0.0899334399923707,0.179889344622198,0.250000000000184,0.33993343999114,
0.375000000000275,0.437500000000322,0.468750000000345,0.484375000000349,
0.493754678879357,0.500000000000354,0.625000000000273,0.687500000000233,
0.716107443505401,0.746125713318513,0.750000000000193,0.922212000166891,
1.),.UNSPECIFIED.);
#1923=B_SPLINE_CURVE_WITH_KNOTS('',3,(#88877,#88878,#88879,#88880,#88881,
#88882,#88883,#88884,#88885,#88886,#88887,#88888,#88889,#88890,#88891,#88892,
#88893,#88894,#88895,#88896,#88897,#88898,#88899,#88900,#88901,#88902,#88903,
#88904,#88905,#88906,#88907,#88908,#88909,#88910,#88911,#88912,#88913,#88914,
#88915,#88916,#88917,#88918,#88919,#88920,#88921,#88922,#88923,#88924,#88925,
#88926,#88927,#88928,#88929,#88930,#88931,#88932,#88933,#88934,#88935,#88936,
#88937,#88938,#88939,#88940,#88941,#88942,#88943,#88944,#88945,#88946,#88947,
#88948,#88949,#88950,#88951,#88952),.UNSPECIFIED.,.F.,.F.,(4,3,3,3,3,3,
3,3,3,3,3,3,3,3,3,3,3,3,3,3,3,3,3,3,3,4),(0.,0.0242541900995737,0.0494242354737045,
0.0625000000000132,0.0881719402073255,0.0937500000000197,0.109375000000023,
0.117187500000025,0.125000000000026,0.175610976137408,0.18750000000002,
0.218750000000019,0.232039870493069,0.245916517104364,0.250000000000018,
0.326620952260722,0.375000000000008,0.437500000000007,0.464652777920398,
0.493263921870045,0.500000000000005,0.592910275330305,0.68947296384216,
0.79016606190966,0.89508303095483,1.),.UNSPECIFIED.);
#1924=B_SPLINE_CURVE_WITH_KNOTS('',4,(#88961,#88962,#88963,#88964,#88965),
 .UNSPECIFIED.,.F.,.F.,(5,5),(0.,1.),.UNSPECIFIED.);
#1925=B_SPLINE_CURVE_WITH_KNOTS('',3,(#89095,#89096,#89097,#89098,#89099,
#89100,#89101,#89102,#89103,#89104,#89105,#89106,#89107,#89108,#89109,#89110,
#89111,#89112,#89113,#89114,#89115,#89116,#89117,#89118,#89119,#89120,#89121,
#89122,#89123,#89124,#89125,#89126,#89127,#89128,#89129,#89130,#89131,#89132,
#89133,#89134,#89135,#89136,#89137,#89138,#89139,#89140,#89141,#89142,#89143,
#89144,#89145,#89146,#89147,#89148,#89149,#89150,#89151,#89152,#89153,#89154,
#89155,#89156,#89157,#89158),.UNSPECIFIED.,.F.,.F.,(4,3,3,3,3,3,3,3,3,3,
3,3,3,3,3,3,3,3,3,3,3,4),(0.,0.0770514482651851,0.124999999999956,0.187499999999936,
0.218749999999927,0.234374999999922,0.242981604744465,0.249999999999918,
0.349959099836821,0.374999999999869,0.437499999999847,0.468749999999839,
0.484374999999837,0.492187499999836,0.49913066454904,0.499999999999836,
0.599155572574395,0.699366679430796,0.788911175184783,0.875447489871574,
0.957947680405176,1.),.UNSPECIFIED.);
#1926=B_SPLINE_CURVE_WITH_KNOTS('',3,(#89235,#89236,#89237,#89238,#89239,
#89240,#89241,#89242,#89243,#89244,#89245,#89246,#89247,#89248,#89249,#89250,
#89251,#89252,#89253,#89254,#89255,#89256,#89257,#89258,#89259,#89260,#89261,
#89262,#89263,#89264,#89265,#89266,#89267,#89268,#89269,#89270,#89271,#89272,
#89273,#89274,#89275,#89276,#89277,#89278,#89279,#89280,#89281,#89282,#89283,
#89284,#89285,#89286,#89287,#89288,#89289,#89290,#89291,#89292,#89293,#89294,
#89295,#89296,#89297,#89298,#89299,#89300,#89301,#89302,#89303,#89304,#89305,
#89306,#89307,#89308,#89309,#89310,#89311,#89312,#89313),.UNSPECIFIED.,
 .F.,.F.,(4,3,3,3,3,3,3,3,3,3,3,3,3,3,3,3,3,3,3,3,3,3,3,3,3,3,4),(0.,0.0229442921754058,
0.0473003732270936,0.0624999999999992,0.124999999999998,0.201744637631312,
0.249999999999976,0.273460893851431,0.298548973900594,0.312499999999973,
0.37499999999997,0.458890962622535,0.499232024585504,0.499999999999961,
0.525549380903742,0.551794820739131,0.562499999999962,0.624999999999963,
0.687812610496059,0.749999999999973,0.772533298335757,0.796386956349032,
0.809112771577217,0.815844489583874,0.907922244791937,0.984801127701866,
1.),.UNSPECIFIED.);
#1927=B_SPLINE_CURVE_WITH_KNOTS('',5,(#89427,#89428,#89429,#89430,#89431,
#89432,#89433,#89434,#89435),.UNSPECIFIED.,.F.,.F.,(6,3,6),(0.,0.414531657823574,
1.),.UNSPECIFIED.);
#1928=B_SPLINE_CURVE_WITH_KNOTS('',5,(#89495,#89496,#89497,#89498,#89499,
#89500,#89501,#89502,#89503),.UNSPECIFIED.,.F.,.F.,(6,3,6),(0.,0.596498812468772,
1.),.UNSPECIFIED.);
#1929=B_SPLINE_CURVE_WITH_KNOTS('',3,(#89544,#89545,#89546,#89547,#89548,
#89549,#89550,#89551,#89552,#89553,#89554,#89555,#89556,#89557,#89558,#89559,
#89560,#89561,#89562,#89563,#89564,#89565,#89566,#89567,#89568,#89569,#89570,
#89571,#89572,#89573,#89574),.UNSPECIFIED.,.F.,.F.,(4,3,3,3,3,3,3,3,3,3,
4),(0.,0.113410126173201,0.231212941658119,0.348973287565832,0.464312568640331,
0.575973606578693,0.68198020493402,0.784775801213408,0.884955399662714,
0.981955778398047,1.),.UNSPECIFIED.);
#1930=B_SPLINE_CURVE_WITH_KNOTS('',3,(#89576,#89577,#89578,#89579,#89580,
#89581,#89582,#89583,#89584,#89585,#89586,#89587,#89588,#89589,#89590,#89591,
#89592,#89593,#89594,#89595,#89596,#89597,#89598,#89599,#89600,#89601,#89602,
#89603,#89604,#89605,#89606,#89607,#89608,#89609,#89610,#89611,#89612,#89613,
#89614,#89615,#89616,#89617,#89618,#89619,#89620,#89621),.UNSPECIFIED.,
 .F.,.F.,(4,3,3,3,3,3,3,3,3,3,3,3,3,3,3,4),(0.,0.0726706660714167,0.146103743511138,
0.220234233777271,0.294302581364791,0.36741929699253,0.43789481134854,0.499999999999996,
0.562499999999997,0.624791030327762,0.68739551516388,0.749999999999998,
0.819280964853742,0.888670436886782,0.956283877925322,1.),.UNSPECIFIED.);
#1931=B_SPLINE_CURVE_WITH_KNOTS('',3,(#89629,#89630,#89631,#89632,#89633,
#89634,#89635,#89636,#89637,#89638),.UNSPECIFIED.,.F.,.F.,(4,3,3,4),(0.,
0.1405201788765,0.24888377189969,0.281040357753),.UNSPECIFIED.);
#1932=B_SPLINE_CURVE_WITH_KNOTS('',3,(#89640,#89641,#89642,#89643,#89644,
#89645,#89646,#89647,#89648,#89649),.UNSPECIFIED.,.F.,.F.,(4,3,3,4),(0.,
0.143504699996,0.239445459249327,0.287009399992),.UNSPECIFIED.);
#1933=B_SPLINE_CURVE_WITH_KNOTS('',5,(#89708,#89709,#89710,#89711,#89712,
#89713,#89714,#89715,#89716),.UNSPECIFIED.,.F.,.F.,(6,3,6),(0.,0.446990882614049,
1.),.UNSPECIFIED.);
#1934=B_SPLINE_CURVE_WITH_KNOTS('',3,(#89717,#89718,#89719,#89720,#89721,
#89722,#89723,#89724,#89725,#89726,#89727,#89728,#89729,#89730,#89731,#89732,
#89733,#89734,#89735,#89736,#89737,#89738,#89739,#89740,#89741,#89742,#89743,
#89744,#89745,#89746,#89747),.UNSPECIFIED.,.F.,.F.,(4,3,3,3,3,3,3,3,3,3,
4),(0.,0.103606039248823,0.209200414240004,0.317311627182045,0.426434884947521,
0.535929191910951,0.645077668364686,0.752572851887125,0.858664995979,0.962443523493216,
0.99999999982195),.UNSPECIFIED.);
#1935=B_SPLINE_CURVE_WITH_KNOTS('',3,(#89896,#89897,#89898,#89899,#89900,
#89901,#89902,#89903,#89904,#89905,#89906,#89907,#89908,#89909,#89910,#89911,
#89912,#89913,#89914,#89915,#89916,#89917,#89918,#89919,#89920,#89921,#89922,
#89923,#89924,#89925,#89926,#89927,#89928,#89929,#89930,#89931,#89932,#89933,
#89934,#89935,#89936,#89937,#89938,#89939,#89940,#89941,#89942,#89943,#89944,
#89945,#89946,#89947,#89948,#89949,#89950,#89951,#89952,#89953,#89954,#89955,
#89956,#89957,#89958,#89959),.UNSPECIFIED.,.F.,.F.,(4,3,3,3,3,3,3,3,3,3,
3,3,3,3,3,3,3,3,3,3,3,4),(0.,0.0373481272818948,0.0788425197254873,0.126446182104601,
0.184791907568511,0.249999999999852,0.345027571690437,0.37499999999978,
0.437499999999744,0.46874999999973,0.484374999999732,0.492187499999735,
0.496093749999737,0.499999999999739,0.558498464864831,0.635836688781905,
0.709773405775254,0.774182065715002,0.837817143450719,0.903585214268584,
0.976677578999226,1.),.UNSPECIFIED.);
#1936=B_SPLINE_CURVE_WITH_KNOTS('',3,(#90034,#90035,#90036,#90037,#90038,
#90039,#90040,#90041,#90042,#90043,#90044,#90045,#90046,#90047,#90048,#90049,
#90050,#90051,#90052,#90053,#90054,#90055,#90056,#90057,#90058,#90059,#90060,
#90061,#90062,#90063,#90064,#90065,#90066,#90067,#90068,#90069,#90070,#90071,
#90072,#90073,#90074,#90075,#90076,#90077,#90078,#90079,#90080,#90081,#90082,
#90083,#90084,#90085,#90086,#90087,#90088),.UNSPECIFIED.,.F.,.F.,(4,3,3,
3,3,3,3,3,3,3,3,3,3,3,3,3,3,3,4),(0.,0.098399225567126,0.19657706045254,
0.249999999999997,0.352225838661693,0.374999999999982,0.437499999999986,
0.465071769090119,0.493567955054625,0.499999999999991,0.572560372932883,
0.642387385962301,0.708319172777275,0.749999999999995,0.812499999999996,
0.873077503807693,0.932131369198034,0.989328858099031,1.),.UNSPECIFIED.);
#1937=B_SPLINE_CURVE_WITH_KNOTS('',3,(#90094,#90095,#90096,#90097,#90098,
#90099,#90100,#90101,#90102,#90103,#90104,#90105,#90106,#90107,#90108,#90109,
#90110,#90111,#90112,#90113,#90114,#90115,#90116,#90117,#90118,#90119,#90120,
#90121,#90122,#90123,#90124,#90125,#90126,#90127,#90128,#90129,#90130,#90131,
#90132,#90133,#90134,#90135,#90136,#90137,#90138,#90139,#90140,#90141,#90142,
#90143,#90144,#90145,#90146,#90147,#90148),.UNSPECIFIED.,.F.,.F.,(4,3,3,
3,3,3,3,3,3,3,3,3,3,3,3,3,3,3,4),(0.,0.0982911914765156,0.196374277996715,
0.249999999999955,0.352161291291609,0.374999999999919,0.437499999999913,
0.46516384899836,0.49374496091657,0.499999999999907,0.572485440727802,0.642240217270967,
0.708099740992737,0.749999999999953,0.812499999999965,0.873008011417871,
0.931994642694371,0.989124166280261,1.),.UNSPECIFIED.);
#1938=B_SPLINE_CURVE_WITH_KNOTS('',3,(#90154,#90155,#90156,#90157,#90158,
#90159,#90160,#90161,#90162,#90163,#90164,#90165,#90166,#90167,#90168,#90169,
#90170,#90171,#90172,#90173,#90174,#90175,#90176,#90177,#90178,#90179,#90180,
#90181,#90182,#90183,#90184,#90185,#90186,#90187,#90188,#90189,#90190,#90191,
#90192,#90193,#90194,#90195,#90196,#90197,#90198,#90199,#90200,#90201,#90202,
#90203,#90204,#90205,#90206,#90207,#90208),.UNSPECIFIED.,.F.,.F.,(4,3,3,
3,3,3,3,3,3,3,3,3,3,3,3,3,3,3,4),(0.,0.0979870042878743,0.195803163964628,
0.250000000000044,0.35198064201211,0.375000000000053,0.437500000000046,
0.465440224692129,0.49427640578226,0.500000000000039,0.572265990346262,
0.641807673307847,0.707452286294341,0.750000000000019,0.812500000000015,
0.872799047234052,0.931582772210694,0.988509432123743,1.),.UNSPECIFIED.);
#1939=B_SPLINE_CURVE_WITH_KNOTS('',3,(#90238,#90239,#90240,#90241,#90242,
#90243,#90244,#90245,#90246,#90247,#90248,#90249,#90250,#90251,#90252,#90253,
#90254,#90255,#90256,#90257,#90258,#90259,#90260,#90261,#90262,#90263,#90264,
#90265,#90266,#90267,#90268,#90269,#90270,#90271,#90272,#90273,#90274,#90275,
#90276,#90277,#90278,#90279,#90280,#90281,#90282,#90283,#90284,#90285,#90286,
#90287,#90288,#90289,#90290,#90291,#90292,#90293,#90294,#90295,#90296,#90297,
#90298,#90299,#90300,#90301),.UNSPECIFIED.,.F.,.F.,(4,3,3,3,3,3,3,3,3,3,
3,3,3,3,3,3,3,3,3,3,3,4),(0.,0.0770564969196051,0.125000000000011,0.187500000000016,
0.218750000000018,0.23437500000002,0.242979652755323,0.250000000000023,
0.349688054350686,0.37500000000004,0.437500000000054,0.468750000000063,
0.484375000000066,0.492187500000072,0.499123753949107,0.500000000000079,
0.599066518850846,0.694261407782884,0.783895704985616,0.870510325616442,
0.953023907192251,1.),.UNSPECIFIED.);
#1940=B_SPLINE_CURVE_WITH_KNOTS('',3,(#90315,#90316,#90317,#90318,#90319,
#90320,#90321,#90322,#90323,#90324,#90325,#90326,#90327,#90328,#90329,#90330,
#90331,#90332,#90333,#90334,#90335,#90336,#90337,#90338,#90339,#90340,#90341,
#90342,#90343,#90344,#90345,#90346,#90347,#90348,#90349,#90350,#90351,#90352,
#90353,#90354,#90355,#90356,#90357,#90358,#90359,#90360,#90361,#90362,#90363,
#90364,#90365,#90366,#90367,#90368,#90369,#90370,#90371,#90372,#90373,#90374,
#90375,#90376,#90377,#90378,#90379,#90380,#90381,#90382,#90383,#90384,#90385,
#90386,#90387),.UNSPECIFIED.,.F.,.F.,(4,3,3,3,3,3,3,3,3,3,3,3,3,3,3,3,3,
3,3,3,3,3,3,3,4),(0.,0.037326049608827,0.0787965281334718,0.126371615676831,
0.184686823653943,0.249999999999854,0.344927243284897,0.37499999999978,
0.437499999999741,0.468749999999728,0.484374999999721,0.492187499999724,
0.496093749999726,0.498062133788789,0.499042481183733,0.499846118883597,
0.500303114481398,0.558840468960887,0.636460597139664,0.710206569093606,
0.774575228181004,0.838206096083458,0.903983913595566,0.977097659626974,
1.),.UNSPECIFIED.);
#1941=B_SPLINE_CURVE_WITH_KNOTS('',3,(#90391,#90392,#90393,#90394,#90395,
#90396,#90397,#90398,#90399,#90400,#90401,#90402,#90403,#90404,#90405),
 .UNSPECIFIED.,.F.,.F.,(4,2,2,3,2,2,4),(0.0594203506933311,0.0618755831119208,
0.064032651702581,0.0656455089088016,0.0672931027322027,0.0695060324935049,
0.0718717314145315),.UNSPECIFIED.);
#1942=B_SPLINE_CURVE_WITH_KNOTS('',3,(#90414,#90415,#90416,#90417,#90418,
#90419,#90420,#90421,#90422,#90423,#90424,#90425,#90426,#90427,#90428,#90429,
#90430,#90431,#90432,#90433,#90434,#90435,#90436,#90437,#90438,#90439,#90440,
#90441,#90442,#90443,#90444,#90445,#90446,#90447),.UNSPECIFIED.,.F.,.F.,
(4,3,3,3,3,3,3,3,3,3,3,4),(0.,0.0934837719039178,0.19091394803162,0.250000000000001,
0.32133120909575,0.39420774789555,0.471882415487507,0.500000000000003,0.625000000000002,
0.750831352586427,0.878474380660453,1.),.UNSPECIFIED.);
#1943=B_SPLINE_CURVE_WITH_KNOTS('',5,(#90477,#90478,#90479,#90480,#90481,
#90482,#90483,#90484,#90485),.UNSPECIFIED.,.F.,.F.,(6,3,6),(0.,0.446990882614049,
1.),.UNSPECIFIED.);
#1944=B_SPLINE_CURVE_WITH_KNOTS('',3,(#90570,#90571,#90572,#90573,#90574,
#90575,#90576,#90577,#90578,#90579,#90580,#90581,#90582,#90583,#90584,#90585,
#90586,#90587,#90588,#90589,#90590,#90591,#90592,#90593,#90594,#90595,#90596,
#90597,#90598,#90599,#90600,#90601,#90602,#90603,#90604,#90605,#90606,#90607,
#90608,#90609,#90610,#90611,#90612),.UNSPECIFIED.,.F.,.F.,(4,3,3,3,3,3,
3,3,3,3,3,3,3,3,4),(1.75158458902,1.82585854461461,1.90397349676335,1.93627831766,
2.01926759576981,2.10594778966711,2.14030218981,2.22559412880545,2.2812742412,
2.38564669191982,2.42220846454,2.53792768505673,2.67402562128176,2.83070830556877,
2.90384942405),.UNSPECIFIED.);
#1945=B_SPLINE_CURVE_WITH_KNOTS('',3,(#90716,#90717,#90718,#90719,#90720,
#90721,#90722,#90723,#90724,#90725,#90726,#90727,#90728,#90729,#90730,#90731,
#90732,#90733,#90734,#90735,#90736,#90737,#90738,#90739,#90740,#90741,#90742,
#90743,#90744,#90745,#90746,#90747,#90748,#90749,#90750,#90751,#90752,#90753,
#90754,#90755,#90756,#90757,#90758,#90759,#90760,#90761,#90762,#90763,#90764,
#90765,#90766,#90767,#90768,#90769,#90770),.UNSPECIFIED.,.F.,.F.,(4,3,3,
3,3,3,3,3,3,3,3,3,3,3,3,3,3,3,4),(1.90916034578814E-14,0.0632531835392224,
0.125000000000021,0.187500000000027,0.21717261086244,0.245838615885173,
0.250000000000034,0.330431396343107,0.375000000000042,0.437500000000041,
0.468750000000041,0.484375000000041,0.498404612002756,0.500000000000041,
0.600061730332378,0.710615960364526,0.819438906035603,0.918207455217059,
1.),.UNSPECIFIED.);
#1946=B_SPLINE_CURVE_WITH_KNOTS('',3,(#90849,#90850,#90851,#90852,#90853,
#90854,#90855,#90856,#90857,#90858,#90859,#90860,#90861,#90862,#90863,#90864,
#90865,#90866,#90867,#90868,#90869,#90870,#90871,#90872,#90873,#90874,#90875,
#90876,#90877,#90878,#90879,#90880,#90881,#90882,#90883,#90884,#90885,#90886,
#90887,#90888,#90889,#90890,#90891,#90892,#90893,#90894,#90895,#90896,#90897,
#90898,#90899,#90900,#90901,#90902,#90903,#90904,#90905,#90906),
 .UNSPECIFIED.,.F.,.F.,(4,3,3,3,3,3,3,3,3,3,3,3,3,3,3,3,3,3,3,4),(0.,0.0968230900403072,
0.201906635741557,0.306544326813906,0.403561202366286,0.449263932419849,
0.499999999999999,0.574890464499785,0.62962833045408,0.678442829509228,
0.722855417361369,0.73519144804672,0.7684367799326,0.803987925548705,0.841333943790706,
0.877807153721906,0.91063890722932,0.941813275174746,0.970955904576958,
1.),.UNSPECIFIED.);
#1947=B_SPLINE_CURVE_WITH_KNOTS('',3,(#90919,#90920,#90921,#90922,#90923,
#90924,#90925,#90926,#90927,#90928,#90929,#90930,#90931,#90932,#90933,#90934,
#90935,#90936,#90937,#90938,#90939,#90940,#90941,#90942,#90943,#90944,#90945,
#90946,#90947,#90948,#90949,#90950,#90951,#90952,#90953,#90954,#90955,#90956,
#90957,#90958,#90959,#90960,#90961,#90962,#90963,#90964,#90965,#90966,#90967,
#90968,#90969,#90970,#90971,#90972,#90973,#90974,#90975,#90976,#90977,#90978,
#90979,#90980,#90981,#90982,#90983,#90984,#90985,#90986,#90987,#90988,#90989,
#90990,#90991,#90992,#90993,#90994,#90995,#90996,#90997,#90998,#90999,#91000,
#91001,#91002,#91003,#91004,#91005,#91006,#91007,#91008,#91009,#91010,#91011,
#91012,#91013,#91014,#91015,#91016,#91017,#91018,#91019,#91020,#91021,#91022,
#91023,#91024,#91025,#91026,#91027,#91028,#91029,#91030,#91031,#91032,#91033,
#91034,#91035,#91036,#91037,#91038,#91039,#91040,#91041,#91042,#91043,#91044,
#91045,#91046,#91047,#91048,#91049,#91050,#91051,#91052,#91053,#91054,#91055,
#91056,#91057),.UNSPECIFIED.,.F.,.F.,(4,3,3,3,3,3,3,3,3,3,3,3,3,3,3,3,3,
3,3,3,3,3,3,3,3,3,3,3,3,3,3,3,3,3,3,3,3,3,3,3,3,3,3,3,3,3,4),(0.,0.0625000000000785,
0.086696354991142,0.11143417047313,0.125000000000157,0.187500000000235,
0.218750000000271,0.234375000000292,0.242187500000302,0.24708318045769,
0.250000000000312,0.262692941916091,0.265625000000332,0.273437500000337,
0.278246584391903,0.281250000000343,0.300621388827372,0.312500000000354,
0.343750000000357,0.375000000000361,0.403949752381917,0.433650417141628,
0.437500000000369,0.468750000000382,0.484375000000398,0.492502293593455,
0.500000000000413,0.521207465216726,0.531250000000391,0.546875000000378,
0.554732671383366,0.562500000000365,0.614860839166667,0.625000000000341,
0.687500000000317,0.718750000000291,0.734375000000279,0.743278564543908,
0.750000000000267,0.772730668789083,0.781250000000243,0.796875000000232,
0.805294656260953,0.812500000000222,0.856624166056844,0.875000000000148,
1.),.UNSPECIFIED.);
#1948=B_SPLINE_CURVE_WITH_KNOTS('',3,(#91061,#91062,#91063,#91064,#91065,
#91066,#91067,#91068,#91069,#91070,#91071,#91072,#91073,#91074,#91075,#91076,
#91077,#91078,#91079,#91080,#91081,#91082,#91083,#91084,#91085,#91086,#91087,
#91088,#91089,#91090,#91091,#91092,#91093,#91094,#91095,#91096,#91097,#91098,
#91099,#91100,#91101,#91102,#91103,#91104,#91105,#91106,#91107,#91108,#91109,
#91110,#91111,#91112,#91113,#91114,#91115),.UNSPECIFIED.,.F.,.F.,(4,3,3,
3,3,3,3,3,3,3,3,3,3,3,3,3,3,3,4),(0.,0.0980793331889885,0.195976519023509,
0.250000000000014,0.352035260039166,0.375000000000008,0.437500000000004,
0.465353490595414,0.494109597505518,0.500000000000001,0.572333705374357,
0.641941232753823,0.707651845844047,0.75,0.8125,0.872864157449969,0.931710851416161,
0.988699096048787,1.),.UNSPECIFIED.);
#1949=B_SPLINE_CURVE_WITH_KNOTS('',3,(#91123,#91124,#91125,#91126,#91127,
#91128,#91129,#91130,#91131,#91132,#91133,#91134,#91135,#91136,#91137,#91138,
#91139,#91140,#91141,#91142,#91143,#91144,#91145,#91146,#91147,#91148,#91149,
#91150,#91151,#91152,#91153,#91154,#91155,#91156,#91157,#91158,#91159,#91160,
#91161,#91162,#91163,#91164,#91165,#91166,#91167,#91168,#91169,#91170,#91171,
#91172,#91173,#91174,#91175,#91176,#91177,#91178,#91179,#91180),
 .UNSPECIFIED.,.F.,.F.,(4,3,3,3,3,3,3,3,3,3,3,3,3,3,3,3,3,3,3,4),(0.,0.0994522270089912,
0.19855275762107,0.249999999999961,0.320807500310168,0.390438933372071,
0.456941047442724,0.499999999999922,0.580884161076493,0.624999999999912,
0.687499999999914,0.718749999999915,0.732736627016244,0.747996545903896,
0.749999999999915,0.805252631848376,0.857501453771511,0.90793686231154,
0.955604059001085,1.),.UNSPECIFIED.);
#1950=B_SPLINE_CURVE_WITH_KNOTS('',3,(#91184,#91185,#91186,#91187,#91188,
#91189,#91190,#91191,#91192,#91193,#91194,#91195,#91196,#91197,#91198,#91199,
#91200,#91201,#91202,#91203,#91204,#91205,#91206,#91207,#91208,#91209,#91210,
#91211,#91212,#91213,#91214,#91215,#91216,#91217,#91218,#91219,#91220,#91221,
#91222,#91223,#91224,#91225,#91226,#91227,#91228,#91229,#91230,#91231,#91232,
#91233,#91234,#91235,#91236,#91237,#91238,#91239,#91240,#91241,#91242,#91243,
#91244,#91245,#91246,#91247,#91248,#91249,#91250),.UNSPECIFIED.,.F.,.F.,
(4,3,3,3,3,3,3,3,3,3,3,3,3,3,3,3,3,3,3,3,3,3,4),(0.,0.0338071905107698,
0.0625000000000105,0.0937500000000157,0.109375000000018,0.118222061923896,
0.125000000000021,0.171255468817826,0.220321915300574,0.250000000000024,
0.320854902327379,0.375000000000027,0.437500000000027,0.46328755320113,
0.490851192655088,0.500000000000028,0.625000000000029,0.669712733186267,
0.715775887477275,0.75000000000003,0.845897353941236,0.944150142413249,
1.),.UNSPECIFIED.);
#1951=B_SPLINE_CURVE_WITH_KNOTS('',3,(#91254,#91255,#91256,#91257,#91258,
#91259,#91260,#91261,#91262,#91263,#91264,#91265,#91266,#91267,#91268,#91269,
#91270,#91271,#91272,#91273,#91274,#91275,#91276,#91277,#91278,#91279,#91280,
#91281,#91282,#91283,#91284,#91285,#91286,#91287,#91288,#91289,#91290,#91291,
#91292,#91293,#91294,#91295,#91296,#91297,#91298,#91299,#91300,#91301,#91302,
#91303,#91304,#91305,#91306,#91307,#91308,#91309,#91310,#91311),
 .UNSPECIFIED.,.F.,.F.,(4,3,3,3,3,3,3,3,3,3,3,3,3,3,3,3,3,3,3,4),(0.,0.0451092776599689,
0.0925039027641494,0.12500000000001,0.174913836077685,0.187500000000022,
0.218750000000022,0.234375000000022,0.248604010257293,0.250000000000022,
0.318607877079331,0.375000000000026,0.41738420156605,0.462520462216422,
0.50000000000003,0.59283675164862,0.689308660068251,0.789872400074604,0.894936200037302,
1.),.UNSPECIFIED.);
#1952=B_SPLINE_CURVE_WITH_KNOTS('',3,(#91433,#91434,#91435,#91436,#91437,
#91438,#91439,#91440,#91441,#91442,#91443,#91444,#91445,#91446,#91447,#91448,
#91449,#91450,#91451,#91452,#91453,#91454,#91455,#91456,#91457,#91458,#91459,
#91460,#91461,#91462,#91463,#91464,#91465,#91466,#91467,#91468,#91469,#91470,
#91471,#91472,#91473,#91474,#91475,#91476,#91477,#91478,#91479,#91480,#91481,
#91482,#91483,#91484,#91485,#91486,#91487),.UNSPECIFIED.,.F.,.F.,(4,3,3,
3,3,3,3,3,3,3,3,3,3,3,3,3,3,3,4),(0.,0.102320181390481,0.201694320732233,
0.249999999999988,0.345937965973561,0.374999999999982,0.43749999999998,
0.468749999999972,0.484374999999968,0.492839606007928,0.499999999999964,
0.576579098012344,0.651305076097686,0.722730977064833,0.749999999999982,
0.81633078076096,0.880405936123099,0.941174730499775,1.),.UNSPECIFIED.);
#1953=B_SPLINE_CURVE_WITH_KNOTS('',5,(#91551,#91552,#91553,#91554,#91555,
#91556,#91557,#91558,#91559),.UNSPECIFIED.,.F.,.F.,(6,3,6),(0.,0.459694365459143,
1.),.UNSPECIFIED.);
#1954=B_SPLINE_CURVE_WITH_KNOTS('',3,(#91561,#91562,#91563,#91564,#91565,
#91566,#91567,#91568,#91569,#91570,#91571,#91572,#91573,#91574,#91575,#91576,
#91577,#91578,#91579,#91580,#91581,#91582,#91583,#91584,#91585,#91586,#91587,
#91588,#91589,#91590,#91591,#91592,#91593,#91594,#91595,#91596,#91597),
 .UNSPECIFIED.,.F.,.F.,(4,3,3,3,3,3,3,3,3,3,3,3,4),(0.,0.0831702685280121,
0.167847262437448,0.25483900256361,0.342953378583159,0.432342539351743,
0.5,0.589502114356238,0.678232387149981,0.76504398598027,0.850564991306322,
0.933989360303386,1.),.UNSPECIFIED.);
#1955=B_SPLINE_CURVE_WITH_KNOTS('',3,(#91622,#91623,#91624,#91625,#91626,
#91627,#91628,#91629,#91630,#91631,#91632,#91633,#91634,#91635,#91636,#91637,
#91638,#91639,#91640,#91641,#91642,#91643,#91644,#91645,#91646,#91647,#91648,
#91649,#91650,#91651,#91652,#91653,#91654,#91655,#91656,#91657,#91658,#91659,
#91660,#91661),.UNSPECIFIED.,.F.,.F.,(4,3,3,3,3,3,3,3,3,3,3,3,3,4),(1.69812247662,
1.82517827643346,1.94835352449351,2.04354239572,2.1493981491557,2.2504202018726,
2.34618007075805,2.37608580106,2.46390218046495,2.55211800019734,2.6379844451379,
2.6897944832,2.77017696446133,2.83469359842),.UNSPECIFIED.);
#1956=B_SPLINE_CURVE_WITH_KNOTS('',3,(#91673,#91674,#91675,#91676,#91677,
#91678,#91679,#91680,#91681,#91682,#91683,#91684,#91685,#91686,#91687,#91688,
#91689,#91690,#91691,#91692,#91693,#91694,#91695,#91696,#91697,#91698,#91699,
#91700,#91701,#91702,#91703,#91704,#91705,#91706,#91707,#91708,#91709,#91710,
#91711,#91712,#91713,#91714,#91715,#91716,#91717,#91718,#91719,#91720,#91721,
#91722,#91723,#91724,#91725,#91726,#91727,#91728,#91729,#91730),
 .UNSPECIFIED.,.F.,.F.,(4,3,3,3,3,3,3,3,3,3,3,3,3,3,3,3,3,3,3,4),(4.76185240083,
4.83763310355387,4.8511070755,4.9237368026632,4.94035737066,5.01616912552097,
5.04125309343,5.11983939701062,5.14214350511,5.21975609722012,5.29603838282238,
5.31344541544,5.40219520324995,5.47351631749,5.56538841319371,5.65858597861109,
5.75320413758695,5.78071175361,5.87661154462981,5.93786871511),
 .UNSPECIFIED.);
#1957=B_SPLINE_CURVE_WITH_KNOTS('',3,(#91734,#91735,#91736,#91737,#91738,
#91739,#91740,#91741,#91742,#91743,#91744,#91745,#91746,#91747,#91748,#91749,
#91750,#91751,#91752,#91753,#91754,#91755,#91756,#91757,#91758,#91759,#91760,
#91761,#91762,#91763,#91764,#91765,#91766,#91767,#91768,#91769,#91770,#91771,
#91772,#91773,#91774,#91775,#91776,#91777,#91778,#91779,#91780,#91781,#91782,
#91783,#91784,#91785,#91786,#91787,#91788,#91789,#91790,#91791),
 .UNSPECIFIED.,.F.,.F.,(4,3,3,3,3,3,3,3,3,3,3,3,3,3,3,3,3,3,3,4),(2.86340882221,
2.96038236608018,2.9912183572,3.08700311846,3.18278787972,3.27460804500352,
3.36346730309093,3.3764526533,3.45865940729478,3.54085709160542,3.57484410128,
3.65773122998382,3.67917202515,3.75805208465001,3.78350088337,3.86115067208,
3.93423338613355,3.93880046079,4.01498217619634,4.03947605191),
 .UNSPECIFIED.);
#1958=B_SPLINE_CURVE_WITH_KNOTS('',3,(#91813,#91814,#91815,#91816,#91817,
#91818,#91819,#91820,#91821,#91822,#91823,#91824,#91825,#91826,#91827,#91828,
#91829,#91830,#91831,#91832,#91833,#91834,#91835,#91836,#91837,#91838,#91839,
#91840,#91841,#91842,#91843,#91844,#91845,#91846,#91847,#91848,#91849),
 .UNSPECIFIED.,.F.,.F.,(4,3,3,3,3,3,3,3,3,3,3,3,4),(9.16687616257107E-11,
0.0777713091928336,0.155304544748419,0.235796293739508,0.250000000000001,
0.375000000000002,0.426033233674526,0.476997002990943,0.500000000000003,
0.647319737369125,0.788544793198841,0.917036474768495,1.),.UNSPECIFIED.);
#1959=B_SPLINE_CURVE_WITH_KNOTS('',3,(#91865,#91866,#91867,#91868,#91869,
#91870,#91871,#91872,#91873,#91874,#91875,#91876,#91877,#91878,#91879,#91880,
#91881,#91882,#91883,#91884,#91885,#91886,#91887,#91888,#91889,#91890,#91891,
#91892,#91893,#91894,#91895,#91896,#91897,#91898,#91899,#91900,#91901),
 .UNSPECIFIED.,.F.,.F.,(4,3,3,3,3,3,3,3,3,3,3,3,4),(9.16667455825459E-11,
0.0777713111959483,0.1553045487284,0.235796299444816,0.249999999999999,
0.374999999999999,0.426033234695566,0.476997005066265,0.499999999999998,
0.647319737403808,0.788544793261829,0.917036474850319,1.),.UNSPECIFIED.);
#1960=B_SPLINE_CURVE_WITH_KNOTS('',3,(#91905,#91906,#91907,#91908),
 .UNSPECIFIED.,.F.,.F.,(4,4),(-1.68203627824,-1.66422823568),
 .UNSPECIFIED.);
#1961=B_SPLINE_CURVE_WITH_KNOTS('',3,(#91910,#91911,#91912,#91913),
 .UNSPECIFIED.,.F.,.F.,(4,4),(-1.04373195388,-1.00826496187),
 .UNSPECIFIED.);
#1962=B_SPLINE_CURVE_WITH_KNOTS('',5,(#91938,#91939,#91940,#91941,#91942,
#91943),.UNSPECIFIED.,.F.,.F.,(6,6),(0.,1.),.UNSPECIFIED.);
#1963=B_SPLINE_CURVE_WITH_KNOTS('',3,(#91948,#91949,#91950,#91951,#91952,
#91953,#91954,#91955,#91956,#91957,#91958,#91959,#91960,#91961,#91962,#91963,
#91964,#91965,#91966,#91967,#91968,#91969,#91970,#91971,#91972,#91973,#91974,
#91975,#91976,#91977,#91978,#91979,#91980,#91981,#91982,#91983,#91984,#91985,
#91986,#91987),.UNSPECIFIED.,.F.,.F.,(4,3,3,3,3,3,3,3,3,3,3,3,3,4),(1.64208556101,
1.72926070554228,1.73827899693,1.8278907907593,1.92154711062456,2.01700443389081,
2.1132071936736,2.12883652195,2.23557388803073,2.32877794125,2.44459839436569,
2.5306802585,2.66108985588594,2.73162696034),.UNSPECIFIED.);
#1964=B_SPLINE_CURVE_WITH_KNOTS('',3,(#92031,#92032,#92033,#92034,#92035,
#92036,#92037,#92038,#92039,#92040,#92041,#92042,#92043,#92044,#92045,#92046,
#92047,#92048,#92049,#92050,#92051,#92052,#92053,#92054,#92055,#92056,#92057,
#92058,#92059,#92060,#92061),.UNSPECIFIED.,.F.,.F.,(4,3,3,3,3,3,3,3,3,3,
4),(0.,0.0955467215590676,0.196660041169301,0.296253107708768,0.398126553854384,
0.5,0.601416708013665,0.701415344786851,0.800181615448635,0.900090807724317,
1.),.UNSPECIFIED.);
#1965=B_SPLINE_CURVE_WITH_KNOTS('',3,(#92172,#92173,#92174,#92175),
 .UNSPECIFIED.,.F.,.F.,(4,4),(-1.04373195388,-1.00826496187),
 .UNSPECIFIED.);
#1966=B_SPLINE_CURVE_WITH_KNOTS('',3,(#92260,#92261,#92262,#92263,#92264,
#92265,#92266,#92267,#92268,#92269,#92270,#92271,#92272,#92273,#92274,#92275,
#92276,#92277,#92278,#92279,#92280,#92281,#92282,#92283,#92284,#92285,#92286,
#92287),.UNSPECIFIED.,.F.,.F.,(4,3,3,3,3,3,3,3,3,4),(3.98942132494305E-9,
0.150497117185246,0.288254537029539,0.376907505501659,0.503498889679138,
0.532680629126244,0.664294493152615,0.802603697848191,0.950070961802982,
1.),.UNSPECIFIED.);
#1967=B_SPLINE_CURVE_WITH_KNOTS('',3,(#92313,#92314,#92315,#92316),
 .UNSPECIFIED.,.F.,.F.,(4,4),(-1.68203627824,-1.66422823568),
 .UNSPECIFIED.);
#1968=B_SPLINE_CURVE_WITH_KNOTS('',3,(#92416,#92417,#92418,#92419,#92420,
#92421,#92422,#92423,#92424,#92425,#92426,#92427,#92428,#92429,#92430,#92431,
#92432,#92433,#92434,#92435,#92436,#92437,#92438,#92439,#92440,#92441,#92442,
#92443),.UNSPECIFIED.,.F.,.F.,(4,3,3,3,3,3,3,3,3,4),(3.98063301892076E-9,
0.150497117191435,0.288254537058802,0.376907505472153,0.503498889669673,
0.532680629104115,0.664294493113039,0.802603697754453,0.950070961594217,
1.),.UNSPECIFIED.);
#1969=B_SPLINE_CURVE_WITH_KNOTS('',3,(#92536,#92537,#92538,#92539,#92540,
#92541,#92542,#92543,#92544,#92545,#92546,#92547,#92548,#92549,#92550,#92551,
#92552,#92553,#92554,#92555,#92556,#92557,#92558,#92559,#92560,#92561,#92562,
#92563,#92564,#92565,#92566,#92567,#92568,#92569,#92570,#92571,#92572,#92573,
#92574,#92575,#92576,#92577,#92578,#92579,#92580,#92581,#92582,#92583,#92584,
#92585,#92586,#92587,#92588,#92589,#92590,#92591,#92592,#92593,#92594,#92595,
#92596,#92597,#92598,#92599,#92600,#92601,#92602,#92603,#92604,#92605,#92606,
#92607,#92608,#92609,#92610,#92611),.UNSPECIFIED.,.F.,.F.,(4,3,3,3,3,3,
3,3,3,3,3,3,3,3,3,3,3,3,3,3,3,3,3,3,3,4),(0.,0.0937499999999247,0.183615921210463,
0.273457967111046,0.363302606689923,0.374999999999699,0.437499999999654,
0.468749999999633,0.481912351571244,0.496444815995831,0.499999999999611,
0.562499999999591,0.593749999999593,0.609374999999607,0.618302120244718,
0.624999999999621,0.650015547301732,0.656249999999664,0.671050151688994,
0.685059338020028,0.687499999999707,0.714547929086675,0.744158092899608,
0.749999999999772,0.922985773999486,1.),.UNSPECIFIED.);
#1970=B_SPLINE_CURVE_WITH_KNOTS('',3,(#92615,#92616,#92617,#92618,#92619,
#92620,#92621,#92622,#92623,#92624,#92625,#92626,#92627,#92628,#92629,#92630,
#92631,#92632,#92633,#92634,#92635,#92636,#92637,#92638,#92639,#92640,#92641,
#92642,#92643,#92644,#92645,#92646,#92647,#92648,#92649,#92650,#92651,#92652,
#92653,#92654,#92655,#92656,#92657,#92658,#92659,#92660,#92661,#92662,#92663,
#92664,#92665,#92666,#92667,#92668,#92669,#92670,#92671,#92672),
 .UNSPECIFIED.,.F.,.F.,(4,3,3,3,3,3,3,3,3,3,3,3,3,3,3,3,3,3,3,4),(0.,0.0443451168985777,
0.0909483516403088,0.125000000000021,0.174152759844734,0.187500000000031,
0.21875000000003,0.234375000000029,0.248688920390979,0.250000000000029,
0.318111984407296,0.375000000000013,0.415894282087958,0.459570458469752,
0.499999999999998,0.592678771259659,0.688958966630604,0.78925342781995,
0.894626713909975,1.),.UNSPECIFIED.);
#1971=B_SPLINE_CURVE_WITH_KNOTS('',3,(#92683,#92684,#92685,#92686,#92687,
#92688,#92689,#92690,#92691,#92692,#92693,#92694,#92695,#92696,#92697,#92698,
#92699,#92700,#92701,#92702,#92703,#92704,#92705,#92706,#92707,#92708,#92709,
#92710,#92711,#92712,#92713,#92714,#92715,#92716,#92717,#92718,#92719,#92720,
#92721,#92722,#92723,#92724,#92725,#92726,#92727,#92728,#92729,#92730,#92731,
#92732,#92733,#92734,#92735,#92736,#92737,#92738,#92739,#92740,#92741,#92742,
#92743,#92744,#92745,#92746,#92747,#92748,#92749,#92750,#92751,#92752,#92753,
#92754,#92755),.UNSPECIFIED.,.F.,.F.,(4,3,3,3,3,3,3,3,3,3,3,3,3,3,3,3,3,
3,3,3,3,3,3,3,4),(0.,0.0943040666939272,0.18898259270498,0.250000000000074,
0.350492487940872,0.375000000000096,0.437500000000093,0.464977671236868,
0.490762671002707,0.500000000000091,0.579331802709907,0.625000000000066,
0.665840272931786,0.707920136465913,0.745842552516937,0.750000000000041,
0.812500000000029,0.843750000000022,0.856467201676309,0.870123765069302,
0.875000000000016,0.912439301208134,0.948859469697768,0.983548250663145,
1.),.UNSPECIFIED.);
#1972=B_SPLINE_CURVE_WITH_KNOTS('',3,(#92759,#92760,#92761,#92762,#92763,
#92764,#92765,#92766,#92767,#92768,#92769,#92770,#92771,#92772,#92773,#92774,
#92775,#92776,#92777,#92778,#92779,#92780,#92781,#92782,#92783,#92784,#92785,
#92786,#92787,#92788,#92789,#92790,#92791,#92792,#92793,#92794,#92795,#92796,
#92797,#92798,#92799,#92800,#92801,#92802,#92803,#92804,#92805,#92806,#92807,
#92808,#92809,#92810,#92811,#92812,#92813,#92814,#92815,#92816,#92817,#92818,
#92819,#92820,#92821,#92822,#92823,#92824,#92825),.UNSPECIFIED.,.F.,.F.,
(4,3,3,3,3,3,3,3,3,3,3,3,3,3,3,3,3,3,3,3,3,3,4),(0.,0.12499999999999,0.188571899414555,
0.24999999999998,0.37499999999997,0.437500000000004,0.466500812528174,0.50000000000004,
0.541171395769626,0.583085697884828,0.62500000000003,0.665266761660683,
0.704453084784077,0.741405254291436,0.776868942642716,0.810906560932425,
0.843624402352047,0.875137715833154,0.906353286874866,0.935335899732279,
0.963556417430368,0.990779891878734,1.),.UNSPECIFIED.);
#1973=B_SPLINE_CURVE_WITH_KNOTS('',3,(#92834,#92835,#92836,#92837,#92838,
#92839,#92840,#92841,#92842,#92843,#92844,#92845,#92846,#92847,#92848,#92849,
#92850,#92851,#92852,#92853,#92854,#92855,#92856,#92857,#92858,#92859,#92860,
#92861,#92862,#92863,#92864,#92865,#92866,#92867,#92868,#92869,#92870,#92871,
#92872,#92873,#92874,#92875,#92876,#92877,#92878,#92879,#92880,#92881,#92882,
#92883,#92884,#92885,#92886,#92887,#92888,#92889,#92890,#92891,#92892,#92893,
#92894,#92895,#92896,#92897,#92898,#92899,#92900,#92901,#92902,#92903,#92904,
#92905,#92906,#92907,#92908,#92909,#92910,#92911,#92912,#92913,#92914,#92915,
#92916,#92917,#92918,#92919,#92920,#92921,#92922,#92923,#92924,#92925,#92926,
#92927,#92928,#92929,#92930,#92931,#92932,#92933,#92934,#92935,#92936,#92937,
#92938,#92939,#92940,#92941,#92942,#92943,#92944,#92945),.UNSPECIFIED.,
 .F.,.F.,(4,3,3,3,3,3,3,3,3,3,3,3,3,3,3,3,3,3,3,3,3,3,3,3,3,3,3,3,3,3,3,
3,3,3,3,3,3,4),(0.,0.125000000002865,0.187500000004281,0.216128186234356,
0.243284284702797,0.250000000005696,0.352348172379624,0.375000000008529,
0.437500000009947,0.462030398295331,0.485130811504489,0.500000000011365,
0.562500000012783,0.593750000013494,0.609375000013851,0.617187500014019,
0.622662434262975,0.625000000014188,0.642795177114311,0.656250000014155,
0.671875000014138,0.678967911692179,0.686342149067149,0.687500000014121,
0.718750000014078,0.734375000014051,0.742187500014035,0.747488512167396,
0.75000000001402,0.781436979920065,0.813065815197281,0.844518835992743,
0.87500000000701,0.904533702371711,0.932006850722208,0.958333127878501,
0.983097804372786,1.),.UNSPECIFIED.);
#1974=B_SPLINE_CURVE_WITH_KNOTS('',3,(#92966,#92967,#92968,#92969,#92970,
#92971,#92972,#92973,#92974,#92975,#92976,#92977,#92978,#92979,#92980,#92981,
#92982,#92983,#92984,#92985,#92986,#92987,#92988,#92989,#92990,#92991,#92992,
#92993,#92994,#92995,#92996,#92997,#92998,#92999,#93000,#93001,#93002,#93003,
#93004,#93005,#93006,#93007,#93008,#93009,#93010,#93011,#93012,#93013,#93014,
#93015,#93016,#93017,#93018,#93019,#93020,#93021,#93022,#93023),
 .UNSPECIFIED.,.F.,.F.,(4,3,3,3,3,3,3,3,3,3,3,3,3,3,3,3,3,3,3,4),(0.,0.125000000000002,
0.250000000000005,0.365236498453909,0.375000000000007,0.421011993194877,
0.467170215472028,0.50000000000001,0.58605609992678,0.625000000000013,0.687500000000008,
0.71875,0.73247917279936,0.747722802633476,0.749999999999991,0.812499999999993,
0.869829956013398,0.925192869595088,0.977789571163086,1.),.UNSPECIFIED.);
#1975=B_SPLINE_CURVE_WITH_KNOTS('',3,(#93100,#93101,#93102,#93103,#93104,
#93105,#93106,#93107,#93108,#93109,#93110,#93111,#93112,#93113,#93114,#93115,
#93116,#93117,#93118,#93119,#93120,#93121,#93122,#93123,#93124,#93125,#93126,
#93127,#93128,#93129,#93130,#93131,#93132,#93133,#93134,#93135,#93136,#93137,
#93138,#93139,#93140,#93141,#93142,#93143,#93144,#93145,#93146,#93147,#93148,
#93149,#93150,#93151,#93152,#93153,#93154,#93155,#93156,#93157,#93158,#93159,
#93160,#93161,#93162,#93163),.UNSPECIFIED.,.F.,.F.,(4,3,3,3,3,3,3,3,3,3,
3,3,3,3,3,3,3,3,3,3,3,4),(1.30569972989664E-13,0.0394023736834368,0.0822011868417158,
0.124999999999995,0.167289105223367,0.187499999999992,0.209945720373917,
0.23456433282999,0.249999999999988,0.325623787343657,0.374999999999979,
0.437499999999978,0.468749999999984,0.484374999999988,0.493888833934045,
0.499999999999991,0.597586484903761,0.69843638032809,0.791729532747611,
0.881731622630255,0.968663051431044,1.),.UNSPECIFIED.);
#1976=B_SPLINE_CURVE_WITH_KNOTS('',3,(#93166,#93167,#93168,#93169,#93170,
#93171,#93172,#93173,#93174,#93175,#93176,#93177,#93178,#93179,#93180,#93181,
#93182,#93183,#93184,#93185,#93186,#93187,#93188,#93189,#93190,#93191,#93192,
#93193,#93194,#93195,#93196,#93197,#93198,#93199,#93200,#93201,#93202,#93203,
#93204,#93205,#93206,#93207,#93208,#93209,#93210,#93211,#93212,#93213,#93214),
 .UNSPECIFIED.,.F.,.F.,(4,3,3,3,3,3,3,3,3,3,3,3,3,3,3,3,4),(0.,0.0646375542710448,
0.131986214404462,0.205237786349825,0.25,0.3363751967743,0.420131595217952,
0.5,0.569501845294344,0.635666297979706,0.697934450928747,0.75,0.808915454001482,
0.865550018011427,0.92107127627776,0.975154358484857,1.),.UNSPECIFIED.);
#1977=B_SPLINE_CURVE_WITH_KNOTS('',3,(#93412,#93413,#93414,#93415,#93416,
#93417,#93418,#93419,#93420,#93421,#93422,#93423,#93424,#93425,#93426,#93427,
#93428,#93429,#93430,#93431,#93432,#93433,#93434,#93435,#93436,#93437,#93438,
#93439,#93440,#93441,#93442,#93443,#93444,#93445,#93446,#93447,#93448,#93449,
#93450,#93451,#93452,#93453,#93454,#93455,#93456,#93457,#93458,#93459,#93460,
#93461,#93462,#93463,#93464,#93465,#93466,#93467,#93468,#93469,#93470,#93471,
#93472,#93473,#93474,#93475),.UNSPECIFIED.,.F.,.F.,(4,3,3,3,3,3,3,3,3,3,
3,3,3,3,3,3,3,3,3,3,3,4),(0.,0.0313265556561311,0.0639694708706069,0.0991532878456469,
0.125000000000003,0.161981198945146,0.197636162313631,0.230727451571766,
0.250000000000005,0.263633961320155,0.302088741633232,0.352565680645548,
0.397399712184553,0.468832078691233,0.500000000000002,0.586077893149075,
0.674777857656565,0.714614915280701,0.807100572165139,0.903550286082569,
0.980940289322871,1.),.UNSPECIFIED.);
#1978=B_SPLINE_CURVE_WITH_KNOTS('',3,(#93477,#93478,#93479,#93480,#93481,
#93482,#93483,#93484,#93485,#93486,#93487,#93488,#93489,#93490,#93491,#93492,
#93493,#93494,#93495,#93496,#93497,#93498,#93499,#93500,#93501,#93502,#93503,
#93504,#93505,#93506,#93507,#93508,#93509,#93510,#93511,#93512,#93513,#93514,
#93515,#93516,#93517,#93518,#93519,#93520,#93521,#93522),.UNSPECIFIED.,
 .F.,.F.,(4,3,3,3,3,3,3,3,3,3,3,3,3,3,3,4),(0.,0.0676469801677771,0.137106796073644,
0.209683116828569,0.250000000000043,0.327522831121316,0.375000000000065,
0.437500000000081,0.468750000000089,0.484661840756592,0.500000000000098,
0.609757695881578,0.72628120414161,0.847292917845917,0.975661564746343,
1.),.UNSPECIFIED.);
#1979=B_SPLINE_CURVE_WITH_KNOTS('',3,(#93542,#93543,#93544,#93545,#93546,
#93547,#93548,#93549,#93550,#93551,#93552,#93553,#93554,#93555,#93556,#93557,
#93558,#93559,#93560,#93561,#93562,#93563,#93564,#93565,#93566,#93567,#93568,
#93569,#93570,#93571,#93572,#93573,#93574,#93575),.UNSPECIFIED.,.F.,.F.,
(4,3,3,3,3,3,3,3,3,3,3,4),(1.25405163269,1.32643264163,1.4055803165725,
1.48574465294545,1.56752327448427,1.6430233414,1.72858124378027,1.81406569145,
1.90733041601598,1.99715560017,2.09477370437,2.19239180857),
 .UNSPECIFIED.);
#1980=B_SPLINE_CURVE_WITH_KNOTS('',3,(#93633,#93634,#93635,#93636,#93637,
#93638,#93639,#93640,#93641,#93642,#93643,#93644,#93645,#93646,#93647,#93648,
#93649,#93650,#93651,#93652,#93653,#93654,#93655,#93656,#93657,#93658,#93659,
#93660,#93661,#93662,#93663,#93664,#93665,#93666,#93667,#93668,#93669,#93670,
#93671,#93672,#93673,#93674,#93675,#93676,#93677,#93678,#93679,#93680,#93681,
#93682,#93683,#93684,#93685,#93686,#93687,#93688,#93689,#93690,#93691,#93692,
#93693),.UNSPECIFIED.,.F.,.F.,(4,3,3,3,3,3,3,3,3,3,3,3,3,3,3,3,3,3,3,3,
4),(0.,0.0757360115643633,0.153309514148711,0.232749548769837,0.249999999999913,
0.329782774192022,0.374999999999877,0.42601283745248,0.437499999999857,
0.468749999999847,0.484374999999842,0.493943320438178,0.499999999999837,
0.562810053136719,0.62772503823603,0.695349843164152,0.749999999999919,
0.823320223135299,0.899885323406126,0.981080192972812,1.),.UNSPECIFIED.);
#1981=B_SPLINE_CURVE_WITH_KNOTS('',3,(#93752,#93753,#93754,#93755,#93756,
#93757,#93758,#93759,#93760,#93761,#93762,#93763,#93764,#93765,#93766,#93767,
#93768,#93769,#93770,#93771,#93772,#93773,#93774,#93775,#93776,#93777,#93778,
#93779,#93780,#93781,#93782,#93783,#93784,#93785,#93786,#93787,#93788,#93789,
#93790,#93791,#93792,#93793,#93794,#93795,#93796,#93797,#93798,#93799,#93800,
#93801,#93802,#93803,#93804,#93805,#93806,#93807,#93808,#93809),
 .UNSPECIFIED.,.F.,.F.,(4,3,3,3,3,3,3,3,3,3,3,3,3,3,3,3,3,3,3,4),(0.,0.0795529238434195,
0.156039645963624,0.227878159961086,0.250000000000057,0.319021097031273,
0.375000000000083,0.4375000000001,0.468750000000104,0.474796994033287,0.484375000000107,
0.493485330168561,0.500000000000109,0.585436846623337,0.667718423311696,
0.750000000000055,0.829338336199628,0.906967603645166,0.981482011220185,
1.),.UNSPECIFIED.);
#1982=B_SPLINE_CURVE_WITH_KNOTS('',3,(#93826,#93827,#93828,#93829,#93830,
#93831,#93832,#93833,#93834,#93835,#93836,#93837),.UNSPECIFIED.,.F.,.F.,
(4,2,2,2,2,4),(-0.2526817413658,-0.252144968685117,-0.231701265952628,-0.221146902348503,
-0.215214602553632,-0.211845320308325),.UNSPECIFIED.);
#1983=B_SPLINE_CURVE_WITH_KNOTS('',5,(#93866,#93867,#93868,#93869,#93870,
#93871),.UNSPECIFIED.,.F.,.F.,(6,6),(0.,0.999999959271343),
 .UNSPECIFIED.);
#1984=B_SPLINE_CURVE_WITH_KNOTS('',3,(#93929,#93930,#93931,#93932,#93933,
#93934,#93935,#93936,#93937,#93938,#93939,#93940,#93941,#93942,#93943,#93944,
#93945,#93946,#93947,#93948,#93949,#93950,#93951,#93952,#93953,#93954,#93955,
#93956,#93957,#93958,#93959,#93960,#93961,#93962,#93963,#93964,#93965,#93966,
#93967,#93968,#93969,#93970,#93971,#93972,#93973,#93974,#93975,#93976,#93977,
#93978,#93979,#93980,#93981,#93982,#93983,#93984,#93985,#93986,#93987,#93988,
#93989,#93990,#93991,#93992),.UNSPECIFIED.,.F.,.F.,(4,3,3,3,3,3,3,3,3,3,
3,3,3,3,3,3,3,3,3,3,3,4),(0.,0.103653379061186,0.20361411417021,0.249999999999959,
0.345078024193049,0.374999999999938,0.437499999999928,0.452274762523055,
0.468749999999922,0.483386774211928,0.499999999999916,0.578583158147426,
0.624999999999938,0.671874999999946,0.684061297709991,0.690640429806601,
0.714634449294438,0.732469796213536,0.74919043395019,0.752709571352447,
0.878649898165962,1.),.UNSPECIFIED.);
#1985=B_SPLINE_CURVE_WITH_KNOTS('',3,(#93995,#93996,#93997,#93998,#93999,
#94000,#94001,#94002,#94003,#94004,#94005,#94006,#94007,#94008,#94009,#94010,
#94011,#94012,#94013,#94014,#94015,#94016,#94017),.UNSPECIFIED.,.F.,.F.,
(4,2,2,2,3,2,2,2,2,2,4),(-0.00491026743302993,-0.00473849995762558,-0.00442749851885031,
-0.00379135806062017,0.,0.00898521807370431,0.01430350641162,0.0224007619062803,
0.0339277546976348,0.0458917612396366,0.0502751707719722),.UNSPECIFIED.);
#1986=B_SPLINE_CURVE_WITH_KNOTS('',3,(#94032,#94033,#94034,#94035,#94036,
#94037,#94038,#94039,#94040,#94041,#94042,#94043,#94044,#94045,#94046,#94047),
 .UNSPECIFIED.,.F.,.F.,(4,2,2,2,2,2,2,4),(-0.120393885459129,-0.119994183646075,
-0.114665415333723,-0.109375283203773,-0.103435268329857,-0.0955923543424567,
-0.0900172452535582,-0.0812505338475646),.UNSPECIFIED.);
#1987=B_SPLINE_CURVE_WITH_KNOTS('',3,(#94132,#94133,#94134,#94135,#94136,
#94137,#94138,#94139,#94140,#94141,#94142,#94143,#94144,#94145,#94146,#94147,
#94148,#94149,#94150,#94151,#94152,#94153,#94154,#94155,#94156,#94157,#94158,
#94159,#94160,#94161,#94162,#94163,#94164,#94165,#94166,#94167,#94168,#94169,
#94170,#94171,#94172,#94173,#94174,#94175,#94176,#94177,#94178,#94179,#94180,
#94181,#94182,#94183,#94184,#94185,#94186,#94187,#94188,#94189,#94190,#94191,
#94192,#94193,#94194,#94195,#94196,#94197,#94198,#94199,#94200,#94201,#94202,
#94203,#94204),.UNSPECIFIED.,.F.,.F.,(4,3,3,3,3,3,3,3,3,3,3,3,3,3,3,3,3,
3,3,3,3,3,3,3,4),(0.,0.0392604588675547,0.0796928782844232,0.121900173659216,
0.124999999999999,0.170760900465759,0.187499999999994,0.218749999999994,
0.234374999999993,0.248731529201415,0.249999999999993,0.315888335880771,
0.375000000000004,0.437500000000008,0.462804796365139,0.489494576915244,
0.500000000000012,0.596805346167588,0.625000000000016,0.666607772440218,
0.70933182444373,0.75000000000002,0.841508009635831,0.936057229296371,1.),
 .UNSPECIFIED.);
#1988=B_SPLINE_CURVE_WITH_KNOTS('',3,(#94232,#94233,#94234,#94235,#94236,
#94237,#94238,#94239,#94240,#94241,#94242,#94243,#94244,#94245,#94246,#94247,
#94248,#94249,#94250,#94251,#94252,#94253,#94254,#94255,#94256,#94257,#94258,
#94259,#94260,#94261,#94262,#94263,#94264,#94265,#94266,#94267,#94268,#94269,
#94270,#94271),.UNSPECIFIED.,.F.,.F.,(4,3,3,3,3,3,3,3,3,3,3,3,3,4),(0.,
0.0879907258885037,0.106017412003521,0.203661923636243,0.212034824007045,
0.318052236010566,0.424069648014091,0.530087060017611,0.636104472021133,
0.699133885047539,0.756356915627061,0.859124793049096,0.929561688516431,
1.),.UNSPECIFIED.);
#1989=B_SPLINE_CURVE_WITH_KNOTS('',3,(#94310,#94311,#94312,#94313,#94314,
#94315,#94316,#94317,#94318,#94319,#94320,#94321,#94322,#94323,#94324,#94325,
#94326,#94327,#94328,#94329,#94330,#94331),.UNSPECIFIED.,.F.,.F.,(4,2,2,
1,1,2,2,2,1,1,2,2,4),(0.,0.250000000000018,0.375000000000027,0.437500000000035,
0.468750000000039,0.484375000000039,0.500000000000038,0.625000000000014,
0.687500000000002,0.71874999999999,0.734374999999992,0.749999999999994,
1.),.UNSPECIFIED.);
#1990=B_SPLINE_CURVE_WITH_KNOTS('',3,(#94333,#94334,#94335,#94336,#94337,
#94338,#94339,#94340,#94341,#94342,#94343,#94344,#94345,#94346,#94347,#94348,
#94349,#94350,#94351,#94352,#94353,#94354,#94355,#94356,#94357,#94358,#94359,
#94360,#94361,#94362,#94363,#94364,#94365,#94366,#94367,#94368,#94369,#94370,
#94371,#94372,#94373,#94374,#94375,#94376,#94377,#94378,#94379,#94380,#94381,
#94382,#94383,#94384,#94385,#94386,#94387,#94388,#94389,#94390,#94391,#94392,
#94393,#94394,#94395,#94396,#94397,#94398,#94399,#94400,#94401,#94402),
 .UNSPECIFIED.,.F.,.F.,(4,3,3,3,3,3,3,3,3,3,3,3,3,3,3,3,3,3,3,3,3,3,3,4),
(0.,0.0421685283686954,0.0866369744043819,0.125000000000004,0.17094832665189,
0.187500000000006,0.218750000000007,0.234375000000007,0.249140524228546,
0.250000000000008,0.321912311030012,0.37500000000001,0.437500000000019,
0.463805676895858,0.491767464400642,0.500000000000027,0.610538966377814,
0.62500000000002,0.669599302244168,0.715427682662428,0.750000000000014,
0.84562680526609,0.943611528143267,1.),.UNSPECIFIED.);
#1991=B_SPLINE_CURVE_WITH_KNOTS('',3,(#94457,#94458,#94459,#94460,#94461,
#94462,#94463,#94464,#94465,#94466,#94467,#94468,#94469,#94470,#94471,#94472,
#94473,#94474,#94475,#94476,#94477,#94478,#94479,#94480,#94481,#94482,#94483,
#94484,#94485,#94486,#94487,#94488,#94489,#94490,#94491,#94492,#94493,#94494,
#94495,#94496,#94497,#94498,#94499,#94500,#94501,#94502,#94503,#94504,#94505,
#94506,#94507,#94508,#94509,#94510,#94511,#94512,#94513,#94514,#94515,#94516,
#94517,#94518,#94519,#94520,#94521,#94522,#94523,#94524,#94525,#94526,#94527,
#94528,#94529,#94530,#94531,#94532,#94533,#94534,#94535,#94536,#94537,#94538,
#94539,#94540,#94541,#94542,#94543,#94544,#94545,#94546,#94547,#94548,#94549,
#94550,#94551,#94552,#94553,#94554,#94555,#94556,#94557,#94558,#94559,#94560,
#94561,#94562,#94563,#94564,#94565,#94566,#94567,#94568,#94569,#94570,#94571,
#94572,#94573,#94574,#94575,#94576,#94577,#94578,#94579,#94580,#94581,#94582,
#94583,#94584,#94585,#94586,#94587,#94588,#94589),.UNSPECIFIED.,.F.,.F.,
(4,3,3,3,3,3,3,3,3,3,3,3,3,3,3,3,3,3,3,3,3,3,3,3,3,3,3,3,3,3,3,3,3,3,3,
3,3,3,3,3,3,3,3,3,4),(0.,0.0624999999997391,0.086998109193101,0.11203275765394,
0.124999999999478,0.187499999999217,0.218749999999087,0.234374999999018,
0.242187499998983,0.247169612134524,0.249999999998949,0.277080795441728,
0.304102886341549,0.312499999998351,0.339182658907482,0.343749999998052,
0.359374999997902,0.367187499997823,0.371093749997786,0.373793883282339,
0.374999999997749,0.402703373425489,0.430374081715073,0.437499999998162,
0.464932402230747,0.468749999998366,0.484374999998472,0.492187499998521,
0.496849922230597,0.49999999999857,0.562499999998951,0.593749999999141,
0.609374999999225,0.618172379943541,0.62499999999931,0.649448676894499,
0.656249999999368,0.670823410234943,0.684559368754563,0.687499999999426,
0.713282747156612,0.741514803940786,0.749999999999541,0.912813131310412,
1.),.UNSPECIFIED.);
#1992=B_SPLINE_CURVE_WITH_KNOTS('',3,(#94624,#94625,#94626,#94627,#94628,
#94629,#94630,#94631,#94632,#94633,#94634,#94635,#94636,#94637,#94638,#94639,
#94640,#94641,#94642,#94643,#94644,#94645,#94646,#94647,#94648,#94649,#94650,
#94651,#94652,#94653,#94654,#94655,#94656,#94657,#94658,#94659,#94660,#94661,
#94662,#94663,#94664,#94665,#94666,#94667,#94668,#94669,#94670,#94671,#94672,
#94673,#94674,#94675,#94676,#94677,#94678),.UNSPECIFIED.,.F.,.F.,(4,3,3,
3,3,3,3,3,3,3,3,3,3,3,3,3,3,3,4),(0.,0.104226424951023,0.205570362215172,
0.250000000000015,0.348038393048773,0.375000000000023,0.437500000000026,
0.468750000000028,0.484375000000025,0.49311565096605,0.500000000000022,
0.578310819460716,0.654062706344688,0.726911775043978,0.795296105809942,
0.861362444821956,0.925281294150355,0.98649217487535,1.),.UNSPECIFIED.);
#1993=B_SPLINE_CURVE_WITH_KNOTS('',5,(#94810,#94811,#94812,#94813,#94814,
#94815,#94816,#94817,#94818,#94819,#94820,#94821,#94822,#94823,#94824,#94825,
#94826,#94827),.UNSPECIFIED.,.F.,.F.,(6,3,3,3,3,6),(0.,0.0563238113023862,
0.160203167534755,0.284130417633147,0.431668352740704,1.),.UNSPECIFIED.);
#1994=B_SPLINE_CURVE_WITH_KNOTS('',5,(#94904,#94905,#94906,#94907,#94908,
#94909,#94910,#94911,#94912),.UNSPECIFIED.,.F.,.F.,(6,3,6),(0.,0.5,1.),
 .UNSPECIFIED.);
#1995=B_SPLINE_CURVE_WITH_KNOTS('',3,(#95027,#95028,#95029,#95030,#95031,
#95032,#95033,#95034,#95035,#95036,#95037,#95038,#95039,#95040,#95041,#95042,
#95043,#95044,#95045,#95046,#95047,#95048,#95049,#95050,#95051,#95052,#95053,
#95054),.UNSPECIFIED.,.F.,.F.,(4,3,3,3,3,3,3,3,3,4),(0.,0.117491825204254,
0.243957063533135,0.37738327291059,0.43527831132456,0.5,0.625775888363041,
0.755819993836895,0.89307218585744,1.),.UNSPECIFIED.);
#1996=B_SPLINE_CURVE_WITH_KNOTS('',3,(#95115,#95116,#95117,#95118,#95119,
#95120,#95121,#95122,#95123,#95124,#95125,#95126,#95127,#95128,#95129,#95130,
#95131,#95132,#95133,#95134,#95135,#95136,#95137,#95138,#95139,#95140,#95141,
#95142,#95143,#95144,#95145,#95146,#95147,#95148,#95149,#95150,#95151,#95152,
#95153,#95154,#95155,#95156,#95157),.UNSPECIFIED.,.F.,.F.,(4,3,3,3,3,3,
3,3,3,3,3,3,3,3,4),(0.,0.0808464238153753,0.164273806551171,0.252181192896881,
0.34484059644842,0.437499999999959,0.468749999999961,0.484374999999962,
0.49822022793353,0.499999999999963,0.589386967039654,0.695533234255982,
0.797674047058454,0.898837023529225,0.999999999999996),.UNSPECIFIED.);
#1997=B_SPLINE_CURVE_WITH_KNOTS('',3,(#95198,#95199,#95200,#95201,#95202,
#95203,#95204,#95205,#95206,#95207,#95208,#95209,#95210,#95211,#95212,#95213,
#95214,#95215,#95216,#95217,#95218,#95219,#95220,#95221,#95222,#95223,#95224,
#95225,#95226,#95227,#95228,#95229,#95230,#95231,#95232,#95233,#95234,#95235,
#95236,#95237,#95238,#95239,#95240),.UNSPECIFIED.,.F.,.F.,(4,3,3,3,3,3,
3,3,3,3,3,3,3,3,4),(0.,0.0938007173938139,0.185901855972414,0.249999999999996,
0.343989025885857,0.374999999999996,0.437499999999994,0.46874999999999,
0.485689475824231,0.499999999999987,0.611288654097174,0.721466525856065,
0.831135504101467,0.939753775588306,1.),.UNSPECIFIED.);
#1998=B_SPLINE_CURVE_WITH_KNOTS('',3,(#95305,#95306,#95307,#95308,#95309,
#95310,#95311,#95312,#95313,#95314),.UNSPECIFIED.,.F.,.F.,(4,3,3,4),(0.,
0.143504699996,0.239445459249329,0.287009399992),.UNSPECIFIED.);
#1999=B_SPLINE_CURVE_WITH_KNOTS('',3,(#95315,#95316,#95317,#95318,#95319,
#95320,#95321,#95322,#95323,#95324),.UNSPECIFIED.,.F.,.F.,(4,3,3,4),(0.,
0.1405201788765,0.248883771899673,0.281040357753),.UNSPECIFIED.);
#2000=B_SPLINE_CURVE_WITH_KNOTS('',3,(#95380,#95381,#95382,#95383,#95384,
#95385,#95386,#95387,#95388,#95389,#95390,#95391,#95392,#95393,#95394,#95395,
#95396,#95397,#95398,#95399,#95400,#95401,#95402,#95403,#95404,#95405,#95406,
#95407,#95408,#95409,#95410),.UNSPECIFIED.,.F.,.F.,(4,3,3,3,3,3,3,3,3,3,
4),(0.,0.103606039248823,0.209200414239989,0.317311627182029,0.426434884947508,
0.535929191910942,0.645077668364674,0.752572851887113,0.858664995978984,
0.962443523493205,0.999999999821951),.UNSPECIFIED.);
#2001=B_SPLINE_CURVE_WITH_KNOTS('',3,(#95412,#95413,#95414,#95415,#95416,
#95417,#95418,#95419,#95420,#95421,#95422,#95423,#95424,#95425,#95426,#95427,
#95428,#95429,#95430,#95431,#95432,#95433,#95434,#95435,#95436,#95437,#95438,
#95439,#95440,#95441,#95442,#95443,#95444,#95445,#95446,#95447,#95448,#95449,
#95450,#95451,#95452,#95453,#95454,#95455,#95456,#95457,#95458,#95459,#95460,
#95461,#95462,#95463,#95464,#95465,#95466,#95467,#95468,#95469,#95470,#95471,
#95472,#95473,#95474,#95475,#95476,#95477,#95478,#95479,#95480,#95481,#95482,
#95483,#95484,#95485,#95486,#95487,#95488,#95489,#95490,#95491,#95492,#95493,
#95494,#95495,#95496,#95497,#95498,#95499,#95500,#95501,#95502),
 .UNSPECIFIED.,.F.,.F.,(4,3,3,3,3,3,3,3,3,3,3,3,3,3,3,3,3,3,3,3,3,3,3,3,
3,3,3,3,3,3,4),(0.,0.0913074651431097,0.114032014272892,0.126273024521462,
0.171275187346726,0.215654286164605,0.250000000000023,0.298193111621357,
0.344962894394445,0.375000000000034,0.437500000000026,0.445173235143761,
0.458879926357822,0.464179160278983,0.46791323451339,0.470646179065875,
0.486232403511859,0.500000000000003,0.55761265328308,0.613032492495676,
0.624999999999972,0.687499999999956,0.71874999999996,0.732930979089932,
0.745933459125306,0.749999999999964,0.825581397342451,0.901338193120674,
0.950669096560337,0.994252840936779,1.),.UNSPECIFIED.);
#2002=B_SPLINE_CURVE_WITH_KNOTS('',3,(#95640,#95641,#95642,#95643,#95644,
#95645,#95646,#95647,#95648,#95649,#95650,#95651,#95652,#95653,#95654,#95655,
#95656,#95657,#95658,#95659,#95660,#95661,#95662,#95663,#95664,#95665,#95666,
#95667,#95668,#95669,#95670,#95671,#95672,#95673,#95674,#95675,#95676,#95677,
#95678,#95679,#95680,#95681,#95682,#95683,#95684,#95685,#95686,#95687,#95688),
 .UNSPECIFIED.,.F.,.F.,(4,3,3,3,3,3,3,3,3,3,3,3,3,3,3,3,4),(0.,0.0625,0.127496392454565,
0.198782421033528,0.25,0.342193251507051,0.429444529148827,0.5,0.567975878480713,
0.632411656728602,0.69280772499897,0.75,0.806943791318981,0.86166436072903,
0.915319828375331,0.967555661113252,1.),.UNSPECIFIED.);
#2003=B_SPLINE_CURVE_WITH_KNOTS('',3,(#95827,#95828,#95829,#95830,#95831,
#95832,#95833,#95834,#95835,#95836,#95837,#95838,#95839,#95840,#95841,#95842,
#95843,#95844,#95845,#95846,#95847,#95848,#95849,#95850,#95851,#95852,#95853,
#95854,#95855,#95856,#95857,#95858,#95859,#95860,#95861,#95862,#95863,#95864,
#95865,#95866,#95867,#95868,#95869,#95870,#95871,#95872,#95873,#95874,#95875,
#95876,#95877,#95878,#95879,#95880,#95881),.UNSPECIFIED.,.F.,.F.,(4,3,3,
3,3,3,3,3,3,3,3,3,3,3,3,3,3,3,4),(0.,0.12433707374752,0.236463112232104,
0.337929106180553,0.432268616281982,0.468749999999944,0.484564663314929,
0.49999999999994,0.579748767028655,0.624999999999925,0.702664260176126,
0.734374999999922,0.743377244119339,0.749999999999923,0.808401595020124,
0.863301770524771,0.915898796756716,0.96483781443388,1.),.UNSPECIFIED.);
#2004=B_SPLINE_CURVE_WITH_KNOTS('',3,(#95915,#95916,#95917,#95918,#95919,
#95920,#95921,#95922,#95923,#95924,#95925,#95926,#95927,#95928,#95929,#95930,
#95931,#95932,#95933,#95934,#95935,#95936,#95937,#95938,#95939,#95940,#95941,
#95942,#95943,#95944,#95945),.UNSPECIFIED.,.F.,.F.,(4,3,3,3,3,3,3,3,3,3,
4),(0.,0.100659233418489,0.201318874239452,0.301978728327487,0.402638920630661,
0.5,0.599561871286431,0.699671403464823,0.800121822811729,0.903065513154291,
1.),.UNSPECIFIED.);
#2005=B_SPLINE_CURVE_WITH_KNOTS('',4,(#95968,#95969,#95970,#95971,#95972),
 .UNSPECIFIED.,.F.,.F.,(5,5),(0.,1.),.UNSPECIFIED.);
#2006=B_SPLINE_CURVE_WITH_KNOTS('',3,(#95993,#95994,#95995,#95996,#95997,
#95998,#95999,#96000,#96001,#96002,#96003,#96004,#96005,#96006,#96007,#96008,
#96009,#96010,#96011,#96012,#96013,#96014,#96015,#96016,#96017,#96018,#96019,
#96020,#96021,#96022,#96023,#96024,#96025,#96026,#96027,#96028,#96029,#96030,
#96031,#96032,#96033,#96034,#96035,#96036,#96037,#96038,#96039,#96040,#96041,
#96042,#96043,#96044,#96045,#96046,#96047),.UNSPECIFIED.,.F.,.F.,(4,3,3,
3,3,3,3,3,3,3,3,3,3,3,3,3,3,3,4),(0.,0.126260093452782,0.241158460346812,
0.339992840904553,0.437500000000044,0.468750000000048,0.484662798051363,
0.500000000000052,0.580119369937759,0.625000000000081,0.70316841264024,
0.734375000000096,0.743449522410721,0.750000000000096,0.809065654268961,
0.864511341100943,0.917619180392791,0.9671021347712,1.),.UNSPECIFIED.);
#2007=B_SPLINE_CURVE_WITH_KNOTS('',5,(#96095,#96096,#96097,#96098,#96099,
#96100,#96101,#96102,#96103,#96104,#96105,#96106,#96107,#96108,#96109,#96110,
#96111,#96112),.UNSPECIFIED.,.F.,.F.,(6,3,3,3,3,6),(2.03426195559,2.39548583384,
2.56639489646,2.72897717597,2.88469745612,2.92554757),.UNSPECIFIED.);
#2008=B_SPLINE_CURVE_WITH_KNOTS('',3,(#96113,#96114,#96115,#96116,#96117,
#96118,#96119,#96120,#96121,#96122),.UNSPECIFIED.,.F.,.F.,(4,3,3,4),(1.69754904882,
1.84161408159244,1.88420275149,2.01561058189),.UNSPECIFIED.);
#2009=B_SPLINE_CURVE_WITH_KNOTS('',3,(#96150,#96151,#96152,#96153,#96154,
#96155,#96156,#96157,#96158,#96159,#96160,#96161,#96162,#96163,#96164,#96165,
#96166,#96167,#96168,#96169,#96170,#96171,#96172,#96173,#96174,#96175,#96176,
#96177,#96178,#96179,#96180,#96181,#96182,#96183,#96184,#96185,#96186),
 .UNSPECIFIED.,.F.,.F.,(4,3,3,3,3,3,3,3,3,3,3,3,4),(1.64809551428,1.7475192804611,
1.85317562308383,1.96283960328877,2.07841864168069,2.10047189796,2.21451207594883,
2.25520583962,2.38637299327516,2.52642486466674,2.57088104253,2.72494913183819,
2.74124708106),.UNSPECIFIED.);
#2010=B_SPLINE_CURVE_WITH_KNOTS('',5,(#96213,#96214,#96215,#96216,#96217,
#96218,#96219,#96220,#96221),.UNSPECIFIED.,.F.,.F.,(6,3,6),(0.,0.436591209475934,
1.),.UNSPECIFIED.);
#2011=B_SPLINE_CURVE_WITH_KNOTS('',3,(#96246,#96247,#96248,#96249,#96250,
#96251,#96252,#96253,#96254,#96255),.UNSPECIFIED.,.F.,.F.,(4,3,3,4),(1.15863824043,
1.30484728031855,1.3519323715,1.47670435084),.UNSPECIFIED.);
#2012=B_SPLINE_CURVE_WITH_KNOTS('',5,(#96257,#96258,#96259,#96260,#96261,
#96262,#96263,#96264,#96265,#96266,#96267,#96268,#96269,#96270,#96271),
 .UNSPECIFIED.,.F.,.F.,(6,3,3,3,6),(1.82800160081,2.13151904383,2.29147741959,
2.45912256669,2.71936718506),.UNSPECIFIED.);
#2013=B_SPLINE_CURVE_WITH_KNOTS('',3,(#96296,#96297,#96298,#96299,#96300,
#96301,#96302,#96303,#96304,#96305,#96306,#96307,#96308,#96309,#96310,#96311,
#96312,#96313,#96314,#96315,#96316,#96317,#96318,#96319,#96320,#96321,#96322,
#96323,#96324,#96325,#96326,#96327,#96328,#96329),.UNSPECIFIED.,.F.,.F.,
(4,3,3,3,3,3,3,3,3,3,3,4),(1.72682805053,1.82706316337451,1.92770774168372,
2.02823087921,2.14486360402001,2.18407667554,2.31552494470154,2.34453942473,
2.49244062175995,2.50972074403,2.678720463,2.86668722779),.UNSPECIFIED.);
#2014=B_SPLINE_CURVE_WITH_KNOTS('',5,(#96381,#96382,#96383,#96384,#96385,
#96386,#96387,#96388,#96389,#96390,#96391,#96392,#96393,#96394,#96395,#96396,
#96397,#96398,#96399,#96400,#96401),.UNSPECIFIED.,.F.,.F.,(6,3,3,3,3,3,
6),(1.66562909398,1.83574953953,2.17637755312,2.34189323073,2.50257634582,
2.65848585647,2.80548129619),.UNSPECIFIED.);
#2015=B_SPLINE_CURVE_WITH_KNOTS('',5,(#96601,#96602,#96603,#96604,#96605,
#96606,#96607,#96608,#96609),.UNSPECIFIED.,.F.,.F.,(6,3,6),(1.82800160081,
2.29147741959,2.71936718506),.UNSPECIFIED.);
#2016=B_SPLINE_CURVE_WITH_KNOTS('',5,(#96615,#96616,#96617,#96618,#96619,
#96620),.UNSPECIFIED.,.F.,.F.,(6,6),(0.,1.),.UNSPECIFIED.);
#2017=B_SPLINE_CURVE_WITH_KNOTS('',5,(#96676,#96677,#96678,#96679,#96680,
#96681,#96682,#96683,#96684),.UNSPECIFIED.,.F.,.F.,(6,3,6),(0.,0.541919025194724,
1.),.UNSPECIFIED.);
#2018=B_SPLINE_CURVE_WITH_KNOTS('',3,(#96800,#96801,#96802,#96803,#96804,
#96805,#96806,#96807,#96808,#96809,#96810,#96811,#96812,#96813,#96814,#96815,
#96816,#96817,#96818,#96819,#96820,#96821,#96822,#96823,#96824,#96825,#96826,
#96827,#96828,#96829,#96830,#96831,#96832,#96833),.UNSPECIFIED.,.F.,.F.,
(4,3,3,3,3,3,3,3,3,3,3,4),(2.03426195559,2.1510096123002,2.25715585151842,
2.35241102166568,2.39548582166195,2.47480008629705,2.55703499531236,2.6389374730589,
2.71532446519286,2.78841164259849,2.85704870664929,2.92554757),
 .UNSPECIFIED.);
#2019=B_SPLINE_CURVE_WITH_KNOTS('',5,(#96895,#96896,#96897,#96898,#96899,
#96900,#96901,#96902,#96903),.UNSPECIFIED.,.F.,.F.,(6,3,6),(0.,0.44808305686451,
1.),.UNSPECIFIED.);
#2020=B_SPLINE_CURVE_WITH_KNOTS('',3,(#96904,#96905,#96906,#96907,#96908,
#96909,#96910,#96911,#96912,#96913,#96914,#96915,#96916,#96917,#96918,#96919,
#96920,#96921,#96922,#96923,#96924,#96925,#96926,#96927,#96928,#96929,#96930,
#96931,#96932,#96933,#96934,#96935,#96936,#96937,#96938,#96939,#96940),
 .UNSPECIFIED.,.F.,.F.,(4,3,3,3,3,3,3,3,3,3,3,3,4),(0.,0.0846906362845857,
0.170916588348621,0.259457677757533,0.349118725584472,0.440002922090847,
0.5,0.590971966453158,0.681170088206319,0.76944906347906,0.856421296291944,
0.941305445099306,1.),.UNSPECIFIED.);
#2021=B_SPLINE_CURVE_WITH_KNOTS('',3,(#96987,#96988,#96989,#96990,#96991,
#96992,#96993,#96994,#96995,#96996,#96997,#96998,#96999),.UNSPECIFIED.,
 .F.,.F.,(4,3,3,3,4),(0.,0.307479208897056,0.622231708274825,0.935862006693834,
1.),.UNSPECIFIED.);
#2022=B_SPLINE_CURVE_WITH_KNOTS('',3,(#97044,#97045,#97046,#97047,#97048,
#97049,#97050,#97051,#97052,#97053,#97054,#97055,#97056),.UNSPECIFIED.,
 .F.,.F.,(4,3,3,3,4),(0.,0.314421563164034,0.629924180845976,0.934742918075105,
1.),.UNSPECIFIED.);
#2023=B_SPLINE_CURVE_WITH_KNOTS('',5,(#97134,#97135,#97136,#97137,#97138,
#97139),.UNSPECIFIED.,.F.,.F.,(6,6),(0.,1.),.UNSPECIFIED.);
#2024=B_SPLINE_CURVE_WITH_KNOTS('',3,(#97140,#97141,#97142,#97143,#97144,
#97145,#97146,#97147,#97148,#97149,#97150,#97151,#97152,#97153,#97154,#97155,
#97156,#97157,#97158,#97159,#97160,#97161,#97162,#97163,#97164,#97165,#97166,
#97167,#97168,#97169,#97170,#97171,#97172,#97173,#97174,#97175,#97176,#97177,
#97178,#97179),.UNSPECIFIED.,.F.,.F.,(4,3,3,3,3,3,3,3,3,3,3,3,3,4),(0.,
0.0817493380761543,0.167757777444047,0.260434121556351,0.356347053996799,
0.453676990608725,0.500000000000004,0.555446107885843,0.657734231357899,
0.750000000000002,0.824982076180982,0.899805956993093,0.97269336693032,
1.),.UNSPECIFIED.);
#2025=B_SPLINE_CURVE_WITH_KNOTS('',3,(#97241,#97242,#97243,#97244,#97245,
#97246,#97247,#97248,#97249,#97250,#97251,#97252,#97253,#97254,#97255,#97256,
#97257,#97258,#97259,#97260,#97261,#97262,#97263,#97264,#97265,#97266,#97267,
#97268,#97269,#97270,#97271,#97272,#97273,#97274),.UNSPECIFIED.,.F.,.F.,
(4,3,3,3,3,3,3,3,3,3,3,4),(0.,0.0958054567289393,0.193447450982335,0.294266519609543,
0.395565390771468,0.499287123804762,0.59780946855357,0.698357101415177,
0.797410250015008,0.898705125007504,0.994263256631534,1.),.UNSPECIFIED.);
#2026=B_SPLINE_CURVE_WITH_KNOTS('',3,(#97275,#97276,#97277,#97278,#97279,
#97280,#97281,#97282,#97283,#97284,#97285,#97286,#97287,#97288,#97289,#97290,
#97291,#97292,#97293,#97294,#97295,#97296,#97297,#97298,#97299,#97300,#97301,
#97302,#97303,#97304,#97305,#97306,#97307,#97308,#97309,#97310,#97311,#97312,
#97313,#97314,#97315,#97316,#97317,#97318,#97319,#97320,#97321,#97322,#97323,
#97324,#97325,#97326),.UNSPECIFIED.,.F.,.F.,(4,3,3,3,3,3,3,3,3,3,3,3,3,
3,3,3,3,4),(0.,0.0625,0.125471806190554,0.187993683396628,0.25,0.312017100075837,
0.374475387343952,0.436933674612067,0.5,0.5625,0.623237451244149,0.683323686394024,
0.741866361912494,0.75,0.819559695460738,0.889734230242426,0.959282737790169,
1.),.UNSPECIFIED.);
#2027=B_SPLINE_CURVE_WITH_KNOTS('',3,(#97465,#97466,#97467,#97468,#97469,
#97470,#97471),.UNSPECIFIED.,.F.,.F.,(4,3,4),(-4.71167786523,-4.28310422559678,
-4.13551354843282),.UNSPECIFIED.);
#2028=B_SPLINE_CURVE_WITH_KNOTS('',5,(#97472,#97473,#97474,#97475,#97476,
#97477),.UNSPECIFIED.,.F.,.F.,(6,6),(-3.40560970652,-2.82953519577),
 .UNSPECIFIED.);
#2029=B_SPLINE_CURVE_WITH_KNOTS('',3,(#97520,#97521,#97522,#97523,#97524,
#97525,#97526,#97527,#97528,#97529,#97530,#97531,#97532,#97533),
 .UNSPECIFIED.,.F.,.F.,(4,2,2,2,2,2,4),(0.22648251624436,0.28310233584346,
0.33972215544256,0.39634359396564,0.452965032488721,0.509586471011801,0.566207909534882),
 .UNSPECIFIED.);
#2030=B_SPLINE_CURVE_WITH_KNOTS('',3,(#97534,#97535,#97536,#97537,#97538,
#97539,#97540,#97541,#97542,#97543,#97544,#97545,#97546,#97547,#97548,#97549,
#97550,#97551,#97552,#97553,#97554,#97555,#97556),.UNSPECIFIED.,.F.,.F.,
(4,2,2,2,2,2,3,2,2,2,4),(0.566207909534882,0.622827729133982,0.679447548733081,
0.736067368332181,0.792687187931281,0.849308626454361,0.905930064977442,
0.962551503500522,1.0191729420236,1.0757927616227,1.1324125812218),
 .UNSPECIFIED.);
#2031=B_SPLINE_CURVE_WITH_KNOTS('',3,(#97583,#97584,#97585,#97586,#97587,
#97588,#97589,#97590,#97591,#97592),.UNSPECIFIED.,.F.,.F.,(4,2,2,2,4),(1.23339450152361,
1.25641237692672,1.35304825225328,1.44970846052674,1.5463686688002),
 .UNSPECIFIED.);
#2032=B_SPLINE_CURVE_WITH_KNOTS('',3,(#97622,#97623,#97624,#97625,#97626,
#97627,#97628,#97629,#97630,#97631),.UNSPECIFIED.,.F.,.F.,(4,2,2,2,4),(0.0736329241578598,
0.0966612073704035,0.193322414740807,0.289959287879085,0.312978165630601),
 .UNSPECIFIED.);
#2033=B_SPLINE_CURVE_WITH_KNOTS('',3,(#97652,#97653,#97654,#97655,#97656,
#97657,#97658,#97659,#97660,#97661),.UNSPECIFIED.,.F.,.F.,(4,2,2,2,4),(-0.699559397876643,
-0.676531114664321,-0.579869907293917,-0.48323303415564,-0.460214156403763),
 .UNSPECIFIED.);
#2034=B_SPLINE_CURVE_WITH_KNOTS('',3,(#97691,#97692,#97693,#97694,#97695,
#97696,#97697,#97698,#97699,#97700),.UNSPECIFIED.,.F.,.F.,(4,2,2,2,4),(0.773184334400102,
0.869844542673565,0.966504750947028,1.06314062627359,1.08615850163623),
 .UNSPECIFIED.);
#2035=B_SPLINE_CURVE_WITH_KNOTS('',3,(#97759,#97760,#97761,#97762,#97763,
#97764),.UNSPECIFIED.,.F.,.F.,(4,2,4),(0.566207909534882,0.622827729133982,
0.679447548733081),.UNSPECIFIED.);
#2036=B_SPLINE_CURVE_WITH_KNOTS('',3,(#97765,#97766,#97767,#97768,#97769,
#97770,#97771,#97772,#97773,#97774,#97775,#97776,#97777,#97778,#97779,#97780,
#97781,#97782,#97783,#97784,#97785,#97786,#97787,#97788,#97789,#97790,#97791,
#97792,#97793,#97794,#97795),.UNSPECIFIED.,.F.,.F.,(4,2,2,2,3,2,2,2,2,2,
2,2,2,2,4),(-0.22648251624436,-0.169862696645261,-0.113242877046161,-0.0566214385230804,
0.,0.0566214385230803,0.113242877046161,0.169862696645261,0.22648251624436,
0.28310233584346,0.33972215544256,0.39634359396564,0.452965032488721,0.509586471011801,
0.566207909534882),.UNSPECIFIED.);
#2037=B_SPLINE_CURVE_WITH_KNOTS('',3,(#97811,#97812,#97813,#97814,#97815,
#97816,#97817,#97818,#97819,#97820),.UNSPECIFIED.,.F.,.F.,(4,2,2,2,4),(-0.312974167276592,
-0.289956291873489,-0.193320416546926,-0.0966602082734631,0.),
 .UNSPECIFIED.);
#2038=B_SPLINE_CURVE_WITH_KNOTS('',3,(#97841,#97842,#97843,#97844,#97845,
#97846,#97847,#97848,#97849,#97850),.UNSPECIFIED.,.F.,.F.,(4,2,2,2,4),(-0.773184334400102,
-0.676524126126639,-0.579863917853176,-0.483228042526613,-0.460210167163969),
 .UNSPECIFIED.);
#2039=B_SPLINE_CURVE_WITH_KNOTS('',3,(#97873,#97874,#97875,#97876,#97877,
#97878,#97879,#97880,#97881,#97882),.UNSPECIFIED.,.F.,.F.,(4,2,2,2,4),(0.846825246192806,
0.869853529405128,0.966514736775532,1.06315160991381,1.08617048766569),
 .UNSPECIFIED.);
#2040=B_SPLINE_CURVE_WITH_KNOTS('',3,(#97903,#97904,#97905,#97906,#97907,
#97908,#97909,#97910,#97911,#97912),.UNSPECIFIED.,.F.,.F.,(4,2,2,2,4),(-1.47275171991159,
-1.44972343669905,-1.35306222932864,-1.25642535619036,-1.23340647843885),
 .UNSPECIFIED.);
#2041=B_SPLINE_CURVE_WITH_KNOTS('',3,(#98184,#98185,#98186,#98187,#98188,
#98189,#98190,#98191,#98192,#98193),.UNSPECIFIED.,.F.,.F.,(4,3,3,4),(-3.40560970652,
-3.15933845109684,-2.86373280280867,-2.82953519577),.UNSPECIFIED.);
#2042=B_SPLINE_CURVE_WITH_KNOTS('',3,(#98244,#98245,#98246,#98247,#98248,
#98249,#98250),.UNSPECIFIED.,.F.,.F.,(4,3,4),(-4.71167786523,-4.23171687797706,
-4.13551351914),.UNSPECIFIED.);
#2043=SHAPE_REPRESENTATION_RELATIONSHIP('SRR','None',#98340,#2053);
#2044=SHAPE_REPRESENTATION_RELATIONSHIP('SRR','None',#98341,#2054);
#2045=SHAPE_REPRESENTATION_RELATIONSHIP('SRR','None',#98342,#2055);
#2046=SHAPE_REPRESENTATION_RELATIONSHIP('SRR','None',#98343,#2056);
#2047=SHAPE_REPRESENTATION_RELATIONSHIP('SRR','None',#98344,#2057);
#2048=SHAPE_REPRESENTATION_RELATIONSHIP('SRR','None',#98345,#2058);
#2049=SHAPE_REPRESENTATION_RELATIONSHIP('SRR','None',#98346,#2059);
#2050=SHAPE_REPRESENTATION_RELATIONSHIP('SRR','None',#98347,#2060);
#2051=SHAPE_REPRESENTATION_RELATIONSHIP('SRR','None',#98348,#2061);
#2052=SHAPE_REPRESENTATION_RELATIONSHIP('SRR','None',#98349,#2062);
#2053=ADVANCED_BREP_SHAPE_REPRESENTATION('',(#2073),#98292);
#2054=ADVANCED_BREP_SHAPE_REPRESENTATION('',(#2074),#98293);
#2055=ADVANCED_BREP_SHAPE_REPRESENTATION('',(#2075),#98294);
#2056=ADVANCED_BREP_SHAPE_REPRESENTATION('',(#2076),#98295);
#2057=ADVANCED_BREP_SHAPE_REPRESENTATION('',(#65),#98296);
#2058=ADVANCED_BREP_SHAPE_REPRESENTATION('',(#2077),#98297);
#2059=ADVANCED_BREP_SHAPE_REPRESENTATION('',(#2078),#98298);
#2060=ADVANCED_BREP_SHAPE_REPRESENTATION('',(#2079),#98299);
#2061=ADVANCED_BREP_SHAPE_REPRESENTATION('',(#2080),#98300);
#2062=ADVANCED_BREP_SHAPE_REPRESENTATION('',(#2081),#98301);
#2063=STYLED_ITEM('',(#98399),#2073);
#2064=STYLED_ITEM('',(#98399),#2074);
#2065=STYLED_ITEM('',(#98399),#2075);
#2066=STYLED_ITEM('',(#98399),#2076);
#2067=STYLED_ITEM('',(#98399),#65);
#2068=STYLED_ITEM('',(#98399),#2077);
#2069=STYLED_ITEM('',(#98399),#2078);
#2070=STYLED_ITEM('',(#98399),#2079);
#2071=STYLED_ITEM('',(#98399),#2080);
#2072=STYLED_ITEM('',(#98399),#2081);
#2073=MANIFOLD_SOLID_BREP('Body1',#34167);
#2074=MANIFOLD_SOLID_BREP('Body1',#34168);
#2075=MANIFOLD_SOLID_BREP('Body1',#34169);
#2076=MANIFOLD_SOLID_BREP('Body1',#34170);
#2077=MANIFOLD_SOLID_BREP('Body1',#34174);
#2078=MANIFOLD_SOLID_BREP('Body1',#34175);
#2079=MANIFOLD_SOLID_BREP('Body1',#34176);
#2080=MANIFOLD_SOLID_BREP('Body1',#34177);
#2081=MANIFOLD_SOLID_BREP('Body1',#34178);
#2082=PLANE('',#34299);
#2083=PLANE('',#34302);
#2084=PLANE('',#34307);
#2085=PLANE('',#34349);
#2086=PLANE('',#34352);
#2087=PLANE('',#34371);
#2088=PLANE('',#34385);
#2089=PLANE('',#34393);
#2090=PLANE('',#34401);
#2091=PLANE('',#34419);
#2092=PLANE('',#34437);
#2093=PLANE('',#34445);
#2094=PLANE('',#34453);
#2095=PLANE('',#34471);
#2096=PLANE('',#34479);
#2097=PLANE('',#34487);
#2098=PLANE('',#34505);
#2099=PLANE('',#34523);
#2100=PLANE('',#34531);
#2101=PLANE('',#34543);
#2102=PLANE('',#34544);
#2103=PLANE('',#34545);
#2104=PLANE('',#34550);
#2105=PLANE('',#34551);
#2106=PLANE('',#34708);
#2107=PLANE('',#34721);
#2108=PLANE('',#34722);
#2109=PLANE('',#34725);
#2110=PLANE('',#34728);
#2111=PLANE('',#34733);
#2112=PLANE('',#34736);
#2113=PLANE('',#34739);
#2114=PLANE('',#34742);
#2115=PLANE('',#34745);
#2116=PLANE('',#34746);
#2117=PLANE('',#34760);
#2118=PLANE('',#34769);
#2119=PLANE('',#34800);
#2120=PLANE('',#34822);
#2121=PLANE('',#34824);
#2122=PLANE('',#34831);
#2123=PLANE('',#34859);
#2124=PLANE('',#34889);
#2125=PLANE('',#34921);
#2126=PLANE('',#34924);
#2127=PLANE('',#34939);
#2128=PLANE('',#34944);
#2129=PLANE('',#34957);
#2130=PLANE('',#34961);
#2131=PLANE('',#34963);
#2132=PLANE('',#34967);
#2133=PLANE('',#34968);
#2134=PLANE('',#34969);
#2135=PLANE('',#34971);
#2136=PLANE('',#34974);
#2137=PLANE('',#34982);
#2138=PLANE('',#34983);
#2139=PLANE('',#35015);
#2140=PLANE('',#35017);
#2141=PLANE('',#35020);
#2142=PLANE('',#35031);
#2143=PLANE('',#35032);
#2144=PLANE('',#35037);
#2145=PLANE('',#35038);
#2146=PLANE('',#35049);
#2147=PLANE('',#35050);
#2148=PLANE('',#35055);
#2149=PLANE('',#35056);
#2150=PLANE('',#35061);
#2151=PLANE('',#35074);
#2152=PLANE('',#35075);
#2153=PLANE('',#35076);
#2154=PLANE('',#35079);
#2155=PLANE('',#35080);
#2156=PLANE('',#35090);
#2157=PLANE('',#35091);
#2158=PLANE('',#35094);
#2159=PLANE('',#35098);
#2160=PLANE('',#35099);
#2161=PLANE('',#35110);
#2162=PLANE('',#35123);
#2163=PLANE('',#35126);
#2164=PLANE('',#35127);
#2165=PLANE('',#35131);
#2166=PLANE('',#35141);
#2167=PLANE('',#35142);
#2168=PLANE('',#35143);
#2169=PLANE('',#35144);
#2170=PLANE('',#35145);
#2171=PLANE('',#35147);
#2172=PLANE('',#35148);
#2173=PLANE('',#35149);
#2174=PLANE('',#35150);
#2175=PLANE('',#35151);
#2176=PLANE('',#35152);
#2177=PLANE('',#35153);
#2178=PLANE('',#35154);
#2179=PLANE('',#35155);
#2180=PLANE('',#35157);
#2181=PLANE('',#35158);
#2182=PLANE('',#35162);
#2183=PLANE('',#35163);
#2184=PLANE('',#35165);
#2185=PLANE('',#35166);
#2186=PLANE('',#35167);
#2187=PLANE('',#35168);
#2188=PLANE('',#35169);
#2189=PLANE('',#35171);
#2190=PLANE('',#35173);
#2191=PLANE('',#35174);
#2192=PLANE('',#35176);
#2193=PLANE('',#35178);
#2194=PLANE('',#35182);
#2195=PLANE('',#35192);
#2196=PLANE('',#35194);
#2197=PLANE('',#35196);
#2198=PLANE('',#35222);
#2199=PLANE('',#35223);
#2200=PLANE('',#35226);
#2201=PLANE('',#35229);
#2202=PLANE('',#35233);
#2203=PLANE('',#35260);
#2204=PLANE('',#35264);
#2205=PLANE('',#35265);
#2206=PLANE('',#35266);
#2207=PLANE('',#35268);
#2208=PLANE('',#35271);
#2209=PLANE('',#35280);
#2210=PLANE('',#35292);
#2211=PLANE('',#35297);
#2212=PLANE('',#35302);
#2213=PLANE('',#35318);
#2214=PLANE('',#35322);
#2215=PLANE('',#35324);
#2216=PLANE('',#35328);
#2217=PLANE('',#35332);
#2218=PLANE('',#35339);
#2219=PLANE('',#35356);
#2220=PLANE('',#35372);
#2221=PLANE('',#35375);
#2222=PLANE('',#35378);
#2223=PLANE('',#35379);
#2224=PLANE('',#35381);
#2225=PLANE('',#35382);
#2226=PLANE('',#35386);
#2227=PLANE('',#35387);
#2228=PLANE('',#35389);
#2229=PLANE('',#35390);
#2230=PLANE('',#35394);
#2231=PLANE('',#35395);
#2232=PLANE('',#35399);
#2233=PLANE('',#35403);
#2234=PLANE('',#35404);
#2235=PLANE('',#35406);
#2236=PLANE('',#35422);
#2237=PLANE('',#35432);
#2238=PLANE('',#35437);
#2239=PLANE('',#35446);
#2240=PLANE('',#35458);
#2241=PLANE('',#35463);
#2242=PLANE('',#35464);
#2243=PLANE('',#35465);
#2244=PLANE('',#35466);
#2245=PLANE('',#35467);
#2246=PLANE('',#35468);
#2247=PLANE('',#35469);
#2248=PLANE('',#35470);
#2249=PLANE('',#35471);
#2250=PLANE('',#35472);
#2251=PLANE('',#35473);
#2252=PLANE('',#35474);
#2253=PLANE('',#35475);
#2254=PLANE('',#35476);
#2255=PLANE('',#35477);
#2256=PLANE('',#35479);
#2257=PLANE('',#35481);
#2258=PLANE('',#35494);
#2259=PLANE('',#35496);
#2260=PLANE('',#35516);
#2261=PLANE('',#35546);
#2262=PLANE('',#35549);
#2263=PLANE('',#35553);
#2264=PLANE('',#35572);
#2265=PLANE('',#35602);
#2266=PLANE('',#35604);
#2267=PLANE('',#35606);
#2268=PLANE('',#35608);
#2269=PLANE('',#35611);
#2270=PLANE('',#35630);
#2271=PLANE('',#35660);
#2272=PLANE('',#35663);
#2273=PLANE('',#35667);
#2274=PLANE('',#35679);
#2275=PLANE('',#35715);
#2276=PLANE('',#35718);
#2277=PLANE('',#35721);
#2278=PLANE('',#35722);
#2279=PLANE('',#35725);
#2280=PLANE('',#35761);
#2281=PLANE('',#35764);
#2282=PLANE('',#35768);
#2283=PLANE('',#35794);
#2284=PLANE('',#35798);
#2285=PLANE('',#35823);
#2286=PLANE('',#35827);
#2287=PLANE('',#35830);
#2288=PLANE('',#35834);
#2289=PLANE('',#35870);
#2290=PLANE('',#35883);
#2291=PLANE('',#35905);
#2292=PLANE('',#35914);
#2293=PLANE('',#36051);
#2294=PLANE('',#36052);
#2295=PLANE('',#36059);
#2296=PLANE('',#36065);
#2297=PLANE('',#36067);
#2298=PLANE('',#36073);
#2299=PLANE('',#36076);
#2300=PLANE('',#36079);
#2301=PLANE('',#36082);
#2302=PLANE('',#36085);
#2303=PLANE('',#36088);
#2304=PLANE('',#36091);
#2305=PLANE('',#36094);
#2306=PLANE('',#36097);
#2307=PLANE('',#36100);
#2308=PLANE('',#36103);
#2309=PLANE('',#36116);
#2310=PLANE('',#36197);
#2311=PLANE('',#36205);
#2312=PLANE('',#36239);
#2313=PLANE('',#36271);
#2314=PLANE('',#36275);
#2315=PLANE('',#36299);
#2316=PLANE('',#36315);
#2317=PLANE('',#36317);
#2318=PLANE('',#36338);
#2319=PLANE('',#36340);
#2320=PLANE('',#36342);
#2321=PLANE('',#36359);
#2322=PLANE('',#36368);
#2323=PLANE('',#36382);
#2324=PLANE('',#36385);
#2325=PLANE('',#36388);
#2326=PLANE('',#36389);
#2327=PLANE('',#36390);
#2328=PLANE('',#36393);
#2329=PLANE('',#36396);
#2330=PLANE('',#36397);
#2331=PLANE('',#36398);
#2332=PLANE('',#36428);
#2333=PLANE('',#36429);
#2334=PLANE('',#36445);
#2335=PLANE('',#36449);
#2336=PLANE('',#36450);
#2337=PLANE('',#36454);
#2338=PLANE('',#36462);
#2339=PLANE('',#36466);
#2340=PLANE('',#36477);
#2341=PLANE('',#36485);
#2342=PLANE('',#36492);
#2343=PLANE('',#36499);
#2344=PLANE('',#36504);
#2345=PLANE('',#36509);
#2346=PLANE('',#36523);
#2347=PLANE('',#36531);
#2348=PLANE('',#36532);
#2349=PLANE('',#36533);
#2350=PLANE('',#36549);
#2351=PLANE('',#36553);
#2352=PLANE('',#36554);
#2353=PLANE('',#36555);
#2354=PLANE('',#36557);
#2355=PLANE('',#36559);
#2356=PLANE('',#36560);
#2357=PLANE('',#36562);
#2358=PLANE('',#36564);
#2359=PLANE('',#36567);
#2360=PLANE('',#36570);
#2361=PLANE('',#36573);
#2362=PLANE('',#36574);
#2363=PLANE('',#36575);
#2364=PLANE('',#36576);
#2365=PLANE('',#36577);
#2366=PLANE('',#36578);
#2367=PLANE('',#36579);
#2368=PLANE('',#36586);
#2369=PLANE('',#36588);
#2370=PLANE('',#36591);
#2371=PLANE('',#36594);
#2372=PLANE('',#36597);
#2373=PLANE('',#36600);
#2374=PLANE('',#36617);
#2375=PLANE('',#36627);
#2376=PLANE('',#36668);
#2377=PLANE('',#36671);
#2378=PLANE('',#36681);
#2379=PLANE('',#36723);
#2380=PLANE('',#36730);
#2381=PLANE('',#36773);
#2382=PLANE('',#36779);
#2383=PLANE('',#36786);
#2384=PLANE('',#36790);
#2385=PLANE('',#36795);
#2386=PLANE('',#36808);
#2387=PLANE('',#36819);
#2388=PLANE('',#36981);
#2389=PLANE('',#37029);
#2390=PLANE('',#37056);
#2391=PLANE('',#37059);
#2392=PLANE('',#37063);
#2393=PLANE('',#37070);
#2394=PLANE('',#37076);
#2395=PLANE('',#37079);
#2396=PLANE('',#37088);
#2397=PLANE('',#37098);
#2398=PLANE('',#37105);
#2399=PLANE('',#37106);
#2400=PLANE('',#37165);
#2401=PLANE('',#37248);
#2402=PLANE('',#37255);
#2403=PLANE('',#37297);
#2404=PLANE('',#37311);
#2405=PLANE('',#37321);
#2406=PLANE('',#37364);
#2407=PLANE('',#37367);
#2408=PLANE('',#37377);
#2409=PLANE('',#37409);
#2410=PLANE('',#37423);
#2411=PLANE('',#37430);
#2412=PLANE('',#37474);
#2413=PLANE('',#37483);
#2414=PLANE('',#37495);
#2415=PLANE('',#37499);
#2416=PLANE('',#37504);
#2417=PLANE('',#37520);
#2418=PLANE('',#37531);
#2419=PLANE('',#37693);
#2420=PLANE('',#37744);
#2421=PLANE('',#37776);
#2422=PLANE('',#37782);
#2423=PLANE('',#37794);
#2424=PLANE('',#37816);
#2425=PLANE('',#37818);
#2426=PLANE('',#37822);
#2427=PLANE('',#37829);
#2428=PLANE('',#37835);
#2429=PLANE('',#37838);
#2430=PLANE('',#37847);
#2431=PLANE('',#37857);
#2432=PLANE('',#37864);
#2433=PLANE('',#37865);
#2434=PLANE('',#37902);
#2435=PLANE('',#37925);
#2436=PLANE('',#37993);
#2437=PLANE('',#38035);
#2438=PLANE('',#38042);
#2439=PLANE('',#38087);
#2440=PLANE('',#38109);
#2441=PLANE('',#38135);
#2442=PLANE('',#38141);
#2443=PLANE('',#38158);
#2444=PLANE('',#38159);
#2445=PLANE('',#38165);
#2446=PLANE('',#38181);
#2447=PLANE('',#38182);
#2448=PLANE('',#38185);
#2449=PLANE('',#38218);
#2450=PLANE('',#38219);
#2451=PLANE('',#38270);
#2452=PLANE('',#38355);
#2453=PLANE('',#38358);
#2454=PLANE('',#38359);
#2455=PLANE('',#38362);
#2456=PLANE('',#38363);
#2457=PLANE('',#38365);
#2458=PLANE('',#38366);
#2459=PLANE('',#38367);
#2460=PLANE('',#38368);
#2461=PLANE('',#38372);
#2462=PLANE('',#38394);
#2463=PLANE('',#38402);
#2464=PLANE('',#38405);
#2465=PLANE('',#38407);
#2466=PLANE('',#38409);
#2467=PLANE('',#38411);
#2468=PLANE('',#38412);
#2469=PLANE('',#38414);
#2470=PLANE('',#38416);
#2471=PLANE('',#38418);
#2472=PLANE('',#38420);
#2473=PLANE('',#38422);
#2474=PLANE('',#38424);
#2475=PLANE('',#38427);
#2476=PLANE('',#38428);
#2477=PLANE('',#38430);
#2478=PLANE('',#38432);
#2479=PLANE('',#38434);
#2480=PLANE('',#38436);
#2481=PLANE('',#38437);
#2482=PLANE('',#38439);
#2483=PLANE('',#38441);
#2484=PLANE('',#38445);
#2485=PLANE('',#38449);
#2486=PLANE('',#38450);
#2487=PLANE('',#38455);
#2488=PLANE('',#38460);
#2489=PLANE('',#38462);
#2490=PLANE('',#38465);
#2491=PLANE('',#38466);
#2492=PLANE('',#38469);
#2493=PLANE('',#38470);
#2494=PLANE('',#38472);
#2495=PLANE('',#38476);
#2496=PLANE('',#38477);
#2497=PLANE('',#38481);
#2498=PLANE('',#38485);
#2499=PLANE('',#38512);
#2500=PLANE('',#38515);
#2501=PLANE('',#38520);
#2502=PLANE('',#38533);
#2503=PLANE('',#38540);
#2504=PLANE('',#38553);
#2505=PLANE('',#38556);
#2506=PLANE('',#38558);
#2507=PLANE('',#38559);
#2508=PLANE('',#38560);
#2509=PLANE('',#38562);
#2510=PLANE('',#38564);
#2511=PLANE('',#38568);
#2512=PLANE('',#38569);
#2513=PLANE('',#38576);
#2514=PLANE('',#38583);
#2515=PLANE('',#38594);
#2516=PLANE('',#38601);
#2517=PLANE('',#38602);
#2518=PLANE('',#38603);
#2519=PLANE('',#38604);
#2520=PLANE('',#38605);
#2521=CYLINDRICAL_SURFACE('',#34296,1.4);
#2522=CYLINDRICAL_SURFACE('',#34304,0.3);
#2523=CYLINDRICAL_SURFACE('',#34350,0.3);
#2524=CYLINDRICAL_SURFACE('',#34353,0.3);
#2525=CYLINDRICAL_SURFACE('',#34359,0.3);
#2526=CYLINDRICAL_SURFACE('',#34361,0.3);
#2527=CYLINDRICAL_SURFACE('',#34363,0.3);
#2528=CYLINDRICAL_SURFACE('',#34368,0.3);
#2529=CYLINDRICAL_SURFACE('',#34372,15.9);
#2530=CYLINDRICAL_SURFACE('',#34381,0.3);
#2531=CYLINDRICAL_SURFACE('',#34383,0.100000000000003);
#2532=CYLINDRICAL_SURFACE('',#34389,0.300000000000001);
#2533=CYLINDRICAL_SURFACE('',#34391,0.100000000000003);
#2534=CYLINDRICAL_SURFACE('',#34397,0.299999999999999);
#2535=CYLINDRICAL_SURFACE('',#34399,0.1);
#2536=CYLINDRICAL_SURFACE('',#34405,0.3);
#2537=CYLINDRICAL_SURFACE('',#34410,15.9);
#2538=CYLINDRICAL_SURFACE('',#34415,0.5);
#2539=CYLINDRICAL_SURFACE('',#34417,0.0999999999999994);
#2540=CYLINDRICAL_SURFACE('',#34423,0.499999999999999);
#2541=CYLINDRICAL_SURFACE('',#34428,15.9);
#2542=CYLINDRICAL_SURFACE('',#34433,0.3);
#2543=CYLINDRICAL_SURFACE('',#34435,0.100000000000003);
#2544=CYLINDRICAL_SURFACE('',#34441,0.3);
#2545=CYLINDRICAL_SURFACE('',#34443,0.1);
#2546=CYLINDRICAL_SURFACE('',#34449,0.300000000000001);
#2547=CYLINDRICAL_SURFACE('',#34451,0.1);
#2548=CYLINDRICAL_SURFACE('',#34457,0.3);
#2549=CYLINDRICAL_SURFACE('',#34459,15.9);
#2550=CYLINDRICAL_SURFACE('',#34467,0.3);
#2551=CYLINDRICAL_SURFACE('',#34469,0.100000000000003);
#2552=CYLINDRICAL_SURFACE('',#34475,0.300000000000001);
#2553=CYLINDRICAL_SURFACE('',#34477,0.100000000000003);
#2554=CYLINDRICAL_SURFACE('',#34483,0.299999999999999);
#2555=CYLINDRICAL_SURFACE('',#34485,0.1);
#2556=CYLINDRICAL_SURFACE('',#34491,0.3);
#2557=CYLINDRICAL_SURFACE('',#34496,15.9);
#2558=CYLINDRICAL_SURFACE('',#34501,0.499999999999999);
#2559=CYLINDRICAL_SURFACE('',#34503,0.100000000000003);
#2560=CYLINDRICAL_SURFACE('',#34509,0.5);
#2561=CYLINDRICAL_SURFACE('',#34514,15.9);
#2562=CYLINDRICAL_SURFACE('',#34519,0.300000000000001);
#2563=CYLINDRICAL_SURFACE('',#34521,0.100000000000003);
#2564=CYLINDRICAL_SURFACE('',#34527,0.3);
#2565=CYLINDRICAL_SURFACE('',#34529,0.1);
#2566=CYLINDRICAL_SURFACE('',#34535,0.3);
#2567=CYLINDRICAL_SURFACE('',#34540,0.3);
#2568=CYLINDRICAL_SURFACE('',#34542,0.1);
#2569=CYLINDRICAL_SURFACE('',#34556,0.999997171346093);
#2570=CYLINDRICAL_SURFACE('',#34601,0.999997171346093);
#2571=CYLINDRICAL_SURFACE('',#34609,0.1);
#2572=CYLINDRICAL_SURFACE('',#34614,0.1);
#2573=CYLINDRICAL_SURFACE('',#34619,0.100000000000003);
#2574=CYLINDRICAL_SURFACE('',#34630,0.100000000000003);
#2575=CYLINDRICAL_SURFACE('',#34641,0.1);
#2576=CYLINDRICAL_SURFACE('',#34646,0.100000000000003);
#2577=CYLINDRICAL_SURFACE('',#34651,0.100000000000003);
#2578=CYLINDRICAL_SURFACE('',#34662,0.1);
#2579=CYLINDRICAL_SURFACE('',#34667,0.1);
#2580=CYLINDRICAL_SURFACE('',#34672,0.100000000000003);
#2581=CYLINDRICAL_SURFACE('',#34683,0.0999999999999994);
#2582=CYLINDRICAL_SURFACE('',#34694,0.1);
#2583=CYLINDRICAL_SURFACE('',#34699,0.100000000000003);
#2584=CYLINDRICAL_SURFACE('',#34707,0.100000000000003);
#2585=CYLINDRICAL_SURFACE('',#34719,14.4);
#2586=CYLINDRICAL_SURFACE('',#34723,1.5);
#2587=CYLINDRICAL_SURFACE('',#34726,1.5);
#2588=CYLINDRICAL_SURFACE('',#34729,1.5);
#2589=CYLINDRICAL_SURFACE('',#34731,1.5);
#2590=CYLINDRICAL_SURFACE('',#34734,14.4);
#2591=CYLINDRICAL_SURFACE('',#34737,1.5);
#2592=CYLINDRICAL_SURFACE('',#34740,1.5);
#2593=CYLINDRICAL_SURFACE('',#34743,1.5);
#2594=CYLINDRICAL_SURFACE('',#34748,1.5);
#2595=CYLINDRICAL_SURFACE('',#34755,4.00389099741);
#2596=CYLINDRICAL_SURFACE('',#34756,4.00389099741);
#2597=CYLINDRICAL_SURFACE('',#34758,0.3);
#2598=CYLINDRICAL_SURFACE('',#34762,0.3);
#2599=CYLINDRICAL_SURFACE('',#34764,3.89050581799);
#2600=CYLINDRICAL_SURFACE('',#34767,0.3);
#2601=CYLINDRICAL_SURFACE('',#34808,16.1875296363);
#2602=CYLINDRICAL_SURFACE('',#34810,26.2647265892);
#2603=CYLINDRICAL_SURFACE('',#34812,12.2773059952);
#2604=CYLINDRICAL_SURFACE('',#34814,12.2773059952);
#2605=CYLINDRICAL_SURFACE('',#34816,26.2647265892);
#2606=CYLINDRICAL_SURFACE('',#34818,16.1875296363);
#2607=CYLINDRICAL_SURFACE('',#34820,5.);
#2608=CYLINDRICAL_SURFACE('',#34842,3.00001776604858);
#2609=CYLINDRICAL_SURFACE('',#34857,0.3);
#2610=CYLINDRICAL_SURFACE('',#34858,0.300000000000002);
#2611=CYLINDRICAL_SURFACE('',#34884,3.00001778010126);
#2612=CYLINDRICAL_SURFACE('',#34885,0.3);
#2613=CYLINDRICAL_SURFACE('',#34887,0.300000000000002);
#2614=CYLINDRICAL_SURFACE('',#34930,5.5);
#2615=CYLINDRICAL_SURFACE('',#34934,5.5);
#2616=CYLINDRICAL_SURFACE('',#34937,0.3);
#2617=CYLINDRICAL_SURFACE('',#34942,0.3);
#2618=CYLINDRICAL_SURFACE('',#34955,0.3);
#2619=CYLINDRICAL_SURFACE('',#34960,0.3);
#2620=CYLINDRICAL_SURFACE('',#34965,6.69050581799);
#2621=CYLINDRICAL_SURFACE('',#34972,6.69050581799);
#2622=CYLINDRICAL_SURFACE('',#34975,4.44342636361);
#2623=CYLINDRICAL_SURFACE('',#34979,6.24342636361);
#2624=CYLINDRICAL_SURFACE('',#35013,16.1);
#2625=CYLINDRICAL_SURFACE('',#35021,16.4);
#2626=CYLINDRICAL_SURFACE('',#35033,17.4);
#2627=CYLINDRICAL_SURFACE('',#35039,16.4);
#2628=CYLINDRICAL_SURFACE('',#35051,17.4);
#2629=CYLINDRICAL_SURFACE('',#35057,16.1);
#2630=CYLINDRICAL_SURFACE('',#35062,7.6);
#2631=CYLINDRICAL_SURFACE('',#35067,0.2);
#2632=CYLINDRICAL_SURFACE('',#35069,7.6);
#2633=CYLINDRICAL_SURFACE('',#35077,16.1);
#2634=CYLINDRICAL_SURFACE('',#35081,7.6);
#2635=CYLINDRICAL_SURFACE('',#35084,0.2);
#2636=CYLINDRICAL_SURFACE('',#35086,0.2);
#2637=CYLINDRICAL_SURFACE('',#35088,7.6);
#2638=CYLINDRICAL_SURFACE('',#35092,7.34342636361001);
#2639=CYLINDRICAL_SURFACE('',#35095,16.1);
#2640=CYLINDRICAL_SURFACE('',#35100,7.34342636361001);
#2641=CYLINDRICAL_SURFACE('',#35102,2.25);
#2642=CYLINDRICAL_SURFACE('',#35108,6.24342636361);
#2643=CYLINDRICAL_SURFACE('',#35111,0.5);
#2644=CYLINDRICAL_SURFACE('',#35113,6.5);
#2645=CYLINDRICAL_SURFACE('',#35115,0.5);
#2646=CYLINDRICAL_SURFACE('',#35117,0.5);
#2647=CYLINDRICAL_SURFACE('',#35119,6.5);
#2648=CYLINDRICAL_SURFACE('',#35121,0.5);
#2649=CYLINDRICAL_SURFACE('',#35124,7.34342636361001);
#2650=CYLINDRICAL_SURFACE('',#35128,16.1);
#2651=CYLINDRICAL_SURFACE('',#35132,7.34342636361001);
#2652=CYLINDRICAL_SURFACE('',#35134,2.25);
#2653=CYLINDRICAL_SURFACE('',#35160,0.700000000000002);
#2654=CYLINDRICAL_SURFACE('',#35161,0.700000000000002);
#2655=CYLINDRICAL_SURFACE('',#35200,0.700000000000002);
#2656=CYLINDRICAL_SURFACE('',#35201,16.4);
#2657=CYLINDRICAL_SURFACE('',#35204,15.4);
#2658=CYLINDRICAL_SURFACE('',#35207,15.4);
#2659=CYLINDRICAL_SURFACE('',#35210,15.4);
#2660=CYLINDRICAL_SURFACE('',#35213,15.4);
#2661=CYLINDRICAL_SURFACE('',#35216,15.4);
#2662=CYLINDRICAL_SURFACE('',#35219,15.4);
#2663=CYLINDRICAL_SURFACE('',#35225,16.7);
#2664=CYLINDRICAL_SURFACE('',#35243,15.4);
#2665=CYLINDRICAL_SURFACE('',#35245,15.4);
#2666=CYLINDRICAL_SURFACE('',#35247,15.4);
#2667=CYLINDRICAL_SURFACE('',#35249,15.4);
#2668=CYLINDRICAL_SURFACE('',#35252,15.4);
#2669=CYLINDRICAL_SURFACE('',#35255,15.4);
#2670=CYLINDRICAL_SURFACE('',#35258,16.4);
#2671=CYLINDRICAL_SURFACE('',#35261,0.700000000000002);
#2672=CYLINDRICAL_SURFACE('',#35262,16.7);
#2673=CYLINDRICAL_SURFACE('',#35282,0.5);
#2674=CYLINDRICAL_SURFACE('',#35284,6.5);
#2675=CYLINDRICAL_SURFACE('',#35286,0.5);
#2676=CYLINDRICAL_SURFACE('',#35288,6.5);
#2677=CYLINDRICAL_SURFACE('',#35290,0.5);
#2678=CYLINDRICAL_SURFACE('',#35293,5.24342636361);
#2679=CYLINDRICAL_SURFACE('',#35295,5.24342636361);
#2680=CYLINDRICAL_SURFACE('',#35298,5.5);
#2681=CYLINDRICAL_SURFACE('',#35300,5.5);
#2682=CYLINDRICAL_SURFACE('',#35304,7.04342636361);
#2683=CYLINDRICAL_SURFACE('',#35306,0.1);
#2684=CYLINDRICAL_SURFACE('',#35308,10.8);
#2685=CYLINDRICAL_SURFACE('',#35310,10.8);
#2686=CYLINDRICAL_SURFACE('',#35312,0.1);
#2687=CYLINDRICAL_SURFACE('',#35314,7.04342636361);
#2688=CYLINDRICAL_SURFACE('',#35316,1.25);
#2689=CYLINDRICAL_SURFACE('',#35326,1.25);
#2690=CYLINDRICAL_SURFACE('',#35329,4.44342636361);
#2691=CYLINDRICAL_SURFACE('',#35333,7.3);
#2692=CYLINDRICAL_SURFACE('',#35336,7.3);
#2693=CYLINDRICAL_SURFACE('',#35340,4.7);
#2694=CYLINDRICAL_SURFACE('',#35348,4.7);
#2695=CYLINDRICAL_SURFACE('',#35357,6.24342636361);
#2696=CYLINDRICAL_SURFACE('',#35360,0.3);
#2697=CYLINDRICAL_SURFACE('',#35363,10.);
#2698=CYLINDRICAL_SURFACE('',#35366,0.3);
#2699=CYLINDRICAL_SURFACE('',#35369,6.24342636361);
#2700=CYLINDRICAL_SURFACE('',#35418,4.44342636361);
#2701=CYLINDRICAL_SURFACE('',#35420,4.44342636361);
#2702=CYLINDRICAL_SURFACE('',#35427,3.);
#2703=CYLINDRICAL_SURFACE('',#35428,0.3);
#2704=CYLINDRICAL_SURFACE('',#35430,0.3);
#2705=CYLINDRICAL_SURFACE('',#35433,0.3);
#2706=CYLINDRICAL_SURFACE('',#35435,0.3);
#2707=CYLINDRICAL_SURFACE('',#35438,0.3);
#2708=CYLINDRICAL_SURFACE('',#35440,0.3);
#2709=CYLINDRICAL_SURFACE('',#35442,5.69050581799);
#2710=CYLINDRICAL_SURFACE('',#35444,0.5);
#2711=CYLINDRICAL_SURFACE('',#35447,1.1);
#2712=CYLINDRICAL_SURFACE('',#35449,3.);
#2713=CYLINDRICAL_SURFACE('',#35451,3.);
#2714=CYLINDRICAL_SURFACE('',#35452,5.24342636361);
#2715=CYLINDRICAL_SURFACE('',#35453,5.24342636361);
#2716=CYLINDRICAL_SURFACE('',#35454,3.);
#2717=CYLINDRICAL_SURFACE('',#35456,1.1);
#2718=CYLINDRICAL_SURFACE('',#35459,0.5);
#2719=CYLINDRICAL_SURFACE('',#35461,5.69050581799);
#2720=CYLINDRICAL_SURFACE('',#35498,0.300000000000002);
#2721=CYLINDRICAL_SURFACE('',#35501,0.299999999999999);
#2722=CYLINDRICAL_SURFACE('',#35505,0.3);
#2723=CYLINDRICAL_SURFACE('',#35512,0.3);
#2724=CYLINDRICAL_SURFACE('',#35520,0.300000000000001);
#2725=CYLINDRICAL_SURFACE('',#35525,0.300000000000001);
#2726=CYLINDRICAL_SURFACE('',#35530,0.300000000000001);
#2727=CYLINDRICAL_SURFACE('',#35535,0.300000000000002);
#2728=CYLINDRICAL_SURFACE('',#35545,0.3);
#2729=CYLINDRICAL_SURFACE('',#35547,0.3);
#2730=CYLINDRICAL_SURFACE('',#35548,0.3);
#2731=CYLINDRICAL_SURFACE('',#35550,0.300000000000001);
#2732=CYLINDRICAL_SURFACE('',#35551,0.300000000000001);
#2733=CYLINDRICAL_SURFACE('',#35552,0.300000000000001);
#2734=CYLINDRICAL_SURFACE('',#35554,0.300000000000002);
#2735=CYLINDRICAL_SURFACE('',#35557,0.3);
#2736=CYLINDRICAL_SURFACE('',#35561,0.3);
#2737=CYLINDRICAL_SURFACE('',#35568,0.299999999999999);
#2738=CYLINDRICAL_SURFACE('',#35576,0.300000000000002);
#2739=CYLINDRICAL_SURFACE('',#35581,0.3);
#2740=CYLINDRICAL_SURFACE('',#35586,0.300000000000002);
#2741=CYLINDRICAL_SURFACE('',#35591,0.300000000000002);
#2742=CYLINDRICAL_SURFACE('',#35601,0.300000000000001);
#2743=CYLINDRICAL_SURFACE('',#35603,0.3);
#2744=CYLINDRICAL_SURFACE('',#35605,0.3);
#2745=CYLINDRICAL_SURFACE('',#35607,0.300000000000001);
#2746=CYLINDRICAL_SURFACE('',#35609,0.300000000000001);
#2747=CYLINDRICAL_SURFACE('',#35610,0.300000000000001);
#2748=CYLINDRICAL_SURFACE('',#35612,0.3);
#2749=CYLINDRICAL_SURFACE('',#35615,0.299999999999999);
#2750=CYLINDRICAL_SURFACE('',#35619,0.3);
#2751=CYLINDRICAL_SURFACE('',#35626,0.3);
#2752=CYLINDRICAL_SURFACE('',#35634,0.300000000000002);
#2753=CYLINDRICAL_SURFACE('',#35639,0.300000000000002);
#2754=CYLINDRICAL_SURFACE('',#35644,0.300000000000002);
#2755=CYLINDRICAL_SURFACE('',#35649,0.300000000000001);
#2756=CYLINDRICAL_SURFACE('',#35659,0.300000000000002);
#2757=CYLINDRICAL_SURFACE('',#35661,0.300000000000001);
#2758=CYLINDRICAL_SURFACE('',#35662,0.3);
#2759=CYLINDRICAL_SURFACE('',#35664,0.3);
#2760=CYLINDRICAL_SURFACE('',#35665,0.300000000000001);
#2761=CYLINDRICAL_SURFACE('',#35666,0.300000000000001);
#2762=CYLINDRICAL_SURFACE('',#35668,0.3);
#2763=CYLINDRICAL_SURFACE('',#35671,0.300000000000001);
#2764=CYLINDRICAL_SURFACE('',#35675,0.3);
#2765=CYLINDRICAL_SURFACE('',#35684,0.3);
#2766=CYLINDRICAL_SURFACE('',#35694,0.3);
#2767=CYLINDRICAL_SURFACE('',#35703,0.300000000000002);
#2768=CYLINDRICAL_SURFACE('',#35704,0.300000000000001);
#2769=CYLINDRICAL_SURFACE('',#35714,0.300000000000002);
#2770=CYLINDRICAL_SURFACE('',#35716,0.300000000000001);
#2771=CYLINDRICAL_SURFACE('',#35717,0.3);
#2772=CYLINDRICAL_SURFACE('',#35719,0.299999999999999);
#2773=CYLINDRICAL_SURFACE('',#35720,0.3);
#2774=CYLINDRICAL_SURFACE('',#35723,0.300000000000001);
#2775=CYLINDRICAL_SURFACE('',#35724,0.3);
#2776=CYLINDRICAL_SURFACE('',#35763,0.300000000000002);
#2777=CYLINDRICAL_SURFACE('',#35767,0.300000000000002);
#2778=CYLINDRICAL_SURFACE('',#35796,0.730765926094);
#2779=CYLINDRICAL_SURFACE('',#35803,0.3);
#2780=CYLINDRICAL_SURFACE('',#35809,0.3);
#2781=CYLINDRICAL_SURFACE('',#35813,0.3);
#2782=CYLINDRICAL_SURFACE('',#35817,0.3);
#2783=CYLINDRICAL_SURFACE('',#35825,1.);
#2784=CYLINDRICAL_SURFACE('',#35828,0.5);
#2785=CYLINDRICAL_SURFACE('',#35831,0.5);
#2786=CYLINDRICAL_SURFACE('',#35838,4.15);
#2787=CYLINDRICAL_SURFACE('',#35841,0.1);
#2788=CYLINDRICAL_SURFACE('',#35844,1.);
#2789=CYLINDRICAL_SURFACE('',#35849,0.0999999999999998);
#2790=CYLINDRICAL_SURFACE('',#35854,0.0999999999999998);
#2791=CYLINDRICAL_SURFACE('',#35860,0.3);
#2792=CYLINDRICAL_SURFACE('',#35862,0.3);
#2793=CYLINDRICAL_SURFACE('',#35865,1.);
#2794=CYLINDRICAL_SURFACE('',#35868,0.1);
#2795=CYLINDRICAL_SURFACE('',#35872,0.5);
#2796=CYLINDRICAL_SURFACE('',#35878,0.5);
#2797=CYLINDRICAL_SURFACE('',#35917,0.3);
#2798=CYLINDRICAL_SURFACE('',#35920,0.3);
#2799=CYLINDRICAL_SURFACE('',#35922,1.);
#2800=CYLINDRICAL_SURFACE('',#35925,0.1);
#2801=CYLINDRICAL_SURFACE('',#35930,0.1);
#2802=CYLINDRICAL_SURFACE('',#35936,0.0999999999999995);
#2803=CYLINDRICAL_SURFACE('',#35944,0.0999999999999999);
#2804=CYLINDRICAL_SURFACE('',#35950,0.1);
#2805=CYLINDRICAL_SURFACE('',#35953,0.0999999999999989);
#2806=CYLINDRICAL_SURFACE('',#35958,0.0999999999999999);
#2807=CYLINDRICAL_SURFACE('',#35967,0.1);
#2808=CYLINDRICAL_SURFACE('',#35972,0.1);
#2809=CYLINDRICAL_SURFACE('',#35977,0.1);
#2810=CYLINDRICAL_SURFACE('',#35982,0.1);
#2811=CYLINDRICAL_SURFACE('',#35987,0.1);
#2812=CYLINDRICAL_SURFACE('',#35989,0.1);
#2813=CYLINDRICAL_SURFACE('',#35992,0.1);
#2814=CYLINDRICAL_SURFACE('',#35998,0.1);
#2815=CYLINDRICAL_SURFACE('',#36000,0.1);
#2816=CYLINDRICAL_SURFACE('',#36003,0.1);
#2817=CYLINDRICAL_SURFACE('',#36009,0.1);
#2818=CYLINDRICAL_SURFACE('',#36020,2.95);
#2819=CYLINDRICAL_SURFACE('',#36025,2.95);
#2820=CYLINDRICAL_SURFACE('',#36030,2.95);
#2821=CYLINDRICAL_SURFACE('',#36034,2.95);
#2822=CYLINDRICAL_SURFACE('',#36039,0.299999999999999);
#2823=CYLINDRICAL_SURFACE('',#36045,0.3);
#2824=CYLINDRICAL_SURFACE('',#36046,0.5);
#2825=CYLINDRICAL_SURFACE('',#36053,1.);
#2826=CYLINDRICAL_SURFACE('',#36060,0.3);
#2827=CYLINDRICAL_SURFACE('',#36062,0.3);
#2828=CYLINDRICAL_SURFACE('',#36066,0.5);
#2829=CYLINDRICAL_SURFACE('',#36070,0.299999999999999);
#2830=CYLINDRICAL_SURFACE('',#36071,0.299999999999999);
#2831=CYLINDRICAL_SURFACE('',#36074,1.);
#2832=CYLINDRICAL_SURFACE('',#36077,0.5);
#2833=CYLINDRICAL_SURFACE('',#36080,0.5);
#2834=CYLINDRICAL_SURFACE('',#36083,0.5);
#2835=CYLINDRICAL_SURFACE('',#36092,0.1);
#2836=CYLINDRICAL_SURFACE('',#36101,0.1);
#2837=CYLINDRICAL_SURFACE('',#36104,2.65);
#2838=CYLINDRICAL_SURFACE('',#36110,0.100000000000001);
#2839=CYLINDRICAL_SURFACE('',#36124,0.0999999999999995);
#2840=CYLINDRICAL_SURFACE('',#36130,0.100000000000001);
#2841=CYLINDRICAL_SURFACE('',#36131,0.0999999999999995);
#2842=CYLINDRICAL_SURFACE('',#36132,0.1);
#2843=CYLINDRICAL_SURFACE('',#36138,0.0999999999999995);
#2844=CYLINDRICAL_SURFACE('',#36146,0.1);
#2845=CYLINDRICAL_SURFACE('',#36151,0.1);
#2846=CYLINDRICAL_SURFACE('',#36156,0.1);
#2847=CYLINDRICAL_SURFACE('',#36161,0.1);
#2848=CYLINDRICAL_SURFACE('',#36166,0.1);
#2849=CYLINDRICAL_SURFACE('',#36168,0.1);
#2850=CYLINDRICAL_SURFACE('',#36170,0.1);
#2851=CYLINDRICAL_SURFACE('',#36173,0.1);
#2852=CYLINDRICAL_SURFACE('',#36175,0.1);
#2853=CYLINDRICAL_SURFACE('',#36181,0.1);
#2854=CYLINDRICAL_SURFACE('',#36183,0.0999999999999994);
#2855=CYLINDRICAL_SURFACE('',#36185,0.1);
#2856=CYLINDRICAL_SURFACE('',#36188,0.1);
#2857=CYLINDRICAL_SURFACE('',#36190,0.1);
#2858=CYLINDRICAL_SURFACE('',#36196,0.1);
#2859=CYLINDRICAL_SURFACE('',#36209,0.3);
#2860=CYLINDRICAL_SURFACE('',#36219,0.3);
#2861=CYLINDRICAL_SURFACE('',#36226,0.299999999999999);
#2862=CYLINDRICAL_SURFACE('',#36232,0.3);
#2863=CYLINDRICAL_SURFACE('',#36249,1.4);
#2864=CYLINDRICAL_SURFACE('',#36251,0.0999999999999999);
#2865=CYLINDRICAL_SURFACE('',#36257,0.0999999999999989);
#2866=CYLINDRICAL_SURFACE('',#36263,0.1);
#2867=CYLINDRICAL_SURFACE('',#36267,1.);
#2868=CYLINDRICAL_SURFACE('',#36281,0.3);
#2869=CYLINDRICAL_SURFACE('',#36287,0.3);
#2870=CYLINDRICAL_SURFACE('',#36288,0.5);
#2871=CYLINDRICAL_SURFACE('',#36289,2.65);
#2872=CYLINDRICAL_SURFACE('',#36290,0.3);
#2873=CYLINDRICAL_SURFACE('',#36297,0.1);
#2874=CYLINDRICAL_SURFACE('',#36310,0.0999999999999999);
#2875=CYLINDRICAL_SURFACE('',#36314,0.5);
#2876=CYLINDRICAL_SURFACE('',#36316,1.);
#2877=CYLINDRICAL_SURFACE('',#36318,0.1);
#2878=CYLINDRICAL_SURFACE('',#36323,0.0999999999999998);
#2879=CYLINDRICAL_SURFACE('',#36328,0.0999999999999998);
#2880=CYLINDRICAL_SURFACE('',#36333,0.1);
#2881=CYLINDRICAL_SURFACE('',#36337,1.);
#2882=CYLINDRICAL_SURFACE('',#36339,1.);
#2883=CYLINDRICAL_SURFACE('',#36341,0.5);
#2884=CYLINDRICAL_SURFACE('',#36343,0.5);
#2885=CYLINDRICAL_SURFACE('',#36347,0.3);
#2886=CYLINDRICAL_SURFACE('',#36352,0.5);
#2887=CYLINDRICAL_SURFACE('',#36353,4.15);
#2888=CYLINDRICAL_SURFACE('',#36355,0.5);
#2889=CYLINDRICAL_SURFACE('',#36357,0.3);
#2890=CYLINDRICAL_SURFACE('',#36367,0.3);
#2891=CYLINDRICAL_SURFACE('',#36379,11.);
#2892=CYLINDRICAL_SURFACE('',#36401,16.4);
#2893=CYLINDRICAL_SURFACE('',#36422,17.4);
#2894=CYLINDRICAL_SURFACE('',#36430,15.);
#2895=CYLINDRICAL_SURFACE('',#36433,2.);
#2896=CYLINDRICAL_SURFACE('',#36436,13.5);
#2897=CYLINDRICAL_SURFACE('',#36439,0.5);
#2898=CYLINDRICAL_SURFACE('',#36442,0.5);
#2899=CYLINDRICAL_SURFACE('',#36446,0.5);
#2900=CYLINDRICAL_SURFACE('',#36451,0.1);
#2901=CYLINDRICAL_SURFACE('',#36455,0.500000000000001);
#2902=CYLINDRICAL_SURFACE('',#36461,0.300000000000002);
#2903=CYLINDRICAL_SURFACE('',#36464,0.3);
#2904=CYLINDRICAL_SURFACE('',#36467,0.1);
#2905=CYLINDRICAL_SURFACE('',#36471,0.300000000000002);
#2906=CYLINDRICAL_SURFACE('',#36476,0.3);
#2907=CYLINDRICAL_SURFACE('',#36479,0.499999999999999);
#2908=CYLINDRICAL_SURFACE('',#36484,0.3);
#2909=CYLINDRICAL_SURFACE('',#36486,15.4);
#2910=CYLINDRICAL_SURFACE('',#36489,0.1);
#2911=CYLINDRICAL_SURFACE('',#36493,0.500000000000001);
#2912=CYLINDRICAL_SURFACE('',#36503,0.300000000000002);
#2913=CYLINDRICAL_SURFACE('',#36506,0.3);
#2914=CYLINDRICAL_SURFACE('',#36510,0.1);
#2915=CYLINDRICAL_SURFACE('',#36512,12.5);
#2916=CYLINDRICAL_SURFACE('',#36517,0.300000000000002);
#2917=CYLINDRICAL_SURFACE('',#36522,0.3);
#2918=CYLINDRICAL_SURFACE('',#36525,0.499999999999999);
#2919=CYLINDRICAL_SURFACE('',#36530,0.3);
#2920=CYLINDRICAL_SURFACE('',#36534,15.);
#2921=CYLINDRICAL_SURFACE('',#36537,2.);
#2922=CYLINDRICAL_SURFACE('',#36540,13.5);
#2923=CYLINDRICAL_SURFACE('',#36543,0.5);
#2924=CYLINDRICAL_SURFACE('',#36546,0.5);
#2925=CYLINDRICAL_SURFACE('',#36550,0.5);
#2926=CYLINDRICAL_SURFACE('',#36556,1.);
#2927=CYLINDRICAL_SURFACE('',#36558,1.);
#2928=CYLINDRICAL_SURFACE('',#36561,1.);
#2929=CYLINDRICAL_SURFACE('',#36563,1.);
#2930=CYLINDRICAL_SURFACE('',#36565,0.5);
#2931=CYLINDRICAL_SURFACE('',#36566,0.5);
#2932=CYLINDRICAL_SURFACE('',#36568,0.5);
#2933=CYLINDRICAL_SURFACE('',#36569,0.5);
#2934=CYLINDRICAL_SURFACE('',#36571,9.15);
#2935=CYLINDRICAL_SURFACE('',#36587,11.2571565141535);
#2936=CYLINDRICAL_SURFACE('',#36589,11.2571565141535);
#2937=CYLINDRICAL_SURFACE('',#36592,11.2571565141535);
#2938=CYLINDRICAL_SURFACE('',#36595,11.2571565141535);
#2939=CYLINDRICAL_SURFACE('',#36598,11.2571565141535);
#2940=CYLINDRICAL_SURFACE('',#36601,11.2571565141535);
#2941=CYLINDRICAL_SURFACE('',#36603,0.3);
#2942=CYLINDRICAL_SURFACE('',#36606,13.516744254);
#2943=CYLINDRICAL_SURFACE('',#36610,0.3);
#2944=CYLINDRICAL_SURFACE('',#36612,0.300000000000001);
#2945=CYLINDRICAL_SURFACE('',#36614,0.3);
#2946=CYLINDRICAL_SURFACE('',#36618,0.3);
#2947=CYLINDRICAL_SURFACE('',#36621,13.516744254);
#2948=CYLINDRICAL_SURFACE('',#36624,0.3);
#2949=CYLINDRICAL_SURFACE('',#36629,0.3);
#2950=CYLINDRICAL_SURFACE('',#36638,0.3);
#2951=CYLINDRICAL_SURFACE('',#36658,0.3);
#2952=CYLINDRICAL_SURFACE('',#36667,0.300000000000002);
#2953=CYLINDRICAL_SURFACE('',#36672,0.3);
#2954=CYLINDRICAL_SURFACE('',#36675,13.6462109523);
#2955=CYLINDRICAL_SURFACE('',#36678,0.3);
#2956=CYLINDRICAL_SURFACE('',#36682,0.3);
#2957=CYLINDRICAL_SURFACE('',#36684,0.3);
#2958=CYLINDRICAL_SURFACE('',#36687,0.3);
#2959=CYLINDRICAL_SURFACE('',#36697,0.300000000000002);
#2960=CYLINDRICAL_SURFACE('',#36710,0.3);
#2961=CYLINDRICAL_SURFACE('',#36715,0.300000000000002);
#2962=CYLINDRICAL_SURFACE('',#36726,7.84541841273);
#2963=CYLINDRICAL_SURFACE('',#36733,14.6875296363);
#2964=CYLINDRICAL_SURFACE('',#36735,0.3);
#2965=CYLINDRICAL_SURFACE('',#36737,0.3);
#2966=CYLINDRICAL_SURFACE('',#36740,0.3);
#2967=CYLINDRICAL_SURFACE('',#36746,0.3);
#2968=CYLINDRICAL_SURFACE('',#36748,0.300000000000002);
#2969=CYLINDRICAL_SURFACE('',#36751,0.300000000000001);
#2970=CYLINDRICAL_SURFACE('',#36780,16.1875296363);
#2971=CYLINDRICAL_SURFACE('',#36788,0.3);
#2972=CYLINDRICAL_SURFACE('',#36793,0.3);
#2973=CYLINDRICAL_SURFACE('',#36797,0.3);
#2974=CYLINDRICAL_SURFACE('',#36806,0.3);
#2975=CYLINDRICAL_SURFACE('',#36810,0.3);
#2976=CYLINDRICAL_SURFACE('',#36813,7.84541841273);
#2977=CYLINDRICAL_SURFACE('',#36816,0.3);
#2978=CYLINDRICAL_SURFACE('',#36820,0.3);
#2979=CYLINDRICAL_SURFACE('',#36822,0.3);
#2980=CYLINDRICAL_SURFACE('',#36825,14.6875296363);
#2981=CYLINDRICAL_SURFACE('',#36828,0.3);
#2982=CYLINDRICAL_SURFACE('',#36840,0.300000000000002);
#2983=CYLINDRICAL_SURFACE('',#36858,0.300000000000002);
#2984=CYLINDRICAL_SURFACE('',#36887,0.3);
#2985=CYLINDRICAL_SURFACE('',#36904,0.299999999999999);
#2986=CYLINDRICAL_SURFACE('',#36922,0.300000000000002);
#2987=CYLINDRICAL_SURFACE('',#36923,0.3);
#2988=CYLINDRICAL_SURFACE('',#36925,0.300000000000002);
#2989=CYLINDRICAL_SURFACE('',#36945,0.3);
#2990=CYLINDRICAL_SURFACE('',#36969,12.5256279976);
#2991=CYLINDRICAL_SURFACE('',#36975,0.3);
#2992=CYLINDRICAL_SURFACE('',#37000,0.3);
#2993=CYLINDRICAL_SURFACE('',#37010,3.);
#2994=CYLINDRICAL_SURFACE('',#37018,0.3);
#2995=CYLINDRICAL_SURFACE('',#37019,0.3);
#2996=CYLINDRICAL_SURFACE('',#37025,0.3);
#2997=CYLINDRICAL_SURFACE('',#37027,0.3);
#2998=CYLINDRICAL_SURFACE('',#37031,0.3);
#2999=CYLINDRICAL_SURFACE('',#37034,0.299999999999999);
#3000=CYLINDRICAL_SURFACE('',#37046,0.3);
#3001=CYLINDRICAL_SURFACE('',#37060,5.19295371933);
#3002=CYLINDRICAL_SURFACE('',#37061,0.3);
#3003=CYLINDRICAL_SURFACE('',#37064,0.3);
#3004=CYLINDRICAL_SURFACE('',#37066,6.34541841273);
#3005=CYLINDRICAL_SURFACE('',#37068,0.3);
#3006=CYLINDRICAL_SURFACE('',#37069,0.3);
#3007=CYLINDRICAL_SURFACE('',#37071,6.34541841273);
#3008=CYLINDRICAL_SURFACE('',#37072,0.3);
#3009=CYLINDRICAL_SURFACE('',#37073,5.19295371933);
#3010=CYLINDRICAL_SURFACE('',#37074,0.3);
#3011=CYLINDRICAL_SURFACE('',#37075,0.3);
#3012=CYLINDRICAL_SURFACE('',#37077,5.19295371933);
#3013=CYLINDRICAL_SURFACE('',#37078,0.3);
#3014=CYLINDRICAL_SURFACE('',#37080,0.3);
#3015=CYLINDRICAL_SURFACE('',#37082,6.34541841273);
#3016=CYLINDRICAL_SURFACE('',#37084,0.3);
#3017=CYLINDRICAL_SURFACE('',#37086,0.3);
#3018=CYLINDRICAL_SURFACE('',#37097,0.300000000000002);
#3019=CYLINDRICAL_SURFACE('',#37107,0.3);
#3020=CYLINDRICAL_SURFACE('',#37108,0.685778366608);
#3021=CYLINDRICAL_SURFACE('',#37113,0.3);
#3022=CYLINDRICAL_SURFACE('',#37115,0.300000000000002);
#3023=CYLINDRICAL_SURFACE('',#37116,0.3);
#3024=CYLINDRICAL_SURFACE('',#37126,0.3);
#3025=CYLINDRICAL_SURFACE('',#37127,7.84541841273);
#3026=CYLINDRICAL_SURFACE('',#37131,0.3);
#3027=CYLINDRICAL_SURFACE('',#37143,0.300000000000002);
#3028=CYLINDRICAL_SURFACE('',#37157,0.3);
#3029=CYLINDRICAL_SURFACE('',#37158,14.6875296363);
#3030=CYLINDRICAL_SURFACE('',#37159,14.6875296363);
#3031=CYLINDRICAL_SURFACE('',#37160,0.3);
#3032=CYLINDRICAL_SURFACE('',#37164,0.300000000000002);
#3033=CYLINDRICAL_SURFACE('',#37166,0.300000000000002);
#3034=CYLINDRICAL_SURFACE('',#37168,0.299999999999999);
#3035=CYLINDRICAL_SURFACE('',#37179,0.3);
#3036=CYLINDRICAL_SURFACE('',#37199,0.300000000000002);
#3037=CYLINDRICAL_SURFACE('',#37202,0.3);
#3038=CYLINDRICAL_SURFACE('',#37204,0.299999999999999);
#3039=CYLINDRICAL_SURFACE('',#37219,0.3);
#3040=CYLINDRICAL_SURFACE('',#37235,0.300000000000002);
#3041=CYLINDRICAL_SURFACE('',#37236,14.6875296363);
#3042=CYLINDRICAL_SURFACE('',#37238,0.999999999999999);
#3043=CYLINDRICAL_SURFACE('',#37240,14.6875296363);
#3044=CYLINDRICAL_SURFACE('',#37242,0.3);
#3045=CYLINDRICAL_SURFACE('',#37244,14.6875296363);
#3046=CYLINDRICAL_SURFACE('',#37246,0.3);
#3047=CYLINDRICAL_SURFACE('',#37249,0.3);
#3048=CYLINDRICAL_SURFACE('',#37251,7.84541841273);
#3049=CYLINDRICAL_SURFACE('',#37253,0.3);
#3050=CYLINDRICAL_SURFACE('',#37256,0.3);
#3051=CYLINDRICAL_SURFACE('',#37279,0.3);
#3052=CYLINDRICAL_SURFACE('',#37286,0.300000000000002);
#3053=CYLINDRICAL_SURFACE('',#37287,0.3);
#3054=CYLINDRICAL_SURFACE('',#37298,0.3);
#3055=CYLINDRICAL_SURFACE('',#37301,13.516744254);
#3056=CYLINDRICAL_SURFACE('',#37305,0.3);
#3057=CYLINDRICAL_SURFACE('',#37307,0.300000000000001);
#3058=CYLINDRICAL_SURFACE('',#37309,0.3);
#3059=CYLINDRICAL_SURFACE('',#37312,0.3);
#3060=CYLINDRICAL_SURFACE('',#37315,13.516744254);
#3061=CYLINDRICAL_SURFACE('',#37318,0.3);
#3062=CYLINDRICAL_SURFACE('',#37323,0.3);
#3063=CYLINDRICAL_SURFACE('',#37333,0.3);
#3064=CYLINDRICAL_SURFACE('',#37353,0.3);
#3065=CYLINDRICAL_SURFACE('',#37362,0.300000000000002);
#3066=CYLINDRICAL_SURFACE('',#37368,0.3);
#3067=CYLINDRICAL_SURFACE('',#37371,13.6462109523);
#3068=CYLINDRICAL_SURFACE('',#37374,0.3);
#3069=CYLINDRICAL_SURFACE('',#37378,0.3);
#3070=CYLINDRICAL_SURFACE('',#37381,0.3);
#3071=CYLINDRICAL_SURFACE('',#37384,0.3);
#3072=CYLINDRICAL_SURFACE('',#37394,0.300000000000002);
#3073=CYLINDRICAL_SURFACE('',#37410,0.3);
#3074=CYLINDRICAL_SURFACE('',#37416,0.300000000000002);
#3075=CYLINDRICAL_SURFACE('',#37426,7.84541841273);
#3076=CYLINDRICAL_SURFACE('',#37433,14.6875296363);
#3077=CYLINDRICAL_SURFACE('',#37435,0.3);
#3078=CYLINDRICAL_SURFACE('',#37437,0.3);
#3079=CYLINDRICAL_SURFACE('',#37440,0.3);
#3080=CYLINDRICAL_SURFACE('',#37446,0.3);
#3081=CYLINDRICAL_SURFACE('',#37448,0.300000000000002);
#3082=CYLINDRICAL_SURFACE('',#37451,0.300000000000001);
#3083=CYLINDRICAL_SURFACE('',#37480,0.3);
#3084=CYLINDRICAL_SURFACE('',#37484,3.);
#3085=CYLINDRICAL_SURFACE('',#37486,16.1875296363);
#3086=CYLINDRICAL_SURFACE('',#37492,0.3);
#3087=CYLINDRICAL_SURFACE('',#37497,0.3);
#3088=CYLINDRICAL_SURFACE('',#37502,0.3);
#3089=CYLINDRICAL_SURFACE('',#37505,0.3);
#3090=CYLINDRICAL_SURFACE('',#37514,15.6875296363);
#3091=CYLINDRICAL_SURFACE('',#37518,0.3);
#3092=CYLINDRICAL_SURFACE('',#37522,0.3);
#3093=CYLINDRICAL_SURFACE('',#37525,7.84541841273);
#3094=CYLINDRICAL_SURFACE('',#37528,0.3);
#3095=CYLINDRICAL_SURFACE('',#37532,0.3);
#3096=CYLINDRICAL_SURFACE('',#37534,0.3);
#3097=CYLINDRICAL_SURFACE('',#37537,14.6875296363);
#3098=CYLINDRICAL_SURFACE('',#37540,0.3);
#3099=CYLINDRICAL_SURFACE('',#37552,0.300000000000002);
#3100=CYLINDRICAL_SURFACE('',#37570,0.300000000000002);
#3101=CYLINDRICAL_SURFACE('',#37598,0.3);
#3102=CYLINDRICAL_SURFACE('',#37615,0.299999999999999);
#3103=CYLINDRICAL_SURFACE('',#37633,0.300000000000002);
#3104=CYLINDRICAL_SURFACE('',#37634,0.3);
#3105=CYLINDRICAL_SURFACE('',#37635,0.300000000000002);
#3106=CYLINDRICAL_SURFACE('',#37655,0.3);
#3107=CYLINDRICAL_SURFACE('',#37678,1.);
#3108=CYLINDRICAL_SURFACE('',#37680,12.5256279976);
#3109=CYLINDRICAL_SURFACE('',#37686,0.3);
#3110=CYLINDRICAL_SURFACE('',#37704,0.0999999999999999);
#3111=CYLINDRICAL_SURFACE('',#37707,0.0999999999999999);
#3112=CYLINDRICAL_SURFACE('',#37713,0.0999999999999999);
#3113=CYLINDRICAL_SURFACE('',#37718,0.0999999999999999);
#3114=CYLINDRICAL_SURFACE('',#37725,0.0999999999999994);
#3115=CYLINDRICAL_SURFACE('',#37730,0.0999999999999994);
#3116=CYLINDRICAL_SURFACE('',#37735,0.0999999999999994);
#3117=CYLINDRICAL_SURFACE('',#37740,0.0999999999999994);
#3118=CYLINDRICAL_SURFACE('',#37754,0.3);
#3119=CYLINDRICAL_SURFACE('',#37763,3.);
#3120=CYLINDRICAL_SURFACE('',#37771,0.3);
#3121=CYLINDRICAL_SURFACE('',#37772,0.3);
#3122=CYLINDRICAL_SURFACE('',#37774,0.300000000000002);
#3123=CYLINDRICAL_SURFACE('',#37777,0.300000000000002);
#3124=CYLINDRICAL_SURFACE('',#37791,0.3);
#3125=CYLINDRICAL_SURFACE('',#37793,0.3);
#3126=CYLINDRICAL_SURFACE('',#37795,0.3);
#3127=CYLINDRICAL_SURFACE('',#37798,0.299999999999999);
#3128=CYLINDRICAL_SURFACE('',#37808,0.3);
#3129=CYLINDRICAL_SURFACE('',#37819,5.19295371933);
#3130=CYLINDRICAL_SURFACE('',#37820,0.3);
#3131=CYLINDRICAL_SURFACE('',#37823,0.3);
#3132=CYLINDRICAL_SURFACE('',#37825,6.34541841273);
#3133=CYLINDRICAL_SURFACE('',#37827,0.3);
#3134=CYLINDRICAL_SURFACE('',#37828,0.3);
#3135=CYLINDRICAL_SURFACE('',#37830,6.34541841273);
#3136=CYLINDRICAL_SURFACE('',#37831,0.3);
#3137=CYLINDRICAL_SURFACE('',#37832,5.19295371933);
#3138=CYLINDRICAL_SURFACE('',#37833,0.3);
#3139=CYLINDRICAL_SURFACE('',#37834,0.3);
#3140=CYLINDRICAL_SURFACE('',#37836,5.19295371933);
#3141=CYLINDRICAL_SURFACE('',#37837,0.3);
#3142=CYLINDRICAL_SURFACE('',#37839,0.3);
#3143=CYLINDRICAL_SURFACE('',#37841,6.34541841273);
#3144=CYLINDRICAL_SURFACE('',#37843,0.3);
#3145=CYLINDRICAL_SURFACE('',#37845,0.3);
#3146=CYLINDRICAL_SURFACE('',#37856,0.300000000000002);
#3147=CYLINDRICAL_SURFACE('',#37866,0.3);
#3148=CYLINDRICAL_SURFACE('',#37867,0.685778366608);
#3149=CYLINDRICAL_SURFACE('',#37872,0.3);
#3150=CYLINDRICAL_SURFACE('',#37874,0.300000000000002);
#3151=CYLINDRICAL_SURFACE('',#37875,0.3);
#3152=CYLINDRICAL_SURFACE('',#37883,0.3);
#3153=CYLINDRICAL_SURFACE('',#37884,7.84541841273);
#3154=CYLINDRICAL_SURFACE('',#37888,0.3);
#3155=CYLINDRICAL_SURFACE('',#37900,0.300000000000002);
#3156=CYLINDRICAL_SURFACE('',#37916,0.3);
#3157=CYLINDRICAL_SURFACE('',#37917,14.6875296363);
#3158=CYLINDRICAL_SURFACE('',#37918,0.999999999999999);
#3159=CYLINDRICAL_SURFACE('',#37919,14.6875296363);
#3160=CYLINDRICAL_SURFACE('',#37920,0.3);
#3161=CYLINDRICAL_SURFACE('',#37924,0.300000000000002);
#3162=CYLINDRICAL_SURFACE('',#37926,0.300000000000002);
#3163=CYLINDRICAL_SURFACE('',#37928,0.299999999999999);
#3164=CYLINDRICAL_SURFACE('',#37939,0.3);
#3165=CYLINDRICAL_SURFACE('',#37959,0.300000000000002);
#3166=CYLINDRICAL_SURFACE('',#37962,0.3);
#3167=CYLINDRICAL_SURFACE('',#37964,0.299999999999999);
#3168=CYLINDRICAL_SURFACE('',#37969,0.0999999999999994);
#3169=CYLINDRICAL_SURFACE('',#37972,0.0999999999999994);
#3170=CYLINDRICAL_SURFACE('',#37974,0.0999999999999994);
#3171=CYLINDRICAL_SURFACE('',#37975,0.0999999999999994);
#3172=CYLINDRICAL_SURFACE('',#37982,0.0999999999999999);
#3173=CYLINDRICAL_SURFACE('',#37987,0.0999999999999999);
#3174=CYLINDRICAL_SURFACE('',#37988,0.0999999999999999);
#3175=CYLINDRICAL_SURFACE('',#37989,0.0999999999999999);
#3176=CYLINDRICAL_SURFACE('',#38009,0.3);
#3177=CYLINDRICAL_SURFACE('',#38022,0.300000000000002);
#3178=CYLINDRICAL_SURFACE('',#38023,14.6875296363);
#3179=CYLINDRICAL_SURFACE('',#38025,0.999999999999999);
#3180=CYLINDRICAL_SURFACE('',#38027,14.6875296363);
#3181=CYLINDRICAL_SURFACE('',#38029,0.3);
#3182=CYLINDRICAL_SURFACE('',#38031,14.6875296363);
#3183=CYLINDRICAL_SURFACE('',#38033,0.3);
#3184=CYLINDRICAL_SURFACE('',#38036,0.3);
#3185=CYLINDRICAL_SURFACE('',#38038,7.84541841273);
#3186=CYLINDRICAL_SURFACE('',#38040,0.3);
#3187=CYLINDRICAL_SURFACE('',#38043,0.3);
#3188=CYLINDRICAL_SURFACE('',#38067,0.3);
#3189=CYLINDRICAL_SURFACE('',#38076,0.300000000000002);
#3190=CYLINDRICAL_SURFACE('',#38077,0.3);
#3191=CYLINDRICAL_SURFACE('',#38094,25.7066723663);
#3192=CYLINDRICAL_SURFACE('',#38097,0.3);
#3193=CYLINDRICAL_SURFACE('',#38100,12.2773059952);
#3194=CYLINDRICAL_SURFACE('',#38117,5.);
#3195=CYLINDRICAL_SURFACE('',#38121,25.7066723663);
#3196=CYLINDRICAL_SURFACE('',#38126,5.);
#3197=CYLINDRICAL_SURFACE('',#38128,0.3);
#3198=CYLINDRICAL_SURFACE('',#38133,12.2773059952);
#3199=CYLINDRICAL_SURFACE('',#38139,0.300000000000002);
#3200=CYLINDRICAL_SURFACE('',#38148,0.300000000000001);
#3201=CYLINDRICAL_SURFACE('',#38150,13.316744254);
#3202=CYLINDRICAL_SURFACE('',#38152,0.3);
#3203=CYLINDRICAL_SURFACE('',#38156,0.3);
#3204=CYLINDRICAL_SURFACE('',#38163,0.300000000000002);
#3205=CYLINDRICAL_SURFACE('',#38169,0.3);
#3206=CYLINDRICAL_SURFACE('',#38171,13.316744254);
#3207=CYLINDRICAL_SURFACE('',#38175,0.3);
#3208=CYLINDRICAL_SURFACE('',#38179,0.300000000000001);
#3209=CYLINDRICAL_SURFACE('',#38183,0.300000000000002);
#3210=CYLINDRICAL_SURFACE('',#38192,0.3);
#3211=CYLINDRICAL_SURFACE('',#38200,13.4462109523);
#3212=CYLINDRICAL_SURFACE('',#38205,2.5);
#3213=CYLINDRICAL_SURFACE('',#38210,13.4462109523);
#3214=CYLINDRICAL_SURFACE('',#38212,0.3);
#3215=CYLINDRICAL_SURFACE('',#38216,0.3);
#3216=CYLINDRICAL_SURFACE('',#38226,0.300000000000002);
#3217=CYLINDRICAL_SURFACE('',#38238,0.3);
#3218=CYLINDRICAL_SURFACE('',#38240,0.300000000000002);
#3219=CYLINDRICAL_SURFACE('',#38248,0.3);
#3220=CYLINDRICAL_SURFACE('',#38250,0.300000000000002);
#3221=CYLINDRICAL_SURFACE('',#38268,0.3);
#3222=CYLINDRICAL_SURFACE('',#38287,0.3);
#3223=CYLINDRICAL_SURFACE('',#38288,0.3);
#3224=CYLINDRICAL_SURFACE('',#38293,16.1875296363);
#3225=CYLINDRICAL_SURFACE('',#38297,3.);
#3226=CYLINDRICAL_SURFACE('',#38311,0.3);
#3227=CYLINDRICAL_SURFACE('',#38315,0.299999999999999);
#3228=CYLINDRICAL_SURFACE('',#38316,16.1875296363);
#3229=CYLINDRICAL_SURFACE('',#38321,3.);
#3230=CYLINDRICAL_SURFACE('',#38326,3.);
#3231=CYLINDRICAL_SURFACE('',#38341,0.3);
#3232=CYLINDRICAL_SURFACE('',#38345,0.3);
#3233=CYLINDRICAL_SURFACE('',#38346,15.6875296363);
#3234=CYLINDRICAL_SURFACE('',#38360,7.28184557105);
#3235=CYLINDRICAL_SURFACE('',#38370,1.2046272227);
#3236=CYLINDRICAL_SURFACE('',#38403,1.5);
#3237=CYLINDRICAL_SURFACE('',#38410,2.54997399005);
#3238=CYLINDRICAL_SURFACE('',#38419,2.55);
#3239=CYLINDRICAL_SURFACE('',#38426,2.55);
#3240=CYLINDRICAL_SURFACE('',#38435,2.54997399005);
#3241=CYLINDRICAL_SURFACE('',#38443,7.35);
#3242=CYLINDRICAL_SURFACE('',#38444,7.35);
#3243=CYLINDRICAL_SURFACE('',#38451,8.85);
#3244=CYLINDRICAL_SURFACE('',#38453,1.8);
#3245=CYLINDRICAL_SURFACE('',#38456,1.8);
#3246=CYLINDRICAL_SURFACE('',#38458,1.5);
#3247=CYLINDRICAL_SURFACE('',#38463,2.54997399005);
#3248=CYLINDRICAL_SURFACE('',#38467,2.54997399005);
#3249=CYLINDRICAL_SURFACE('',#38474,2.55);
#3250=CYLINDRICAL_SURFACE('',#38479,2.55);
#3251=CYLINDRICAL_SURFACE('',#38482,0.3);
#3252=CYLINDRICAL_SURFACE('',#38510,12.3);
#3253=CYLINDRICAL_SURFACE('',#38513,10.35);
#3254=CYLINDRICAL_SURFACE('',#38516,12.3);
#3255=CYLINDRICAL_SURFACE('',#38518,0.3);
#3256=CYLINDRICAL_SURFACE('',#38521,0.3);
#3257=CYLINDRICAL_SURFACE('',#38523,15.55);
#3258=CYLINDRICAL_SURFACE('',#38525,0.3);
#3259=CYLINDRICAL_SURFACE('',#38527,0.299999999999999);
#3260=CYLINDRICAL_SURFACE('',#38529,15.0204936174);
#3261=CYLINDRICAL_SURFACE('',#38531,0.3);
#3262=CYLINDRICAL_SURFACE('',#38534,0.3);
#3263=CYLINDRICAL_SURFACE('',#38536,15.55);
#3264=CYLINDRICAL_SURFACE('',#38538,0.3);
#3265=CYLINDRICAL_SURFACE('',#38541,0.3);
#3266=CYLINDRICAL_SURFACE('',#38543,15.0204936174);
#3267=CYLINDRICAL_SURFACE('',#38545,0.3);
#3268=CYLINDRICAL_SURFACE('',#38547,0.3);
#3269=CYLINDRICAL_SURFACE('',#38549,15.55);
#3270=CYLINDRICAL_SURFACE('',#38551,0.3);
#3271=CYLINDRICAL_SURFACE('',#38554,0.3);
#3272=CYLINDRICAL_SURFACE('',#38565,8.85);
#3273=CYLINDRICAL_SURFACE('',#38573,0.3);
#3274=CYLINDRICAL_SURFACE('',#38574,0.3);
#3275=CYLINDRICAL_SURFACE('',#38580,0.3);
#3276=CYLINDRICAL_SURFACE('',#38581,0.300000000000002);
#3277=CYLINDRICAL_SURFACE('',#38590,0.3);
#3278=CYLINDRICAL_SURFACE('',#38600,0.3);
#3279=FACE_OUTER_BOUND('',#5419,.T.);
#3280=FACE_OUTER_BOUND('',#5420,.T.);
#3281=FACE_OUTER_BOUND('',#5421,.T.);
#3282=FACE_OUTER_BOUND('',#5422,.T.);
#3283=FACE_OUTER_BOUND('',#5423,.T.);
#3284=FACE_OUTER_BOUND('',#5424,.T.);
#3285=FACE_OUTER_BOUND('',#5425,.T.);
#3286=FACE_OUTER_BOUND('',#5429,.T.);
#3287=FACE_OUTER_BOUND('',#5430,.T.);
#3288=FACE_OUTER_BOUND('',#5431,.T.);
#3289=FACE_OUTER_BOUND('',#5432,.T.);
#3290=FACE_OUTER_BOUND('',#5433,.T.);
#3291=FACE_OUTER_BOUND('',#5434,.T.);
#3292=FACE_OUTER_BOUND('',#5435,.T.);
#3293=FACE_OUTER_BOUND('',#5436,.T.);
#3294=FACE_OUTER_BOUND('',#5437,.T.);
#3295=FACE_OUTER_BOUND('',#5438,.T.);
#3296=FACE_OUTER_BOUND('',#5439,.T.);
#3297=FACE_OUTER_BOUND('',#5440,.T.);
#3298=FACE_OUTER_BOUND('',#5441,.T.);
#3299=FACE_OUTER_BOUND('',#5442,.T.);
#3300=FACE_OUTER_BOUND('',#5443,.T.);
#3301=FACE_OUTER_BOUND('',#5444,.T.);
#3302=FACE_OUTER_BOUND('',#5445,.T.);
#3303=FACE_OUTER_BOUND('',#5446,.T.);
#3304=FACE_OUTER_BOUND('',#5447,.T.);
#3305=FACE_OUTER_BOUND('',#5448,.T.);
#3306=FACE_OUTER_BOUND('',#5449,.T.);
#3307=FACE_OUTER_BOUND('',#5450,.T.);
#3308=FACE_OUTER_BOUND('',#5451,.T.);
#3309=FACE_OUTER_BOUND('',#5452,.T.);
#3310=FACE_OUTER_BOUND('',#5453,.T.);
#3311=FACE_OUTER_BOUND('',#5454,.T.);
#3312=FACE_OUTER_BOUND('',#5455,.T.);
#3313=FACE_OUTER_BOUND('',#5456,.T.);
#3314=FACE_OUTER_BOUND('',#5457,.T.);
#3315=FACE_OUTER_BOUND('',#5458,.T.);
#3316=FACE_OUTER_BOUND('',#5459,.T.);
#3317=FACE_OUTER_BOUND('',#5460,.T.);
#3318=FACE_OUTER_BOUND('',#5461,.T.);
#3319=FACE_OUTER_BOUND('',#5462,.T.);
#3320=FACE_OUTER_BOUND('',#5463,.T.);
#3321=FACE_OUTER_BOUND('',#5464,.T.);
#3322=FACE_OUTER_BOUND('',#5465,.T.);
#3323=FACE_OUTER_BOUND('',#5466,.T.);
#3324=FACE_OUTER_BOUND('',#5467,.T.);
#3325=FACE_OUTER_BOUND('',#5468,.T.);
#3326=FACE_OUTER_BOUND('',#5469,.T.);
#3327=FACE_OUTER_BOUND('',#5470,.T.);
#3328=FACE_OUTER_BOUND('',#5471,.T.);
#3329=FACE_OUTER_BOUND('',#5472,.T.);
#3330=FACE_OUTER_BOUND('',#5473,.T.);
#3331=FACE_OUTER_BOUND('',#5474,.T.);
#3332=FACE_OUTER_BOUND('',#5475,.T.);
#3333=FACE_OUTER_BOUND('',#5476,.T.);
#3334=FACE_OUTER_BOUND('',#5477,.T.);
#3335=FACE_OUTER_BOUND('',#5478,.T.);
#3336=FACE_OUTER_BOUND('',#5479,.T.);
#3337=FACE_OUTER_BOUND('',#5480,.T.);
#3338=FACE_OUTER_BOUND('',#5481,.T.);
#3339=FACE_OUTER_BOUND('',#5482,.T.);
#3340=FACE_OUTER_BOUND('',#5483,.T.);
#3341=FACE_OUTER_BOUND('',#5484,.T.);
#3342=FACE_OUTER_BOUND('',#5485,.T.);
#3343=FACE_OUTER_BOUND('',#5486,.T.);
#3344=FACE_OUTER_BOUND('',#5487,.T.);
#3345=FACE_OUTER_BOUND('',#5488,.T.);
#3346=FACE_OUTER_BOUND('',#5489,.T.);
#3347=FACE_OUTER_BOUND('',#5490,.T.);
#3348=FACE_OUTER_BOUND('',#5491,.T.);
#3349=FACE_OUTER_BOUND('',#5492,.T.);
#3350=FACE_OUTER_BOUND('',#5493,.T.);
#3351=FACE_OUTER_BOUND('',#5494,.T.);
#3352=FACE_OUTER_BOUND('',#5495,.T.);
#3353=FACE_OUTER_BOUND('',#5496,.T.);
#3354=FACE_OUTER_BOUND('',#5497,.T.);
#3355=FACE_OUTER_BOUND('',#5498,.T.);
#3356=FACE_OUTER_BOUND('',#5499,.T.);
#3357=FACE_OUTER_BOUND('',#5500,.T.);
#3358=FACE_OUTER_BOUND('',#5501,.T.);
#3359=FACE_OUTER_BOUND('',#5502,.T.);
#3360=FACE_OUTER_BOUND('',#5503,.T.);
#3361=FACE_OUTER_BOUND('',#5504,.T.);
#3362=FACE_OUTER_BOUND('',#5505,.T.);
#3363=FACE_OUTER_BOUND('',#5506,.T.);
#3364=FACE_OUTER_BOUND('',#5507,.T.);
#3365=FACE_OUTER_BOUND('',#5508,.T.);
#3366=FACE_OUTER_BOUND('',#5509,.T.);
#3367=FACE_OUTER_BOUND('',#5510,.T.);
#3368=FACE_OUTER_BOUND('',#5511,.T.);
#3369=FACE_OUTER_BOUND('',#5512,.T.);
#3370=FACE_OUTER_BOUND('',#5513,.T.);
#3371=FACE_OUTER_BOUND('',#5514,.T.);
#3372=FACE_OUTER_BOUND('',#5515,.T.);
#3373=FACE_OUTER_BOUND('',#5516,.T.);
#3374=FACE_OUTER_BOUND('',#5517,.T.);
#3375=FACE_OUTER_BOUND('',#5518,.T.);
#3376=FACE_OUTER_BOUND('',#5519,.T.);
#3377=FACE_OUTER_BOUND('',#5520,.T.);
#3378=FACE_OUTER_BOUND('',#5521,.T.);
#3379=FACE_OUTER_BOUND('',#5522,.T.);
#3380=FACE_OUTER_BOUND('',#5523,.T.);
#3381=FACE_OUTER_BOUND('',#5524,.T.);
#3382=FACE_OUTER_BOUND('',#5525,.T.);
#3383=FACE_OUTER_BOUND('',#5526,.T.);
#3384=FACE_OUTER_BOUND('',#5527,.T.);
#3385=FACE_OUTER_BOUND('',#5528,.T.);
#3386=FACE_OUTER_BOUND('',#5529,.T.);
#3387=FACE_OUTER_BOUND('',#5530,.T.);
#3388=FACE_OUTER_BOUND('',#5531,.T.);
#3389=FACE_OUTER_BOUND('',#5532,.T.);
#3390=FACE_OUTER_BOUND('',#5533,.T.);
#3391=FACE_OUTER_BOUND('',#5534,.T.);
#3392=FACE_OUTER_BOUND('',#5535,.T.);
#3393=FACE_OUTER_BOUND('',#5536,.T.);
#3394=FACE_OUTER_BOUND('',#5537,.T.);
#3395=FACE_OUTER_BOUND('',#5538,.T.);
#3396=FACE_OUTER_BOUND('',#5539,.T.);
#3397=FACE_OUTER_BOUND('',#5540,.T.);
#3398=FACE_OUTER_BOUND('',#5541,.T.);
#3399=FACE_OUTER_BOUND('',#5542,.T.);
#3400=FACE_OUTER_BOUND('',#5543,.T.);
#3401=FACE_OUTER_BOUND('',#5544,.T.);
#3402=FACE_OUTER_BOUND('',#5545,.T.);
#3403=FACE_OUTER_BOUND('',#5546,.T.);
#3404=FACE_OUTER_BOUND('',#5547,.T.);
#3405=FACE_OUTER_BOUND('',#5548,.T.);
#3406=FACE_OUTER_BOUND('',#5549,.T.);
#3407=FACE_OUTER_BOUND('',#5550,.T.);
#3408=FACE_OUTER_BOUND('',#5551,.T.);
#3409=FACE_OUTER_BOUND('',#5552,.T.);
#3410=FACE_OUTER_BOUND('',#5553,.T.);
#3411=FACE_OUTER_BOUND('',#5554,.T.);
#3412=FACE_OUTER_BOUND('',#5555,.T.);
#3413=FACE_OUTER_BOUND('',#5556,.T.);
#3414=FACE_OUTER_BOUND('',#5557,.T.);
#3415=FACE_OUTER_BOUND('',#5558,.T.);
#3416=FACE_OUTER_BOUND('',#5559,.T.);
#3417=FACE_OUTER_BOUND('',#5560,.T.);
#3418=FACE_OUTER_BOUND('',#5561,.T.);
#3419=FACE_OUTER_BOUND('',#5562,.T.);
#3420=FACE_OUTER_BOUND('',#5563,.T.);
#3421=FACE_OUTER_BOUND('',#5564,.T.);
#3422=FACE_OUTER_BOUND('',#5565,.T.);
#3423=FACE_OUTER_BOUND('',#5566,.T.);
#3424=FACE_OUTER_BOUND('',#5567,.T.);
#3425=FACE_OUTER_BOUND('',#5568,.T.);
#3426=FACE_OUTER_BOUND('',#5569,.T.);
#3427=FACE_OUTER_BOUND('',#5570,.T.);
#3428=FACE_OUTER_BOUND('',#5571,.T.);
#3429=FACE_OUTER_BOUND('',#5572,.T.);
#3430=FACE_OUTER_BOUND('',#5573,.T.);
#3431=FACE_OUTER_BOUND('',#5574,.T.);
#3432=FACE_OUTER_BOUND('',#5575,.T.);
#3433=FACE_OUTER_BOUND('',#5576,.T.);
#3434=FACE_OUTER_BOUND('',#5577,.T.);
#3435=FACE_OUTER_BOUND('',#5578,.T.);
#3436=FACE_OUTER_BOUND('',#5579,.T.);
#3437=FACE_OUTER_BOUND('',#5580,.T.);
#3438=FACE_OUTER_BOUND('',#5581,.T.);
#3439=FACE_OUTER_BOUND('',#5582,.T.);
#3440=FACE_OUTER_BOUND('',#5583,.T.);
#3441=FACE_OUTER_BOUND('',#5584,.T.);
#3442=FACE_OUTER_BOUND('',#5585,.T.);
#3443=FACE_OUTER_BOUND('',#5586,.T.);
#3444=FACE_OUTER_BOUND('',#5587,.T.);
#3445=FACE_OUTER_BOUND('',#5588,.T.);
#3446=FACE_OUTER_BOUND('',#5589,.T.);
#3447=FACE_OUTER_BOUND('',#5590,.T.);
#3448=FACE_OUTER_BOUND('',#5591,.T.);
#3449=FACE_OUTER_BOUND('',#5592,.T.);
#3450=FACE_OUTER_BOUND('',#5593,.T.);
#3451=FACE_OUTER_BOUND('',#5594,.T.);
#3452=FACE_OUTER_BOUND('',#5595,.T.);
#3453=FACE_OUTER_BOUND('',#5596,.T.);
#3454=FACE_OUTER_BOUND('',#5597,.T.);
#3455=FACE_OUTER_BOUND('',#5598,.T.);
#3456=FACE_OUTER_BOUND('',#5599,.T.);
#3457=FACE_OUTER_BOUND('',#5600,.T.);
#3458=FACE_OUTER_BOUND('',#5601,.T.);
#3459=FACE_OUTER_BOUND('',#5602,.T.);
#3460=FACE_OUTER_BOUND('',#5603,.T.);
#3461=FACE_OUTER_BOUND('',#5604,.T.);
#3462=FACE_OUTER_BOUND('',#5605,.T.);
#3463=FACE_OUTER_BOUND('',#5606,.T.);
#3464=FACE_OUTER_BOUND('',#5607,.T.);
#3465=FACE_OUTER_BOUND('',#5608,.T.);
#3466=FACE_OUTER_BOUND('',#5609,.T.);
#3467=FACE_OUTER_BOUND('',#5610,.T.);
#3468=FACE_OUTER_BOUND('',#5611,.T.);
#3469=FACE_OUTER_BOUND('',#5612,.T.);
#3470=FACE_OUTER_BOUND('',#5613,.T.);
#3471=FACE_OUTER_BOUND('',#5614,.T.);
#3472=FACE_OUTER_BOUND('',#5615,.T.);
#3473=FACE_OUTER_BOUND('',#5616,.T.);
#3474=FACE_OUTER_BOUND('',#5617,.T.);
#3475=FACE_OUTER_BOUND('',#5618,.T.);
#3476=FACE_OUTER_BOUND('',#5619,.T.);
#3477=FACE_OUTER_BOUND('',#5620,.T.);
#3478=FACE_OUTER_BOUND('',#5621,.T.);
#3479=FACE_OUTER_BOUND('',#5622,.T.);
#3480=FACE_OUTER_BOUND('',#5623,.T.);
#3481=FACE_OUTER_BOUND('',#5624,.T.);
#3482=FACE_OUTER_BOUND('',#5625,.T.);
#3483=FACE_OUTER_BOUND('',#5626,.T.);
#3484=FACE_OUTER_BOUND('',#5627,.T.);
#3485=FACE_OUTER_BOUND('',#5628,.T.);
#3486=FACE_OUTER_BOUND('',#5629,.T.);
#3487=FACE_OUTER_BOUND('',#5630,.T.);
#3488=FACE_OUTER_BOUND('',#5631,.T.);
#3489=FACE_OUTER_BOUND('',#5632,.T.);
#3490=FACE_OUTER_BOUND('',#5634,.T.);
#3491=FACE_OUTER_BOUND('',#5635,.T.);
#3492=FACE_OUTER_BOUND('',#5636,.T.);
#3493=FACE_OUTER_BOUND('',#5637,.T.);
#3494=FACE_OUTER_BOUND('',#5638,.T.);
#3495=FACE_OUTER_BOUND('',#5639,.T.);
#3496=FACE_OUTER_BOUND('',#5640,.T.);
#3497=FACE_OUTER_BOUND('',#5641,.T.);
#3498=FACE_OUTER_BOUND('',#5642,.T.);
#3499=FACE_OUTER_BOUND('',#5643,.T.);
#3500=FACE_OUTER_BOUND('',#5644,.T.);
#3501=FACE_OUTER_BOUND('',#5645,.T.);
#3502=FACE_OUTER_BOUND('',#5646,.T.);
#3503=FACE_OUTER_BOUND('',#5647,.T.);
#3504=FACE_OUTER_BOUND('',#5648,.T.);
#3505=FACE_OUTER_BOUND('',#5649,.T.);
#3506=FACE_OUTER_BOUND('',#5650,.T.);
#3507=FACE_OUTER_BOUND('',#5651,.T.);
#3508=FACE_OUTER_BOUND('',#5652,.T.);
#3509=FACE_OUTER_BOUND('',#5653,.T.);
#3510=FACE_OUTER_BOUND('',#5654,.T.);
#3511=FACE_OUTER_BOUND('',#5655,.T.);
#3512=FACE_OUTER_BOUND('',#5656,.T.);
#3513=FACE_OUTER_BOUND('',#5657,.T.);
#3514=FACE_OUTER_BOUND('',#5658,.T.);
#3515=FACE_OUTER_BOUND('',#5659,.T.);
#3516=FACE_OUTER_BOUND('',#5660,.T.);
#3517=FACE_OUTER_BOUND('',#5661,.T.);
#3518=FACE_OUTER_BOUND('',#5662,.T.);
#3519=FACE_OUTER_BOUND('',#5663,.T.);
#3520=FACE_OUTER_BOUND('',#5664,.T.);
#3521=FACE_OUTER_BOUND('',#5665,.T.);
#3522=FACE_OUTER_BOUND('',#5666,.T.);
#3523=FACE_OUTER_BOUND('',#5667,.T.);
#3524=FACE_OUTER_BOUND('',#5668,.T.);
#3525=FACE_OUTER_BOUND('',#5669,.T.);
#3526=FACE_OUTER_BOUND('',#5670,.T.);
#3527=FACE_OUTER_BOUND('',#5671,.T.);
#3528=FACE_OUTER_BOUND('',#5672,.T.);
#3529=FACE_OUTER_BOUND('',#5673,.T.);
#3530=FACE_OUTER_BOUND('',#5674,.T.);
#3531=FACE_OUTER_BOUND('',#5675,.T.);
#3532=FACE_OUTER_BOUND('',#5676,.T.);
#3533=FACE_OUTER_BOUND('',#5677,.T.);
#3534=FACE_OUTER_BOUND('',#5678,.T.);
#3535=FACE_OUTER_BOUND('',#5679,.T.);
#3536=FACE_OUTER_BOUND('',#5680,.T.);
#3537=FACE_OUTER_BOUND('',#5681,.T.);
#3538=FACE_OUTER_BOUND('',#5682,.T.);
#3539=FACE_OUTER_BOUND('',#5683,.T.);
#3540=FACE_OUTER_BOUND('',#5684,.T.);
#3541=FACE_OUTER_BOUND('',#5685,.T.);
#3542=FACE_OUTER_BOUND('',#5686,.T.);
#3543=FACE_OUTER_BOUND('',#5687,.T.);
#3544=FACE_OUTER_BOUND('',#5688,.T.);
#3545=FACE_OUTER_BOUND('',#5689,.T.);
#3546=FACE_OUTER_BOUND('',#5690,.T.);
#3547=FACE_OUTER_BOUND('',#5691,.T.);
#3548=FACE_OUTER_BOUND('',#5692,.T.);
#3549=FACE_OUTER_BOUND('',#5693,.T.);
#3550=FACE_OUTER_BOUND('',#5694,.T.);
#3551=FACE_OUTER_BOUND('',#5695,.T.);
#3552=FACE_OUTER_BOUND('',#5696,.T.);
#3553=FACE_OUTER_BOUND('',#5697,.T.);
#3554=FACE_OUTER_BOUND('',#5698,.T.);
#3555=FACE_OUTER_BOUND('',#5699,.T.);
#3556=FACE_OUTER_BOUND('',#5700,.T.);
#3557=FACE_OUTER_BOUND('',#5701,.T.);
#3558=FACE_OUTER_BOUND('',#5702,.T.);
#3559=FACE_OUTER_BOUND('',#5703,.T.);
#3560=FACE_OUTER_BOUND('',#5704,.T.);
#3561=FACE_OUTER_BOUND('',#5705,.T.);
#3562=FACE_OUTER_BOUND('',#5706,.T.);
#3563=FACE_OUTER_BOUND('',#5707,.T.);
#3564=FACE_OUTER_BOUND('',#5708,.T.);
#3565=FACE_OUTER_BOUND('',#5709,.T.);
#3566=FACE_OUTER_BOUND('',#5710,.T.);
#3567=FACE_OUTER_BOUND('',#5714,.T.);
#3568=FACE_OUTER_BOUND('',#5715,.T.);
#3569=FACE_OUTER_BOUND('',#5716,.T.);
#3570=FACE_OUTER_BOUND('',#5717,.T.);
#3571=FACE_OUTER_BOUND('',#5718,.T.);
#3572=FACE_OUTER_BOUND('',#5719,.T.);
#3573=FACE_OUTER_BOUND('',#5720,.T.);
#3574=FACE_OUTER_BOUND('',#5721,.T.);
#3575=FACE_OUTER_BOUND('',#5723,.T.);
#3576=FACE_OUTER_BOUND('',#5727,.T.);
#3577=FACE_OUTER_BOUND('',#5731,.T.);
#3578=FACE_OUTER_BOUND('',#5732,.T.);
#3579=FACE_OUTER_BOUND('',#5733,.T.);
#3580=FACE_OUTER_BOUND('',#5734,.T.);
#3581=FACE_OUTER_BOUND('',#5735,.T.);
#3582=FACE_OUTER_BOUND('',#5736,.T.);
#3583=FACE_OUTER_BOUND('',#5737,.T.);
#3584=FACE_OUTER_BOUND('',#5738,.T.);
#3585=FACE_OUTER_BOUND('',#5739,.T.);
#3586=FACE_OUTER_BOUND('',#5740,.T.);
#3587=FACE_OUTER_BOUND('',#5741,.T.);
#3588=FACE_OUTER_BOUND('',#5742,.T.);
#3589=FACE_OUTER_BOUND('',#5743,.T.);
#3590=FACE_OUTER_BOUND('',#5744,.T.);
#3591=FACE_OUTER_BOUND('',#5745,.T.);
#3592=FACE_OUTER_BOUND('',#5746,.T.);
#3593=FACE_OUTER_BOUND('',#5747,.T.);
#3594=FACE_OUTER_BOUND('',#5748,.T.);
#3595=FACE_OUTER_BOUND('',#5749,.T.);
#3596=FACE_OUTER_BOUND('',#5750,.T.);
#3597=FACE_OUTER_BOUND('',#5751,.T.);
#3598=FACE_OUTER_BOUND('',#5752,.T.);
#3599=FACE_OUTER_BOUND('',#5753,.T.);
#3600=FACE_OUTER_BOUND('',#5754,.T.);
#3601=FACE_OUTER_BOUND('',#5755,.T.);
#3602=FACE_OUTER_BOUND('',#5756,.T.);
#3603=FACE_OUTER_BOUND('',#5757,.T.);
#3604=FACE_OUTER_BOUND('',#5758,.T.);
#3605=FACE_OUTER_BOUND('',#5759,.T.);
#3606=FACE_OUTER_BOUND('',#5760,.T.);
#3607=FACE_OUTER_BOUND('',#5761,.T.);
#3608=FACE_OUTER_BOUND('',#5762,.T.);
#3609=FACE_OUTER_BOUND('',#5763,.T.);
#3610=FACE_OUTER_BOUND('',#5764,.T.);
#3611=FACE_OUTER_BOUND('',#5765,.T.);
#3612=FACE_OUTER_BOUND('',#5766,.T.);
#3613=FACE_OUTER_BOUND('',#5767,.T.);
#3614=FACE_OUTER_BOUND('',#5768,.T.);
#3615=FACE_OUTER_BOUND('',#5769,.T.);
#3616=FACE_OUTER_BOUND('',#5770,.T.);
#3617=FACE_OUTER_BOUND('',#5771,.T.);
#3618=FACE_OUTER_BOUND('',#5772,.T.);
#3619=FACE_OUTER_BOUND('',#5773,.T.);
#3620=FACE_OUTER_BOUND('',#5774,.T.);
#3621=FACE_OUTER_BOUND('',#5775,.T.);
#3622=FACE_OUTER_BOUND('',#5776,.T.);
#3623=FACE_OUTER_BOUND('',#5777,.T.);
#3624=FACE_OUTER_BOUND('',#5778,.T.);
#3625=FACE_OUTER_BOUND('',#5779,.T.);
#3626=FACE_OUTER_BOUND('',#5780,.T.);
#3627=FACE_OUTER_BOUND('',#5781,.T.);
#3628=FACE_OUTER_BOUND('',#5782,.T.);
#3629=FACE_OUTER_BOUND('',#5783,.T.);
#3630=FACE_OUTER_BOUND('',#5784,.T.);
#3631=FACE_OUTER_BOUND('',#5785,.T.);
#3632=FACE_OUTER_BOUND('',#5786,.T.);
#3633=FACE_OUTER_BOUND('',#5787,.T.);
#3634=FACE_OUTER_BOUND('',#5788,.T.);
#3635=FACE_OUTER_BOUND('',#5789,.T.);
#3636=FACE_OUTER_BOUND('',#5790,.T.);
#3637=FACE_OUTER_BOUND('',#5791,.T.);
#3638=FACE_OUTER_BOUND('',#5792,.T.);
#3639=FACE_OUTER_BOUND('',#5793,.T.);
#3640=FACE_OUTER_BOUND('',#5794,.T.);
#3641=FACE_OUTER_BOUND('',#5795,.T.);
#3642=FACE_OUTER_BOUND('',#5796,.T.);
#3643=FACE_OUTER_BOUND('',#5797,.T.);
#3644=FACE_OUTER_BOUND('',#5798,.T.);
#3645=FACE_OUTER_BOUND('',#5799,.T.);
#3646=FACE_OUTER_BOUND('',#5800,.T.);
#3647=FACE_OUTER_BOUND('',#5801,.T.);
#3648=FACE_OUTER_BOUND('',#5802,.T.);
#3649=FACE_OUTER_BOUND('',#5803,.T.);
#3650=FACE_OUTER_BOUND('',#5804,.T.);
#3651=FACE_OUTER_BOUND('',#5805,.T.);
#3652=FACE_OUTER_BOUND('',#5806,.T.);
#3653=FACE_OUTER_BOUND('',#5807,.T.);
#3654=FACE_OUTER_BOUND('',#5808,.T.);
#3655=FACE_OUTER_BOUND('',#5809,.T.);
#3656=FACE_OUTER_BOUND('',#5810,.T.);
#3657=FACE_OUTER_BOUND('',#5811,.T.);
#3658=FACE_OUTER_BOUND('',#5812,.T.);
#3659=FACE_OUTER_BOUND('',#5813,.T.);
#3660=FACE_OUTER_BOUND('',#5814,.T.);
#3661=FACE_OUTER_BOUND('',#5815,.T.);
#3662=FACE_OUTER_BOUND('',#5816,.T.);
#3663=FACE_OUTER_BOUND('',#5817,.T.);
#3664=FACE_OUTER_BOUND('',#5818,.T.);
#3665=FACE_OUTER_BOUND('',#5819,.T.);
#3666=FACE_OUTER_BOUND('',#5820,.T.);
#3667=FACE_OUTER_BOUND('',#5821,.T.);
#3668=FACE_OUTER_BOUND('',#5822,.T.);
#3669=FACE_OUTER_BOUND('',#5823,.T.);
#3670=FACE_OUTER_BOUND('',#5824,.T.);
#3671=FACE_OUTER_BOUND('',#5825,.T.);
#3672=FACE_OUTER_BOUND('',#5826,.T.);
#3673=FACE_OUTER_BOUND('',#5827,.T.);
#3674=FACE_OUTER_BOUND('',#5828,.T.);
#3675=FACE_OUTER_BOUND('',#5829,.T.);
#3676=FACE_OUTER_BOUND('',#5830,.T.);
#3677=FACE_OUTER_BOUND('',#5831,.T.);
#3678=FACE_OUTER_BOUND('',#5832,.T.);
#3679=FACE_OUTER_BOUND('',#5833,.T.);
#3680=FACE_OUTER_BOUND('',#5834,.T.);
#3681=FACE_OUTER_BOUND('',#5835,.T.);
#3682=FACE_OUTER_BOUND('',#5836,.T.);
#3683=FACE_OUTER_BOUND('',#5837,.T.);
#3684=FACE_OUTER_BOUND('',#5838,.T.);
#3685=FACE_OUTER_BOUND('',#5839,.T.);
#3686=FACE_OUTER_BOUND('',#5843,.T.);
#3687=FACE_OUTER_BOUND('',#5847,.T.);
#3688=FACE_OUTER_BOUND('',#5848,.T.);
#3689=FACE_OUTER_BOUND('',#5849,.T.);
#3690=FACE_OUTER_BOUND('',#5850,.T.);
#3691=FACE_OUTER_BOUND('',#5851,.T.);
#3692=FACE_OUTER_BOUND('',#5852,.T.);
#3693=FACE_OUTER_BOUND('',#5853,.T.);
#3694=FACE_OUTER_BOUND('',#5854,.T.);
#3695=FACE_OUTER_BOUND('',#5855,.T.);
#3696=FACE_OUTER_BOUND('',#5856,.T.);
#3697=FACE_OUTER_BOUND('',#5857,.T.);
#3698=FACE_OUTER_BOUND('',#5858,.T.);
#3699=FACE_OUTER_BOUND('',#5859,.T.);
#3700=FACE_OUTER_BOUND('',#5860,.T.);
#3701=FACE_OUTER_BOUND('',#5861,.T.);
#3702=FACE_OUTER_BOUND('',#5862,.T.);
#3703=FACE_OUTER_BOUND('',#5863,.T.);
#3704=FACE_OUTER_BOUND('',#5864,.T.);
#3705=FACE_OUTER_BOUND('',#5865,.T.);
#3706=FACE_OUTER_BOUND('',#5866,.T.);
#3707=FACE_OUTER_BOUND('',#5867,.T.);
#3708=FACE_OUTER_BOUND('',#5868,.T.);
#3709=FACE_OUTER_BOUND('',#5869,.T.);
#3710=FACE_OUTER_BOUND('',#5870,.T.);
#3711=FACE_OUTER_BOUND('',#5871,.T.);
#3712=FACE_OUTER_BOUND('',#5872,.T.);
#3713=FACE_OUTER_BOUND('',#5873,.T.);
#3714=FACE_OUTER_BOUND('',#5874,.T.);
#3715=FACE_OUTER_BOUND('',#5875,.T.);
#3716=FACE_OUTER_BOUND('',#5876,.T.);
#3717=FACE_OUTER_BOUND('',#5877,.T.);
#3718=FACE_OUTER_BOUND('',#5878,.T.);
#3719=FACE_OUTER_BOUND('',#5879,.T.);
#3720=FACE_OUTER_BOUND('',#5880,.T.);
#3721=FACE_OUTER_BOUND('',#5881,.T.);
#3722=FACE_OUTER_BOUND('',#5882,.T.);
#3723=FACE_OUTER_BOUND('',#5883,.T.);
#3724=FACE_OUTER_BOUND('',#5884,.T.);
#3725=FACE_OUTER_BOUND('',#5885,.T.);
#3726=FACE_OUTER_BOUND('',#5886,.T.);
#3727=FACE_OUTER_BOUND('',#5887,.T.);
#3728=FACE_OUTER_BOUND('',#5888,.T.);
#3729=FACE_OUTER_BOUND('',#5889,.T.);
#3730=FACE_OUTER_BOUND('',#5890,.T.);
#3731=FACE_OUTER_BOUND('',#5891,.T.);
#3732=FACE_OUTER_BOUND('',#5892,.T.);
#3733=FACE_OUTER_BOUND('',#5893,.T.);
#3734=FACE_OUTER_BOUND('',#5894,.T.);
#3735=FACE_OUTER_BOUND('',#5895,.T.);
#3736=FACE_OUTER_BOUND('',#5896,.T.);
#3737=FACE_OUTER_BOUND('',#5897,.T.);
#3738=FACE_OUTER_BOUND('',#5898,.T.);
#3739=FACE_OUTER_BOUND('',#5899,.T.);
#3740=FACE_OUTER_BOUND('',#5900,.T.);
#3741=FACE_OUTER_BOUND('',#5901,.T.);
#3742=FACE_OUTER_BOUND('',#5902,.T.);
#3743=FACE_OUTER_BOUND('',#5909,.T.);
#3744=FACE_OUTER_BOUND('',#5910,.T.);
#3745=FACE_OUTER_BOUND('',#5911,.T.);
#3746=FACE_OUTER_BOUND('',#5912,.T.);
#3747=FACE_OUTER_BOUND('',#5913,.T.);
#3748=FACE_OUTER_BOUND('',#5914,.T.);
#3749=FACE_OUTER_BOUND('',#5915,.T.);
#3750=FACE_OUTER_BOUND('',#5916,.T.);
#3751=FACE_OUTER_BOUND('',#5917,.T.);
#3752=FACE_OUTER_BOUND('',#5918,.T.);
#3753=FACE_OUTER_BOUND('',#5919,.T.);
#3754=FACE_OUTER_BOUND('',#5920,.T.);
#3755=FACE_OUTER_BOUND('',#5921,.T.);
#3756=FACE_OUTER_BOUND('',#5922,.T.);
#3757=FACE_OUTER_BOUND('',#5923,.T.);
#3758=FACE_OUTER_BOUND('',#5924,.T.);
#3759=FACE_OUTER_BOUND('',#5925,.T.);
#3760=FACE_OUTER_BOUND('',#5926,.T.);
#3761=FACE_OUTER_BOUND('',#5927,.T.);
#3762=FACE_OUTER_BOUND('',#5928,.T.);
#3763=FACE_OUTER_BOUND('',#5929,.T.);
#3764=FACE_OUTER_BOUND('',#5930,.T.);
#3765=FACE_OUTER_BOUND('',#5931,.T.);
#3766=FACE_OUTER_BOUND('',#5932,.T.);
#3767=FACE_OUTER_BOUND('',#5933,.T.);
#3768=FACE_OUTER_BOUND('',#5934,.T.);
#3769=FACE_OUTER_BOUND('',#5935,.T.);
#3770=FACE_OUTER_BOUND('',#5936,.T.);
#3771=FACE_OUTER_BOUND('',#5937,.T.);
#3772=FACE_OUTER_BOUND('',#5938,.T.);
#3773=FACE_OUTER_BOUND('',#5939,.T.);
#3774=FACE_OUTER_BOUND('',#5940,.T.);
#3775=FACE_OUTER_BOUND('',#5941,.T.);
#3776=FACE_OUTER_BOUND('',#5942,.T.);
#3777=FACE_OUTER_BOUND('',#5943,.T.);
#3778=FACE_OUTER_BOUND('',#5944,.T.);
#3779=FACE_OUTER_BOUND('',#5945,.T.);
#3780=FACE_OUTER_BOUND('',#5946,.T.);
#3781=FACE_OUTER_BOUND('',#5947,.T.);
#3782=FACE_OUTER_BOUND('',#5948,.T.);
#3783=FACE_OUTER_BOUND('',#5949,.T.);
#3784=FACE_OUTER_BOUND('',#5950,.T.);
#3785=FACE_OUTER_BOUND('',#5951,.T.);
#3786=FACE_OUTER_BOUND('',#5952,.T.);
#3787=FACE_OUTER_BOUND('',#5953,.T.);
#3788=FACE_OUTER_BOUND('',#5954,.T.);
#3789=FACE_OUTER_BOUND('',#5955,.T.);
#3790=FACE_OUTER_BOUND('',#5956,.T.);
#3791=FACE_OUTER_BOUND('',#5957,.T.);
#3792=FACE_OUTER_BOUND('',#5958,.T.);
#3793=FACE_OUTER_BOUND('',#5959,.T.);
#3794=FACE_OUTER_BOUND('',#5960,.T.);
#3795=FACE_OUTER_BOUND('',#5961,.T.);
#3796=FACE_OUTER_BOUND('',#5962,.T.);
#3797=FACE_OUTER_BOUND('',#5963,.T.);
#3798=FACE_OUTER_BOUND('',#5964,.T.);
#3799=FACE_OUTER_BOUND('',#5965,.T.);
#3800=FACE_OUTER_BOUND('',#5966,.T.);
#3801=FACE_OUTER_BOUND('',#5967,.T.);
#3802=FACE_OUTER_BOUND('',#5968,.T.);
#3803=FACE_OUTER_BOUND('',#5969,.T.);
#3804=FACE_OUTER_BOUND('',#5970,.T.);
#3805=FACE_OUTER_BOUND('',#5971,.T.);
#3806=FACE_OUTER_BOUND('',#5972,.T.);
#3807=FACE_OUTER_BOUND('',#5973,.T.);
#3808=FACE_OUTER_BOUND('',#5974,.T.);
#3809=FACE_OUTER_BOUND('',#5975,.T.);
#3810=FACE_OUTER_BOUND('',#5976,.T.);
#3811=FACE_OUTER_BOUND('',#5977,.T.);
#3812=FACE_OUTER_BOUND('',#5978,.T.);
#3813=FACE_OUTER_BOUND('',#5979,.T.);
#3814=FACE_OUTER_BOUND('',#5980,.T.);
#3815=FACE_OUTER_BOUND('',#5981,.T.);
#3816=FACE_OUTER_BOUND('',#5982,.T.);
#3817=FACE_OUTER_BOUND('',#5983,.T.);
#3818=FACE_OUTER_BOUND('',#5984,.T.);
#3819=FACE_OUTER_BOUND('',#5985,.T.);
#3820=FACE_OUTER_BOUND('',#5986,.T.);
#3821=FACE_OUTER_BOUND('',#5987,.T.);
#3822=FACE_OUTER_BOUND('',#5988,.T.);
#3823=FACE_OUTER_BOUND('',#5989,.T.);
#3824=FACE_OUTER_BOUND('',#5990,.T.);
#3825=FACE_OUTER_BOUND('',#5991,.T.);
#3826=FACE_OUTER_BOUND('',#5992,.T.);
#3827=FACE_OUTER_BOUND('',#5993,.T.);
#3828=FACE_OUTER_BOUND('',#5994,.T.);
#3829=FACE_OUTER_BOUND('',#5995,.T.);
#3830=FACE_OUTER_BOUND('',#5996,.T.);
#3831=FACE_OUTER_BOUND('',#5997,.T.);
#3832=FACE_OUTER_BOUND('',#5998,.T.);
#3833=FACE_OUTER_BOUND('',#5999,.T.);
#3834=FACE_OUTER_BOUND('',#6000,.T.);
#3835=FACE_OUTER_BOUND('',#6004,.T.);
#3836=FACE_OUTER_BOUND('',#6005,.T.);
#3837=FACE_OUTER_BOUND('',#6006,.T.);
#3838=FACE_OUTER_BOUND('',#6007,.T.);
#3839=FACE_OUTER_BOUND('',#6008,.T.);
#3840=FACE_OUTER_BOUND('',#6009,.T.);
#3841=FACE_OUTER_BOUND('',#6010,.T.);
#3842=FACE_OUTER_BOUND('',#6011,.T.);
#3843=FACE_OUTER_BOUND('',#6012,.T.);
#3844=FACE_OUTER_BOUND('',#6013,.T.);
#3845=FACE_OUTER_BOUND('',#6014,.T.);
#3846=FACE_OUTER_BOUND('',#6015,.T.);
#3847=FACE_OUTER_BOUND('',#6016,.T.);
#3848=FACE_OUTER_BOUND('',#6017,.T.);
#3849=FACE_OUTER_BOUND('',#6018,.T.);
#3850=FACE_OUTER_BOUND('',#6019,.T.);
#3851=FACE_OUTER_BOUND('',#6020,.T.);
#3852=FACE_OUTER_BOUND('',#6021,.T.);
#3853=FACE_OUTER_BOUND('',#6022,.T.);
#3854=FACE_OUTER_BOUND('',#6023,.T.);
#3855=FACE_OUTER_BOUND('',#6024,.T.);
#3856=FACE_OUTER_BOUND('',#6025,.T.);
#3857=FACE_OUTER_BOUND('',#6026,.T.);
#3858=FACE_OUTER_BOUND('',#6027,.T.);
#3859=FACE_OUTER_BOUND('',#6028,.T.);
#3860=FACE_OUTER_BOUND('',#6029,.T.);
#3861=FACE_OUTER_BOUND('',#6030,.T.);
#3862=FACE_OUTER_BOUND('',#6031,.T.);
#3863=FACE_OUTER_BOUND('',#6032,.T.);
#3864=FACE_OUTER_BOUND('',#6033,.T.);
#3865=FACE_OUTER_BOUND('',#6034,.T.);
#3866=FACE_OUTER_BOUND('',#6035,.T.);
#3867=FACE_OUTER_BOUND('',#6036,.T.);
#3868=FACE_OUTER_BOUND('',#6037,.T.);
#3869=FACE_OUTER_BOUND('',#6039,.T.);
#3870=FACE_OUTER_BOUND('',#6040,.T.);
#3871=FACE_OUTER_BOUND('',#6041,.T.);
#3872=FACE_OUTER_BOUND('',#6042,.T.);
#3873=FACE_OUTER_BOUND('',#6043,.T.);
#3874=FACE_OUTER_BOUND('',#6044,.T.);
#3875=FACE_OUTER_BOUND('',#6045,.T.);
#3876=FACE_OUTER_BOUND('',#6046,.T.);
#3877=FACE_OUTER_BOUND('',#6047,.T.);
#3878=FACE_OUTER_BOUND('',#6048,.T.);
#3879=FACE_OUTER_BOUND('',#6049,.T.);
#3880=FACE_OUTER_BOUND('',#6050,.T.);
#3881=FACE_OUTER_BOUND('',#6052,.T.);
#3882=FACE_OUTER_BOUND('',#6053,.T.);
#3883=FACE_OUTER_BOUND('',#6054,.T.);
#3884=FACE_OUTER_BOUND('',#6055,.T.);
#3885=FACE_OUTER_BOUND('',#6056,.T.);
#3886=FACE_OUTER_BOUND('',#6057,.T.);
#3887=FACE_OUTER_BOUND('',#6058,.T.);
#3888=FACE_OUTER_BOUND('',#6059,.T.);
#3889=FACE_OUTER_BOUND('',#6060,.T.);
#3890=FACE_OUTER_BOUND('',#6061,.T.);
#3891=FACE_OUTER_BOUND('',#6062,.T.);
#3892=FACE_OUTER_BOUND('',#6063,.T.);
#3893=FACE_OUTER_BOUND('',#6064,.T.);
#3894=FACE_OUTER_BOUND('',#6065,.T.);
#3895=FACE_OUTER_BOUND('',#6066,.T.);
#3896=FACE_OUTER_BOUND('',#6067,.T.);
#3897=FACE_OUTER_BOUND('',#6068,.T.);
#3898=FACE_OUTER_BOUND('',#6069,.T.);
#3899=FACE_OUTER_BOUND('',#6071,.T.);
#3900=FACE_OUTER_BOUND('',#6073,.T.);
#3901=FACE_OUTER_BOUND('',#6075,.T.);
#3902=FACE_OUTER_BOUND('',#6076,.T.);
#3903=FACE_OUTER_BOUND('',#6077,.T.);
#3904=FACE_OUTER_BOUND('',#6078,.T.);
#3905=FACE_OUTER_BOUND('',#6079,.T.);
#3906=FACE_OUTER_BOUND('',#6080,.T.);
#3907=FACE_OUTER_BOUND('',#6081,.T.);
#3908=FACE_OUTER_BOUND('',#6082,.T.);
#3909=FACE_OUTER_BOUND('',#6083,.T.);
#3910=FACE_OUTER_BOUND('',#6084,.T.);
#3911=FACE_OUTER_BOUND('',#6085,.T.);
#3912=FACE_OUTER_BOUND('',#6086,.T.);
#3913=FACE_OUTER_BOUND('',#6087,.T.);
#3914=FACE_OUTER_BOUND('',#6088,.T.);
#3915=FACE_OUTER_BOUND('',#6089,.T.);
#3916=FACE_OUTER_BOUND('',#6090,.T.);
#3917=FACE_OUTER_BOUND('',#6091,.T.);
#3918=FACE_OUTER_BOUND('',#6092,.T.);
#3919=FACE_OUTER_BOUND('',#6093,.T.);
#3920=FACE_OUTER_BOUND('',#6094,.T.);
#3921=FACE_OUTER_BOUND('',#6095,.T.);
#3922=FACE_OUTER_BOUND('',#6096,.T.);
#3923=FACE_OUTER_BOUND('',#6097,.T.);
#3924=FACE_OUTER_BOUND('',#6098,.T.);
#3925=FACE_OUTER_BOUND('',#6099,.T.);
#3926=FACE_OUTER_BOUND('',#6100,.T.);
#3927=FACE_OUTER_BOUND('',#6101,.T.);
#3928=FACE_OUTER_BOUND('',#6102,.T.);
#3929=FACE_OUTER_BOUND('',#6103,.T.);
#3930=FACE_OUTER_BOUND('',#6104,.T.);
#3931=FACE_OUTER_BOUND('',#6105,.T.);
#3932=FACE_OUTER_BOUND('',#6106,.T.);
#3933=FACE_OUTER_BOUND('',#6107,.T.);
#3934=FACE_OUTER_BOUND('',#6108,.T.);
#3935=FACE_OUTER_BOUND('',#6109,.T.);
#3936=FACE_OUTER_BOUND('',#6110,.T.);
#3937=FACE_OUTER_BOUND('',#6111,.T.);
#3938=FACE_OUTER_BOUND('',#6112,.T.);
#3939=FACE_OUTER_BOUND('',#6113,.T.);
#3940=FACE_OUTER_BOUND('',#6117,.T.);
#3941=FACE_OUTER_BOUND('',#6118,.T.);
#3942=FACE_OUTER_BOUND('',#6119,.T.);
#3943=FACE_OUTER_BOUND('',#6120,.T.);
#3944=FACE_OUTER_BOUND('',#6122,.T.);
#3945=FACE_OUTER_BOUND('',#6123,.T.);
#3946=FACE_OUTER_BOUND('',#6124,.T.);
#3947=FACE_OUTER_BOUND('',#6125,.T.);
#3948=FACE_OUTER_BOUND('',#6126,.T.);
#3949=FACE_OUTER_BOUND('',#6127,.T.);
#3950=FACE_OUTER_BOUND('',#6128,.T.);
#3951=FACE_OUTER_BOUND('',#6129,.T.);
#3952=FACE_OUTER_BOUND('',#6130,.T.);
#3953=FACE_OUTER_BOUND('',#6131,.T.);
#3954=FACE_OUTER_BOUND('',#6132,.T.);
#3955=FACE_OUTER_BOUND('',#6133,.T.);
#3956=FACE_OUTER_BOUND('',#6134,.T.);
#3957=FACE_OUTER_BOUND('',#6135,.T.);
#3958=FACE_OUTER_BOUND('',#6136,.T.);
#3959=FACE_OUTER_BOUND('',#6137,.T.);
#3960=FACE_OUTER_BOUND('',#6138,.T.);
#3961=FACE_OUTER_BOUND('',#6139,.T.);
#3962=FACE_OUTER_BOUND('',#6140,.T.);
#3963=FACE_OUTER_BOUND('',#6141,.T.);
#3964=FACE_OUTER_BOUND('',#6142,.T.);
#3965=FACE_OUTER_BOUND('',#6143,.T.);
#3966=FACE_OUTER_BOUND('',#6144,.T.);
#3967=FACE_OUTER_BOUND('',#6145,.T.);
#3968=FACE_OUTER_BOUND('',#6146,.T.);
#3969=FACE_OUTER_BOUND('',#6147,.T.);
#3970=FACE_OUTER_BOUND('',#6148,.T.);
#3971=FACE_OUTER_BOUND('',#6149,.T.);
#3972=FACE_OUTER_BOUND('',#6150,.T.);
#3973=FACE_OUTER_BOUND('',#6151,.T.);
#3974=FACE_OUTER_BOUND('',#6152,.T.);
#3975=FACE_OUTER_BOUND('',#6153,.T.);
#3976=FACE_OUTER_BOUND('',#6154,.T.);
#3977=FACE_OUTER_BOUND('',#6155,.T.);
#3978=FACE_OUTER_BOUND('',#6156,.T.);
#3979=FACE_OUTER_BOUND('',#6157,.T.);
#3980=FACE_OUTER_BOUND('',#6158,.T.);
#3981=FACE_OUTER_BOUND('',#6159,.T.);
#3982=FACE_OUTER_BOUND('',#6160,.T.);
#3983=FACE_OUTER_BOUND('',#6161,.T.);
#3984=FACE_OUTER_BOUND('',#6162,.T.);
#3985=FACE_OUTER_BOUND('',#6163,.T.);
#3986=FACE_OUTER_BOUND('',#6164,.T.);
#3987=FACE_OUTER_BOUND('',#6165,.T.);
#3988=FACE_OUTER_BOUND('',#6166,.T.);
#3989=FACE_OUTER_BOUND('',#6167,.T.);
#3990=FACE_OUTER_BOUND('',#6168,.T.);
#3991=FACE_OUTER_BOUND('',#6169,.T.);
#3992=FACE_OUTER_BOUND('',#6171,.T.);
#3993=FACE_OUTER_BOUND('',#6173,.T.);
#3994=FACE_OUTER_BOUND('',#6174,.T.);
#3995=FACE_OUTER_BOUND('',#6175,.T.);
#3996=FACE_OUTER_BOUND('',#6176,.T.);
#3997=FACE_OUTER_BOUND('',#6177,.T.);
#3998=FACE_OUTER_BOUND('',#6178,.T.);
#3999=FACE_OUTER_BOUND('',#6179,.T.);
#4000=FACE_OUTER_BOUND('',#6180,.T.);
#4001=FACE_OUTER_BOUND('',#6181,.T.);
#4002=FACE_OUTER_BOUND('',#6182,.T.);
#4003=FACE_OUTER_BOUND('',#6183,.T.);
#4004=FACE_OUTER_BOUND('',#6184,.T.);
#4005=FACE_OUTER_BOUND('',#6185,.T.);
#4006=FACE_OUTER_BOUND('',#6186,.T.);
#4007=FACE_OUTER_BOUND('',#6187,.T.);
#4008=FACE_OUTER_BOUND('',#6189,.T.);
#4009=FACE_OUTER_BOUND('',#6190,.T.);
#4010=FACE_OUTER_BOUND('',#6191,.T.);
#4011=FACE_OUTER_BOUND('',#6192,.T.);
#4012=FACE_OUTER_BOUND('',#6193,.T.);
#4013=FACE_OUTER_BOUND('',#6194,.T.);
#4014=FACE_OUTER_BOUND('',#6195,.T.);
#4015=FACE_OUTER_BOUND('',#6196,.T.);
#4016=FACE_OUTER_BOUND('',#6197,.T.);
#4017=FACE_OUTER_BOUND('',#6198,.T.);
#4018=FACE_OUTER_BOUND('',#6199,.T.);
#4019=FACE_OUTER_BOUND('',#6200,.T.);
#4020=FACE_OUTER_BOUND('',#6201,.T.);
#4021=FACE_OUTER_BOUND('',#6202,.T.);
#4022=FACE_OUTER_BOUND('',#6203,.T.);
#4023=FACE_OUTER_BOUND('',#6204,.T.);
#4024=FACE_OUTER_BOUND('',#6205,.T.);
#4025=FACE_OUTER_BOUND('',#6206,.T.);
#4026=FACE_OUTER_BOUND('',#6207,.T.);
#4027=FACE_OUTER_BOUND('',#6208,.T.);
#4028=FACE_OUTER_BOUND('',#6209,.T.);
#4029=FACE_OUTER_BOUND('',#6210,.T.);
#4030=FACE_OUTER_BOUND('',#6211,.T.);
#4031=FACE_OUTER_BOUND('',#6212,.T.);
#4032=FACE_OUTER_BOUND('',#6213,.T.);
#4033=FACE_OUTER_BOUND('',#6214,.T.);
#4034=FACE_OUTER_BOUND('',#6215,.T.);
#4035=FACE_OUTER_BOUND('',#6216,.T.);
#4036=FACE_OUTER_BOUND('',#6217,.T.);
#4037=FACE_OUTER_BOUND('',#6218,.T.);
#4038=FACE_OUTER_BOUND('',#6219,.T.);
#4039=FACE_OUTER_BOUND('',#6220,.T.);
#4040=FACE_OUTER_BOUND('',#6221,.T.);
#4041=FACE_OUTER_BOUND('',#6222,.T.);
#4042=FACE_OUTER_BOUND('',#6223,.T.);
#4043=FACE_OUTER_BOUND('',#6224,.T.);
#4044=FACE_OUTER_BOUND('',#6225,.T.);
#4045=FACE_OUTER_BOUND('',#6226,.T.);
#4046=FACE_OUTER_BOUND('',#6227,.T.);
#4047=FACE_OUTER_BOUND('',#6228,.T.);
#4048=FACE_OUTER_BOUND('',#6229,.T.);
#4049=FACE_OUTER_BOUND('',#6230,.T.);
#4050=FACE_OUTER_BOUND('',#6231,.T.);
#4051=FACE_OUTER_BOUND('',#6232,.T.);
#4052=FACE_OUTER_BOUND('',#6233,.T.);
#4053=FACE_OUTER_BOUND('',#6234,.T.);
#4054=FACE_OUTER_BOUND('',#6235,.T.);
#4055=FACE_OUTER_BOUND('',#6236,.T.);
#4056=FACE_OUTER_BOUND('',#6237,.T.);
#4057=FACE_OUTER_BOUND('',#6238,.T.);
#4058=FACE_OUTER_BOUND('',#6239,.T.);
#4059=FACE_OUTER_BOUND('',#6240,.T.);
#4060=FACE_OUTER_BOUND('',#6241,.T.);
#4061=FACE_OUTER_BOUND('',#6242,.T.);
#4062=FACE_OUTER_BOUND('',#6243,.T.);
#4063=FACE_OUTER_BOUND('',#6244,.T.);
#4064=FACE_OUTER_BOUND('',#6245,.T.);
#4065=FACE_OUTER_BOUND('',#6246,.T.);
#4066=FACE_OUTER_BOUND('',#6247,.T.);
#4067=FACE_OUTER_BOUND('',#6248,.T.);
#4068=FACE_OUTER_BOUND('',#6249,.T.);
#4069=FACE_OUTER_BOUND('',#6250,.T.);
#4070=FACE_OUTER_BOUND('',#6251,.T.);
#4071=FACE_OUTER_BOUND('',#6252,.T.);
#4072=FACE_OUTER_BOUND('',#6253,.T.);
#4073=FACE_OUTER_BOUND('',#6254,.T.);
#4074=FACE_OUTER_BOUND('',#6255,.T.);
#4075=FACE_OUTER_BOUND('',#6256,.T.);
#4076=FACE_OUTER_BOUND('',#6257,.T.);
#4077=FACE_OUTER_BOUND('',#6258,.T.);
#4078=FACE_OUTER_BOUND('',#6259,.T.);
#4079=FACE_OUTER_BOUND('',#6260,.T.);
#4080=FACE_OUTER_BOUND('',#6261,.T.);
#4081=FACE_OUTER_BOUND('',#6262,.T.);
#4082=FACE_OUTER_BOUND('',#6263,.T.);
#4083=FACE_OUTER_BOUND('',#6264,.T.);
#4084=FACE_OUTER_BOUND('',#6265,.T.);
#4085=FACE_OUTER_BOUND('',#6266,.T.);
#4086=FACE_OUTER_BOUND('',#6267,.T.);
#4087=FACE_OUTER_BOUND('',#6268,.T.);
#4088=FACE_OUTER_BOUND('',#6269,.T.);
#4089=FACE_OUTER_BOUND('',#6270,.T.);
#4090=FACE_OUTER_BOUND('',#6271,.T.);
#4091=FACE_OUTER_BOUND('',#6272,.T.);
#4092=FACE_OUTER_BOUND('',#6273,.T.);
#4093=FACE_OUTER_BOUND('',#6274,.T.);
#4094=FACE_OUTER_BOUND('',#6275,.T.);
#4095=FACE_OUTER_BOUND('',#6276,.T.);
#4096=FACE_OUTER_BOUND('',#6277,.T.);
#4097=FACE_OUTER_BOUND('',#6278,.T.);
#4098=FACE_OUTER_BOUND('',#6279,.T.);
#4099=FACE_OUTER_BOUND('',#6280,.T.);
#4100=FACE_OUTER_BOUND('',#6281,.T.);
#4101=FACE_OUTER_BOUND('',#6282,.T.);
#4102=FACE_OUTER_BOUND('',#6283,.T.);
#4103=FACE_OUTER_BOUND('',#6284,.T.);
#4104=FACE_OUTER_BOUND('',#6285,.T.);
#4105=FACE_OUTER_BOUND('',#6286,.T.);
#4106=FACE_OUTER_BOUND('',#6287,.T.);
#4107=FACE_OUTER_BOUND('',#6288,.T.);
#4108=FACE_OUTER_BOUND('',#6289,.T.);
#4109=FACE_OUTER_BOUND('',#6290,.T.);
#4110=FACE_OUTER_BOUND('',#6291,.T.);
#4111=FACE_OUTER_BOUND('',#6292,.T.);
#4112=FACE_OUTER_BOUND('',#6293,.T.);
#4113=FACE_OUTER_BOUND('',#6294,.T.);
#4114=FACE_OUTER_BOUND('',#6295,.T.);
#4115=FACE_OUTER_BOUND('',#6296,.T.);
#4116=FACE_OUTER_BOUND('',#6297,.T.);
#4117=FACE_OUTER_BOUND('',#6298,.T.);
#4118=FACE_OUTER_BOUND('',#6299,.T.);
#4119=FACE_OUTER_BOUND('',#6300,.T.);
#4120=FACE_OUTER_BOUND('',#6301,.T.);
#4121=FACE_OUTER_BOUND('',#6302,.T.);
#4122=FACE_OUTER_BOUND('',#6303,.T.);
#4123=FACE_OUTER_BOUND('',#6304,.T.);
#4124=FACE_OUTER_BOUND('',#6305,.T.);
#4125=FACE_OUTER_BOUND('',#6306,.T.);
#4126=FACE_OUTER_BOUND('',#6307,.T.);
#4127=FACE_OUTER_BOUND('',#6308,.T.);
#4128=FACE_OUTER_BOUND('',#6309,.T.);
#4129=FACE_OUTER_BOUND('',#6310,.T.);
#4130=FACE_OUTER_BOUND('',#6311,.T.);
#4131=FACE_OUTER_BOUND('',#6312,.T.);
#4132=FACE_OUTER_BOUND('',#6313,.T.);
#4133=FACE_OUTER_BOUND('',#6314,.T.);
#4134=FACE_OUTER_BOUND('',#6315,.T.);
#4135=FACE_OUTER_BOUND('',#6316,.T.);
#4136=FACE_OUTER_BOUND('',#6317,.T.);
#4137=FACE_OUTER_BOUND('',#6318,.T.);
#4138=FACE_OUTER_BOUND('',#6319,.T.);
#4139=FACE_OUTER_BOUND('',#6320,.T.);
#4140=FACE_OUTER_BOUND('',#6321,.T.);
#4141=FACE_OUTER_BOUND('',#6323,.T.);
#4142=FACE_OUTER_BOUND('',#6324,.T.);
#4143=FACE_OUTER_BOUND('',#6325,.T.);
#4144=FACE_OUTER_BOUND('',#6326,.T.);
#4145=FACE_OUTER_BOUND('',#6327,.T.);
#4146=FACE_OUTER_BOUND('',#6328,.T.);
#4147=FACE_OUTER_BOUND('',#6329,.T.);
#4148=FACE_OUTER_BOUND('',#6331,.T.);
#4149=FACE_OUTER_BOUND('',#6332,.T.);
#4150=FACE_OUTER_BOUND('',#6333,.T.);
#4151=FACE_OUTER_BOUND('',#6334,.T.);
#4152=FACE_OUTER_BOUND('',#6335,.T.);
#4153=FACE_OUTER_BOUND('',#6336,.T.);
#4154=FACE_OUTER_BOUND('',#6337,.T.);
#4155=FACE_OUTER_BOUND('',#6338,.T.);
#4156=FACE_OUTER_BOUND('',#6339,.T.);
#4157=FACE_OUTER_BOUND('',#6340,.T.);
#4158=FACE_OUTER_BOUND('',#6341,.T.);
#4159=FACE_OUTER_BOUND('',#6342,.T.);
#4160=FACE_OUTER_BOUND('',#6343,.T.);
#4161=FACE_OUTER_BOUND('',#6344,.T.);
#4162=FACE_OUTER_BOUND('',#6345,.T.);
#4163=FACE_OUTER_BOUND('',#6346,.T.);
#4164=FACE_OUTER_BOUND('',#6347,.T.);
#4165=FACE_OUTER_BOUND('',#6348,.T.);
#4166=FACE_OUTER_BOUND('',#6349,.T.);
#4167=FACE_OUTER_BOUND('',#6350,.T.);
#4168=FACE_OUTER_BOUND('',#6351,.T.);
#4169=FACE_OUTER_BOUND('',#6352,.T.);
#4170=FACE_OUTER_BOUND('',#6353,.T.);
#4171=FACE_OUTER_BOUND('',#6354,.T.);
#4172=FACE_OUTER_BOUND('',#6355,.T.);
#4173=FACE_OUTER_BOUND('',#6356,.T.);
#4174=FACE_OUTER_BOUND('',#6357,.T.);
#4175=FACE_OUTER_BOUND('',#6358,.T.);
#4176=FACE_OUTER_BOUND('',#6359,.T.);
#4177=FACE_OUTER_BOUND('',#6360,.T.);
#4178=FACE_OUTER_BOUND('',#6361,.T.);
#4179=FACE_OUTER_BOUND('',#6362,.T.);
#4180=FACE_OUTER_BOUND('',#6363,.T.);
#4181=FACE_OUTER_BOUND('',#6364,.T.);
#4182=FACE_OUTER_BOUND('',#6365,.T.);
#4183=FACE_OUTER_BOUND('',#6366,.T.);
#4184=FACE_OUTER_BOUND('',#6367,.T.);
#4185=FACE_OUTER_BOUND('',#6368,.T.);
#4186=FACE_OUTER_BOUND('',#6369,.T.);
#4187=FACE_OUTER_BOUND('',#6370,.T.);
#4188=FACE_OUTER_BOUND('',#6371,.T.);
#4189=FACE_OUTER_BOUND('',#6372,.T.);
#4190=FACE_OUTER_BOUND('',#6373,.T.);
#4191=FACE_OUTER_BOUND('',#6374,.T.);
#4192=FACE_OUTER_BOUND('',#6376,.T.);
#4193=FACE_OUTER_BOUND('',#6377,.T.);
#4194=FACE_OUTER_BOUND('',#6378,.T.);
#4195=FACE_OUTER_BOUND('',#6379,.T.);
#4196=FACE_OUTER_BOUND('',#6380,.T.);
#4197=FACE_OUTER_BOUND('',#6381,.T.);
#4198=FACE_OUTER_BOUND('',#6382,.T.);
#4199=FACE_OUTER_BOUND('',#6383,.T.);
#4200=FACE_OUTER_BOUND('',#6384,.T.);
#4201=FACE_OUTER_BOUND('',#6385,.T.);
#4202=FACE_OUTER_BOUND('',#6386,.T.);
#4203=FACE_OUTER_BOUND('',#6387,.T.);
#4204=FACE_OUTER_BOUND('',#6388,.T.);
#4205=FACE_OUTER_BOUND('',#6389,.T.);
#4206=FACE_OUTER_BOUND('',#6390,.T.);
#4207=FACE_OUTER_BOUND('',#6391,.T.);
#4208=FACE_OUTER_BOUND('',#6392,.T.);
#4209=FACE_OUTER_BOUND('',#6393,.T.);
#4210=FACE_OUTER_BOUND('',#6394,.T.);
#4211=FACE_OUTER_BOUND('',#6395,.T.);
#4212=FACE_OUTER_BOUND('',#6396,.T.);
#4213=FACE_OUTER_BOUND('',#6397,.T.);
#4214=FACE_OUTER_BOUND('',#6398,.T.);
#4215=FACE_OUTER_BOUND('',#6399,.T.);
#4216=FACE_OUTER_BOUND('',#6400,.T.);
#4217=FACE_OUTER_BOUND('',#6401,.T.);
#4218=FACE_OUTER_BOUND('',#6402,.T.);
#4219=FACE_OUTER_BOUND('',#6403,.T.);
#4220=FACE_OUTER_BOUND('',#6404,.T.);
#4221=FACE_OUTER_BOUND('',#6405,.T.);
#4222=FACE_OUTER_BOUND('',#6406,.T.);
#4223=FACE_OUTER_BOUND('',#6407,.T.);
#4224=FACE_OUTER_BOUND('',#6408,.T.);
#4225=FACE_OUTER_BOUND('',#6409,.T.);
#4226=FACE_OUTER_BOUND('',#6410,.T.);
#4227=FACE_OUTER_BOUND('',#6411,.T.);
#4228=FACE_OUTER_BOUND('',#6412,.T.);
#4229=FACE_OUTER_BOUND('',#6413,.T.);
#4230=FACE_OUTER_BOUND('',#6414,.T.);
#4231=FACE_OUTER_BOUND('',#6415,.T.);
#4232=FACE_OUTER_BOUND('',#6416,.T.);
#4233=FACE_OUTER_BOUND('',#6417,.T.);
#4234=FACE_OUTER_BOUND('',#6418,.T.);
#4235=FACE_OUTER_BOUND('',#6419,.T.);
#4236=FACE_OUTER_BOUND('',#6420,.T.);
#4237=FACE_OUTER_BOUND('',#6421,.T.);
#4238=FACE_OUTER_BOUND('',#6422,.T.);
#4239=FACE_OUTER_BOUND('',#6423,.T.);
#4240=FACE_OUTER_BOUND('',#6424,.T.);
#4241=FACE_OUTER_BOUND('',#6425,.T.);
#4242=FACE_OUTER_BOUND('',#6426,.T.);
#4243=FACE_OUTER_BOUND('',#6427,.T.);
#4244=FACE_OUTER_BOUND('',#6428,.T.);
#4245=FACE_OUTER_BOUND('',#6429,.T.);
#4246=FACE_OUTER_BOUND('',#6430,.T.);
#4247=FACE_OUTER_BOUND('',#6431,.T.);
#4248=FACE_OUTER_BOUND('',#6432,.T.);
#4249=FACE_OUTER_BOUND('',#6433,.T.);
#4250=FACE_OUTER_BOUND('',#6434,.T.);
#4251=FACE_OUTER_BOUND('',#6435,.T.);
#4252=FACE_OUTER_BOUND('',#6436,.T.);
#4253=FACE_OUTER_BOUND('',#6437,.T.);
#4254=FACE_OUTER_BOUND('',#6438,.T.);
#4255=FACE_OUTER_BOUND('',#6439,.T.);
#4256=FACE_OUTER_BOUND('',#6440,.T.);
#4257=FACE_OUTER_BOUND('',#6441,.T.);
#4258=FACE_OUTER_BOUND('',#6442,.T.);
#4259=FACE_OUTER_BOUND('',#6443,.T.);
#4260=FACE_OUTER_BOUND('',#6444,.T.);
#4261=FACE_OUTER_BOUND('',#6445,.T.);
#4262=FACE_OUTER_BOUND('',#6446,.T.);
#4263=FACE_OUTER_BOUND('',#6447,.T.);
#4264=FACE_OUTER_BOUND('',#6448,.T.);
#4265=FACE_OUTER_BOUND('',#6449,.T.);
#4266=FACE_OUTER_BOUND('',#6450,.T.);
#4267=FACE_OUTER_BOUND('',#6451,.T.);
#4268=FACE_OUTER_BOUND('',#6452,.T.);
#4269=FACE_OUTER_BOUND('',#6453,.T.);
#4270=FACE_OUTER_BOUND('',#6454,.T.);
#4271=FACE_OUTER_BOUND('',#6455,.T.);
#4272=FACE_OUTER_BOUND('',#6456,.T.);
#4273=FACE_OUTER_BOUND('',#6457,.T.);
#4274=FACE_OUTER_BOUND('',#6458,.T.);
#4275=FACE_OUTER_BOUND('',#6459,.T.);
#4276=FACE_OUTER_BOUND('',#6460,.T.);
#4277=FACE_OUTER_BOUND('',#6461,.T.);
#4278=FACE_OUTER_BOUND('',#6462,.T.);
#4279=FACE_OUTER_BOUND('',#6463,.T.);
#4280=FACE_OUTER_BOUND('',#6464,.T.);
#4281=FACE_OUTER_BOUND('',#6465,.T.);
#4282=FACE_OUTER_BOUND('',#6466,.T.);
#4283=FACE_OUTER_BOUND('',#6467,.T.);
#4284=FACE_OUTER_BOUND('',#6468,.T.);
#4285=FACE_OUTER_BOUND('',#6469,.T.);
#4286=FACE_OUTER_BOUND('',#6470,.T.);
#4287=FACE_OUTER_BOUND('',#6471,.T.);
#4288=FACE_OUTER_BOUND('',#6472,.T.);
#4289=FACE_OUTER_BOUND('',#6473,.T.);
#4290=FACE_OUTER_BOUND('',#6474,.T.);
#4291=FACE_OUTER_BOUND('',#6475,.T.);
#4292=FACE_OUTER_BOUND('',#6476,.T.);
#4293=FACE_OUTER_BOUND('',#6477,.T.);
#4294=FACE_OUTER_BOUND('',#6478,.T.);
#4295=FACE_OUTER_BOUND('',#6479,.T.);
#4296=FACE_OUTER_BOUND('',#6480,.T.);
#4297=FACE_OUTER_BOUND('',#6482,.T.);
#4298=FACE_OUTER_BOUND('',#6483,.T.);
#4299=FACE_OUTER_BOUND('',#6484,.T.);
#4300=FACE_OUTER_BOUND('',#6485,.T.);
#4301=FACE_OUTER_BOUND('',#6486,.T.);
#4302=FACE_OUTER_BOUND('',#6487,.T.);
#4303=FACE_OUTER_BOUND('',#6488,.T.);
#4304=FACE_OUTER_BOUND('',#6489,.T.);
#4305=FACE_OUTER_BOUND('',#6490,.T.);
#4306=FACE_OUTER_BOUND('',#6491,.T.);
#4307=FACE_OUTER_BOUND('',#6492,.T.);
#4308=FACE_OUTER_BOUND('',#6493,.T.);
#4309=FACE_OUTER_BOUND('',#6494,.T.);
#4310=FACE_OUTER_BOUND('',#6495,.T.);
#4311=FACE_OUTER_BOUND('',#6496,.T.);
#4312=FACE_OUTER_BOUND('',#6497,.T.);
#4313=FACE_OUTER_BOUND('',#6498,.T.);
#4314=FACE_OUTER_BOUND('',#6499,.T.);
#4315=FACE_OUTER_BOUND('',#6500,.T.);
#4316=FACE_OUTER_BOUND('',#6501,.T.);
#4317=FACE_OUTER_BOUND('',#6502,.T.);
#4318=FACE_OUTER_BOUND('',#6503,.T.);
#4319=FACE_OUTER_BOUND('',#6504,.T.);
#4320=FACE_OUTER_BOUND('',#6505,.T.);
#4321=FACE_OUTER_BOUND('',#6506,.T.);
#4322=FACE_OUTER_BOUND('',#6507,.T.);
#4323=FACE_OUTER_BOUND('',#6508,.T.);
#4324=FACE_OUTER_BOUND('',#6509,.T.);
#4325=FACE_OUTER_BOUND('',#6510,.T.);
#4326=FACE_OUTER_BOUND('',#6511,.T.);
#4327=FACE_OUTER_BOUND('',#6512,.T.);
#4328=FACE_OUTER_BOUND('',#6513,.T.);
#4329=FACE_OUTER_BOUND('',#6514,.T.);
#4330=FACE_OUTER_BOUND('',#6515,.T.);
#4331=FACE_OUTER_BOUND('',#6517,.T.);
#4332=FACE_OUTER_BOUND('',#6518,.T.);
#4333=FACE_OUTER_BOUND('',#6519,.T.);
#4334=FACE_OUTER_BOUND('',#6520,.T.);
#4335=FACE_OUTER_BOUND('',#6521,.T.);
#4336=FACE_OUTER_BOUND('',#6522,.T.);
#4337=FACE_OUTER_BOUND('',#6523,.T.);
#4338=FACE_OUTER_BOUND('',#6524,.T.);
#4339=FACE_OUTER_BOUND('',#6525,.T.);
#4340=FACE_OUTER_BOUND('',#6526,.T.);
#4341=FACE_OUTER_BOUND('',#6527,.T.);
#4342=FACE_OUTER_BOUND('',#6528,.T.);
#4343=FACE_OUTER_BOUND('',#6529,.T.);
#4344=FACE_OUTER_BOUND('',#6530,.T.);
#4345=FACE_OUTER_BOUND('',#6531,.T.);
#4346=FACE_OUTER_BOUND('',#6532,.T.);
#4347=FACE_OUTER_BOUND('',#6533,.T.);
#4348=FACE_OUTER_BOUND('',#6534,.T.);
#4349=FACE_OUTER_BOUND('',#6535,.T.);
#4350=FACE_OUTER_BOUND('',#6536,.T.);
#4351=FACE_OUTER_BOUND('',#6537,.T.);
#4352=FACE_OUTER_BOUND('',#6538,.T.);
#4353=FACE_OUTER_BOUND('',#6539,.T.);
#4354=FACE_OUTER_BOUND('',#6540,.T.);
#4355=FACE_OUTER_BOUND('',#6541,.T.);
#4356=FACE_OUTER_BOUND('',#6542,.T.);
#4357=FACE_OUTER_BOUND('',#6543,.T.);
#4358=FACE_OUTER_BOUND('',#6544,.T.);
#4359=FACE_OUTER_BOUND('',#6545,.T.);
#4360=FACE_OUTER_BOUND('',#6546,.T.);
#4361=FACE_OUTER_BOUND('',#6547,.T.);
#4362=FACE_OUTER_BOUND('',#6548,.T.);
#4363=FACE_OUTER_BOUND('',#6549,.T.);
#4364=FACE_OUTER_BOUND('',#6550,.T.);
#4365=FACE_OUTER_BOUND('',#6552,.T.);
#4366=FACE_OUTER_BOUND('',#6553,.T.);
#4367=FACE_OUTER_BOUND('',#6554,.T.);
#4368=FACE_OUTER_BOUND('',#6555,.T.);
#4369=FACE_OUTER_BOUND('',#6556,.T.);
#4370=FACE_OUTER_BOUND('',#6557,.T.);
#4371=FACE_OUTER_BOUND('',#6558,.T.);
#4372=FACE_OUTER_BOUND('',#6559,.T.);
#4373=FACE_OUTER_BOUND('',#6560,.T.);
#4374=FACE_OUTER_BOUND('',#6561,.T.);
#4375=FACE_OUTER_BOUND('',#6562,.T.);
#4376=FACE_OUTER_BOUND('',#6563,.T.);
#4377=FACE_OUTER_BOUND('',#6564,.T.);
#4378=FACE_OUTER_BOUND('',#6565,.T.);
#4379=FACE_OUTER_BOUND('',#6566,.T.);
#4380=FACE_OUTER_BOUND('',#6567,.T.);
#4381=FACE_OUTER_BOUND('',#6568,.T.);
#4382=FACE_OUTER_BOUND('',#6569,.T.);
#4383=FACE_OUTER_BOUND('',#6570,.T.);
#4384=FACE_OUTER_BOUND('',#6571,.T.);
#4385=FACE_OUTER_BOUND('',#6572,.T.);
#4386=FACE_OUTER_BOUND('',#6573,.T.);
#4387=FACE_OUTER_BOUND('',#6574,.T.);
#4388=FACE_OUTER_BOUND('',#6575,.T.);
#4389=FACE_OUTER_BOUND('',#6576,.T.);
#4390=FACE_OUTER_BOUND('',#6577,.T.);
#4391=FACE_OUTER_BOUND('',#6578,.T.);
#4392=FACE_OUTER_BOUND('',#6579,.T.);
#4393=FACE_OUTER_BOUND('',#6580,.T.);
#4394=FACE_OUTER_BOUND('',#6581,.T.);
#4395=FACE_OUTER_BOUND('',#6582,.T.);
#4396=FACE_OUTER_BOUND('',#6583,.T.);
#4397=FACE_OUTER_BOUND('',#6584,.T.);
#4398=FACE_OUTER_BOUND('',#6585,.T.);
#4399=FACE_OUTER_BOUND('',#6586,.T.);
#4400=FACE_OUTER_BOUND('',#6587,.T.);
#4401=FACE_OUTER_BOUND('',#6588,.T.);
#4402=FACE_OUTER_BOUND('',#6589,.T.);
#4403=FACE_OUTER_BOUND('',#6590,.T.);
#4404=FACE_OUTER_BOUND('',#6591,.T.);
#4405=FACE_OUTER_BOUND('',#6592,.T.);
#4406=FACE_OUTER_BOUND('',#6593,.T.);
#4407=FACE_OUTER_BOUND('',#6594,.T.);
#4408=FACE_OUTER_BOUND('',#6595,.T.);
#4409=FACE_OUTER_BOUND('',#6596,.T.);
#4410=FACE_OUTER_BOUND('',#6597,.T.);
#4411=FACE_OUTER_BOUND('',#6598,.T.);
#4412=FACE_OUTER_BOUND('',#6599,.T.);
#4413=FACE_OUTER_BOUND('',#6600,.T.);
#4414=FACE_OUTER_BOUND('',#6601,.T.);
#4415=FACE_OUTER_BOUND('',#6602,.T.);
#4416=FACE_OUTER_BOUND('',#6603,.T.);
#4417=FACE_OUTER_BOUND('',#6604,.T.);
#4418=FACE_OUTER_BOUND('',#6605,.T.);
#4419=FACE_OUTER_BOUND('',#6606,.T.);
#4420=FACE_OUTER_BOUND('',#6607,.T.);
#4421=FACE_OUTER_BOUND('',#6608,.T.);
#4422=FACE_OUTER_BOUND('',#6610,.T.);
#4423=FACE_OUTER_BOUND('',#6611,.T.);
#4424=FACE_OUTER_BOUND('',#6612,.T.);
#4425=FACE_OUTER_BOUND('',#6613,.T.);
#4426=FACE_OUTER_BOUND('',#6614,.T.);
#4427=FACE_OUTER_BOUND('',#6615,.T.);
#4428=FACE_OUTER_BOUND('',#6616,.T.);
#4429=FACE_OUTER_BOUND('',#6617,.T.);
#4430=FACE_OUTER_BOUND('',#6618,.T.);
#4431=FACE_OUTER_BOUND('',#6621,.T.);
#4432=FACE_OUTER_BOUND('',#6624,.T.);
#4433=FACE_OUTER_BOUND('',#6625,.T.);
#4434=FACE_OUTER_BOUND('',#6626,.T.);
#4435=FACE_OUTER_BOUND('',#6627,.T.);
#4436=FACE_OUTER_BOUND('',#6628,.T.);
#4437=FACE_OUTER_BOUND('',#6629,.T.);
#4438=FACE_OUTER_BOUND('',#6630,.T.);
#4439=FACE_OUTER_BOUND('',#6631,.T.);
#4440=FACE_OUTER_BOUND('',#6632,.T.);
#4441=FACE_OUTER_BOUND('',#6633,.T.);
#4442=FACE_OUTER_BOUND('',#6634,.T.);
#4443=FACE_OUTER_BOUND('',#6635,.T.);
#4444=FACE_OUTER_BOUND('',#6636,.T.);
#4445=FACE_OUTER_BOUND('',#6637,.T.);
#4446=FACE_OUTER_BOUND('',#6638,.T.);
#4447=FACE_OUTER_BOUND('',#6639,.T.);
#4448=FACE_OUTER_BOUND('',#6640,.T.);
#4449=FACE_OUTER_BOUND('',#6641,.T.);
#4450=FACE_OUTER_BOUND('',#6642,.T.);
#4451=FACE_OUTER_BOUND('',#6643,.T.);
#4452=FACE_OUTER_BOUND('',#6644,.T.);
#4453=FACE_OUTER_BOUND('',#6645,.T.);
#4454=FACE_OUTER_BOUND('',#6646,.T.);
#4455=FACE_OUTER_BOUND('',#6647,.T.);
#4456=FACE_OUTER_BOUND('',#6648,.T.);
#4457=FACE_OUTER_BOUND('',#6649,.T.);
#4458=FACE_OUTER_BOUND('',#6650,.T.);
#4459=FACE_OUTER_BOUND('',#6651,.T.);
#4460=FACE_OUTER_BOUND('',#6652,.T.);
#4461=FACE_OUTER_BOUND('',#6653,.T.);
#4462=FACE_OUTER_BOUND('',#6654,.T.);
#4463=FACE_OUTER_BOUND('',#6655,.T.);
#4464=FACE_OUTER_BOUND('',#6656,.T.);
#4465=FACE_OUTER_BOUND('',#6657,.T.);
#4466=FACE_OUTER_BOUND('',#6658,.T.);
#4467=FACE_OUTER_BOUND('',#6659,.T.);
#4468=FACE_OUTER_BOUND('',#6660,.T.);
#4469=FACE_OUTER_BOUND('',#6661,.T.);
#4470=FACE_OUTER_BOUND('',#6663,.T.);
#4471=FACE_OUTER_BOUND('',#6664,.T.);
#4472=FACE_OUTER_BOUND('',#6665,.T.);
#4473=FACE_OUTER_BOUND('',#6666,.T.);
#4474=FACE_OUTER_BOUND('',#6667,.T.);
#4475=FACE_OUTER_BOUND('',#6668,.T.);
#4476=FACE_OUTER_BOUND('',#6669,.T.);
#4477=FACE_OUTER_BOUND('',#6670,.T.);
#4478=FACE_OUTER_BOUND('',#6671,.T.);
#4479=FACE_OUTER_BOUND('',#6672,.T.);
#4480=FACE_OUTER_BOUND('',#6673,.T.);
#4481=FACE_OUTER_BOUND('',#6674,.T.);
#4482=FACE_OUTER_BOUND('',#6675,.T.);
#4483=FACE_OUTER_BOUND('',#6676,.T.);
#4484=FACE_OUTER_BOUND('',#6677,.T.);
#4485=FACE_OUTER_BOUND('',#6678,.T.);
#4486=FACE_OUTER_BOUND('',#6679,.T.);
#4487=FACE_OUTER_BOUND('',#6680,.T.);
#4488=FACE_OUTER_BOUND('',#6681,.T.);
#4489=FACE_OUTER_BOUND('',#6682,.T.);
#4490=FACE_OUTER_BOUND('',#6683,.T.);
#4491=FACE_OUTER_BOUND('',#6684,.T.);
#4492=FACE_OUTER_BOUND('',#6685,.T.);
#4493=FACE_OUTER_BOUND('',#6686,.T.);
#4494=FACE_OUTER_BOUND('',#6687,.T.);
#4495=FACE_OUTER_BOUND('',#6688,.T.);
#4496=FACE_OUTER_BOUND('',#6689,.T.);
#4497=FACE_OUTER_BOUND('',#6690,.T.);
#4498=FACE_OUTER_BOUND('',#6691,.T.);
#4499=FACE_OUTER_BOUND('',#6692,.T.);
#4500=FACE_OUTER_BOUND('',#6693,.T.);
#4501=FACE_OUTER_BOUND('',#6694,.T.);
#4502=FACE_OUTER_BOUND('',#6695,.T.);
#4503=FACE_OUTER_BOUND('',#6696,.T.);
#4504=FACE_OUTER_BOUND('',#6697,.T.);
#4505=FACE_OUTER_BOUND('',#6698,.T.);
#4506=FACE_OUTER_BOUND('',#6699,.T.);
#4507=FACE_OUTER_BOUND('',#6700,.T.);
#4508=FACE_OUTER_BOUND('',#6701,.T.);
#4509=FACE_OUTER_BOUND('',#6702,.T.);
#4510=FACE_OUTER_BOUND('',#6703,.T.);
#4511=FACE_OUTER_BOUND('',#6704,.T.);
#4512=FACE_OUTER_BOUND('',#6705,.T.);
#4513=FACE_OUTER_BOUND('',#6706,.T.);
#4514=FACE_OUTER_BOUND('',#6707,.T.);
#4515=FACE_OUTER_BOUND('',#6708,.T.);
#4516=FACE_OUTER_BOUND('',#6709,.T.);
#4517=FACE_OUTER_BOUND('',#6710,.T.);
#4518=FACE_OUTER_BOUND('',#6711,.T.);
#4519=FACE_OUTER_BOUND('',#6712,.T.);
#4520=FACE_OUTER_BOUND('',#6713,.T.);
#4521=FACE_OUTER_BOUND('',#6714,.T.);
#4522=FACE_OUTER_BOUND('',#6716,.T.);
#4523=FACE_OUTER_BOUND('',#6717,.T.);
#4524=FACE_OUTER_BOUND('',#6719,.T.);
#4525=FACE_OUTER_BOUND('',#6720,.T.);
#4526=FACE_OUTER_BOUND('',#6721,.T.);
#4527=FACE_OUTER_BOUND('',#6722,.T.);
#4528=FACE_OUTER_BOUND('',#6723,.T.);
#4529=FACE_OUTER_BOUND('',#6724,.T.);
#4530=FACE_OUTER_BOUND('',#6725,.T.);
#4531=FACE_OUTER_BOUND('',#6726,.T.);
#4532=FACE_OUTER_BOUND('',#6727,.T.);
#4533=FACE_OUTER_BOUND('',#6728,.T.);
#4534=FACE_OUTER_BOUND('',#6729,.T.);
#4535=FACE_OUTER_BOUND('',#6730,.T.);
#4536=FACE_OUTER_BOUND('',#6731,.T.);
#4537=FACE_OUTER_BOUND('',#6732,.T.);
#4538=FACE_OUTER_BOUND('',#6733,.T.);
#4539=FACE_OUTER_BOUND('',#6734,.T.);
#4540=FACE_OUTER_BOUND('',#6735,.T.);
#4541=FACE_OUTER_BOUND('',#6736,.T.);
#4542=FACE_OUTER_BOUND('',#6737,.T.);
#4543=FACE_OUTER_BOUND('',#6738,.T.);
#4544=FACE_OUTER_BOUND('',#6739,.T.);
#4545=FACE_OUTER_BOUND('',#6740,.T.);
#4546=FACE_OUTER_BOUND('',#6741,.T.);
#4547=FACE_OUTER_BOUND('',#6742,.T.);
#4548=FACE_OUTER_BOUND('',#6743,.T.);
#4549=FACE_OUTER_BOUND('',#6744,.T.);
#4550=FACE_OUTER_BOUND('',#6745,.T.);
#4551=FACE_OUTER_BOUND('',#6746,.T.);
#4552=FACE_OUTER_BOUND('',#6747,.T.);
#4553=FACE_OUTER_BOUND('',#6748,.T.);
#4554=FACE_OUTER_BOUND('',#6749,.T.);
#4555=FACE_OUTER_BOUND('',#6750,.T.);
#4556=FACE_OUTER_BOUND('',#6751,.T.);
#4557=FACE_OUTER_BOUND('',#6752,.T.);
#4558=FACE_OUTER_BOUND('',#6753,.T.);
#4559=FACE_OUTER_BOUND('',#6754,.T.);
#4560=FACE_OUTER_BOUND('',#6755,.T.);
#4561=FACE_OUTER_BOUND('',#6756,.T.);
#4562=FACE_OUTER_BOUND('',#6757,.T.);
#4563=FACE_OUTER_BOUND('',#6758,.T.);
#4564=FACE_OUTER_BOUND('',#6759,.T.);
#4565=FACE_OUTER_BOUND('',#6760,.T.);
#4566=FACE_OUTER_BOUND('',#6761,.T.);
#4567=FACE_OUTER_BOUND('',#6762,.T.);
#4568=FACE_OUTER_BOUND('',#6763,.T.);
#4569=FACE_OUTER_BOUND('',#6764,.T.);
#4570=FACE_OUTER_BOUND('',#6765,.T.);
#4571=FACE_OUTER_BOUND('',#6766,.T.);
#4572=FACE_OUTER_BOUND('',#6767,.T.);
#4573=FACE_OUTER_BOUND('',#6768,.T.);
#4574=FACE_OUTER_BOUND('',#6769,.T.);
#4575=FACE_OUTER_BOUND('',#6770,.T.);
#4576=FACE_OUTER_BOUND('',#6771,.T.);
#4577=FACE_OUTER_BOUND('',#6772,.T.);
#4578=FACE_OUTER_BOUND('',#6773,.T.);
#4579=FACE_OUTER_BOUND('',#6774,.T.);
#4580=FACE_OUTER_BOUND('',#6775,.T.);
#4581=FACE_OUTER_BOUND('',#6776,.T.);
#4582=FACE_OUTER_BOUND('',#6777,.T.);
#4583=FACE_OUTER_BOUND('',#6778,.T.);
#4584=FACE_OUTER_BOUND('',#6779,.T.);
#4585=FACE_OUTER_BOUND('',#6780,.T.);
#4586=FACE_OUTER_BOUND('',#6781,.T.);
#4587=FACE_OUTER_BOUND('',#6782,.T.);
#4588=FACE_OUTER_BOUND('',#6783,.T.);
#4589=FACE_OUTER_BOUND('',#6784,.T.);
#4590=FACE_OUTER_BOUND('',#6785,.T.);
#4591=FACE_OUTER_BOUND('',#6786,.T.);
#4592=FACE_OUTER_BOUND('',#6787,.T.);
#4593=FACE_OUTER_BOUND('',#6788,.T.);
#4594=FACE_OUTER_BOUND('',#6789,.T.);
#4595=FACE_OUTER_BOUND('',#6790,.T.);
#4596=FACE_OUTER_BOUND('',#6791,.T.);
#4597=FACE_OUTER_BOUND('',#6792,.T.);
#4598=FACE_OUTER_BOUND('',#6793,.T.);
#4599=FACE_OUTER_BOUND('',#6794,.T.);
#4600=FACE_OUTER_BOUND('',#6795,.T.);
#4601=FACE_OUTER_BOUND('',#6796,.T.);
#4602=FACE_OUTER_BOUND('',#6797,.T.);
#4603=FACE_OUTER_BOUND('',#6798,.T.);
#4604=FACE_OUTER_BOUND('',#6799,.T.);
#4605=FACE_OUTER_BOUND('',#6800,.T.);
#4606=FACE_OUTER_BOUND('',#6801,.T.);
#4607=FACE_OUTER_BOUND('',#6802,.T.);
#4608=FACE_OUTER_BOUND('',#6803,.T.);
#4609=FACE_OUTER_BOUND('',#6804,.T.);
#4610=FACE_OUTER_BOUND('',#6805,.T.);
#4611=FACE_OUTER_BOUND('',#6806,.T.);
#4612=FACE_OUTER_BOUND('',#6807,.T.);
#4613=FACE_OUTER_BOUND('',#6808,.T.);
#4614=FACE_OUTER_BOUND('',#6809,.T.);
#4615=FACE_OUTER_BOUND('',#6810,.T.);
#4616=FACE_OUTER_BOUND('',#6811,.T.);
#4617=FACE_OUTER_BOUND('',#6812,.T.);
#4618=FACE_OUTER_BOUND('',#6813,.T.);
#4619=FACE_OUTER_BOUND('',#6814,.T.);
#4620=FACE_OUTER_BOUND('',#6815,.T.);
#4621=FACE_OUTER_BOUND('',#6816,.T.);
#4622=FACE_OUTER_BOUND('',#6817,.T.);
#4623=FACE_OUTER_BOUND('',#6818,.T.);
#4624=FACE_OUTER_BOUND('',#6819,.T.);
#4625=FACE_OUTER_BOUND('',#6820,.T.);
#4626=FACE_OUTER_BOUND('',#6821,.T.);
#4627=FACE_OUTER_BOUND('',#6822,.T.);
#4628=FACE_OUTER_BOUND('',#6823,.T.);
#4629=FACE_OUTER_BOUND('',#6824,.T.);
#4630=FACE_OUTER_BOUND('',#6825,.T.);
#4631=FACE_OUTER_BOUND('',#6826,.T.);
#4632=FACE_OUTER_BOUND('',#6827,.T.);
#4633=FACE_OUTER_BOUND('',#6828,.T.);
#4634=FACE_OUTER_BOUND('',#6829,.T.);
#4635=FACE_OUTER_BOUND('',#6830,.T.);
#4636=FACE_OUTER_BOUND('',#6831,.T.);
#4637=FACE_OUTER_BOUND('',#6832,.T.);
#4638=FACE_OUTER_BOUND('',#6833,.T.);
#4639=FACE_OUTER_BOUND('',#6834,.T.);
#4640=FACE_OUTER_BOUND('',#6835,.T.);
#4641=FACE_OUTER_BOUND('',#6836,.T.);
#4642=FACE_OUTER_BOUND('',#6837,.T.);
#4643=FACE_OUTER_BOUND('',#6838,.T.);
#4644=FACE_OUTER_BOUND('',#6839,.T.);
#4645=FACE_OUTER_BOUND('',#6840,.T.);
#4646=FACE_OUTER_BOUND('',#6841,.T.);
#4647=FACE_OUTER_BOUND('',#6842,.T.);
#4648=FACE_OUTER_BOUND('',#6843,.T.);
#4649=FACE_OUTER_BOUND('',#6844,.T.);
#4650=FACE_OUTER_BOUND('',#6845,.T.);
#4651=FACE_OUTER_BOUND('',#6846,.T.);
#4652=FACE_OUTER_BOUND('',#6847,.T.);
#4653=FACE_OUTER_BOUND('',#6848,.T.);
#4654=FACE_OUTER_BOUND('',#6849,.T.);
#4655=FACE_OUTER_BOUND('',#6850,.T.);
#4656=FACE_OUTER_BOUND('',#6851,.T.);
#4657=FACE_OUTER_BOUND('',#6852,.T.);
#4658=FACE_OUTER_BOUND('',#6853,.T.);
#4659=FACE_OUTER_BOUND('',#6854,.T.);
#4660=FACE_OUTER_BOUND('',#6855,.T.);
#4661=FACE_OUTER_BOUND('',#6856,.T.);
#4662=FACE_OUTER_BOUND('',#6857,.T.);
#4663=FACE_OUTER_BOUND('',#6858,.T.);
#4664=FACE_OUTER_BOUND('',#6859,.T.);
#4665=FACE_OUTER_BOUND('',#6860,.T.);
#4666=FACE_OUTER_BOUND('',#6861,.T.);
#4667=FACE_OUTER_BOUND('',#6862,.T.);
#4668=FACE_OUTER_BOUND('',#6863,.T.);
#4669=FACE_OUTER_BOUND('',#6864,.T.);
#4670=FACE_OUTER_BOUND('',#6865,.T.);
#4671=FACE_OUTER_BOUND('',#6866,.T.);
#4672=FACE_OUTER_BOUND('',#6867,.T.);
#4673=FACE_OUTER_BOUND('',#6868,.T.);
#4674=FACE_OUTER_BOUND('',#6869,.T.);
#4675=FACE_OUTER_BOUND('',#6870,.T.);
#4676=FACE_OUTER_BOUND('',#6871,.T.);
#4677=FACE_OUTER_BOUND('',#6872,.T.);
#4678=FACE_OUTER_BOUND('',#6873,.T.);
#4679=FACE_OUTER_BOUND('',#6874,.T.);
#4680=FACE_OUTER_BOUND('',#6875,.T.);
#4681=FACE_OUTER_BOUND('',#6876,.T.);
#4682=FACE_OUTER_BOUND('',#6877,.T.);
#4683=FACE_OUTER_BOUND('',#6878,.T.);
#4684=FACE_OUTER_BOUND('',#6879,.T.);
#4685=FACE_OUTER_BOUND('',#6880,.T.);
#4686=FACE_OUTER_BOUND('',#6881,.T.);
#4687=FACE_OUTER_BOUND('',#6882,.T.);
#4688=FACE_OUTER_BOUND('',#6883,.T.);
#4689=FACE_OUTER_BOUND('',#6884,.T.);
#4690=FACE_OUTER_BOUND('',#6885,.T.);
#4691=FACE_OUTER_BOUND('',#6886,.T.);
#4692=FACE_OUTER_BOUND('',#6887,.T.);
#4693=FACE_OUTER_BOUND('',#6888,.T.);
#4694=FACE_OUTER_BOUND('',#6889,.T.);
#4695=FACE_OUTER_BOUND('',#6890,.T.);
#4696=FACE_OUTER_BOUND('',#6891,.T.);
#4697=FACE_OUTER_BOUND('',#6892,.T.);
#4698=FACE_OUTER_BOUND('',#6893,.T.);
#4699=FACE_OUTER_BOUND('',#6894,.T.);
#4700=FACE_OUTER_BOUND('',#6895,.T.);
#4701=FACE_OUTER_BOUND('',#6896,.T.);
#4702=FACE_OUTER_BOUND('',#6897,.T.);
#4703=FACE_OUTER_BOUND('',#6898,.T.);
#4704=FACE_OUTER_BOUND('',#6899,.T.);
#4705=FACE_OUTER_BOUND('',#6900,.T.);
#4706=FACE_OUTER_BOUND('',#6901,.T.);
#4707=FACE_OUTER_BOUND('',#6902,.T.);
#4708=FACE_OUTER_BOUND('',#6903,.T.);
#4709=FACE_OUTER_BOUND('',#6904,.T.);
#4710=FACE_OUTER_BOUND('',#6905,.T.);
#4711=FACE_OUTER_BOUND('',#6906,.T.);
#4712=FACE_OUTER_BOUND('',#6907,.T.);
#4713=FACE_OUTER_BOUND('',#6908,.T.);
#4714=FACE_OUTER_BOUND('',#6909,.T.);
#4715=FACE_OUTER_BOUND('',#6910,.T.);
#4716=FACE_OUTER_BOUND('',#6911,.T.);
#4717=FACE_OUTER_BOUND('',#6912,.T.);
#4718=FACE_OUTER_BOUND('',#6913,.T.);
#4719=FACE_OUTER_BOUND('',#6914,.T.);
#4720=FACE_OUTER_BOUND('',#6915,.T.);
#4721=FACE_OUTER_BOUND('',#6916,.T.);
#4722=FACE_OUTER_BOUND('',#6917,.T.);
#4723=FACE_OUTER_BOUND('',#6918,.T.);
#4724=FACE_OUTER_BOUND('',#6919,.T.);
#4725=FACE_OUTER_BOUND('',#6920,.T.);
#4726=FACE_OUTER_BOUND('',#6921,.T.);
#4727=FACE_OUTER_BOUND('',#6922,.T.);
#4728=FACE_OUTER_BOUND('',#6923,.T.);
#4729=FACE_OUTER_BOUND('',#6924,.T.);
#4730=FACE_OUTER_BOUND('',#6925,.T.);
#4731=FACE_OUTER_BOUND('',#6926,.T.);
#4732=FACE_OUTER_BOUND('',#6927,.T.);
#4733=FACE_OUTER_BOUND('',#6928,.T.);
#4734=FACE_OUTER_BOUND('',#6929,.T.);
#4735=FACE_OUTER_BOUND('',#6930,.T.);
#4736=FACE_OUTER_BOUND('',#6931,.T.);
#4737=FACE_OUTER_BOUND('',#6932,.T.);
#4738=FACE_OUTER_BOUND('',#6933,.T.);
#4739=FACE_OUTER_BOUND('',#6934,.T.);
#4740=FACE_OUTER_BOUND('',#6935,.T.);
#4741=FACE_OUTER_BOUND('',#6936,.T.);
#4742=FACE_OUTER_BOUND('',#6937,.T.);
#4743=FACE_OUTER_BOUND('',#6938,.T.);
#4744=FACE_OUTER_BOUND('',#6939,.T.);
#4745=FACE_OUTER_BOUND('',#6940,.T.);
#4746=FACE_OUTER_BOUND('',#6941,.T.);
#4747=FACE_OUTER_BOUND('',#6942,.T.);
#4748=FACE_OUTER_BOUND('',#6943,.T.);
#4749=FACE_OUTER_BOUND('',#6944,.T.);
#4750=FACE_OUTER_BOUND('',#6945,.T.);
#4751=FACE_OUTER_BOUND('',#6946,.T.);
#4752=FACE_OUTER_BOUND('',#6947,.T.);
#4753=FACE_OUTER_BOUND('',#6948,.T.);
#4754=FACE_OUTER_BOUND('',#6949,.T.);
#4755=FACE_OUTER_BOUND('',#6950,.T.);
#4756=FACE_OUTER_BOUND('',#6951,.T.);
#4757=FACE_OUTER_BOUND('',#6952,.T.);
#4758=FACE_OUTER_BOUND('',#6953,.T.);
#4759=FACE_OUTER_BOUND('',#6954,.T.);
#4760=FACE_OUTER_BOUND('',#6955,.T.);
#4761=FACE_OUTER_BOUND('',#6956,.T.);
#4762=FACE_OUTER_BOUND('',#6957,.T.);
#4763=FACE_OUTER_BOUND('',#6958,.T.);
#4764=FACE_OUTER_BOUND('',#6959,.T.);
#4765=FACE_OUTER_BOUND('',#6960,.T.);
#4766=FACE_OUTER_BOUND('',#6961,.T.);
#4767=FACE_OUTER_BOUND('',#6962,.T.);
#4768=FACE_OUTER_BOUND('',#6963,.T.);
#4769=FACE_OUTER_BOUND('',#6964,.T.);
#4770=FACE_OUTER_BOUND('',#6965,.T.);
#4771=FACE_OUTER_BOUND('',#6966,.T.);
#4772=FACE_OUTER_BOUND('',#6967,.T.);
#4773=FACE_OUTER_BOUND('',#6968,.T.);
#4774=FACE_OUTER_BOUND('',#6969,.T.);
#4775=FACE_OUTER_BOUND('',#6970,.T.);
#4776=FACE_OUTER_BOUND('',#6971,.T.);
#4777=FACE_OUTER_BOUND('',#6972,.T.);
#4778=FACE_OUTER_BOUND('',#6973,.T.);
#4779=FACE_OUTER_BOUND('',#6974,.T.);
#4780=FACE_OUTER_BOUND('',#6975,.T.);
#4781=FACE_OUTER_BOUND('',#6976,.T.);
#4782=FACE_OUTER_BOUND('',#6977,.T.);
#4783=FACE_OUTER_BOUND('',#6978,.T.);
#4784=FACE_OUTER_BOUND('',#6979,.T.);
#4785=FACE_OUTER_BOUND('',#6980,.T.);
#4786=FACE_OUTER_BOUND('',#6981,.T.);
#4787=FACE_OUTER_BOUND('',#6982,.T.);
#4788=FACE_OUTER_BOUND('',#6983,.T.);
#4789=FACE_OUTER_BOUND('',#6984,.T.);
#4790=FACE_OUTER_BOUND('',#6985,.T.);
#4791=FACE_OUTER_BOUND('',#6986,.T.);
#4792=FACE_OUTER_BOUND('',#6987,.T.);
#4793=FACE_OUTER_BOUND('',#6988,.T.);
#4794=FACE_OUTER_BOUND('',#6989,.T.);
#4795=FACE_OUTER_BOUND('',#6990,.T.);
#4796=FACE_OUTER_BOUND('',#6991,.T.);
#4797=FACE_OUTER_BOUND('',#6992,.T.);
#4798=FACE_OUTER_BOUND('',#6993,.T.);
#4799=FACE_OUTER_BOUND('',#6994,.T.);
#4800=FACE_OUTER_BOUND('',#6995,.T.);
#4801=FACE_OUTER_BOUND('',#6996,.T.);
#4802=FACE_OUTER_BOUND('',#6997,.T.);
#4803=FACE_OUTER_BOUND('',#6998,.T.);
#4804=FACE_OUTER_BOUND('',#6999,.T.);
#4805=FACE_OUTER_BOUND('',#7000,.T.);
#4806=FACE_OUTER_BOUND('',#7001,.T.);
#4807=FACE_OUTER_BOUND('',#7002,.T.);
#4808=FACE_OUTER_BOUND('',#7003,.T.);
#4809=FACE_OUTER_BOUND('',#7004,.T.);
#4810=FACE_OUTER_BOUND('',#7005,.T.);
#4811=FACE_OUTER_BOUND('',#7006,.T.);
#4812=FACE_OUTER_BOUND('',#7007,.T.);
#4813=FACE_OUTER_BOUND('',#7008,.T.);
#4814=FACE_OUTER_BOUND('',#7009,.T.);
#4815=FACE_OUTER_BOUND('',#7010,.T.);
#4816=FACE_OUTER_BOUND('',#7011,.T.);
#4817=FACE_OUTER_BOUND('',#7012,.T.);
#4818=FACE_OUTER_BOUND('',#7013,.T.);
#4819=FACE_OUTER_BOUND('',#7014,.T.);
#4820=FACE_OUTER_BOUND('',#7015,.T.);
#4821=FACE_OUTER_BOUND('',#7016,.T.);
#4822=FACE_OUTER_BOUND('',#7017,.T.);
#4823=FACE_OUTER_BOUND('',#7018,.T.);
#4824=FACE_OUTER_BOUND('',#7019,.T.);
#4825=FACE_OUTER_BOUND('',#7020,.T.);
#4826=FACE_OUTER_BOUND('',#7021,.T.);
#4827=FACE_OUTER_BOUND('',#7022,.T.);
#4828=FACE_OUTER_BOUND('',#7023,.T.);
#4829=FACE_OUTER_BOUND('',#7024,.T.);
#4830=FACE_OUTER_BOUND('',#7025,.T.);
#4831=FACE_OUTER_BOUND('',#7026,.T.);
#4832=FACE_OUTER_BOUND('',#7027,.T.);
#4833=FACE_OUTER_BOUND('',#7028,.T.);
#4834=FACE_OUTER_BOUND('',#7029,.T.);
#4835=FACE_OUTER_BOUND('',#7030,.T.);
#4836=FACE_OUTER_BOUND('',#7031,.T.);
#4837=FACE_OUTER_BOUND('',#7032,.T.);
#4838=FACE_OUTER_BOUND('',#7033,.T.);
#4839=FACE_OUTER_BOUND('',#7034,.T.);
#4840=FACE_OUTER_BOUND('',#7035,.T.);
#4841=FACE_OUTER_BOUND('',#7036,.T.);
#4842=FACE_OUTER_BOUND('',#7037,.T.);
#4843=FACE_OUTER_BOUND('',#7038,.T.);
#4844=FACE_OUTER_BOUND('',#7039,.T.);
#4845=FACE_OUTER_BOUND('',#7040,.T.);
#4846=FACE_OUTER_BOUND('',#7041,.T.);
#4847=FACE_OUTER_BOUND('',#7042,.T.);
#4848=FACE_OUTER_BOUND('',#7043,.T.);
#4849=FACE_OUTER_BOUND('',#7044,.T.);
#4850=FACE_OUTER_BOUND('',#7045,.T.);
#4851=FACE_OUTER_BOUND('',#7046,.T.);
#4852=FACE_OUTER_BOUND('',#7047,.T.);
#4853=FACE_OUTER_BOUND('',#7048,.T.);
#4854=FACE_OUTER_BOUND('',#7049,.T.);
#4855=FACE_OUTER_BOUND('',#7050,.T.);
#4856=FACE_OUTER_BOUND('',#7051,.T.);
#4857=FACE_OUTER_BOUND('',#7052,.T.);
#4858=FACE_OUTER_BOUND('',#7053,.T.);
#4859=FACE_OUTER_BOUND('',#7054,.T.);
#4860=FACE_OUTER_BOUND('',#7055,.T.);
#4861=FACE_OUTER_BOUND('',#7056,.T.);
#4862=FACE_OUTER_BOUND('',#7057,.T.);
#4863=FACE_OUTER_BOUND('',#7058,.T.);
#4864=FACE_OUTER_BOUND('',#7059,.T.);
#4865=FACE_OUTER_BOUND('',#7060,.T.);
#4866=FACE_OUTER_BOUND('',#7061,.T.);
#4867=FACE_OUTER_BOUND('',#7062,.T.);
#4868=FACE_OUTER_BOUND('',#7063,.T.);
#4869=FACE_OUTER_BOUND('',#7064,.T.);
#4870=FACE_OUTER_BOUND('',#7065,.T.);
#4871=FACE_OUTER_BOUND('',#7066,.T.);
#4872=FACE_OUTER_BOUND('',#7067,.T.);
#4873=FACE_OUTER_BOUND('',#7068,.T.);
#4874=FACE_OUTER_BOUND('',#7069,.T.);
#4875=FACE_OUTER_BOUND('',#7070,.T.);
#4876=FACE_OUTER_BOUND('',#7071,.T.);
#4877=FACE_OUTER_BOUND('',#7072,.T.);
#4878=FACE_OUTER_BOUND('',#7073,.T.);
#4879=FACE_OUTER_BOUND('',#7074,.T.);
#4880=FACE_OUTER_BOUND('',#7075,.T.);
#4881=FACE_OUTER_BOUND('',#7076,.T.);
#4882=FACE_OUTER_BOUND('',#7077,.T.);
#4883=FACE_OUTER_BOUND('',#7078,.T.);
#4884=FACE_OUTER_BOUND('',#7079,.T.);
#4885=FACE_OUTER_BOUND('',#7080,.T.);
#4886=FACE_OUTER_BOUND('',#7081,.T.);
#4887=FACE_OUTER_BOUND('',#7082,.T.);
#4888=FACE_OUTER_BOUND('',#7083,.T.);
#4889=FACE_OUTER_BOUND('',#7084,.T.);
#4890=FACE_OUTER_BOUND('',#7085,.T.);
#4891=FACE_OUTER_BOUND('',#7086,.T.);
#4892=FACE_OUTER_BOUND('',#7087,.T.);
#4893=FACE_OUTER_BOUND('',#7088,.T.);
#4894=FACE_OUTER_BOUND('',#7089,.T.);
#4895=FACE_OUTER_BOUND('',#7090,.T.);
#4896=FACE_OUTER_BOUND('',#7091,.T.);
#4897=FACE_OUTER_BOUND('',#7092,.T.);
#4898=FACE_OUTER_BOUND('',#7093,.T.);
#4899=FACE_OUTER_BOUND('',#7094,.T.);
#4900=FACE_OUTER_BOUND('',#7095,.T.);
#4901=FACE_OUTER_BOUND('',#7096,.T.);
#4902=FACE_OUTER_BOUND('',#7097,.T.);
#4903=FACE_OUTER_BOUND('',#7098,.T.);
#4904=FACE_OUTER_BOUND('',#7099,.T.);
#4905=FACE_OUTER_BOUND('',#7100,.T.);
#4906=FACE_OUTER_BOUND('',#7101,.T.);
#4907=FACE_OUTER_BOUND('',#7102,.T.);
#4908=FACE_OUTER_BOUND('',#7103,.T.);
#4909=FACE_OUTER_BOUND('',#7104,.T.);
#4910=FACE_OUTER_BOUND('',#7105,.T.);
#4911=FACE_OUTER_BOUND('',#7106,.T.);
#4912=FACE_OUTER_BOUND('',#7107,.T.);
#4913=FACE_OUTER_BOUND('',#7108,.T.);
#4914=FACE_OUTER_BOUND('',#7109,.T.);
#4915=FACE_OUTER_BOUND('',#7110,.T.);
#4916=FACE_OUTER_BOUND('',#7111,.T.);
#4917=FACE_OUTER_BOUND('',#7112,.T.);
#4918=FACE_OUTER_BOUND('',#7113,.T.);
#4919=FACE_OUTER_BOUND('',#7114,.T.);
#4920=FACE_OUTER_BOUND('',#7115,.T.);
#4921=FACE_OUTER_BOUND('',#7116,.T.);
#4922=FACE_OUTER_BOUND('',#7117,.T.);
#4923=FACE_OUTER_BOUND('',#7118,.T.);
#4924=FACE_OUTER_BOUND('',#7119,.T.);
#4925=FACE_OUTER_BOUND('',#7120,.T.);
#4926=FACE_OUTER_BOUND('',#7121,.T.);
#4927=FACE_OUTER_BOUND('',#7122,.T.);
#4928=FACE_OUTER_BOUND('',#7123,.T.);
#4929=FACE_OUTER_BOUND('',#7124,.T.);
#4930=FACE_OUTER_BOUND('',#7125,.T.);
#4931=FACE_OUTER_BOUND('',#7126,.T.);
#4932=FACE_OUTER_BOUND('',#7127,.T.);
#4933=FACE_OUTER_BOUND('',#7128,.T.);
#4934=FACE_OUTER_BOUND('',#7129,.T.);
#4935=FACE_OUTER_BOUND('',#7130,.T.);
#4936=FACE_OUTER_BOUND('',#7131,.T.);
#4937=FACE_OUTER_BOUND('',#7132,.T.);
#4938=FACE_OUTER_BOUND('',#7133,.T.);
#4939=FACE_OUTER_BOUND('',#7134,.T.);
#4940=FACE_OUTER_BOUND('',#7135,.T.);
#4941=FACE_OUTER_BOUND('',#7136,.T.);
#4942=FACE_OUTER_BOUND('',#7137,.T.);
#4943=FACE_OUTER_BOUND('',#7138,.T.);
#4944=FACE_OUTER_BOUND('',#7139,.T.);
#4945=FACE_OUTER_BOUND('',#7140,.T.);
#4946=FACE_OUTER_BOUND('',#7141,.T.);
#4947=FACE_OUTER_BOUND('',#7142,.T.);
#4948=FACE_OUTER_BOUND('',#7143,.T.);
#4949=FACE_OUTER_BOUND('',#7144,.T.);
#4950=FACE_OUTER_BOUND('',#7145,.T.);
#4951=FACE_OUTER_BOUND('',#7146,.T.);
#4952=FACE_OUTER_BOUND('',#7147,.T.);
#4953=FACE_OUTER_BOUND('',#7148,.T.);
#4954=FACE_OUTER_BOUND('',#7149,.T.);
#4955=FACE_OUTER_BOUND('',#7150,.T.);
#4956=FACE_OUTER_BOUND('',#7151,.T.);
#4957=FACE_OUTER_BOUND('',#7152,.T.);
#4958=FACE_OUTER_BOUND('',#7153,.T.);
#4959=FACE_OUTER_BOUND('',#7154,.T.);
#4960=FACE_OUTER_BOUND('',#7155,.T.);
#4961=FACE_OUTER_BOUND('',#7156,.T.);
#4962=FACE_OUTER_BOUND('',#7157,.T.);
#4963=FACE_OUTER_BOUND('',#7158,.T.);
#4964=FACE_OUTER_BOUND('',#7159,.T.);
#4965=FACE_OUTER_BOUND('',#7160,.T.);
#4966=FACE_OUTER_BOUND('',#7161,.T.);
#4967=FACE_OUTER_BOUND('',#7162,.T.);
#4968=FACE_OUTER_BOUND('',#7163,.T.);
#4969=FACE_OUTER_BOUND('',#7164,.T.);
#4970=FACE_OUTER_BOUND('',#7165,.T.);
#4971=FACE_OUTER_BOUND('',#7166,.T.);
#4972=FACE_OUTER_BOUND('',#7167,.T.);
#4973=FACE_OUTER_BOUND('',#7168,.T.);
#4974=FACE_OUTER_BOUND('',#7169,.T.);
#4975=FACE_OUTER_BOUND('',#7170,.T.);
#4976=FACE_OUTER_BOUND('',#7171,.T.);
#4977=FACE_OUTER_BOUND('',#7172,.T.);
#4978=FACE_OUTER_BOUND('',#7173,.T.);
#4979=FACE_OUTER_BOUND('',#7174,.T.);
#4980=FACE_OUTER_BOUND('',#7175,.T.);
#4981=FACE_OUTER_BOUND('',#7176,.T.);
#4982=FACE_OUTER_BOUND('',#7177,.T.);
#4983=FACE_OUTER_BOUND('',#7178,.T.);
#4984=FACE_OUTER_BOUND('',#7179,.T.);
#4985=FACE_OUTER_BOUND('',#7180,.T.);
#4986=FACE_OUTER_BOUND('',#7181,.T.);
#4987=FACE_OUTER_BOUND('',#7182,.T.);
#4988=FACE_OUTER_BOUND('',#7183,.T.);
#4989=FACE_OUTER_BOUND('',#7184,.T.);
#4990=FACE_OUTER_BOUND('',#7185,.T.);
#4991=FACE_OUTER_BOUND('',#7186,.T.);
#4992=FACE_OUTER_BOUND('',#7187,.T.);
#4993=FACE_OUTER_BOUND('',#7188,.T.);
#4994=FACE_OUTER_BOUND('',#7189,.T.);
#4995=FACE_OUTER_BOUND('',#7190,.T.);
#4996=FACE_OUTER_BOUND('',#7191,.T.);
#4997=FACE_OUTER_BOUND('',#7192,.T.);
#4998=FACE_OUTER_BOUND('',#7193,.T.);
#4999=FACE_OUTER_BOUND('',#7194,.T.);
#5000=FACE_OUTER_BOUND('',#7195,.T.);
#5001=FACE_OUTER_BOUND('',#7196,.T.);
#5002=FACE_OUTER_BOUND('',#7197,.T.);
#5003=FACE_OUTER_BOUND('',#7198,.T.);
#5004=FACE_OUTER_BOUND('',#7199,.T.);
#5005=FACE_OUTER_BOUND('',#7200,.T.);
#5006=FACE_OUTER_BOUND('',#7202,.T.);
#5007=FACE_OUTER_BOUND('',#7203,.T.);
#5008=FACE_OUTER_BOUND('',#7204,.T.);
#5009=FACE_OUTER_BOUND('',#7205,.T.);
#5010=FACE_OUTER_BOUND('',#7206,.T.);
#5011=FACE_OUTER_BOUND('',#7207,.T.);
#5012=FACE_OUTER_BOUND('',#7208,.T.);
#5013=FACE_OUTER_BOUND('',#7209,.T.);
#5014=FACE_OUTER_BOUND('',#7210,.T.);
#5015=FACE_OUTER_BOUND('',#7211,.T.);
#5016=FACE_OUTER_BOUND('',#7212,.T.);
#5017=FACE_OUTER_BOUND('',#7213,.T.);
#5018=FACE_OUTER_BOUND('',#7214,.T.);
#5019=FACE_OUTER_BOUND('',#7215,.T.);
#5020=FACE_OUTER_BOUND('',#7216,.T.);
#5021=FACE_OUTER_BOUND('',#7217,.T.);
#5022=FACE_OUTER_BOUND('',#7218,.T.);
#5023=FACE_OUTER_BOUND('',#7219,.T.);
#5024=FACE_OUTER_BOUND('',#7220,.T.);
#5025=FACE_OUTER_BOUND('',#7221,.T.);
#5026=FACE_OUTER_BOUND('',#7222,.T.);
#5027=FACE_OUTER_BOUND('',#7223,.T.);
#5028=FACE_OUTER_BOUND('',#7224,.T.);
#5029=FACE_OUTER_BOUND('',#7225,.T.);
#5030=FACE_OUTER_BOUND('',#7226,.T.);
#5031=FACE_OUTER_BOUND('',#7227,.T.);
#5032=FACE_OUTER_BOUND('',#7228,.T.);
#5033=FACE_OUTER_BOUND('',#7229,.T.);
#5034=FACE_OUTER_BOUND('',#7230,.T.);
#5035=FACE_OUTER_BOUND('',#7231,.T.);
#5036=FACE_OUTER_BOUND('',#7232,.T.);
#5037=FACE_OUTER_BOUND('',#7233,.T.);
#5038=FACE_OUTER_BOUND('',#7234,.T.);
#5039=FACE_OUTER_BOUND('',#7235,.T.);
#5040=FACE_OUTER_BOUND('',#7236,.T.);
#5041=FACE_OUTER_BOUND('',#7237,.T.);
#5042=FACE_OUTER_BOUND('',#7238,.T.);
#5043=FACE_OUTER_BOUND('',#7239,.T.);
#5044=FACE_OUTER_BOUND('',#7240,.T.);
#5045=FACE_OUTER_BOUND('',#7241,.T.);
#5046=FACE_OUTER_BOUND('',#7242,.T.);
#5047=FACE_OUTER_BOUND('',#7243,.T.);
#5048=FACE_OUTER_BOUND('',#7244,.T.);
#5049=FACE_OUTER_BOUND('',#7245,.T.);
#5050=FACE_OUTER_BOUND('',#7246,.T.);
#5051=FACE_OUTER_BOUND('',#7247,.T.);
#5052=FACE_OUTER_BOUND('',#7248,.T.);
#5053=FACE_OUTER_BOUND('',#7249,.T.);
#5054=FACE_OUTER_BOUND('',#7250,.T.);
#5055=FACE_OUTER_BOUND('',#7251,.T.);
#5056=FACE_OUTER_BOUND('',#7252,.T.);
#5057=FACE_OUTER_BOUND('',#7253,.T.);
#5058=FACE_OUTER_BOUND('',#7254,.T.);
#5059=FACE_OUTER_BOUND('',#7255,.T.);
#5060=FACE_OUTER_BOUND('',#7256,.T.);
#5061=FACE_OUTER_BOUND('',#7257,.T.);
#5062=FACE_OUTER_BOUND('',#7258,.T.);
#5063=FACE_OUTER_BOUND('',#7259,.T.);
#5064=FACE_OUTER_BOUND('',#7260,.T.);
#5065=FACE_OUTER_BOUND('',#7261,.T.);
#5066=FACE_OUTER_BOUND('',#7262,.T.);
#5067=FACE_OUTER_BOUND('',#7263,.T.);
#5068=FACE_OUTER_BOUND('',#7264,.T.);
#5069=FACE_OUTER_BOUND('',#7265,.T.);
#5070=FACE_OUTER_BOUND('',#7266,.T.);
#5071=FACE_OUTER_BOUND('',#7267,.T.);
#5072=FACE_OUTER_BOUND('',#7268,.T.);
#5073=FACE_OUTER_BOUND('',#7269,.T.);
#5074=FACE_OUTER_BOUND('',#7270,.T.);
#5075=FACE_OUTER_BOUND('',#7271,.T.);
#5076=FACE_OUTER_BOUND('',#7272,.T.);
#5077=FACE_OUTER_BOUND('',#7273,.T.);
#5078=FACE_OUTER_BOUND('',#7274,.T.);
#5079=FACE_OUTER_BOUND('',#7275,.T.);
#5080=FACE_OUTER_BOUND('',#7276,.T.);
#5081=FACE_OUTER_BOUND('',#7277,.T.);
#5082=FACE_OUTER_BOUND('',#7278,.T.);
#5083=FACE_OUTER_BOUND('',#7279,.T.);
#5084=FACE_OUTER_BOUND('',#7280,.T.);
#5085=FACE_OUTER_BOUND('',#7281,.T.);
#5086=FACE_OUTER_BOUND('',#7282,.T.);
#5087=FACE_OUTER_BOUND('',#7283,.T.);
#5088=FACE_OUTER_BOUND('',#7284,.T.);
#5089=FACE_OUTER_BOUND('',#7285,.T.);
#5090=FACE_OUTER_BOUND('',#7286,.T.);
#5091=FACE_OUTER_BOUND('',#7287,.T.);
#5092=FACE_OUTER_BOUND('',#7288,.T.);
#5093=FACE_OUTER_BOUND('',#7289,.T.);
#5094=FACE_OUTER_BOUND('',#7290,.T.);
#5095=FACE_OUTER_BOUND('',#7291,.T.);
#5096=FACE_OUTER_BOUND('',#7292,.T.);
#5097=FACE_OUTER_BOUND('',#7293,.T.);
#5098=FACE_OUTER_BOUND('',#7294,.T.);
#5099=FACE_OUTER_BOUND('',#7295,.T.);
#5100=FACE_OUTER_BOUND('',#7296,.T.);
#5101=FACE_OUTER_BOUND('',#7297,.T.);
#5102=FACE_OUTER_BOUND('',#7298,.T.);
#5103=FACE_OUTER_BOUND('',#7299,.T.);
#5104=FACE_OUTER_BOUND('',#7300,.T.);
#5105=FACE_OUTER_BOUND('',#7301,.T.);
#5106=FACE_OUTER_BOUND('',#7302,.T.);
#5107=FACE_OUTER_BOUND('',#7303,.T.);
#5108=FACE_OUTER_BOUND('',#7304,.T.);
#5109=FACE_OUTER_BOUND('',#7305,.T.);
#5110=FACE_OUTER_BOUND('',#7306,.T.);
#5111=FACE_OUTER_BOUND('',#7307,.T.);
#5112=FACE_OUTER_BOUND('',#7308,.T.);
#5113=FACE_OUTER_BOUND('',#7309,.T.);
#5114=FACE_OUTER_BOUND('',#7310,.T.);
#5115=FACE_OUTER_BOUND('',#7311,.T.);
#5116=FACE_OUTER_BOUND('',#7312,.T.);
#5117=FACE_OUTER_BOUND('',#7313,.T.);
#5118=FACE_OUTER_BOUND('',#7314,.T.);
#5119=FACE_OUTER_BOUND('',#7315,.T.);
#5120=FACE_OUTER_BOUND('',#7316,.T.);
#5121=FACE_OUTER_BOUND('',#7317,.T.);
#5122=FACE_OUTER_BOUND('',#7318,.T.);
#5123=FACE_OUTER_BOUND('',#7319,.T.);
#5124=FACE_OUTER_BOUND('',#7320,.T.);
#5125=FACE_OUTER_BOUND('',#7321,.T.);
#5126=FACE_OUTER_BOUND('',#7322,.T.);
#5127=FACE_OUTER_BOUND('',#7323,.T.);
#5128=FACE_OUTER_BOUND('',#7324,.T.);
#5129=FACE_OUTER_BOUND('',#7325,.T.);
#5130=FACE_OUTER_BOUND('',#7326,.T.);
#5131=FACE_OUTER_BOUND('',#7327,.T.);
#5132=FACE_OUTER_BOUND('',#7328,.T.);
#5133=FACE_OUTER_BOUND('',#7329,.T.);
#5134=FACE_OUTER_BOUND('',#7330,.T.);
#5135=FACE_OUTER_BOUND('',#7331,.T.);
#5136=FACE_OUTER_BOUND('',#7332,.T.);
#5137=FACE_OUTER_BOUND('',#7333,.T.);
#5138=FACE_OUTER_BOUND('',#7334,.T.);
#5139=FACE_OUTER_BOUND('',#7335,.T.);
#5140=FACE_OUTER_BOUND('',#7336,.T.);
#5141=FACE_OUTER_BOUND('',#7337,.T.);
#5142=FACE_OUTER_BOUND('',#7338,.T.);
#5143=FACE_OUTER_BOUND('',#7344,.T.);
#5144=FACE_OUTER_BOUND('',#7345,.T.);
#5145=FACE_OUTER_BOUND('',#7346,.T.);
#5146=FACE_OUTER_BOUND('',#7347,.T.);
#5147=FACE_OUTER_BOUND('',#7348,.T.);
#5148=FACE_OUTER_BOUND('',#7349,.T.);
#5149=FACE_OUTER_BOUND('',#7350,.T.);
#5150=FACE_OUTER_BOUND('',#7351,.T.);
#5151=FACE_OUTER_BOUND('',#7352,.T.);
#5152=FACE_OUTER_BOUND('',#7353,.T.);
#5153=FACE_OUTER_BOUND('',#7354,.T.);
#5154=FACE_OUTER_BOUND('',#7355,.T.);
#5155=FACE_OUTER_BOUND('',#7356,.T.);
#5156=FACE_OUTER_BOUND('',#7357,.T.);
#5157=FACE_OUTER_BOUND('',#7358,.T.);
#5158=FACE_OUTER_BOUND('',#7359,.T.);
#5159=FACE_OUTER_BOUND('',#7360,.T.);
#5160=FACE_OUTER_BOUND('',#7361,.T.);
#5161=FACE_OUTER_BOUND('',#7362,.T.);
#5162=FACE_OUTER_BOUND('',#7363,.T.);
#5163=FACE_OUTER_BOUND('',#7364,.T.);
#5164=FACE_OUTER_BOUND('',#7365,.T.);
#5165=FACE_OUTER_BOUND('',#7366,.T.);
#5166=FACE_OUTER_BOUND('',#7367,.T.);
#5167=FACE_OUTER_BOUND('',#7368,.T.);
#5168=FACE_OUTER_BOUND('',#7369,.T.);
#5169=FACE_OUTER_BOUND('',#7370,.T.);
#5170=FACE_OUTER_BOUND('',#7371,.T.);
#5171=FACE_OUTER_BOUND('',#7372,.T.);
#5172=FACE_OUTER_BOUND('',#7373,.T.);
#5173=FACE_OUTER_BOUND('',#7374,.T.);
#5174=FACE_OUTER_BOUND('',#7375,.T.);
#5175=FACE_OUTER_BOUND('',#7376,.T.);
#5176=FACE_OUTER_BOUND('',#7377,.T.);
#5177=FACE_OUTER_BOUND('',#7378,.T.);
#5178=FACE_OUTER_BOUND('',#7379,.T.);
#5179=FACE_OUTER_BOUND('',#7380,.T.);
#5180=FACE_OUTER_BOUND('',#7381,.T.);
#5181=FACE_OUTER_BOUND('',#7382,.T.);
#5182=FACE_OUTER_BOUND('',#7383,.T.);
#5183=FACE_OUTER_BOUND('',#7384,.T.);
#5184=FACE_OUTER_BOUND('',#7385,.T.);
#5185=FACE_OUTER_BOUND('',#7386,.T.);
#5186=FACE_OUTER_BOUND('',#7387,.T.);
#5187=FACE_OUTER_BOUND('',#7388,.T.);
#5188=FACE_OUTER_BOUND('',#7389,.T.);
#5189=FACE_OUTER_BOUND('',#7390,.T.);
#5190=FACE_OUTER_BOUND('',#7391,.T.);
#5191=FACE_OUTER_BOUND('',#7392,.T.);
#5192=FACE_OUTER_BOUND('',#7393,.T.);
#5193=FACE_OUTER_BOUND('',#7394,.T.);
#5194=FACE_OUTER_BOUND('',#7395,.T.);
#5195=FACE_OUTER_BOUND('',#7396,.T.);
#5196=FACE_OUTER_BOUND('',#7397,.T.);
#5197=FACE_OUTER_BOUND('',#7398,.T.);
#5198=FACE_OUTER_BOUND('',#7399,.T.);
#5199=FACE_OUTER_BOUND('',#7400,.T.);
#5200=FACE_OUTER_BOUND('',#7401,.T.);
#5201=FACE_OUTER_BOUND('',#7402,.T.);
#5202=FACE_OUTER_BOUND('',#7403,.T.);
#5203=FACE_OUTER_BOUND('',#7404,.T.);
#5204=FACE_OUTER_BOUND('',#7405,.T.);
#5205=FACE_OUTER_BOUND('',#7406,.T.);
#5206=FACE_OUTER_BOUND('',#7407,.T.);
#5207=FACE_OUTER_BOUND('',#7408,.T.);
#5208=FACE_OUTER_BOUND('',#7409,.T.);
#5209=FACE_OUTER_BOUND('',#7410,.T.);
#5210=FACE_OUTER_BOUND('',#7411,.T.);
#5211=FACE_OUTER_BOUND('',#7412,.T.);
#5212=FACE_OUTER_BOUND('',#7413,.T.);
#5213=FACE_OUTER_BOUND('',#7414,.T.);
#5214=FACE_OUTER_BOUND('',#7415,.T.);
#5215=FACE_OUTER_BOUND('',#7416,.T.);
#5216=FACE_OUTER_BOUND('',#7417,.T.);
#5217=FACE_OUTER_BOUND('',#7418,.T.);
#5218=FACE_OUTER_BOUND('',#7419,.T.);
#5219=FACE_OUTER_BOUND('',#7420,.T.);
#5220=FACE_OUTER_BOUND('',#7421,.T.);
#5221=FACE_OUTER_BOUND('',#7422,.T.);
#5222=FACE_OUTER_BOUND('',#7423,.T.);
#5223=FACE_OUTER_BOUND('',#7424,.T.);
#5224=FACE_OUTER_BOUND('',#7425,.T.);
#5225=FACE_OUTER_BOUND('',#7426,.T.);
#5226=FACE_OUTER_BOUND('',#7427,.T.);
#5227=FACE_OUTER_BOUND('',#7428,.T.);
#5228=FACE_OUTER_BOUND('',#7429,.T.);
#5229=FACE_OUTER_BOUND('',#7430,.T.);
#5230=FACE_OUTER_BOUND('',#7431,.T.);
#5231=FACE_OUTER_BOUND('',#7432,.T.);
#5232=FACE_OUTER_BOUND('',#7433,.T.);
#5233=FACE_OUTER_BOUND('',#7434,.T.);
#5234=FACE_OUTER_BOUND('',#7435,.T.);
#5235=FACE_OUTER_BOUND('',#7436,.T.);
#5236=FACE_OUTER_BOUND('',#7437,.T.);
#5237=FACE_OUTER_BOUND('',#7438,.T.);
#5238=FACE_OUTER_BOUND('',#7439,.T.);
#5239=FACE_OUTER_BOUND('',#7440,.T.);
#5240=FACE_OUTER_BOUND('',#7441,.T.);
#5241=FACE_OUTER_BOUND('',#7443,.T.);
#5242=FACE_OUTER_BOUND('',#7444,.T.);
#5243=FACE_OUTER_BOUND('',#7445,.T.);
#5244=FACE_OUTER_BOUND('',#7446,.T.);
#5245=FACE_OUTER_BOUND('',#7447,.T.);
#5246=FACE_OUTER_BOUND('',#7448,.T.);
#5247=FACE_OUTER_BOUND('',#7449,.T.);
#5248=FACE_OUTER_BOUND('',#7450,.T.);
#5249=FACE_OUTER_BOUND('',#7451,.T.);
#5250=FACE_OUTER_BOUND('',#7452,.T.);
#5251=FACE_OUTER_BOUND('',#7453,.T.);
#5252=FACE_OUTER_BOUND('',#7454,.T.);
#5253=FACE_OUTER_BOUND('',#7455,.T.);
#5254=FACE_OUTER_BOUND('',#7456,.T.);
#5255=FACE_OUTER_BOUND('',#7457,.T.);
#5256=FACE_OUTER_BOUND('',#7458,.T.);
#5257=FACE_OUTER_BOUND('',#7459,.T.);
#5258=FACE_OUTER_BOUND('',#7460,.T.);
#5259=FACE_OUTER_BOUND('',#7461,.T.);
#5260=FACE_OUTER_BOUND('',#7462,.T.);
#5261=FACE_OUTER_BOUND('',#7463,.T.);
#5262=FACE_OUTER_BOUND('',#7464,.T.);
#5263=FACE_OUTER_BOUND('',#7465,.T.);
#5264=FACE_OUTER_BOUND('',#7466,.T.);
#5265=FACE_OUTER_BOUND('',#7467,.T.);
#5266=FACE_OUTER_BOUND('',#7468,.T.);
#5267=FACE_OUTER_BOUND('',#7469,.T.);
#5268=FACE_OUTER_BOUND('',#7470,.T.);
#5269=FACE_OUTER_BOUND('',#7471,.T.);
#5270=FACE_OUTER_BOUND('',#7472,.T.);
#5271=FACE_OUTER_BOUND('',#7473,.T.);
#5272=FACE_OUTER_BOUND('',#7474,.T.);
#5273=FACE_OUTER_BOUND('',#7475,.T.);
#5274=FACE_OUTER_BOUND('',#7476,.T.);
#5275=FACE_OUTER_BOUND('',#7477,.T.);
#5276=FACE_OUTER_BOUND('',#7478,.T.);
#5277=FACE_OUTER_BOUND('',#7479,.T.);
#5278=FACE_OUTER_BOUND('',#7480,.T.);
#5279=FACE_OUTER_BOUND('',#7481,.T.);
#5280=FACE_OUTER_BOUND('',#7482,.T.);
#5281=FACE_OUTER_BOUND('',#7483,.T.);
#5282=FACE_OUTER_BOUND('',#7484,.T.);
#5283=FACE_OUTER_BOUND('',#7485,.T.);
#5284=FACE_OUTER_BOUND('',#7486,.T.);
#5285=FACE_OUTER_BOUND('',#7487,.T.);
#5286=FACE_OUTER_BOUND('',#7488,.T.);
#5287=FACE_OUTER_BOUND('',#7489,.T.);
#5288=FACE_OUTER_BOUND('',#7490,.T.);
#5289=FACE_OUTER_BOUND('',#7491,.T.);
#5290=FACE_OUTER_BOUND('',#7492,.T.);
#5291=FACE_OUTER_BOUND('',#7493,.T.);
#5292=FACE_OUTER_BOUND('',#7494,.T.);
#5293=FACE_OUTER_BOUND('',#7495,.T.);
#5294=FACE_OUTER_BOUND('',#7496,.T.);
#5295=FACE_OUTER_BOUND('',#7497,.T.);
#5296=FACE_OUTER_BOUND('',#7498,.T.);
#5297=FACE_OUTER_BOUND('',#7499,.T.);
#5298=FACE_OUTER_BOUND('',#7500,.T.);
#5299=FACE_OUTER_BOUND('',#7501,.T.);
#5300=FACE_OUTER_BOUND('',#7502,.T.);
#5301=FACE_OUTER_BOUND('',#7503,.T.);
#5302=FACE_OUTER_BOUND('',#7504,.T.);
#5303=FACE_OUTER_BOUND('',#7505,.T.);
#5304=FACE_OUTER_BOUND('',#7506,.T.);
#5305=FACE_OUTER_BOUND('',#7507,.T.);
#5306=FACE_OUTER_BOUND('',#7508,.T.);
#5307=FACE_OUTER_BOUND('',#7510,.T.);
#5308=FACE_OUTER_BOUND('',#7511,.T.);
#5309=FACE_OUTER_BOUND('',#7512,.T.);
#5310=FACE_OUTER_BOUND('',#7513,.T.);
#5311=FACE_OUTER_BOUND('',#7514,.T.);
#5312=FACE_OUTER_BOUND('',#7515,.T.);
#5313=FACE_OUTER_BOUND('',#7516,.T.);
#5314=FACE_OUTER_BOUND('',#7517,.T.);
#5315=FACE_OUTER_BOUND('',#7518,.T.);
#5316=FACE_OUTER_BOUND('',#7519,.T.);
#5317=FACE_OUTER_BOUND('',#7520,.T.);
#5318=FACE_OUTER_BOUND('',#7521,.T.);
#5319=FACE_OUTER_BOUND('',#7522,.T.);
#5320=FACE_OUTER_BOUND('',#7523,.T.);
#5321=FACE_OUTER_BOUND('',#7524,.T.);
#5322=FACE_OUTER_BOUND('',#7525,.T.);
#5323=FACE_OUTER_BOUND('',#7526,.T.);
#5324=FACE_OUTER_BOUND('',#7527,.T.);
#5325=FACE_OUTER_BOUND('',#7528,.T.);
#5326=FACE_OUTER_BOUND('',#7529,.T.);
#5327=FACE_OUTER_BOUND('',#7530,.T.);
#5328=FACE_OUTER_BOUND('',#7531,.T.);
#5329=FACE_OUTER_BOUND('',#7532,.T.);
#5330=FACE_OUTER_BOUND('',#7533,.T.);
#5331=FACE_OUTER_BOUND('',#7534,.T.);
#5332=FACE_OUTER_BOUND('',#7535,.T.);
#5333=FACE_OUTER_BOUND('',#7536,.T.);
#5334=FACE_OUTER_BOUND('',#7537,.T.);
#5335=FACE_OUTER_BOUND('',#7538,.T.);
#5336=FACE_OUTER_BOUND('',#7539,.T.);
#5337=FACE_OUTER_BOUND('',#7540,.T.);
#5338=FACE_OUTER_BOUND('',#7541,.T.);
#5339=FACE_OUTER_BOUND('',#7542,.T.);
#5340=FACE_OUTER_BOUND('',#7543,.T.);
#5341=FACE_OUTER_BOUND('',#7544,.T.);
#5342=FACE_OUTER_BOUND('',#7545,.T.);
#5343=FACE_OUTER_BOUND('',#7546,.T.);
#5344=FACE_OUTER_BOUND('',#7547,.T.);
#5345=FACE_OUTER_BOUND('',#7548,.T.);
#5346=FACE_OUTER_BOUND('',#7549,.T.);
#5347=FACE_OUTER_BOUND('',#7550,.T.);
#5348=FACE_OUTER_BOUND('',#7551,.T.);
#5349=FACE_OUTER_BOUND('',#7552,.T.);
#5350=FACE_OUTER_BOUND('',#7553,.T.);
#5351=FACE_OUTER_BOUND('',#7554,.T.);
#5352=FACE_OUTER_BOUND('',#7555,.T.);
#5353=FACE_OUTER_BOUND('',#7556,.T.);
#5354=FACE_OUTER_BOUND('',#7557,.T.);
#5355=FACE_OUTER_BOUND('',#7558,.T.);
#5356=FACE_OUTER_BOUND('',#7559,.T.);
#5357=FACE_OUTER_BOUND('',#7560,.T.);
#5358=FACE_OUTER_BOUND('',#7561,.T.);
#5359=FACE_OUTER_BOUND('',#7562,.T.);
#5360=FACE_OUTER_BOUND('',#7563,.T.);
#5361=FACE_OUTER_BOUND('',#7566,.T.);
#5362=FACE_OUTER_BOUND('',#7567,.T.);
#5363=FACE_OUTER_BOUND('',#7568,.T.);
#5364=FACE_OUTER_BOUND('',#7569,.T.);
#5365=FACE_OUTER_BOUND('',#7570,.T.);
#5366=FACE_OUTER_BOUND('',#7571,.T.);
#5367=FACE_OUTER_BOUND('',#7572,.T.);
#5368=FACE_OUTER_BOUND('',#7573,.T.);
#5369=FACE_OUTER_BOUND('',#7574,.T.);
#5370=FACE_OUTER_BOUND('',#7575,.T.);
#5371=FACE_OUTER_BOUND('',#7576,.T.);
#5372=FACE_OUTER_BOUND('',#7577,.T.);
#5373=FACE_OUTER_BOUND('',#7578,.T.);
#5374=FACE_OUTER_BOUND('',#7579,.T.);
#5375=FACE_OUTER_BOUND('',#7580,.T.);
#5376=FACE_OUTER_BOUND('',#7581,.T.);
#5377=FACE_OUTER_BOUND('',#7582,.T.);
#5378=FACE_OUTER_BOUND('',#7583,.T.);
#5379=FACE_OUTER_BOUND('',#7584,.T.);
#5380=FACE_OUTER_BOUND('',#7585,.T.);
#5381=FACE_OUTER_BOUND('',#7586,.T.);
#5382=FACE_OUTER_BOUND('',#7587,.T.);
#5383=FACE_OUTER_BOUND('',#7588,.T.);
#5384=FACE_OUTER_BOUND('',#7589,.T.);
#5385=FACE_OUTER_BOUND('',#7590,.T.);
#5386=FACE_OUTER_BOUND('',#7591,.T.);
#5387=FACE_OUTER_BOUND('',#7592,.T.);
#5388=FACE_OUTER_BOUND('',#7593,.T.);
#5389=FACE_OUTER_BOUND('',#7594,.T.);
#5390=FACE_OUTER_BOUND('',#7595,.T.);
#5391=FACE_OUTER_BOUND('',#7596,.T.);
#5392=FACE_OUTER_BOUND('',#7597,.T.);
#5393=FACE_OUTER_BOUND('',#7598,.T.);
#5394=FACE_OUTER_BOUND('',#7609,.T.);
#5395=FACE_OUTER_BOUND('',#7610,.T.);
#5396=FACE_OUTER_BOUND('',#7611,.T.);
#5397=FACE_OUTER_BOUND('',#7612,.T.);
#5398=FACE_OUTER_BOUND('',#7613,.T.);
#5399=FACE_OUTER_BOUND('',#7614,.T.);
#5400=FACE_OUTER_BOUND('',#7615,.T.);
#5401=FACE_OUTER_BOUND('',#7616,.T.);
#5402=FACE_OUTER_BOUND('',#7617,.T.);
#5403=FACE_OUTER_BOUND('',#7618,.T.);
#5404=FACE_OUTER_BOUND('',#7620,.T.);
#5405=FACE_OUTER_BOUND('',#7621,.T.);
#5406=FACE_OUTER_BOUND('',#7622,.T.);
#5407=FACE_OUTER_BOUND('',#7623,.T.);
#5408=FACE_OUTER_BOUND('',#7624,.T.);
#5409=FACE_OUTER_BOUND('',#7625,.T.);
#5410=FACE_OUTER_BOUND('',#7626,.T.);
#5411=FACE_OUTER_BOUND('',#7627,.T.);
#5412=FACE_OUTER_BOUND('',#7628,.T.);
#5413=FACE_OUTER_BOUND('',#7629,.T.);
#5414=FACE_OUTER_BOUND('',#7630,.T.);
#5415=FACE_OUTER_BOUND('',#7632,.T.);
#5416=FACE_OUTER_BOUND('',#7633,.T.);
#5417=FACE_OUTER_BOUND('',#7635,.T.);
#5418=FACE_OUTER_BOUND('',#7636,.T.);
#5419=EDGE_LOOP('',(#21783,#21784,#21785,#21786,#21787));
#5420=EDGE_LOOP('',(#21788,#21789,#21790,#21791,#21792,#21793));
#5421=EDGE_LOOP('',(#21794));
#5422=EDGE_LOOP('',(#21795,#21796,#21797,#21798,#21799));
#5423=EDGE_LOOP('',(#21800));
#5424=EDGE_LOOP('',(#21801,#21802,#21803,#21804));
#5425=EDGE_LOOP('',(#21805,#21806,#21807,#21808,#21809,#21810,#21811,#21812,
#21813,#21814,#21815,#21816,#21817,#21818,#21819,#21820,#21821,#21822,#21823,
#21824,#21825,#21826,#21827,#21828,#21829,#21830,#21831,#21832,#21833,#21834,
#21835,#21836,#21837,#21838,#21839,#21840,#21841,#21842,#21843,#21844));
#5426=EDGE_LOOP('',(#21845,#21846,#21847,#21848,#21849,#21850,#21851,#21852,
#21853,#21854));
#5427=EDGE_LOOP('',(#21855,#21856,#21857,#21858,#21859,#21860,#21861,#21862,
#21863));
#5428=EDGE_LOOP('',(#21864,#21865,#21866,#21867,#21868,#21869,#21870,#21871,
#21872,#21873));
#5429=EDGE_LOOP('',(#21874,#21875,#21876,#21877,#21878));
#5430=EDGE_LOOP('',(#21879,#21880,#21881));
#5431=EDGE_LOOP('',(#21882,#21883,#21884,#21885));
#5432=EDGE_LOOP('',(#21886,#21887,#21888,#21889));
#5433=EDGE_LOOP('',(#21890,#21891,#21892,#21893,#21894));
#5434=EDGE_LOOP('',(#21895,#21896,#21897,#21898));
#5435=EDGE_LOOP('',(#21899,#21900,#21901,#21902,#21903,#21904));
#5436=EDGE_LOOP('',(#21905,#21906,#21907,#21908,#21909,#21910,#21911));
#5437=EDGE_LOOP('',(#21912,#21913,#21914,#21915,#21916));
#5438=EDGE_LOOP('',(#21917,#21918,#21919,#21920,#21921,#21922,#21923));
#5439=EDGE_LOOP('',(#21924,#21925,#21926,#21927,#21928));
#5440=EDGE_LOOP('',(#21929,#21930,#21931,#21932,#21933));
#5441=EDGE_LOOP('',(#21934,#21935,#21936,#21937,#21938,#21939));
#5442=EDGE_LOOP('',(#21940,#21941,#21942,#21943,#21944));
#5443=EDGE_LOOP('',(#21945,#21946,#21947,#21948));
#5444=EDGE_LOOP('',(#21949,#21950,#21951,#21952,#21953,#21954));
#5445=EDGE_LOOP('',(#21955,#21956,#21957,#21958,#21959));
#5446=EDGE_LOOP('',(#21960,#21961,#21962,#21963,#21964));
#5447=EDGE_LOOP('',(#21965,#21966,#21967,#21968,#21969,#21970,#21971));
#5448=EDGE_LOOP('',(#21972,#21973,#21974,#21975,#21976));
#5449=EDGE_LOOP('',(#21977,#21978,#21979,#21980,#21981,#21982,#21983));
#5450=EDGE_LOOP('',(#21984,#21985,#21986,#21987,#21988,#21989));
#5451=EDGE_LOOP('',(#21990,#21991,#21992,#21993));
#5452=EDGE_LOOP('',(#21994,#21995,#21996,#21997));
#5453=EDGE_LOOP('',(#21998,#21999,#22000,#22001));
#5454=EDGE_LOOP('',(#22002,#22003,#22004,#22005));
#5455=EDGE_LOOP('',(#22006,#22007,#22008,#22009));
#5456=EDGE_LOOP('',(#22010,#22011,#22012,#22013));
#5457=EDGE_LOOP('',(#22014,#22015,#22016,#22017));
#5458=EDGE_LOOP('',(#22018,#22019,#22020,#22021));
#5459=EDGE_LOOP('',(#22022,#22023,#22024,#22025));
#5460=EDGE_LOOP('',(#22026,#22027,#22028,#22029));
#5461=EDGE_LOOP('',(#22030,#22031,#22032,#22033));
#5462=EDGE_LOOP('',(#22034,#22035,#22036,#22037));
#5463=EDGE_LOOP('',(#22038,#22039,#22040,#22041));
#5464=EDGE_LOOP('',(#22042,#22043,#22044,#22045));
#5465=EDGE_LOOP('',(#22046,#22047,#22048,#22049));
#5466=EDGE_LOOP('',(#22050,#22051,#22052,#22053));
#5467=EDGE_LOOP('',(#22054,#22055,#22056,#22057));
#5468=EDGE_LOOP('',(#22058,#22059,#22060,#22061));
#5469=EDGE_LOOP('',(#22062,#22063,#22064,#22065));
#5470=EDGE_LOOP('',(#22066,#22067,#22068,#22069));
#5471=EDGE_LOOP('',(#22070,#22071,#22072,#22073));
#5472=EDGE_LOOP('',(#22074,#22075,#22076,#22077));
#5473=EDGE_LOOP('',(#22078,#22079,#22080,#22081));
#5474=EDGE_LOOP('',(#22082,#22083,#22084,#22085));
#5475=EDGE_LOOP('',(#22086,#22087,#22088,#22089));
#5476=EDGE_LOOP('',(#22090,#22091,#22092,#22093));
#5477=EDGE_LOOP('',(#22094,#22095,#22096,#22097));
#5478=EDGE_LOOP('',(#22098,#22099,#22100,#22101));
#5479=EDGE_LOOP('',(#22102,#22103,#22104,#22105));
#5480=EDGE_LOOP('',(#22106,#22107,#22108,#22109));
#5481=EDGE_LOOP('',(#22110,#22111,#22112,#22113));
#5482=EDGE_LOOP('',(#22114,#22115,#22116,#22117));
#5483=EDGE_LOOP('',(#22118,#22119,#22120,#22121));
#5484=EDGE_LOOP('',(#22122,#22123,#22124,#22125));
#5485=EDGE_LOOP('',(#22126,#22127,#22128,#22129));
#5486=EDGE_LOOP('',(#22130,#22131,#22132,#22133));
#5487=EDGE_LOOP('',(#22134,#22135,#22136,#22137));
#5488=EDGE_LOOP('',(#22138,#22139,#22140,#22141));
#5489=EDGE_LOOP('',(#22142,#22143,#22144,#22145));
#5490=EDGE_LOOP('',(#22146,#22147,#22148,#22149));
#5491=EDGE_LOOP('',(#22150,#22151,#22152,#22153));
#5492=EDGE_LOOP('',(#22154,#22155,#22156,#22157));
#5493=EDGE_LOOP('',(#22158,#22159,#22160,#22161));
#5494=EDGE_LOOP('',(#22162,#22163,#22164,#22165));
#5495=EDGE_LOOP('',(#22166,#22167,#22168,#22169));
#5496=EDGE_LOOP('',(#22170,#22171,#22172,#22173));
#5497=EDGE_LOOP('',(#22174,#22175,#22176,#22177));
#5498=EDGE_LOOP('',(#22178,#22179,#22180,#22181));
#5499=EDGE_LOOP('',(#22182,#22183,#22184,#22185));
#5500=EDGE_LOOP('',(#22186,#22187,#22188,#22189));
#5501=EDGE_LOOP('',(#22190,#22191,#22192,#22193));
#5502=EDGE_LOOP('',(#22194,#22195,#22196,#22197));
#5503=EDGE_LOOP('',(#22198,#22199,#22200,#22201));
#5504=EDGE_LOOP('',(#22202,#22203,#22204,#22205));
#5505=EDGE_LOOP('',(#22206,#22207,#22208,#22209));
#5506=EDGE_LOOP('',(#22210,#22211,#22212,#22213));
#5507=EDGE_LOOP('',(#22214,#22215,#22216,#22217));
#5508=EDGE_LOOP('',(#22218,#22219,#22220,#22221));
#5509=EDGE_LOOP('',(#22222,#22223,#22224,#22225));
#5510=EDGE_LOOP('',(#22226,#22227,#22228,#22229));
#5511=EDGE_LOOP('',(#22230,#22231,#22232,#22233));
#5512=EDGE_LOOP('',(#22234,#22235,#22236,#22237));
#5513=EDGE_LOOP('',(#22238,#22239,#22240,#22241));
#5514=EDGE_LOOP('',(#22242,#22243,#22244,#22245));
#5515=EDGE_LOOP('',(#22246,#22247,#22248,#22249));
#5516=EDGE_LOOP('',(#22250,#22251,#22252,#22253));
#5517=EDGE_LOOP('',(#22254,#22255,#22256,#22257));
#5518=EDGE_LOOP('',(#22258,#22259,#22260,#22261));
#5519=EDGE_LOOP('',(#22262,#22263,#22264,#22265));
#5520=EDGE_LOOP('',(#22266,#22267,#22268,#22269));
#5521=EDGE_LOOP('',(#22270,#22271,#22272,#22273));
#5522=EDGE_LOOP('',(#22274,#22275,#22276,#22277));
#5523=EDGE_LOOP('',(#22278,#22279,#22280,#22281));
#5524=EDGE_LOOP('',(#22282,#22283,#22284,#22285));
#5525=EDGE_LOOP('',(#22286,#22287,#22288,#22289));
#5526=EDGE_LOOP('',(#22290,#22291,#22292,#22293));
#5527=EDGE_LOOP('',(#22294,#22295,#22296,#22297));
#5528=EDGE_LOOP('',(#22298,#22299,#22300,#22301));
#5529=EDGE_LOOP('',(#22302,#22303,#22304,#22305));
#5530=EDGE_LOOP('',(#22306,#22307,#22308,#22309));
#5531=EDGE_LOOP('',(#22310,#22311,#22312,#22313));
#5532=EDGE_LOOP('',(#22314,#22315,#22316,#22317));
#5533=EDGE_LOOP('',(#22318,#22319,#22320,#22321));
#5534=EDGE_LOOP('',(#22322,#22323,#22324,#22325,#22326));
#5535=EDGE_LOOP('',(#22327,#22328,#22329,#22330,#22331));
#5536=EDGE_LOOP('',(#22332,#22333,#22334,#22335));
#5537=EDGE_LOOP('',(#22336,#22337,#22338,#22339));
#5538=EDGE_LOOP('',(#22340,#22341,#22342,#22343));
#5539=EDGE_LOOP('',(#22344,#22345,#22346,#22347));
#5540=EDGE_LOOP('',(#22348,#22349,#22350,#22351));
#5541=EDGE_LOOP('',(#22352,#22353,#22354,#22355,#22356));
#5542=EDGE_LOOP('',(#22357,#22358,#22359,#22360));
#5543=EDGE_LOOP('',(#22361,#22362,#22363,#22364));
#5544=EDGE_LOOP('',(#22365,#22366,#22367,#22368));
#5545=EDGE_LOOP('',(#22369,#22370,#22371,#22372));
#5546=EDGE_LOOP('',(#22373,#22374,#22375,#22376));
#5547=EDGE_LOOP('',(#22377,#22378,#22379,#22380));
#5548=EDGE_LOOP('',(#22381,#22382,#22383,#22384));
#5549=EDGE_LOOP('',(#22385,#22386,#22387,#22388));
#5550=EDGE_LOOP('',(#22389,#22390,#22391,#22392));
#5551=EDGE_LOOP('',(#22393,#22394,#22395,#22396));
#5552=EDGE_LOOP('',(#22397,#22398,#22399,#22400));
#5553=EDGE_LOOP('',(#22401,#22402,#22403,#22404));
#5554=EDGE_LOOP('',(#22405,#22406,#22407,#22408));
#5555=EDGE_LOOP('',(#22409,#22410,#22411,#22412));
#5556=EDGE_LOOP('',(#22413,#22414,#22415,#22416));
#5557=EDGE_LOOP('',(#22417,#22418,#22419,#22420));
#5558=EDGE_LOOP('',(#22421,#22422,#22423,#22424));
#5559=EDGE_LOOP('',(#22425,#22426,#22427,#22428));
#5560=EDGE_LOOP('',(#22429,#22430,#22431,#22432));
#5561=EDGE_LOOP('',(#22433,#22434,#22435,#22436,#22437,#22438));
#5562=EDGE_LOOP('',(#22439,#22440,#22441));
#5563=EDGE_LOOP('',(#22442,#22443,#22444,#22445,#22446,#22447));
#5564=EDGE_LOOP('',(#22448,#22449,#22450));
#5565=EDGE_LOOP('',(#22451,#22452,#22453,#22454));
#5566=EDGE_LOOP('',(#22455,#22456,#22457,#22458));
#5567=EDGE_LOOP('',(#22459,#22460,#22461,#22462));
#5568=EDGE_LOOP('',(#22463,#22464,#22465,#22466));
#5569=EDGE_LOOP('',(#22467,#22468,#22469,#22470));
#5570=EDGE_LOOP('',(#22471,#22472,#22473,#22474));
#5571=EDGE_LOOP('',(#22475,#22476,#22477,#22478));
#5572=EDGE_LOOP('',(#22479,#22480,#22481,#22482));
#5573=EDGE_LOOP('',(#22483,#22484,#22485,#22486));
#5574=EDGE_LOOP('',(#22487,#22488,#22489));
#5575=EDGE_LOOP('',(#22490,#22491,#22492,#22493,#22494,#22495));
#5576=EDGE_LOOP('',(#22496,#22497,#22498,#22499,#22500,#22501));
#5577=EDGE_LOOP('',(#22502,#22503,#22504));
#5578=EDGE_LOOP('',(#22505,#22506,#22507,#22508));
#5579=EDGE_LOOP('',(#22509,#22510,#22511,#22512));
#5580=EDGE_LOOP('',(#22513,#22514,#22515,#22516));
#5581=EDGE_LOOP('',(#22517,#22518,#22519,#22520));
#5582=EDGE_LOOP('',(#22521,#22522,#22523,#22524));
#5583=EDGE_LOOP('',(#22525,#22526,#22527,#22528));
#5584=EDGE_LOOP('',(#22529,#22530,#22531,#22532));
#5585=EDGE_LOOP('',(#22533,#22534,#22535,#22536));
#5586=EDGE_LOOP('',(#22537,#22538,#22539,#22540));
#5587=EDGE_LOOP('',(#22541,#22542,#22543,#22544));
#5588=EDGE_LOOP('',(#22545,#22546,#22547,#22548));
#5589=EDGE_LOOP('',(#22549,#22550,#22551,#22552));
#5590=EDGE_LOOP('',(#22553,#22554,#22555,#22556));
#5591=EDGE_LOOP('',(#22557,#22558,#22559,#22560));
#5592=EDGE_LOOP('',(#22561,#22562,#22563,#22564));
#5593=EDGE_LOOP('',(#22565,#22566,#22567,#22568));
#5594=EDGE_LOOP('',(#22569,#22570,#22571,#22572));
#5595=EDGE_LOOP('',(#22573,#22574,#22575,#22576));
#5596=EDGE_LOOP('',(#22577,#22578,#22579,#22580));
#5597=EDGE_LOOP('',(#22581,#22582,#22583,#22584));
#5598=EDGE_LOOP('',(#22585,#22586,#22587,#22588));
#5599=EDGE_LOOP('',(#22589,#22590,#22591,#22592));
#5600=EDGE_LOOP('',(#22593,#22594,#22595,#22596));
#5601=EDGE_LOOP('',(#22597,#22598,#22599,#22600));
#5602=EDGE_LOOP('',(#22601,#22602,#22603,#22604));
#5603=EDGE_LOOP('',(#22605,#22606,#22607,#22608));
#5604=EDGE_LOOP('',(#22609,#22610,#22611,#22612));
#5605=EDGE_LOOP('',(#22613,#22614,#22615,#22616));
#5606=EDGE_LOOP('',(#22617,#22618,#22619,#22620));
#5607=EDGE_LOOP('',(#22621,#22622,#22623,#22624));
#5608=EDGE_LOOP('',(#22625,#22626,#22627,#22628));
#5609=EDGE_LOOP('',(#22629,#22630,#22631,#22632));
#5610=EDGE_LOOP('',(#22633,#22634,#22635,#22636));
#5611=EDGE_LOOP('',(#22637,#22638,#22639,#22640));
#5612=EDGE_LOOP('',(#22641,#22642,#22643,#22644));
#5613=EDGE_LOOP('',(#22645,#22646,#22647,#22648));
#5614=EDGE_LOOP('',(#22649,#22650,#22651,#22652));
#5615=EDGE_LOOP('',(#22653,#22654,#22655,#22656));
#5616=EDGE_LOOP('',(#22657,#22658,#22659,#22660));
#5617=EDGE_LOOP('',(#22661,#22662,#22663,#22664));
#5618=EDGE_LOOP('',(#22665,#22666,#22667,#22668));
#5619=EDGE_LOOP('',(#22669,#22670,#22671,#22672));
#5620=EDGE_LOOP('',(#22673,#22674,#22675,#22676));
#5621=EDGE_LOOP('',(#22677,#22678,#22679,#22680));
#5622=EDGE_LOOP('',(#22681,#22682,#22683,#22684));
#5623=EDGE_LOOP('',(#22685,#22686,#22687,#22688));
#5624=EDGE_LOOP('',(#22689,#22690,#22691,#22692));
#5625=EDGE_LOOP('',(#22693,#22694,#22695,#22696));
#5626=EDGE_LOOP('',(#22697,#22698,#22699,#22700));
#5627=EDGE_LOOP('',(#22701,#22702,#22703,#22704));
#5628=EDGE_LOOP('',(#22705,#22706,#22707,#22708));
#5629=EDGE_LOOP('',(#22709,#22710,#22711,#22712));
#5630=EDGE_LOOP('',(#22713,#22714,#22715,#22716));
#5631=EDGE_LOOP('',(#22717,#22718,#22719,#22720));
#5632=EDGE_LOOP('',(#22721,#22722,#22723,#22724,#22725,#22726,#22727,#22728,
#22729,#22730,#22731,#22732,#22733,#22734,#22735,#22736,#22737,#22738,#22739,
#22740,#22741,#22742,#22743,#22744,#22745,#22746,#22747,#22748,#22749,#22750,
#22751,#22752,#22753,#22754,#22755,#22756,#22757,#22758,#22759,#22760));
#5633=EDGE_LOOP('',(#22761,#22762,#22763,#22764,#22765,#22766,#22767,#22768,
#22769,#22770,#22771,#22772,#22773,#22774,#22775,#22776,#22777,#22778,#22779,
#22780,#22781,#22782,#22783));
#5634=EDGE_LOOP('',(#22784,#22785,#22786,#22787));
#5635=EDGE_LOOP('',(#22788,#22789,#22790,#22791));
#5636=EDGE_LOOP('',(#22792,#22793,#22794,#22795));
#5637=EDGE_LOOP('',(#22796,#22797,#22798,#22799));
#5638=EDGE_LOOP('',(#22800,#22801,#22802,#22803));
#5639=EDGE_LOOP('',(#22804,#22805,#22806,#22807));
#5640=EDGE_LOOP('',(#22808,#22809,#22810,#22811));
#5641=EDGE_LOOP('',(#22812,#22813,#22814,#22815));
#5642=EDGE_LOOP('',(#22816,#22817,#22818,#22819));
#5643=EDGE_LOOP('',(#22820,#22821,#22822,#22823));
#5644=EDGE_LOOP('',(#22824,#22825,#22826,#22827));
#5645=EDGE_LOOP('',(#22828,#22829,#22830,#22831));
#5646=EDGE_LOOP('',(#22832,#22833,#22834,#22835));
#5647=EDGE_LOOP('',(#22836,#22837,#22838,#22839));
#5648=EDGE_LOOP('',(#22840,#22841,#22842,#22843));
#5649=EDGE_LOOP('',(#22844,#22845,#22846,#22847));
#5650=EDGE_LOOP('',(#22848,#22849,#22850,#22851));
#5651=EDGE_LOOP('',(#22852,#22853,#22854,#22855));
#5652=EDGE_LOOP('',(#22856,#22857,#22858,#22859,#22860,#22861));
#5653=EDGE_LOOP('',(#22862,#22863,#22864,#22865));
#5654=EDGE_LOOP('',(#22866,#22867,#22868,#22869,#22870));
#5655=EDGE_LOOP('',(#22871,#22872,#22873,#22874,#22875));
#5656=EDGE_LOOP('',(#22876,#22877,#22878,#22879));
#5657=EDGE_LOOP('',(#22880,#22881,#22882,#22883));
#5658=EDGE_LOOP('',(#22884,#22885,#22886,#22887));
#5659=EDGE_LOOP('',(#22888,#22889,#22890,#22891,#22892));
#5660=EDGE_LOOP('',(#22893,#22894,#22895,#22896,#22897));
#5661=EDGE_LOOP('',(#22898,#22899,#22900,#22901));
#5662=EDGE_LOOP('',(#22902,#22903,#22904,#22905));
#5663=EDGE_LOOP('',(#22906,#22907,#22908,#22909));
#5664=EDGE_LOOP('',(#22910,#22911,#22912,#22913));
#5665=EDGE_LOOP('',(#22914,#22915,#22916,#22917,#22918,#22919));
#5666=EDGE_LOOP('',(#22920,#22921,#22922,#22923));
#5667=EDGE_LOOP('',(#22924,#22925,#22926,#22927));
#5668=EDGE_LOOP('',(#22928,#22929,#22930,#22931));
#5669=EDGE_LOOP('',(#22932,#22933,#22934,#22935));
#5670=EDGE_LOOP('',(#22936,#22937,#22938,#22939));
#5671=EDGE_LOOP('',(#22940,#22941,#22942,#22943,#22944,#22945,#22946));
#5672=EDGE_LOOP('',(#22947,#22948,#22949,#22950,#22951,#22952,#22953));
#5673=EDGE_LOOP('',(#22954,#22955,#22956,#22957));
#5674=EDGE_LOOP('',(#22958,#22959,#22960,#22961,#22962));
#5675=EDGE_LOOP('',(#22963,#22964,#22965,#22966,#22967));
#5676=EDGE_LOOP('',(#22968,#22969,#22970,#22971,#22972,#22973,#22974));
#5677=EDGE_LOOP('',(#22975,#22976,#22977,#22978,#22979));
#5678=EDGE_LOOP('',(#22980,#22981,#22982,#22983,#22984));
#5679=EDGE_LOOP('',(#22985,#22986,#22987,#22988));
#5680=EDGE_LOOP('',(#22989,#22990,#22991,#22992));
#5681=EDGE_LOOP('',(#22993,#22994,#22995,#22996));
#5682=EDGE_LOOP('',(#22997,#22998,#22999,#23000));
#5683=EDGE_LOOP('',(#23001,#23002,#23003,#23004));
#5684=EDGE_LOOP('',(#23005,#23006,#23007,#23008));
#5685=EDGE_LOOP('',(#23009,#23010,#23011,#23012));
#5686=EDGE_LOOP('',(#23013,#23014,#23015,#23016));
#5687=EDGE_LOOP('',(#23017,#23018,#23019,#23020));
#5688=EDGE_LOOP('',(#23021,#23022,#23023,#23024));
#5689=EDGE_LOOP('',(#23025,#23026,#23027,#23028));
#5690=EDGE_LOOP('',(#23029,#23030,#23031,#23032));
#5691=EDGE_LOOP('',(#23033,#23034,#23035));
#5692=EDGE_LOOP('',(#23036,#23037,#23038,#23039));
#5693=EDGE_LOOP('',(#23040,#23041,#23042,#23043));
#5694=EDGE_LOOP('',(#23044,#23045,#23046,#23047));
#5695=EDGE_LOOP('',(#23048,#23049,#23050,#23051));
#5696=EDGE_LOOP('',(#23052,#23053,#23054,#23055,#23056));
#5697=EDGE_LOOP('',(#23057,#23058,#23059,#23060,#23061));
#5698=EDGE_LOOP('',(#23062,#23063,#23064,#23065));
#5699=EDGE_LOOP('',(#23066,#23067,#23068,#23069));
#5700=EDGE_LOOP('',(#23070,#23071,#23072,#23073,#23074));
#5701=EDGE_LOOP('',(#23075,#23076,#23077,#23078,#23079));
#5702=EDGE_LOOP('',(#23080,#23081,#23082,#23083,#23084));
#5703=EDGE_LOOP('',(#23085,#23086,#23087,#23088));
#5704=EDGE_LOOP('',(#23089,#23090,#23091,#23092));
#5705=EDGE_LOOP('',(#23093,#23094,#23095,#23096,#23097));
#5706=EDGE_LOOP('',(#23098,#23099,#23100,#23101,#23102));
#5707=EDGE_LOOP('',(#23103,#23104,#23105,#23106,#23107));
#5708=EDGE_LOOP('',(#23108,#23109,#23110,#23111));
#5709=EDGE_LOOP('',(#23112,#23113,#23114,#23115));
#5710=EDGE_LOOP('',(#23116,#23117,#23118,#23119,#23120,#23121,#23122));
#5711=EDGE_LOOP('',(#23123,#23124,#23125,#23126,#23127,#23128,#23129,#23130,
#23131,#23132,#23133,#23134,#23135,#23136));
#5712=EDGE_LOOP('',(#23137,#23138,#23139,#23140,#23141,#23142,#23143,#23144,
#23145,#23146,#23147,#23148,#23149,#23150));
#5713=EDGE_LOOP('',(#23151,#23152,#23153,#23154,#23155,#23156,#23157,#23158,
#23159,#23160,#23161,#23162,#23163,#23164));
#5714=EDGE_LOOP('',(#23165,#23166,#23167,#23168));
#5715=EDGE_LOOP('',(#23169,#23170,#23171,#23172));
#5716=EDGE_LOOP('',(#23173,#23174,#23175,#23176));
#5717=EDGE_LOOP('',(#23177,#23178,#23179,#23180));
#5718=EDGE_LOOP('',(#23181,#23182,#23183,#23184));
#5719=EDGE_LOOP('',(#23185,#23186,#23187,#23188));
#5720=EDGE_LOOP('',(#23189,#23190,#23191,#23192));
#5721=EDGE_LOOP('',(#23193,#23194,#23195,#23196,#23197,#23198,#23199,#23200,
#23201,#23202,#23203,#23204,#23205,#23206,#23207,#23208,#23209,#23210,#23211,
#23212,#23213,#23214,#23215));
#5722=EDGE_LOOP('',(#23216,#23217,#23218,#23219,#23220,#23221,#23222));
#5723=EDGE_LOOP('',(#23223,#23224,#23225,#23226,#23227,#23228,#23229,#23230,
#23231,#23232,#23233));
#5724=EDGE_LOOP('',(#23234,#23235,#23236,#23237,#23238,#23239,#23240,#23241,
#23242));
#5725=EDGE_LOOP('',(#23243,#23244,#23245,#23246,#23247,#23248,#23249,#23250,
#23251));
#5726=EDGE_LOOP('',(#23252,#23253,#23254,#23255,#23256,#23257,#23258));
#5727=EDGE_LOOP('',(#23259,#23260,#23261,#23262,#23263,#23264,#23265,#23266,
#23267,#23268,#23269));
#5728=EDGE_LOOP('',(#23270,#23271,#23272,#23273,#23274,#23275,#23276,#23277,
#23278));
#5729=EDGE_LOOP('',(#23279,#23280,#23281,#23282,#23283,#23284,#23285,#23286,
#23287));
#5730=EDGE_LOOP('',(#23288,#23289,#23290,#23291,#23292,#23293,#23294));
#5731=EDGE_LOOP('',(#23295,#23296,#23297,#23298));
#5732=EDGE_LOOP('',(#23299,#23300,#23301,#23302));
#5733=EDGE_LOOP('',(#23303,#23304,#23305,#23306));
#5734=EDGE_LOOP('',(#23307,#23308,#23309,#23310));
#5735=EDGE_LOOP('',(#23311,#23312,#23313,#23314));
#5736=EDGE_LOOP('',(#23315,#23316,#23317,#23318));
#5737=EDGE_LOOP('',(#23319,#23320,#23321,#23322));
#5738=EDGE_LOOP('',(#23323,#23324,#23325,#23326));
#5739=EDGE_LOOP('',(#23327,#23328,#23329,#23330));
#5740=EDGE_LOOP('',(#23331,#23332,#23333,#23334));
#5741=EDGE_LOOP('',(#23335,#23336,#23337,#23338));
#5742=EDGE_LOOP('',(#23339,#23340,#23341,#23342));
#5743=EDGE_LOOP('',(#23343,#23344,#23345,#23346));
#5744=EDGE_LOOP('',(#23347,#23348,#23349,#23350));
#5745=EDGE_LOOP('',(#23351,#23352,#23353,#23354));
#5746=EDGE_LOOP('',(#23355,#23356,#23357,#23358));
#5747=EDGE_LOOP('',(#23359,#23360,#23361,#23362));
#5748=EDGE_LOOP('',(#23363,#23364,#23365,#23366));
#5749=EDGE_LOOP('',(#23367,#23368,#23369,#23370));
#5750=EDGE_LOOP('',(#23371,#23372,#23373,#23374));
#5751=EDGE_LOOP('',(#23375,#23376,#23377,#23378));
#5752=EDGE_LOOP('',(#23379,#23380,#23381,#23382));
#5753=EDGE_LOOP('',(#23383,#23384,#23385,#23386));
#5754=EDGE_LOOP('',(#23387,#23388,#23389,#23390));
#5755=EDGE_LOOP('',(#23391,#23392,#23393,#23394));
#5756=EDGE_LOOP('',(#23395,#23396,#23397,#23398));
#5757=EDGE_LOOP('',(#23399,#23400,#23401,#23402));
#5758=EDGE_LOOP('',(#23403,#23404,#23405,#23406));
#5759=EDGE_LOOP('',(#23407,#23408,#23409,#23410));
#5760=EDGE_LOOP('',(#23411,#23412,#23413,#23414));
#5761=EDGE_LOOP('',(#23415,#23416,#23417,#23418));
#5762=EDGE_LOOP('',(#23419,#23420,#23421,#23422));
#5763=EDGE_LOOP('',(#23423,#23424,#23425,#23426));
#5764=EDGE_LOOP('',(#23427,#23428,#23429,#23430));
#5765=EDGE_LOOP('',(#23431,#23432,#23433,#23434));
#5766=EDGE_LOOP('',(#23435,#23436,#23437,#23438));
#5767=EDGE_LOOP('',(#23439,#23440,#23441,#23442));
#5768=EDGE_LOOP('',(#23443,#23444,#23445,#23446));
#5769=EDGE_LOOP('',(#23447,#23448,#23449,#23450));
#5770=EDGE_LOOP('',(#23451,#23452,#23453,#23454));
#5771=EDGE_LOOP('',(#23455,#23456,#23457,#23458));
#5772=EDGE_LOOP('',(#23459,#23460,#23461,#23462));
#5773=EDGE_LOOP('',(#23463,#23464,#23465,#23466));
#5774=EDGE_LOOP('',(#23467,#23468,#23469,#23470));
#5775=EDGE_LOOP('',(#23471,#23472,#23473,#23474));
#5776=EDGE_LOOP('',(#23475,#23476,#23477,#23478));
#5777=EDGE_LOOP('',(#23479,#23480,#23481,#23482));
#5778=EDGE_LOOP('',(#23483,#23484,#23485,#23486));
#5779=EDGE_LOOP('',(#23487,#23488,#23489,#23490));
#5780=EDGE_LOOP('',(#23491,#23492,#23493,#23494));
#5781=EDGE_LOOP('',(#23495,#23496,#23497,#23498));
#5782=EDGE_LOOP('',(#23499,#23500,#23501,#23502));
#5783=EDGE_LOOP('',(#23503,#23504,#23505,#23506));
#5784=EDGE_LOOP('',(#23507,#23508,#23509,#23510));
#5785=EDGE_LOOP('',(#23511,#23512,#23513,#23514));
#5786=EDGE_LOOP('',(#23515,#23516,#23517,#23518));
#5787=EDGE_LOOP('',(#23519,#23520,#23521,#23522));
#5788=EDGE_LOOP('',(#23523,#23524,#23525,#23526));
#5789=EDGE_LOOP('',(#23527,#23528,#23529,#23530));
#5790=EDGE_LOOP('',(#23531,#23532,#23533,#23534));
#5791=EDGE_LOOP('',(#23535,#23536,#23537,#23538));
#5792=EDGE_LOOP('',(#23539,#23540,#23541,#23542));
#5793=EDGE_LOOP('',(#23543,#23544,#23545,#23546));
#5794=EDGE_LOOP('',(#23547,#23548,#23549,#23550));
#5795=EDGE_LOOP('',(#23551,#23552,#23553,#23554));
#5796=EDGE_LOOP('',(#23555,#23556,#23557,#23558));
#5797=EDGE_LOOP('',(#23559,#23560,#23561,#23562));
#5798=EDGE_LOOP('',(#23563,#23564,#23565,#23566));
#5799=EDGE_LOOP('',(#23567,#23568,#23569,#23570));
#5800=EDGE_LOOP('',(#23571,#23572,#23573,#23574));
#5801=EDGE_LOOP('',(#23575,#23576,#23577,#23578));
#5802=EDGE_LOOP('',(#23579,#23580,#23581,#23582));
#5803=EDGE_LOOP('',(#23583,#23584,#23585,#23586));
#5804=EDGE_LOOP('',(#23587,#23588,#23589,#23590));
#5805=EDGE_LOOP('',(#23591,#23592,#23593,#23594));
#5806=EDGE_LOOP('',(#23595,#23596,#23597,#23598));
#5807=EDGE_LOOP('',(#23599,#23600,#23601,#23602));
#5808=EDGE_LOOP('',(#23603,#23604,#23605,#23606));
#5809=EDGE_LOOP('',(#23607,#23608,#23609,#23610));
#5810=EDGE_LOOP('',(#23611,#23612,#23613,#23614));
#5811=EDGE_LOOP('',(#23615,#23616,#23617,#23618));
#5812=EDGE_LOOP('',(#23619,#23620,#23621,#23622));
#5813=EDGE_LOOP('',(#23623,#23624,#23625,#23626));
#5814=EDGE_LOOP('',(#23627,#23628,#23629,#23630));
#5815=EDGE_LOOP('',(#23631,#23632,#23633,#23634));
#5816=EDGE_LOOP('',(#23635,#23636,#23637,#23638));
#5817=EDGE_LOOP('',(#23639,#23640,#23641,#23642));
#5818=EDGE_LOOP('',(#23643,#23644,#23645,#23646));
#5819=EDGE_LOOP('',(#23647,#23648,#23649,#23650));
#5820=EDGE_LOOP('',(#23651,#23652,#23653,#23654));
#5821=EDGE_LOOP('',(#23655,#23656,#23657,#23658));
#5822=EDGE_LOOP('',(#23659,#23660,#23661,#23662));
#5823=EDGE_LOOP('',(#23663,#23664,#23665,#23666));
#5824=EDGE_LOOP('',(#23667,#23668,#23669,#23670));
#5825=EDGE_LOOP('',(#23671,#23672,#23673,#23674));
#5826=EDGE_LOOP('',(#23675,#23676,#23677,#23678));
#5827=EDGE_LOOP('',(#23679,#23680,#23681,#23682));
#5828=EDGE_LOOP('',(#23683,#23684,#23685,#23686));
#5829=EDGE_LOOP('',(#23687,#23688,#23689,#23690));
#5830=EDGE_LOOP('',(#23691,#23692,#23693,#23694));
#5831=EDGE_LOOP('',(#23695,#23696,#23697,#23698));
#5832=EDGE_LOOP('',(#23699,#23700,#23701,#23702));
#5833=EDGE_LOOP('',(#23703,#23704,#23705,#23706));
#5834=EDGE_LOOP('',(#23707,#23708,#23709,#23710));
#5835=EDGE_LOOP('',(#23711,#23712,#23713,#23714));
#5836=EDGE_LOOP('',(#23715,#23716,#23717,#23718));
#5837=EDGE_LOOP('',(#23719,#23720,#23721,#23722));
#5838=EDGE_LOOP('',(#23723,#23724,#23725,#23726));
#5839=EDGE_LOOP('',(#23727,#23728,#23729,#23730,#23731,#23732,#23733,#23734,
#23735,#23736));
#5840=EDGE_LOOP('',(#23737,#23738,#23739,#23740,#23741,#23742,#23743,#23744,
#23745));
#5841=EDGE_LOOP('',(#23746));
#5842=EDGE_LOOP('',(#23747));
#5843=EDGE_LOOP('',(#23748,#23749,#23750,#23751,#23752,#23753,#23754,#23755,
#23756,#23757));
#5844=EDGE_LOOP('',(#23758));
#5845=EDGE_LOOP('',(#23759));
#5846=EDGE_LOOP('',(#23760,#23761,#23762,#23763,#23764,#23765,#23766,#23767,
#23768));
#5847=EDGE_LOOP('',(#23769,#23770,#23771,#23772));
#5848=EDGE_LOOP('',(#23773,#23774,#23775,#23776));
#5849=EDGE_LOOP('',(#23777,#23778,#23779,#23780));
#5850=EDGE_LOOP('',(#23781,#23782,#23783,#23784));
#5851=EDGE_LOOP('',(#23785,#23786,#23787,#23788));
#5852=EDGE_LOOP('',(#23789,#23790,#23791,#23792));
#5853=EDGE_LOOP('',(#23793,#23794,#23795,#23796));
#5854=EDGE_LOOP('',(#23797,#23798,#23799,#23800));
#5855=EDGE_LOOP('',(#23801,#23802,#23803,#23804));
#5856=EDGE_LOOP('',(#23805,#23806,#23807,#23808));
#5857=EDGE_LOOP('',(#23809,#23810,#23811,#23812));
#5858=EDGE_LOOP('',(#23813,#23814,#23815,#23816));
#5859=EDGE_LOOP('',(#23817,#23818,#23819,#23820));
#5860=EDGE_LOOP('',(#23821,#23822,#23823,#23824));
#5861=EDGE_LOOP('',(#23825,#23826,#23827,#23828));
#5862=EDGE_LOOP('',(#23829,#23830,#23831,#23832));
#5863=EDGE_LOOP('',(#23833,#23834,#23835,#23836));
#5864=EDGE_LOOP('',(#23837,#23838,#23839,#23840));
#5865=EDGE_LOOP('',(#23841,#23842,#23843,#23844));
#5866=EDGE_LOOP('',(#23845,#23846,#23847,#23848));
#5867=EDGE_LOOP('',(#23849,#23850,#23851,#23852));
#5868=EDGE_LOOP('',(#23853,#23854,#23855,#23856));
#5869=EDGE_LOOP('',(#23857,#23858,#23859,#23860));
#5870=EDGE_LOOP('',(#23861,#23862,#23863,#23864));
#5871=EDGE_LOOP('',(#23865,#23866,#23867,#23868));
#5872=EDGE_LOOP('',(#23869,#23870,#23871,#23872));
#5873=EDGE_LOOP('',(#23873,#23874,#23875,#23876));
#5874=EDGE_LOOP('',(#23877,#23878,#23879,#23880));
#5875=EDGE_LOOP('',(#23881,#23882,#23883,#23884));
#5876=EDGE_LOOP('',(#23885,#23886,#23887,#23888));
#5877=EDGE_LOOP('',(#23889,#23890,#23891,#23892));
#5878=EDGE_LOOP('',(#23893,#23894,#23895,#23896));
#5879=EDGE_LOOP('',(#23897,#23898,#23899,#23900));
#5880=EDGE_LOOP('',(#23901,#23902,#23903,#23904));
#5881=EDGE_LOOP('',(#23905,#23906,#23907,#23908));
#5882=EDGE_LOOP('',(#23909,#23910,#23911,#23912));
#5883=EDGE_LOOP('',(#23913,#23914,#23915,#23916));
#5884=EDGE_LOOP('',(#23917,#23918,#23919,#23920));
#5885=EDGE_LOOP('',(#23921,#23922,#23923,#23924));
#5886=EDGE_LOOP('',(#23925,#23926,#23927,#23928));
#5887=EDGE_LOOP('',(#23929,#23930,#23931,#23932));
#5888=EDGE_LOOP('',(#23933,#23934,#23935,#23936));
#5889=EDGE_LOOP('',(#23937,#23938,#23939));
#5890=EDGE_LOOP('',(#23940,#23941,#23942,#23943));
#5891=EDGE_LOOP('',(#23944,#23945,#23946,#23947));
#5892=EDGE_LOOP('',(#23948,#23949,#23950,#23951));
#5893=EDGE_LOOP('',(#23952,#23953,#23954));
#5894=EDGE_LOOP('',(#23955,#23956,#23957));
#5895=EDGE_LOOP('',(#23958,#23959,#23960,#23961));
#5896=EDGE_LOOP('',(#23962,#23963,#23964,#23965));
#5897=EDGE_LOOP('',(#23966,#23967,#23968,#23969));
#5898=EDGE_LOOP('',(#23970,#23971,#23972));
#5899=EDGE_LOOP('',(#23973,#23974,#23975,#23976,#23977));
#5900=EDGE_LOOP('',(#23978,#23979,#23980,#23981));
#5901=EDGE_LOOP('',(#23982,#23983,#23984,#23985,#23986));
#5902=EDGE_LOOP('',(#23987,#23988,#23989,#23990,#23991,#23992,#23993,#23994,
#23995,#23996,#23997,#23998,#23999,#24000,#24001,#24002));
#5903=EDGE_LOOP('',(#24003,#24004,#24005,#24006,#24007,#24008));
#5904=EDGE_LOOP('',(#24009,#24010,#24011,#24012,#24013,#24014,#24015));
#5905=EDGE_LOOP('',(#24016,#24017,#24018,#24019,#24020,#24021,#24022));
#5906=EDGE_LOOP('',(#24023,#24024,#24025,#24026,#24027,#24028,#24029));
#5907=EDGE_LOOP('',(#24030,#24031,#24032,#24033,#24034,#24035,#24036,#24037,
#24038,#24039));
#5908=EDGE_LOOP('',(#24040,#24041,#24042,#24043,#24044,#24045,#24046));
#5909=EDGE_LOOP('',(#24047,#24048,#24049,#24050));
#5910=EDGE_LOOP('',(#24051,#24052,#24053,#24054));
#5911=EDGE_LOOP('',(#24055,#24056,#24057,#24058,#24059,#24060,#24061,#24062));
#5912=EDGE_LOOP('',(#24063,#24064,#24065,#24066,#24067));
#5913=EDGE_LOOP('',(#24068,#24069,#24070,#24071,#24072,#24073,#24074,#24075,
#24076,#24077,#24078,#24079,#24080,#24081,#24082,#24083,#24084,#24085,#24086,
#24087));
#5914=EDGE_LOOP('',(#24088,#24089,#24090,#24091));
#5915=EDGE_LOOP('',(#24092,#24093,#24094,#24095));
#5916=EDGE_LOOP('',(#24096,#24097,#24098,#24099));
#5917=EDGE_LOOP('',(#24100,#24101,#24102,#24103,#24104,#24105,#24106,#24107,
#24108,#24109));
#5918=EDGE_LOOP('',(#24110,#24111,#24112,#24113));
#5919=EDGE_LOOP('',(#24114,#24115,#24116,#24117));
#5920=EDGE_LOOP('',(#24118,#24119,#24120,#24121));
#5921=EDGE_LOOP('',(#24122,#24123,#24124,#24125,#24126,#24127,#24128,#24129,
#24130,#24131,#24132,#24133,#24134,#24135,#24136,#24137,#24138,#24139,#24140,
#24141));
#5922=EDGE_LOOP('',(#24142,#24143,#24144,#24145));
#5923=EDGE_LOOP('',(#24146,#24147,#24148,#24149));
#5924=EDGE_LOOP('',(#24150,#24151,#24152,#24153));
#5925=EDGE_LOOP('',(#24154,#24155,#24156,#24157,#24158,#24159,#24160,#24161,
#24162,#24163));
#5926=EDGE_LOOP('',(#24164,#24165,#24166,#24167));
#5927=EDGE_LOOP('',(#24168,#24169,#24170,#24171));
#5928=EDGE_LOOP('',(#24172,#24173,#24174,#24175));
#5929=EDGE_LOOP('',(#24176,#24177,#24178,#24179,#24180,#24181));
#5930=EDGE_LOOP('',(#24182,#24183,#24184,#24185,#24186));
#5931=EDGE_LOOP('',(#24187,#24188,#24189,#24190,#24191,#24192,#24193));
#5932=EDGE_LOOP('',(#24194,#24195,#24196,#24197));
#5933=EDGE_LOOP('',(#24198,#24199,#24200,#24201,#24202,#24203,#24204));
#5934=EDGE_LOOP('',(#24205,#24206,#24207,#24208,#24209));
#5935=EDGE_LOOP('',(#24210,#24211,#24212,#24213,#24214));
#5936=EDGE_LOOP('',(#24215,#24216,#24217,#24218,#24219));
#5937=EDGE_LOOP('',(#24220,#24221,#24222,#24223));
#5938=EDGE_LOOP('',(#24224,#24225,#24226,#24227,#24228));
#5939=EDGE_LOOP('',(#24229,#24230,#24231,#24232));
#5940=EDGE_LOOP('',(#24233,#24234,#24235,#24236,#24237));
#5941=EDGE_LOOP('',(#24238,#24239,#24240,#24241));
#5942=EDGE_LOOP('',(#24242,#24243,#24244,#24245));
#5943=EDGE_LOOP('',(#24246,#24247,#24248,#24249,#24250));
#5944=EDGE_LOOP('',(#24251,#24252,#24253,#24254));
#5945=EDGE_LOOP('',(#24255,#24256,#24257,#24258,#24259));
#5946=EDGE_LOOP('',(#24260,#24261,#24262,#24263));
#5947=EDGE_LOOP('',(#24264,#24265,#24266,#24267));
#5948=EDGE_LOOP('',(#24268,#24269,#24270,#24271,#24272));
#5949=EDGE_LOOP('',(#24273,#24274,#24275,#24276,#24277));
#5950=EDGE_LOOP('',(#24278,#24279,#24280,#24281));
#5951=EDGE_LOOP('',(#24282,#24283,#24284,#24285));
#5952=EDGE_LOOP('',(#24286,#24287,#24288,#24289,#24290,#24291,#24292,#24293,
#24294,#24295));
#5953=EDGE_LOOP('',(#24296,#24297,#24298,#24299));
#5954=EDGE_LOOP('',(#24300,#24301,#24302,#24303));
#5955=EDGE_LOOP('',(#24304,#24305,#24306,#24307));
#5956=EDGE_LOOP('',(#24308,#24309,#24310,#24311));
#5957=EDGE_LOOP('',(#24312,#24313,#24314,#24315));
#5958=EDGE_LOOP('',(#24316,#24317,#24318,#24319));
#5959=EDGE_LOOP('',(#24320,#24321,#24322,#24323));
#5960=EDGE_LOOP('',(#24324,#24325,#24326,#24327));
#5961=EDGE_LOOP('',(#24328,#24329,#24330,#24331));
#5962=EDGE_LOOP('',(#24332,#24333,#24334,#24335));
#5963=EDGE_LOOP('',(#24336,#24337,#24338,#24339));
#5964=EDGE_LOOP('',(#24340,#24341,#24342,#24343,#24344));
#5965=EDGE_LOOP('',(#24345,#24346,#24347,#24348,#24349));
#5966=EDGE_LOOP('',(#24350,#24351,#24352,#24353));
#5967=EDGE_LOOP('',(#24354,#24355,#24356,#24357));
#5968=EDGE_LOOP('',(#24358,#24359,#24360,#24361,#24362,#24363,#24364,#24365,
#24366,#24367,#24368));
#5969=EDGE_LOOP('',(#24369,#24370,#24371,#24372,#24373));
#5970=EDGE_LOOP('',(#24374,#24375,#24376,#24377,#24378,#24379));
#5971=EDGE_LOOP('',(#24380,#24381,#24382,#24383,#24384));
#5972=EDGE_LOOP('',(#24385,#24386,#24387,#24388,#24389,#24390,#24391,#24392));
#5973=EDGE_LOOP('',(#24393,#24394,#24395,#24396));
#5974=EDGE_LOOP('',(#24397,#24398,#24399,#24400,#24401,#24402,#24403,#24404));
#5975=EDGE_LOOP('',(#24405,#24406,#24407,#24408,#24409));
#5976=EDGE_LOOP('',(#24410,#24411,#24412,#24413,#24414,#24415));
#5977=EDGE_LOOP('',(#24416,#24417,#24418,#24419,#24420,#24421));
#5978=EDGE_LOOP('',(#24422,#24423,#24424,#24425,#24426));
#5979=EDGE_LOOP('',(#24427,#24428,#24429,#24430,#24431,#24432));
#5980=EDGE_LOOP('',(#24433,#24434,#24435,#24436,#24437));
#5981=EDGE_LOOP('',(#24438,#24439,#24440,#24441,#24442,#24443,#24444,#24445));
#5982=EDGE_LOOP('',(#24446,#24447,#24448,#24449));
#5983=EDGE_LOOP('',(#24450,#24451,#24452,#24453,#24454,#24455,#24456,#24457));
#5984=EDGE_LOOP('',(#24458,#24459,#24460,#24461));
#5985=EDGE_LOOP('',(#24462,#24463,#24464,#24465));
#5986=EDGE_LOOP('',(#24466,#24467,#24468,#24469));
#5987=EDGE_LOOP('',(#24470,#24471,#24472,#24473));
#5988=EDGE_LOOP('',(#24474,#24475,#24476,#24477,#24478,#24479,#24480,#24481,
#24482,#24483,#24484,#24485));
#5989=EDGE_LOOP('',(#24486,#24487,#24488,#24489));
#5990=EDGE_LOOP('',(#24490,#24491,#24492,#24493,#24494,#24495,#24496,#24497,
#24498,#24499,#24500,#24501));
#5991=EDGE_LOOP('',(#24502,#24503,#24504));
#5992=EDGE_LOOP('',(#24505,#24506,#24507));
#5993=EDGE_LOOP('',(#24508,#24509,#24510,#24511,#24512));
#5994=EDGE_LOOP('',(#24513,#24514,#24515,#24516,#24517,#24518,#24519,#24520));
#5995=EDGE_LOOP('',(#24521,#24522,#24523,#24524));
#5996=EDGE_LOOP('',(#24525,#24526,#24527,#24528,#24529,#24530));
#5997=EDGE_LOOP('',(#24531,#24532,#24533,#24534,#24535,#24536));
#5998=EDGE_LOOP('',(#24537,#24538,#24539,#24540,#24541,#24542));
#5999=EDGE_LOOP('',(#24543,#24544,#24545,#24546));
#6000=EDGE_LOOP('',(#24547,#24548,#24549,#24550,#24551,#24552,#24553,#24554,
#24555,#24556));
#6001=EDGE_LOOP('',(#24557,#24558,#24559,#24560,#24561,#24562,#24563,#24564,
#24565));
#6002=EDGE_LOOP('',(#24566));
#6003=EDGE_LOOP('',(#24567));
#6004=EDGE_LOOP('',(#24568,#24569,#24570,#24571,#24572,#24573));
#6005=EDGE_LOOP('',(#24574,#24575,#24576,#24577,#24578,#24579));
#6006=EDGE_LOOP('',(#24580,#24581,#24582,#24583,#24584,#24585));
#6007=EDGE_LOOP('',(#24586,#24587,#24588,#24589,#24590));
#6008=EDGE_LOOP('',(#24591,#24592,#24593,#24594));
#6009=EDGE_LOOP('',(#24595,#24596,#24597,#24598,#24599,#24600));
#6010=EDGE_LOOP('',(#24601,#24602,#24603,#24604));
#6011=EDGE_LOOP('',(#24605,#24606,#24607,#24608));
#6012=EDGE_LOOP('',(#24609,#24610,#24611,#24612));
#6013=EDGE_LOOP('',(#24613,#24614,#24615,#24616));
#6014=EDGE_LOOP('',(#24617,#24618,#24619,#24620));
#6015=EDGE_LOOP('',(#24621,#24622,#24623,#24624));
#6016=EDGE_LOOP('',(#24625,#24626,#24627,#24628));
#6017=EDGE_LOOP('',(#24629,#24630,#24631,#24632));
#6018=EDGE_LOOP('',(#24633,#24634,#24635,#24636));
#6019=EDGE_LOOP('',(#24637,#24638,#24639,#24640,#24641));
#6020=EDGE_LOOP('',(#24642,#24643,#24644,#24645,#24646,#24647));
#6021=EDGE_LOOP('',(#24648,#24649,#24650,#24651,#24652,#24653,#24654,#24655,
#24656,#24657,#24658,#24659,#24660,#24661,#24662,#24663,#24664,#24665,#24666,
#24667,#24668,#24669,#24670,#24671,#24672,#24673));
#6022=EDGE_LOOP('',(#24674,#24675,#24676,#24677));
#6023=EDGE_LOOP('',(#24678,#24679,#24680,#24681));
#6024=EDGE_LOOP('',(#24682,#24683,#24684,#24685));
#6025=EDGE_LOOP('',(#24686,#24687,#24688,#24689));
#6026=EDGE_LOOP('',(#24690,#24691,#24692,#24693));
#6027=EDGE_LOOP('',(#24694,#24695,#24696,#24697));
#6028=EDGE_LOOP('',(#24698,#24699,#24700,#24701,#24702,#24703));
#6029=EDGE_LOOP('',(#24704,#24705,#24706,#24707));
#6030=EDGE_LOOP('',(#24708,#24709,#24710,#24711));
#6031=EDGE_LOOP('',(#24712,#24713,#24714,#24715));
#6032=EDGE_LOOP('',(#24716,#24717,#24718,#24719));
#6033=EDGE_LOOP('',(#24720,#24721,#24722,#24723));
#6034=EDGE_LOOP('',(#24724,#24725,#24726,#24727,#24728));
#6035=EDGE_LOOP('',(#24729,#24730,#24731,#24732,#24733,#24734));
#6036=EDGE_LOOP('',(#24735,#24736,#24737,#24738,#24739,#24740,#24741,#24742,
#24743,#24744,#24745,#24746,#24747,#24748,#24749,#24750,#24751,#24752,#24753,
#24754,#24755,#24756,#24757,#24758,#24759,#24760));
#6037=EDGE_LOOP('',(#24761));
#6038=EDGE_LOOP('',(#24762));
#6039=EDGE_LOOP('',(#24763,#24764,#24765,#24766));
#6040=EDGE_LOOP('',(#24767,#24768,#24769,#24770));
#6041=EDGE_LOOP('',(#24771,#24772,#24773,#24774));
#6042=EDGE_LOOP('',(#24775,#24776,#24777,#24778));
#6043=EDGE_LOOP('',(#24779,#24780,#24781,#24782));
#6044=EDGE_LOOP('',(#24783,#24784,#24785,#24786));
#6045=EDGE_LOOP('',(#24787,#24788,#24789,#24790));
#6046=EDGE_LOOP('',(#24791,#24792,#24793,#24794));
#6047=EDGE_LOOP('',(#24795,#24796,#24797,#24798));
#6048=EDGE_LOOP('',(#24799,#24800,#24801,#24802));
#6049=EDGE_LOOP('',(#24803,#24804,#24805,#24806));
#6050=EDGE_LOOP('',(#24807));
#6051=EDGE_LOOP('',(#24808));
#6052=EDGE_LOOP('',(#24809,#24810,#24811,#24812));
#6053=EDGE_LOOP('',(#24813,#24814,#24815,#24816));
#6054=EDGE_LOOP('',(#24817,#24818,#24819,#24820));
#6055=EDGE_LOOP('',(#24821,#24822,#24823,#24824));
#6056=EDGE_LOOP('',(#24825,#24826,#24827,#24828));
#6057=EDGE_LOOP('',(#24829,#24830,#24831,#24832));
#6058=EDGE_LOOP('',(#24833,#24834,#24835,#24836));
#6059=EDGE_LOOP('',(#24837,#24838,#24839,#24840));
#6060=EDGE_LOOP('',(#24841,#24842,#24843,#24844));
#6061=EDGE_LOOP('',(#24845,#24846,#24847,#24848));
#6062=EDGE_LOOP('',(#24849,#24850,#24851,#24852));
#6063=EDGE_LOOP('',(#24853,#24854,#24855,#24856));
#6064=EDGE_LOOP('',(#24857,#24858,#24859,#24860));
#6065=EDGE_LOOP('',(#24861,#24862,#24863,#24864));
#6066=EDGE_LOOP('',(#24865,#24866,#24867,#24868));
#6067=EDGE_LOOP('',(#24869,#24870,#24871,#24872));
#6068=EDGE_LOOP('',(#24873,#24874,#24875,#24876));
#6069=EDGE_LOOP('',(#24877,#24878,#24879,#24880,#24881,#24882,#24883,#24884,
#24885));
#6070=EDGE_LOOP('',(#24886,#24887,#24888,#24889,#24890,#24891));
#6071=EDGE_LOOP('',(#24892));
#6072=EDGE_LOOP('',(#24893));
#6073=EDGE_LOOP('',(#24894));
#6074=EDGE_LOOP('',(#24895));
#6075=EDGE_LOOP('',(#24896,#24897,#24898,#24899));
#6076=EDGE_LOOP('',(#24900));
#6077=EDGE_LOOP('',(#24901,#24902,#24903,#24904,#24905));
#6078=EDGE_LOOP('',(#24906,#24907,#24908,#24909,#24910,#24911));
#6079=EDGE_LOOP('',(#24912,#24913,#24914,#24915,#24916));
#6080=EDGE_LOOP('',(#24917,#24918,#24919,#24920,#24921));
#6081=EDGE_LOOP('',(#24922,#24923,#24924,#24925,#24926,#24927));
#6082=EDGE_LOOP('',(#24928,#24929,#24930,#24931,#24932,#24933,#24934,#24935,
#24936,#24937));
#6083=EDGE_LOOP('',(#24938,#24939,#24940,#24941,#24942,#24943,#24944,#24945,
#24946,#24947));
#6084=EDGE_LOOP('',(#24948));
#6085=EDGE_LOOP('',(#24949,#24950,#24951,#24952));
#6086=EDGE_LOOP('',(#24953,#24954,#24955,#24956));
#6087=EDGE_LOOP('',(#24957,#24958,#24959,#24960));
#6088=EDGE_LOOP('',(#24961,#24962,#24963,#24964));
#6089=EDGE_LOOP('',(#24965,#24966,#24967,#24968));
#6090=EDGE_LOOP('',(#24969,#24970,#24971,#24972));
#6091=EDGE_LOOP('',(#24973,#24974,#24975,#24976));
#6092=EDGE_LOOP('',(#24977,#24978,#24979,#24980));
#6093=EDGE_LOOP('',(#24981,#24982,#24983,#24984));
#6094=EDGE_LOOP('',(#24985,#24986,#24987,#24988));
#6095=EDGE_LOOP('',(#24989,#24990,#24991,#24992));
#6096=EDGE_LOOP('',(#24993,#24994,#24995,#24996));
#6097=EDGE_LOOP('',(#24997,#24998,#24999,#25000,#25001,#25002,#25003,#25004,
#25005,#25006));
#6098=EDGE_LOOP('',(#25007,#25008,#25009));
#6099=EDGE_LOOP('',(#25010,#25011,#25012,#25013,#25014,#25015,#25016));
#6100=EDGE_LOOP('',(#25017,#25018,#25019,#25020,#25021,#25022,#25023));
#6101=EDGE_LOOP('',(#25024,#25025,#25026));
#6102=EDGE_LOOP('',(#25027,#25028,#25029,#25030,#25031,#25032,#25033));
#6103=EDGE_LOOP('',(#25034,#25035,#25036,#25037,#25038,#25039,#25040,#25041));
#6104=EDGE_LOOP('',(#25042,#25043,#25044,#25045));
#6105=EDGE_LOOP('',(#25046,#25047,#25048,#25049,#25050,#25051));
#6106=EDGE_LOOP('',(#25052,#25053,#25054));
#6107=EDGE_LOOP('',(#25055,#25056,#25057,#25058,#25059,#25060));
#6108=EDGE_LOOP('',(#25061,#25062,#25063));
#6109=EDGE_LOOP('',(#25064,#25065,#25066,#25067,#25068,#25069));
#6110=EDGE_LOOP('',(#25070,#25071,#25072,#25073,#25074,#25075,#25076,#25077));
#6111=EDGE_LOOP('',(#25078,#25079,#25080,#25081));
#6112=EDGE_LOOP('',(#25082,#25083,#25084,#25085,#25086,#25087));
#6113=EDGE_LOOP('',(#25088,#25089,#25090,#25091,#25092,#25093,#25094,#25095,
#25096,#25097,#25098));
#6114=EDGE_LOOP('',(#25099,#25100,#25101,#25102,#25103,#25104,#25105,#25106,
#25107));
#6115=EDGE_LOOP('',(#25108,#25109,#25110,#25111,#25112,#25113,#25114));
#6116=EDGE_LOOP('',(#25115,#25116,#25117,#25118,#25119,#25120,#25121,#25122,
#25123));
#6117=EDGE_LOOP('',(#25124,#25125,#25126,#25127));
#6118=EDGE_LOOP('',(#25128,#25129,#25130,#25131));
#6119=EDGE_LOOP('',(#25132,#25133,#25134,#25135));
#6120=EDGE_LOOP('',(#25136,#25137,#25138,#25139,#25140,#25141,#25142));
#6121=EDGE_LOOP('',(#25143,#25144,#25145,#25146,#25147,#25148,#25149));
#6122=EDGE_LOOP('',(#25150,#25151,#25152,#25153));
#6123=EDGE_LOOP('',(#25154,#25155,#25156,#25157));
#6124=EDGE_LOOP('',(#25158,#25159,#25160,#25161,#25162));
#6125=EDGE_LOOP('',(#25163,#25164,#25165,#25166));
#6126=EDGE_LOOP('',(#25167,#25168,#25169,#25170,#25171));
#6127=EDGE_LOOP('',(#25172,#25173,#25174,#25175));
#6128=EDGE_LOOP('',(#25176,#25177,#25178,#25179));
#6129=EDGE_LOOP('',(#25180,#25181,#25182,#25183));
#6130=EDGE_LOOP('',(#25184,#25185,#25186,#25187,#25188,#25189));
#6131=EDGE_LOOP('',(#25190,#25191,#25192,#25193));
#6132=EDGE_LOOP('',(#25194,#25195,#25196,#25197));
#6133=EDGE_LOOP('',(#25198,#25199,#25200,#25201));
#6134=EDGE_LOOP('',(#25202,#25203,#25204,#25205,#25206,#25207));
#6135=EDGE_LOOP('',(#25208,#25209,#25210,#25211,#25212));
#6136=EDGE_LOOP('',(#25213,#25214,#25215,#25216));
#6137=EDGE_LOOP('',(#25217,#25218,#25219,#25220));
#6138=EDGE_LOOP('',(#25221,#25222,#25223,#25224));
#6139=EDGE_LOOP('',(#25225,#25226,#25227,#25228));
#6140=EDGE_LOOP('',(#25229,#25230,#25231,#25232,#25233));
#6141=EDGE_LOOP('',(#25234,#25235,#25236,#25237));
#6142=EDGE_LOOP('',(#25238,#25239,#25240,#25241));
#6143=EDGE_LOOP('',(#25242,#25243,#25244,#25245));
#6144=EDGE_LOOP('',(#25246,#25247,#25248,#25249));
#6145=EDGE_LOOP('',(#25250,#25251,#25252,#25253));
#6146=EDGE_LOOP('',(#25254,#25255,#25256,#25257));
#6147=EDGE_LOOP('',(#25258,#25259,#25260,#25261));
#6148=EDGE_LOOP('',(#25262,#25263,#25264,#25265));
#6149=EDGE_LOOP('',(#25266,#25267,#25268,#25269));
#6150=EDGE_LOOP('',(#25270,#25271,#25272,#25273));
#6151=EDGE_LOOP('',(#25274,#25275,#25276,#25277));
#6152=EDGE_LOOP('',(#25278,#25279,#25280,#25281));
#6153=EDGE_LOOP('',(#25282,#25283,#25284,#25285));
#6154=EDGE_LOOP('',(#25286,#25287,#25288,#25289));
#6155=EDGE_LOOP('',(#25290,#25291,#25292,#25293));
#6156=EDGE_LOOP('',(#25294,#25295,#25296,#25297));
#6157=EDGE_LOOP('',(#25298,#25299,#25300,#25301));
#6158=EDGE_LOOP('',(#25302,#25303,#25304,#25305));
#6159=EDGE_LOOP('',(#25306,#25307,#25308,#25309));
#6160=EDGE_LOOP('',(#25310,#25311,#25312,#25313));
#6161=EDGE_LOOP('',(#25314,#25315,#25316,#25317));
#6162=EDGE_LOOP('',(#25318,#25319,#25320,#25321));
#6163=EDGE_LOOP('',(#25322,#25323,#25324,#25325));
#6164=EDGE_LOOP('',(#25326,#25327,#25328,#25329));
#6165=EDGE_LOOP('',(#25330,#25331,#25332,#25333));
#6166=EDGE_LOOP('',(#25334,#25335,#25336,#25337));
#6167=EDGE_LOOP('',(#25338,#25339,#25340,#25341));
#6168=EDGE_LOOP('',(#25342,#25343,#25344,#25345));
#6169=EDGE_LOOP('',(#25346,#25347,#25348,#25349,#25350,#25351,#25352,#25353,
#25354));
#6170=EDGE_LOOP('',(#25355,#25356,#25357,#25358,#25359,#25360,#25361,#25362,
#25363,#25364));
#6171=EDGE_LOOP('',(#25365,#25366,#25367,#25368,#25369,#25370,#25371,#25372,
#25373));
#6172=EDGE_LOOP('',(#25374,#25375,#25376,#25377,#25378,#25379,#25380,#25381,
#25382,#25383));
#6173=EDGE_LOOP('',(#25384,#25385,#25386,#25387));
#6174=EDGE_LOOP('',(#25388,#25389,#25390,#25391));
#6175=EDGE_LOOP('',(#25392,#25393,#25394,#25395));
#6176=EDGE_LOOP('',(#25396,#25397,#25398,#25399));
#6177=EDGE_LOOP('',(#25400,#25401,#25402,#25403,#25404,#25405));
#6178=EDGE_LOOP('',(#25406,#25407,#25408,#25409,#25410,#25411,#25412,#25413));
#6179=EDGE_LOOP('',(#25414,#25415,#25416,#25417,#25418,#25419,#25420,#25421));
#6180=EDGE_LOOP('',(#25422,#25423,#25424,#25425,#25426,#25427));
#6181=EDGE_LOOP('',(#25428,#25429,#25430,#25431,#25432,#25433));
#6182=EDGE_LOOP('',(#25434,#25435,#25436,#25437,#25438,#25439,#25440,#25441));
#6183=EDGE_LOOP('',(#25442,#25443,#25444,#25445,#25446,#25447,#25448,#25449));
#6184=EDGE_LOOP('',(#25450,#25451,#25452,#25453,#25454,#25455));
#6185=EDGE_LOOP('',(#25456,#25457,#25458,#25459,#25460));
#6186=EDGE_LOOP('',(#25461,#25462,#25463,#25464,#25465));
#6187=EDGE_LOOP('',(#25466,#25467,#25468,#25469,#25470,#25471,#25472,#25473,
#25474,#25475,#25476,#25477,#25478,#25479,#25480,#25481,#25482,#25483,#25484,
#25485,#25486,#25487,#25488,#25489,#25490,#25491,#25492,#25493,#25494,#25495,
#25496,#25497,#25498,#25499,#25500,#25501,#25502,#25503,#25504,#25505,#25506,
#25507,#25508,#25509,#25510,#25511,#25512,#25513,#25514,#25515,#25516,#25517,
#25518,#25519,#25520,#25521,#25522,#25523));
#6188=EDGE_LOOP('',(#25524,#25525,#25526,#25527,#25528,#25529,#25530,#25531,
#25532,#25533,#25534));
#6189=EDGE_LOOP('',(#25535,#25536,#25537,#25538,#25539));
#6190=EDGE_LOOP('',(#25540,#25541,#25542,#25543,#25544));
#6191=EDGE_LOOP('',(#25545,#25546,#25547,#25548));
#6192=EDGE_LOOP('',(#25549,#25550,#25551,#25552));
#6193=EDGE_LOOP('',(#25553,#25554,#25555));
#6194=EDGE_LOOP('',(#25556,#25557,#25558,#25559));
#6195=EDGE_LOOP('',(#25560,#25561,#25562));
#6196=EDGE_LOOP('',(#25563,#25564,#25565,#25566));
#6197=EDGE_LOOP('',(#25567,#25568,#25569,#25570));
#6198=EDGE_LOOP('',(#25571,#25572,#25573));
#6199=EDGE_LOOP('',(#25574,#25575,#25576,#25577,#25578,#25579,#25580,#25581,
#25582,#25583));
#6200=EDGE_LOOP('',(#25584,#25585,#25586,#25587));
#6201=EDGE_LOOP('',(#25588,#25589,#25590));
#6202=EDGE_LOOP('',(#25591,#25592,#25593,#25594));
#6203=EDGE_LOOP('',(#25595,#25596,#25597));
#6204=EDGE_LOOP('',(#25598,#25599,#25600,#25601));
#6205=EDGE_LOOP('',(#25602,#25603,#25604));
#6206=EDGE_LOOP('',(#25605,#25606,#25607,#25608));
#6207=EDGE_LOOP('',(#25609,#25610,#25611,#25612));
#6208=EDGE_LOOP('',(#25613,#25614,#25615,#25616));
#6209=EDGE_LOOP('',(#25617,#25618,#25619,#25620));
#6210=EDGE_LOOP('',(#25621,#25622,#25623,#25624));
#6211=EDGE_LOOP('',(#25625,#25626,#25627,#25628));
#6212=EDGE_LOOP('',(#25629,#25630,#25631,#25632));
#6213=EDGE_LOOP('',(#25633,#25634,#25635,#25636));
#6214=EDGE_LOOP('',(#25637,#25638,#25639,#25640));
#6215=EDGE_LOOP('',(#25641,#25642,#25643,#25644));
#6216=EDGE_LOOP('',(#25645,#25646,#25647,#25648));
#6217=EDGE_LOOP('',(#25649,#25650,#25651,#25652));
#6218=EDGE_LOOP('',(#25653,#25654,#25655,#25656,#25657,#25658));
#6219=EDGE_LOOP('',(#25659,#25660,#25661,#25662));
#6220=EDGE_LOOP('',(#25663,#25664,#25665,#25666));
#6221=EDGE_LOOP('',(#25667,#25668,#25669));
#6222=EDGE_LOOP('',(#25670,#25671,#25672,#25673));
#6223=EDGE_LOOP('',(#25674,#25675,#25676));
#6224=EDGE_LOOP('',(#25677,#25678,#25679,#25680));
#6225=EDGE_LOOP('',(#25681,#25682,#25683,#25684));
#6226=EDGE_LOOP('',(#25685,#25686,#25687));
#6227=EDGE_LOOP('',(#25688,#25689,#25690,#25691,#25692,#25693,#25694,#25695,
#25696,#25697));
#6228=EDGE_LOOP('',(#25698,#25699,#25700,#25701));
#6229=EDGE_LOOP('',(#25702,#25703,#25704));
#6230=EDGE_LOOP('',(#25705,#25706,#25707,#25708));
#6231=EDGE_LOOP('',(#25709,#25710,#25711));
#6232=EDGE_LOOP('',(#25712,#25713,#25714,#25715));
#6233=EDGE_LOOP('',(#25716,#25717,#25718));
#6234=EDGE_LOOP('',(#25719,#25720,#25721,#25722));
#6235=EDGE_LOOP('',(#25723,#25724,#25725,#25726));
#6236=EDGE_LOOP('',(#25727,#25728,#25729,#25730));
#6237=EDGE_LOOP('',(#25731,#25732,#25733,#25734));
#6238=EDGE_LOOP('',(#25735,#25736,#25737,#25738));
#6239=EDGE_LOOP('',(#25739,#25740,#25741,#25742));
#6240=EDGE_LOOP('',(#25743,#25744,#25745,#25746));
#6241=EDGE_LOOP('',(#25747,#25748,#25749,#25750,#25751,#25752));
#6242=EDGE_LOOP('',(#25753,#25754,#25755,#25756));
#6243=EDGE_LOOP('',(#25757,#25758,#25759,#25760));
#6244=EDGE_LOOP('',(#25761,#25762,#25763,#25764));
#6245=EDGE_LOOP('',(#25765,#25766,#25767,#25768));
#6246=EDGE_LOOP('',(#25769,#25770,#25771,#25772));
#6247=EDGE_LOOP('',(#25773,#25774,#25775,#25776));
#6248=EDGE_LOOP('',(#25777,#25778,#25779,#25780));
#6249=EDGE_LOOP('',(#25781,#25782,#25783,#25784));
#6250=EDGE_LOOP('',(#25785,#25786,#25787,#25788));
#6251=EDGE_LOOP('',(#25789,#25790,#25791));
#6252=EDGE_LOOP('',(#25792,#25793,#25794,#25795));
#6253=EDGE_LOOP('',(#25796,#25797,#25798));
#6254=EDGE_LOOP('',(#25799,#25800,#25801,#25802));
#6255=EDGE_LOOP('',(#25803,#25804,#25805,#25806));
#6256=EDGE_LOOP('',(#25807,#25808,#25809));
#6257=EDGE_LOOP('',(#25810,#25811,#25812,#25813,#25814,#25815,#25816,#25817,
#25818,#25819));
#6258=EDGE_LOOP('',(#25820,#25821,#25822,#25823));
#6259=EDGE_LOOP('',(#25824,#25825,#25826));
#6260=EDGE_LOOP('',(#25827,#25828,#25829,#25830));
#6261=EDGE_LOOP('',(#25831,#25832,#25833));
#6262=EDGE_LOOP('',(#25834,#25835,#25836,#25837));
#6263=EDGE_LOOP('',(#25838,#25839,#25840));
#6264=EDGE_LOOP('',(#25841,#25842,#25843,#25844));
#6265=EDGE_LOOP('',(#25845,#25846,#25847,#25848));
#6266=EDGE_LOOP('',(#25849,#25850,#25851,#25852));
#6267=EDGE_LOOP('',(#25853,#25854,#25855,#25856));
#6268=EDGE_LOOP('',(#25857,#25858,#25859,#25860));
#6269=EDGE_LOOP('',(#25861,#25862,#25863,#25864));
#6270=EDGE_LOOP('',(#25865,#25866,#25867,#25868));
#6271=EDGE_LOOP('',(#25869,#25870,#25871,#25872));
#6272=EDGE_LOOP('',(#25873,#25874,#25875,#25876));
#6273=EDGE_LOOP('',(#25877,#25878,#25879,#25880));
#6274=EDGE_LOOP('',(#25881,#25882,#25883,#25884));
#6275=EDGE_LOOP('',(#25885,#25886,#25887,#25888));
#6276=EDGE_LOOP('',(#25889,#25890,#25891,#25892,#25893,#25894));
#6277=EDGE_LOOP('',(#25895,#25896,#25897,#25898));
#6278=EDGE_LOOP('',(#25899,#25900,#25901,#25902));
#6279=EDGE_LOOP('',(#25903,#25904,#25905));
#6280=EDGE_LOOP('',(#25906,#25907,#25908,#25909));
#6281=EDGE_LOOP('',(#25910,#25911,#25912));
#6282=EDGE_LOOP('',(#25913,#25914,#25915,#25916,#25917,#25918,#25919,#25920,
#25921,#25922));
#6283=EDGE_LOOP('',(#25923,#25924,#25925,#25926));
#6284=EDGE_LOOP('',(#25927,#25928,#25929));
#6285=EDGE_LOOP('',(#25930,#25931,#25932,#25933));
#6286=EDGE_LOOP('',(#25934,#25935,#25936));
#6287=EDGE_LOOP('',(#25937,#25938,#25939,#25940));
#6288=EDGE_LOOP('',(#25941,#25942,#25943));
#6289=EDGE_LOOP('',(#25944,#25945,#25946));
#6290=EDGE_LOOP('',(#25947,#25948,#25949,#25950));
#6291=EDGE_LOOP('',(#25951,#25952,#25953,#25954));
#6292=EDGE_LOOP('',(#25955,#25956,#25957,#25958));
#6293=EDGE_LOOP('',(#25959,#25960,#25961,#25962));
#6294=EDGE_LOOP('',(#25963,#25964,#25965,#25966));
#6295=EDGE_LOOP('',(#25967,#25968,#25969,#25970));
#6296=EDGE_LOOP('',(#25971,#25972,#25973,#25974));
#6297=EDGE_LOOP('',(#25975,#25976,#25977,#25978));
#6298=EDGE_LOOP('',(#25979,#25980,#25981,#25982));
#6299=EDGE_LOOP('',(#25983,#25984,#25985,#25986));
#6300=EDGE_LOOP('',(#25987,#25988,#25989,#25990));
#6301=EDGE_LOOP('',(#25991,#25992,#25993,#25994));
#6302=EDGE_LOOP('',(#25995,#25996,#25997,#25998,#25999,#26000));
#6303=EDGE_LOOP('',(#26001,#26002,#26003,#26004));
#6304=EDGE_LOOP('',(#26005,#26006,#26007,#26008));
#6305=EDGE_LOOP('',(#26009,#26010,#26011,#26012));
#6306=EDGE_LOOP('',(#26013,#26014,#26015,#26016));
#6307=EDGE_LOOP('',(#26017,#26018,#26019,#26020,#26021,#26022));
#6308=EDGE_LOOP('',(#26023,#26024,#26025,#26026,#26027,#26028));
#6309=EDGE_LOOP('',(#26029,#26030,#26031,#26032,#26033,#26034));
#6310=EDGE_LOOP('',(#26035,#26036,#26037,#26038,#26039,#26040));
#6311=EDGE_LOOP('',(#26041,#26042,#26043,#26044,#26045,#26046));
#6312=EDGE_LOOP('',(#26047,#26048,#26049,#26050,#26051,#26052));
#6313=EDGE_LOOP('',(#26053,#26054));
#6314=EDGE_LOOP('',(#26055,#26056,#26057,#26058));
#6315=EDGE_LOOP('',(#26059,#26060,#26061,#26062));
#6316=EDGE_LOOP('',(#26063,#26064,#26065,#26066));
#6317=EDGE_LOOP('',(#26067,#26068));
#6318=EDGE_LOOP('',(#26069,#26070,#26071));
#6319=EDGE_LOOP('',(#26072,#26073,#26074,#26075));
#6320=EDGE_LOOP('',(#26076,#26077,#26078,#26079));
#6321=EDGE_LOOP('',(#26080,#26081,#26082,#26083,#26084,#26085,#26086,#26087,
#26088,#26089,#26090));
#6322=EDGE_LOOP('',(#26091,#26092,#26093,#26094,#26095,#26096,#26097,#26098,
#26099,#26100,#26101,#26102,#26103,#26104,#26105,#26106,#26107,#26108,#26109,
#26110,#26111,#26112,#26113,#26114,#26115,#26116));
#6323=EDGE_LOOP('',(#26117,#26118,#26119));
#6324=EDGE_LOOP('',(#26120,#26121,#26122,#26123));
#6325=EDGE_LOOP('',(#26124,#26125,#26126,#26127));
#6326=EDGE_LOOP('',(#26128,#26129,#26130,#26131,#26132));
#6327=EDGE_LOOP('',(#26133));
#6328=EDGE_LOOP('',(#26134,#26135,#26136,#26137));
#6329=EDGE_LOOP('',(#26138,#26139,#26140,#26141,#26142,#26143,#26144,#26145));
#6330=EDGE_LOOP('',(#26146));
#6331=EDGE_LOOP('',(#26147,#26148,#26149,#26150));
#6332=EDGE_LOOP('',(#26151,#26152,#26153,#26154));
#6333=EDGE_LOOP('',(#26155,#26156,#26157,#26158));
#6334=EDGE_LOOP('',(#26159,#26160,#26161,#26162));
#6335=EDGE_LOOP('',(#26163,#26164,#26165,#26166));
#6336=EDGE_LOOP('',(#26167,#26168,#26169,#26170));
#6337=EDGE_LOOP('',(#26171,#26172,#26173,#26174));
#6338=EDGE_LOOP('',(#26175,#26176,#26177,#26178,#26179,#26180,#26181,#26182));
#6339=EDGE_LOOP('',(#26183,#26184,#26185,#26186,#26187));
#6340=EDGE_LOOP('',(#26188,#26189,#26190,#26191));
#6341=EDGE_LOOP('',(#26192,#26193,#26194,#26195));
#6342=EDGE_LOOP('',(#26196,#26197,#26198,#26199));
#6343=EDGE_LOOP('',(#26200,#26201,#26202,#26203));
#6344=EDGE_LOOP('',(#26204,#26205,#26206,#26207));
#6345=EDGE_LOOP('',(#26208,#26209,#26210,#26211));
#6346=EDGE_LOOP('',(#26212,#26213,#26214,#26215));
#6347=EDGE_LOOP('',(#26216,#26217,#26218,#26219,#26220,#26221,#26222,#26223));
#6348=EDGE_LOOP('',(#26224,#26225,#26226,#26227));
#6349=EDGE_LOOP('',(#26228,#26229,#26230,#26231));
#6350=EDGE_LOOP('',(#26232,#26233,#26234));
#6351=EDGE_LOOP('',(#26235,#26236,#26237,#26238));
#6352=EDGE_LOOP('',(#26239,#26240,#26241));
#6353=EDGE_LOOP('',(#26242,#26243,#26244,#26245));
#6354=EDGE_LOOP('',(#26246,#26247,#26248,#26249));
#6355=EDGE_LOOP('',(#26250,#26251,#26252,#26253));
#6356=EDGE_LOOP('',(#26254,#26255,#26256,#26257));
#6357=EDGE_LOOP('',(#26258,#26259,#26260,#26261));
#6358=EDGE_LOOP('',(#26262,#26263,#26264,#26265));
#6359=EDGE_LOOP('',(#26266,#26267,#26268,#26269));
#6360=EDGE_LOOP('',(#26270,#26271,#26272,#26273));
#6361=EDGE_LOOP('',(#26274,#26275,#26276,#26277));
#6362=EDGE_LOOP('',(#26278,#26279,#26280,#26281));
#6363=EDGE_LOOP('',(#26282,#26283,#26284,#26285));
#6364=EDGE_LOOP('',(#26286,#26287,#26288,#26289));
#6365=EDGE_LOOP('',(#26290,#26291,#26292,#26293,#26294,#26295,#26296));
#6366=EDGE_LOOP('',(#26297,#26298,#26299,#26300));
#6367=EDGE_LOOP('',(#26301,#26302,#26303,#26304));
#6368=EDGE_LOOP('',(#26305,#26306,#26307,#26308));
#6369=EDGE_LOOP('',(#26309,#26310,#26311,#26312));
#6370=EDGE_LOOP('',(#26313,#26314,#26315,#26316));
#6371=EDGE_LOOP('',(#26317,#26318,#26319,#26320,#26321,#26322,#26323,#26324,
#26325,#26326,#26327,#26328,#26329,#26330,#26331,#26332,#26333,#26334,#26335,
#26336,#26337,#26338,#26339,#26340,#26341,#26342,#26343,#26344,#26345,#26346,
#26347,#26348,#26349,#26350,#26351,#26352,#26353,#26354,#26355,#26356,#26357));
#6372=EDGE_LOOP('',(#26358,#26359,#26360));
#6373=EDGE_LOOP('',(#26361,#26362,#26363,#26364));
#6374=EDGE_LOOP('',(#26365,#26366,#26367,#26368,#26369,#26370,#26371,#26372,
#26373,#26374,#26375));
#6375=EDGE_LOOP('',(#26376));
#6376=EDGE_LOOP('',(#26377,#26378,#26379,#26380));
#6377=EDGE_LOOP('',(#26381,#26382,#26383,#26384));
#6378=EDGE_LOOP('',(#26385,#26386,#26387,#26388));
#6379=EDGE_LOOP('',(#26389,#26390,#26391,#26392));
#6380=EDGE_LOOP('',(#26393,#26394,#26395,#26396));
#6381=EDGE_LOOP('',(#26397,#26398,#26399,#26400));
#6382=EDGE_LOOP('',(#26401,#26402,#26403,#26404));
#6383=EDGE_LOOP('',(#26405,#26406,#26407,#26408));
#6384=EDGE_LOOP('',(#26409,#26410,#26411,#26412));
#6385=EDGE_LOOP('',(#26413,#26414,#26415,#26416));
#6386=EDGE_LOOP('',(#26417,#26418,#26419,#26420));
#6387=EDGE_LOOP('',(#26421,#26422,#26423,#26424));
#6388=EDGE_LOOP('',(#26425,#26426,#26427,#26428));
#6389=EDGE_LOOP('',(#26429,#26430,#26431,#26432));
#6390=EDGE_LOOP('',(#26433,#26434,#26435,#26436));
#6391=EDGE_LOOP('',(#26437,#26438,#26439,#26440));
#6392=EDGE_LOOP('',(#26441,#26442,#26443,#26444));
#6393=EDGE_LOOP('',(#26445,#26446,#26447,#26448));
#6394=EDGE_LOOP('',(#26449,#26450,#26451,#26452));
#6395=EDGE_LOOP('',(#26453,#26454,#26455,#26456));
#6396=EDGE_LOOP('',(#26457,#26458,#26459,#26460));
#6397=EDGE_LOOP('',(#26461,#26462,#26463,#26464));
#6398=EDGE_LOOP('',(#26465,#26466,#26467,#26468));
#6399=EDGE_LOOP('',(#26469,#26470,#26471,#26472));
#6400=EDGE_LOOP('',(#26473,#26474,#26475,#26476));
#6401=EDGE_LOOP('',(#26477,#26478,#26479,#26480));
#6402=EDGE_LOOP('',(#26481,#26482,#26483,#26484));
#6403=EDGE_LOOP('',(#26485,#26486,#26487,#26488));
#6404=EDGE_LOOP('',(#26489,#26490,#26491,#26492));
#6405=EDGE_LOOP('',(#26493,#26494,#26495,#26496));
#6406=EDGE_LOOP('',(#26497,#26498,#26499,#26500));
#6407=EDGE_LOOP('',(#26501,#26502,#26503,#26504));
#6408=EDGE_LOOP('',(#26505,#26506,#26507,#26508));
#6409=EDGE_LOOP('',(#26509,#26510,#26511,#26512));
#6410=EDGE_LOOP('',(#26513,#26514,#26515,#26516));
#6411=EDGE_LOOP('',(#26517,#26518,#26519,#26520));
#6412=EDGE_LOOP('',(#26521,#26522,#26523,#26524));
#6413=EDGE_LOOP('',(#26525,#26526,#26527,#26528));
#6414=EDGE_LOOP('',(#26529,#26530,#26531,#26532));
#6415=EDGE_LOOP('',(#26533,#26534,#26535,#26536));
#6416=EDGE_LOOP('',(#26537,#26538,#26539,#26540,#26541));
#6417=EDGE_LOOP('',(#26542,#26543,#26544,#26545));
#6418=EDGE_LOOP('',(#26546,#26547,#26548,#26549));
#6419=EDGE_LOOP('',(#26550,#26551,#26552,#26553));
#6420=EDGE_LOOP('',(#26554,#26555,#26556,#26557));
#6421=EDGE_LOOP('',(#26558,#26559,#26560,#26561));
#6422=EDGE_LOOP('',(#26562,#26563,#26564,#26565));
#6423=EDGE_LOOP('',(#26566,#26567,#26568,#26569));
#6424=EDGE_LOOP('',(#26570,#26571,#26572,#26573));
#6425=EDGE_LOOP('',(#26574,#26575,#26576,#26577));
#6426=EDGE_LOOP('',(#26578,#26579,#26580));
#6427=EDGE_LOOP('',(#26581,#26582,#26583,#26584));
#6428=EDGE_LOOP('',(#26585,#26586,#26587));
#6429=EDGE_LOOP('',(#26588,#26589,#26590,#26591));
#6430=EDGE_LOOP('',(#26592,#26593,#26594,#26595));
#6431=EDGE_LOOP('',(#26596,#26597,#26598,#26599,#26600));
#6432=EDGE_LOOP('',(#26601,#26602,#26603,#26604,#26605));
#6433=EDGE_LOOP('',(#26606,#26607,#26608));
#6434=EDGE_LOOP('',(#26609,#26610,#26611,#26612));
#6435=EDGE_LOOP('',(#26613,#26614,#26615,#26616,#26617));
#6436=EDGE_LOOP('',(#26618,#26619,#26620,#26621));
#6437=EDGE_LOOP('',(#26622,#26623,#26624,#26625));
#6438=EDGE_LOOP('',(#26626,#26627,#26628,#26629));
#6439=EDGE_LOOP('',(#26630,#26631,#26632,#26633,#26634,#26635));
#6440=EDGE_LOOP('',(#26636,#26637,#26638,#26639));
#6441=EDGE_LOOP('',(#26640,#26641,#26642,#26643));
#6442=EDGE_LOOP('',(#26644,#26645,#26646,#26647));
#6443=EDGE_LOOP('',(#26648,#26649,#26650,#26651));
#6444=EDGE_LOOP('',(#26652,#26653,#26654));
#6445=EDGE_LOOP('',(#26655,#26656,#26657,#26658));
#6446=EDGE_LOOP('',(#26659,#26660,#26661,#26662,#26663));
#6447=EDGE_LOOP('',(#26664,#26665,#26666,#26667));
#6448=EDGE_LOOP('',(#26668,#26669,#26670,#26671));
#6449=EDGE_LOOP('',(#26672,#26673,#26674));
#6450=EDGE_LOOP('',(#26675,#26676,#26677,#26678,#26679));
#6451=EDGE_LOOP('',(#26680,#26681,#26682,#26683));
#6452=EDGE_LOOP('',(#26684,#26685,#26686,#26687,#26688));
#6453=EDGE_LOOP('',(#26689,#26690,#26691,#26692));
#6454=EDGE_LOOP('',(#26693,#26694,#26695,#26696,#26697,#26698));
#6455=EDGE_LOOP('',(#26699,#26700,#26701,#26702));
#6456=EDGE_LOOP('',(#26703,#26704,#26705,#26706));
#6457=EDGE_LOOP('',(#26707,#26708,#26709,#26710));
#6458=EDGE_LOOP('',(#26711,#26712,#26713,#26714));
#6459=EDGE_LOOP('',(#26715,#26716,#26717,#26718));
#6460=EDGE_LOOP('',(#26719,#26720,#26721,#26722));
#6461=EDGE_LOOP('',(#26723,#26724,#26725,#26726));
#6462=EDGE_LOOP('',(#26727,#26728,#26729,#26730));
#6463=EDGE_LOOP('',(#26731,#26732,#26733));
#6464=EDGE_LOOP('',(#26734,#26735,#26736,#26737));
#6465=EDGE_LOOP('',(#26738,#26739,#26740));
#6466=EDGE_LOOP('',(#26741,#26742,#26743,#26744));
#6467=EDGE_LOOP('',(#26745,#26746,#26747,#26748));
#6468=EDGE_LOOP('',(#26749,#26750,#26751,#26752));
#6469=EDGE_LOOP('',(#26753,#26754,#26755));
#6470=EDGE_LOOP('',(#26756,#26757,#26758,#26759));
#6471=EDGE_LOOP('',(#26760,#26761,#26762));
#6472=EDGE_LOOP('',(#26763,#26764,#26765,#26766));
#6473=EDGE_LOOP('',(#26767,#26768,#26769,#26770));
#6474=EDGE_LOOP('',(#26771,#26772,#26773,#26774));
#6475=EDGE_LOOP('',(#26775,#26776,#26777,#26778,#26779));
#6476=EDGE_LOOP('',(#26780,#26781,#26782,#26783));
#6477=EDGE_LOOP('',(#26784,#26785,#26786,#26787,#26788));
#6478=EDGE_LOOP('',(#26789,#26790,#26791,#26792));
#6479=EDGE_LOOP('',(#26793,#26794,#26795,#26796));
#6480=EDGE_LOOP('',(#26797,#26798,#26799,#26800,#26801,#26802,#26803,#26804,
#26805,#26806,#26807));
#6481=EDGE_LOOP('',(#26808));
#6482=EDGE_LOOP('',(#26809,#26810,#26811,#26812,#26813));
#6483=EDGE_LOOP('',(#26814,#26815,#26816,#26817));
#6484=EDGE_LOOP('',(#26818,#26819,#26820));
#6485=EDGE_LOOP('',(#26821,#26822,#26823,#26824,#26825));
#6486=EDGE_LOOP('',(#26826,#26827,#26828,#26829));
#6487=EDGE_LOOP('',(#26830,#26831,#26832,#26833,#26834));
#6488=EDGE_LOOP('',(#26835,#26836,#26837,#26838));
#6489=EDGE_LOOP('',(#26839,#26840,#26841,#26842));
#6490=EDGE_LOOP('',(#26843,#26844,#26845,#26846));
#6491=EDGE_LOOP('',(#26847,#26848,#26849,#26850));
#6492=EDGE_LOOP('',(#26851,#26852,#26853,#26854));
#6493=EDGE_LOOP('',(#26855,#26856,#26857,#26858));
#6494=EDGE_LOOP('',(#26859,#26860,#26861,#26862));
#6495=EDGE_LOOP('',(#26863,#26864,#26865,#26866));
#6496=EDGE_LOOP('',(#26867,#26868,#26869,#26870));
#6497=EDGE_LOOP('',(#26871,#26872,#26873,#26874));
#6498=EDGE_LOOP('',(#26875,#26876,#26877,#26878));
#6499=EDGE_LOOP('',(#26879,#26880,#26881,#26882));
#6500=EDGE_LOOP('',(#26883,#26884,#26885,#26886));
#6501=EDGE_LOOP('',(#26887,#26888,#26889,#26890));
#6502=EDGE_LOOP('',(#26891,#26892,#26893,#26894));
#6503=EDGE_LOOP('',(#26895,#26896,#26897,#26898));
#6504=EDGE_LOOP('',(#26899,#26900,#26901,#26902));
#6505=EDGE_LOOP('',(#26903,#26904,#26905,#26906));
#6506=EDGE_LOOP('',(#26907,#26908,#26909,#26910));
#6507=EDGE_LOOP('',(#26911,#26912,#26913,#26914));
#6508=EDGE_LOOP('',(#26915,#26916,#26917,#26918));
#6509=EDGE_LOOP('',(#26919,#26920,#26921,#26922));
#6510=EDGE_LOOP('',(#26923,#26924,#26925,#26926));
#6511=EDGE_LOOP('',(#26927,#26928,#26929,#26930));
#6512=EDGE_LOOP('',(#26931,#26932,#26933,#26934));
#6513=EDGE_LOOP('',(#26935,#26936,#26937,#26938));
#6514=EDGE_LOOP('',(#26939,#26940,#26941,#26942));
#6515=EDGE_LOOP('',(#26943));
#6516=EDGE_LOOP('',(#26944));
#6517=EDGE_LOOP('',(#26945,#26946,#26947));
#6518=EDGE_LOOP('',(#26948,#26949,#26950,#26951,#26952));
#6519=EDGE_LOOP('',(#26953,#26954,#26955,#26956));
#6520=EDGE_LOOP('',(#26957,#26958,#26959,#26960));
#6521=EDGE_LOOP('',(#26961,#26962,#26963,#26964));
#6522=EDGE_LOOP('',(#26965,#26966,#26967,#26968));
#6523=EDGE_LOOP('',(#26969,#26970,#26971,#26972));
#6524=EDGE_LOOP('',(#26973,#26974,#26975,#26976));
#6525=EDGE_LOOP('',(#26977,#26978,#26979,#26980));
#6526=EDGE_LOOP('',(#26981,#26982,#26983));
#6527=EDGE_LOOP('',(#26984,#26985,#26986,#26987));
#6528=EDGE_LOOP('',(#26988,#26989,#26990));
#6529=EDGE_LOOP('',(#26991,#26992,#26993,#26994));
#6530=EDGE_LOOP('',(#26995,#26996,#26997,#26998));
#6531=EDGE_LOOP('',(#26999,#27000,#27001,#27002));
#6532=EDGE_LOOP('',(#27003,#27004,#27005,#27006));
#6533=EDGE_LOOP('',(#27007,#27008,#27009,#27010));
#6534=EDGE_LOOP('',(#27011,#27012,#27013,#27014,#27015,#27016,#27017));
#6535=EDGE_LOOP('',(#27018,#27019,#27020));
#6536=EDGE_LOOP('',(#27021,#27022,#27023));
#6537=EDGE_LOOP('',(#27024,#27025,#27026));
#6538=EDGE_LOOP('',(#27027,#27028,#27029));
#6539=EDGE_LOOP('',(#27030,#27031,#27032,#27033));
#6540=EDGE_LOOP('',(#27034,#27035,#27036,#27037));
#6541=EDGE_LOOP('',(#27038,#27039,#27040,#27041));
#6542=EDGE_LOOP('',(#27042,#27043,#27044,#27045));
#6543=EDGE_LOOP('',(#27046,#27047,#27048,#27049));
#6544=EDGE_LOOP('',(#27050,#27051,#27052,#27053));
#6545=EDGE_LOOP('',(#27054,#27055,#27056));
#6546=EDGE_LOOP('',(#27057,#27058,#27059,#27060));
#6547=EDGE_LOOP('',(#27061,#27062,#27063,#27064));
#6548=EDGE_LOOP('',(#27065,#27066,#27067,#27068,#27069));
#6549=EDGE_LOOP('',(#27070,#27071,#27072,#27073));
#6550=EDGE_LOOP('',(#27074,#27075,#27076));
#6551=EDGE_LOOP('',(#27077));
#6552=EDGE_LOOP('',(#27078,#27079,#27080,#27081));
#6553=EDGE_LOOP('',(#27082,#27083,#27084,#27085));
#6554=EDGE_LOOP('',(#27086,#27087,#27088,#27089));
#6555=EDGE_LOOP('',(#27090,#27091,#27092,#27093));
#6556=EDGE_LOOP('',(#27094,#27095,#27096,#27097,#27098));
#6557=EDGE_LOOP('',(#27099,#27100,#27101,#27102));
#6558=EDGE_LOOP('',(#27103,#27104,#27105,#27106));
#6559=EDGE_LOOP('',(#27107,#27108,#27109,#27110));
#6560=EDGE_LOOP('',(#27111,#27112,#27113,#27114));
#6561=EDGE_LOOP('',(#27115,#27116,#27117,#27118));
#6562=EDGE_LOOP('',(#27119,#27120,#27121,#27122,#27123,#27124,#27125,#27126,
#27127,#27128,#27129,#27130,#27131,#27132,#27133,#27134,#27135,#27136,#27137,
#27138,#27139,#27140,#27141,#27142,#27143,#27144,#27145,#27146,#27147,#27148,
#27149,#27150,#27151,#27152,#27153,#27154,#27155,#27156,#27157,#27158,#27159));
#6563=EDGE_LOOP('',(#27160,#27161,#27162,#27163));
#6564=EDGE_LOOP('',(#27164,#27165,#27166));
#6565=EDGE_LOOP('',(#27167,#27168,#27169,#27170));
#6566=EDGE_LOOP('',(#27171,#27172,#27173,#27174));
#6567=EDGE_LOOP('',(#27175,#27176,#27177,#27178,#27179));
#6568=EDGE_LOOP('',(#27180,#27181,#27182,#27183,#27184));
#6569=EDGE_LOOP('',(#27185,#27186,#27187,#27188));
#6570=EDGE_LOOP('',(#27189,#27190,#27191,#27192));
#6571=EDGE_LOOP('',(#27193,#27194,#27195,#27196,#27197,#27198,#27199,#27200));
#6572=EDGE_LOOP('',(#27201,#27202,#27203,#27204));
#6573=EDGE_LOOP('',(#27205,#27206,#27207,#27208));
#6574=EDGE_LOOP('',(#27209,#27210,#27211,#27212));
#6575=EDGE_LOOP('',(#27213,#27214,#27215,#27216));
#6576=EDGE_LOOP('',(#27217,#27218,#27219,#27220));
#6577=EDGE_LOOP('',(#27221,#27222,#27223,#27224));
#6578=EDGE_LOOP('',(#27225,#27226,#27227,#27228));
#6579=EDGE_LOOP('',(#27229,#27230,#27231,#27232));
#6580=EDGE_LOOP('',(#27233,#27234,#27235,#27236));
#6581=EDGE_LOOP('',(#27237,#27238,#27239,#27240,#27241));
#6582=EDGE_LOOP('',(#27242,#27243,#27244,#27245));
#6583=EDGE_LOOP('',(#27246,#27247,#27248,#27249));
#6584=EDGE_LOOP('',(#27250,#27251,#27252,#27253));
#6585=EDGE_LOOP('',(#27254,#27255,#27256,#27257));
#6586=EDGE_LOOP('',(#27258,#27259,#27260,#27261));
#6587=EDGE_LOOP('',(#27262,#27263,#27264,#27265));
#6588=EDGE_LOOP('',(#27266,#27267,#27268,#27269));
#6589=EDGE_LOOP('',(#27270,#27271,#27272,#27273));
#6590=EDGE_LOOP('',(#27274,#27275,#27276,#27277));
#6591=EDGE_LOOP('',(#27278,#27279,#27280));
#6592=EDGE_LOOP('',(#27281,#27282,#27283,#27284));
#6593=EDGE_LOOP('',(#27285,#27286,#27287,#27288));
#6594=EDGE_LOOP('',(#27289,#27290,#27291,#27292));
#6595=EDGE_LOOP('',(#27293,#27294,#27295,#27296));
#6596=EDGE_LOOP('',(#27297,#27298,#27299,#27300,#27301,#27302,#27303));
#6597=EDGE_LOOP('',(#27304,#27305,#27306,#27307));
#6598=EDGE_LOOP('',(#27308,#27309,#27310,#27311));
#6599=EDGE_LOOP('',(#27312,#27313,#27314));
#6600=EDGE_LOOP('',(#27315,#27316,#27317,#27318,#27319,#27320,#27321,#27322));
#6601=EDGE_LOOP('',(#27323,#27324,#27325,#27326));
#6602=EDGE_LOOP('',(#27327,#27328,#27329,#27330));
#6603=EDGE_LOOP('',(#27331,#27332,#27333,#27334));
#6604=EDGE_LOOP('',(#27335,#27336,#27337,#27338,#27339,#27340,#27341,#27342));
#6605=EDGE_LOOP('',(#27343,#27344,#27345,#27346,#27347,#27348,#27349,#27350,
#27351,#27352));
#6606=EDGE_LOOP('',(#27353,#27354,#27355,#27356,#27357));
#6607=EDGE_LOOP('',(#27358,#27359,#27360,#27361,#27362,#27363,#27364,#27365));
#6608=EDGE_LOOP('',(#27366,#27367));
#6609=EDGE_LOOP('',(#27368));
#6610=EDGE_LOOP('',(#27369,#27370,#27371,#27372));
#6611=EDGE_LOOP('',(#27373,#27374,#27375,#27376));
#6612=EDGE_LOOP('',(#27377,#27378,#27379,#27380));
#6613=EDGE_LOOP('',(#27381,#27382,#27383,#27384));
#6614=EDGE_LOOP('',(#27385,#27386,#27387,#27388));
#6615=EDGE_LOOP('',(#27389,#27390,#27391,#27392));
#6616=EDGE_LOOP('',(#27393,#27394,#27395,#27396));
#6617=EDGE_LOOP('',(#27397,#27398,#27399,#27400));
#6618=EDGE_LOOP('',(#27401,#27402,#27403,#27404,#27405,#27406,#27407,#27408,
#27409,#27410,#27411,#27412,#27413,#27414,#27415,#27416,#27417,#27418,#27419,
#27420,#27421,#27422,#27423,#27424,#27425,#27426,#27427,#27428,#27429,#27430,
#27431,#27432,#27433,#27434,#27435,#27436,#27437,#27438,#27439,#27440,#27441,
#27442,#27443,#27444,#27445,#27446,#27447,#27448,#27449,#27450,#27451,#27452,
#27453,#27454));
#6619=EDGE_LOOP('',(#27455,#27456,#27457,#27458));
#6620=EDGE_LOOP('',(#27459,#27460,#27461,#27462));
#6621=EDGE_LOOP('',(#27463,#27464,#27465,#27466,#27467,#27468,#27469,#27470,
#27471,#27472,#27473,#27474,#27475,#27476,#27477,#27478,#27479,#27480,#27481,
#27482,#27483));
#6622=EDGE_LOOP('',(#27484,#27485,#27486,#27487));
#6623=EDGE_LOOP('',(#27488,#27489,#27490,#27491));
#6624=EDGE_LOOP('',(#27492,#27493,#27494,#27495));
#6625=EDGE_LOOP('',(#27496,#27497,#27498,#27499));
#6626=EDGE_LOOP('',(#27500,#27501,#27502,#27503));
#6627=EDGE_LOOP('',(#27504,#27505,#27506,#27507));
#6628=EDGE_LOOP('',(#27508,#27509,#27510,#27511));
#6629=EDGE_LOOP('',(#27512,#27513,#27514,#27515));
#6630=EDGE_LOOP('',(#27516,#27517,#27518,#27519));
#6631=EDGE_LOOP('',(#27520,#27521,#27522,#27523));
#6632=EDGE_LOOP('',(#27524,#27525,#27526,#27527));
#6633=EDGE_LOOP('',(#27528,#27529,#27530,#27531,#27532,#27533,#27534,#27535,
#27536,#27537,#27538,#27539));
#6634=EDGE_LOOP('',(#27540,#27541,#27542,#27543));
#6635=EDGE_LOOP('',(#27544,#27545,#27546,#27547));
#6636=EDGE_LOOP('',(#27548,#27549,#27550,#27551));
#6637=EDGE_LOOP('',(#27552,#27553,#27554,#27555));
#6638=EDGE_LOOP('',(#27556,#27557,#27558,#27559));
#6639=EDGE_LOOP('',(#27560,#27561,#27562,#27563));
#6640=EDGE_LOOP('',(#27564,#27565,#27566,#27567,#27568,#27569,#27570));
#6641=EDGE_LOOP('',(#27571,#27572,#27573,#27574));
#6642=EDGE_LOOP('',(#27575,#27576,#27577,#27578));
#6643=EDGE_LOOP('',(#27579,#27580,#27581,#27582));
#6644=EDGE_LOOP('',(#27583,#27584,#27585,#27586));
#6645=EDGE_LOOP('',(#27587,#27588,#27589,#27590));
#6646=EDGE_LOOP('',(#27591,#27592,#27593));
#6647=EDGE_LOOP('',(#27594,#27595,#27596,#27597,#27598));
#6648=EDGE_LOOP('',(#27599,#27600,#27601,#27602,#27603));
#6649=EDGE_LOOP('',(#27604,#27605,#27606,#27607));
#6650=EDGE_LOOP('',(#27608,#27609,#27610,#27611));
#6651=EDGE_LOOP('',(#27612,#27613,#27614,#27615));
#6652=EDGE_LOOP('',(#27616,#27617,#27618,#27619));
#6653=EDGE_LOOP('',(#27620,#27621,#27622,#27623));
#6654=EDGE_LOOP('',(#27624,#27625,#27626,#27627));
#6655=EDGE_LOOP('',(#27628,#27629,#27630,#27631,#27632,#27633));
#6656=EDGE_LOOP('',(#27634,#27635,#27636,#27637));
#6657=EDGE_LOOP('',(#27638,#27639,#27640,#27641));
#6658=EDGE_LOOP('',(#27642,#27643,#27644,#27645));
#6659=EDGE_LOOP('',(#27646,#27647,#27648,#27649));
#6660=EDGE_LOOP('',(#27650,#27651,#27652,#27653));
#6661=EDGE_LOOP('',(#27654,#27655,#27656,#27657,#27658,#27659));
#6662=EDGE_LOOP('',(#27660,#27661,#27662,#27663,#27664,#27665,#27666,#27667));
#6663=EDGE_LOOP('',(#27668,#27669,#27670,#27671));
#6664=EDGE_LOOP('',(#27672,#27673,#27674,#27675,#27676,#27677,#27678));
#6665=EDGE_LOOP('',(#27679,#27680,#27681,#27682));
#6666=EDGE_LOOP('',(#27683,#27684,#27685,#27686));
#6667=EDGE_LOOP('',(#27687,#27688,#27689,#27690));
#6668=EDGE_LOOP('',(#27691,#27692,#27693,#27694));
#6669=EDGE_LOOP('',(#27695,#27696,#27697,#27698));
#6670=EDGE_LOOP('',(#27699,#27700,#27701,#27702));
#6671=EDGE_LOOP('',(#27703,#27704,#27705,#27706));
#6672=EDGE_LOOP('',(#27707,#27708,#27709));
#6673=EDGE_LOOP('',(#27710,#27711,#27712,#27713,#27714));
#6674=EDGE_LOOP('',(#27715,#27716,#27717,#27718,#27719));
#6675=EDGE_LOOP('',(#27720,#27721,#27722,#27723));
#6676=EDGE_LOOP('',(#27724,#27725,#27726,#27727));
#6677=EDGE_LOOP('',(#27728,#27729,#27730,#27731));
#6678=EDGE_LOOP('',(#27732,#27733,#27734,#27735));
#6679=EDGE_LOOP('',(#27736,#27737,#27738,#27739));
#6680=EDGE_LOOP('',(#27740,#27741,#27742,#27743));
#6681=EDGE_LOOP('',(#27744,#27745,#27746,#27747,#27748,#27749));
#6682=EDGE_LOOP('',(#27750,#27751,#27752,#27753));
#6683=EDGE_LOOP('',(#27754,#27755,#27756,#27757));
#6684=EDGE_LOOP('',(#27758,#27759,#27760,#27761));
#6685=EDGE_LOOP('',(#27762,#27763,#27764,#27765));
#6686=EDGE_LOOP('',(#27766,#27767,#27768,#27769));
#6687=EDGE_LOOP('',(#27770,#27771,#27772,#27773));
#6688=EDGE_LOOP('',(#27774,#27775,#27776,#27777));
#6689=EDGE_LOOP('',(#27778,#27779,#27780,#27781));
#6690=EDGE_LOOP('',(#27782,#27783,#27784,#27785));
#6691=EDGE_LOOP('',(#27786,#27787,#27788,#27789,#27790,#27791,#27792,#27793,
#27794,#27795,#27796,#27797));
#6692=EDGE_LOOP('',(#27798,#27799,#27800,#27801));
#6693=EDGE_LOOP('',(#27802,#27803,#27804,#27805));
#6694=EDGE_LOOP('',(#27806,#27807,#27808,#27809));
#6695=EDGE_LOOP('',(#27810,#27811,#27812,#27813));
#6696=EDGE_LOOP('',(#27814,#27815,#27816,#27817));
#6697=EDGE_LOOP('',(#27818,#27819,#27820,#27821));
#6698=EDGE_LOOP('',(#27822,#27823,#27824,#27825));
#6699=EDGE_LOOP('',(#27826,#27827,#27828,#27829));
#6700=EDGE_LOOP('',(#27830,#27831,#27832,#27833));
#6701=EDGE_LOOP('',(#27834,#27835,#27836,#27837));
#6702=EDGE_LOOP('',(#27838,#27839,#27840,#27841));
#6703=EDGE_LOOP('',(#27842,#27843,#27844,#27845));
#6704=EDGE_LOOP('',(#27846,#27847,#27848,#27849));
#6705=EDGE_LOOP('',(#27850,#27851,#27852,#27853,#27854,#27855));
#6706=EDGE_LOOP('',(#27856,#27857,#27858,#27859));
#6707=EDGE_LOOP('',(#27860,#27861,#27862,#27863));
#6708=EDGE_LOOP('',(#27864,#27865,#27866,#27867));
#6709=EDGE_LOOP('',(#27868,#27869,#27870,#27871));
#6710=EDGE_LOOP('',(#27872,#27873,#27874,#27875));
#6711=EDGE_LOOP('',(#27876,#27877,#27878,#27879,#27880,#27881,#27882,#27883));
#6712=EDGE_LOOP('',(#27884,#27885,#27886,#27887));
#6713=EDGE_LOOP('',(#27888,#27889,#27890,#27891,#27892));
#6714=EDGE_LOOP('',(#27893,#27894,#27895,#27896,#27897,#27898,#27899,#27900,
#27901,#27902,#27903,#27904,#27905,#27906,#27907,#27908,#27909,#27910,#27911,
#27912,#27913));
#6715=EDGE_LOOP('',(#27914));
#6716=EDGE_LOOP('',(#27915,#27916,#27917,#27918,#27919));
#6717=EDGE_LOOP('',(#27920));
#6718=EDGE_LOOP('',(#27921,#27922,#27923,#27924,#27925,#27926,#27927,#27928,
#27929,#27930,#27931,#27932));
#6719=EDGE_LOOP('',(#27933,#27934,#27935,#27936));
#6720=EDGE_LOOP('',(#27937,#27938,#27939,#27940));
#6721=EDGE_LOOP('',(#27941,#27942,#27943,#27944));
#6722=EDGE_LOOP('',(#27945,#27946,#27947,#27948,#27949));
#6723=EDGE_LOOP('',(#27950,#27951,#27952,#27953));
#6724=EDGE_LOOP('',(#27954,#27955,#27956,#27957));
#6725=EDGE_LOOP('',(#27958,#27959,#27960,#27961));
#6726=EDGE_LOOP('',(#27962,#27963,#27964,#27965));
#6727=EDGE_LOOP('',(#27966,#27967,#27968,#27969));
#6728=EDGE_LOOP('',(#27970,#27971,#27972,#27973,#27974));
#6729=EDGE_LOOP('',(#27975,#27976,#27977,#27978));
#6730=EDGE_LOOP('',(#27979,#27980,#27981,#27982));
#6731=EDGE_LOOP('',(#27983,#27984,#27985,#27986,#27987,#27988,#27989,#27990,
#27991,#27992));
#6732=EDGE_LOOP('',(#27993,#27994,#27995,#27996,#27997));
#6733=EDGE_LOOP('',(#27998,#27999,#28000,#28001,#28002));
#6734=EDGE_LOOP('',(#28003,#28004,#28005,#28006));
#6735=EDGE_LOOP('',(#28007,#28008,#28009,#28010));
#6736=EDGE_LOOP('',(#28011,#28012,#28013,#28014));
#6737=EDGE_LOOP('',(#28015,#28016,#28017,#28018));
#6738=EDGE_LOOP('',(#28019,#28020,#28021,#28022));
#6739=EDGE_LOOP('',(#28023,#28024,#28025,#28026));
#6740=EDGE_LOOP('',(#28027,#28028,#28029,#28030,#28031,#28032));
#6741=EDGE_LOOP('',(#28033,#28034,#28035,#28036,#28037));
#6742=EDGE_LOOP('',(#28038,#28039,#28040,#28041));
#6743=EDGE_LOOP('',(#28042,#28043,#28044));
#6744=EDGE_LOOP('',(#28045,#28046,#28047,#28048));
#6745=EDGE_LOOP('',(#28049,#28050,#28051));
#6746=EDGE_LOOP('',(#28052,#28053,#28054,#28055));
#6747=EDGE_LOOP('',(#28056,#28057,#28058,#28059));
#6748=EDGE_LOOP('',(#28060,#28061,#28062,#28063));
#6749=EDGE_LOOP('',(#28064,#28065,#28066,#28067));
#6750=EDGE_LOOP('',(#28068,#28069,#28070,#28071));
#6751=EDGE_LOOP('',(#28072,#28073,#28074,#28075));
#6752=EDGE_LOOP('',(#28076,#28077,#28078,#28079));
#6753=EDGE_LOOP('',(#28080,#28081,#28082));
#6754=EDGE_LOOP('',(#28083,#28084,#28085,#28086));
#6755=EDGE_LOOP('',(#28087,#28088,#28089));
#6756=EDGE_LOOP('',(#28090,#28091,#28092,#28093));
#6757=EDGE_LOOP('',(#28094,#28095,#28096,#28097,#28098,#28099,#28100,#28101,
#28102,#28103,#28104,#28105,#28106));
#6758=EDGE_LOOP('',(#28107,#28108,#28109,#28110,#28111,#28112,#28113));
#6759=EDGE_LOOP('',(#28114,#28115,#28116,#28117));
#6760=EDGE_LOOP('',(#28118,#28119,#28120,#28121));
#6761=EDGE_LOOP('',(#28122,#28123,#28124,#28125));
#6762=EDGE_LOOP('',(#28126,#28127,#28128,#28129));
#6763=EDGE_LOOP('',(#28130,#28131,#28132,#28133));
#6764=EDGE_LOOP('',(#28134,#28135,#28136,#28137));
#6765=EDGE_LOOP('',(#28138,#28139,#28140,#28141));
#6766=EDGE_LOOP('',(#28142,#28143,#28144));
#6767=EDGE_LOOP('',(#28145,#28146,#28147,#28148));
#6768=EDGE_LOOP('',(#28149,#28150,#28151));
#6769=EDGE_LOOP('',(#28152,#28153,#28154,#28155));
#6770=EDGE_LOOP('',(#28156,#28157,#28158,#28159));
#6771=EDGE_LOOP('',(#28160,#28161,#28162,#28163));
#6772=EDGE_LOOP('',(#28164,#28165,#28166));
#6773=EDGE_LOOP('',(#28167,#28168,#28169,#28170));
#6774=EDGE_LOOP('',(#28171,#28172,#28173,#28174));
#6775=EDGE_LOOP('',(#28175,#28176,#28177,#28178));
#6776=EDGE_LOOP('',(#28179,#28180,#28181,#28182));
#6777=EDGE_LOOP('',(#28183,#28184,#28185,#28186));
#6778=EDGE_LOOP('',(#28187,#28188,#28189));
#6779=EDGE_LOOP('',(#28190,#28191,#28192,#28193));
#6780=EDGE_LOOP('',(#28194,#28195,#28196));
#6781=EDGE_LOOP('',(#28197,#28198,#28199,#28200));
#6782=EDGE_LOOP('',(#28201,#28202,#28203));
#6783=EDGE_LOOP('',(#28204,#28205,#28206,#28207));
#6784=EDGE_LOOP('',(#28208,#28209,#28210));
#6785=EDGE_LOOP('',(#28211,#28212,#28213,#28214));
#6786=EDGE_LOOP('',(#28215,#28216,#28217,#28218));
#6787=EDGE_LOOP('',(#28219,#28220,#28221,#28222));
#6788=EDGE_LOOP('',(#28223,#28224,#28225,#28226));
#6789=EDGE_LOOP('',(#28227,#28228,#28229,#28230));
#6790=EDGE_LOOP('',(#28231,#28232,#28233,#28234));
#6791=EDGE_LOOP('',(#28235,#28236,#28237,#28238));
#6792=EDGE_LOOP('',(#28239,#28240,#28241,#28242));
#6793=EDGE_LOOP('',(#28243,#28244,#28245,#28246));
#6794=EDGE_LOOP('',(#28247,#28248,#28249,#28250));
#6795=EDGE_LOOP('',(#28251,#28252,#28253));
#6796=EDGE_LOOP('',(#28254,#28255,#28256,#28257));
#6797=EDGE_LOOP('',(#28258,#28259,#28260,#28261));
#6798=EDGE_LOOP('',(#28262,#28263,#28264,#28265));
#6799=EDGE_LOOP('',(#28266,#28267,#28268,#28269));
#6800=EDGE_LOOP('',(#28270,#28271,#28272,#28273));
#6801=EDGE_LOOP('',(#28274,#28275,#28276,#28277));
#6802=EDGE_LOOP('',(#28278,#28279,#28280,#28281));
#6803=EDGE_LOOP('',(#28282,#28283,#28284,#28285));
#6804=EDGE_LOOP('',(#28286,#28287,#28288,#28289,#28290,#28291,#28292,#28293,
#28294,#28295,#28296,#28297,#28298,#28299));
#6805=EDGE_LOOP('',(#28300,#28301,#28302,#28303,#28304));
#6806=EDGE_LOOP('',(#28305,#28306,#28307,#28308));
#6807=EDGE_LOOP('',(#28309,#28310,#28311,#28312,#28313,#28314));
#6808=EDGE_LOOP('',(#28315,#28316,#28317,#28318));
#6809=EDGE_LOOP('',(#28319,#28320,#28321,#28322,#28323,#28324));
#6810=EDGE_LOOP('',(#28325,#28326,#28327,#28328));
#6811=EDGE_LOOP('',(#28329,#28330,#28331));
#6812=EDGE_LOOP('',(#28332,#28333,#28334,#28335));
#6813=EDGE_LOOP('',(#28336,#28337,#28338,#28339));
#6814=EDGE_LOOP('',(#28340,#28341,#28342,#28343,#28344,#28345,#28346,#28347,
#28348));
#6815=EDGE_LOOP('',(#28349,#28350,#28351,#28352));
#6816=EDGE_LOOP('',(#28353,#28354,#28355,#28356));
#6817=EDGE_LOOP('',(#28357,#28358,#28359,#28360));
#6818=EDGE_LOOP('',(#28361,#28362,#28363,#28364));
#6819=EDGE_LOOP('',(#28365,#28366,#28367,#28368));
#6820=EDGE_LOOP('',(#28369,#28370,#28371,#28372));
#6821=EDGE_LOOP('',(#28373,#28374,#28375,#28376));
#6822=EDGE_LOOP('',(#28377,#28378,#28379,#28380));
#6823=EDGE_LOOP('',(#28381,#28382,#28383,#28384));
#6824=EDGE_LOOP('',(#28385,#28386,#28387,#28388));
#6825=EDGE_LOOP('',(#28389,#28390,#28391,#28392));
#6826=EDGE_LOOP('',(#28393,#28394,#28395,#28396));
#6827=EDGE_LOOP('',(#28397,#28398,#28399,#28400));
#6828=EDGE_LOOP('',(#28401,#28402,#28403,#28404));
#6829=EDGE_LOOP('',(#28405,#28406,#28407,#28408));
#6830=EDGE_LOOP('',(#28409,#28410,#28411,#28412));
#6831=EDGE_LOOP('',(#28413,#28414,#28415,#28416));
#6832=EDGE_LOOP('',(#28417,#28418,#28419,#28420));
#6833=EDGE_LOOP('',(#28421,#28422,#28423,#28424,#28425));
#6834=EDGE_LOOP('',(#28426,#28427,#28428,#28429));
#6835=EDGE_LOOP('',(#28430,#28431,#28432,#28433));
#6836=EDGE_LOOP('',(#28434,#28435,#28436,#28437));
#6837=EDGE_LOOP('',(#28438,#28439,#28440,#28441,#28442,#28443,#28444));
#6838=EDGE_LOOP('',(#28445,#28446,#28447,#28448));
#6839=EDGE_LOOP('',(#28449,#28450,#28451,#28452));
#6840=EDGE_LOOP('',(#28453,#28454,#28455,#28456));
#6841=EDGE_LOOP('',(#28457,#28458,#28459,#28460));
#6842=EDGE_LOOP('',(#28461,#28462,#28463,#28464));
#6843=EDGE_LOOP('',(#28465,#28466,#28467,#28468));
#6844=EDGE_LOOP('',(#28469,#28470,#28471,#28472,#28473,#28474,#28475,#28476));
#6845=EDGE_LOOP('',(#28477,#28478,#28479,#28480));
#6846=EDGE_LOOP('',(#28481,#28482,#28483,#28484));
#6847=EDGE_LOOP('',(#28485,#28486,#28487,#28488));
#6848=EDGE_LOOP('',(#28489,#28490,#28491,#28492));
#6849=EDGE_LOOP('',(#28493,#28494,#28495,#28496));
#6850=EDGE_LOOP('',(#28497,#28498,#28499,#28500));
#6851=EDGE_LOOP('',(#28501,#28502,#28503,#28504));
#6852=EDGE_LOOP('',(#28505,#28506,#28507,#28508));
#6853=EDGE_LOOP('',(#28509,#28510,#28511,#28512));
#6854=EDGE_LOOP('',(#28513,#28514,#28515,#28516));
#6855=EDGE_LOOP('',(#28517,#28518,#28519));
#6856=EDGE_LOOP('',(#28520,#28521,#28522,#28523));
#6857=EDGE_LOOP('',(#28524,#28525,#28526));
#6858=EDGE_LOOP('',(#28527,#28528,#28529));
#6859=EDGE_LOOP('',(#28530,#28531,#28532));
#6860=EDGE_LOOP('',(#28533,#28534,#28535,#28536));
#6861=EDGE_LOOP('',(#28537,#28538,#28539,#28540));
#6862=EDGE_LOOP('',(#28541,#28542,#28543,#28544));
#6863=EDGE_LOOP('',(#28545,#28546,#28547,#28548));
#6864=EDGE_LOOP('',(#28549,#28550,#28551,#28552));
#6865=EDGE_LOOP('',(#28553,#28554,#28555,#28556));
#6866=EDGE_LOOP('',(#28557,#28558,#28559));
#6867=EDGE_LOOP('',(#28560,#28561,#28562,#28563));
#6868=EDGE_LOOP('',(#28564,#28565,#28566));
#6869=EDGE_LOOP('',(#28567,#28568,#28569,#28570));
#6870=EDGE_LOOP('',(#28571,#28572,#28573,#28574));
#6871=EDGE_LOOP('',(#28575,#28576,#28577,#28578));
#6872=EDGE_LOOP('',(#28579,#28580));
#6873=EDGE_LOOP('',(#28581,#28582,#28583,#28584));
#6874=EDGE_LOOP('',(#28585,#28586,#28587,#28588));
#6875=EDGE_LOOP('',(#28589,#28590,#28591,#28592));
#6876=EDGE_LOOP('',(#28593,#28594,#28595,#28596));
#6877=EDGE_LOOP('',(#28597,#28598,#28599,#28600));
#6878=EDGE_LOOP('',(#28601,#28602,#28603));
#6879=EDGE_LOOP('',(#28604,#28605,#28606,#28607));
#6880=EDGE_LOOP('',(#28608,#28609,#28610,#28611));
#6881=EDGE_LOOP('',(#28612,#28613,#28614,#28615,#28616,#28617));
#6882=EDGE_LOOP('',(#28618,#28619,#28620,#28621));
#6883=EDGE_LOOP('',(#28622,#28623,#28624,#28625));
#6884=EDGE_LOOP('',(#28626,#28627,#28628,#28629));
#6885=EDGE_LOOP('',(#28630,#28631,#28632));
#6886=EDGE_LOOP('',(#28633,#28634,#28635,#28636));
#6887=EDGE_LOOP('',(#28637,#28638,#28639,#28640));
#6888=EDGE_LOOP('',(#28641,#28642,#28643,#28644,#28645));
#6889=EDGE_LOOP('',(#28646,#28647,#28648,#28649));
#6890=EDGE_LOOP('',(#28650,#28651,#28652,#28653));
#6891=EDGE_LOOP('',(#28654,#28655,#28656,#28657));
#6892=EDGE_LOOP('',(#28658,#28659,#28660,#28661));
#6893=EDGE_LOOP('',(#28662,#28663,#28664,#28665,#28666,#28667,#28668));
#6894=EDGE_LOOP('',(#28669,#28670,#28671,#28672));
#6895=EDGE_LOOP('',(#28673,#28674,#28675));
#6896=EDGE_LOOP('',(#28676,#28677,#28678,#28679,#28680,#28681,#28682,#28683));
#6897=EDGE_LOOP('',(#28684,#28685,#28686,#28687));
#6898=EDGE_LOOP('',(#28688,#28689,#28690,#28691));
#6899=EDGE_LOOP('',(#28692,#28693,#28694));
#6900=EDGE_LOOP('',(#28695,#28696,#28697,#28698));
#6901=EDGE_LOOP('',(#28699,#28700,#28701,#28702,#28703,#28704));
#6902=EDGE_LOOP('',(#28705,#28706,#28707,#28708));
#6903=EDGE_LOOP('',(#28709,#28710,#28711,#28712));
#6904=EDGE_LOOP('',(#28713,#28714,#28715,#28716));
#6905=EDGE_LOOP('',(#28717,#28718,#28719,#28720));
#6906=EDGE_LOOP('',(#28721,#28722,#28723,#28724));
#6907=EDGE_LOOP('',(#28725,#28726,#28727,#28728));
#6908=EDGE_LOOP('',(#28729,#28730,#28731,#28732));
#6909=EDGE_LOOP('',(#28733,#28734,#28735,#28736));
#6910=EDGE_LOOP('',(#28737,#28738,#28739,#28740));
#6911=EDGE_LOOP('',(#28741,#28742,#28743,#28744));
#6912=EDGE_LOOP('',(#28745,#28746,#28747,#28748));
#6913=EDGE_LOOP('',(#28749,#28750,#28751,#28752));
#6914=EDGE_LOOP('',(#28753,#28754,#28755,#28756));
#6915=EDGE_LOOP('',(#28757,#28758,#28759,#28760));
#6916=EDGE_LOOP('',(#28761,#28762,#28763,#28764));
#6917=EDGE_LOOP('',(#28765,#28766,#28767,#28768));
#6918=EDGE_LOOP('',(#28769,#28770,#28771,#28772));
#6919=EDGE_LOOP('',(#28773,#28774,#28775,#28776));
#6920=EDGE_LOOP('',(#28777,#28778,#28779,#28780));
#6921=EDGE_LOOP('',(#28781,#28782,#28783,#28784));
#6922=EDGE_LOOP('',(#28785,#28786,#28787,#28788));
#6923=EDGE_LOOP('',(#28789,#28790,#28791,#28792));
#6924=EDGE_LOOP('',(#28793,#28794,#28795,#28796));
#6925=EDGE_LOOP('',(#28797,#28798,#28799,#28800));
#6926=EDGE_LOOP('',(#28801,#28802,#28803,#28804));
#6927=EDGE_LOOP('',(#28805,#28806,#28807));
#6928=EDGE_LOOP('',(#28808,#28809,#28810,#28811));
#6929=EDGE_LOOP('',(#28812,#28813,#28814));
#6930=EDGE_LOOP('',(#28815,#28816,#28817));
#6931=EDGE_LOOP('',(#28818,#28819,#28820,#28821));
#6932=EDGE_LOOP('',(#28822,#28823,#28824,#28825));
#6933=EDGE_LOOP('',(#28826,#28827,#28828));
#6934=EDGE_LOOP('',(#28829,#28830,#28831));
#6935=EDGE_LOOP('',(#28832,#28833,#28834));
#6936=EDGE_LOOP('',(#28835,#28836,#28837,#28838));
#6937=EDGE_LOOP('',(#28839,#28840,#28841,#28842));
#6938=EDGE_LOOP('',(#28843,#28844,#28845,#28846));
#6939=EDGE_LOOP('',(#28847,#28848,#28849));
#6940=EDGE_LOOP('',(#28850,#28851,#28852,#28853));
#6941=EDGE_LOOP('',(#28854,#28855,#28856,#28857));
#6942=EDGE_LOOP('',(#28858,#28859,#28860));
#6943=EDGE_LOOP('',(#28861,#28862,#28863,#28864));
#6944=EDGE_LOOP('',(#28865,#28866,#28867,#28868));
#6945=EDGE_LOOP('',(#28869,#28870,#28871));
#6946=EDGE_LOOP('',(#28872,#28873,#28874,#28875));
#6947=EDGE_LOOP('',(#28876,#28877,#28878,#28879));
#6948=EDGE_LOOP('',(#28880,#28881,#28882));
#6949=EDGE_LOOP('',(#28883,#28884,#28885,#28886));
#6950=EDGE_LOOP('',(#28887,#28888,#28889,#28890));
#6951=EDGE_LOOP('',(#28891,#28892,#28893,#28894));
#6952=EDGE_LOOP('',(#28895,#28896,#28897,#28898));
#6953=EDGE_LOOP('',(#28899,#28900,#28901,#28902));
#6954=EDGE_LOOP('',(#28903,#28904,#28905,#28906));
#6955=EDGE_LOOP('',(#28907,#28908,#28909,#28910));
#6956=EDGE_LOOP('',(#28911,#28912,#28913,#28914));
#6957=EDGE_LOOP('',(#28915,#28916,#28917,#28918,#28919));
#6958=EDGE_LOOP('',(#28920,#28921,#28922,#28923));
#6959=EDGE_LOOP('',(#28924,#28925,#28926));
#6960=EDGE_LOOP('',(#28927,#28928,#28929,#28930));
#6961=EDGE_LOOP('',(#28931,#28932,#28933,#28934));
#6962=EDGE_LOOP('',(#28935,#28936,#28937,#28938));
#6963=EDGE_LOOP('',(#28939,#28940,#28941,#28942));
#6964=EDGE_LOOP('',(#28943,#28944,#28945,#28946));
#6965=EDGE_LOOP('',(#28947,#28948,#28949));
#6966=EDGE_LOOP('',(#28950,#28951,#28952,#28953));
#6967=EDGE_LOOP('',(#28954,#28955,#28956,#28957));
#6968=EDGE_LOOP('',(#28958,#28959,#28960,#28961));
#6969=EDGE_LOOP('',(#28962,#28963,#28964));
#6970=EDGE_LOOP('',(#28965,#28966,#28967,#28968));
#6971=EDGE_LOOP('',(#28969,#28970,#28971,#28972));
#6972=EDGE_LOOP('',(#28973,#28974,#28975,#28976));
#6973=EDGE_LOOP('',(#28977,#28978,#28979,#28980));
#6974=EDGE_LOOP('',(#28981,#28982,#28983,#28984));
#6975=EDGE_LOOP('',(#28985,#28986,#28987,#28988));
#6976=EDGE_LOOP('',(#28989,#28990,#28991));
#6977=EDGE_LOOP('',(#28992,#28993,#28994,#28995));
#6978=EDGE_LOOP('',(#28996,#28997,#28998,#28999));
#6979=EDGE_LOOP('',(#29000,#29001,#29002,#29003));
#6980=EDGE_LOOP('',(#29004,#29005,#29006,#29007));
#6981=EDGE_LOOP('',(#29008,#29009,#29010,#29011));
#6982=EDGE_LOOP('',(#29012,#29013,#29014,#29015));
#6983=EDGE_LOOP('',(#29016,#29017,#29018,#29019,#29020));
#6984=EDGE_LOOP('',(#29021,#29022,#29023,#29024));
#6985=EDGE_LOOP('',(#29025,#29026,#29027,#29028));
#6986=EDGE_LOOP('',(#29029,#29030,#29031,#29032));
#6987=EDGE_LOOP('',(#29033,#29034,#29035,#29036));
#6988=EDGE_LOOP('',(#29037,#29038,#29039,#29040));
#6989=EDGE_LOOP('',(#29041,#29042,#29043,#29044));
#6990=EDGE_LOOP('',(#29045,#29046,#29047,#29048));
#6991=EDGE_LOOP('',(#29049,#29050,#29051,#29052));
#6992=EDGE_LOOP('',(#29053,#29054,#29055,#29056,#29057));
#6993=EDGE_LOOP('',(#29058,#29059,#29060,#29061));
#6994=EDGE_LOOP('',(#29062,#29063,#29064,#29065));
#6995=EDGE_LOOP('',(#29066,#29067,#29068,#29069));
#6996=EDGE_LOOP('',(#29070,#29071,#29072,#29073));
#6997=EDGE_LOOP('',(#29074,#29075,#29076,#29077));
#6998=EDGE_LOOP('',(#29078,#29079,#29080,#29081));
#6999=EDGE_LOOP('',(#29082,#29083,#29084));
#7000=EDGE_LOOP('',(#29085,#29086,#29087,#29088,#29089));
#7001=EDGE_LOOP('',(#29090,#29091,#29092,#29093,#29094,#29095));
#7002=EDGE_LOOP('',(#29096,#29097,#29098,#29099));
#7003=EDGE_LOOP('',(#29100,#29101,#29102,#29103,#29104,#29105));
#7004=EDGE_LOOP('',(#29106,#29107,#29108,#29109));
#7005=EDGE_LOOP('',(#29110,#29111,#29112,#29113));
#7006=EDGE_LOOP('',(#29114,#29115,#29116,#29117));
#7007=EDGE_LOOP('',(#29118,#29119,#29120,#29121));
#7008=EDGE_LOOP('',(#29122,#29123,#29124,#29125));
#7009=EDGE_LOOP('',(#29126,#29127,#29128,#29129));
#7010=EDGE_LOOP('',(#29130,#29131,#29132,#29133));
#7011=EDGE_LOOP('',(#29134,#29135,#29136,#29137,#29138,#29139));
#7012=EDGE_LOOP('',(#29140,#29141,#29142,#29143));
#7013=EDGE_LOOP('',(#29144,#29145,#29146));
#7014=EDGE_LOOP('',(#29147,#29148,#29149,#29150));
#7015=EDGE_LOOP('',(#29151,#29152,#29153,#29154));
#7016=EDGE_LOOP('',(#29155,#29156,#29157));
#7017=EDGE_LOOP('',(#29158,#29159,#29160,#29161));
#7018=EDGE_LOOP('',(#29162,#29163,#29164));
#7019=EDGE_LOOP('',(#29165,#29166,#29167,#29168));
#7020=EDGE_LOOP('',(#29169,#29170,#29171));
#7021=EDGE_LOOP('',(#29172,#29173,#29174,#29175));
#7022=EDGE_LOOP('',(#29176,#29177,#29178));
#7023=EDGE_LOOP('',(#29179,#29180,#29181,#29182));
#7024=EDGE_LOOP('',(#29183,#29184,#29185));
#7025=EDGE_LOOP('',(#29186,#29187,#29188,#29189));
#7026=EDGE_LOOP('',(#29190,#29191,#29192,#29193));
#7027=EDGE_LOOP('',(#29194,#29195,#29196,#29197));
#7028=EDGE_LOOP('',(#29198,#29199,#29200,#29201));
#7029=EDGE_LOOP('',(#29202,#29203,#29204,#29205));
#7030=EDGE_LOOP('',(#29206,#29207,#29208,#29209,#29210,#29211,#29212,#29213,
#29214,#29215,#29216));
#7031=EDGE_LOOP('',(#29217,#29218,#29219,#29220,#29221));
#7032=EDGE_LOOP('',(#29222,#29223,#29224,#29225,#29226));
#7033=EDGE_LOOP('',(#29227,#29228,#29229,#29230));
#7034=EDGE_LOOP('',(#29231,#29232,#29233,#29234));
#7035=EDGE_LOOP('',(#29235,#29236,#29237,#29238));
#7036=EDGE_LOOP('',(#29239,#29240,#29241,#29242));
#7037=EDGE_LOOP('',(#29243,#29244,#29245,#29246));
#7038=EDGE_LOOP('',(#29247,#29248,#29249,#29250));
#7039=EDGE_LOOP('',(#29251,#29252,#29253,#29254,#29255,#29256));
#7040=EDGE_LOOP('',(#29257,#29258,#29259,#29260,#29261));
#7041=EDGE_LOOP('',(#29262,#29263,#29264,#29265));
#7042=EDGE_LOOP('',(#29266,#29267,#29268));
#7043=EDGE_LOOP('',(#29269,#29270,#29271,#29272));
#7044=EDGE_LOOP('',(#29273,#29274,#29275));
#7045=EDGE_LOOP('',(#29276,#29277,#29278,#29279));
#7046=EDGE_LOOP('',(#29280,#29281,#29282,#29283));
#7047=EDGE_LOOP('',(#29284,#29285,#29286,#29287));
#7048=EDGE_LOOP('',(#29288,#29289,#29290,#29291));
#7049=EDGE_LOOP('',(#29292,#29293,#29294,#29295));
#7050=EDGE_LOOP('',(#29296,#29297,#29298,#29299));
#7051=EDGE_LOOP('',(#29300,#29301,#29302,#29303));
#7052=EDGE_LOOP('',(#29304,#29305,#29306));
#7053=EDGE_LOOP('',(#29307,#29308,#29309,#29310));
#7054=EDGE_LOOP('',(#29311,#29312,#29313));
#7055=EDGE_LOOP('',(#29314,#29315,#29316,#29317));
#7056=EDGE_LOOP('',(#29318,#29319,#29320,#29321,#29322,#29323,#29324,#29325,
#29326,#29327,#29328,#29329,#29330));
#7057=EDGE_LOOP('',(#29331,#29332,#29333,#29334,#29335,#29336,#29337));
#7058=EDGE_LOOP('',(#29338,#29339,#29340,#29341));
#7059=EDGE_LOOP('',(#29342,#29343,#29344,#29345));
#7060=EDGE_LOOP('',(#29346,#29347,#29348,#29349));
#7061=EDGE_LOOP('',(#29350,#29351,#29352,#29353));
#7062=EDGE_LOOP('',(#29354,#29355,#29356,#29357));
#7063=EDGE_LOOP('',(#29358,#29359,#29360,#29361));
#7064=EDGE_LOOP('',(#29362,#29363,#29364,#29365));
#7065=EDGE_LOOP('',(#29366,#29367,#29368));
#7066=EDGE_LOOP('',(#29369,#29370,#29371,#29372));
#7067=EDGE_LOOP('',(#29373,#29374,#29375));
#7068=EDGE_LOOP('',(#29376,#29377,#29378,#29379));
#7069=EDGE_LOOP('',(#29380,#29381,#29382,#29383));
#7070=EDGE_LOOP('',(#29384,#29385,#29386));
#7071=EDGE_LOOP('',(#29387,#29388,#29389,#29390));
#7072=EDGE_LOOP('',(#29391,#29392,#29393));
#7073=EDGE_LOOP('',(#29394,#29395,#29396));
#7074=EDGE_LOOP('',(#29397,#29398,#29399,#29400));
#7075=EDGE_LOOP('',(#29401,#29402,#29403,#29404,#29405,#29406,#29407,#29408,
#29409,#29410,#29411,#29412));
#7076=EDGE_LOOP('',(#29413,#29414,#29415,#29416));
#7077=EDGE_LOOP('',(#29417,#29418,#29419,#29420));
#7078=EDGE_LOOP('',(#29421,#29422,#29423,#29424));
#7079=EDGE_LOOP('',(#29425,#29426,#29427,#29428));
#7080=EDGE_LOOP('',(#29429,#29430,#29431));
#7081=EDGE_LOOP('',(#29432,#29433,#29434,#29435));
#7082=EDGE_LOOP('',(#29436,#29437,#29438));
#7083=EDGE_LOOP('',(#29439,#29440,#29441,#29442));
#7084=EDGE_LOOP('',(#29443,#29444,#29445));
#7085=EDGE_LOOP('',(#29446,#29447,#29448,#29449));
#7086=EDGE_LOOP('',(#29450,#29451,#29452));
#7087=EDGE_LOOP('',(#29453,#29454,#29455,#29456));
#7088=EDGE_LOOP('',(#29457,#29458,#29459,#29460));
#7089=EDGE_LOOP('',(#29461,#29462,#29463,#29464));
#7090=EDGE_LOOP('',(#29465,#29466,#29467,#29468));
#7091=EDGE_LOOP('',(#29469,#29470,#29471,#29472));
#7092=EDGE_LOOP('',(#29473,#29474,#29475,#29476));
#7093=EDGE_LOOP('',(#29477,#29478,#29479,#29480));
#7094=EDGE_LOOP('',(#29481,#29482,#29483,#29484));
#7095=EDGE_LOOP('',(#29485,#29486,#29487,#29488));
#7096=EDGE_LOOP('',(#29489,#29490,#29491,#29492));
#7097=EDGE_LOOP('',(#29493,#29494,#29495));
#7098=EDGE_LOOP('',(#29496,#29497,#29498,#29499));
#7099=EDGE_LOOP('',(#29500,#29501,#29502,#29503));
#7100=EDGE_LOOP('',(#29504,#29505,#29506,#29507));
#7101=EDGE_LOOP('',(#29508,#29509,#29510));
#7102=EDGE_LOOP('',(#29511,#29512,#29513,#29514));
#7103=EDGE_LOOP('',(#29515,#29516,#29517,#29518));
#7104=EDGE_LOOP('',(#29519,#29520,#29521,#29522));
#7105=EDGE_LOOP('',(#29523,#29524,#29525,#29526));
#7106=EDGE_LOOP('',(#29527,#29528,#29529,#29530));
#7107=EDGE_LOOP('',(#29531,#29532,#29533,#29534));
#7108=EDGE_LOOP('',(#29535,#29536,#29537,#29538));
#7109=EDGE_LOOP('',(#29539,#29540,#29541,#29542,#29543,#29544,#29545,#29546,
#29547,#29548,#29549,#29550,#29551,#29552));
#7110=EDGE_LOOP('',(#29553,#29554,#29555,#29556));
#7111=EDGE_LOOP('',(#29557,#29558,#29559,#29560,#29561));
#7112=EDGE_LOOP('',(#29562,#29563,#29564,#29565));
#7113=EDGE_LOOP('',(#29566,#29567,#29568,#29569,#29570,#29571));
#7114=EDGE_LOOP('',(#29572,#29573,#29574,#29575));
#7115=EDGE_LOOP('',(#29576,#29577,#29578,#29579,#29580,#29581));
#7116=EDGE_LOOP('',(#29582,#29583,#29584,#29585));
#7117=EDGE_LOOP('',(#29586,#29587,#29588));
#7118=EDGE_LOOP('',(#29589,#29590,#29591,#29592));
#7119=EDGE_LOOP('',(#29593,#29594,#29595,#29596,#29597,#29598,#29599,#29600,
#29601,#29602,#29603,#29604,#29605,#29606,#29607,#29608));
#7120=EDGE_LOOP('',(#29609,#29610,#29611,#29612));
#7121=EDGE_LOOP('',(#29613,#29614,#29615,#29616,#29617,#29618,#29619,#29620,
#29621));
#7122=EDGE_LOOP('',(#29622,#29623,#29624,#29625));
#7123=EDGE_LOOP('',(#29626,#29627,#29628,#29629));
#7124=EDGE_LOOP('',(#29630,#29631,#29632,#29633));
#7125=EDGE_LOOP('',(#29634,#29635,#29636,#29637));
#7126=EDGE_LOOP('',(#29638,#29639,#29640,#29641));
#7127=EDGE_LOOP('',(#29642,#29643,#29644,#29645));
#7128=EDGE_LOOP('',(#29646,#29647,#29648,#29649));
#7129=EDGE_LOOP('',(#29650,#29651,#29652,#29653));
#7130=EDGE_LOOP('',(#29654,#29655,#29656,#29657));
#7131=EDGE_LOOP('',(#29658,#29659,#29660,#29661));
#7132=EDGE_LOOP('',(#29662,#29663,#29664,#29665));
#7133=EDGE_LOOP('',(#29666,#29667,#29668,#29669));
#7134=EDGE_LOOP('',(#29670,#29671,#29672,#29673));
#7135=EDGE_LOOP('',(#29674,#29675,#29676,#29677));
#7136=EDGE_LOOP('',(#29678,#29679,#29680,#29681));
#7137=EDGE_LOOP('',(#29682,#29683,#29684,#29685));
#7138=EDGE_LOOP('',(#29686,#29687,#29688,#29689));
#7139=EDGE_LOOP('',(#29690,#29691,#29692,#29693));
#7140=EDGE_LOOP('',(#29694,#29695,#29696,#29697,#29698));
#7141=EDGE_LOOP('',(#29699,#29700,#29701,#29702));
#7142=EDGE_LOOP('',(#29703,#29704,#29705,#29706));
#7143=EDGE_LOOP('',(#29707,#29708,#29709,#29710));
#7144=EDGE_LOOP('',(#29711,#29712,#29713,#29714,#29715,#29716,#29717));
#7145=EDGE_LOOP('',(#29718,#29719,#29720,#29721));
#7146=EDGE_LOOP('',(#29722,#29723,#29724,#29725));
#7147=EDGE_LOOP('',(#29726,#29727,#29728,#29729));
#7148=EDGE_LOOP('',(#29730,#29731,#29732,#29733));
#7149=EDGE_LOOP('',(#29734,#29735,#29736,#29737));
#7150=EDGE_LOOP('',(#29738,#29739,#29740,#29741));
#7151=EDGE_LOOP('',(#29742,#29743,#29744,#29745,#29746,#29747,#29748,#29749));
#7152=EDGE_LOOP('',(#29750,#29751,#29752,#29753));
#7153=EDGE_LOOP('',(#29754,#29755,#29756,#29757));
#7154=EDGE_LOOP('',(#29758,#29759,#29760,#29761));
#7155=EDGE_LOOP('',(#29762,#29763,#29764,#29765));
#7156=EDGE_LOOP('',(#29766,#29767,#29768,#29769));
#7157=EDGE_LOOP('',(#29770,#29771,#29772,#29773));
#7158=EDGE_LOOP('',(#29774,#29775,#29776,#29777));
#7159=EDGE_LOOP('',(#29778,#29779,#29780,#29781));
#7160=EDGE_LOOP('',(#29782,#29783,#29784,#29785));
#7161=EDGE_LOOP('',(#29786,#29787,#29788,#29789));
#7162=EDGE_LOOP('',(#29790,#29791,#29792));
#7163=EDGE_LOOP('',(#29793,#29794,#29795,#29796));
#7164=EDGE_LOOP('',(#29797,#29798,#29799));
#7165=EDGE_LOOP('',(#29800,#29801,#29802));
#7166=EDGE_LOOP('',(#29803,#29804,#29805));
#7167=EDGE_LOOP('',(#29806,#29807,#29808,#29809));
#7168=EDGE_LOOP('',(#29810,#29811,#29812,#29813));
#7169=EDGE_LOOP('',(#29814,#29815,#29816,#29817));
#7170=EDGE_LOOP('',(#29818,#29819,#29820,#29821));
#7171=EDGE_LOOP('',(#29822,#29823,#29824,#29825));
#7172=EDGE_LOOP('',(#29826,#29827,#29828,#29829));
#7173=EDGE_LOOP('',(#29830,#29831,#29832));
#7174=EDGE_LOOP('',(#29833,#29834,#29835,#29836));
#7175=EDGE_LOOP('',(#29837,#29838,#29839,#29840));
#7176=EDGE_LOOP('',(#29841,#29842,#29843));
#7177=EDGE_LOOP('',(#29844,#29845,#29846));
#7178=EDGE_LOOP('',(#29847,#29848,#29849,#29850));
#7179=EDGE_LOOP('',(#29851,#29852,#29853,#29854));
#7180=EDGE_LOOP('',(#29855,#29856,#29857,#29858));
#7181=EDGE_LOOP('',(#29859,#29860));
#7182=EDGE_LOOP('',(#29861,#29862,#29863,#29864));
#7183=EDGE_LOOP('',(#29865,#29866,#29867,#29868));
#7184=EDGE_LOOP('',(#29869,#29870,#29871,#29872));
#7185=EDGE_LOOP('',(#29873,#29874,#29875,#29876));
#7186=EDGE_LOOP('',(#29877,#29878,#29879,#29880));
#7187=EDGE_LOOP('',(#29881,#29882,#29883,#29884));
#7188=EDGE_LOOP('',(#29885,#29886,#29887,#29888));
#7189=EDGE_LOOP('',(#29889,#29890,#29891,#29892));
#7190=EDGE_LOOP('',(#29893,#29894,#29895,#29896));
#7191=EDGE_LOOP('',(#29897,#29898,#29899,#29900));
#7192=EDGE_LOOP('',(#29901,#29902,#29903,#29904));
#7193=EDGE_LOOP('',(#29905,#29906,#29907,#29908));
#7194=EDGE_LOOP('',(#29909,#29910,#29911,#29912));
#7195=EDGE_LOOP('',(#29913,#29914,#29915,#29916));
#7196=EDGE_LOOP('',(#29917,#29918,#29919,#29920));
#7197=EDGE_LOOP('',(#29921,#29922,#29923,#29924));
#7198=EDGE_LOOP('',(#29925,#29926,#29927,#29928));
#7199=EDGE_LOOP('',(#29929,#29930,#29931,#29932));
#7200=EDGE_LOOP('',(#29933,#29934,#29935,#29936,#29937,#29938,#29939,#29940,
#29941,#29942,#29943,#29944,#29945,#29946,#29947));
#7201=EDGE_LOOP('',(#29948,#29949,#29950,#29951,#29952,#29953,#29954,#29955,
#29956,#29957,#29958,#29959,#29960,#29961,#29962,#29963));
#7202=EDGE_LOOP('',(#29964,#29965,#29966));
#7203=EDGE_LOOP('',(#29967,#29968,#29969,#29970));
#7204=EDGE_LOOP('',(#29971,#29972,#29973,#29974));
#7205=EDGE_LOOP('',(#29975,#29976,#29977,#29978));
#7206=EDGE_LOOP('',(#29979,#29980,#29981));
#7207=EDGE_LOOP('',(#29982,#29983,#29984,#29985));
#7208=EDGE_LOOP('',(#29986,#29987,#29988,#29989));
#7209=EDGE_LOOP('',(#29990,#29991,#29992,#29993,#29994,#29995));
#7210=EDGE_LOOP('',(#29996,#29997,#29998,#29999));
#7211=EDGE_LOOP('',(#30000,#30001,#30002,#30003));
#7212=EDGE_LOOP('',(#30004,#30005,#30006,#30007));
#7213=EDGE_LOOP('',(#30008,#30009,#30010));
#7214=EDGE_LOOP('',(#30011,#30012,#30013,#30014));
#7215=EDGE_LOOP('',(#30015,#30016,#30017,#30018));
#7216=EDGE_LOOP('',(#30019,#30020,#30021,#30022));
#7217=EDGE_LOOP('',(#30023,#30024,#30025,#30026));
#7218=EDGE_LOOP('',(#30027,#30028,#30029,#30030,#30031,#30032));
#7219=EDGE_LOOP('',(#30033,#30034,#30035,#30036));
#7220=EDGE_LOOP('',(#30037,#30038,#30039,#30040,#30041,#30042,#30043,#30044,
#30045,#30046,#30047,#30048,#30049,#30050));
#7221=EDGE_LOOP('',(#30051,#30052,#30053,#30054,#30055));
#7222=EDGE_LOOP('',(#30056,#30057,#30058,#30059));
#7223=EDGE_LOOP('',(#30060,#30061,#30062,#30063));
#7224=EDGE_LOOP('',(#30064,#30065,#30066,#30067));
#7225=EDGE_LOOP('',(#30068,#30069,#30070,#30071));
#7226=EDGE_LOOP('',(#30072,#30073,#30074,#30075,#30076,#30077,#30078));
#7227=EDGE_LOOP('',(#30079,#30080,#30081,#30082));
#7228=EDGE_LOOP('',(#30083,#30084,#30085));
#7229=EDGE_LOOP('',(#30086,#30087,#30088,#30089,#30090,#30091,#30092,#30093));
#7230=EDGE_LOOP('',(#30094,#30095,#30096,#30097));
#7231=EDGE_LOOP('',(#30098,#30099,#30100,#30101));
#7232=EDGE_LOOP('',(#30102,#30103,#30104));
#7233=EDGE_LOOP('',(#30105,#30106,#30107,#30108));
#7234=EDGE_LOOP('',(#30109,#30110,#30111,#30112,#30113,#30114));
#7235=EDGE_LOOP('',(#30115,#30116,#30117,#30118));
#7236=EDGE_LOOP('',(#30119,#30120,#30121,#30122));
#7237=EDGE_LOOP('',(#30123,#30124,#30125,#30126));
#7238=EDGE_LOOP('',(#30127,#30128,#30129,#30130));
#7239=EDGE_LOOP('',(#30131,#30132,#30133,#30134));
#7240=EDGE_LOOP('',(#30135,#30136,#30137,#30138));
#7241=EDGE_LOOP('',(#30139,#30140,#30141,#30142));
#7242=EDGE_LOOP('',(#30143,#30144,#30145,#30146));
#7243=EDGE_LOOP('',(#30147,#30148,#30149,#30150));
#7244=EDGE_LOOP('',(#30151,#30152,#30153,#30154));
#7245=EDGE_LOOP('',(#30155,#30156,#30157,#30158));
#7246=EDGE_LOOP('',(#30159,#30160,#30161,#30162));
#7247=EDGE_LOOP('',(#30163,#30164,#30165,#30166));
#7248=EDGE_LOOP('',(#30167,#30168,#30169,#30170));
#7249=EDGE_LOOP('',(#30171,#30172,#30173,#30174));
#7250=EDGE_LOOP('',(#30175,#30176,#30177,#30178));
#7251=EDGE_LOOP('',(#30179,#30180,#30181,#30182));
#7252=EDGE_LOOP('',(#30183,#30184,#30185,#30186));
#7253=EDGE_LOOP('',(#30187,#30188,#30189,#30190));
#7254=EDGE_LOOP('',(#30191,#30192,#30193,#30194));
#7255=EDGE_LOOP('',(#30195,#30196,#30197,#30198));
#7256=EDGE_LOOP('',(#30199,#30200,#30201,#30202));
#7257=EDGE_LOOP('',(#30203,#30204,#30205,#30206));
#7258=EDGE_LOOP('',(#30207,#30208,#30209,#30210));
#7259=EDGE_LOOP('',(#30211,#30212,#30213,#30214));
#7260=EDGE_LOOP('',(#30215,#30216,#30217));
#7261=EDGE_LOOP('',(#30218,#30219,#30220,#30221));
#7262=EDGE_LOOP('',(#30222,#30223,#30224));
#7263=EDGE_LOOP('',(#30225,#30226,#30227));
#7264=EDGE_LOOP('',(#30228,#30229,#30230,#30231));
#7265=EDGE_LOOP('',(#30232,#30233,#30234,#30235));
#7266=EDGE_LOOP('',(#30236,#30237,#30238));
#7267=EDGE_LOOP('',(#30239,#30240,#30241));
#7268=EDGE_LOOP('',(#30242,#30243,#30244));
#7269=EDGE_LOOP('',(#30245,#30246,#30247,#30248));
#7270=EDGE_LOOP('',(#30249,#30250,#30251,#30252));
#7271=EDGE_LOOP('',(#30253,#30254,#30255,#30256));
#7272=EDGE_LOOP('',(#30257,#30258,#30259));
#7273=EDGE_LOOP('',(#30260,#30261,#30262,#30263));
#7274=EDGE_LOOP('',(#30264,#30265,#30266,#30267));
#7275=EDGE_LOOP('',(#30268,#30269,#30270));
#7276=EDGE_LOOP('',(#30271,#30272,#30273,#30274));
#7277=EDGE_LOOP('',(#30275,#30276,#30277,#30278));
#7278=EDGE_LOOP('',(#30279,#30280,#30281));
#7279=EDGE_LOOP('',(#30282,#30283,#30284,#30285));
#7280=EDGE_LOOP('',(#30286,#30287,#30288,#30289));
#7281=EDGE_LOOP('',(#30290,#30291,#30292));
#7282=EDGE_LOOP('',(#30293,#30294,#30295,#30296));
#7283=EDGE_LOOP('',(#30297,#30298,#30299,#30300));
#7284=EDGE_LOOP('',(#30301,#30302,#30303,#30304));
#7285=EDGE_LOOP('',(#30305,#30306,#30307,#30308));
#7286=EDGE_LOOP('',(#30309,#30310,#30311,#30312));
#7287=EDGE_LOOP('',(#30313,#30314,#30315,#30316));
#7288=EDGE_LOOP('',(#30317,#30318,#30319,#30320));
#7289=EDGE_LOOP('',(#30321,#30322,#30323,#30324));
#7290=EDGE_LOOP('',(#30325,#30326,#30327,#30328,#30329,#30330,#30331,#30332,
#30333,#30334,#30335,#30336,#30337,#30338,#30339,#30340,#30341,#30342,#30343,
#30344,#30345,#30346));
#7291=EDGE_LOOP('',(#30347,#30348,#30349,#30350,#30351));
#7292=EDGE_LOOP('',(#30352,#30353,#30354,#30355));
#7293=EDGE_LOOP('',(#30356,#30357,#30358));
#7294=EDGE_LOOP('',(#30359,#30360,#30361));
#7295=EDGE_LOOP('',(#30362,#30363,#30364,#30365));
#7296=EDGE_LOOP('',(#30366,#30367,#30368,#30369));
#7297=EDGE_LOOP('',(#30370,#30371,#30372,#30373));
#7298=EDGE_LOOP('',(#30374,#30375,#30376,#30377));
#7299=EDGE_LOOP('',(#30378,#30379,#30380,#30381));
#7300=EDGE_LOOP('',(#30382,#30383,#30384,#30385));
#7301=EDGE_LOOP('',(#30386,#30387,#30388));
#7302=EDGE_LOOP('',(#30389,#30390,#30391,#30392));
#7303=EDGE_LOOP('',(#30393,#30394,#30395,#30396));
#7304=EDGE_LOOP('',(#30397,#30398,#30399,#30400));
#7305=EDGE_LOOP('',(#30401,#30402,#30403));
#7306=EDGE_LOOP('',(#30404,#30405,#30406,#30407));
#7307=EDGE_LOOP('',(#30408,#30409,#30410,#30411));
#7308=EDGE_LOOP('',(#30412,#30413,#30414,#30415));
#7309=EDGE_LOOP('',(#30416,#30417,#30418,#30419));
#7310=EDGE_LOOP('',(#30420,#30421,#30422,#30423));
#7311=EDGE_LOOP('',(#30424,#30425,#30426,#30427));
#7312=EDGE_LOOP('',(#30428,#30429,#30430));
#7313=EDGE_LOOP('',(#30431,#30432,#30433,#30434));
#7314=EDGE_LOOP('',(#30435,#30436,#30437,#30438));
#7315=EDGE_LOOP('',(#30439,#30440,#30441,#30442));
#7316=EDGE_LOOP('',(#30443,#30444,#30445,#30446));
#7317=EDGE_LOOP('',(#30447,#30448,#30449,#30450));
#7318=EDGE_LOOP('',(#30451,#30452,#30453,#30454));
#7319=EDGE_LOOP('',(#30455,#30456,#30457,#30458,#30459));
#7320=EDGE_LOOP('',(#30460,#30461,#30462,#30463));
#7321=EDGE_LOOP('',(#30464,#30465,#30466,#30467));
#7322=EDGE_LOOP('',(#30468,#30469,#30470,#30471));
#7323=EDGE_LOOP('',(#30472,#30473,#30474,#30475));
#7324=EDGE_LOOP('',(#30476,#30477,#30478,#30479));
#7325=EDGE_LOOP('',(#30480,#30481,#30482,#30483));
#7326=EDGE_LOOP('',(#30484,#30485,#30486,#30487));
#7327=EDGE_LOOP('',(#30488,#30489,#30490,#30491));
#7328=EDGE_LOOP('',(#30492,#30493,#30494,#30495));
#7329=EDGE_LOOP('',(#30496,#30497,#30498,#30499));
#7330=EDGE_LOOP('',(#30500,#30501,#30502,#30503));
#7331=EDGE_LOOP('',(#30504,#30505,#30506,#30507));
#7332=EDGE_LOOP('',(#30508,#30509,#30510,#30511));
#7333=EDGE_LOOP('',(#30512,#30513,#30514,#30515));
#7334=EDGE_LOOP('',(#30516,#30517,#30518,#30519));
#7335=EDGE_LOOP('',(#30520,#30521,#30522,#30523));
#7336=EDGE_LOOP('',(#30524,#30525,#30526,#30527));
#7337=EDGE_LOOP('',(#30528,#30529,#30530,#30531));
#7338=EDGE_LOOP('',(#30532,#30533,#30534,#30535,#30536,#30537,#30538,#30539,
#30540,#30541,#30542,#30543,#30544,#30545,#30546,#30547,#30548,#30549,#30550,
#30551,#30552,#30553,#30554,#30555,#30556,#30557,#30558,#30559,#30560,#30561,
#30562,#30563,#30564,#30565,#30566,#30567,#30568,#30569,#30570,#30571,#30572,
#30573,#30574,#30575,#30576,#30577,#30578,#30579,#30580,#30581,#30582,#30583,
#30584,#30585,#30586,#30587,#30588,#30589,#30590));
#7339=EDGE_LOOP('',(#30591,#30592,#30593,#30594,#30595,#30596,#30597,#30598));
#7340=EDGE_LOOP('',(#30599,#30600,#30601,#30602,#30603,#30604,#30605,#30606));
#7341=EDGE_LOOP('',(#30607,#30608,#30609,#30610,#30611,#30612,#30613,#30614));
#7342=EDGE_LOOP('',(#30615,#30616,#30617,#30618,#30619,#30620,#30621,#30622,
#30623,#30624,#30625,#30626,#30627,#30628,#30629,#30630,#30631,#30632,#30633,
#30634,#30635,#30636,#30637,#30638,#30639,#30640,#30641,#30642,#30643,#30644,
#30645,#30646,#30647,#30648,#30649,#30650,#30651,#30652,#30653,#30654,#30655,
#30656));
#7343=EDGE_LOOP('',(#30657,#30658,#30659,#30660,#30661,#30662,#30663,#30664));
#7344=EDGE_LOOP('',(#30665,#30666,#30667,#30668));
#7345=EDGE_LOOP('',(#30669,#30670,#30671,#30672));
#7346=EDGE_LOOP('',(#30673,#30674,#30675,#30676));
#7347=EDGE_LOOP('',(#30677,#30678,#30679,#30680,#30681));
#7348=EDGE_LOOP('',(#30682,#30683,#30684,#30685));
#7349=EDGE_LOOP('',(#30686,#30687,#30688,#30689));
#7350=EDGE_LOOP('',(#30690,#30691,#30692,#30693));
#7351=EDGE_LOOP('',(#30694,#30695,#30696,#30697));
#7352=EDGE_LOOP('',(#30698,#30699,#30700,#30701));
#7353=EDGE_LOOP('',(#30702,#30703,#30704,#30705));
#7354=EDGE_LOOP('',(#30706,#30707,#30708));
#7355=EDGE_LOOP('',(#30709,#30710,#30711,#30712,#30713));
#7356=EDGE_LOOP('',(#30714,#30715,#30716,#30717,#30718,#30719));
#7357=EDGE_LOOP('',(#30720,#30721,#30722,#30723));
#7358=EDGE_LOOP('',(#30724,#30725,#30726,#30727,#30728,#30729));
#7359=EDGE_LOOP('',(#30730,#30731,#30732,#30733));
#7360=EDGE_LOOP('',(#30734,#30735,#30736,#30737));
#7361=EDGE_LOOP('',(#30738,#30739,#30740,#30741));
#7362=EDGE_LOOP('',(#30742,#30743,#30744,#30745));
#7363=EDGE_LOOP('',(#30746,#30747,#30748,#30749));
#7364=EDGE_LOOP('',(#30750,#30751,#30752,#30753));
#7365=EDGE_LOOP('',(#30754,#30755,#30756,#30757));
#7366=EDGE_LOOP('',(#30758,#30759,#30760,#30761,#30762,#30763));
#7367=EDGE_LOOP('',(#30764,#30765,#30766,#30767));
#7368=EDGE_LOOP('',(#30768,#30769,#30770));
#7369=EDGE_LOOP('',(#30771,#30772,#30773,#30774));
#7370=EDGE_LOOP('',(#30775,#30776,#30777,#30778));
#7371=EDGE_LOOP('',(#30779,#30780,#30781));
#7372=EDGE_LOOP('',(#30782,#30783,#30784,#30785));
#7373=EDGE_LOOP('',(#30786,#30787,#30788));
#7374=EDGE_LOOP('',(#30789,#30790,#30791,#30792));
#7375=EDGE_LOOP('',(#30793,#30794,#30795));
#7376=EDGE_LOOP('',(#30796,#30797,#30798,#30799));
#7377=EDGE_LOOP('',(#30800,#30801,#30802));
#7378=EDGE_LOOP('',(#30803,#30804,#30805,#30806));
#7379=EDGE_LOOP('',(#30807,#30808,#30809));
#7380=EDGE_LOOP('',(#30810,#30811,#30812,#30813));
#7381=EDGE_LOOP('',(#30814,#30815,#30816,#30817));
#7382=EDGE_LOOP('',(#30818,#30819,#30820,#30821));
#7383=EDGE_LOOP('',(#30822,#30823,#30824,#30825));
#7384=EDGE_LOOP('',(#30826,#30827,#30828,#30829));
#7385=EDGE_LOOP('',(#30830,#30831,#30832,#30833,#30834,#30835,#30836,#30837,
#30838,#30839,#30840));
#7386=EDGE_LOOP('',(#30841,#30842,#30843,#30844));
#7387=EDGE_LOOP('',(#30845,#30846,#30847,#30848));
#7388=EDGE_LOOP('',(#30849,#30850,#30851,#30852));
#7389=EDGE_LOOP('',(#30853,#30854,#30855,#30856));
#7390=EDGE_LOOP('',(#30857,#30858,#30859,#30860));
#7391=EDGE_LOOP('',(#30861,#30862,#30863));
#7392=EDGE_LOOP('',(#30864,#30865,#30866,#30867));
#7393=EDGE_LOOP('',(#30868,#30869,#30870,#30871,#30872,#30873));
#7394=EDGE_LOOP('',(#30874,#30875,#30876,#30877));
#7395=EDGE_LOOP('',(#30878,#30879,#30880,#30881));
#7396=EDGE_LOOP('',(#30882,#30883,#30884,#30885));
#7397=EDGE_LOOP('',(#30886,#30887,#30888,#30889));
#7398=EDGE_LOOP('',(#30890,#30891,#30892,#30893));
#7399=EDGE_LOOP('',(#30894,#30895,#30896,#30897));
#7400=EDGE_LOOP('',(#30898,#30899,#30900,#30901));
#7401=EDGE_LOOP('',(#30902,#30903,#30904,#30905));
#7402=EDGE_LOOP('',(#30906,#30907,#30908));
#7403=EDGE_LOOP('',(#30909,#30910,#30911,#30912));
#7404=EDGE_LOOP('',(#30913,#30914,#30915,#30916,#30917));
#7405=EDGE_LOOP('',(#30918,#30919,#30920,#30921,#30922));
#7406=EDGE_LOOP('',(#30923,#30924,#30925,#30926));
#7407=EDGE_LOOP('',(#30927,#30928,#30929,#30930));
#7408=EDGE_LOOP('',(#30931,#30932,#30933));
#7409=EDGE_LOOP('',(#30934,#30935,#30936,#30937));
#7410=EDGE_LOOP('',(#30938,#30939,#30940,#30941));
#7411=EDGE_LOOP('',(#30942,#30943,#30944,#30945));
#7412=EDGE_LOOP('',(#30946,#30947,#30948));
#7413=EDGE_LOOP('',(#30949,#30950,#30951,#30952));
#7414=EDGE_LOOP('',(#30953,#30954,#30955,#30956));
#7415=EDGE_LOOP('',(#30957,#30958,#30959,#30960,#30961));
#7416=EDGE_LOOP('',(#30962,#30963,#30964,#30965));
#7417=EDGE_LOOP('',(#30966,#30967,#30968,#30969));
#7418=EDGE_LOOP('',(#30970,#30971,#30972));
#7419=EDGE_LOOP('',(#30973,#30974,#30975,#30976));
#7420=EDGE_LOOP('',(#30977,#30978,#30979,#30980));
#7421=EDGE_LOOP('',(#30981,#30982,#30983,#30984));
#7422=EDGE_LOOP('',(#30985,#30986,#30987,#30988,#30989));
#7423=EDGE_LOOP('',(#30990,#30991,#30992));
#7424=EDGE_LOOP('',(#30993,#30994,#30995,#30996));
#7425=EDGE_LOOP('',(#30997,#30998,#30999,#31000));
#7426=EDGE_LOOP('',(#31001,#31002,#31003,#31004));
#7427=EDGE_LOOP('',(#31005,#31006,#31007,#31008));
#7428=EDGE_LOOP('',(#31009,#31010,#31011,#31012,#31013,#31014,#31015,#31016));
#7429=EDGE_LOOP('',(#31017,#31018,#31019,#31020));
#7430=EDGE_LOOP('',(#31021,#31022,#31023));
#7431=EDGE_LOOP('',(#31024,#31025,#31026,#31027));
#7432=EDGE_LOOP('',(#31028,#31029,#31030,#31031));
#7433=EDGE_LOOP('',(#31032,#31033,#31034,#31035));
#7434=EDGE_LOOP('',(#31036,#31037,#31038,#31039));
#7435=EDGE_LOOP('',(#31040,#31041,#31042,#31043));
#7436=EDGE_LOOP('',(#31044,#31045,#31046,#31047));
#7437=EDGE_LOOP('',(#31048,#31049,#31050,#31051));
#7438=EDGE_LOOP('',(#31052,#31053,#31054));
#7439=EDGE_LOOP('',(#31055,#31056,#31057,#31058));
#7440=EDGE_LOOP('',(#31059,#31060,#31061,#31062));
#7441=EDGE_LOOP('',(#31063,#31064,#31065,#31066,#31067,#31068));
#7442=EDGE_LOOP('',(#31069,#31070,#31071,#31072,#31073,#31074,#31075,#31076));
#7443=EDGE_LOOP('',(#31077,#31078,#31079,#31080));
#7444=EDGE_LOOP('',(#31081,#31082,#31083,#31084));
#7445=EDGE_LOOP('',(#31085,#31086,#31087,#31088));
#7446=EDGE_LOOP('',(#31089,#31090,#31091,#31092));
#7447=EDGE_LOOP('',(#31093,#31094,#31095,#31096));
#7448=EDGE_LOOP('',(#31097,#31098,#31099,#31100));
#7449=EDGE_LOOP('',(#31101,#31102,#31103,#31104));
#7450=EDGE_LOOP('',(#31105,#31106,#31107,#31108));
#7451=EDGE_LOOP('',(#31109,#31110,#31111,#31112));
#7452=EDGE_LOOP('',(#31113,#31114,#31115,#31116));
#7453=EDGE_LOOP('',(#31117,#31118,#31119,#31120));
#7454=EDGE_LOOP('',(#31121,#31122,#31123,#31124));
#7455=EDGE_LOOP('',(#31125,#31126,#31127,#31128));
#7456=EDGE_LOOP('',(#31129,#31130,#31131,#31132));
#7457=EDGE_LOOP('',(#31133,#31134,#31135,#31136));
#7458=EDGE_LOOP('',(#31137,#31138,#31139,#31140));
#7459=EDGE_LOOP('',(#31141,#31142,#31143,#31144,#31145,#31146,#31147,#31148,
#31149,#31150,#31151,#31152,#31153,#31154,#31155,#31156,#31157,#31158,#31159,
#31160));
#7460=EDGE_LOOP('',(#31161,#31162,#31163,#31164,#31165));
#7461=EDGE_LOOP('',(#31166,#31167,#31168,#31169,#31170,#31171));
#7462=EDGE_LOOP('',(#31172,#31173,#31174,#31175));
#7463=EDGE_LOOP('',(#31176,#31177,#31178,#31179));
#7464=EDGE_LOOP('',(#31180,#31181,#31182,#31183));
#7465=EDGE_LOOP('',(#31184,#31185,#31186,#31187,#31188));
#7466=EDGE_LOOP('',(#31189,#31190,#31191,#31192));
#7467=EDGE_LOOP('',(#31193,#31194,#31195,#31196));
#7468=EDGE_LOOP('',(#31197,#31198,#31199,#31200,#31201,#31202,#31203,#31204,
#31205));
#7469=EDGE_LOOP('',(#31206,#31207,#31208,#31209));
#7470=EDGE_LOOP('',(#31210,#31211,#31212,#31213));
#7471=EDGE_LOOP('',(#31214,#31215,#31216,#31217,#31218,#31219));
#7472=EDGE_LOOP('',(#31220,#31221,#31222,#31223,#31224));
#7473=EDGE_LOOP('',(#31225,#31226,#31227,#31228));
#7474=EDGE_LOOP('',(#31229,#31230,#31231,#31232));
#7475=EDGE_LOOP('',(#31233,#31234,#31235,#31236,#31237));
#7476=EDGE_LOOP('',(#31238,#31239,#31240,#31241));
#7477=EDGE_LOOP('',(#31242,#31243,#31244,#31245));
#7478=EDGE_LOOP('',(#31246,#31247,#31248,#31249));
#7479=EDGE_LOOP('',(#31250,#31251,#31252,#31253,#31254,#31255,#31256,#31257,
#31258));
#7480=EDGE_LOOP('',(#31259,#31260,#31261,#31262));
#7481=EDGE_LOOP('',(#31263,#31264,#31265,#31266));
#7482=EDGE_LOOP('',(#31267,#31268,#31269,#31270,#31271));
#7483=EDGE_LOOP('',(#31272,#31273,#31274,#31275));
#7484=EDGE_LOOP('',(#31276,#31277,#31278,#31279));
#7485=EDGE_LOOP('',(#31280,#31281,#31282,#31283,#31284));
#7486=EDGE_LOOP('',(#31285,#31286,#31287,#31288,#31289));
#7487=EDGE_LOOP('',(#31290,#31291,#31292,#31293,#31294,#31295));
#7488=EDGE_LOOP('',(#31296,#31297,#31298,#31299));
#7489=EDGE_LOOP('',(#31300,#31301,#31302,#31303));
#7490=EDGE_LOOP('',(#31304,#31305,#31306,#31307));
#7491=EDGE_LOOP('',(#31308,#31309,#31310,#31311));
#7492=EDGE_LOOP('',(#31312,#31313,#31314,#31315));
#7493=EDGE_LOOP('',(#31316,#31317,#31318,#31319));
#7494=EDGE_LOOP('',(#31320,#31321,#31322,#31323,#31324));
#7495=EDGE_LOOP('',(#31325,#31326,#31327,#31328,#31329,#31330,#31331,#31332,
#31333,#31334));
#7496=EDGE_LOOP('',(#31335,#31336,#31337,#31338,#31339,#31340));
#7497=EDGE_LOOP('',(#31341,#31342,#31343,#31344,#31345));
#7498=EDGE_LOOP('',(#31346,#31347,#31348,#31349));
#7499=EDGE_LOOP('',(#31350,#31351,#31352,#31353));
#7500=EDGE_LOOP('',(#31354,#31355,#31356,#31357));
#7501=EDGE_LOOP('',(#31358,#31359,#31360,#31361));
#7502=EDGE_LOOP('',(#31362,#31363,#31364,#31365));
#7503=EDGE_LOOP('',(#31366,#31367,#31368,#31369));
#7504=EDGE_LOOP('',(#31370,#31371,#31372,#31373));
#7505=EDGE_LOOP('',(#31374,#31375,#31376,#31377));
#7506=EDGE_LOOP('',(#31378));
#7507=EDGE_LOOP('',(#31379,#31380,#31381,#31382));
#7508=EDGE_LOOP('',(#31383,#31384,#31385,#31386,#31387,#31388,#31389,#31390,
#31391,#31392,#31393,#31394,#31395,#31396,#31397,#31398,#31399,#31400,#31401,
#31402,#31403,#31404,#31405,#31406,#31407,#31408,#31409,#31410,#31411,#31412));
#7509=EDGE_LOOP('',(#31413));
#7510=EDGE_LOOP('',(#31414,#31415,#31416,#31417));
#7511=EDGE_LOOP('',(#31418,#31419,#31420,#31421,#31422,#31423,#31424,#31425,
#31426,#31427,#31428,#31429,#31430,#31431,#31432,#31433,#31434,#31435,#31436,
#31437,#31438,#31439));
#7512=EDGE_LOOP('',(#31440,#31441,#31442,#31443,#31444,#31445,#31446,#31447));
#7513=EDGE_LOOP('',(#31448,#31449,#31450,#31451,#31452));
#7514=EDGE_LOOP('',(#31453,#31454,#31455,#31456,#31457,#31458));
#7515=EDGE_LOOP('',(#31459,#31460,#31461));
#7516=EDGE_LOOP('',(#31462,#31463,#31464,#31465));
#7517=EDGE_LOOP('',(#31466,#31467,#31468,#31469));
#7518=EDGE_LOOP('',(#31470,#31471,#31472,#31473));
#7519=EDGE_LOOP('',(#31474,#31475,#31476));
#7520=EDGE_LOOP('',(#31477,#31478,#31479));
#7521=EDGE_LOOP('',(#31480,#31481,#31482,#31483,#31484));
#7522=EDGE_LOOP('',(#31485,#31486,#31487,#31488));
#7523=EDGE_LOOP('',(#31489,#31490,#31491,#31492));
#7524=EDGE_LOOP('',(#31493,#31494,#31495));
#7525=EDGE_LOOP('',(#31496,#31497,#31498,#31499,#31500));
#7526=EDGE_LOOP('',(#31501,#31502,#31503));
#7527=EDGE_LOOP('',(#31504,#31505,#31506,#31507));
#7528=EDGE_LOOP('',(#31508,#31509,#31510,#31511));
#7529=EDGE_LOOP('',(#31512,#31513,#31514));
#7530=EDGE_LOOP('',(#31515,#31516,#31517));
#7531=EDGE_LOOP('',(#31518,#31519,#31520,#31521,#31522,#31523));
#7532=EDGE_LOOP('',(#31524,#31525,#31526,#31527));
#7533=EDGE_LOOP('',(#31528,#31529,#31530,#31531));
#7534=EDGE_LOOP('',(#31532,#31533,#31534,#31535));
#7535=EDGE_LOOP('',(#31536,#31537,#31538));
#7536=EDGE_LOOP('',(#31539,#31540));
#7537=EDGE_LOOP('',(#31541,#31542));
#7538=EDGE_LOOP('',(#31543,#31544,#31545,#31546));
#7539=EDGE_LOOP('',(#31547,#31548,#31549,#31550));
#7540=EDGE_LOOP('',(#31551,#31552,#31553,#31554));
#7541=EDGE_LOOP('',(#31555,#31556,#31557,#31558));
#7542=EDGE_LOOP('',(#31559,#31560,#31561,#31562));
#7543=EDGE_LOOP('',(#31563,#31564,#31565,#31566));
#7544=EDGE_LOOP('',(#31567,#31568,#31569,#31570));
#7545=EDGE_LOOP('',(#31571,#31572,#31573,#31574));
#7546=EDGE_LOOP('',(#31575,#31576,#31577,#31578));
#7547=EDGE_LOOP('',(#31579,#31580,#31581,#31582,#31583));
#7548=EDGE_LOOP('',(#31584,#31585,#31586));
#7549=EDGE_LOOP('',(#31587,#31588,#31589,#31590));
#7550=EDGE_LOOP('',(#31591,#31592,#31593,#31594));
#7551=EDGE_LOOP('',(#31595,#31596,#31597,#31598));
#7552=EDGE_LOOP('',(#31599,#31600,#31601,#31602));
#7553=EDGE_LOOP('',(#31603,#31604,#31605,#31606));
#7554=EDGE_LOOP('',(#31607,#31608,#31609,#31610));
#7555=EDGE_LOOP('',(#31611,#31612,#31613));
#7556=EDGE_LOOP('',(#31614,#31615,#31616));
#7557=EDGE_LOOP('',(#31617,#31618,#31619,#31620));
#7558=EDGE_LOOP('',(#31621,#31622,#31623,#31624));
#7559=EDGE_LOOP('',(#31625,#31626,#31627));
#7560=EDGE_LOOP('',(#31628,#31629,#31630,#31631));
#7561=EDGE_LOOP('',(#31632,#31633,#31634,#31635));
#7562=EDGE_LOOP('',(#31636,#31637,#31638,#31639));
#7563=EDGE_LOOP('',(#31640,#31641,#31642,#31643,#31644,#31645,#31646,#31647,
#31648,#31649,#31650,#31651,#31652,#31653,#31654,#31655,#31656,#31657,#31658,
#31659,#31660,#31661,#31662,#31663,#31664,#31665));
#7564=EDGE_LOOP('',(#31666,#31667,#31668,#31669));
#7565=EDGE_LOOP('',(#31670,#31671,#31672,#31673,#31674,#31675,#31676,#31677,
#31678,#31679,#31680,#31681,#31682,#31683,#31684,#31685,#31686,#31687,#31688,
#31689,#31690,#31691,#31692,#31693,#31694,#31695,#31696,#31697,#31698,#31699,
#31700,#31701,#31702,#31703,#31704,#31705,#31706,#31707));
#7566=EDGE_LOOP('',(#31708,#31709,#31710,#31711));
#7567=EDGE_LOOP('',(#31712,#31713,#31714,#31715));
#7568=EDGE_LOOP('',(#31716,#31717,#31718,#31719));
#7569=EDGE_LOOP('',(#31720,#31721,#31722,#31723));
#7570=EDGE_LOOP('',(#31724,#31725,#31726,#31727));
#7571=EDGE_LOOP('',(#31728,#31729,#31730,#31731));
#7572=EDGE_LOOP('',(#31732,#31733,#31734,#31735));
#7573=EDGE_LOOP('',(#31736,#31737,#31738,#31739));
#7574=EDGE_LOOP('',(#31740,#31741,#31742,#31743));
#7575=EDGE_LOOP('',(#31744,#31745,#31746,#31747));
#7576=EDGE_LOOP('',(#31748,#31749,#31750,#31751));
#7577=EDGE_LOOP('',(#31752,#31753,#31754,#31755));
#7578=EDGE_LOOP('',(#31756,#31757,#31758,#31759));
#7579=EDGE_LOOP('',(#31760,#31761,#31762,#31763));
#7580=EDGE_LOOP('',(#31764,#31765,#31766,#31767));
#7581=EDGE_LOOP('',(#31768,#31769,#31770,#31771));
#7582=EDGE_LOOP('',(#31772,#31773,#31774,#31775));
#7583=EDGE_LOOP('',(#31776,#31777,#31778,#31779));
#7584=EDGE_LOOP('',(#31780,#31781,#31782,#31783));
#7585=EDGE_LOOP('',(#31784,#31785,#31786,#31787));
#7586=EDGE_LOOP('',(#31788,#31789,#31790,#31791));
#7587=EDGE_LOOP('',(#31792,#31793,#31794,#31795));
#7588=EDGE_LOOP('',(#31796,#31797,#31798,#31799));
#7589=EDGE_LOOP('',(#31800,#31801,#31802,#31803));
#7590=EDGE_LOOP('',(#31804,#31805,#31806,#31807));
#7591=EDGE_LOOP('',(#31808,#31809,#31810,#31811));
#7592=EDGE_LOOP('',(#31812,#31813,#31814));
#7593=EDGE_LOOP('',(#31815,#31816,#31817,#31818,#31819));
#7594=EDGE_LOOP('',(#31820,#31821,#31822,#31823,#31824,#31825));
#7595=EDGE_LOOP('',(#31826,#31827,#31828));
#7596=EDGE_LOOP('',(#31829,#31830,#31831));
#7597=EDGE_LOOP('',(#31832,#31833,#31834,#31835,#31836,#31837));
#7598=EDGE_LOOP('',(#31838,#31839,#31840,#31841,#31842,#31843,#31844,#31845,
#31846,#31847,#31848,#31849));
#7599=EDGE_LOOP('',(#31850,#31851,#31852,#31853,#31854));
#7600=EDGE_LOOP('',(#31855,#31856,#31857,#31858,#31859));
#7601=EDGE_LOOP('',(#31860,#31861,#31862,#31863,#31864,#31865));
#7602=EDGE_LOOP('',(#31866,#31867));
#7603=EDGE_LOOP('',(#31868,#31869,#31870,#31871,#31872,#31873));
#7604=EDGE_LOOP('',(#31874,#31875,#31876,#31877,#31878));
#7605=EDGE_LOOP('',(#31879,#31880,#31881,#31882,#31883));
#7606=EDGE_LOOP('',(#31884,#31885,#31886,#31887,#31888,#31889));
#7607=EDGE_LOOP('',(#31890,#31891,#31892,#31893,#31894,#31895));
#7608=EDGE_LOOP('',(#31896,#31897));
#7609=EDGE_LOOP('',(#31898,#31899,#31900,#31901,#31902));
#7610=EDGE_LOOP('',(#31903,#31904,#31905));
#7611=EDGE_LOOP('',(#31906,#31907,#31908,#31909));
#7612=EDGE_LOOP('',(#31910,#31911,#31912,#31913));
#7613=EDGE_LOOP('',(#31914,#31915,#31916,#31917));
#7614=EDGE_LOOP('',(#31918,#31919,#31920,#31921));
#7615=EDGE_LOOP('',(#31922,#31923,#31924,#31925));
#7616=EDGE_LOOP('',(#31926,#31927,#31928,#31929));
#7617=EDGE_LOOP('',(#31930,#31931,#31932,#31933));
#7618=EDGE_LOOP('',(#31934,#31935,#31936,#31937));
#7619=EDGE_LOOP('',(#31938));
#7620=EDGE_LOOP('',(#31939,#31940,#31941,#31942));
#7621=EDGE_LOOP('',(#31943,#31944,#31945));
#7622=EDGE_LOOP('',(#31946,#31947,#31948,#31949));
#7623=EDGE_LOOP('',(#31950,#31951,#31952,#31953,#31954));
#7624=EDGE_LOOP('',(#31955,#31956,#31957,#31958));
#7625=EDGE_LOOP('',(#31959,#31960,#31961,#31962));
#7626=EDGE_LOOP('',(#31963,#31964,#31965,#31966));
#7627=EDGE_LOOP('',(#31967,#31968,#31969));
#7628=EDGE_LOOP('',(#31970,#31971,#31972,#31973));
#7629=EDGE_LOOP('',(#31974,#31975,#31976,#31977,#31978));
#7630=EDGE_LOOP('',(#31979,#31980,#31981,#31982,#31983,#31984,#31985,#31986,
#31987,#31988,#31989,#31990,#31991,#31992,#31993,#31994,#31995,#31996,#31997,
#31998,#31999,#32000,#32001,#32002,#32003,#32004));
#7631=EDGE_LOOP('',(#32005));
#7632=EDGE_LOOP('',(#32006,#32007,#32008,#32009));
#7633=EDGE_LOOP('',(#32010,#32011,#32012,#32013));
#7634=EDGE_LOOP('',(#32014));
#7635=EDGE_LOOP('',(#32015,#32016,#32017,#32018));
#7636=EDGE_LOOP('',(#32019,#32020,#32021,#32022));
#7637=LINE('',#49115,#9477);
#7638=LINE('',#49122,#9478);
#7639=LINE('',#49127,#9479);
#7640=LINE('',#49134,#9480);
#7641=LINE('',#49138,#9481);
#7642=LINE('',#49143,#9482);
#7643=LINE('',#49151,#9483);
#7644=LINE('',#49155,#9484);
#7645=LINE('',#49159,#9485);
#7646=LINE('',#49167,#9486);
#7647=LINE('',#49171,#9487);
#7648=LINE('',#49175,#9488);
#7649=LINE('',#49183,#9489);
#7650=LINE('',#49191,#9490);
#7651=LINE('',#49195,#9491);
#7652=LINE('',#49199,#9492);
#7653=LINE('',#49207,#9493);
#7654=LINE('',#49211,#9494);
#7655=LINE('',#49215,#9495);
#7656=LINE('',#49273,#9496);
#7657=LINE('',#49291,#9497);
#7658=LINE('',#49298,#9498);
#7659=LINE('',#49301,#9499);
#7660=LINE('',#49386,#9500);
#7661=LINE('',#49398,#9501);
#7662=LINE('',#49460,#9502);
#7663=LINE('',#49462,#9503);
#7664=LINE('',#49464,#9504);
#7665=LINE('',#49465,#9505);
#7666=LINE('',#49485,#9506);
#7667=LINE('',#49521,#9507);
#7668=LINE('',#49524,#9508);
#7669=LINE('',#49538,#9509);
#7670=LINE('',#49539,#9510);
#7671=LINE('',#49542,#9511);
#7672=LINE('',#49624,#9512);
#7673=LINE('',#49759,#9513);
#7674=LINE('',#49822,#9514);
#7675=LINE('',#49886,#9515);
#7676=LINE('',#49951,#9516);
#7677=LINE('',#50022,#9517);
#7678=LINE('',#50066,#9518);
#7679=LINE('',#50086,#9519);
#7680=LINE('',#50120,#9520);
#7681=LINE('',#50184,#9521);
#7682=LINE('',#50294,#9522);
#7683=LINE('',#50371,#9523);
#7684=LINE('',#50568,#9524);
#7685=LINE('',#50637,#9525);
#7686=LINE('',#50875,#9526);
#7687=LINE('',#50921,#9527);
#7688=LINE('',#50927,#9528);
#7689=LINE('',#50930,#9529);
#7690=LINE('',#50940,#9530);
#7691=LINE('',#50945,#9531);
#7692=LINE('',#50948,#9532);
#7693=LINE('',#50949,#9533);
#7694=LINE('',#50956,#9534);
#7695=LINE('',#50961,#9535);
#7696=LINE('',#50964,#9536);
#7697=LINE('',#50965,#9537);
#7698=LINE('',#50972,#9538);
#7699=LINE('',#50977,#9539);
#7700=LINE('',#50980,#9540);
#7701=LINE('',#50981,#9541);
#7702=LINE('',#50988,#9542);
#7703=LINE('',#50996,#9543);
#7704=LINE('',#51004,#9544);
#7705=LINE('',#51009,#9545);
#7706=LINE('',#51012,#9546);
#7707=LINE('',#51013,#9547);
#7708=LINE('',#51020,#9548);
#7709=LINE('',#51028,#9549);
#7710=LINE('',#51036,#9550);
#7711=LINE('',#51041,#9551);
#7712=LINE('',#51044,#9552);
#7713=LINE('',#51045,#9553);
#7714=LINE('',#51052,#9554);
#7715=LINE('',#51057,#9555);
#7716=LINE('',#51060,#9556);
#7717=LINE('',#51061,#9557);
#7718=LINE('',#51068,#9558);
#7719=LINE('',#51073,#9559);
#7720=LINE('',#51076,#9560);
#7721=LINE('',#51077,#9561);
#7722=LINE('',#51084,#9562);
#7723=LINE('',#51091,#9563);
#7724=LINE('',#51100,#9564);
#7725=LINE('',#51105,#9565);
#7726=LINE('',#51108,#9566);
#7727=LINE('',#51109,#9567);
#7728=LINE('',#51116,#9568);
#7729=LINE('',#51121,#9569);
#7730=LINE('',#51124,#9570);
#7731=LINE('',#51125,#9571);
#7732=LINE('',#51132,#9572);
#7733=LINE('',#51137,#9573);
#7734=LINE('',#51140,#9574);
#7735=LINE('',#51141,#9575);
#7736=LINE('',#51148,#9576);
#7737=LINE('',#51156,#9577);
#7738=LINE('',#51164,#9578);
#7739=LINE('',#51169,#9579);
#7740=LINE('',#51172,#9580);
#7741=LINE('',#51173,#9581);
#7742=LINE('',#51180,#9582);
#7743=LINE('',#51188,#9583);
#7744=LINE('',#51196,#9584);
#7745=LINE('',#51201,#9585);
#7746=LINE('',#51204,#9586);
#7747=LINE('',#51205,#9587);
#7748=LINE('',#51212,#9588);
#7749=LINE('',#51217,#9589);
#7750=LINE('',#51220,#9590);
#7751=LINE('',#51221,#9591);
#7752=LINE('',#51229,#9592);
#7753=LINE('',#51236,#9593);
#7754=LINE('',#51239,#9594);
#7755=LINE('',#51241,#9595);
#7756=LINE('',#51245,#9596);
#7757=LINE('',#51247,#9597);
#7758=LINE('',#51249,#9598);
#7759=LINE('',#51250,#9599);
#7760=LINE('',#51265,#9600);
#7761=LINE('',#51278,#9601);
#7762=LINE('',#51331,#9602);
#7763=LINE('',#51332,#9603);
#7764=LINE('',#51335,#9604);
#7765=LINE('',#51356,#9605);
#7766=LINE('',#51458,#9606);
#7767=LINE('',#51528,#9607);
#7768=LINE('',#51532,#9608);
#7769=LINE('',#51596,#9609);
#7770=LINE('',#51666,#9610);
#7771=LINE('',#51693,#9611);
#7772=LINE('',#51820,#9612);
#7773=LINE('',#51821,#9613);
#7774=LINE('',#51822,#9614);
#7775=LINE('',#51825,#9615);
#7776=LINE('',#51827,#9616);
#7777=LINE('',#51828,#9617);
#7778=LINE('',#52044,#9618);
#7779=LINE('',#53277,#9619);
#7780=LINE('',#53285,#9620);
#7781=LINE('',#53459,#9621);
#7782=LINE('',#54081,#9622);
#7783=LINE('',#54817,#9623);
#7784=LINE('',#54825,#9624);
#7785=LINE('',#54833,#9625);
#7786=LINE('',#54849,#9626);
#7787=LINE('',#54865,#9627);
#7788=LINE('',#54873,#9628);
#7789=LINE('',#54881,#9629);
#7790=LINE('',#54897,#9630);
#7791=LINE('',#54905,#9631);
#7792=LINE('',#54913,#9632);
#7793=LINE('',#54929,#9633);
#7794=LINE('',#54945,#9634);
#7795=LINE('',#54953,#9635);
#7796=LINE('',#54963,#9636);
#7797=LINE('',#54966,#9637);
#7798=LINE('',#54970,#9638);
#7799=LINE('',#54974,#9639);
#7800=LINE('',#54978,#9640);
#7801=LINE('',#54982,#9641);
#7802=LINE('',#54987,#9642);
#7803=LINE('',#54991,#9643);
#7804=LINE('',#54995,#9644);
#7805=LINE('',#54999,#9645);
#7806=LINE('',#55003,#9646);
#7807=LINE('',#55005,#9647);
#7808=LINE('',#55009,#9648);
#7809=LINE('',#55010,#9649);
#7810=LINE('',#55013,#9650);
#7811=LINE('',#55014,#9651);
#7812=LINE('',#55018,#9652);
#7813=LINE('',#55021,#9653);
#7814=LINE('',#55022,#9654);
#7815=LINE('',#55027,#9655);
#7816=LINE('',#55029,#9656);
#7817=LINE('',#55030,#9657);
#7818=LINE('',#55036,#9658);
#7819=LINE('',#55039,#9659);
#7820=LINE('',#55040,#9660);
#7821=LINE('',#55044,#9661);
#7822=LINE('',#55047,#9662);
#7823=LINE('',#55048,#9663);
#7824=LINE('',#55052,#9664);
#7825=LINE('',#55055,#9665);
#7826=LINE('',#55056,#9666);
#7827=LINE('',#55060,#9667);
#7828=LINE('',#55063,#9668);
#7829=LINE('',#55064,#9669);
#7830=LINE('',#55068,#9670);
#7831=LINE('',#55070,#9671);
#7832=LINE('',#55084,#9672);
#7833=LINE('',#55108,#9673);
#7834=LINE('',#55122,#9674);
#7835=LINE('',#55135,#9675);
#7836=LINE('',#55136,#9676);
#7837=LINE('',#55150,#9677);
#7838=LINE('',#55158,#9678);
#7839=LINE('',#55206,#9679);
#7840=LINE('',#55284,#9680);
#7841=LINE('',#55310,#9681);
#7842=LINE('',#55364,#9682);
#7843=LINE('',#55409,#9683);
#7844=LINE('',#55552,#9684);
#7845=LINE('',#56067,#9685);
#7846=LINE('',#56157,#9686);
#7847=LINE('',#56161,#9687);
#7848=LINE('',#56188,#9688);
#7849=LINE('',#56221,#9689);
#7850=LINE('',#56329,#9690);
#7851=LINE('',#56362,#9691);
#7852=LINE('',#57611,#9692);
#7853=LINE('',#57667,#9693);
#7854=LINE('',#57687,#9694);
#7855=LINE('',#57702,#9695);
#7856=LINE('',#57717,#9696);
#7857=LINE('',#57732,#9697);
#7858=LINE('',#57752,#9698);
#7859=LINE('',#57767,#9699);
#7860=LINE('',#57782,#9700);
#7861=LINE('',#57797,#9701);
#7862=LINE('',#57812,#9702);
#7863=LINE('',#57832,#9703);
#7864=LINE('',#57847,#9704);
#7865=LINE('',#57881,#9705);
#7866=LINE('',#57882,#9706);
#7867=LINE('',#57885,#9707);
#7868=LINE('',#57889,#9708);
#7869=LINE('',#57894,#9709);
#7870=LINE('',#57898,#9710);
#7871=LINE('',#57902,#9711);
#7872=LINE('',#59325,#9712);
#7873=LINE('',#59592,#9713);
#7874=LINE('',#61893,#9714);
#7875=LINE('',#62811,#9715);
#7876=LINE('',#63497,#9716);
#7877=LINE('',#63498,#9717);
#7878=LINE('',#63912,#9718);
#7879=LINE('',#64113,#9719);
#7880=LINE('',#64470,#9720);
#7881=LINE('',#64917,#9721);
#7882=LINE('',#65044,#9722);
#7883=LINE('',#65184,#9723);
#7884=LINE('',#65218,#9724);
#7885=LINE('',#65221,#9725);
#7886=LINE('',#65254,#9726);
#7887=LINE('',#65617,#9727);
#7888=LINE('',#65618,#9728);
#7889=LINE('',#65760,#9729);
#7890=LINE('',#65995,#9730);
#7891=LINE('',#66249,#9731);
#7892=LINE('',#66573,#9732);
#7893=LINE('',#66700,#9733);
#7894=LINE('',#67207,#9734);
#7895=LINE('',#67208,#9735);
#7896=LINE('',#67406,#9736);
#7897=LINE('',#67823,#9737);
#7898=LINE('',#67921,#9738);
#7899=LINE('',#68118,#9739);
#7900=LINE('',#68122,#9740);
#7901=LINE('',#68125,#9741);
#7902=LINE('',#68128,#9742);
#7903=LINE('',#68268,#9743);
#7904=LINE('',#68395,#9744);
#7905=LINE('',#68950,#9745);
#7906=LINE('',#68951,#9746);
#7907=LINE('',#69125,#9747);
#7908=LINE('',#69265,#9748);
#7909=LINE('',#69405,#9749);
#7910=LINE('',#69579,#9750);
#7911=LINE('',#69812,#9751);
#7912=LINE('',#70133,#9752);
#7913=LINE('',#70654,#9753);
#7914=LINE('',#70781,#9754);
#7915=LINE('',#71450,#9755);
#7916=LINE('',#71967,#9756);
#7917=LINE('',#72093,#9757);
#7918=LINE('',#72397,#9758);
#7919=LINE('',#72646,#9759);
#7920=LINE('',#72843,#9760);
#7921=LINE('',#72858,#9761);
#7922=LINE('',#72872,#9762);
#7923=LINE('',#72888,#9763);
#7924=LINE('',#72921,#9764);
#7925=LINE('',#72927,#9765);
#7926=LINE('',#73004,#9766);
#7927=LINE('',#73005,#9767);
#7928=LINE('',#73009,#9768);
#7929=LINE('',#73011,#9769);
#7930=LINE('',#73086,#9770);
#7931=LINE('',#73213,#9771);
#7932=LINE('',#73217,#9772);
#7933=LINE('',#73219,#9773);
#7934=LINE('',#73294,#9774);
#7935=LINE('',#73369,#9775);
#7936=LINE('',#73490,#9776);
#7937=LINE('',#73639,#9777);
#7938=LINE('',#73640,#9778);
#7939=LINE('',#73778,#9779);
#7940=LINE('',#73853,#9780);
#7941=LINE('',#73928,#9781);
#7942=LINE('',#74066,#9782);
#7943=LINE('',#74141,#9783);
#7944=LINE('',#74145,#9784);
#7945=LINE('',#74147,#9785);
#7946=LINE('',#74222,#9786);
#7947=LINE('',#74297,#9787);
#7948=LINE('',#74299,#9788);
#7949=LINE('',#74310,#9789);
#7950=LINE('',#74314,#9790);
#7951=LINE('',#74316,#9791);
#7952=LINE('',#74320,#9792);
#7953=LINE('',#74321,#9793);
#7954=LINE('',#74344,#9794);
#7955=LINE('',#74347,#9795);
#7956=LINE('',#74349,#9796);
#7957=LINE('',#74350,#9797);
#7958=LINE('',#74353,#9798);
#7959=LINE('',#74373,#9799);
#7960=LINE('',#74378,#9800);
#7961=LINE('',#74384,#9801);
#7962=LINE('',#74387,#9802);
#7963=LINE('',#74391,#9803);
#7964=LINE('',#74393,#9804);
#7965=LINE('',#74395,#9805);
#7966=LINE('',#74397,#9806);
#7967=LINE('',#74398,#9807);
#7968=LINE('',#74402,#9808);
#7969=LINE('',#74410,#9809);
#7970=LINE('',#74414,#9810);
#7971=LINE('',#74422,#9811);
#7972=LINE('',#74426,#9812);
#7973=LINE('',#74434,#9813);
#7974=LINE('',#74438,#9814);
#7975=LINE('',#74446,#9815);
#7976=LINE('',#74450,#9816);
#7977=LINE('',#74458,#9817);
#7978=LINE('',#74466,#9818);
#7979=LINE('',#74468,#9819);
#7980=LINE('',#74472,#9820);
#7981=LINE('',#74473,#9821);
#7982=LINE('',#74476,#9822);
#7983=LINE('',#74478,#9823);
#7984=LINE('',#74483,#9824);
#7985=LINE('',#74491,#9825);
#7986=LINE('',#74493,#9826);
#7987=LINE('',#74497,#9827);
#7988=LINE('',#74501,#9828);
#7989=LINE('',#74514,#9829);
#7990=LINE('',#74522,#9830);
#7991=LINE('',#74526,#9831);
#7992=LINE('',#74528,#9832);
#7993=LINE('',#74533,#9833);
#7994=LINE('',#74537,#9834);
#7995=LINE('',#74540,#9835);
#7996=LINE('',#74553,#9836);
#7997=LINE('',#74554,#9837);
#7998=LINE('',#74557,#9838);
#7999=LINE('',#74558,#9839);
#8000=LINE('',#74562,#9840);
#8001=LINE('',#74566,#9841);
#8002=LINE('',#74570,#9842);
#8003=LINE('',#74574,#9843);
#8004=LINE('',#74578,#9844);
#8005=LINE('',#74582,#9845);
#8006=LINE('',#74586,#9846);
#8007=LINE('',#74589,#9847);
#8008=LINE('',#74591,#9848);
#8009=LINE('',#74595,#9849);
#8010=LINE('',#74599,#9850);
#8011=LINE('',#74600,#9851);
#8012=LINE('',#74612,#9852);
#8013=LINE('',#74620,#9853);
#8014=LINE('',#74621,#9854);
#8015=LINE('',#74624,#9855);
#8016=LINE('',#74628,#9856);
#8017=LINE('',#74654,#9857);
#8018=LINE('',#74658,#9858);
#8019=LINE('',#74659,#9859);
#8020=LINE('',#74671,#9860);
#8021=LINE('',#74679,#9861);
#8022=LINE('',#74680,#9862);
#8023=LINE('',#74684,#9863);
#8024=LINE('',#74688,#9864);
#8025=LINE('',#74692,#9865);
#8026=LINE('',#74696,#9866);
#8027=LINE('',#74700,#9867);
#8028=LINE('',#74704,#9868);
#8029=LINE('',#74708,#9869);
#8030=LINE('',#74711,#9870);
#8031=LINE('',#74715,#9871);
#8032=LINE('',#74719,#9872);
#8033=LINE('',#74720,#9873);
#8034=LINE('',#74732,#9874);
#8035=LINE('',#74740,#9875);
#8036=LINE('',#74741,#9876);
#8037=LINE('',#74744,#9877);
#8038=LINE('',#74748,#9878);
#8039=LINE('',#74774,#9879);
#8040=LINE('',#74778,#9880);
#8041=LINE('',#74779,#9881);
#8042=LINE('',#74796,#9882);
#8043=LINE('',#74798,#9883);
#8044=LINE('',#74801,#9884);
#8045=LINE('',#74803,#9885);
#8046=LINE('',#74811,#9886);
#8047=LINE('',#74813,#9887);
#8048=LINE('',#74814,#9888);
#8049=LINE('',#74817,#9889);
#8050=LINE('',#74827,#9890);
#8051=LINE('',#74838,#9891);
#8052=LINE('',#74841,#9892);
#8053=LINE('',#74842,#9893);
#8054=LINE('',#74845,#9894);
#8055=LINE('',#74847,#9895);
#8056=LINE('',#74849,#9896);
#8057=LINE('',#74850,#9897);
#8058=LINE('',#74853,#9898);
#8059=LINE('',#74855,#9899);
#8060=LINE('',#74856,#9900);
#8061=LINE('',#74859,#9901);
#8062=LINE('',#74863,#9902);
#8063=LINE('',#74865,#9903);
#8064=LINE('',#74866,#9904);
#8065=LINE('',#74869,#9905);
#8066=LINE('',#74870,#9906);
#8067=LINE('',#74873,#9907);
#8068=LINE('',#74881,#9908);
#8069=LINE('',#74885,#9909);
#8070=LINE('',#74887,#9910);
#8071=LINE('',#74891,#9911);
#8072=LINE('',#74894,#9912);
#8073=LINE('',#74897,#9913);
#8074=LINE('',#74898,#9914);
#8075=LINE('',#74901,#9915);
#8076=LINE('',#74907,#9916);
#8077=LINE('',#74909,#9917);
#8078=LINE('',#74910,#9918);
#8079=LINE('',#74913,#9919);
#8080=LINE('',#74914,#9920);
#8081=LINE('',#74918,#9921);
#8082=LINE('',#74923,#9922);
#8083=LINE('',#74932,#9923);
#8084=LINE('',#74936,#9924);
#8085=LINE('',#74937,#9925);
#8086=LINE('',#74941,#9926);
#8087=LINE('',#74945,#9927);
#8088=LINE('',#74949,#9928);
#8089=LINE('',#74953,#9929);
#8090=LINE('',#74956,#9930);
#8091=LINE('',#74961,#9931);
#8092=LINE('',#74963,#9932);
#8093=LINE('',#74966,#9933);
#8094=LINE('',#74969,#9934);
#8095=LINE('',#74972,#9935);
#8096=LINE('',#74973,#9936);
#8097=LINE('',#74976,#9937);
#8098=LINE('',#74978,#9938);
#8099=LINE('',#74979,#9939);
#8100=LINE('',#74982,#9940);
#8101=LINE('',#74988,#9941);
#8102=LINE('',#74989,#9942);
#8103=LINE('',#74993,#9943);
#8104=LINE('',#75003,#9944);
#8105=LINE('',#75009,#9945);
#8106=LINE('',#75012,#9946);
#8107=LINE('',#75013,#9947);
#8108=LINE('',#75017,#9948);
#8109=LINE('',#75019,#9949);
#8110=LINE('',#75021,#9950);
#8111=LINE('',#75022,#9951);
#8112=LINE('',#75024,#9952);
#8113=LINE('',#75026,#9953);
#8114=LINE('',#75027,#9954);
#8115=LINE('',#75031,#9955);
#8116=LINE('',#75035,#9956);
#8117=LINE('',#75037,#9957);
#8118=LINE('',#75038,#9958);
#8119=LINE('',#75040,#9959);
#8120=LINE('',#75042,#9960);
#8121=LINE('',#75043,#9961);
#8122=LINE('',#75046,#9962);
#8123=LINE('',#75047,#9963);
#8124=LINE('',#75048,#9964);
#8125=LINE('',#75051,#9965);
#8126=LINE('',#75054,#9966);
#8127=LINE('',#75055,#9967);
#8128=LINE('',#75057,#9968);
#8129=LINE('',#75060,#9969);
#8130=LINE('',#75061,#9970);
#8131=LINE('',#75064,#9971);
#8132=LINE('',#75066,#9972);
#8133=LINE('',#75068,#9973);
#8134=LINE('',#75070,#9974);
#8135=LINE('',#75072,#9975);
#8136=LINE('',#75074,#9976);
#8137=LINE('',#75075,#9977);
#8138=LINE('',#75079,#9978);
#8139=LINE('',#75082,#9979);
#8140=LINE('',#75084,#9980);
#8141=LINE('',#75086,#9981);
#8142=LINE('',#75088,#9982);
#8143=LINE('',#75090,#9983);
#8144=LINE('',#75091,#9984);
#8145=LINE('',#75094,#9985);
#8146=LINE('',#75096,#9986);
#8147=LINE('',#75122,#9987);
#8148=LINE('',#75146,#9988);
#8149=LINE('',#75161,#9989);
#8150=LINE('',#75163,#9990);
#8151=LINE('',#75185,#9991);
#8152=LINE('',#75207,#9992);
#8153=LINE('',#75212,#9993);
#8154=LINE('',#75221,#9994);
#8155=LINE('',#75230,#9995);
#8156=LINE('',#75258,#9996);
#8157=LINE('',#75266,#9997);
#8158=LINE('',#75269,#9998);
#8159=LINE('',#75273,#9999);
#8160=LINE('',#75277,#10000);
#8161=LINE('',#75282,#10001);
#8162=LINE('',#75286,#10002);
#8163=LINE('',#75293,#10003);
#8164=LINE('',#75296,#10004);
#8165=LINE('',#75300,#10005);
#8166=LINE('',#75304,#10006);
#8167=LINE('',#75305,#10007);
#8168=LINE('',#75312,#10008);
#8169=LINE('',#75326,#10009);
#8170=LINE('',#75335,#10010);
#8171=LINE('',#75366,#10011);
#8172=LINE('',#75371,#10012);
#8173=LINE('',#75374,#10013);
#8174=LINE('',#75378,#10014);
#8175=LINE('',#75382,#10015);
#8176=LINE('',#75387,#10016);
#8177=LINE('',#75391,#10017);
#8178=LINE('',#75394,#10018);
#8179=LINE('',#75396,#10019);
#8180=LINE('',#75441,#10020);
#8181=LINE('',#75445,#10021);
#8182=LINE('',#75448,#10022);
#8183=LINE('',#75451,#10023);
#8184=LINE('',#75453,#10024);
#8185=LINE('',#75458,#10025);
#8186=LINE('',#75462,#10026);
#8187=LINE('',#75469,#10027);
#8188=LINE('',#75472,#10028);
#8189=LINE('',#75476,#10029);
#8190=LINE('',#75482,#10030);
#8191=LINE('',#75487,#10031);
#8192=LINE('',#75489,#10032);
#8193=LINE('',#75492,#10033);
#8194=LINE('',#75505,#10034);
#8195=LINE('',#75509,#10035);
#8196=LINE('',#75514,#10036);
#8197=LINE('',#75547,#10037);
#8198=LINE('',#75551,#10038);
#8199=LINE('',#75554,#10039);
#8200=LINE('',#75556,#10040);
#8201=LINE('',#75600,#10041);
#8202=LINE('',#75602,#10042);
#8203=LINE('',#75606,#10043);
#8204=LINE('',#75610,#10044);
#8205=LINE('',#75617,#10045);
#8206=LINE('',#75620,#10046);
#8207=LINE('',#75624,#10047);
#8208=LINE('',#75628,#10048);
#8209=LINE('',#75631,#10049);
#8210=LINE('',#75636,#10050);
#8211=LINE('',#75639,#10051);
#8212=LINE('',#75640,#10052);
#8213=LINE('',#75644,#10053);
#8214=LINE('',#75648,#10054);
#8215=LINE('',#75650,#10055);
#8216=LINE('',#75653,#10056);
#8217=LINE('',#75658,#10057);
#8218=LINE('',#75666,#10058);
#8219=LINE('',#75667,#10059);
#8220=LINE('',#75671,#10060);
#8221=LINE('',#75697,#10061);
#8222=LINE('',#75747,#10062);
#8223=LINE('',#75785,#10063);
#8224=LINE('',#75805,#10064);
#8225=LINE('',#75835,#10065);
#8226=LINE('',#75865,#10066);
#8227=LINE('',#75866,#10067);
#8228=LINE('',#75870,#10068);
#8229=LINE('',#75875,#10069);
#8230=LINE('',#75876,#10070);
#8231=LINE('',#75896,#10071);
#8232=LINE('',#75925,#10072);
#8233=LINE('',#75927,#10073);
#8234=LINE('',#75981,#10074);
#8235=LINE('',#75995,#10075);
#8236=LINE('',#76021,#10076);
#8237=LINE('',#76071,#10077);
#8238=LINE('',#76075,#10078);
#8239=LINE('',#76079,#10079);
#8240=LINE('',#76083,#10080);
#8241=LINE('',#76088,#10081);
#8242=LINE('',#76093,#10082);
#8243=LINE('',#76102,#10083);
#8244=LINE('',#76107,#10084);
#8245=LINE('',#76113,#10085);
#8246=LINE('',#76122,#10086);
#8247=LINE('',#76123,#10087);
#8248=LINE('',#76129,#10088);
#8249=LINE('',#76135,#10089);
#8250=LINE('',#76138,#10090);
#8251=LINE('',#76140,#10091);
#8252=LINE('',#76141,#10092);
#8253=LINE('',#76144,#10093);
#8254=LINE('',#76162,#10094);
#8255=LINE('',#76180,#10095);
#8256=LINE('',#76183,#10096);
#8257=LINE('',#76187,#10097);
#8258=LINE('',#76237,#10098);
#8259=LINE('',#76273,#10099);
#8260=LINE('',#76366,#10100);
#8261=LINE('',#76372,#10101);
#8262=LINE('',#76411,#10102);
#8263=LINE('',#76486,#10103);
#8264=LINE('',#76519,#10104);
#8265=LINE('',#76553,#10105);
#8266=LINE('',#76609,#10106);
#8267=LINE('',#76616,#10107);
#8268=LINE('',#76679,#10108);
#8269=LINE('',#76681,#10109);
#8270=LINE('',#76785,#10110);
#8271=LINE('',#76811,#10111);
#8272=LINE('',#76920,#10112);
#8273=LINE('',#77018,#10113);
#8274=LINE('',#77074,#10114);
#8275=LINE('',#77132,#10115);
#8276=LINE('',#77217,#10116);
#8277=LINE('',#77279,#10117);
#8278=LINE('',#77293,#10118);
#8279=LINE('',#77297,#10119);
#8280=LINE('',#77317,#10120);
#8281=LINE('',#77340,#10121);
#8282=LINE('',#77378,#10122);
#8283=LINE('',#77413,#10123);
#8284=LINE('',#77460,#10124);
#8285=LINE('',#77464,#10125);
#8286=LINE('',#77467,#10126);
#8287=LINE('',#77468,#10127);
#8288=LINE('',#77518,#10128);
#8289=LINE('',#77519,#10129);
#8290=LINE('',#77549,#10130);
#8291=LINE('',#77550,#10131);
#8292=LINE('',#77554,#10132);
#8293=LINE('',#77557,#10133);
#8294=LINE('',#77558,#10134);
#8295=LINE('',#77564,#10135);
#8296=LINE('',#77602,#10136);
#8297=LINE('',#77622,#10137);
#8298=LINE('',#77669,#10138);
#8299=LINE('',#77719,#10139);
#8300=LINE('',#77736,#10140);
#8301=LINE('',#77756,#10141);
#8302=LINE('',#77760,#10142);
#8303=LINE('',#77763,#10143);
#8304=LINE('',#77767,#10144);
#8305=LINE('',#77768,#10145);
#8306=LINE('',#77771,#10146);
#8307=LINE('',#77776,#10147);
#8308=LINE('',#77823,#10148);
#8309=LINE('',#77869,#10149);
#8310=LINE('',#77870,#10150);
#8311=LINE('',#77905,#10151);
#8312=LINE('',#77907,#10152);
#8313=LINE('',#77932,#10153);
#8314=LINE('',#77961,#10154);
#8315=LINE('',#77963,#10155);
#8316=LINE('',#77969,#10156);
#8317=LINE('',#77970,#10157);
#8318=LINE('',#77974,#10158);
#8319=LINE('',#77977,#10159);
#8320=LINE('',#77978,#10160);
#8321=LINE('',#77982,#10161);
#8322=LINE('',#77986,#10162);
#8323=LINE('',#78006,#10163);
#8324=LINE('',#78053,#10164);
#8325=LINE('',#78082,#10165);
#8326=LINE('',#78131,#10166);
#8327=LINE('',#78133,#10167);
#8328=LINE('',#78135,#10168);
#8329=LINE('',#78137,#10169);
#8330=LINE('',#78140,#10170);
#8331=LINE('',#78142,#10171);
#8332=LINE('',#78144,#10172);
#8333=LINE('',#78145,#10173);
#8334=LINE('',#78148,#10174);
#8335=LINE('',#78150,#10175);
#8336=LINE('',#78152,#10176);
#8337=LINE('',#78154,#10177);
#8338=LINE('',#78155,#10178);
#8339=LINE('',#78158,#10179);
#8340=LINE('',#78160,#10180);
#8341=LINE('',#78162,#10181);
#8342=LINE('',#78164,#10182);
#8343=LINE('',#78165,#10183);
#8344=LINE('',#78168,#10184);
#8345=LINE('',#78170,#10185);
#8346=LINE('',#78172,#10186);
#8347=LINE('',#78173,#10187);
#8348=LINE('',#78176,#10188);
#8349=LINE('',#78178,#10189);
#8350=LINE('',#78180,#10190);
#8351=LINE('',#78181,#10191);
#8352=LINE('',#78184,#10192);
#8353=LINE('',#78186,#10193);
#8354=LINE('',#78188,#10194);
#8355=LINE('',#78190,#10195);
#8356=LINE('',#78191,#10196);
#8357=LINE('',#78194,#10197);
#8358=LINE('',#78196,#10198);
#8359=LINE('',#78198,#10199);
#8360=LINE('',#78200,#10200);
#8361=LINE('',#78201,#10201);
#8362=LINE('',#78204,#10202);
#8363=LINE('',#78206,#10203);
#8364=LINE('',#78208,#10204);
#8365=LINE('',#78209,#10205);
#8366=LINE('',#78214,#10206);
#8367=LINE('',#78220,#10207);
#8368=LINE('',#78227,#10208);
#8369=LINE('',#78232,#10209);
#8370=LINE('',#78235,#10210);
#8371=LINE('',#78239,#10211);
#8372=LINE('',#78243,#10212);
#8373=LINE('',#78250,#10213);
#8374=LINE('',#78256,#10214);
#8375=LINE('',#78264,#10215);
#8376=LINE('',#78277,#10216);
#8377=LINE('',#78279,#10217);
#8378=LINE('',#78281,#10218);
#8379=LINE('',#78289,#10219);
#8380=LINE('',#78290,#10220);
#8381=LINE('',#78294,#10221);
#8382=LINE('',#78306,#10222);
#8383=LINE('',#78323,#10223);
#8384=LINE('',#78326,#10224);
#8385=LINE('',#78328,#10225);
#8386=LINE('',#78334,#10226);
#8387=LINE('',#78336,#10227);
#8388=LINE('',#78337,#10228);
#8389=LINE('',#78343,#10229);
#8390=LINE('',#78350,#10230);
#8391=LINE('',#78360,#10231);
#8392=LINE('',#78366,#10232);
#8393=LINE('',#78368,#10233);
#8394=LINE('',#78370,#10234);
#8395=LINE('',#78378,#10235);
#8396=LINE('',#78379,#10236);
#8397=LINE('',#78383,#10237);
#8398=LINE('',#78390,#10238);
#8399=LINE('',#78398,#10239);
#8400=LINE('',#78406,#10240);
#8401=LINE('',#78418,#10241);
#8402=LINE('',#78420,#10242);
#8403=LINE('',#78422,#10243);
#8404=LINE('',#78424,#10244);
#8405=LINE('',#78426,#10245);
#8406=LINE('',#78428,#10246);
#8407=LINE('',#78430,#10247);
#8408=LINE('',#78432,#10248);
#8409=LINE('',#78435,#10249);
#8410=LINE('',#78441,#10250);
#8411=LINE('',#78449,#10251);
#8412=LINE('',#78463,#10252);
#8413=LINE('',#78465,#10253);
#8414=LINE('',#78473,#10254);
#8415=LINE('',#78475,#10255);
#8416=LINE('',#78476,#10256);
#8417=LINE('',#78480,#10257);
#8418=LINE('',#78493,#10258);
#8419=LINE('',#78509,#10259);
#8420=LINE('',#78512,#10260);
#8421=LINE('',#78514,#10261);
#8422=LINE('',#78520,#10262);
#8423=LINE('',#78522,#10263);
#8424=LINE('',#78523,#10264);
#8425=LINE('',#78528,#10265);
#8426=LINE('',#78532,#10266);
#8427=LINE('',#78542,#10267);
#8428=LINE('',#78544,#10268);
#8429=LINE('',#78552,#10269);
#8430=LINE('',#78554,#10270);
#8431=LINE('',#78556,#10271);
#8432=LINE('',#78561,#10272);
#8433=LINE('',#78577,#10273);
#8434=LINE('',#78587,#10274);
#8435=LINE('',#78591,#10275);
#8436=LINE('',#78602,#10276);
#8437=LINE('',#78604,#10277);
#8438=LINE('',#78606,#10278);
#8439=LINE('',#78608,#10279);
#8440=LINE('',#78610,#10280);
#8441=LINE('',#78611,#10281);
#8442=LINE('',#78613,#10282);
#8443=LINE('',#78615,#10283);
#8444=LINE('',#78618,#10284);
#8445=LINE('',#78621,#10285);
#8446=LINE('',#78996,#10286);
#8447=LINE('',#79068,#10287);
#8448=LINE('',#79139,#10288);
#8449=LINE('',#79165,#10289);
#8450=LINE('',#79756,#10290);
#8451=LINE('',#79763,#10291);
#8452=LINE('',#79767,#10292);
#8453=LINE('',#79771,#10293);
#8454=LINE('',#79774,#10294);
#8455=LINE('',#79779,#10295);
#8456=LINE('',#79788,#10296);
#8457=LINE('',#79804,#10297);
#8458=LINE('',#79820,#10298);
#8459=LINE('',#79883,#10299);
#8460=LINE('',#79885,#10300);
#8461=LINE('',#79923,#10301);
#8462=LINE('',#79963,#10302);
#8463=LINE('',#79967,#10303);
#8464=LINE('',#79968,#10304);
#8465=LINE('',#79972,#10305);
#8466=LINE('',#79975,#10306);
#8467=LINE('',#79976,#10307);
#8468=LINE('',#79980,#10308);
#8469=LINE('',#80087,#10309);
#8470=LINE('',#80089,#10310);
#8471=LINE('',#80091,#10311);
#8472=LINE('',#80092,#10312);
#8473=LINE('',#80212,#10313);
#8474=LINE('',#80213,#10314);
#8475=LINE('',#80238,#10315);
#8476=LINE('',#80243,#10316);
#8477=LINE('',#80251,#10317);
#8478=LINE('',#80259,#10318);
#8479=LINE('',#80322,#10319);
#8480=LINE('',#80326,#10320);
#8481=LINE('',#80334,#10321);
#8482=LINE('',#80338,#10322);
#8483=LINE('',#80341,#10323);
#8484=LINE('',#80343,#10324);
#8485=LINE('',#80345,#10325);
#8486=LINE('',#80347,#10326);
#8487=LINE('',#80460,#10327);
#8488=LINE('',#80477,#10328);
#8489=LINE('',#80481,#10329);
#8490=LINE('',#80483,#10330);
#8491=LINE('',#80485,#10331);
#8492=LINE('',#80489,#10332);
#8493=LINE('',#80491,#10333);
#8494=LINE('',#80493,#10334);
#8495=LINE('',#80497,#10335);
#8496=LINE('',#80501,#10336);
#8497=LINE('',#80505,#10337);
#8498=LINE('',#80509,#10338);
#8499=LINE('',#80515,#10339);
#8500=LINE('',#80519,#10340);
#8501=LINE('',#80522,#10341);
#8502=LINE('',#80526,#10342);
#8503=LINE('',#80530,#10343);
#8504=LINE('',#80536,#10344);
#8505=LINE('',#80539,#10345);
#8506=LINE('',#80552,#10346);
#8507=LINE('',#80558,#10347);
#8508=LINE('',#80561,#10348);
#8509=LINE('',#80568,#10349);
#8510=LINE('',#80570,#10350);
#8511=LINE('',#80571,#10351);
#8512=LINE('',#80583,#10352);
#8513=LINE('',#80594,#10353);
#8514=LINE('',#80603,#10354);
#8515=LINE('',#80617,#10355);
#8516=LINE('',#80627,#10356);
#8517=LINE('',#80635,#10357);
#8518=LINE('',#80649,#10358);
#8519=LINE('',#80657,#10359);
#8520=LINE('',#80665,#10360);
#8521=LINE('',#80673,#10361);
#8522=LINE('',#80681,#10362);
#8523=LINE('',#80687,#10363);
#8524=LINE('',#80693,#10364);
#8525=LINE('',#80701,#10365);
#8526=LINE('',#80707,#10366);
#8527=LINE('',#80713,#10367);
#8528=LINE('',#80719,#10368);
#8529=LINE('',#80735,#10369);
#8530=LINE('',#80736,#10370);
#8531=LINE('',#80745,#10371);
#8532=LINE('',#80748,#10372);
#8533=LINE('',#80761,#10373);
#8534=LINE('',#80762,#10374);
#8535=LINE('',#80780,#10375);
#8536=LINE('',#80783,#10376);
#8537=LINE('',#80789,#10377);
#8538=LINE('',#80878,#10378);
#8539=LINE('',#80885,#10379);
#8540=LINE('',#80888,#10380);
#8541=LINE('',#80890,#10381);
#8542=LINE('',#80891,#10382);
#8543=LINE('',#80894,#10383);
#8544=LINE('',#80904,#10384);
#8545=LINE('',#80905,#10385);
#8546=LINE('',#80906,#10386);
#8547=LINE('',#81242,#10387);
#8548=LINE('',#81380,#10388);
#8549=LINE('',#81382,#10389);
#8550=LINE('',#81522,#10390);
#8551=LINE('',#81649,#10391);
#8552=LINE('',#81653,#10392);
#8553=LINE('',#81654,#10393);
#8554=LINE('',#81657,#10394);
#8555=LINE('',#81661,#10395);
#8556=LINE('',#81662,#10396);
#8557=LINE('',#81665,#10397);
#8558=LINE('',#81669,#10398);
#8559=LINE('',#81670,#10399);
#8560=LINE('',#81673,#10400);
#8561=LINE('',#81677,#10401);
#8562=LINE('',#81678,#10402);
#8563=LINE('',#81681,#10403);
#8564=LINE('',#81685,#10404);
#8565=LINE('',#81686,#10405);
#8566=LINE('',#81691,#10406);
#8567=LINE('',#81693,#10407);
#8568=LINE('',#81694,#10408);
#8569=LINE('',#81699,#10409);
#8570=LINE('',#81701,#10410);
#8571=LINE('',#81702,#10411);
#8572=LINE('',#81705,#10412);
#8573=LINE('',#81709,#10413);
#8574=LINE('',#81710,#10414);
#8575=LINE('',#81715,#10415);
#8576=LINE('',#81717,#10416);
#8577=LINE('',#81718,#10417);
#8578=LINE('',#81723,#10418);
#8579=LINE('',#81725,#10419);
#8580=LINE('',#81726,#10420);
#8581=LINE('',#81729,#10421);
#8582=LINE('',#81732,#10422);
#8583=LINE('',#81736,#10423);
#8584=LINE('',#81813,#10424);
#8585=LINE('',#81822,#10425);
#8586=LINE('',#81826,#10426);
#8587=LINE('',#81834,#10427);
#8588=LINE('',#81838,#10428);
#8589=LINE('',#81890,#10429);
#8590=LINE('',#82018,#10430);
#8591=LINE('',#82026,#10431);
#8592=LINE('',#82038,#10432);
#8593=LINE('',#82046,#10433);
#8594=LINE('',#82054,#10434);
#8595=LINE('',#82062,#10435);
#8596=LINE('',#82070,#10436);
#8597=LINE('',#82076,#10437);
#8598=LINE('',#82083,#10438);
#8599=LINE('',#82092,#10439);
#8600=LINE('',#82098,#10440);
#8601=LINE('',#82105,#10441);
#8602=LINE('',#82112,#10442);
#8603=LINE('',#82122,#10443);
#8604=LINE('',#82128,#10444);
#8605=LINE('',#82129,#10445);
#8606=LINE('',#82138,#10446);
#8607=LINE('',#82151,#10447);
#8608=LINE('',#82161,#10448);
#8609=LINE('',#82201,#10449);
#8610=LINE('',#82212,#10450);
#8611=LINE('',#82213,#10451);
#8612=LINE('',#82229,#10452);
#8613=LINE('',#82232,#10453);
#8614=LINE('',#82242,#10454);
#8615=LINE('',#82244,#10455);
#8616=LINE('',#82254,#10456);
#8617=LINE('',#82256,#10457);
#8618=LINE('',#82261,#10458);
#8619=LINE('',#82262,#10459);
#8620=LINE('',#82268,#10460);
#8621=LINE('',#82285,#10461);
#8622=LINE('',#82288,#10462);
#8623=LINE('',#82307,#10463);
#8624=LINE('',#82308,#10464);
#8625=LINE('',#82438,#10465);
#8626=LINE('',#82441,#10466);
#8627=LINE('',#82444,#10467);
#8628=LINE('',#82456,#10468);
#8629=LINE('',#82458,#10469);
#8630=LINE('',#82464,#10470);
#8631=LINE('',#82467,#10471);
#8632=LINE('',#82471,#10472);
#8633=LINE('',#82475,#10473);
#8634=LINE('',#82479,#10474);
#8635=LINE('',#82539,#10475);
#8636=LINE('',#82541,#10476);
#8637=LINE('',#82543,#10477);
#8638=LINE('',#82546,#10478);
#8639=LINE('',#82615,#10479);
#8640=LINE('',#82616,#10480);
#8641=LINE('',#82625,#10481);
#8642=LINE('',#82633,#10482);
#8643=LINE('',#82641,#10483);
#8644=LINE('',#82647,#10484);
#8645=LINE('',#82665,#10485);
#8646=LINE('',#82667,#10486);
#8647=LINE('',#82669,#10487);
#8648=LINE('',#82708,#10488);
#8649=LINE('',#82710,#10489);
#8650=LINE('',#82712,#10490);
#8651=LINE('',#82714,#10491);
#8652=LINE('',#82732,#10492);
#8653=LINE('',#82915,#10493);
#8654=LINE('',#82918,#10494);
#8655=LINE('',#82922,#10495);
#8656=LINE('',#82926,#10496);
#8657=LINE('',#83279,#10497);
#8658=LINE('',#83433,#10498);
#8659=LINE('',#83440,#10499);
#8660=LINE('',#83453,#10500);
#8661=LINE('',#83457,#10501);
#8662=LINE('',#83469,#10502);
#8663=LINE('',#83477,#10503);
#8664=LINE('',#83481,#10504);
#8665=LINE('',#83485,#10505);
#8666=LINE('',#83487,#10506);
#8667=LINE('',#83488,#10507);
#8668=LINE('',#83492,#10508);
#8669=LINE('',#83493,#10509);
#8670=LINE('',#83494,#10510);
#8671=LINE('',#83501,#10511);
#8672=LINE('',#83505,#10512);
#8673=LINE('',#83509,#10513);
#8674=LINE('',#83511,#10514);
#8675=LINE('',#83512,#10515);
#8676=LINE('',#83515,#10516);
#8677=LINE('',#83517,#10517);
#8678=LINE('',#83518,#10518);
#8679=LINE('',#83527,#10519);
#8680=LINE('',#83531,#10520);
#8681=LINE('',#83535,#10521);
#8682=LINE('',#83539,#10522);
#8683=LINE('',#83543,#10523);
#8684=LINE('',#83547,#10524);
#8685=LINE('',#83573,#10525);
#8686=LINE('',#83577,#10526);
#8687=LINE('',#83603,#10527);
#8688=LINE('',#83607,#10528);
#8689=LINE('',#83633,#10529);
#8690=LINE('',#83637,#10530);
#8691=LINE('',#83641,#10531);
#8692=LINE('',#83645,#10532);
#8693=LINE('',#83649,#10533);
#8694=LINE('',#83665,#10534);
#8695=LINE('',#83691,#10535);
#8696=LINE('',#83717,#10536);
#8697=LINE('',#83743,#10537);
#8698=LINE('',#83756,#10538);
#8699=LINE('',#83771,#10539);
#8700=LINE('',#83797,#10540);
#8701=LINE('',#83823,#10541);
#8702=LINE('',#83849,#10542);
#8703=LINE('',#83864,#10543);
#8704=LINE('',#83866,#10544);
#8705=LINE('',#83867,#10545);
#8706=LINE('',#83870,#10546);
#8707=LINE('',#83872,#10547);
#8708=LINE('',#83873,#10548);
#8709=LINE('',#83879,#10549);
#8710=LINE('',#83886,#10550);
#8711=LINE('',#83890,#10551);
#8712=LINE('',#83895,#10552);
#8713=LINE('',#83902,#10553);
#8714=LINE('',#83905,#10554);
#8715=LINE('',#83906,#10555);
#8716=LINE('',#83912,#10556);
#8717=LINE('',#83914,#10557);
#8718=LINE('',#83916,#10558);
#8719=LINE('',#83922,#10559);
#8720=LINE('',#83925,#10560);
#8721=LINE('',#83928,#10561);
#8722=LINE('',#83930,#10562);
#8723=LINE('',#83931,#10563);
#8724=LINE('',#83937,#10564);
#8725=LINE('',#83969,#10565);
#8726=LINE('',#83970,#10566);
#8727=LINE('',#83973,#10567);
#8728=LINE('',#83977,#10568);
#8729=LINE('',#83978,#10569);
#8730=LINE('',#83988,#10570);
#8731=LINE('',#83991,#10571);
#8732=LINE('',#83992,#10572);
#8733=LINE('',#83997,#10573);
#8734=LINE('',#84111,#10574);
#8735=LINE('',#84179,#10575);
#8736=LINE('',#84187,#10576);
#8737=LINE('',#84278,#10577);
#8738=LINE('',#84418,#10578);
#8739=LINE('',#84420,#10579);
#8740=LINE('',#84424,#10580);
#8741=LINE('',#84431,#10581);
#8742=LINE('',#84435,#10582);
#8743=LINE('',#84437,#10583);
#8744=LINE('',#84438,#10584);
#8745=LINE('',#84442,#10585);
#8746=LINE('',#84476,#10586);
#8747=LINE('',#84482,#10587);
#8748=LINE('',#84485,#10588);
#8749=LINE('',#84487,#10589);
#8750=LINE('',#84490,#10590);
#8751=LINE('',#84495,#10591);
#8752=LINE('',#84498,#10592);
#8753=LINE('',#84499,#10593);
#8754=LINE('',#84502,#10594);
#8755=LINE('',#84565,#10595);
#8756=LINE('',#84676,#10596);
#8757=LINE('',#84678,#10597);
#8758=LINE('',#84765,#10598);
#8759=LINE('',#84906,#10599);
#8760=LINE('',#84908,#10600);
#8761=LINE('',#84911,#10601);
#8762=LINE('',#84913,#10602);
#8763=LINE('',#84914,#10603);
#8764=LINE('',#84917,#10604);
#8765=LINE('',#84919,#10605);
#8766=LINE('',#84920,#10606);
#8767=LINE('',#84926,#10607);
#8768=LINE('',#84933,#10608);
#8769=LINE('',#84937,#10609);
#8770=LINE('',#84942,#10610);
#8771=LINE('',#84949,#10611);
#8772=LINE('',#84952,#10612);
#8773=LINE('',#84953,#10613);
#8774=LINE('',#84959,#10614);
#8775=LINE('',#84961,#10615);
#8776=LINE('',#84963,#10616);
#8777=LINE('',#84965,#10617);
#8778=LINE('',#84966,#10618);
#8779=LINE('',#84968,#10619);
#8780=LINE('',#84970,#10620);
#8781=LINE('',#84972,#10621);
#8782=LINE('',#84974,#10622);
#8783=LINE('',#84976,#10623);
#8784=LINE('',#84977,#10624);
#8785=LINE('',#84979,#10625);
#8786=LINE('',#84981,#10626);
#8787=LINE('',#84983,#10627);
#8788=LINE('',#84985,#10628);
#8789=LINE('',#84987,#10629);
#8790=LINE('',#84989,#10630);
#8791=LINE('',#84992,#10631);
#8792=LINE('',#84994,#10632);
#8793=LINE('',#84999,#10633);
#8794=LINE('',#85011,#10634);
#8795=LINE('',#85015,#10635);
#8796=LINE('',#85019,#10636);
#8797=LINE('',#85023,#10637);
#8798=LINE('',#85027,#10638);
#8799=LINE('',#85030,#10639);
#8800=LINE('',#85032,#10640);
#8801=LINE('',#85033,#10641);
#8802=LINE('',#85035,#10642);
#8803=LINE('',#85037,#10643);
#8804=LINE('',#85040,#10644);
#8805=LINE('',#85044,#10645);
#8806=LINE('',#85077,#10646);
#8807=LINE('',#85081,#10647);
#8808=LINE('',#85118,#10648);
#8809=LINE('',#85122,#10649);
#8810=LINE('',#85154,#10650);
#8811=LINE('',#85157,#10651);
#8812=LINE('',#85212,#10652);
#8813=LINE('',#85215,#10653);
#8814=LINE('',#85219,#10654);
#8815=LINE('',#85276,#10655);
#8816=LINE('',#85281,#10656);
#8817=LINE('',#85285,#10657);
#8818=LINE('',#85304,#10658);
#8819=LINE('',#85308,#10659);
#8820=LINE('',#85313,#10660);
#8821=LINE('',#85314,#10661);
#8822=LINE('',#85315,#10662);
#8823=LINE('',#85320,#10663);
#8824=LINE('',#85325,#10664);
#8825=LINE('',#85332,#10665);
#8826=LINE('',#85390,#10666);
#8827=LINE('',#85395,#10667);
#8828=LINE('',#85396,#10668);
#8829=LINE('',#85399,#10669);
#8830=LINE('',#85455,#10670);
#8831=LINE('',#85458,#10671);
#8832=LINE('',#85469,#10672);
#8833=LINE('',#85471,#10673);
#8834=LINE('',#85499,#10674);
#8835=LINE('',#85554,#10675);
#8836=LINE('',#85562,#10676);
#8837=LINE('',#85564,#10677);
#8838=LINE('',#85566,#10678);
#8839=LINE('',#85568,#10679);
#8840=LINE('',#85614,#10680);
#8841=LINE('',#85615,#10681);
#8842=LINE('',#85620,#10682);
#8843=LINE('',#85625,#10683);
#8844=LINE('',#85632,#10684);
#8845=LINE('',#85636,#10685);
#8846=LINE('',#85638,#10686);
#8847=LINE('',#85639,#10687);
#8848=LINE('',#85643,#10688);
#8849=LINE('',#85687,#10689);
#8850=LINE('',#85691,#10690);
#8851=LINE('',#85704,#10691);
#8852=LINE('',#85825,#10692);
#8853=LINE('',#85904,#10693);
#8854=LINE('',#86027,#10694);
#8855=LINE('',#86076,#10695);
#8856=LINE('',#86198,#10696);
#8857=LINE('',#86199,#10697);
#8858=LINE('',#86200,#10698);
#8859=LINE('',#86207,#10699);
#8860=LINE('',#86208,#10700);
#8861=LINE('',#86213,#10701);
#8862=LINE('',#86215,#10702);
#8863=LINE('',#86216,#10703);
#8864=LINE('',#86221,#10704);
#8865=LINE('',#86223,#10705);
#8866=LINE('',#86231,#10706);
#8867=LINE('',#86247,#10707);
#8868=LINE('',#86435,#10708);
#8869=LINE('',#86437,#10709);
#8870=LINE('',#86439,#10710);
#8871=LINE('',#86440,#10711);
#8872=LINE('',#86446,#10712);
#8873=LINE('',#86568,#10713);
#8874=LINE('',#86572,#10714);
#8875=LINE('',#86617,#10715);
#8876=LINE('',#86621,#10716);
#8877=LINE('',#86623,#10717);
#8878=LINE('',#86627,#10718);
#8879=LINE('',#86628,#10719);
#8880=LINE('',#86633,#10720);
#8881=LINE('',#86676,#10721);
#8882=LINE('',#86678,#10722);
#8883=LINE('',#86682,#10723);
#8884=LINE('',#86688,#10724);
#8885=LINE('',#86731,#10725);
#8886=LINE('',#86733,#10726);
#8887=LINE('',#86735,#10727);
#8888=LINE('',#86757,#10728);
#8889=LINE('',#86759,#10729);
#8890=LINE('',#86763,#10730);
#8891=LINE('',#86767,#10731);
#8892=LINE('',#86769,#10732);
#8893=LINE('',#86771,#10733);
#8894=LINE('',#86772,#10734);
#8895=LINE('',#86777,#10735);
#8896=LINE('',#86784,#10736);
#8897=LINE('',#86789,#10737);
#8898=LINE('',#86793,#10738);
#8899=LINE('',#86795,#10739);
#8900=LINE('',#86796,#10740);
#8901=LINE('',#86800,#10741);
#8902=LINE('',#86812,#10742);
#8903=LINE('',#86820,#10743);
#8904=LINE('',#86823,#10744);
#8905=LINE('',#86842,#10745);
#8906=LINE('',#86844,#10746);
#8907=LINE('',#86871,#10747);
#8908=LINE('',#86872,#10748);
#8909=LINE('',#87088,#10749);
#8910=LINE('',#87089,#10750);
#8911=LINE('',#87254,#10751);
#8912=LINE('',#87256,#10752);
#8913=LINE('',#87283,#10753);
#8914=LINE('',#87284,#10754);
#8915=LINE('',#87288,#10755);
#8916=LINE('',#87292,#10756);
#8917=LINE('',#87374,#10757);
#8918=LINE('',#87437,#10758);
#8919=LINE('',#87641,#10759);
#8920=LINE('',#87642,#10760);
#8921=LINE('',#87681,#10761);
#8922=LINE('',#87682,#10762);
#8923=LINE('',#87728,#10763);
#8924=LINE('',#87732,#10764);
#8925=LINE('',#87981,#10765);
#8926=LINE('',#87991,#10766);
#8927=LINE('',#88227,#10767);
#8928=LINE('',#88229,#10768);
#8929=LINE('',#88239,#10769);
#8930=LINE('',#88241,#10770);
#8931=LINE('',#88244,#10771);
#8932=LINE('',#88247,#10772);
#8933=LINE('',#88249,#10773);
#8934=LINE('',#88362,#10774);
#8935=LINE('',#88387,#10775);
#8936=LINE('',#88393,#10776);
#8937=LINE('',#88435,#10777);
#8938=LINE('',#88451,#10778);
#8939=LINE('',#88453,#10779);
#8940=LINE('',#88454,#10780);
#8941=LINE('',#88456,#10781);
#8942=LINE('',#88457,#10782);
#8943=LINE('',#88461,#10783);
#8944=LINE('',#88464,#10784);
#8945=LINE('',#88465,#10785);
#8946=LINE('',#88469,#10786);
#8947=LINE('',#88472,#10787);
#8948=LINE('',#88474,#10788);
#8949=LINE('',#88476,#10789);
#8950=LINE('',#88479,#10790);
#8951=LINE('',#88480,#10791);
#8952=LINE('',#88482,#10792);
#8953=LINE('',#88484,#10793);
#8954=LINE('',#88486,#10794);
#8955=LINE('',#88488,#10795);
#8956=LINE('',#88491,#10796);
#8957=LINE('',#88492,#10797);
#8958=LINE('',#88494,#10798);
#8959=LINE('',#88496,#10799);
#8960=LINE('',#88500,#10800);
#8961=LINE('',#88504,#10801);
#8962=LINE('',#88507,#10802);
#8963=LINE('',#88512,#10803);
#8964=LINE('',#88514,#10804);
#8965=LINE('',#88583,#10805);
#8966=LINE('',#88586,#10806);
#8967=LINE('',#88598,#10807);
#8968=LINE('',#88824,#10808);
#8969=LINE('',#88839,#10809);
#8970=LINE('',#88840,#10810);
#8971=LINE('',#88850,#10811);
#8972=LINE('',#88866,#10812);
#8973=LINE('',#88967,#10813);
#8974=LINE('',#88969,#10814);
#8975=LINE('',#88971,#10815);
#8976=LINE('',#88974,#10816);
#8977=LINE('',#88979,#10817);
#8978=LINE('',#88980,#10818);
#8979=LINE('',#88982,#10819);
#8980=LINE('',#88984,#10820);
#8981=LINE('',#89162,#10821);
#8982=LINE('',#89178,#10822);
#8983=LINE('',#89439,#10823);
#8984=LINE('',#89506,#10824);
#8985=LINE('',#89624,#10825);
#8986=LINE('',#89799,#10826);
#8987=LINE('',#89802,#10827);
#8988=LINE('',#89961,#10828);
#8989=LINE('',#89962,#10829);
#8990=LINE('',#89965,#10830);
#8991=LINE('',#89968,#10831);
#8992=LINE('',#89972,#10832);
#8993=LINE('',#89978,#10833);
#8994=LINE('',#89982,#10834);
#8995=LINE('',#89986,#10835);
#8996=LINE('',#89989,#10836);
#8997=LINE('',#89990,#10837);
#8998=LINE('',#89994,#10838);
#8999=LINE('',#89998,#10839);
#9000=LINE('',#90002,#10840);
#9001=LINE('',#90005,#10841);
#9002=LINE('',#90006,#10842);
#9003=LINE('',#90093,#10843);
#9004=LINE('',#90212,#10844);
#9005=LINE('',#90215,#10845);
#9006=LINE('',#90231,#10846);
#9007=LINE('',#90235,#10847);
#9008=LINE('',#90309,#10848);
#9009=LINE('',#90314,#10849);
#9010=LINE('',#90407,#10850);
#9011=LINE('',#90410,#10851);
#9012=LINE('',#90449,#10852);
#9013=LINE('',#90452,#10853);
#9014=LINE('',#90455,#10854);
#9015=LINE('',#90457,#10855);
#9016=LINE('',#90458,#10856);
#9017=LINE('',#90463,#10857);
#9018=LINE('',#90470,#10858);
#9019=LINE('',#90475,#10859);
#9020=LINE('',#90487,#10860);
#9021=LINE('',#90492,#10861);
#9022=LINE('',#90495,#10862);
#9023=LINE('',#90496,#10863);
#9024=LINE('',#90500,#10864);
#9025=LINE('',#90503,#10865);
#9026=LINE('',#90517,#10866);
#9027=LINE('',#90518,#10867);
#9028=LINE('',#90546,#10868);
#9029=LINE('',#90557,#10869);
#9030=LINE('',#90566,#10870);
#9031=LINE('',#90568,#10871);
#9032=LINE('',#90614,#10872);
#9033=LINE('',#90616,#10873);
#9034=LINE('',#90618,#10874);
#9035=LINE('',#90619,#10875);
#9036=LINE('',#90624,#10876);
#9037=LINE('',#90631,#10877);
#9038=LINE('',#90636,#10878);
#9039=LINE('',#90640,#10879);
#9040=LINE('',#90642,#10880);
#9041=LINE('',#90643,#10881);
#9042=LINE('',#90649,#10882);
#9043=LINE('',#90653,#10883);
#9044=LINE('',#90661,#10884);
#9045=LINE('',#90673,#10885);
#9046=LINE('',#90917,#10886);
#9047=LINE('',#91058,#10887);
#9048=LINE('',#91182,#10888);
#9049=LINE('',#91251,#10889);
#9050=LINE('',#91320,#10890);
#9051=LINE('',#91322,#10891);
#9052=LINE('',#91323,#10892);
#9053=LINE('',#91328,#10893);
#9054=LINE('',#91330,#10894);
#9055=LINE('',#91337,#10895);
#9056=LINE('',#91338,#10896);
#9057=LINE('',#91339,#10897);
#9058=LINE('',#91346,#10898);
#9059=LINE('',#91347,#10899);
#9060=LINE('',#91354,#10900);
#9061=LINE('',#91370,#10901);
#9062=LINE('',#91608,#10902);
#9063=LINE('',#91613,#10903);
#9064=LINE('',#91614,#10904);
#9065=LINE('',#91615,#10905);
#9066=LINE('',#91618,#10906);
#9067=LINE('',#91667,#10907);
#9068=LINE('',#91671,#10908);
#9069=LINE('',#91793,#10909);
#9070=LINE('',#91800,#10910);
#9071=LINE('',#91803,#10911);
#9072=LINE('',#91807,#10912);
#9073=LINE('',#91808,#10913);
#9074=LINE('',#91850,#10914);
#9075=LINE('',#91855,#10915);
#9076=LINE('',#91859,#10916);
#9077=LINE('',#91860,#10917);
#9078=LINE('',#91902,#10918);
#9079=LINE('',#91915,#10919);
#9080=LINE('',#91917,#10920);
#9081=LINE('',#91918,#10921);
#9082=LINE('',#91934,#10922);
#9083=LINE('',#91936,#10923);
#9084=LINE('',#91988,#10924);
#9085=LINE('',#91992,#10925);
#9086=LINE('',#91995,#10926);
#9087=LINE('',#91997,#10927);
#9088=LINE('',#91999,#10928);
#9089=LINE('',#92001,#10929);
#9090=LINE('',#92004,#10930);
#9091=LINE('',#92009,#10931);
#9092=LINE('',#92014,#10932);
#9093=LINE('',#92021,#10933);
#9094=LINE('',#92026,#10934);
#9095=LINE('',#92027,#10935);
#9096=LINE('',#92028,#10936);
#9097=LINE('',#92064,#10937);
#9098=LINE('',#92069,#10938);
#9099=LINE('',#92078,#10939);
#9100=LINE('',#92081,#10940);
#9101=LINE('',#92101,#10941);
#9102=LINE('',#92102,#10942);
#9103=LINE('',#92128,#10943);
#9104=LINE('',#92129,#10944);
#9105=LINE('',#92336,#10945);
#9106=LINE('',#92337,#10946);
#9107=LINE('',#92504,#10947);
#9108=LINE('',#92505,#10948);
#9109=LINE('',#92531,#10949);
#9110=LINE('',#92532,#10950);
#9111=LINE('',#92613,#10951);
#9112=LINE('',#92673,#10952);
#9113=LINE('',#92676,#10953);
#9114=LINE('',#92679,#10954);
#9115=LINE('',#92961,#10955);
#9116=LINE('',#92962,#10956);
#9117=LINE('',#93057,#10957);
#9118=LINE('',#93060,#10958);
#9119=LINE('',#93221,#10959);
#9120=LINE('',#93224,#10960);
#9121=LINE('',#93252,#10961);
#9122=LINE('',#93258,#10962);
#9123=LINE('',#93266,#10963);
#9124=LINE('',#93274,#10964);
#9125=LINE('',#93284,#10965);
#9126=LINE('',#93293,#10966);
#9127=LINE('',#93301,#10967);
#9128=LINE('',#93309,#10968);
#9129=LINE('',#93315,#10969);
#9130=LINE('',#93318,#10970);
#9131=LINE('',#93533,#10971);
#9132=LINE('',#93813,#10972);
#9133=LINE('',#93816,#10973);
#9134=LINE('',#93819,#10974);
#9135=LINE('',#93821,#10975);
#9136=LINE('',#93838,#10976);
#9137=LINE('',#93849,#10977);
#9138=LINE('',#93854,#10978);
#9139=LINE('',#93862,#10979);
#9140=LINE('',#93872,#10980);
#9141=LINE('',#93874,#10981);
#9142=LINE('',#94019,#10982);
#9143=LINE('',#94026,#10983);
#9144=LINE('',#94064,#10984);
#9145=LINE('',#94066,#10985);
#9146=LINE('',#94067,#10986);
#9147=LINE('',#94069,#10987);
#9148=LINE('',#94070,#10988);
#9149=LINE('',#94073,#10989);
#9150=LINE('',#94077,#10990);
#9151=LINE('',#94078,#10991);
#9152=LINE('',#94081,#10992);
#9153=LINE('',#94084,#10993);
#9154=LINE('',#94087,#10994);
#9155=LINE('',#94089,#10995);
#9156=LINE('',#94092,#10996);
#9157=LINE('',#94093,#10997);
#9158=LINE('',#94095,#10998);
#9159=LINE('',#94097,#10999);
#9160=LINE('',#94099,#11000);
#9161=LINE('',#94101,#11001);
#9162=LINE('',#94104,#11002);
#9163=LINE('',#94105,#11003);
#9164=LINE('',#94107,#11004);
#9165=LINE('',#94109,#11005);
#9166=LINE('',#94112,#11006);
#9167=LINE('',#94116,#11007);
#9168=LINE('',#94121,#11008);
#9169=LINE('',#94124,#11009);
#9170=LINE('',#94127,#11010);
#9171=LINE('',#94211,#11011);
#9172=LINE('',#94215,#11012);
#9173=LINE('',#94226,#11013);
#9174=LINE('',#94404,#11014);
#9175=LINE('',#94416,#11015);
#9176=LINE('',#94417,#11016);
#9177=LINE('',#94425,#11017);
#9178=LINE('',#94442,#11018);
#9179=LINE('',#94447,#11019);
#9180=LINE('',#94683,#11020);
#9181=LINE('',#94685,#11021);
#9182=LINE('',#94687,#11022);
#9183=LINE('',#94692,#11023);
#9184=LINE('',#94696,#11024);
#9185=LINE('',#94698,#11025);
#9186=LINE('',#94700,#11026);
#9187=LINE('',#94831,#11027);
#9188=LINE('',#94847,#11028);
#9189=LINE('',#95057,#11029);
#9190=LINE('',#95159,#11030);
#9191=LINE('',#95242,#11031);
#9192=LINE('',#95251,#11032);
#9193=LINE('',#95255,#11033);
#9194=LINE('',#95258,#11034);
#9195=LINE('',#95262,#11035);
#9196=LINE('',#95272,#11036);
#9197=LINE('',#95278,#11037);
#9198=LINE('',#95280,#11038);
#9199=LINE('',#95283,#11039);
#9200=LINE('',#95289,#11040);
#9201=LINE('',#95297,#11041);
#9202=LINE('',#95552,#11042);
#9203=LINE('',#95690,#11043);
#9204=LINE('',#95693,#11044);
#9205=LINE('',#95696,#11045);
#9206=LINE('',#95699,#11046);
#9207=LINE('',#95705,#11047);
#9208=LINE('',#95709,#11048);
#9209=LINE('',#95713,#11049);
#9210=LINE('',#95717,#11050);
#9211=LINE('',#95718,#11051);
#9212=LINE('',#95721,#11052);
#9213=LINE('',#95725,#11053);
#9214=LINE('',#95729,#11054);
#9215=LINE('',#95733,#11055);
#9216=LINE('',#95734,#11056);
#9217=LINE('',#95768,#11057);
#9218=LINE('',#95778,#11058);
#9219=LINE('',#95782,#11059);
#9220=LINE('',#95809,#11060);
#9221=LINE('',#95812,#11061);
#9222=LINE('',#95818,#11062);
#9223=LINE('',#95824,#11063);
#9224=LINE('',#95964,#11064);
#9225=LINE('',#95976,#11065);
#9226=LINE('',#95985,#11066);
#9227=LINE('',#95990,#11067);
#9228=LINE('',#96084,#11068);
#9229=LINE('',#96088,#11069);
#9230=LINE('',#96125,#11070);
#9231=LINE('',#96129,#11071);
#9232=LINE('',#96130,#11072);
#9233=LINE('',#96131,#11073);
#9234=LINE('',#96143,#11074);
#9235=LINE('',#96146,#11075);
#9236=LINE('',#96188,#11076);
#9237=LINE('',#96195,#11077);
#9238=LINE('',#96198,#11078);
#9239=LINE('',#96199,#11079);
#9240=LINE('',#96203,#11080);
#9241=LINE('',#96207,#11081);
#9242=LINE('',#96224,#11082);
#9243=LINE('',#96228,#11083);
#9244=LINE('',#96229,#11084);
#9245=LINE('',#96230,#11085);
#9246=LINE('',#96237,#11086);
#9247=LINE('',#96241,#11087);
#9248=LINE('',#96273,#11088);
#9249=LINE('',#96280,#11089);
#9250=LINE('',#96283,#11090);
#9251=LINE('',#96284,#11091);
#9252=LINE('',#96288,#11092);
#9253=LINE('',#96290,#11093);
#9254=LINE('',#96292,#11094);
#9255=LINE('',#96293,#11095);
#9256=LINE('',#96331,#11096);
#9257=LINE('',#96336,#11097);
#9258=LINE('',#96352,#11098);
#9259=LINE('',#96361,#11099);
#9260=LINE('',#96369,#11100);
#9261=LINE('',#96377,#11101);
#9262=LINE('',#96403,#11102);
#9263=LINE('',#96410,#11103);
#9264=LINE('',#96413,#11104);
#9265=LINE('',#96414,#11105);
#9266=LINE('',#96433,#11106);
#9267=LINE('',#96449,#11107);
#9268=LINE('',#96455,#11108);
#9269=LINE('',#96465,#11109);
#9270=LINE('',#96470,#11110);
#9271=LINE('',#96495,#11111);
#9272=LINE('',#96611,#11112);
#9273=LINE('',#96614,#11113);
#9274=LINE('',#96691,#11114);
#9275=LINE('',#96692,#11115);
#9276=LINE('',#96698,#11116);
#9277=LINE('',#96835,#11117);
#9278=LINE('',#96942,#11118);
#9279=LINE('',#96944,#11119);
#9280=LINE('',#97001,#11120);
#9281=LINE('',#97058,#11121);
#9282=LINE('',#97181,#11122);
#9283=LINE('',#97328,#11123);
#9284=LINE('',#97349,#11124);
#9285=LINE('',#97353,#11125);
#9286=LINE('',#97354,#11126);
#9287=LINE('',#97357,#11127);
#9288=LINE('',#97359,#11128);
#9289=LINE('',#97360,#11129);
#9290=LINE('',#97363,#11130);
#9291=LINE('',#97364,#11131);
#9292=LINE('',#97367,#11132);
#9293=LINE('',#97371,#11133);
#9294=LINE('',#97372,#11134);
#9295=LINE('',#97376,#11135);
#9296=LINE('',#97378,#11136);
#9297=LINE('',#97381,#11137);
#9298=LINE('',#97385,#11138);
#9299=LINE('',#97386,#11139);
#9300=LINE('',#97387,#11140);
#9301=LINE('',#97390,#11141);
#9302=LINE('',#97391,#11142);
#9303=LINE('',#97394,#11143);
#9304=LINE('',#97395,#11144);
#9305=LINE('',#97401,#11145);
#9306=LINE('',#97405,#11146);
#9307=LINE('',#97409,#11147);
#9308=LINE('',#97413,#11148);
#9309=LINE('',#97419,#11149);
#9310=LINE('',#97425,#11150);
#9311=LINE('',#97441,#11151);
#9312=LINE('',#97447,#11152);
#9313=LINE('',#97453,#11153);
#9314=LINE('',#97457,#11154);
#9315=LINE('',#97460,#11155);
#9316=LINE('',#97482,#11156);
#9317=LINE('',#97486,#11157);
#9318=LINE('',#97488,#11158);
#9319=LINE('',#97490,#11159);
#9320=LINE('',#97492,#11160);
#9321=LINE('',#97494,#11161);
#9322=LINE('',#97498,#11162);
#9323=LINE('',#97501,#11163);
#9324=LINE('',#97509,#11164);
#9325=LINE('',#97510,#11165);
#9326=LINE('',#97512,#11166);
#9327=LINE('',#97514,#11167);
#9328=LINE('',#97515,#11168);
#9329=LINE('',#97516,#11169);
#9330=LINE('',#97558,#11170);
#9331=LINE('',#97563,#11171);
#9332=LINE('',#97565,#11172);
#9333=LINE('',#97567,#11173);
#9334=LINE('',#97571,#11174);
#9335=LINE('',#97572,#11175);
#9336=LINE('',#97575,#11176);
#9337=LINE('',#97579,#11177);
#9338=LINE('',#97580,#11178);
#9339=LINE('',#97593,#11179);
#9340=LINE('',#97596,#11180);
#9341=LINE('',#97597,#11181);
#9342=LINE('',#97605,#11182);
#9343=LINE('',#97606,#11183);
#9344=LINE('',#97609,#11184);
#9345=LINE('',#97611,#11185);
#9346=LINE('',#97614,#11186);
#9347=LINE('',#97617,#11187);
#9348=LINE('',#97618,#11188);
#9349=LINE('',#97621,#11189);
#9350=LINE('',#97637,#11190);
#9351=LINE('',#97639,#11191);
#9352=LINE('',#97641,#11192);
#9353=LINE('',#97644,#11193);
#9354=LINE('',#97648,#11194);
#9355=LINE('',#97651,#11195);
#9356=LINE('',#97664,#11196);
#9357=LINE('',#97665,#11197);
#9358=LINE('',#97673,#11198);
#9359=LINE('',#97674,#11199);
#9360=LINE('',#97677,#11200);
#9361=LINE('',#97679,#11201);
#9362=LINE('',#97681,#11202);
#9363=LINE('',#97684,#11203);
#9364=LINE('',#97687,#11204);
#9365=LINE('',#97688,#11205);
#9366=LINE('',#97701,#11206);
#9367=LINE('',#97704,#11207);
#9368=LINE('',#97705,#11208);
#9369=LINE('',#97712,#11209);
#9370=LINE('',#97717,#11210);
#9371=LINE('',#97719,#11211);
#9372=LINE('',#97720,#11212);
#9373=LINE('',#97722,#11213);
#9374=LINE('',#97723,#11214);
#9375=LINE('',#97731,#11215);
#9376=LINE('',#97734,#11216);
#9377=LINE('',#97736,#11217);
#9378=LINE('',#97741,#11218);
#9379=LINE('',#97742,#11219);
#9380=LINE('',#97746,#11220);
#9381=LINE('',#97749,#11221);
#9382=LINE('',#97750,#11222);
#9383=LINE('',#97757,#11223);
#9384=LINE('',#97801,#11224);
#9385=LINE('',#97802,#11225);
#9386=LINE('',#97805,#11226);
#9387=LINE('',#97807,#11227);
#9388=LINE('',#97808,#11228);
#9389=LINE('',#97822,#11229);
#9390=LINE('',#97827,#11230);
#9391=LINE('',#97828,#11231);
#9392=LINE('',#97829,#11232);
#9393=LINE('',#97833,#11233);
#9394=LINE('',#97835,#11234);
#9395=LINE('',#97837,#11235);
#9396=LINE('',#97838,#11236);
#9397=LINE('',#97852,#11237);
#9398=LINE('',#97856,#11238);
#9399=LINE('',#97858,#11239);
#9400=LINE('',#97859,#11240);
#9401=LINE('',#97863,#11241);
#9402=LINE('',#97867,#11242);
#9403=LINE('',#97870,#11243);
#9404=LINE('',#97884,#11244);
#9405=LINE('',#97888,#11245);
#9406=LINE('',#97890,#11246);
#9407=LINE('',#97891,#11247);
#9408=LINE('',#97895,#11248);
#9409=LINE('',#97897,#11249);
#9410=LINE('',#97902,#11250);
#9411=LINE('',#97916,#11251);
#9412=LINE('',#97918,#11252);
#9413=LINE('',#97919,#11253);
#9414=LINE('',#97925,#11254);
#9415=LINE('',#97929,#11255);
#9416=LINE('',#97935,#11256);
#9417=LINE('',#97949,#11257);
#9418=LINE('',#97957,#11258);
#9419=LINE('',#97971,#11259);
#9420=LINE('',#97977,#11260);
#9421=LINE('',#97983,#11261);
#9422=LINE('',#97987,#11262);
#9423=LINE('',#97991,#11263);
#9424=LINE('',#97993,#11264);
#9425=LINE('',#97997,#11265);
#9426=LINE('',#97998,#11266);
#9427=LINE('',#98002,#11267);
#9428=LINE('',#98005,#11268);
#9429=LINE('',#98006,#11269);
#9430=LINE('',#98009,#11270);
#9431=LINE('',#98013,#11271);
#9432=LINE('',#98017,#11272);
#9433=LINE('',#98018,#11273);
#9434=LINE('',#98022,#11274);
#9435=LINE('',#98026,#11275);
#9436=LINE('',#98030,#11276);
#9437=LINE('',#98033,#11277);
#9438=LINE('',#98037,#11278);
#9439=LINE('',#98041,#11279);
#9440=LINE('',#98045,#11280);
#9441=LINE('',#98046,#11281);
#9442=LINE('',#98050,#11282);
#9443=LINE('',#98053,#11283);
#9444=LINE('',#98058,#11284);
#9445=LINE('',#98061,#11285);
#9446=LINE('',#98062,#11286);
#9447=LINE('',#98065,#11287);
#9448=LINE('',#98069,#11288);
#9449=LINE('',#98073,#11289);
#9450=LINE('',#98078,#11290);
#9451=LINE('',#98081,#11291);
#9452=LINE('',#98086,#11292);
#9453=LINE('',#98089,#11293);
#9454=LINE('',#98090,#11294);
#9455=LINE('',#98096,#11295);
#9456=LINE('',#98098,#11296);
#9457=LINE('',#98101,#11297);
#9458=LINE('',#98102,#11298);
#9459=LINE('',#98108,#11299);
#9460=LINE('',#98110,#11300);
#9461=LINE('',#98113,#11301);
#9462=LINE('',#98117,#11302);
#9463=LINE('',#98119,#11303);
#9464=LINE('',#98126,#11304);
#9465=LINE('',#98129,#11305);
#9466=LINE('',#98132,#11306);
#9467=LINE('',#98138,#11307);
#9468=LINE('',#98141,#11308);
#9469=LINE('',#98144,#11309);
#9470=LINE('',#98200,#11310);
#9471=LINE('',#98206,#11311);
#9472=LINE('',#98260,#11312);
#9473=LINE('',#98261,#11313);
#9474=LINE('',#98264,#11314);
#9475=LINE('',#98265,#11315);
#9476=LINE('',#98267,#11316);
#9477=VECTOR('',#38624,0.999999999999103);
#9478=VECTOR('',#38633,1.4);
#9479=VECTOR('',#38640,0.999999999999103);
#9480=VECTOR('',#38649,1000.);
#9481=VECTOR('',#38652,1000.);
#9482=VECTOR('',#38657,1000.);
#9483=VECTOR('',#38664,1000.);
#9484=VECTOR('',#38667,1000.);
#9485=VECTOR('',#38670,1000.);
#9486=VECTOR('',#38677,1000.);
#9487=VECTOR('',#38680,1000.);
#9488=VECTOR('',#38683,1000.);
#9489=VECTOR('',#38690,1000.);
#9490=VECTOR('',#38697,1000.);
#9491=VECTOR('',#38700,1000.);
#9492=VECTOR('',#38703,1000.);
#9493=VECTOR('',#38710,1000.);
#9494=VECTOR('',#38713,1000.);
#9495=VECTOR('',#38716,1000.);
#9496=VECTOR('',#38727,1000.);
#9497=VECTOR('',#38736,1000.);
#9498=VECTOR('',#38743,1000.);
#9499=VECTOR('',#38744,1000.);
#9500=VECTOR('',#38751,10.);
#9501=VECTOR('',#38752,10.);
#9502=VECTOR('',#38761,1000.);
#9503=VECTOR('',#38762,1000.);
#9504=VECTOR('',#38763,1000.);
#9505=VECTOR('',#38764,1000.);
#9506=VECTOR('',#38765,1000.);
#9507=VECTOR('',#38766,1000.);
#9508=VECTOR('',#38769,1000.);
#9509=VECTOR('',#38774,1000.);
#9510=VECTOR('',#38775,10.);
#9511=VECTOR('',#38778,1000.);
#9512=VECTOR('',#38783,1000.);
#9513=VECTOR('',#38788,1000.);
#9514=VECTOR('',#38789,1000.);
#9515=VECTOR('',#38792,1000.);
#9516=VECTOR('',#38793,1000.);
#9517=VECTOR('',#38800,1000.);
#9518=VECTOR('',#38803,1000.);
#9519=VECTOR('',#38804,1000.);
#9520=VECTOR('',#38807,1000.);
#9521=VECTOR('',#38810,1000.);
#9522=VECTOR('',#38811,1000.);
#9523=VECTOR('',#38812,1000.);
#9524=VECTOR('',#38815,1000.);
#9525=VECTOR('',#38816,1000.);
#9526=VECTOR('',#38823,1000.);
#9527=VECTOR('',#38830,10.);
#9528=VECTOR('',#38835,1000.);
#9529=VECTOR('',#38838,1000.);
#9530=VECTOR('',#38853,1000.);
#9531=VECTOR('',#38860,1000.);
#9532=VECTOR('',#38863,1000.);
#9533=VECTOR('',#38864,1000.);
#9534=VECTOR('',#38873,1000.);
#9535=VECTOR('',#38880,1000.);
#9536=VECTOR('',#38883,1000.);
#9537=VECTOR('',#38884,1000.);
#9538=VECTOR('',#38893,1000.);
#9539=VECTOR('',#38900,1000.);
#9540=VECTOR('',#38903,1000.);
#9541=VECTOR('',#38904,1000.);
#9542=VECTOR('',#38913,1000.);
#9543=VECTOR('',#38924,1000.);
#9544=VECTOR('',#38935,1000.);
#9545=VECTOR('',#38942,1000.);
#9546=VECTOR('',#38945,1000.);
#9547=VECTOR('',#38946,1000.);
#9548=VECTOR('',#38955,1000.);
#9549=VECTOR('',#38966,1000.);
#9550=VECTOR('',#38977,1000.);
#9551=VECTOR('',#38984,1000.);
#9552=VECTOR('',#38987,1000.);
#9553=VECTOR('',#38988,1000.);
#9554=VECTOR('',#38997,1000.);
#9555=VECTOR('',#39004,1000.);
#9556=VECTOR('',#39007,1000.);
#9557=VECTOR('',#39008,1000.);
#9558=VECTOR('',#39017,1000.);
#9559=VECTOR('',#39024,1000.);
#9560=VECTOR('',#39027,1000.);
#9561=VECTOR('',#39028,1000.);
#9562=VECTOR('',#39037,1000.);
#9563=VECTOR('',#39046,1000.);
#9564=VECTOR('',#39059,1000.);
#9565=VECTOR('',#39066,1000.);
#9566=VECTOR('',#39069,1000.);
#9567=VECTOR('',#39070,1000.);
#9568=VECTOR('',#39079,1000.);
#9569=VECTOR('',#39086,1000.);
#9570=VECTOR('',#39089,1000.);
#9571=VECTOR('',#39090,1000.);
#9572=VECTOR('',#39099,1000.);
#9573=VECTOR('',#39106,1000.);
#9574=VECTOR('',#39109,1000.);
#9575=VECTOR('',#39110,1000.);
#9576=VECTOR('',#39119,1000.);
#9577=VECTOR('',#39130,1000.);
#9578=VECTOR('',#39141,1000.);
#9579=VECTOR('',#39148,1000.);
#9580=VECTOR('',#39151,1000.);
#9581=VECTOR('',#39152,1000.);
#9582=VECTOR('',#39161,1000.);
#9583=VECTOR('',#39172,1000.);
#9584=VECTOR('',#39183,1000.);
#9585=VECTOR('',#39190,1000.);
#9586=VECTOR('',#39193,1000.);
#9587=VECTOR('',#39194,1000.);
#9588=VECTOR('',#39203,1000.);
#9589=VECTOR('',#39210,1000.);
#9590=VECTOR('',#39213,1000.);
#9591=VECTOR('',#39214,1000.);
#9592=VECTOR('',#39225,1000.);
#9593=VECTOR('',#39234,1000.);
#9594=VECTOR('',#39239,1000.);
#9595=VECTOR('',#39242,1000.);
#9596=VECTOR('',#39245,1000.);
#9597=VECTOR('',#39246,1000.);
#9598=VECTOR('',#39247,1000.);
#9599=VECTOR('',#39248,1000.);
#9600=VECTOR('',#39249,10.);
#9601=VECTOR('',#39250,10.);
#9602=VECTOR('',#39253,10.);
#9603=VECTOR('',#39254,10.);
#9604=VECTOR('',#39257,10.);
#9605=VECTOR('',#39258,10.);
#9606=VECTOR('',#39261,10.);
#9607=VECTOR('',#39262,10.);
#9608=VECTOR('',#39265,10.);
#9609=VECTOR('',#39266,10.);
#9610=VECTOR('',#39267,10.);
#9611=VECTOR('',#39268,10.);
#9612=VECTOR('',#39273,1000.);
#9613=VECTOR('',#39274,10.);
#9614=VECTOR('',#39275,1000.);
#9615=VECTOR('',#39278,1000.);
#9616=VECTOR('',#39279,10.);
#9617=VECTOR('',#39280,1000.);
#9618=VECTOR('',#39293,10.);
#9619=VECTOR('',#39324,10.);
#9620=VECTOR('',#39325,10.);
#9621=VECTOR('',#39328,10.);
#9622=VECTOR('',#39355,10.);
#9623=VECTOR('',#39404,1000.);
#9624=VECTOR('',#39415,1000.);
#9625=VECTOR('',#39426,1000.);
#9626=VECTOR('',#39449,1000.);
#9627=VECTOR('',#39472,1000.);
#9628=VECTOR('',#39483,1000.);
#9629=VECTOR('',#39494,1000.);
#9630=VECTOR('',#39517,1000.);
#9631=VECTOR('',#39528,1000.);
#9632=VECTOR('',#39539,1000.);
#9633=VECTOR('',#39562,1000.);
#9634=VECTOR('',#39585,1000.);
#9635=VECTOR('',#39596,1000.);
#9636=VECTOR('',#39611,1000.);
#9637=VECTOR('',#39614,1000.);
#9638=VECTOR('',#39617,1000.);
#9639=VECTOR('',#39620,1000.);
#9640=VECTOR('',#39623,1000.);
#9641=VECTOR('',#39626,1000.);
#9642=VECTOR('',#39631,1000.);
#9643=VECTOR('',#39634,1000.);
#9644=VECTOR('',#39637,1000.);
#9645=VECTOR('',#39640,1000.);
#9646=VECTOR('',#39645,1000.);
#9647=VECTOR('',#39646,1000.);
#9648=VECTOR('',#39651,10.);
#9649=VECTOR('',#39652,1000.);
#9650=VECTOR('',#39655,10.);
#9651=VECTOR('',#39656,1000.);
#9652=VECTOR('',#39661,1000.);
#9653=VECTOR('',#39664,10.);
#9654=VECTOR('',#39665,1000.);
#9655=VECTOR('',#39672,1000.);
#9656=VECTOR('',#39673,10.);
#9657=VECTOR('',#39674,1000.);
#9658=VECTOR('',#39683,1000.);
#9659=VECTOR('',#39686,10.);
#9660=VECTOR('',#39687,1000.);
#9661=VECTOR('',#39692,1000.);
#9662=VECTOR('',#39695,1000.);
#9663=VECTOR('',#39696,10.);
#9664=VECTOR('',#39701,1000.);
#9665=VECTOR('',#39704,1000.);
#9666=VECTOR('',#39705,10.);
#9667=VECTOR('',#39710,1000.);
#9668=VECTOR('',#39713,1000.);
#9669=VECTOR('',#39714,10.);
#9670=VECTOR('',#39719,1000.);
#9671=VECTOR('',#39722,10.);
#9672=VECTOR('',#39723,10.);
#9673=VECTOR('',#39724,10.);
#9674=VECTOR('',#39725,10.);
#9675=VECTOR('',#39728,10.);
#9676=VECTOR('',#39729,10.);
#9677=VECTOR('',#39730,10.);
#9678=VECTOR('',#39731,10.);
#9679=VECTOR('',#39732,10.);
#9680=VECTOR('',#39733,10.);
#9681=VECTOR('',#39734,10.);
#9682=VECTOR('',#39735,10.);
#9683=VECTOR('',#39736,10.);
#9684=VECTOR('',#39745,10.);
#9685=VECTOR('',#39756,1000.);
#9686=VECTOR('',#39761,1000.);
#9687=VECTOR('',#39766,1000.);
#9688=VECTOR('',#39771,1000.);
#9689=VECTOR('',#39776,1000.);
#9690=VECTOR('',#39783,1000.);
#9691=VECTOR('',#39788,1000.);
#9692=VECTOR('',#39831,10.);
#9693=VECTOR('',#39832,10.);
#9694=VECTOR('',#39833,10.);
#9695=VECTOR('',#39836,10.);
#9696=VECTOR('',#39839,10.);
#9697=VECTOR('',#39842,10.);
#9698=VECTOR('',#39843,10.);
#9699=VECTOR('',#39846,10.);
#9700=VECTOR('',#39849,10.);
#9701=VECTOR('',#39852,10.);
#9702=VECTOR('',#39855,10.);
#9703=VECTOR('',#39856,10.);
#9704=VECTOR('',#39859,10.);
#9705=VECTOR('',#39884,1000.);
#9706=VECTOR('',#39885,1000.);
#9707=VECTOR('',#39888,1000.);
#9708=VECTOR('',#39893,1000.);
#9709=VECTOR('',#39900,1000.);
#9710=VECTOR('',#39905,1000.);
#9711=VECTOR('',#39910,1000.);
#9712=VECTOR('',#39925,1000.);
#9713=VECTOR('',#39930,1000.);
#9714=VECTOR('',#39939,1000.);
#9715=VECTOR('',#39944,1000.);
#9716=VECTOR('',#39961,1000.);
#9717=VECTOR('',#39962,1000.);
#9718=VECTOR('',#39967,1000.);
#9719=VECTOR('',#39972,1000.);
#9720=VECTOR('',#39977,1000.);
#9721=VECTOR('',#39982,1000.);
#9722=VECTOR('',#39991,1000.);
#9723=VECTOR('',#39996,1000.);
#9724=VECTOR('',#39999,1000.);
#9725=VECTOR('',#40002,1000.);
#9726=VECTOR('',#40005,1000.);
#9727=VECTOR('',#40010,1000.);
#9728=VECTOR('',#40011,1000.);
#9729=VECTOR('',#40014,1000.);
#9730=VECTOR('',#40019,1000.);
#9731=VECTOR('',#40022,1000.);
#9732=VECTOR('',#40027,1000.);
#9733=VECTOR('',#40036,1000.);
#9734=VECTOR('',#40045,1000.);
#9735=VECTOR('',#40046,1000.);
#9736=VECTOR('',#40051,1000.);
#9737=VECTOR('',#40056,1000.);
#9738=VECTOR('',#40067,1000.);
#9739=VECTOR('',#40068,1000.);
#9740=VECTOR('',#40073,1000.);
#9741=VECTOR('',#40076,1000.);
#9742=VECTOR('',#40081,1000.);
#9743=VECTOR('',#40086,1000.);
#9744=VECTOR('',#40095,1000.);
#9745=VECTOR('',#40104,1000.);
#9746=VECTOR('',#40105,1000.);
#9747=VECTOR('',#40110,1000.);
#9748=VECTOR('',#40115,1000.);
#9749=VECTOR('',#40120,1000.);
#9750=VECTOR('',#40125,1000.);
#9751=VECTOR('',#40130,1000.);
#9752=VECTOR('',#40135,1000.);
#9753=VECTOR('',#40140,1000.);
#9754=VECTOR('',#40149,1000.);
#9755=VECTOR('',#40154,1000.);
#9756=VECTOR('',#40159,1000.);
#9757=VECTOR('',#40160,1000.);
#9758=VECTOR('',#40161,1000.);
#9759=VECTOR('',#40162,1000.);
#9760=VECTOR('',#40169,1000.);
#9761=VECTOR('',#40170,1000.);
#9762=VECTOR('',#40175,1000.);
#9763=VECTOR('',#40176,1000.);
#9764=VECTOR('',#40185,5.5);
#9765=VECTOR('',#40194,5.5);
#9766=VECTOR('',#40199,1000.);
#9767=VECTOR('',#40200,1000.);
#9768=VECTOR('',#40205,1000.);
#9769=VECTOR('',#40208,1000.);
#9770=VECTOR('',#40211,1000.);
#9771=VECTOR('',#40214,1000.);
#9772=VECTOR('',#40219,1000.);
#9773=VECTOR('',#40222,1000.);
#9774=VECTOR('',#40225,1000.);
#9775=VECTOR('',#40228,1000.);
#9776=VECTOR('',#40231,1000.);
#9777=VECTOR('',#40236,1000.);
#9778=VECTOR('',#40237,1000.);
#9779=VECTOR('',#40240,1000.);
#9780=VECTOR('',#40243,1000.);
#9781=VECTOR('',#40246,1000.);
#9782=VECTOR('',#40249,1000.);
#9783=VECTOR('',#40252,1000.);
#9784=VECTOR('',#40257,1000.);
#9785=VECTOR('',#40260,1000.);
#9786=VECTOR('',#40263,1000.);
#9787=VECTOR('',#40266,1000.);
#9788=VECTOR('',#40269,1000.);
#9789=VECTOR('',#40276,1000.);
#9790=VECTOR('',#40281,1000.);
#9791=VECTOR('',#40282,1000.);
#9792=VECTOR('',#40287,1000.);
#9793=VECTOR('',#40288,1000.);
#9794=VECTOR('',#40295,1000.);
#9795=VECTOR('',#40298,1000.);
#9796=VECTOR('',#40299,1000.);
#9797=VECTOR('',#40300,1000.);
#9798=VECTOR('',#40303,1000.);
#9799=VECTOR('',#40312,1000.);
#9800=VECTOR('',#40317,1000.);
#9801=VECTOR('',#40322,1000.);
#9802=VECTOR('',#40325,1000.);
#9803=VECTOR('',#40328,1000.);
#9804=VECTOR('',#40329,1000.);
#9805=VECTOR('',#40330,1000.);
#9806=VECTOR('',#40331,1000.);
#9807=VECTOR('',#40332,1000.);
#9808=VECTOR('',#40335,1000.);
#9809=VECTOR('',#40336,1000.);
#9810=VECTOR('',#40339,1000.);
#9811=VECTOR('',#40340,1000.);
#9812=VECTOR('',#40343,1000.);
#9813=VECTOR('',#40344,1000.);
#9814=VECTOR('',#40347,1000.);
#9815=VECTOR('',#40348,1000.);
#9816=VECTOR('',#40351,1000.);
#9817=VECTOR('',#40358,1000.);
#9818=VECTOR('',#40365,1000.);
#9819=VECTOR('',#40366,1000.);
#9820=VECTOR('',#40369,1000.);
#9821=VECTOR('',#40370,1000.);
#9822=VECTOR('',#40371,1000.);
#9823=VECTOR('',#40372,1000.);
#9824=VECTOR('',#40377,1000.);
#9825=VECTOR('',#40384,1000.);
#9826=VECTOR('',#40385,1000.);
#9827=VECTOR('',#40388,1000.);
#9828=VECTOR('',#40391,1000.);
#9829=VECTOR('',#40404,1000.);
#9830=VECTOR('',#40411,1000.);
#9831=VECTOR('',#40414,1000.);
#9832=VECTOR('',#40415,1000.);
#9833=VECTOR('',#40422,1000.);
#9834=VECTOR('',#40427,1000.);
#9835=VECTOR('',#40430,1000.);
#9836=VECTOR('',#40435,1000.);
#9837=VECTOR('',#40436,1000.);
#9838=VECTOR('',#40439,1000.);
#9839=VECTOR('',#40440,1000.);
#9840=VECTOR('',#40443,1000.);
#9841=VECTOR('',#40446,1000.);
#9842=VECTOR('',#40449,1000.);
#9843=VECTOR('',#40452,1000.);
#9844=VECTOR('',#40455,1000.);
#9845=VECTOR('',#40458,1000.);
#9846=VECTOR('',#40461,1000.);
#9847=VECTOR('',#40464,1000.);
#9848=VECTOR('',#40465,1000.);
#9849=VECTOR('',#40468,1000.);
#9850=VECTOR('',#40473,1000.);
#9851=VECTOR('',#40474,1000.);
#9852=VECTOR('',#40475,1000.);
#9853=VECTOR('',#40478,1000.);
#9854=VECTOR('',#40479,1000.);
#9855=VECTOR('',#40482,1000.);
#9856=VECTOR('',#40485,1000.);
#9857=VECTOR('',#40488,1000.);
#9858=VECTOR('',#40493,1000.);
#9859=VECTOR('',#40494,1000.);
#9860=VECTOR('',#40495,1000.);
#9861=VECTOR('',#40498,1000.);
#9862=VECTOR('',#40499,1000.);
#9863=VECTOR('',#40502,1000.);
#9864=VECTOR('',#40505,1000.);
#9865=VECTOR('',#40508,1000.);
#9866=VECTOR('',#40511,1000.);
#9867=VECTOR('',#40514,1000.);
#9868=VECTOR('',#40517,1000.);
#9869=VECTOR('',#40520,1000.);
#9870=VECTOR('',#40523,1000.);
#9871=VECTOR('',#40526,1000.);
#9872=VECTOR('',#40531,1000.);
#9873=VECTOR('',#40532,1000.);
#9874=VECTOR('',#40533,1000.);
#9875=VECTOR('',#40536,1000.);
#9876=VECTOR('',#40537,1000.);
#9877=VECTOR('',#40540,1000.);
#9878=VECTOR('',#40543,1000.);
#9879=VECTOR('',#40546,1000.);
#9880=VECTOR('',#40551,1000.);
#9881=VECTOR('',#40552,1000.);
#9882=VECTOR('',#40553,1000.);
#9883=VECTOR('',#40556,1000.);
#9884=VECTOR('',#40559,1000.);
#9885=VECTOR('',#40560,1000.);
#9886=VECTOR('',#40569,1000.);
#9887=VECTOR('',#40570,1000.);
#9888=VECTOR('',#40571,1000.);
#9889=VECTOR('',#40574,1000.);
#9890=VECTOR('',#40585,1000.);
#9891=VECTOR('',#40598,1000.);
#9892=VECTOR('',#40601,1000.);
#9893=VECTOR('',#40602,1000.);
#9894=VECTOR('',#40605,1000.);
#9895=VECTOR('',#40606,1000.);
#9896=VECTOR('',#40607,1000.);
#9897=VECTOR('',#40608,1000.);
#9898=VECTOR('',#40611,1000.);
#9899=VECTOR('',#40612,1000.);
#9900=VECTOR('',#40613,1000.);
#9901=VECTOR('',#40616,1000.);
#9902=VECTOR('',#40621,1000.);
#9903=VECTOR('',#40622,1000.);
#9904=VECTOR('',#40623,1000.);
#9905=VECTOR('',#40626,1000.);
#9906=VECTOR('',#40627,1000.);
#9907=VECTOR('',#40630,1000.);
#9908=VECTOR('',#40641,1000.);
#9909=VECTOR('',#40648,1000.);
#9910=VECTOR('',#40651,1000.);
#9911=VECTOR('',#40656,1000.);
#9912=VECTOR('',#40659,1000.);
#9913=VECTOR('',#40662,1000.);
#9914=VECTOR('',#40663,1000.);
#9915=VECTOR('',#40666,1000.);
#9916=VECTOR('',#40673,1000.);
#9917=VECTOR('',#40674,1000.);
#9918=VECTOR('',#40675,1000.);
#9919=VECTOR('',#40678,1000.);
#9920=VECTOR('',#40679,1000.);
#9921=VECTOR('',#40684,1000.);
#9922=VECTOR('',#40689,2.25);
#9923=VECTOR('',#40700,1000.);
#9924=VECTOR('',#40705,1000.);
#9925=VECTOR('',#40706,1000.);
#9926=VECTOR('',#40711,1000.);
#9927=VECTOR('',#40716,1000.);
#9928=VECTOR('',#40721,1000.);
#9929=VECTOR('',#40726,1000.);
#9930=VECTOR('',#40729,1000.);
#9931=VECTOR('',#40736,1000.);
#9932=VECTOR('',#40739,1000.);
#9933=VECTOR('',#40742,1000.);
#9934=VECTOR('',#40745,1000.);
#9935=VECTOR('',#40748,1000.);
#9936=VECTOR('',#40749,1000.);
#9937=VECTOR('',#40752,1000.);
#9938=VECTOR('',#40753,1000.);
#9939=VECTOR('',#40754,1000.);
#9940=VECTOR('',#40757,1000.);
#9941=VECTOR('',#40764,1000.);
#9942=VECTOR('',#40765,1000.);
#9943=VECTOR('',#40770,1000.);
#9944=VECTOR('',#40781,2.25);
#9945=VECTOR('',#40790,1000.);
#9946=VECTOR('',#40793,1000.);
#9947=VECTOR('',#40794,1000.);
#9948=VECTOR('',#40797,1000.);
#9949=VECTOR('',#40798,1000.);
#9950=VECTOR('',#40799,1000.);
#9951=VECTOR('',#40800,1000.);
#9952=VECTOR('',#40801,1000.);
#9953=VECTOR('',#40802,1000.);
#9954=VECTOR('',#40803,1000.);
#9955=VECTOR('',#40808,1000.);
#9956=VECTOR('',#40811,1000.);
#9957=VECTOR('',#40812,1000.);
#9958=VECTOR('',#40813,1000.);
#9959=VECTOR('',#40814,1000.);
#9960=VECTOR('',#40815,1000.);
#9961=VECTOR('',#40816,1000.);
#9962=VECTOR('',#40819,1000.);
#9963=VECTOR('',#40820,1000.);
#9964=VECTOR('',#40821,1000.);
#9965=VECTOR('',#40826,1000.);
#9966=VECTOR('',#40829,1000.);
#9967=VECTOR('',#40830,1000.);
#9968=VECTOR('',#40833,1000.);
#9969=VECTOR('',#40836,1000.);
#9970=VECTOR('',#40837,1000.);
#9971=VECTOR('',#40840,1000.);
#9972=VECTOR('',#40841,1000.);
#9973=VECTOR('',#40842,1000.);
#9974=VECTOR('',#40843,1000.);
#9975=VECTOR('',#40844,1000.);
#9976=VECTOR('',#40845,1000.);
#9977=VECTOR('',#40846,1000.);
#9978=VECTOR('',#40851,1000.);
#9979=VECTOR('',#40854,1000.);
#9980=VECTOR('',#40855,1000.);
#9981=VECTOR('',#40856,1000.);
#9982=VECTOR('',#40857,1000.);
#9983=VECTOR('',#40858,1000.);
#9984=VECTOR('',#40859,1000.);
#9985=VECTOR('',#40862,1000.);
#9986=VECTOR('',#40863,1000.);
#9987=VECTOR('',#40872,1000.);
#9988=VECTOR('',#40877,1000.);
#9989=VECTOR('',#40882,1000.);
#9990=VECTOR('',#40883,1000.);
#9991=VECTOR('',#40900,1000.);
#9992=VECTOR('',#40927,1000.);
#9993=VECTOR('',#40932,1000.);
#9994=VECTOR('',#40943,1000.);
#9995=VECTOR('',#40956,1000.);
#9996=VECTOR('',#40965,1000.);
#9997=VECTOR('',#40974,1000.);
#9998=VECTOR('',#40977,1000.);
#9999=VECTOR('',#40980,1000.);
#10000=VECTOR('',#40983,1000.);
#10001=VECTOR('',#40988,1000.);
#10002=VECTOR('',#40991,1000.);
#10003=VECTOR('',#40998,1000.);
#10004=VECTOR('',#41001,1000.);
#10005=VECTOR('',#41004,1000.);
#10006=VECTOR('',#41011,1000.);
#10007=VECTOR('',#41012,1000.);
#10008=VECTOR('',#41021,10.);
#10009=VECTOR('',#41024,1000.);
#10010=VECTOR('',#41033,10.);
#10011=VECTOR('',#41034,10.);
#10012=VECTOR('',#41039,10.);
#10013=VECTOR('',#41042,10.);
#10014=VECTOR('',#41045,10.);
#10015=VECTOR('',#41048,10.);
#10016=VECTOR('',#41053,10.);
#10017=VECTOR('',#41056,10.);
#10018=VECTOR('',#41059,10.);
#10019=VECTOR('',#41060,1000.);
#10020=VECTOR('',#41067,1000.);
#10021=VECTOR('',#41072,1000.);
#10022=VECTOR('',#41075,1000.);
#10023=VECTOR('',#41078,1000.);
#10024=VECTOR('',#41079,1000.);
#10025=VECTOR('',#41084,1000.);
#10026=VECTOR('',#41087,1000.);
#10027=VECTOR('',#41094,1000.);
#10028=VECTOR('',#41097,1000.);
#10029=VECTOR('',#41100,1000.);
#10030=VECTOR('',#41111,1000.);
#10031=VECTOR('',#41120,1000.);
#10032=VECTOR('',#41123,1000.);
#10033=VECTOR('',#41126,1000.);
#10034=VECTOR('',#41129,10.);
#10035=VECTOR('',#41132,10.);
#10036=VECTOR('',#41137,10.);
#10037=VECTOR('',#41142,10.);
#10038=VECTOR('',#41145,10.);
#10039=VECTOR('',#41148,10.);
#10040=VECTOR('',#41149,10.);
#10041=VECTOR('',#41154,1000.);
#10042=VECTOR('',#41155,10.);
#10043=VECTOR('',#41158,10.);
#10044=VECTOR('',#41161,10.);
#10045=VECTOR('',#41170,1000.);
#10046=VECTOR('',#41173,1000.);
#10047=VECTOR('',#41178,1000.);
#10048=VECTOR('',#41183,1000.);
#10049=VECTOR('',#41186,1000.);
#10050=VECTOR('',#41193,1000.);
#10051=VECTOR('',#41196,1000.);
#10052=VECTOR('',#41197,1000.);
#10053=VECTOR('',#41202,1000.);
#10054=VECTOR('',#41207,1000.);
#10055=VECTOR('',#41210,1000.);
#10056=VECTOR('',#41213,5.5);
#10057=VECTOR('',#41220,5.5);
#10058=VECTOR('',#41229,1000.);
#10059=VECTOR('',#41230,1000.);
#10060=VECTOR('',#41235,1000.);
#10061=VECTOR('',#41236,1000.);
#10062=VECTOR('',#41237,1000.);
#10063=VECTOR('',#41238,1000.);
#10064=VECTOR('',#41239,1000.);
#10065=VECTOR('',#41240,1000.);
#10066=VECTOR('',#41241,1000.);
#10067=VECTOR('',#41242,1000.);
#10068=VECTOR('',#41247,1000.);
#10069=VECTOR('',#41252,1000.);
#10070=VECTOR('',#41253,1000.);
#10071=VECTOR('',#41254,1000.);
#10072=VECTOR('',#41255,1000.);
#10073=VECTOR('',#41256,1000.);
#10074=VECTOR('',#41257,1000.);
#10075=VECTOR('',#41258,1000.);
#10076=VECTOR('',#41259,1000.);
#10077=VECTOR('',#41260,1000.);
#10078=VECTOR('',#41265,1000.);
#10079=VECTOR('',#41270,1000.);
#10080=VECTOR('',#41275,1.25);
#10081=VECTOR('',#41280,1000.);
#10082=VECTOR('',#41285,1000.);
#10083=VECTOR('',#41296,1.25);
#10084=VECTOR('',#41303,1000.);
#10085=VECTOR('',#41310,1000.);
#10086=VECTOR('',#41311,1000.);
#10087=VECTOR('',#41312,1000.);
#10088=VECTOR('',#41319,10.);
#10089=VECTOR('',#41326,1000.);
#10090=VECTOR('',#41329,1000.);
#10091=VECTOR('',#41330,10.);
#10092=VECTOR('',#41331,1000.);
#10093=VECTOR('',#41334,4.7);
#10094=VECTOR('',#41353,4.7);
#10095=VECTOR('',#41372,1000.);
#10096=VECTOR('',#41375,1000.);
#10097=VECTOR('',#41378,1000.);
#10098=VECTOR('',#41383,1000.);
#10099=VECTOR('',#41384,1000.);
#10100=VECTOR('',#41385,1000.);
#10101=VECTOR('',#41392,1000.);
#10102=VECTOR('',#41393,1000.);
#10103=VECTOR('',#41394,1000.);
#10104=VECTOR('',#41395,1000.);
#10105=VECTOR('',#41398,1000.);
#10106=VECTOR('',#41423,1000.);
#10107=VECTOR('',#41424,1000.);
#10108=VECTOR('',#41431,1000.);
#10109=VECTOR('',#41432,1000.);
#10110=VECTOR('',#41453,1000.);
#10111=VECTOR('',#41466,1000.);
#10112=VECTOR('',#41489,1000.);
#10113=VECTOR('',#41504,1000.);
#10114=VECTOR('',#41513,1000.);
#10115=VECTOR('',#41518,1000.);
#10116=VECTOR('',#41531,1000.);
#10117=VECTOR('',#41532,1000.);
#10118=VECTOR('',#41533,1000.);
#10119=VECTOR('',#41538,1000.);
#10120=VECTOR('',#41539,1000.);
#10121=VECTOR('',#41540,1000.);
#10122=VECTOR('',#41541,1000.);
#10123=VECTOR('',#41542,1000.);
#10124=VECTOR('',#41543,1000.);
#10125=VECTOR('',#41548,1000.);
#10126=VECTOR('',#41551,1000.);
#10127=VECTOR('',#41552,1000.);
#10128=VECTOR('',#41557,1000.);
#10129=VECTOR('',#41558,1000.);
#10130=VECTOR('',#41559,1000.);
#10131=VECTOR('',#41560,1000.);
#10132=VECTOR('',#41565,1000.);
#10133=VECTOR('',#41568,1000.);
#10134=VECTOR('',#41569,1000.);
#10135=VECTOR('',#41578,1000.);
#10136=VECTOR('',#41579,1000.);
#10137=VECTOR('',#41580,1000.);
#10138=VECTOR('',#41581,1000.);
#10139=VECTOR('',#41582,1000.);
#10140=VECTOR('',#41583,1000.);
#10141=VECTOR('',#41584,1000.);
#10142=VECTOR('',#41589,1000.);
#10143=VECTOR('',#41592,1000.);
#10144=VECTOR('',#41597,1000.);
#10145=VECTOR('',#41598,1000.);
#10146=VECTOR('',#41601,1000.);
#10147=VECTOR('',#41608,1000.);
#10148=VECTOR('',#41609,1000.);
#10149=VECTOR('',#41610,1000.);
#10150=VECTOR('',#41611,1000.);
#10151=VECTOR('',#41612,1000.);
#10152=VECTOR('',#41615,1000.);
#10153=VECTOR('',#41616,1000.);
#10154=VECTOR('',#41617,1000.);
#10155=VECTOR('',#41620,1000.);
#10156=VECTOR('',#41627,1000.);
#10157=VECTOR('',#41628,1000.);
#10158=VECTOR('',#41633,1000.);
#10159=VECTOR('',#41636,1000.);
#10160=VECTOR('',#41637,1000.);
#10161=VECTOR('',#41642,1000.);
#10162=VECTOR('',#41647,1000.);
#10163=VECTOR('',#41648,1000.);
#10164=VECTOR('',#41649,1000.);
#10165=VECTOR('',#41650,1000.);
#10166=VECTOR('',#41657,1000.);
#10167=VECTOR('',#41660,1000.);
#10168=VECTOR('',#41663,1000.);
#10169=VECTOR('',#41666,1000.);
#10170=VECTOR('',#41669,1000.);
#10171=VECTOR('',#41670,1000.);
#10172=VECTOR('',#41671,1000.);
#10173=VECTOR('',#41672,1000.);
#10174=VECTOR('',#41675,1000.);
#10175=VECTOR('',#41676,1000.);
#10176=VECTOR('',#41677,1000.);
#10177=VECTOR('',#41678,1000.);
#10178=VECTOR('',#41679,1000.);
#10179=VECTOR('',#41682,1000.);
#10180=VECTOR('',#41683,1000.);
#10181=VECTOR('',#41684,1000.);
#10182=VECTOR('',#41685,1000.);
#10183=VECTOR('',#41686,1000.);
#10184=VECTOR('',#41689,1000.);
#10185=VECTOR('',#41690,1000.);
#10186=VECTOR('',#41691,1000.);
#10187=VECTOR('',#41692,1000.);
#10188=VECTOR('',#41695,1000.);
#10189=VECTOR('',#41696,1000.);
#10190=VECTOR('',#41697,1000.);
#10191=VECTOR('',#41698,1000.);
#10192=VECTOR('',#41701,1000.);
#10193=VECTOR('',#41702,1000.);
#10194=VECTOR('',#41703,1000.);
#10195=VECTOR('',#41704,1000.);
#10196=VECTOR('',#41705,1000.);
#10197=VECTOR('',#41708,1000.);
#10198=VECTOR('',#41709,1000.);
#10199=VECTOR('',#41710,1000.);
#10200=VECTOR('',#41711,1000.);
#10201=VECTOR('',#41712,1000.);
#10202=VECTOR('',#41715,1000.);
#10203=VECTOR('',#41716,1000.);
#10204=VECTOR('',#41717,1000.);
#10205=VECTOR('',#41718,1000.);
#10206=VECTOR('',#41725,1000.);
#10207=VECTOR('',#41732,1000.);
#10208=VECTOR('',#41741,1000.);
#10209=VECTOR('',#41746,1000.);
#10210=VECTOR('',#41749,1000.);
#10211=VECTOR('',#41754,1000.);
#10212=VECTOR('',#41757,1000.);
#10213=VECTOR('',#41768,1000.);
#10214=VECTOR('',#41775,1000.);
#10215=VECTOR('',#41788,1000.);
#10216=VECTOR('',#41809,1000.);
#10217=VECTOR('',#41810,1000.);
#10218=VECTOR('',#41811,1000.);
#10219=VECTOR('',#41818,1000.);
#10220=VECTOR('',#41819,1000.);
#10221=VECTOR('',#41824,1000.);
#10222=VECTOR('',#41843,1000.);
#10223=VECTOR('',#41876,1000.);
#10224=VECTOR('',#41881,1000.);
#10225=VECTOR('',#41884,1000.);
#10226=VECTOR('',#41893,1000.);
#10227=VECTOR('',#41894,1000.);
#10228=VECTOR('',#41895,1000.);
#10229=VECTOR('',#41902,1000.);
#10230=VECTOR('',#41913,1000.);
#10231=VECTOR('',#41928,1000.);
#10232=VECTOR('',#41937,1000.);
#10233=VECTOR('',#41938,1000.);
#10234=VECTOR('',#41939,1000.);
#10235=VECTOR('',#41946,1000.);
#10236=VECTOR('',#41947,1000.);
#10237=VECTOR('',#41952,1000.);
#10238=VECTOR('',#41961,1000.);
#10239=VECTOR('',#41972,1000.);
#10240=VECTOR('',#41983,1000.);
#10241=VECTOR('',#42004,1000.);
#10242=VECTOR('',#42007,1000.);
#10243=VECTOR('',#42010,1000.);
#10244=VECTOR('',#42013,1000.);
#10245=VECTOR('',#42016,1000.);
#10246=VECTOR('',#42019,1000.);
#10247=VECTOR('',#42022,1000.);
#10248=VECTOR('',#42025,1000.);
#10249=VECTOR('',#42030,1000.);
#10250=VECTOR('',#42037,1000.);
#10251=VECTOR('',#42050,1000.);
#10252=VECTOR('',#42073,1000.);
#10253=VECTOR('',#42074,1000.);
#10254=VECTOR('',#42081,1000.);
#10255=VECTOR('',#42082,1000.);
#10256=VECTOR('',#42083,1000.);
#10257=VECTOR('',#42088,1000.);
#10258=VECTOR('',#42109,1000.);
#10259=VECTOR('',#42140,1000.);
#10260=VECTOR('',#42145,1000.);
#10261=VECTOR('',#42148,1000.);
#10262=VECTOR('',#42157,1000.);
#10263=VECTOR('',#42158,1000.);
#10264=VECTOR('',#42159,1000.);
#10265=VECTOR('',#42164,1000.);
#10266=VECTOR('',#42169,1000.);
#10267=VECTOR('',#42186,1000.);
#10268=VECTOR('',#42187,1000.);
#10269=VECTOR('',#42194,1000.);
#10270=VECTOR('',#42195,1000.);
#10271=VECTOR('',#42196,1000.);
#10272=VECTOR('',#42203,1000.);
#10273=VECTOR('',#42226,1000.);
#10274=VECTOR('',#42241,1000.);
#10275=VECTOR('',#42246,1000.);
#10276=VECTOR('',#42265,1000.);
#10277=VECTOR('',#42268,1000.);
#10278=VECTOR('',#42271,1000.);
#10279=VECTOR('',#42274,1000.);
#10280=VECTOR('',#42277,1000.);
#10281=VECTOR('',#42278,1000.);
#10282=VECTOR('',#42281,1000.);
#10283=VECTOR('',#42284,1000.);
#10284=VECTOR('',#42289,1000.);
#10285=VECTOR('',#42294,1000.);
#10286=VECTOR('',#42369,1000.);
#10287=VECTOR('',#42374,1000.);
#10288=VECTOR('',#42377,1000.);
#10289=VECTOR('',#42384,1000.);
#10290=VECTOR('',#42443,0.730765926094);
#10291=VECTOR('',#42450,1000.);
#10292=VECTOR('',#42453,1000.);
#10293=VECTOR('',#42456,1000.);
#10294=VECTOR('',#42459,1000.);
#10295=VECTOR('',#42464,1000.);
#10296=VECTOR('',#42477,1000.);
#10297=VECTOR('',#42486,1000.);
#10298=VECTOR('',#42495,1000.);
#10299=VECTOR('',#42506,1000.);
#10300=VECTOR('',#42507,1000.);
#10301=VECTOR('',#42508,1000.);
#10302=VECTOR('',#42513,1000.);
#10303=VECTOR('',#42518,1000.);
#10304=VECTOR('',#42519,1000.);
#10305=VECTOR('',#42524,1000.);
#10306=VECTOR('',#42527,1000.);
#10307=VECTOR('',#42528,1000.);
#10308=VECTOR('',#42533,1000.);
#10309=VECTOR('',#42538,1000.);
#10310=VECTOR('',#42539,1000.);
#10311=VECTOR('',#42540,1000.);
#10312=VECTOR('',#42541,1000.);
#10313=VECTOR('',#42552,1000.);
#10314=VECTOR('',#42553,1000.);
#10315=VECTOR('',#42560,1000.);
#10316=VECTOR('',#42567,1000.);
#10317=VECTOR('',#42578,1000.);
#10318=VECTOR('',#42589,1000.);
#10319=VECTOR('',#42602,1000.);
#10320=VECTOR('',#42605,1000.);
#10321=VECTOR('',#42616,1000.);
#10322=VECTOR('',#42621,1000.);
#10323=VECTOR('',#42624,1000.);
#10324=VECTOR('',#42625,1000.);
#10325=VECTOR('',#42626,1000.);
#10326=VECTOR('',#42627,1000.);
#10327=VECTOR('',#42632,1000.);
#10328=VECTOR('',#42655,1000.);
#10329=VECTOR('',#42658,1000.);
#10330=VECTOR('',#42659,1000.);
#10331=VECTOR('',#42660,1000.);
#10332=VECTOR('',#42663,1000.);
#10333=VECTOR('',#42664,1000.);
#10334=VECTOR('',#42665,1000.);
#10335=VECTOR('',#42668,1000.);
#10336=VECTOR('',#42671,1000.);
#10337=VECTOR('',#42674,1000.);
#10338=VECTOR('',#42677,1000.);
#10339=VECTOR('',#42682,1000.);
#10340=VECTOR('',#42685,1000.);
#10341=VECTOR('',#42688,1000.);
#10342=VECTOR('',#42691,1000.);
#10343=VECTOR('',#42694,1000.);
#10344=VECTOR('',#42699,1000.);
#10345=VECTOR('',#42702,1000.);
#10346=VECTOR('',#42719,1000.);
#10347=VECTOR('',#42726,1000.);
#10348=VECTOR('',#42729,1000.);
#10349=VECTOR('',#42738,1000.);
#10350=VECTOR('',#42739,1000.);
#10351=VECTOR('',#42740,1000.);
#10352=VECTOR('',#42759,1000.);
#10353=VECTOR('',#42776,1000.);
#10354=VECTOR('',#42789,1000.);
#10355=VECTOR('',#42808,1000.);
#10356=VECTOR('',#42825,1000.);
#10357=VECTOR('',#42836,1000.);
#10358=VECTOR('',#42855,1000.);
#10359=VECTOR('',#42866,1000.);
#10360=VECTOR('',#42877,1000.);
#10361=VECTOR('',#42888,1000.);
#10362=VECTOR('',#42899,1000.);
#10363=VECTOR('',#42906,1000.);
#10364=VECTOR('',#42913,1000.);
#10365=VECTOR('',#42924,1000.);
#10366=VECTOR('',#42931,1000.);
#10367=VECTOR('',#42938,1000.);
#10368=VECTOR('',#42947,1000.);
#10369=VECTOR('',#42970,1000.);
#10370=VECTOR('',#42971,1000.);
#10371=VECTOR('',#42982,1000.);
#10372=VECTOR('',#42985,1000.);
#10373=VECTOR('',#42994,1000.);
#10374=VECTOR('',#42995,1000.);
#10375=VECTOR('',#43004,1000.);
#10376=VECTOR('',#43007,1000.);
#10377=VECTOR('',#43016,1000.);
#10378=VECTOR('',#43031,1000.);
#10379=VECTOR('',#43042,1000.);
#10380=VECTOR('',#43045,1000.);
#10381=VECTOR('',#43046,1000.);
#10382=VECTOR('',#43047,1000.);
#10383=VECTOR('',#43050,1000.);
#10384=VECTOR('',#43063,1000.);
#10385=VECTOR('',#43064,1000.);
#10386=VECTOR('',#43065,1000.);
#10387=VECTOR('',#43078,1000.);
#10388=VECTOR('',#43081,1000.);
#10389=VECTOR('',#43084,1000.);
#10390=VECTOR('',#43091,1000.);
#10391=VECTOR('',#43094,1000.);
#10392=VECTOR('',#43099,1000.);
#10393=VECTOR('',#43100,1000.);
#10394=VECTOR('',#43103,1000.);
#10395=VECTOR('',#43108,1000.);
#10396=VECTOR('',#43109,1000.);
#10397=VECTOR('',#43112,1000.);
#10398=VECTOR('',#43117,1000.);
#10399=VECTOR('',#43118,1000.);
#10400=VECTOR('',#43121,1000.);
#10401=VECTOR('',#43126,1000.);
#10402=VECTOR('',#43127,1000.);
#10403=VECTOR('',#43130,1000.);
#10404=VECTOR('',#43135,1000.);
#10405=VECTOR('',#43136,1000.);
#10406=VECTOR('',#43143,1000.);
#10407=VECTOR('',#43144,1000.);
#10408=VECTOR('',#43145,1000.);
#10409=VECTOR('',#43152,1000.);
#10410=VECTOR('',#43153,1000.);
#10411=VECTOR('',#43154,1000.);
#10412=VECTOR('',#43157,1000.);
#10413=VECTOR('',#43162,1000.);
#10414=VECTOR('',#43163,1000.);
#10415=VECTOR('',#43170,1000.);
#10416=VECTOR('',#43171,1000.);
#10417=VECTOR('',#43172,1000.);
#10418=VECTOR('',#43179,1000.);
#10419=VECTOR('',#43180,1000.);
#10420=VECTOR('',#43181,1000.);
#10421=VECTOR('',#43184,1000.);
#10422=VECTOR('',#43189,1000.);
#10423=VECTOR('',#43194,2.65);
#10424=VECTOR('',#43207,1000.);
#10425=VECTOR('',#43218,1000.);
#10426=VECTOR('',#43221,1000.);
#10427=VECTOR('',#43228,1000.);
#10428=VECTOR('',#43231,1000.);
#10429=VECTOR('',#43238,1000.);
#10430=VECTOR('',#43259,1000.);
#10431=VECTOR('',#43270,1000.);
#10432=VECTOR('',#43287,1000.);
#10433=VECTOR('',#43298,1000.);
#10434=VECTOR('',#43309,1000.);
#10435=VECTOR('',#43320,1000.);
#10436=VECTOR('',#43331,1000.);
#10437=VECTOR('',#43340,1000.);
#10438=VECTOR('',#43351,1000.);
#10439=VECTOR('',#43364,1000.);
#10440=VECTOR('',#43373,1000.);
#10441=VECTOR('',#43384,1000.);
#10442=VECTOR('',#43395,1000.);
#10443=VECTOR('',#43408,0.781285626506968);
#10444=VECTOR('',#43415,1000.);
#10445=VECTOR('',#43416,1000.);
#10446=VECTOR('',#43427,1000.);
#10447=VECTOR('',#43446,1000.);
#10448=VECTOR('',#43461,1000.);
#10449=VECTOR('',#43474,1000.);
#10450=VECTOR('',#43489,1000.);
#10451=VECTOR('',#43490,1000.);
#10452=VECTOR('',#43513,1.4);
#10453=VECTOR('',#43516,1000.);
#10454=VECTOR('',#43529,1000.);
#10455=VECTOR('',#43530,1000.);
#10456=VECTOR('',#43543,1000.);
#10457=VECTOR('',#43544,1000.);
#10458=VECTOR('',#43553,1000.);
#10459=VECTOR('',#43554,1000.);
#10460=VECTOR('',#43563,1000.);
#10461=VECTOR('',#43584,1000.);
#10462=VECTOR('',#43587,1000.);
#10463=VECTOR('',#43598,1000.);
#10464=VECTOR('',#43599,1000.);
#10465=VECTOR('',#43604,2.65);
#10466=VECTOR('',#43607,1000.);
#10467=VECTOR('',#43610,1000.);
#10468=VECTOR('',#43623,1000.);
#10469=VECTOR('',#43624,1000.);
#10470=VECTOR('',#43631,1000.);
#10471=VECTOR('',#43634,1000.);
#10472=VECTOR('',#43637,1000.);
#10473=VECTOR('',#43640,1000.);
#10474=VECTOR('',#43643,1000.);
#10475=VECTOR('',#43664,1000.);
#10476=VECTOR('',#43667,1000.);
#10477=VECTOR('',#43670,1000.);
#10478=VECTOR('',#43673,1000.);
#10479=VECTOR('',#43674,1000.);
#10480=VECTOR('',#43675,1000.);
#10481=VECTOR('',#43688,1000.);
#10482=VECTOR('',#43699,1000.);
#10483=VECTOR('',#43710,1000.);
#10484=VECTOR('',#43719,1000.);
#10485=VECTOR('',#43720,1000.);
#10486=VECTOR('',#43723,1000.);
#10487=VECTOR('',#43724,1000.);
#10488=VECTOR('',#43727,1000.);
#10489=VECTOR('',#43730,1000.);
#10490=VECTOR('',#43733,1000.);
#10491=VECTOR('',#43736,1000.);
#10492=VECTOR('',#43749,1000.);
#10493=VECTOR('',#43758,1000.);
#10494=VECTOR('',#43761,1000.);
#10495=VECTOR('',#43766,1000.);
#10496=VECTOR('',#43771,1000.);
#10497=VECTOR('',#43792,1000.);
#10498=VECTOR('',#43813,16.4);
#10499=VECTOR('',#43820,1000.);
#10500=VECTOR('',#43821,1000.);
#10501=VECTOR('',#43824,1000.);
#10502=VECTOR('',#43825,1000.);
#10503=VECTOR('',#43834,1000.);
#10504=VECTOR('',#43837,1000.);
#10505=VECTOR('',#43842,1000.);
#10506=VECTOR('',#43843,1000.);
#10507=VECTOR('',#43844,1000.);
#10508=VECTOR('',#43847,1000.);
#10509=VECTOR('',#43848,1000.);
#10510=VECTOR('',#43849,1000.);
#10511=VECTOR('',#43858,1000.);
#10512=VECTOR('',#43861,1000.);
#10513=VECTOR('',#43866,1000.);
#10514=VECTOR('',#43867,1000.);
#10515=VECTOR('',#43868,1000.);
#10516=VECTOR('',#43871,1000.);
#10517=VECTOR('',#43872,1000.);
#10518=VECTOR('',#43873,1000.);
#10519=VECTOR('',#43884,16.4);
#10520=VECTOR('',#43887,1000.);
#10521=VECTOR('',#43890,1000.);
#10522=VECTOR('',#43893,1000.);
#10523=VECTOR('',#43896,1000.);
#10524=VECTOR('',#43899,1000.);
#10525=VECTOR('',#43902,1000.);
#10526=VECTOR('',#43905,1000.);
#10527=VECTOR('',#43908,1000.);
#10528=VECTOR('',#43911,1000.);
#10529=VECTOR('',#43914,1000.);
#10530=VECTOR('',#43917,1000.);
#10531=VECTOR('',#43920,1000.);
#10532=VECTOR('',#43923,1000.);
#10533=VECTOR('',#43926,1000.);
#10534=VECTOR('',#43931,1000.);
#10535=VECTOR('',#43934,1000.);
#10536=VECTOR('',#43937,1000.);
#10537=VECTOR('',#43940,1000.);
#10538=VECTOR('',#43943,17.4);
#10539=VECTOR('',#43946,1000.);
#10540=VECTOR('',#43949,1000.);
#10541=VECTOR('',#43952,1000.);
#10542=VECTOR('',#43955,1000.);
#10543=VECTOR('',#43960,10.);
#10544=VECTOR('',#43961,1000.);
#10545=VECTOR('',#43962,1000.);
#10546=VECTOR('',#43965,1000.);
#10547=VECTOR('',#43966,1000.);
#10548=VECTOR('',#43967,10.);
#10549=VECTOR('',#43974,1000.);
#10550=VECTOR('',#43983,1000.);
#10551=VECTOR('',#43986,1000.);
#10552=VECTOR('',#43991,1000.);
#10553=VECTOR('',#44000,1000.);
#10554=VECTOR('',#44005,1000.);
#10555=VECTOR('',#44006,10.);
#10556=VECTOR('',#44013,1000.);
#10557=VECTOR('',#44016,1000.);
#10558=VECTOR('',#44019,10.);
#10559=VECTOR('',#44024,1000.);
#10560=VECTOR('',#44027,1000.);
#10561=VECTOR('',#44030,10.);
#10562=VECTOR('',#44031,1000.);
#10563=VECTOR('',#44032,1000.);
#10564=VECTOR('',#44039,1000.);
#10565=VECTOR('',#44048,1000.);
#10566=VECTOR('',#44049,1000.);
#10567=VECTOR('',#44052,1000.);
#10568=VECTOR('',#44055,1000.);
#10569=VECTOR('',#44056,10.);
#10570=VECTOR('',#44059,1000.);
#10571=VECTOR('',#44064,1000.);
#10572=VECTOR('',#44065,10.);
#10573=VECTOR('',#44070,1000.);
#10574=VECTOR('',#44077,1000.);
#10575=VECTOR('',#44088,1000.);
#10576=VECTOR('',#44091,1000.);
#10577=VECTOR('',#44098,1000.);
#10578=VECTOR('',#44107,1000.);
#10579=VECTOR('',#44110,10.);
#10580=VECTOR('',#44113,1000.);
#10581=VECTOR('',#44122,1000.);
#10582=VECTOR('',#44127,1000.);
#10583=VECTOR('',#44128,1000.);
#10584=VECTOR('',#44129,10.);
#10585=VECTOR('',#44132,1000.);
#10586=VECTOR('',#44145,1000.);
#10587=VECTOR('',#44154,1000.);
#10588=VECTOR('',#44157,10.);
#10589=VECTOR('',#44158,1000.);
#10590=VECTOR('',#44161,1000.);
#10591=VECTOR('',#44166,1000.);
#10592=VECTOR('',#44171,10.);
#10593=VECTOR('',#44172,1000.);
#10594=VECTOR('',#44175,1000.);
#10595=VECTOR('',#44190,1000.);
#10596=VECTOR('',#44201,1000.);
#10597=VECTOR('',#44204,1000.);
#10598=VECTOR('',#44209,1000.);
#10599=VECTOR('',#44220,1000.);
#10600=VECTOR('',#44223,10.);
#10601=VECTOR('',#44226,10.);
#10602=VECTOR('',#44227,1000.);
#10603=VECTOR('',#44228,1000.);
#10604=VECTOR('',#44231,1000.);
#10605=VECTOR('',#44232,1000.);
#10606=VECTOR('',#44233,10.);
#10607=VECTOR('',#44240,1000.);
#10608=VECTOR('',#44249,1000.);
#10609=VECTOR('',#44252,1000.);
#10610=VECTOR('',#44257,1000.);
#10611=VECTOR('',#44266,1000.);
#10612=VECTOR('',#44271,1000.);
#10613=VECTOR('',#44272,10.);
#10614=VECTOR('',#44279,1000.);
#10615=VECTOR('',#44282,1000.);
#10616=VECTOR('',#44285,10.);
#10617=VECTOR('',#44288,1000.);
#10618=VECTOR('',#44289,1000.);
#10619=VECTOR('',#44292,1000.);
#10620=VECTOR('',#44295,1000.);
#10621=VECTOR('',#44298,1000.);
#10622=VECTOR('',#44301,1000.);
#10623=VECTOR('',#44304,1000.);
#10624=VECTOR('',#44305,1000.);
#10625=VECTOR('',#44308,1000.);
#10626=VECTOR('',#44311,1000.);
#10627=VECTOR('',#44314,1000.);
#10628=VECTOR('',#44317,1000.);
#10629=VECTOR('',#44320,1000.);
#10630=VECTOR('',#44323,1000.);
#10631=VECTOR('',#44328,1000.);
#10632=VECTOR('',#44331,1000.);
#10633=VECTOR('',#44338,9.15);
#10634=VECTOR('',#44355,1000.);
#10635=VECTOR('',#44358,1000.);
#10636=VECTOR('',#44361,1000.);
#10637=VECTOR('',#44364,1000.);
#10638=VECTOR('',#44367,1000.);
#10639=VECTOR('',#44370,1000.);
#10640=VECTOR('',#44373,1000.);
#10641=VECTOR('',#44374,1000.);
#10642=VECTOR('',#44377,1000.);
#10643=VECTOR('',#44380,1000.);
#10644=VECTOR('',#44383,1000.);
#10645=VECTOR('',#44388,1000.);
#10646=VECTOR('',#44391,1000.);
#10647=VECTOR('',#44396,1000.);
#10648=VECTOR('',#44399,1000.);
#10649=VECTOR('',#44404,1000.);
#10650=VECTOR('',#44407,1000.);
#10651=VECTOR('',#44412,1000.);
#10652=VECTOR('',#44421,1000.);
#10653=VECTOR('',#44424,1000.);
#10654=VECTOR('',#44427,1000.);
#10655=VECTOR('',#44436,1000.);
#10656=VECTOR('',#44441,1000.);
#10657=VECTOR('',#44444,1000.);
#10658=VECTOR('',#44447,1000.);
#10659=VECTOR('',#44450,1000.);
#10660=VECTOR('',#44455,1000.);
#10661=VECTOR('',#44456,1000.);
#10662=VECTOR('',#44457,1000.);
#10663=VECTOR('',#44462,1000.);
#10664=VECTOR('',#44467,1000.);
#10665=VECTOR('',#44476,1000.);
#10666=VECTOR('',#44477,1000.);
#10667=VECTOR('',#44482,1000.);
#10668=VECTOR('',#44483,1000.);
#10669=VECTOR('',#44486,1000.);
#10670=VECTOR('',#44489,1000.);
#10671=VECTOR('',#44492,1000.);
#10672=VECTOR('',#44509,1000.);
#10673=VECTOR('',#44510,1000.);
#10674=VECTOR('',#44551,1000.);
#10675=VECTOR('',#44570,1000.);
#10676=VECTOR('',#44579,1000.);
#10677=VECTOR('',#44580,1000.);
#10678=VECTOR('',#44581,1000.);
#10679=VECTOR('',#44582,1000.);
#10680=VECTOR('',#44583,1000.);
#10681=VECTOR('',#44584,1000.);
#10682=VECTOR('',#44589,1000.);
#10683=VECTOR('',#44594,1000.);
#10684=VECTOR('',#44603,1000.);
#10685=VECTOR('',#44608,1000.);
#10686=VECTOR('',#44609,1000.);
#10687=VECTOR('',#44610,1000.);
#10688=VECTOR('',#44613,1000.);
#10689=VECTOR('',#44622,1000.);
#10690=VECTOR('',#44625,1000.);
#10691=VECTOR('',#44646,1000.);
#10692=VECTOR('',#44673,1000.);
#10693=VECTOR('',#44674,1000.);
#10694=VECTOR('',#44685,1000.);
#10695=VECTOR('',#44686,1000.);
#10696=VECTOR('',#44703,1000.);
#10697=VECTOR('',#44704,1000.);
#10698=VECTOR('',#44705,1000.);
#10699=VECTOR('',#44714,1000.);
#10700=VECTOR('',#44715,1000.);
#10701=VECTOR('',#44722,1000.);
#10702=VECTOR('',#44723,1000.);
#10703=VECTOR('',#44724,1000.);
#10704=VECTOR('',#44731,1000.);
#10705=VECTOR('',#44732,1000.);
#10706=VECTOR('',#44743,1000.);
#10707=VECTOR('',#44766,1000.);
#10708=VECTOR('',#44827,1000.);
#10709=VECTOR('',#44828,1000.);
#10710=VECTOR('',#44829,1000.);
#10711=VECTOR('',#44830,1000.);
#10712=VECTOR('',#44835,1000.);
#10713=VECTOR('',#44838,1000.);
#10714=VECTOR('',#44841,1000.);
#10715=VECTOR('',#44846,1000.);
#10716=VECTOR('',#44849,1000.);
#10717=VECTOR('',#44850,1000.);
#10718=VECTOR('',#44853,1000.);
#10719=VECTOR('',#44854,1000.);
#10720=VECTOR('',#44859,1000.);
#10721=VECTOR('',#44862,1000.);
#10722=VECTOR('',#44863,1000.);
#10723=VECTOR('',#44866,1000.);
#10724=VECTOR('',#44873,1000.);
#10725=VECTOR('',#44876,1000.);
#10726=VECTOR('',#44877,1000.);
#10727=VECTOR('',#44878,1000.);
#10728=VECTOR('',#44901,1000.);
#10729=VECTOR('',#44902,1000.);
#10730=VECTOR('',#44907,1000.);
#10731=VECTOR('',#44910,1000.);
#10732=VECTOR('',#44911,1000.);
#10733=VECTOR('',#44912,1000.);
#10734=VECTOR('',#44913,1000.);
#10735=VECTOR('',#44918,1000.);
#10736=VECTOR('',#44927,1000.);
#10737=VECTOR('',#44932,1000.);
#10738=VECTOR('',#44937,1000.);
#10739=VECTOR('',#44938,1000.);
#10740=VECTOR('',#44939,1000.);
#10741=VECTOR('',#44942,1000.);
#10742=VECTOR('',#44949,1000.);
#10743=VECTOR('',#44960,1000.);
#10744=VECTOR('',#44963,1000.);
#10745=VECTOR('',#44986,1000.);
#10746=VECTOR('',#44987,1000.);
#10747=VECTOR('',#45024,1000.);
#10748=VECTOR('',#45025,1000.);
#10749=VECTOR('',#45084,1000.);
#10750=VECTOR('',#45085,1000.);
#10751=VECTOR('',#45120,1000.);
#10752=VECTOR('',#45121,1000.);
#10753=VECTOR('',#45158,1000.);
#10754=VECTOR('',#45159,1000.);
#10755=VECTOR('',#45162,1000.);
#10756=VECTOR('',#45165,1000.);
#10757=VECTOR('',#45168,1000.);
#10758=VECTOR('',#45169,1000.);
#10759=VECTOR('',#45210,1000.);
#10760=VECTOR('',#45211,1000.);
#10761=VECTOR('',#45262,1000.);
#10762=VECTOR('',#45263,1000.);
#10763=VECTOR('',#45274,1000.);
#10764=VECTOR('',#45277,1000.);
#10765=VECTOR('',#45328,1000.);
#10766=VECTOR('',#45347,1000.);
#10767=VECTOR('',#45364,1000.);
#10768=VECTOR('',#45367,1000.);
#10769=VECTOR('',#45380,1000.);
#10770=VECTOR('',#45383,1000.);
#10771=VECTOR('',#45386,1000.);
#10772=VECTOR('',#45389,1000.);
#10773=VECTOR('',#45392,1000.);
#10774=VECTOR('',#45401,1000.);
#10775=VECTOR('',#45402,1000.);
#10776=VECTOR('',#45409,1000.);
#10777=VECTOR('',#45430,1000.);
#10778=VECTOR('',#45457,1000.);
#10779=VECTOR('',#45458,1000.);
#10780=VECTOR('',#45459,1000.);
#10781=VECTOR('',#45462,1000.);
#10782=VECTOR('',#45463,1000.);
#10783=VECTOR('',#45468,1000.);
#10784=VECTOR('',#45471,1000.);
#10785=VECTOR('',#45472,1000.);
#10786=VECTOR('',#45477,1000.);
#10787=VECTOR('',#45482,1000.);
#10788=VECTOR('',#45485,1000.);
#10789=VECTOR('',#45488,1000.);
#10790=VECTOR('',#45493,1000.);
#10791=VECTOR('',#45494,1000.);
#10792=VECTOR('',#45497,1000.);
#10793=VECTOR('',#45500,1000.);
#10794=VECTOR('',#45503,1000.);
#10795=VECTOR('',#45506,1000.);
#10796=VECTOR('',#45511,1000.);
#10797=VECTOR('',#45512,1000.);
#10798=VECTOR('',#45515,1000.);
#10799=VECTOR('',#45518,1000.);
#10800=VECTOR('',#45523,1000.);
#10801=VECTOR('',#45528,1000.);
#10802=VECTOR('',#45531,1000.);
#10803=VECTOR('',#45538,1000.);
#10804=VECTOR('',#45541,1000.);
#10805=VECTOR('',#45560,1000.);
#10806=VECTOR('',#45563,1000.);
#10807=VECTOR('',#45582,1000.);
#10808=VECTOR('',#45601,1000.);
#10809=VECTOR('',#45622,1000.);
#10810=VECTOR('',#45623,1000.);
#10811=VECTOR('',#45638,1000.);
#10812=VECTOR('',#45661,1000.);
#10813=VECTOR('',#45688,1000.);
#10814=VECTOR('',#45691,1000.);
#10815=VECTOR('',#45694,1000.);
#10816=VECTOR('',#45697,1000.);
#10817=VECTOR('',#45706,1000.);
#10818=VECTOR('',#45707,1000.);
#10819=VECTOR('',#45710,1000.);
#10820=VECTOR('',#45713,1000.);
#10821=VECTOR('',#45720,1000.);
#10822=VECTOR('',#45743,1000.);
#10823=VECTOR('',#45784,1000.);
#10824=VECTOR('',#45789,1000.);
#10825=VECTOR('',#45794,1000.);
#10826=VECTOR('',#45825,1000.);
#10827=VECTOR('',#45828,1000.);
#10828=VECTOR('',#45859,1000.);
#10829=VECTOR('',#45860,1000.);
#10830=VECTOR('',#45863,1000.);
#10831=VECTOR('',#45866,1000.);
#10832=VECTOR('',#45871,1000.);
#10833=VECTOR('',#45880,1000.);
#10834=VECTOR('',#45885,1000.);
#10835=VECTOR('',#45890,1000.);
#10836=VECTOR('',#45893,1000.);
#10837=VECTOR('',#45894,1000.);
#10838=VECTOR('',#45899,1000.);
#10839=VECTOR('',#45904,1000.);
#10840=VECTOR('',#45909,1000.);
#10841=VECTOR('',#45912,1000.);
#10842=VECTOR('',#45913,1000.);
#10843=VECTOR('',#45962,1000.);
#10844=VECTOR('',#45977,1000.);
#10845=VECTOR('',#45980,1000.);
#10846=VECTOR('',#46003,1000.);
#10847=VECTOR('',#46006,1000.);
#10848=VECTOR('',#46017,1000.);
#10849=VECTOR('',#46022,1000.);
#10850=VECTOR('',#46025,1000.);
#10851=VECTOR('',#46028,1000.);
#10852=VECTOR('',#46031,1000.);
#10853=VECTOR('',#46034,1000.);
#10854=VECTOR('',#46037,1000.);
#10855=VECTOR('',#46038,1000.);
#10856=VECTOR('',#46039,1000.);
#10857=VECTOR('',#46044,1000.);
#10858=VECTOR('',#46053,1000.);
#10859=VECTOR('',#46058,1000.);
#10860=VECTOR('',#46059,1000.);
#10861=VECTOR('',#46064,1000.);
#10862=VECTOR('',#46067,1000.);
#10863=VECTOR('',#46068,1000.);
#10864=VECTOR('',#46071,1000.);
#10865=VECTOR('',#46074,1000.);
#10866=VECTOR('',#46095,1000.);
#10867=VECTOR('',#46096,1000.);
#10868=VECTOR('',#46137,1000.);
#10869=VECTOR('',#46154,1000.);
#10870=VECTOR('',#46165,1000.);
#10871=VECTOR('',#46166,1000.);
#10872=VECTOR('',#46167,1000.);
#10873=VECTOR('',#46168,1000.);
#10874=VECTOR('',#46169,1000.);
#10875=VECTOR('',#46170,1000.);
#10876=VECTOR('',#46175,1000.);
#10877=VECTOR('',#46184,1000.);
#10878=VECTOR('',#46189,1000.);
#10879=VECTOR('',#46194,1000.);
#10880=VECTOR('',#46195,1000.);
#10881=VECTOR('',#46196,1000.);
#10882=VECTOR('',#46203,1000.);
#10883=VECTOR('',#46206,1000.);
#10884=VECTOR('',#46217,1000.);
#10885=VECTOR('',#46236,1000.);
#10886=VECTOR('',#46269,1000.);
#10887=VECTOR('',#46270,1000.);
#10888=VECTOR('',#46281,1000.);
#10889=VECTOR('',#46282,1000.);
#10890=VECTOR('',#46297,1000.);
#10891=VECTOR('',#46298,1000.);
#10892=VECTOR('',#46299,1000.);
#10893=VECTOR('',#46306,1000.);
#10894=VECTOR('',#46307,1000.);
#10895=VECTOR('',#46316,1000.);
#10896=VECTOR('',#46317,1000.);
#10897=VECTOR('',#46318,1000.);
#10898=VECTOR('',#46327,1000.);
#10899=VECTOR('',#46328,1000.);
#10900=VECTOR('',#46337,1000.);
#10901=VECTOR('',#46360,1000.);
#10902=VECTOR('',#46425,1000.);
#10903=VECTOR('',#46430,1000.);
#10904=VECTOR('',#46431,1000.);
#10905=VECTOR('',#46432,1000.);
#10906=VECTOR('',#46435,1000.);
#10907=VECTOR('',#46444,1000.);
#10908=VECTOR('',#46447,1000.);
#10909=VECTOR('',#46450,1000.);
#10910=VECTOR('',#46459,1000.);
#10911=VECTOR('',#46462,1000.);
#10912=VECTOR('',#46465,1000.);
#10913=VECTOR('',#46466,1000.);
#10914=VECTOR('',#46471,1000.);
#10915=VECTOR('',#46476,1000.);
#10916=VECTOR('',#46479,1000.);
#10917=VECTOR('',#46480,1000.);
#10918=VECTOR('',#46485,1000.);
#10919=VECTOR('',#46488,1000.);
#10920=VECTOR('',#46489,1000.);
#10921=VECTOR('',#46490,1000.);
#10922=VECTOR('',#46513,1000.);
#10923=VECTOR('',#46514,1000.);
#10924=VECTOR('',#46519,1000.);
#10925=VECTOR('',#46524,1000.);
#10926=VECTOR('',#46527,1000.);
#10927=VECTOR('',#46528,1000.);
#10928=VECTOR('',#46529,1000.);
#10929=VECTOR('',#46530,1000.);
#10930=VECTOR('',#46533,1000.);
#10931=VECTOR('',#46538,1000.);
#10932=VECTOR('',#46543,1000.);
#10933=VECTOR('',#46552,1000.);
#10934=VECTOR('',#46557,1000.);
#10935=VECTOR('',#46558,1000.);
#10936=VECTOR('',#46559,1000.);
#10937=VECTOR('',#46564,1000.);
#10938=VECTOR('',#46569,1000.);
#10939=VECTOR('',#46582,1000.);
#10940=VECTOR('',#46585,1000.);
#10941=VECTOR('',#46608,1000.);
#10942=VECTOR('',#46609,1000.);
#10943=VECTOR('',#46644,1000.);
#10944=VECTOR('',#46645,1000.);
#10945=VECTOR('',#46702,1000.);
#10946=VECTOR('',#46703,1000.);
#10947=VECTOR('',#46740,1000.);
#10948=VECTOR('',#46741,1000.);
#10949=VECTOR('',#46776,1000.);
#10950=VECTOR('',#46777,1000.);
#10951=VECTOR('',#46780,1000.);
#10952=VECTOR('',#46781,1000.);
#10953=VECTOR('',#46784,1000.);
#10954=VECTOR('',#46787,1000.);
#10955=VECTOR('',#46826,1000.);
#10956=VECTOR('',#46827,1000.);
#10957=VECTOR('',#46876,1000.);
#10958=VECTOR('',#46879,1000.);
#10959=VECTOR('',#46894,1000.);
#10960=VECTOR('',#46897,1000.);
#10961=VECTOR('',#46932,1000.);
#10962=VECTOR('',#46939,1000.);
#10963=VECTOR('',#46950,1000.);
#10964=VECTOR('',#46961,1000.);
#10965=VECTOR('',#46976,1000.);
#10966=VECTOR('',#46989,1000.);
#10967=VECTOR('',#47000,1000.);
#10968=VECTOR('',#47011,1000.);
#10969=VECTOR('',#47020,1000.);
#10970=VECTOR('',#47023,1000.);
#10971=VECTOR('',#47042,1000.);
#10972=VECTOR('',#47075,1000.);
#10973=VECTOR('',#47080,1000.);
#10974=VECTOR('',#47085,1000.);
#10975=VECTOR('',#47088,1000.);
#10976=VECTOR('',#47093,1000.);
#10977=VECTOR('',#47106,1000.);
#10978=VECTOR('',#47111,1000.);
#10979=VECTOR('',#47122,1000.);
#10980=VECTOR('',#47127,1000.);
#10981=VECTOR('',#47130,1000.);
#10982=VECTOR('',#47133,1000.);
#10983=VECTOR('',#47140,1000.);
#10984=VECTOR('',#47181,1000.);
#10985=VECTOR('',#47182,1000.);
#10986=VECTOR('',#47183,1000.);
#10987=VECTOR('',#47186,1000.);
#10988=VECTOR('',#47187,1000.);
#10989=VECTOR('',#47190,1000.);
#10990=VECTOR('',#47195,1000.);
#10991=VECTOR('',#47196,1000.);
#10992=VECTOR('',#47199,1000.);
#10993=VECTOR('',#47204,1000.);
#10994=VECTOR('',#47209,1000.);
#10995=VECTOR('',#47212,1000.);
#10996=VECTOR('',#47217,1000.);
#10997=VECTOR('',#47218,1000.);
#10998=VECTOR('',#47221,1000.);
#10999=VECTOR('',#47224,1000.);
#11000=VECTOR('',#47227,1000.);
#11001=VECTOR('',#47230,1000.);
#11002=VECTOR('',#47235,1000.);
#11003=VECTOR('',#47236,1000.);
#11004=VECTOR('',#47239,1000.);
#11005=VECTOR('',#47242,1000.);
#11006=VECTOR('',#47245,1000.);
#11007=VECTOR('',#47250,1000.);
#11008=VECTOR('',#47257,1000.);
#11009=VECTOR('',#47260,1000.);
#11010=VECTOR('',#47265,1000.);
#11011=VECTOR('',#47284,1000.);
#11012=VECTOR('',#47289,1000.);
#11013=VECTOR('',#47306,1000.);
#11014=VECTOR('',#47325,1000.);
#11015=VECTOR('',#47342,1000.);
#11016=VECTOR('',#47343,1000.);
#11017=VECTOR('',#47354,1000.);
#11018=VECTOR('',#47379,1000.);
#11019=VECTOR('',#47386,1000.);
#11020=VECTOR('',#47413,1000.);
#11021=VECTOR('',#47416,1000.);
#11022=VECTOR('',#47419,1000.);
#11023=VECTOR('',#47426,1000.);
#11024=VECTOR('',#47433,1000.);
#11025=VECTOR('',#47436,1000.);
#11026=VECTOR('',#47439,1000.);
#11027=VECTOR('',#47444,1000.);
#11028=VECTOR('',#47467,1000.);
#11029=VECTOR('',#47508,1000.);
#11030=VECTOR('',#47515,1000.);
#11031=VECTOR('',#47520,1000.);
#11032=VECTOR('',#47533,1000.);
#11033=VECTOR('',#47538,1000.);
#11034=VECTOR('',#47543,1000.);
#11035=VECTOR('',#47548,1000.);
#11036=VECTOR('',#47563,1000.);
#11037=VECTOR('',#47572,1000.);
#11038=VECTOR('',#47575,1000.);
#11039=VECTOR('',#47578,1000.);
#11040=VECTOR('',#47587,1000.);
#11041=VECTOR('',#47594,1000.);
#11042=VECTOR('',#47623,1000.);
#11043=VECTOR('',#47648,1000.);
#11044=VECTOR('',#47651,1000.);
#11045=VECTOR('',#47654,1000.);
#11046=VECTOR('',#47657,1000.);
#11047=VECTOR('',#47666,1000.);
#11048=VECTOR('',#47671,1000.);
#11049=VECTOR('',#47676,1000.);
#11050=VECTOR('',#47681,1000.);
#11051=VECTOR('',#47682,1000.);
#11052=VECTOR('',#47685,1000.);
#11053=VECTOR('',#47690,1000.);
#11054=VECTOR('',#47695,1000.);
#11055=VECTOR('',#47700,1000.);
#11056=VECTOR('',#47701,1000.);
#11057=VECTOR('',#47754,1000.);
#11058=VECTOR('',#47771,1000.);
#11059=VECTOR('',#47776,1000.);
#11060=VECTOR('',#47811,1000.);
#11061=VECTOR('',#47814,1000.);
#11062=VECTOR('',#47821,1000.);
#11063=VECTOR('',#47828,1000.);
#11064=VECTOR('',#47859,1000.);
#11065=VECTOR('',#47868,1000.);
#11066=VECTOR('',#47881,1000.);
#11067=VECTOR('',#47886,1000.);
#11068=VECTOR('',#47899,1000.);
#11069=VECTOR('',#47902,1000.);
#11070=VECTOR('',#47911,1000.);
#11071=VECTOR('',#47914,1000.);
#11072=VECTOR('',#47915,1000.);
#11073=VECTOR('',#47916,1000.);
#11074=VECTOR('',#47933,1000.);
#11075=VECTOR('',#47936,1000.);
#11076=VECTOR('',#47941,1000.);
#11077=VECTOR('',#47952,1000.);
#11078=VECTOR('',#47955,1000.);
#11079=VECTOR('',#47956,1000.);
#11080=VECTOR('',#47959,1000.);
#11081=VECTOR('',#47962,1000.);
#11082=VECTOR('',#47971,1000.);
#11083=VECTOR('',#47974,1000.);
#11084=VECTOR('',#47975,1000.);
#11085=VECTOR('',#47976,1000.);
#11086=VECTOR('',#47987,1000.);
#11087=VECTOR('',#47992,1000.);
#11088=VECTOR('',#47999,1000.);
#11089=VECTOR('',#48010,1000.);
#11090=VECTOR('',#48013,1000.);
#11091=VECTOR('',#48014,1000.);
#11092=VECTOR('',#48017,1000.);
#11093=VECTOR('',#48018,1000.);
#11094=VECTOR('',#48019,1000.);
#11095=VECTOR('',#48020,1000.);
#11096=VECTOR('',#48023,1000.);
#11097=VECTOR('',#48028,1000.);
#11098=VECTOR('',#48047,1000.);
#11099=VECTOR('',#48060,1000.);
#11100=VECTOR('',#48071,1000.);
#11101=VECTOR('',#48082,1000.);
#11102=VECTOR('',#48087,1000.);
#11103=VECTOR('',#48098,1000.);
#11104=VECTOR('',#48101,1000.);
#11105=VECTOR('',#48102,1000.);
#11106=VECTOR('',#48123,1000.);
#11107=VECTOR('',#48146,1000.);
#11108=VECTOR('',#48153,1000.);
#11109=VECTOR('',#48168,1000.);
#11110=VECTOR('',#48173,1000.);
#11111=VECTOR('',#48210,1000.);
#11112=VECTOR('',#48247,1000.);
#11113=VECTOR('',#48250,1000.);
#11114=VECTOR('',#48261,1000.);
#11115=VECTOR('',#48262,1000.);
#11116=VECTOR('',#48271,1000.);
#11117=VECTOR('',#48300,1000.);
#11118=VECTOR('',#48309,1000.);
#11119=VECTOR('',#48312,1000.);
#11120=VECTOR('',#48323,1000.);
#11121=VECTOR('',#48334,1000.);
#11122=VECTOR('',#48365,1000.);
#11123=VECTOR('',#48374,1000.);
#11124=VECTOR('',#48397,1000.);
#11125=VECTOR('',#48400,1000.);
#11126=VECTOR('',#48401,1000.);
#11127=VECTOR('',#48404,1000.);
#11128=VECTOR('',#48405,1000.);
#11129=VECTOR('',#48406,1000.);
#11130=VECTOR('',#48409,1000.);
#11131=VECTOR('',#48410,1000.);
#11132=VECTOR('',#48413,1000.);
#11133=VECTOR('',#48418,1000.);
#11134=VECTOR('',#48419,1000.);
#11135=VECTOR('',#48422,1000.);
#11136=VECTOR('',#48423,1000.);
#11137=VECTOR('',#48426,1000.);
#11138=VECTOR('',#48429,1000.);
#11139=VECTOR('',#48430,1000.);
#11140=VECTOR('',#48431,1000.);
#11141=VECTOR('',#48434,1000.);
#11142=VECTOR('',#48435,1000.);
#11143=VECTOR('',#48438,1000.);
#11144=VECTOR('',#48439,1000.);
#11145=VECTOR('',#48446,1.2046272227);
#11146=VECTOR('',#48451,1000.);
#11147=VECTOR('',#48454,1000.);
#11148=VECTOR('',#48457,1000.);
#11149=VECTOR('',#48462,1000.);
#11150=VECTOR('',#48467,1000.);
#11151=VECTOR('',#48482,1000.);
#11152=VECTOR('',#48487,1000.);
#11153=VECTOR('',#48492,1000.);
#11154=VECTOR('',#48495,1000.);
#11155=VECTOR('',#48498,1000.);
#11156=VECTOR('',#48507,1000.);
#11157=VECTOR('',#48510,1000.);
#11158=VECTOR('',#48511,1000.);
#11159=VECTOR('',#48512,1000.);
#11160=VECTOR('',#48513,1000.);
#11161=VECTOR('',#48514,1000.);
#11162=VECTOR('',#48517,1000.);
#11163=VECTOR('',#48520,1000.);
#11164=VECTOR('',#48529,1000.);
#11165=VECTOR('',#48530,1000.);
#11166=VECTOR('',#48531,1000.);
#11167=VECTOR('',#48532,1000.);
#11168=VECTOR('',#48533,1000.);
#11169=VECTOR('',#48534,1000.);
#11170=VECTOR('',#48537,1.5);
#11171=VECTOR('',#48542,1000.);
#11172=VECTOR('',#48543,1000.);
#11173=VECTOR('',#48544,1000.);
#11174=VECTOR('',#48547,1000.);
#11175=VECTOR('',#48548,1000.);
#11176=VECTOR('',#48551,1000.);
#11177=VECTOR('',#48556,1000.);
#11178=VECTOR('',#48557,1000.);
#11179=VECTOR('',#48560,1000.);
#11180=VECTOR('',#48563,1000.);
#11181=VECTOR('',#48564,1000.);
#11182=VECTOR('',#48573,1000.);
#11183=VECTOR('',#48574,1000.);
#11184=VECTOR('',#48577,1000.);
#11185=VECTOR('',#48578,1000.);
#11186=VECTOR('',#48581,1000.);
#11187=VECTOR('',#48584,1000.);
#11188=VECTOR('',#48585,1000.);
#11189=VECTOR('',#48588,1000.);
#11190=VECTOR('',#48595,1000.);
#11191=VECTOR('',#48596,1000.);
#11192=VECTOR('',#48597,1000.);
#11193=VECTOR('',#48600,1000.);
#11194=VECTOR('',#48605,1000.);
#11195=VECTOR('',#48608,1000.);
#11196=VECTOR('',#48611,1000.);
#11197=VECTOR('',#48612,1000.);
#11198=VECTOR('',#48621,1000.);
#11199=VECTOR('',#48622,1000.);
#11200=VECTOR('',#48625,1000.);
#11201=VECTOR('',#48626,1000.);
#11202=VECTOR('',#48627,1000.);
#11203=VECTOR('',#48630,1000.);
#11204=VECTOR('',#48633,1000.);
#11205=VECTOR('',#48634,1000.);
#11206=VECTOR('',#48637,1000.);
#11207=VECTOR('',#48640,1000.);
#11208=VECTOR('',#48641,1000.);
#11209=VECTOR('',#48650,1000.);
#11210=VECTOR('',#48655,1000.);
#11211=VECTOR('',#48658,1000.);
#11212=VECTOR('',#48659,1000.);
#11213=VECTOR('',#48662,1000.);
#11214=VECTOR('',#48663,1000.);
#11215=VECTOR('',#48670,1000.);
#11216=VECTOR('',#48675,1000.);
#11217=VECTOR('',#48678,1000.);
#11218=VECTOR('',#48683,1000.);
#11219=VECTOR('',#48684,1000.);
#11220=VECTOR('',#48689,1000.);
#11221=VECTOR('',#48692,1000.);
#11222=VECTOR('',#48693,1000.);
#11223=VECTOR('',#48702,1.5);
#11224=VECTOR('',#48707,1000.);
#11225=VECTOR('',#48708,1000.);
#11226=VECTOR('',#48711,1000.);
#11227=VECTOR('',#48712,1000.);
#11228=VECTOR('',#48713,1000.);
#11229=VECTOR('',#48716,1000.);
#11230=VECTOR('',#48721,1000.);
#11231=VECTOR('',#48722,1000.);
#11232=VECTOR('',#48723,1000.);
#11233=VECTOR('',#48726,1000.);
#11234=VECTOR('',#48727,1000.);
#11235=VECTOR('',#48728,1000.);
#11236=VECTOR('',#48729,1000.);
#11237=VECTOR('',#48732,1000.);
#11238=VECTOR('',#48737,1000.);
#11239=VECTOR('',#48738,1000.);
#11240=VECTOR('',#48739,1000.);
#11241=VECTOR('',#48744,1000.);
#11242=VECTOR('',#48747,1000.);
#11243=VECTOR('',#48750,1000.);
#11244=VECTOR('',#48753,1000.);
#11245=VECTOR('',#48758,1000.);
#11246=VECTOR('',#48759,1000.);
#11247=VECTOR('',#48760,1000.);
#11248=VECTOR('',#48763,1000.);
#11249=VECTOR('',#48764,1000.);
#11250=VECTOR('',#48769,1000.);
#11251=VECTOR('',#48774,1000.);
#11252=VECTOR('',#48775,1000.);
#11253=VECTOR('',#48776,1000.);
#11254=VECTOR('',#48783,1000.);
#11255=VECTOR('',#48786,1000.);
#11256=VECTOR('',#48791,1000.);
#11257=VECTOR('',#48804,1000.);
#11258=VECTOR('',#48811,1000.);
#11259=VECTOR('',#48824,1000.);
#11260=VECTOR('',#48829,1000.);
#11261=VECTOR('',#48836,1000.);
#11262=VECTOR('',#48839,1000.);
#11263=VECTOR('',#48844,1000.);
#11264=VECTOR('',#48845,1000.);
#11265=VECTOR('',#48850,1000.);
#11266=VECTOR('',#48851,1000.);
#11267=VECTOR('',#48856,1000.);
#11268=VECTOR('',#48859,1000.);
#11269=VECTOR('',#48860,1000.);
#11270=VECTOR('',#48863,1000.);
#11271=VECTOR('',#48868,1000.);
#11272=VECTOR('',#48873,1000.);
#11273=VECTOR('',#48874,1000.);
#11274=VECTOR('',#48879,1000.);
#11275=VECTOR('',#48884,1000.);
#11276=VECTOR('',#48889,1000.);
#11277=VECTOR('',#48892,1000.);
#11278=VECTOR('',#48897,1000.);
#11279=VECTOR('',#48902,1000.);
#11280=VECTOR('',#48907,1000.);
#11281=VECTOR('',#48908,1000.);
#11282=VECTOR('',#48913,1000.);
#11283=VECTOR('',#48916,1000.);
#11284=VECTOR('',#48923,1000.);
#11285=VECTOR('',#48926,1000.);
#11286=VECTOR('',#48927,1000.);
#11287=VECTOR('',#48930,1000.);
#11288=VECTOR('',#48935,1000.);
#11289=VECTOR('',#48940,1000.);
#11290=VECTOR('',#48947,1000.);
#11291=VECTOR('',#48950,1000.);
#11292=VECTOR('',#48957,1000.);
#11293=VECTOR('',#48960,1000.);
#11294=VECTOR('',#48961,1000.);
#11295=VECTOR('',#48970,1000.);
#11296=VECTOR('',#48973,1000.);
#11297=VECTOR('',#48976,1000.);
#11298=VECTOR('',#48977,1000.);
#11299=VECTOR('',#48986,1000.);
#11300=VECTOR('',#48989,1000.);
#11301=VECTOR('',#48992,8.85);
#11302=VECTOR('',#48997,1000.);
#11303=VECTOR('',#49000,1000.);
#11304=VECTOR('',#49011,1000.);
#11305=VECTOR('',#49014,1000.);
#11306=VECTOR('',#49019,1000.);
#11307=VECTOR('',#49028,1000.);
#11308=VECTOR('',#49031,1000.);
#11309=VECTOR('',#49036,1000.);
#11310=VECTOR('',#49051,1000.);
#11311=VECTOR('',#49060,1000.);
#11312=VECTOR('',#49077,1000.);
#11313=VECTOR('',#49078,1000.);
#11314=VECTOR('',#49081,1000.);
#11315=VECTOR('',#49082,1000.);
#11316=VECTOR('',#49085,1000.);
#11317=CIRCLE('',#34293,1.4);
#11318=CIRCLE('',#34294,1.3);
#11319=CIRCLE('',#34295,1.4);
#11320=CIRCLE('',#34297,1.4);
#11321=CIRCLE('',#34298,1.4);
#11322=CIRCLE('',#34301,1.3);
#11323=CIRCLE('',#34305,0.299999999999997);
#11324=CIRCLE('',#34306,0.3);
#11325=CIRCLE('',#34308,0.399999999999999);
#11326=CIRCLE('',#34309,15.8);
#11327=CIRCLE('',#34310,0.200000000000001);
#11328=CIRCLE('',#34311,0.399999999999999);
#11329=CIRCLE('',#34312,0.399999999999999);
#11330=CIRCLE('',#34313,0.200000000000001);
#11331=CIRCLE('',#34314,15.8);
#11332=CIRCLE('',#34315,0.200000000000001);
#11333=CIRCLE('',#34316,0.399999999999999);
#11334=CIRCLE('',#34317,0.399999999999999);
#11335=CIRCLE('',#34318,0.200000000000001);
#11336=CIRCLE('',#34319,15.8);
#11337=CIRCLE('',#34320,0.399999999999999);
#11338=CIRCLE('',#34321,0.399999999999999);
#11339=CIRCLE('',#34322,15.8);
#11340=CIRCLE('',#34323,0.200000000000001);
#11341=CIRCLE('',#34324,0.399999999999999);
#11342=CIRCLE('',#34325,0.399999999999999);
#11343=CIRCLE('',#34326,0.200000000000001);
#11344=CIRCLE('',#34327,15.8);
#11345=CIRCLE('',#34328,0.200000000000001);
#11346=CIRCLE('',#34329,0.4);
#11347=CIRCLE('',#34330,0.399999999999999);
#11348=CIRCLE('',#34331,0.200000000000001);
#11349=CIRCLE('',#34332,15.8);
#11350=CIRCLE('',#34333,0.399999999999999);
#11351=CIRCLE('',#34334,0.3);
#11352=CIRCLE('',#34335,0.3);
#11353=CIRCLE('',#34336,0.3);
#11354=CIRCLE('',#34337,0.3);
#11355=CIRCLE('',#34338,3.89050581799);
#11356=CIRCLE('',#34339,0.3);
#11357=CIRCLE('',#34340,4.00389099741);
#11358=CIRCLE('',#34341,4.00389099741);
#11359=CIRCLE('',#34342,0.3);
#11360=CIRCLE('',#34343,0.3);
#11361=CIRCLE('',#34344,0.3);
#11362=CIRCLE('',#34345,0.3);
#11363=CIRCLE('',#34347,0.300011835782053);
#11364=CIRCLE('',#34348,0.300012859472308);
#11365=CIRCLE('',#34357,2.21359789376355);
#11366=CIRCLE('',#34366,2.21359789376338);
#11367=CIRCLE('',#34373,15.9);
#11368=CIRCLE('',#34374,15.9);
#11369=CIRCLE('',#34376,0.0999999999999996);
#11370=CIRCLE('',#34377,0.0999999999999996);
#11371=CIRCLE('',#34379,0.1);
#11372=CIRCLE('',#34380,0.3);
#11373=CIRCLE('',#34382,0.3);
#11374=CIRCLE('',#34384,0.1);
#11375=CIRCLE('',#34387,0.1);
#11376=CIRCLE('',#34388,0.3);
#11377=CIRCLE('',#34390,0.3);
#11378=CIRCLE('',#34392,0.1);
#11379=CIRCLE('',#34395,0.0999999999999997);
#11380=CIRCLE('',#34396,0.3);
#11381=CIRCLE('',#34398,0.3);
#11382=CIRCLE('',#34400,0.1);
#11383=CIRCLE('',#34403,0.0999999999999997);
#11384=CIRCLE('',#34404,0.3);
#11385=CIRCLE('',#34406,0.3);
#11386=CIRCLE('',#34408,0.1);
#11387=CIRCLE('',#34409,15.9);
#11388=CIRCLE('',#34411,15.9);
#11389=CIRCLE('',#34413,0.0999999999999994);
#11390=CIRCLE('',#34414,0.5);
#11391=CIRCLE('',#34416,0.5);
#11392=CIRCLE('',#34418,0.0999999999999994);
#11393=CIRCLE('',#34421,0.1);
#11394=CIRCLE('',#34422,0.5);
#11395=CIRCLE('',#34424,0.5);
#11396=CIRCLE('',#34426,0.0999999999999997);
#11397=CIRCLE('',#34427,15.9);
#11398=CIRCLE('',#34429,15.9);
#11399=CIRCLE('',#34431,0.1);
#11400=CIRCLE('',#34432,0.3);
#11401=CIRCLE('',#34434,0.3);
#11402=CIRCLE('',#34436,0.0999999999999997);
#11403=CIRCLE('',#34439,0.1);
#11404=CIRCLE('',#34440,0.3);
#11405=CIRCLE('',#34442,0.3);
#11406=CIRCLE('',#34444,0.1);
#11407=CIRCLE('',#34447,0.1);
#11408=CIRCLE('',#34448,0.3);
#11409=CIRCLE('',#34450,0.3);
#11410=CIRCLE('',#34452,0.1);
#11411=CIRCLE('',#34455,0.0999999999999996);
#11412=CIRCLE('',#34456,0.3);
#11413=CIRCLE('',#34458,0.3);
#11414=CIRCLE('',#34460,15.9);
#11415=CIRCLE('',#34461,15.9);
#11416=CIRCLE('',#34463,0.0999999999999996);
#11417=CIRCLE('',#34465,0.1);
#11418=CIRCLE('',#34466,0.3);
#11419=CIRCLE('',#34468,0.3);
#11420=CIRCLE('',#34470,0.1);
#11421=CIRCLE('',#34473,0.1);
#11422=CIRCLE('',#34474,0.3);
#11423=CIRCLE('',#34476,0.3);
#11424=CIRCLE('',#34478,0.1);
#11425=CIRCLE('',#34481,0.0999999999999997);
#11426=CIRCLE('',#34482,0.3);
#11427=CIRCLE('',#34484,0.3);
#11428=CIRCLE('',#34486,0.1);
#11429=CIRCLE('',#34489,0.0999999999999997);
#11430=CIRCLE('',#34490,0.3);
#11431=CIRCLE('',#34492,0.3);
#11432=CIRCLE('',#34494,0.1);
#11433=CIRCLE('',#34495,15.9);
#11434=CIRCLE('',#34497,15.9);
#11435=CIRCLE('',#34499,0.0999999999999994);
#11436=CIRCLE('',#34500,0.5);
#11437=CIRCLE('',#34502,0.5);
#11438=CIRCLE('',#34504,0.0999999999999994);
#11439=CIRCLE('',#34507,0.1);
#11440=CIRCLE('',#34508,0.5);
#11441=CIRCLE('',#34510,0.5);
#11442=CIRCLE('',#34512,0.100000000000001);
#11443=CIRCLE('',#34513,15.9);
#11444=CIRCLE('',#34515,15.9);
#11445=CIRCLE('',#34517,0.1);
#11446=CIRCLE('',#34518,0.3);
#11447=CIRCLE('',#34520,0.3);
#11448=CIRCLE('',#34522,0.0999999999999997);
#11449=CIRCLE('',#34525,0.1);
#11450=CIRCLE('',#34526,0.3);
#11451=CIRCLE('',#34528,0.3);
#11452=CIRCLE('',#34530,0.0999999999999997);
#11453=CIRCLE('',#34533,0.3);
#11454=CIRCLE('',#34534,0.1);
#11455=CIRCLE('',#34536,0.3);
#11456=CIRCLE('',#34538,0.1);
#11457=CIRCLE('',#34539,0.3);
#11458=CIRCLE('',#34541,0.3);
#11459=CIRCLE('',#34547,0.199628863365679);
#11460=CIRCLE('',#34548,25.8578696504043);
#11461=CIRCLE('',#34549,25.2720864994101);
#11462=CIRCLE('',#34552,1.00000028469603);
#11463=CIRCLE('',#34553,1.00000044523891);
#11464=CIRCLE('',#34554,1.00003251262321);
#11465=CIRCLE('',#34555,1.00000027785337);
#11466=CIRCLE('',#34557,1.00000151494447);
#11467=CIRCLE('',#34558,1.00000061628411);
#11468=CIRCLE('',#34559,0.199580166399456);
#11469=CIRCLE('',#34560,1.00000059230394);
#11470=CIRCLE('',#34561,1.00000225038159);
#11471=CIRCLE('',#34563,1.00000028769429);
#11472=CIRCLE('',#34564,1.00000056588799);
#11473=CIRCLE('',#34565,1.00094397097147);
#11474=CIRCLE('',#34566,1.00000104682485);
#11475=CIRCLE('',#34567,1.00000115828043);
#11476=CIRCLE('',#34568,1.0000112573725);
#11477=CIRCLE('',#34569,1.00001575325937);
#11478=CIRCLE('',#34570,1.0000246775636);
#11479=CIRCLE('',#34571,0.999999920339783);
#11480=CIRCLE('',#34572,1.00000014419189);
#11481=CIRCLE('',#34574,1.0000008808516);
#11482=CIRCLE('',#34576,1.00000035796375);
#11483=CIRCLE('',#34577,0.99999967643586);
#11484=CIRCLE('',#34578,1.00000028469559);
#11485=CIRCLE('',#34579,1.00000027785327);
#11486=CIRCLE('',#34580,1.0000022192481);
#11487=CIRCLE('',#34581,1.00000044523891);
#11488=CIRCLE('',#34582,1.00000088028536);
#11489=CIRCLE('',#34584,1.00000078095249);
#11490=CIRCLE('',#34585,1.00000035796383);
#11491=CIRCLE('',#34587,1.00000014499945);
#11492=CIRCLE('',#34588,1.00000027111426);
#11493=CIRCLE('',#34589,1.00002467755638);
#11494=CIRCLE('',#34590,1.00001261620148);
#11495=CIRCLE('',#34591,1.00001153699998);
#11496=CIRCLE('',#34592,1.00000072628758);
#11497=CIRCLE('',#34593,1.00000103074381);
#11498=CIRCLE('',#34594,1.00094348029171);
#11499=CIRCLE('',#34595,1.00000030121054);
#11500=CIRCLE('',#34596,1.00000056588799);
#11501=CIRCLE('',#34597,1.00000061628416);
#11502=CIRCLE('',#34598,1.00000151494756);
#11503=CIRCLE('',#34599,1.00000225038157);
#11504=CIRCLE('',#34600,1.00000062699678);
#11505=CIRCLE('',#34603,0.0999999999999996);
#11506=CIRCLE('',#34604,15.8);
#11507=CIRCLE('',#34605,0.0999999999999996);
#11508=CIRCLE('',#34607,0.1);
#11509=CIRCLE('',#34608,0.200000000000001);
#11510=CIRCLE('',#34610,0.1);
#11511=CIRCLE('',#34612,0.1);
#11512=CIRCLE('',#34613,0.399999999999999);
#11513=CIRCLE('',#34615,0.1);
#11514=CIRCLE('',#34617,0.0999999999999997);
#11515=CIRCLE('',#34618,0.399999999999999);
#11516=CIRCLE('',#34620,0.1);
#11517=CIRCLE('',#34622,0.0999999999999997);
#11518=CIRCLE('',#34623,0.200000000000001);
#11519=CIRCLE('',#34625,0.1);
#11520=CIRCLE('',#34626,15.8);
#11521=CIRCLE('',#34628,0.0999999999999994);
#11522=CIRCLE('',#34629,0.399999999999999);
#11523=CIRCLE('',#34631,0.0999999999999994);
#11524=CIRCLE('',#34633,0.1);
#11525=CIRCLE('',#34634,0.399999999999999);
#11526=CIRCLE('',#34636,0.0999999999999997);
#11527=CIRCLE('',#34637,15.8);
#11528=CIRCLE('',#34639,0.1);
#11529=CIRCLE('',#34640,0.200000000000001);
#11530=CIRCLE('',#34642,0.0999999999999994);
#11531=CIRCLE('',#34644,0.1);
#11532=CIRCLE('',#34645,0.399999999999999);
#11533=CIRCLE('',#34647,0.1);
#11534=CIRCLE('',#34649,0.1);
#11535=CIRCLE('',#34650,0.399999999999999);
#11536=CIRCLE('',#34652,0.1);
#11537=CIRCLE('',#34654,0.0999999999999996);
#11538=CIRCLE('',#34655,0.200000000000001);
#11539=CIRCLE('',#34657,0.0999999999999996);
#11540=CIRCLE('',#34658,15.8);
#11541=CIRCLE('',#34660,0.1);
#11542=CIRCLE('',#34661,0.200000000000001);
#11543=CIRCLE('',#34663,0.1);
#11544=CIRCLE('',#34665,0.1);
#11545=CIRCLE('',#34666,0.399999999999999);
#11546=CIRCLE('',#34668,0.1);
#11547=CIRCLE('',#34670,0.0999999999999997);
#11548=CIRCLE('',#34671,0.399999999999999);
#11549=CIRCLE('',#34673,0.1);
#11550=CIRCLE('',#34675,0.0999999999999997);
#11551=CIRCLE('',#34676,0.200000000000001);
#11552=CIRCLE('',#34678,0.1);
#11553=CIRCLE('',#34679,15.8);
#11554=CIRCLE('',#34681,0.0999999999999994);
#11555=CIRCLE('',#34682,0.399999999999999);
#11556=CIRCLE('',#34684,0.0999999999999994);
#11557=CIRCLE('',#34686,0.1);
#11558=CIRCLE('',#34687,0.399999999999999);
#11559=CIRCLE('',#34689,0.100000000000001);
#11560=CIRCLE('',#34690,15.8);
#11561=CIRCLE('',#34692,0.1);
#11562=CIRCLE('',#34693,0.200000000000001);
#11563=CIRCLE('',#34695,0.0999999999999997);
#11564=CIRCLE('',#34697,0.1);
#11565=CIRCLE('',#34698,0.399999999999999);
#11566=CIRCLE('',#34700,0.0999999999999994);
#11567=CIRCLE('',#34702,0.200000000000001);
#11568=CIRCLE('',#34703,0.1);
#11569=CIRCLE('',#34705,0.1);
#11570=CIRCLE('',#34706,0.4);
#11571=CIRCLE('',#34709,1.5);
#11572=CIRCLE('',#34710,1.5);
#11573=CIRCLE('',#34711,14.4);
#11574=CIRCLE('',#34712,1.5);
#11575=CIRCLE('',#34713,1.5);
#11576=CIRCLE('',#34714,1.5);
#11577=CIRCLE('',#34715,1.5);
#11578=CIRCLE('',#34716,14.4);
#11579=CIRCLE('',#34717,1.5);
#11580=CIRCLE('',#34718,1.5);
#11581=CIRCLE('',#34720,14.4);
#11582=CIRCLE('',#34724,1.5);
#11583=CIRCLE('',#34727,1.5);
#11584=CIRCLE('',#34730,1.5);
#11585=CIRCLE('',#34732,1.5);
#11586=CIRCLE('',#34735,14.4);
#11587=CIRCLE('',#34738,1.5);
#11588=CIRCLE('',#34741,1.5);
#11589=CIRCLE('',#34744,1.5);
#11590=CIRCLE('',#34747,25.2720864994101);
#11591=CIRCLE('',#34749,1.5);
#11592=CIRCLE('',#34750,25.8578696504043);
#11593=CIRCLE('',#34751,0.300021606146326);
#11594=CIRCLE('',#34752,0.300022261835106);
#11595=CIRCLE('',#34753,0.300005681511778);
#11596=CIRCLE('',#34759,0.300000000000001);
#11597=CIRCLE('',#34771,0.300006142570235);
#11598=CIRCLE('',#34775,0.300000544869244);
#11599=CIRCLE('',#34776,0.300000585046962);
#11600=CIRCLE('',#34777,0.300165537902904);
#11601=CIRCLE('',#34778,0.300000598082167);
#11602=CIRCLE('',#34779,0.300000584963546);
#11603=CIRCLE('',#34783,0.300006218981457);
#11604=CIRCLE('',#34784,0.3);
#11605=CIRCLE('',#34786,0.300012869270441);
#11606=CIRCLE('',#34787,0.300007072562979);
#11607=CIRCLE('',#34788,0.300022294497527);
#11608=CIRCLE('',#34789,0.300021607322509);
#11609=CIRCLE('',#34790,0.999998074024125);
#11610=CIRCLE('',#34791,24.7051161323679);
#11611=CIRCLE('',#34792,24.8400616948579);
#11612=CIRCLE('',#34794,24.7051633159733);
#11613=CIRCLE('',#34795,24.7051633159701);
#11614=CIRCLE('',#34797,24.8400616948579);
#11615=CIRCLE('',#34798,24.7051161323679);
#11616=CIRCLE('',#34799,0.999998074024125);
#11617=CIRCLE('',#34801,5.);
#11618=CIRCLE('',#34802,16.1875296363);
#11619=CIRCLE('',#34803,26.2647265892);
#11620=CIRCLE('',#34804,12.2773059952);
#11621=CIRCLE('',#34805,12.2773059952);
#11622=CIRCLE('',#34806,26.2647265892);
#11623=CIRCLE('',#34807,16.1875296363);
#11624=CIRCLE('',#34809,16.1875296363);
#11625=CIRCLE('',#34811,26.2647265891997);
#11626=CIRCLE('',#34813,12.2773059952);
#11627=CIRCLE('',#34815,12.2773059952);
#11628=CIRCLE('',#34817,26.2647265892);
#11629=CIRCLE('',#34819,16.1875296363);
#11630=CIRCLE('',#34821,4.99999999999993);
#11631=CIRCLE('',#34922,5.8);
#11632=CIRCLE('',#34923,5.8);
#11633=CIRCLE('',#34925,5.5);
#11634=CIRCLE('',#34926,5.5);
#11635=CIRCLE('',#34928,5.5);
#11636=CIRCLE('',#34929,0.3);
#11637=CIRCLE('',#34932,5.5);
#11638=CIRCLE('',#34933,0.3);
#11639=CIRCLE('',#34938,0.300000000000002);
#11640=CIRCLE('',#34964,6.6905058179921);
#11641=CIRCLE('',#34966,6.69050581799);
#11642=CIRCLE('',#34970,6.69050581798971);
#11643=CIRCLE('',#34973,6.69050581799);
#11644=CIRCLE('',#34976,4.44342636361);
#11645=CIRCLE('',#34977,4.44342636361);
#11646=CIRCLE('',#34978,4.44342636361);
#11647=CIRCLE('',#34980,6.24342636361);
#11648=CIRCLE('',#34981,6.24342636361);
#11649=CIRCLE('',#34984,17.4);
#11650=CIRCLE('',#34985,16.4);
#11651=CIRCLE('',#34986,17.4);
#11652=CIRCLE('',#34987,16.4);
#11653=CIRCLE('',#34988,7.6);
#11654=CIRCLE('',#34989,0.2);
#11655=CIRCLE('',#34990,7.6);
#11656=CIRCLE('',#34991,16.1);
#11657=CIRCLE('',#34992,0.2);
#11658=CIRCLE('',#34993,7.6);
#11659=CIRCLE('',#34994,16.1);
#11660=CIRCLE('',#34995,7.6);
#11661=CIRCLE('',#34996,0.2);
#11662=CIRCLE('',#34997,16.1);
#11663=CIRCLE('',#34998,2.25);
#11664=CIRCLE('',#34999,7.34342636361);
#11665=CIRCLE('',#35000,16.1);
#11666=CIRCLE('',#35001,7.34342636361);
#11667=CIRCLE('',#35002,0.5);
#11668=CIRCLE('',#35003,6.5);
#11669=CIRCLE('',#35004,0.5);
#11670=CIRCLE('',#35005,0.5);
#11671=CIRCLE('',#35006,6.5);
#11672=CIRCLE('',#35007,0.5);
#11673=CIRCLE('',#35008,6.24342636361);
#11674=CIRCLE('',#35009,2.25);
#11675=CIRCLE('',#35010,7.34342636361);
#11676=CIRCLE('',#35011,16.1);
#11677=CIRCLE('',#35012,7.34342636361);
#11678=CIRCLE('',#35014,16.1);
#11679=CIRCLE('',#35019,7.59999999999999);
#11680=CIRCLE('',#35022,16.4);
#11681=CIRCLE('',#35023,16.4);
#11682=CIRCLE('',#35024,16.4);
#11683=CIRCLE('',#35025,16.4);
#11684=CIRCLE('',#35026,16.4);
#11685=CIRCLE('',#35027,16.4);
#11686=CIRCLE('',#35028,16.4);
#11687=CIRCLE('',#35029,16.4);
#11688=CIRCLE('',#35030,16.4);
#11689=CIRCLE('',#35034,17.4);
#11690=CIRCLE('',#35035,17.4);
#11691=CIRCLE('',#35036,17.4);
#11692=CIRCLE('',#35040,16.4);
#11693=CIRCLE('',#35041,16.4);
#11694=CIRCLE('',#35042,16.4);
#11695=CIRCLE('',#35043,16.4);
#11696=CIRCLE('',#35044,16.4);
#11697=CIRCLE('',#35045,16.4);
#11698=CIRCLE('',#35046,16.4);
#11699=CIRCLE('',#35047,16.4);
#11700=CIRCLE('',#35048,16.4);
#11701=CIRCLE('',#35052,17.4);
#11702=CIRCLE('',#35053,17.4);
#11703=CIRCLE('',#35054,17.4);
#11704=CIRCLE('',#35058,16.1);
#11705=CIRCLE('',#35059,16.1);
#11706=CIRCLE('',#35060,16.1);
#11707=CIRCLE('',#35063,7.6);
#11708=CIRCLE('',#35064,7.6);
#11709=CIRCLE('',#35065,7.6);
#11710=CIRCLE('',#35066,7.6);
#11711=CIRCLE('',#35068,0.2);
#11712=CIRCLE('',#35070,7.6);
#11713=CIRCLE('',#35071,7.6);
#11714=CIRCLE('',#35072,7.6);
#11715=CIRCLE('',#35073,7.6);
#11716=CIRCLE('',#35078,16.1);
#11717=CIRCLE('',#35082,7.6);
#11718=CIRCLE('',#35083,7.6);
#11719=CIRCLE('',#35085,0.2);
#11720=CIRCLE('',#35087,0.2);
#11721=CIRCLE('',#35089,7.6);
#11722=CIRCLE('',#35093,7.34342636361);
#11723=CIRCLE('',#35096,16.1);
#11724=CIRCLE('',#35097,16.1);
#11725=CIRCLE('',#35101,7.34342636361);
#11726=CIRCLE('',#35103,2.25);
#11727=CIRCLE('',#35104,2.25);
#11728=CIRCLE('',#35105,2.25);
#11729=CIRCLE('',#35106,2.25);
#11730=CIRCLE('',#35107,2.25);
#11731=CIRCLE('',#35109,6.24342636361);
#11732=CIRCLE('',#35112,0.5);
#11733=CIRCLE('',#35114,6.5);
#11734=CIRCLE('',#35116,0.5);
#11735=CIRCLE('',#35118,0.5);
#11736=CIRCLE('',#35120,6.5);
#11737=CIRCLE('',#35122,0.5);
#11738=CIRCLE('',#35125,7.34342636361);
#11739=CIRCLE('',#35129,16.1);
#11740=CIRCLE('',#35130,16.1);
#11741=CIRCLE('',#35133,7.34342636361);
#11742=CIRCLE('',#35135,2.25);
#11743=CIRCLE('',#35136,2.25);
#11744=CIRCLE('',#35137,2.25);
#11745=CIRCLE('',#35138,2.25);
#11746=CIRCLE('',#35139,2.25);
#11747=CIRCLE('',#35140,2.25);
#11748=CIRCLE('',#35146,16.7);
#11749=CIRCLE('',#35156,16.7);
#11750=CIRCLE('',#35159,16.4000000000001);
#11751=CIRCLE('',#35180,0.5);
#11752=CIRCLE('',#35181,1.75);
#11753=CIRCLE('',#35183,0.5);
#11754=CIRCLE('',#35184,6.5);
#11755=CIRCLE('',#35185,0.5);
#11756=CIRCLE('',#35186,6.5);
#11757=CIRCLE('',#35187,0.5);
#11758=CIRCLE('',#35188,5.24342636361);
#11759=CIRCLE('',#35189,5.24342636361);
#11760=CIRCLE('',#35190,5.5);
#11761=CIRCLE('',#35191,5.5);
#11762=CIRCLE('',#35198,0.5);
#11763=CIRCLE('',#35199,1.75);
#11764=CIRCLE('',#35202,16.4);
#11765=CIRCLE('',#35203,16.4);
#11766=CIRCLE('',#35205,15.4);
#11767=CIRCLE('',#35206,15.4);
#11768=CIRCLE('',#35208,15.4);
#11769=CIRCLE('',#35209,15.4);
#11770=CIRCLE('',#35211,15.4);
#11771=CIRCLE('',#35212,15.4);
#11772=CIRCLE('',#35214,15.4);
#11773=CIRCLE('',#35215,15.4);
#11774=CIRCLE('',#35217,15.4);
#11775=CIRCLE('',#35218,15.4);
#11776=CIRCLE('',#35220,15.4);
#11777=CIRCLE('',#35221,15.4);
#11778=CIRCLE('',#35224,16.7);
#11779=CIRCLE('',#35227,10.8000000000012);
#11780=CIRCLE('',#35228,15.4);
#11781=CIRCLE('',#35230,15.4000000000006);
#11782=CIRCLE('',#35231,0.299999999999997);
#11783=CIRCLE('',#35232,0.300000000000003);
#11784=CIRCLE('',#35234,15.4);
#11785=CIRCLE('',#35235,0.300000000000001);
#11786=CIRCLE('',#35236,0.299999999999996);
#11787=CIRCLE('',#35237,0.3);
#11788=CIRCLE('',#35238,0.300000000000001);
#11789=CIRCLE('',#35239,0.300000000000001);
#11790=CIRCLE('',#35240,0.300000000000001);
#11791=CIRCLE('',#35241,7.04342636361);
#11792=CIRCLE('',#35242,0.0999999999999999);
#11793=CIRCLE('',#35244,15.4);
#11794=CIRCLE('',#35246,15.4);
#11795=CIRCLE('',#35248,15.4);
#11796=CIRCLE('',#35250,15.4);
#11797=CIRCLE('',#35251,15.4);
#11798=CIRCLE('',#35253,15.4);
#11799=CIRCLE('',#35254,15.4);
#11800=CIRCLE('',#35256,15.4);
#11801=CIRCLE('',#35257,15.4);
#11802=CIRCLE('',#35259,16.4);
#11803=CIRCLE('',#35263,16.7);
#11804=CIRCLE('',#35267,10.7999999999998);
#11805=CIRCLE('',#35269,0.299999999999998);
#11806=CIRCLE('',#35270,0.300000000000003);
#11807=CIRCLE('',#35272,0.299999999999997);
#11808=CIRCLE('',#35273,0.300000000000004);
#11809=CIRCLE('',#35274,0.3);
#11810=CIRCLE('',#35275,0.0999999999999991);
#11811=CIRCLE('',#35276,7.04342636361);
#11812=CIRCLE('',#35277,0.299999999999999);
#11813=CIRCLE('',#35278,0.300000000000001);
#11814=CIRCLE('',#35279,0.300000000000003);
#11815=CIRCLE('',#35281,1.25);
#11816=CIRCLE('',#35283,0.5);
#11817=CIRCLE('',#35285,6.5);
#11818=CIRCLE('',#35287,0.5);
#11819=CIRCLE('',#35289,6.5);
#11820=CIRCLE('',#35291,0.5);
#11821=CIRCLE('',#35294,5.24342636361);
#11822=CIRCLE('',#35296,5.24342636361);
#11823=CIRCLE('',#35299,5.5);
#11824=CIRCLE('',#35301,5.5);
#11825=CIRCLE('',#35303,1.25);
#11826=CIRCLE('',#35305,7.04342636361);
#11827=CIRCLE('',#35307,0.1);
#11828=CIRCLE('',#35309,10.8);
#11829=CIRCLE('',#35311,10.8);
#11830=CIRCLE('',#35313,0.1);
#11831=CIRCLE('',#35315,7.04342636361);
#11832=CIRCLE('',#35317,1.25);
#11833=CIRCLE('',#35319,4.44342636361);
#11834=CIRCLE('',#35320,7.3);
#11835=CIRCLE('',#35321,7.3);
#11836=CIRCLE('',#35323,4.7);
#11837=CIRCLE('',#35325,4.7);
#11838=CIRCLE('',#35327,1.25);
#11839=CIRCLE('',#35330,4.44342636361);
#11840=CIRCLE('',#35331,4.44342636361);
#11841=CIRCLE('',#35334,7.3);
#11842=CIRCLE('',#35335,7.3);
#11843=CIRCLE('',#35337,7.3);
#11844=CIRCLE('',#35338,7.3);
#11845=CIRCLE('',#35341,4.7);
#11846=CIRCLE('',#35342,4.7);
#11847=CIRCLE('',#35343,4.7);
#11848=CIRCLE('',#35344,4.7);
#11849=CIRCLE('',#35345,4.7);
#11850=CIRCLE('',#35346,4.7);
#11851=CIRCLE('',#35347,4.7);
#11852=CIRCLE('',#35349,4.7);
#11853=CIRCLE('',#35350,4.7);
#11854=CIRCLE('',#35351,4.7);
#11855=CIRCLE('',#35352,4.7);
#11856=CIRCLE('',#35353,4.7);
#11857=CIRCLE('',#35354,4.7);
#11858=CIRCLE('',#35355,4.7);
#11859=CIRCLE('',#35358,6.24342636361);
#11860=CIRCLE('',#35359,6.24342636361);
#11861=CIRCLE('',#35361,0.3);
#11862=CIRCLE('',#35362,0.3);
#11863=CIRCLE('',#35364,10.);
#11864=CIRCLE('',#35365,10.);
#11865=CIRCLE('',#35367,0.3);
#11866=CIRCLE('',#35368,0.3);
#11867=CIRCLE('',#35370,6.24342636361);
#11868=CIRCLE('',#35371,6.24342636361);
#11869=CIRCLE('',#35376,4.44342636361);
#11870=CIRCLE('',#35377,4.44342636361);
#11871=CIRCLE('',#35380,3.);
#11872=CIRCLE('',#35384,0.300000000000001);
#11873=CIRCLE('',#35391,0.3);
#11874=CIRCLE('',#35392,0.3);
#11875=CIRCLE('',#35397,0.3);
#11876=CIRCLE('',#35398,0.3);
#11877=CIRCLE('',#35400,0.299999999999995);
#11878=CIRCLE('',#35407,5.69050581798992);
#11879=CIRCLE('',#35408,0.500000000000001);
#11880=CIRCLE('',#35409,1.1);
#11881=CIRCLE('',#35410,3.00000194400981);
#11882=CIRCLE('',#35411,3.);
#11883=CIRCLE('',#35412,5.24342636360999);
#11884=CIRCLE('',#35413,5.24342636361);
#11885=CIRCLE('',#35414,3.00000180903519);
#11886=CIRCLE('',#35415,1.1);
#11887=CIRCLE('',#35416,0.5);
#11888=CIRCLE('',#35417,5.69050581798992);
#11889=CIRCLE('',#35419,4.44342636361);
#11890=CIRCLE('',#35421,4.44342636361);
#11891=CIRCLE('',#35423,5.24342636361);
#11892=CIRCLE('',#35424,5.24342636361);
#11893=CIRCLE('',#35425,3.);
#11894=CIRCLE('',#35426,3.);
#11895=CIRCLE('',#35429,0.3);
#11896=CIRCLE('',#35431,0.3);
#11897=CIRCLE('',#35434,0.3);
#11898=CIRCLE('',#35436,0.3);
#11899=CIRCLE('',#35439,0.3);
#11900=CIRCLE('',#35441,0.3);
#11901=CIRCLE('',#35443,5.69050581799);
#11902=CIRCLE('',#35445,0.5);
#11903=CIRCLE('',#35448,1.1);
#11904=CIRCLE('',#35450,3.);
#11905=CIRCLE('',#35455,3.);
#11906=CIRCLE('',#35457,1.1);
#11907=CIRCLE('',#35460,0.5);
#11908=CIRCLE('',#35462,5.69050581799);
#11909=CIRCLE('',#35478,0.3);
#11910=CIRCLE('',#35480,0.3);
#11911=CIRCLE('',#35482,0.3);
#11912=CIRCLE('',#35483,0.3);
#11913=CIRCLE('',#35484,0.3);
#11914=CIRCLE('',#35485,0.3);
#11915=CIRCLE('',#35486,0.3);
#11916=CIRCLE('',#35487,0.3);
#11917=CIRCLE('',#35488,0.3);
#11918=CIRCLE('',#35489,0.3);
#11919=CIRCLE('',#35490,0.3);
#11920=CIRCLE('',#35491,0.3);
#11921=CIRCLE('',#35492,0.3);
#11922=CIRCLE('',#35493,0.3);
#11923=CIRCLE('',#35495,0.3);
#11924=CIRCLE('',#35497,0.3);
#11925=CIRCLE('',#35499,0.3);
#11926=CIRCLE('',#35500,0.300000000000001);
#11927=CIRCLE('',#35502,0.3);
#11928=CIRCLE('',#35504,0.299999999999999);
#11929=CIRCLE('',#35506,0.3);
#11930=CIRCLE('',#35508,0.3);
#11931=CIRCLE('',#35510,0.300000000000001);
#11932=CIRCLE('',#35511,16.1);
#11933=CIRCLE('',#35513,0.3);
#11934=CIRCLE('',#35515,0.300000000000001);
#11935=CIRCLE('',#35517,0.6);
#11936=CIRCLE('',#35518,15.7);
#11937=CIRCLE('',#35519,0.6);
#11938=CIRCLE('',#35521,0.300000000000001);
#11939=CIRCLE('',#35523,0.3);
#11940=CIRCLE('',#35524,0.3);
#11941=CIRCLE('',#35526,0.3);
#11942=CIRCLE('',#35528,0.3);
#11943=CIRCLE('',#35529,0.3);
#11944=CIRCLE('',#35531,0.300000000000001);
#11945=CIRCLE('',#35533,0.3);
#11946=CIRCLE('',#35534,0.3);
#11947=CIRCLE('',#35536,0.3);
#11948=CIRCLE('',#35538,0.3);
#11949=CIRCLE('',#35539,0.3);
#11950=CIRCLE('',#35541,0.299999999999999);
#11951=CIRCLE('',#35543,0.3);
#11952=CIRCLE('',#35544,0.300000000000001);
#11953=CIRCLE('',#35555,0.3);
#11954=CIRCLE('',#35556,0.300000000000001);
#11955=CIRCLE('',#35558,0.3);
#11956=CIRCLE('',#35560,0.300000000000001);
#11957=CIRCLE('',#35562,0.3);
#11958=CIRCLE('',#35564,0.3);
#11959=CIRCLE('',#35566,0.299999999999999);
#11960=CIRCLE('',#35567,16.1);
#11961=CIRCLE('',#35569,0.3);
#11962=CIRCLE('',#35571,0.300000000000001);
#11963=CIRCLE('',#35573,0.6);
#11964=CIRCLE('',#35574,15.7);
#11965=CIRCLE('',#35575,0.6);
#11966=CIRCLE('',#35577,0.300000000000001);
#11967=CIRCLE('',#35579,0.3);
#11968=CIRCLE('',#35580,0.3);
#11969=CIRCLE('',#35582,0.3);
#11970=CIRCLE('',#35584,0.3);
#11971=CIRCLE('',#35585,0.3);
#11972=CIRCLE('',#35587,0.300000000000001);
#11973=CIRCLE('',#35589,0.3);
#11974=CIRCLE('',#35590,0.3);
#11975=CIRCLE('',#35592,0.300000000000001);
#11976=CIRCLE('',#35594,0.3);
#11977=CIRCLE('',#35595,0.299999999999999);
#11978=CIRCLE('',#35597,0.3);
#11979=CIRCLE('',#35599,0.3);
#11980=CIRCLE('',#35600,0.3);
#11981=CIRCLE('',#35613,0.3);
#11982=CIRCLE('',#35614,0.300000000000001);
#11983=CIRCLE('',#35616,0.3);
#11984=CIRCLE('',#35618,0.299999999999999);
#11985=CIRCLE('',#35620,0.3);
#11986=CIRCLE('',#35622,0.3);
#11987=CIRCLE('',#35624,16.1);
#11988=CIRCLE('',#35625,0.300000000000001);
#11989=CIRCLE('',#35627,0.3);
#11990=CIRCLE('',#35629,0.300000000000001);
#11991=CIRCLE('',#35631,0.6);
#11992=CIRCLE('',#35632,15.7);
#11993=CIRCLE('',#35633,0.6);
#11994=CIRCLE('',#35635,0.300000000000001);
#11995=CIRCLE('',#35637,0.3);
#11996=CIRCLE('',#35638,0.3);
#11997=CIRCLE('',#35640,0.3);
#11998=CIRCLE('',#35642,0.3);
#11999=CIRCLE('',#35643,0.3);
#12000=CIRCLE('',#35645,0.300000000000001);
#12001=CIRCLE('',#35647,0.3);
#12002=CIRCLE('',#35648,0.3);
#12003=CIRCLE('',#35650,0.3);
#12004=CIRCLE('',#35652,0.3);
#12005=CIRCLE('',#35653,0.3);
#12006=CIRCLE('',#35655,0.299999999999999);
#12007=CIRCLE('',#35657,0.300000000000001);
#12008=CIRCLE('',#35658,0.3);
#12009=CIRCLE('',#35669,0.300000000000001);
#12010=CIRCLE('',#35670,0.3);
#12011=CIRCLE('',#35672,0.3);
#12012=CIRCLE('',#35674,0.3);
#12013=CIRCLE('',#35676,0.3);
#12014=CIRCLE('',#35678,0.3);
#12015=CIRCLE('',#35680,0.6);
#12016=CIRCLE('',#35681,15.7);
#12017=CIRCLE('',#35682,0.6);
#12018=CIRCLE('',#35683,16.1);
#12019=CIRCLE('',#35685,0.300000000000001);
#12020=CIRCLE('',#35687,0.300000000000001);
#12021=CIRCLE('',#35688,0.3);
#12022=CIRCLE('',#35690,0.3);
#12023=CIRCLE('',#35692,0.300000000000001);
#12024=CIRCLE('',#35693,0.3);
#12025=CIRCLE('',#35695,0.299999999999999);
#12026=CIRCLE('',#35696,0.3);
#12027=CIRCLE('',#35698,0.3);
#12028=CIRCLE('',#35699,0.3);
#12029=CIRCLE('',#35701,0.3);
#12030=CIRCLE('',#35702,0.3);
#12031=CIRCLE('',#35705,0.300000000000001);
#12032=CIRCLE('',#35707,0.299999999999999);
#12033=CIRCLE('',#35708,0.3);
#12034=CIRCLE('',#35710,0.300000000000001);
#12035=CIRCLE('',#35712,0.300000000000001);
#12036=CIRCLE('',#35713,0.3);
#12037=CIRCLE('',#35729,3.98587879194);
#12038=CIRCLE('',#35731,4.25458972003406);
#12039=CIRCLE('',#35734,0.299547728742047);
#12040=CIRCLE('',#35735,4.12347080401);
#12041=CIRCLE('',#35736,0.3);
#12042=CIRCLE('',#35737,0.3);
#12043=CIRCLE('',#35738,4.40314384042832);
#12044=CIRCLE('',#35740,0.300000000000001);
#12045=CIRCLE('',#35741,0.300000000000001);
#12046=CIRCLE('',#35742,4.72461821943);
#12047=CIRCLE('',#35743,0.300000000000001);
#12048=CIRCLE('',#35744,0.300000000000001);
#12049=CIRCLE('',#35745,4.42622127925);
#12050=CIRCLE('',#35747,0.300126293190847);
#12051=CIRCLE('',#35748,4.40312534809379);
#12052=CIRCLE('',#35749,0.299998398909284);
#12053=CIRCLE('',#35750,0.299965609274366);
#12054=CIRCLE('',#35751,4.12347080401);
#12055=CIRCLE('',#35754,4.25458975164979);
#12056=CIRCLE('',#35756,3.98587879194);
#12057=CIRCLE('',#35758,4.1423251838);
#12058=CIRCLE('',#35759,4.44177037781);
#12059=CIRCLE('',#35760,0.300000000000024);
#12060=CIRCLE('',#35762,3.93623398426);
#12061=CIRCLE('',#35765,4.00032353732);
#12062=CIRCLE('',#35766,4.00032353732);
#12063=CIRCLE('',#35770,0.3);
#12064=CIRCLE('',#35771,0.3);
#12065=CIRCLE('',#35773,0.299999999999949);
#12066=CIRCLE('',#35774,4.28950984611483);
#12067=CIRCLE('',#35776,4.28950741312049);
#12068=CIRCLE('',#35777,4.45);
#12069=CIRCLE('',#35778,4.22078101927);
#12070=CIRCLE('',#35779,4.17921044955);
#12071=CIRCLE('',#35780,2.48263157895);
#12072=CIRCLE('',#35781,3.8935342738);
#12073=CIRCLE('',#35782,3.73004103777);
#12074=CIRCLE('',#35783,2.48263157895);
#12075=CIRCLE('',#35784,2.48263157895);
#12076=CIRCLE('',#35785,3.73004103777);
#12077=CIRCLE('',#35786,3.8935342738);
#12078=CIRCLE('',#35787,2.48263157895);
#12079=CIRCLE('',#35789,0.3);
#12080=CIRCLE('',#35790,0.3);
#12081=CIRCLE('',#35792,0.300000000000001);
#12082=CIRCLE('',#35795,0.730765926094);
#12083=CIRCLE('',#35797,0.730765926094);
#12084=CIRCLE('',#35799,4.45);
#12085=CIRCLE('',#35800,0.2);
#12086=CIRCLE('',#35801,0.2);
#12087=CIRCLE('',#35802,1.3);
#12088=CIRCLE('',#35804,0.3);
#12089=CIRCLE('',#35807,0.3);
#12090=CIRCLE('',#35808,1.);
#12091=CIRCLE('',#35810,0.3);
#12092=CIRCLE('',#35811,0.3);
#12093=CIRCLE('',#35812,0.5);
#12094=CIRCLE('',#35814,0.3);
#12095=CIRCLE('',#35815,0.3);
#12096=CIRCLE('',#35816,0.5);
#12097=CIRCLE('',#35818,0.3);
#12098=CIRCLE('',#35820,0.3);
#12099=CIRCLE('',#35821,4.15);
#12100=CIRCLE('',#35822,0.3);
#12101=CIRCLE('',#35826,1.);
#12102=CIRCLE('',#35829,0.5);
#12103=CIRCLE('',#35832,0.5);
#12104=CIRCLE('',#35837,0.5);
#12105=CIRCLE('',#35839,4.15);
#12106=CIRCLE('',#35840,0.5);
#12107=CIRCLE('',#35842,0.1);
#12108=CIRCLE('',#35843,0.1);
#12109=CIRCLE('',#35845,1.);
#12110=CIRCLE('',#35847,0.1);
#12111=CIRCLE('',#35848,0.9);
#12112=CIRCLE('',#35850,0.1);
#12113=CIRCLE('',#35852,0.1);
#12114=CIRCLE('',#35853,0.6);
#12115=CIRCLE('',#35855,0.1);
#12116=CIRCLE('',#35857,0.1);
#12117=CIRCLE('',#35858,0.6);
#12118=CIRCLE('',#35859,0.300088662990782);
#12119=CIRCLE('',#35861,0.3);
#12120=CIRCLE('',#35863,0.3);
#12121=CIRCLE('',#35864,0.3);
#12122=CIRCLE('',#35866,0.999999999999999);
#12123=CIRCLE('',#35867,0.999999999999999);
#12124=CIRCLE('',#35869,0.1);
#12125=CIRCLE('',#35871,0.300088662500368);
#12126=CIRCLE('',#35873,0.5);
#12127=CIRCLE('',#35875,3.85);
#12128=CIRCLE('',#35876,0.3);
#12129=CIRCLE('',#35877,0.3);
#12130=CIRCLE('',#35879,0.5);
#12131=CIRCLE('',#35881,1.1);
#12132=CIRCLE('',#35882,0.1);
#12133=CIRCLE('',#35884,0.2);
#12134=CIRCLE('',#35885,0.2);
#12135=CIRCLE('',#35886,0.6);
#12136=CIRCLE('',#35887,0.6);
#12137=CIRCLE('',#35888,0.4);
#12138=CIRCLE('',#35889,0.9);
#12139=CIRCLE('',#35890,0.199999999999999);
#12140=CIRCLE('',#35891,3.05);
#12141=CIRCLE('',#35892,0.400000000000001);
#12142=CIRCLE('',#35893,1.1);
#12143=CIRCLE('',#35894,1.1);
#12144=CIRCLE('',#35895,0.400000000000001);
#12145=CIRCLE('',#35896,3.05);
#12146=CIRCLE('',#35897,0.199999999999999);
#12147=CIRCLE('',#35898,0.9);
#12148=CIRCLE('',#35900,0.3);
#12149=CIRCLE('',#35902,0.3);
#12150=CIRCLE('',#35903,4.15601973046);
#12151=CIRCLE('',#35904,0.3);
#12152=CIRCLE('',#35906,0.799999999999999);
#12153=CIRCLE('',#35907,0.699999999999999);
#12154=CIRCLE('',#35908,0.8);
#12155=CIRCLE('',#35909,0.8);
#12156=CIRCLE('',#35910,0.699999999999999);
#12157=CIRCLE('',#35911,2.95);
#12158=CIRCLE('',#35913,0.3);
#12159=CIRCLE('',#35916,0.1);
#12160=CIRCLE('',#35918,0.3);
#12161=CIRCLE('',#35919,0.3);
#12162=CIRCLE('',#35921,0.3);
#12163=CIRCLE('',#35923,1.);
#12164=CIRCLE('',#35924,1.);
#12165=CIRCLE('',#35926,0.1);
#12166=CIRCLE('',#35928,0.3);
#12167=CIRCLE('',#35931,0.1);
#12168=CIRCLE('',#35934,0.1);
#12169=CIRCLE('',#35935,1.);
#12170=CIRCLE('',#35937,0.1);
#12171=CIRCLE('',#35939,0.1);
#12172=CIRCLE('',#35940,0.300000000000002);
#12173=CIRCLE('',#35942,0.1);
#12174=CIRCLE('',#35943,2.95);
#12175=CIRCLE('',#35945,0.1);
#12176=CIRCLE('',#35946,0.1);
#12177=CIRCLE('',#35948,0.1);
#12178=CIRCLE('',#35949,0.5);
#12179=CIRCLE('',#35952,0.1);
#12180=CIRCLE('',#35954,0.1);
#12181=CIRCLE('',#35956,0.1);
#12182=CIRCLE('',#35957,0.5);
#12183=CIRCLE('',#35959,0.1);
#12184=CIRCLE('',#35961,0.1);
#12185=CIRCLE('',#35962,0.1);
#12186=CIRCLE('',#35963,2.95);
#12187=CIRCLE('',#35965,0.1);
#12188=CIRCLE('',#35966,0.300000000000002);
#12189=CIRCLE('',#35968,0.1);
#12190=CIRCLE('',#35970,0.1);
#12191=CIRCLE('',#35971,1.);
#12192=CIRCLE('',#35973,0.1);
#12193=CIRCLE('',#35975,0.1);
#12194=CIRCLE('',#35976,0.5);
#12195=CIRCLE('',#35978,0.1);
#12196=CIRCLE('',#35980,0.1);
#12197=CIRCLE('',#35981,0.5);
#12198=CIRCLE('',#35983,0.1);
#12199=CIRCLE('',#35985,0.1);
#12200=CIRCLE('',#35986,0.5);
#12201=CIRCLE('',#35988,0.1);
#12202=CIRCLE('',#35990,0.1);
#12203=CIRCLE('',#35991,0.1);
#12204=CIRCLE('',#35993,0.1);
#12205=CIRCLE('',#35994,0.1);
#12206=CIRCLE('',#35996,0.1);
#12207=CIRCLE('',#35997,0.1);
#12208=CIRCLE('',#35999,0.1);
#12209=CIRCLE('',#36001,0.1);
#12210=CIRCLE('',#36002,0.1);
#12211=CIRCLE('',#36004,0.1);
#12212=CIRCLE('',#36005,0.1);
#12213=CIRCLE('',#36007,0.1);
#12214=CIRCLE('',#36008,0.1);
#12215=CIRCLE('',#36011,2.65);
#12216=CIRCLE('',#36012,2.65);
#12217=CIRCLE('',#36013,0.3);
#12218=CIRCLE('',#36015,0.3);
#12219=CIRCLE('',#36017,0.300000000000001);
#12220=CIRCLE('',#36018,2.95);
#12221=CIRCLE('',#36019,0.300000018904248);
#12222=CIRCLE('',#36022,0.299999999999999);
#12223=CIRCLE('',#36023,2.95);
#12224=CIRCLE('',#36024,0.300000075511691);
#12225=CIRCLE('',#36026,2.95);
#12226=CIRCLE('',#36028,0.3);
#12227=CIRCLE('',#36029,2.95);
#12228=CIRCLE('',#36032,2.95);
#12229=CIRCLE('',#36033,0.300000017917961);
#12230=CIRCLE('',#36035,2.95);
#12231=CIRCLE('',#36037,0.3);
#12232=CIRCLE('',#36038,0.300000000000001);
#12233=CIRCLE('',#36041,0.3);
#12234=CIRCLE('',#36043,0.5);
#12235=CIRCLE('',#36044,0.3);
#12236=CIRCLE('',#36049,3.98150447852);
#12237=CIRCLE('',#36050,0.299999999999992);
#12238=CIRCLE('',#36054,1.);
#12239=CIRCLE('',#36056,0.300000000004292);
#12240=CIRCLE('',#36057,4.46095497423);
#12241=CIRCLE('',#36058,0.299999910435179);
#12242=CIRCLE('',#36061,0.300000000000002);
#12243=CIRCLE('',#36064,0.0999999999999994);
#12244=CIRCLE('',#36069,0.0999999999999994);
#12245=CIRCLE('',#36072,0.300000000000002);
#12246=CIRCLE('',#36075,1.);
#12247=CIRCLE('',#36078,0.5);
#12248=CIRCLE('',#36081,0.5);
#12249=CIRCLE('',#36084,0.5);
#12250=CIRCLE('',#36087,0.1);
#12251=CIRCLE('',#36090,0.1);
#12252=CIRCLE('',#36093,0.1);
#12253=CIRCLE('',#36096,0.0999999999999994);
#12254=CIRCLE('',#36099,0.0999999999999994);
#12255=CIRCLE('',#36102,0.1);
#12256=CIRCLE('',#36105,2.65);
#12257=CIRCLE('',#36107,0.1);
#12258=CIRCLE('',#36108,3.05);
#12259=CIRCLE('',#36109,0.1);
#12260=CIRCLE('',#36111,0.0999999999999994);
#12261=CIRCLE('',#36113,0.3);
#12262=CIRCLE('',#36114,4.15601973046);
#12263=CIRCLE('',#36115,0.3);
#12264=CIRCLE('',#36117,0.699999999999999);
#12265=CIRCLE('',#36118,0.8);
#12266=CIRCLE('',#36119,3.85);
#12267=CIRCLE('',#36120,0.8);
#12268=CIRCLE('',#36121,0.699999999999999);
#12269=CIRCLE('',#36122,0.799999999999999);
#12270=CIRCLE('',#36123,2.95);
#12271=CIRCLE('',#36125,0.0999999999999994);
#12272=CIRCLE('',#36127,0.3);
#12273=CIRCLE('',#36128,0.3);
#12274=CIRCLE('',#36129,0.3);
#12275=CIRCLE('',#36134,0.1);
#12276=CIRCLE('',#36136,0.1);
#12277=CIRCLE('',#36137,0.9);
#12278=CIRCLE('',#36139,0.1);
#12279=CIRCLE('',#36141,0.1);
#12280=CIRCLE('',#36142,0.199999999999999);
#12281=CIRCLE('',#36144,0.1);
#12282=CIRCLE('',#36145,0.199999999999999);
#12283=CIRCLE('',#36147,0.1);
#12284=CIRCLE('',#36149,0.1);
#12285=CIRCLE('',#36150,0.9);
#12286=CIRCLE('',#36152,0.1);
#12287=CIRCLE('',#36154,0.1);
#12288=CIRCLE('',#36155,0.4);
#12289=CIRCLE('',#36157,0.1);
#12290=CIRCLE('',#36159,0.1);
#12291=CIRCLE('',#36160,0.6);
#12292=CIRCLE('',#36162,0.1);
#12293=CIRCLE('',#36164,0.1);
#12294=CIRCLE('',#36165,0.6);
#12295=CIRCLE('',#36167,0.1);
#12296=CIRCLE('',#36169,0.1);
#12297=CIRCLE('',#36171,0.1);
#12298=CIRCLE('',#36172,0.1);
#12299=CIRCLE('',#36174,0.1);
#12300=CIRCLE('',#36176,0.1);
#12301=CIRCLE('',#36177,0.1);
#12302=CIRCLE('',#36179,0.1);
#12303=CIRCLE('',#36180,0.2);
#12304=CIRCLE('',#36182,0.1);
#12305=CIRCLE('',#36184,0.0999999999999994);
#12306=CIRCLE('',#36186,0.1);
#12307=CIRCLE('',#36187,0.1);
#12308=CIRCLE('',#36189,0.0999999999999994);
#12309=CIRCLE('',#36191,0.1);
#12310=CIRCLE('',#36192,0.1);
#12311=CIRCLE('',#36194,0.1);
#12312=CIRCLE('',#36195,0.2);
#12313=CIRCLE('',#36198,1.4);
#12314=CIRCLE('',#36200,0.1);
#12315=CIRCLE('',#36202,2.62880107536);
#12316=CIRCLE('',#36203,2.44564212855);
#12317=CIRCLE('',#36204,2.44564212855);
#12318=CIRCLE('',#36207,2.65);
#12319=CIRCLE('',#36208,0.3);
#12320=CIRCLE('',#36210,0.3);
#12321=CIRCLE('',#36211,0.3);
#12322=CIRCLE('',#36213,0.3);
#12323=CIRCLE('',#36214,1.);
#12324=CIRCLE('',#36216,0.3);
#12325=CIRCLE('',#36217,0.999999999999999);
#12326=CIRCLE('',#36218,0.3);
#12327=CIRCLE('',#36221,0.3);
#12328=CIRCLE('',#36222,0.5);
#12329=CIRCLE('',#36224,0.300000000000001);
#12330=CIRCLE('',#36225,0.3);
#12331=CIRCLE('',#36228,0.3);
#12332=CIRCLE('',#36230,0.3);
#12333=CIRCLE('',#36231,0.5);
#12334=CIRCLE('',#36234,0.3);
#12335=CIRCLE('',#36235,0.5);
#12336=CIRCLE('',#36236,0.3);
#12337=CIRCLE('',#36238,4.15);
#12338=CIRCLE('',#36241,0.1);
#12339=CIRCLE('',#36242,2.36684105317747);
#12340=CIRCLE('',#36243,2.36684105317747);
#12341=CIRCLE('',#36244,2.36684105317747);
#12342=CIRCLE('',#36250,1.4);
#12343=CIRCLE('',#36252,0.1);
#12344=CIRCLE('',#36254,0.5);
#12345=CIRCLE('',#36255,0.400000000000001);
#12346=CIRCLE('',#36256,0.1);
#12347=CIRCLE('',#36258,0.1);
#12348=CIRCLE('',#36260,1.);
#12349=CIRCLE('',#36261,1.1);
#12350=CIRCLE('',#36262,0.1);
#12351=CIRCLE('',#36264,0.1);
#12352=CIRCLE('',#36266,0.3);
#12353=CIRCLE('',#36269,0.300045031714467);
#12354=CIRCLE('',#36270,3.98150447852);
#12355=CIRCLE('',#36273,0.1);
#12356=CIRCLE('',#36274,2.65);
#12357=CIRCLE('',#36277,0.3);
#12358=CIRCLE('',#36278,1.);
#12359=CIRCLE('',#36279,0.3);
#12360=CIRCLE('',#36280,1.3);
#12361=CIRCLE('',#36282,0.299999999999998);
#12362=CIRCLE('',#36283,0.3);
#12363=CIRCLE('',#36284,0.5);
#12364=CIRCLE('',#36285,0.3);
#12365=CIRCLE('',#36286,0.2);
#12366=CIRCLE('',#36291,0.3);
#12367=CIRCLE('',#36293,0.999999999999999);
#12368=CIRCLE('',#36294,0.1);
#12369=CIRCLE('',#36295,1.1);
#12370=CIRCLE('',#36296,0.1);
#12371=CIRCLE('',#36298,0.1);
#12372=CIRCLE('',#36300,3.05);
#12373=CIRCLE('',#36301,0.400000000000001);
#12374=CIRCLE('',#36302,0.6);
#12375=CIRCLE('',#36303,0.6);
#12376=CIRCLE('',#36304,0.9);
#12377=CIRCLE('',#36305,1.1);
#12378=CIRCLE('',#36307,0.1);
#12379=CIRCLE('',#36309,0.1);
#12380=CIRCLE('',#36311,0.1);
#12381=CIRCLE('',#36313,0.5);
#12382=CIRCLE('',#36319,0.1);
#12383=CIRCLE('',#36321,0.5);
#12384=CIRCLE('',#36322,0.1);
#12385=CIRCLE('',#36324,0.1);
#12386=CIRCLE('',#36326,0.5);
#12387=CIRCLE('',#36327,0.1);
#12388=CIRCLE('',#36329,0.1);
#12389=CIRCLE('',#36331,1.);
#12390=CIRCLE('',#36332,0.1);
#12391=CIRCLE('',#36334,0.1);
#12392=CIRCLE('',#36336,1.);
#12393=CIRCLE('',#36344,0.5);
#12394=CIRCLE('',#36345,0.3);
#12395=CIRCLE('',#36346,0.2);
#12396=CIRCLE('',#36350,0.5);
#12397=CIRCLE('',#36351,0.3);
#12398=CIRCLE('',#36354,4.15);
#12399=CIRCLE('',#36356,0.5);
#12400=CIRCLE('',#36358,0.300088662981395);
#12401=CIRCLE('',#36362,0.3);
#12402=CIRCLE('',#36364,4.45);
#12403=CIRCLE('',#36370,11.2571565141535);
#12404=CIRCLE('',#36371,10.527435261753);
#12405=CIRCLE('',#36372,11.2571565141535);
#12406=CIRCLE('',#36373,11.2571565141535);
#12407=CIRCLE('',#36374,11.2571565141535);
#12408=CIRCLE('',#36376,17.4);
#12409=CIRCLE('',#36377,17.4);
#12410=CIRCLE('',#36378,16.4);
#12411=CIRCLE('',#36380,11.);
#12412=CIRCLE('',#36381,11.);
#12413=CIRCLE('',#36383,10.527435261753);
#12414=CIRCLE('',#36384,9.15);
#12415=CIRCLE('',#36386,17.4);
#12416=CIRCLE('',#36387,16.4);
#12417=CIRCLE('',#36391,17.4);
#12418=CIRCLE('',#36392,16.4);
#12419=CIRCLE('',#36394,17.4);
#12420=CIRCLE('',#36395,16.4);
#12421=CIRCLE('',#36399,17.4);
#12422=CIRCLE('',#36400,16.4);
#12423=CIRCLE('',#36402,16.4);
#12424=CIRCLE('',#36403,16.4);
#12425=CIRCLE('',#36404,16.4);
#12426=CIRCLE('',#36405,16.4);
#12427=CIRCLE('',#36406,16.4);
#12428=CIRCLE('',#36407,16.4);
#12429=CIRCLE('',#36408,16.4);
#12430=CIRCLE('',#36409,16.4);
#12431=CIRCLE('',#36410,16.4);
#12432=CIRCLE('',#36411,16.4000000000001);
#12433=CIRCLE('',#36412,16.4);
#12434=CIRCLE('',#36413,16.3999999999877);
#12435=CIRCLE('',#36414,16.4);
#12436=CIRCLE('',#36415,16.3999999999998);
#12437=CIRCLE('',#36416,16.4);
#12438=CIRCLE('',#36417,16.4);
#12439=CIRCLE('',#36418,16.4);
#12440=CIRCLE('',#36419,16.4);
#12441=CIRCLE('',#36420,16.4);
#12442=CIRCLE('',#36421,16.4);
#12443=CIRCLE('',#36423,17.4);
#12444=CIRCLE('',#36424,17.4);
#12445=CIRCLE('',#36425,17.4);
#12446=CIRCLE('',#36426,17.4);
#12447=CIRCLE('',#36427,17.4);
#12448=CIRCLE('',#36431,15.);
#12449=CIRCLE('',#36432,15.0000000000004);
#12450=CIRCLE('',#36434,2.);
#12451=CIRCLE('',#36435,2.);
#12452=CIRCLE('',#36437,13.4999999999999);
#12453=CIRCLE('',#36438,13.5);
#12454=CIRCLE('',#36440,0.500000000000003);
#12455=CIRCLE('',#36441,0.5);
#12456=CIRCLE('',#36443,0.5);
#12457=CIRCLE('',#36444,0.5);
#12458=CIRCLE('',#36447,0.5);
#12459=CIRCLE('',#36448,0.499999999999994);
#12460=CIRCLE('',#36452,0.100000000000004);
#12461=CIRCLE('',#36453,0.1);
#12462=CIRCLE('',#36456,0.5);
#12463=CIRCLE('',#36457,0.5);
#12464=CIRCLE('',#36458,0.2);
#12465=CIRCLE('',#36459,0.299999999999999);
#12466=CIRCLE('',#36460,0.3);
#12467=CIRCLE('',#36465,0.3);
#12468=CIRCLE('',#36468,0.0999999999999997);
#12469=CIRCLE('',#36469,0.1);
#12470=CIRCLE('',#36472,0.71602073105324);
#12471=CIRCLE('',#36473,0.30000057515613);
#12472=CIRCLE('',#36475,0.3);
#12473=CIRCLE('',#36478,0.300001459552508);
#12474=CIRCLE('',#36480,0.500000000000001);
#12475=CIRCLE('',#36487,15.4);
#12476=CIRCLE('',#36488,15.4);
#12477=CIRCLE('',#36490,0.1);
#12478=CIRCLE('',#36491,0.100000000000002);
#12479=CIRCLE('',#36494,0.5);
#12480=CIRCLE('',#36495,0.5);
#12481=CIRCLE('',#36496,0.3);
#12482=CIRCLE('',#36497,0.299999999999999);
#12483=CIRCLE('',#36498,0.2);
#12484=CIRCLE('',#36500,11.3);
#12485=CIRCLE('',#36501,12.5);
#12486=CIRCLE('',#36502,0.1);
#12487=CIRCLE('',#36507,0.3);
#12488=CIRCLE('',#36508,0.30000000000001);
#12489=CIRCLE('',#36511,0.0999999999999998);
#12490=CIRCLE('',#36513,12.5000000000001);
#12491=CIRCLE('',#36518,0.30000057515613);
#12492=CIRCLE('',#36521,0.3);
#12493=CIRCLE('',#36524,0.300001459552676);
#12494=CIRCLE('',#36526,0.499999999999989);
#12495=CIRCLE('',#36535,15.);
#12496=CIRCLE('',#36536,15.0000000000004);
#12497=CIRCLE('',#36538,2.);
#12498=CIRCLE('',#36539,2.);
#12499=CIRCLE('',#36541,13.4999999999999);
#12500=CIRCLE('',#36542,13.5);
#12501=CIRCLE('',#36544,0.500000000000003);
#12502=CIRCLE('',#36545,0.5);
#12503=CIRCLE('',#36547,0.5);
#12504=CIRCLE('',#36548,0.5);
#12505=CIRCLE('',#36551,0.5);
#12506=CIRCLE('',#36552,0.499999999999994);
#12507=CIRCLE('',#36572,9.15);
#12508=CIRCLE('',#36580,11.2571565141535);
#12509=CIRCLE('',#36581,11.2571565141535);
#12510=CIRCLE('',#36582,11.2571565141535);
#12511=CIRCLE('',#36583,11.2571565141535);
#12512=CIRCLE('',#36584,11.2571565141535);
#12513=CIRCLE('',#36585,11.2571565141535);
#12514=CIRCLE('',#36590,11.2571565141535);
#12515=CIRCLE('',#36593,11.2571565141535);
#12516=CIRCLE('',#36596,11.2571565141535);
#12517=CIRCLE('',#36599,11.2571565141535);
#12518=CIRCLE('',#36604,0.3);
#12519=CIRCLE('',#36605,0.3);
#12520=CIRCLE('',#36607,13.516744254);
#12521=CIRCLE('',#36608,13.516744254);
#12522=CIRCLE('',#36611,0.3);
#12523=CIRCLE('',#36613,0.3);
#12524=CIRCLE('',#36615,0.3);
#12525=CIRCLE('',#36616,0.300000000000007);
#12526=CIRCLE('',#36619,0.3);
#12527=CIRCLE('',#36620,0.3);
#12528=CIRCLE('',#36622,13.516744254);
#12529=CIRCLE('',#36623,13.516744254);
#12530=CIRCLE('',#36625,0.3);
#12531=CIRCLE('',#36626,0.3);
#12532=CIRCLE('',#36628,0.861212043428353);
#12533=CIRCLE('',#36630,0.3);
#12534=CIRCLE('',#36632,0.299999999999999);
#12535=CIRCLE('',#36634,13.816744254);
#12536=CIRCLE('',#36635,0.3);
#12537=CIRCLE('',#36637,0.3);
#12538=CIRCLE('',#36639,0.3);
#12539=CIRCLE('',#36641,0.6);
#12540=CIRCLE('',#36642,0.3);
#12541=CIRCLE('',#36643,0.3);
#12542=CIRCLE('',#36645,14.9875296363);
#12543=CIRCLE('',#36646,14.6875296363);
#12544=CIRCLE('',#36647,0.300000000000001);
#12545=CIRCLE('',#36649,0.6);
#12546=CIRCLE('',#36650,0.299999999999999);
#12547=CIRCLE('',#36652,14.9875296363);
#12548=CIRCLE('',#36653,14.6875296363);
#12549=CIRCLE('',#36654,0.300000000000001);
#12550=CIRCLE('',#36656,0.6);
#12551=CIRCLE('',#36657,0.3);
#12552=CIRCLE('',#36659,0.3);
#12553=CIRCLE('',#36661,0.299999999999999);
#12554=CIRCLE('',#36663,13.816744254);
#12555=CIRCLE('',#36664,0.299999999999999);
#12556=CIRCLE('',#36666,0.3);
#12557=CIRCLE('',#36669,2.7);
#12558=CIRCLE('',#36670,15.3875296363);
#12559=CIRCLE('',#36673,0.3);
#12560=CIRCLE('',#36674,0.3);
#12561=CIRCLE('',#36676,13.6462109523);
#12562=CIRCLE('',#36677,13.6462109523);
#12563=CIRCLE('',#36679,0.3);
#12564=CIRCLE('',#36680,0.3);
#12565=CIRCLE('',#36683,0.3);
#12566=CIRCLE('',#36685,0.299999999999999);
#12567=CIRCLE('',#36686,0.3);
#12568=CIRCLE('',#36688,0.3);
#12569=CIRCLE('',#36689,0.3);
#12570=CIRCLE('',#36691,0.3);
#12571=CIRCLE('',#36693,13.9462109523);
#12572=CIRCLE('',#36694,0.3);
#12573=CIRCLE('',#36696,0.3);
#12574=CIRCLE('',#36698,0.3);
#12575=CIRCLE('',#36700,0.6);
#12576=CIRCLE('',#36701,0.3);
#12577=CIRCLE('',#36703,14.9875296363);
#12578=CIRCLE('',#36704,14.6875296363);
#12579=CIRCLE('',#36706,0.3);
#12580=CIRCLE('',#36708,16.1875296363);
#12581=CIRCLE('',#36709,15.8875296363);
#12582=CIRCLE('',#36712,8.14541841273);
#12583=CIRCLE('',#36713,7.84541841273);
#12584=CIRCLE('',#36714,0.299999999999994);
#12585=CIRCLE('',#36716,0.300000000000002);
#12586=CIRCLE('',#36718,14.6875296363);
#12587=CIRCLE('',#36719,14.3875296363);
#12588=CIRCLE('',#36720,0.299999999999999);
#12589=CIRCLE('',#36722,0.3);
#12590=CIRCLE('',#36725,0.3);
#12591=CIRCLE('',#36727,7.84541841273);
#12592=CIRCLE('',#36729,0.3);
#12593=CIRCLE('',#36732,0.3);
#12594=CIRCLE('',#36734,14.6875296363);
#12595=CIRCLE('',#36736,0.3);
#12596=CIRCLE('',#36738,0.3);
#12597=CIRCLE('',#36739,0.3);
#12598=CIRCLE('',#36741,0.3);
#12599=CIRCLE('',#36743,0.3);
#12600=CIRCLE('',#36744,7.54541841273);
#12601=CIRCLE('',#36745,0.3);
#12602=CIRCLE('',#36747,0.3);
#12603=CIRCLE('',#36749,0.300000000000002);
#12604=CIRCLE('',#36750,0.300000000000002);
#12605=CIRCLE('',#36752,0.3);
#12606=CIRCLE('',#36754,0.3);
#12607=CIRCLE('',#36755,14.9875296363);
#12608=CIRCLE('',#36756,0.300000000000001);
#12609=CIRCLE('',#36758,0.6);
#12610=CIRCLE('',#36760,0.3);
#12611=CIRCLE('',#36761,0.3);
#12612=CIRCLE('',#36762,0.299999999999999);
#12613=CIRCLE('',#36764,0.6);
#12614=CIRCLE('',#36766,0.6);
#12615=CIRCLE('',#36768,0.6);
#12616=CIRCLE('',#36770,12.5256279976);
#12617=CIRCLE('',#36771,0.3);
#12618=CIRCLE('',#36772,12.2256279976);
#12619=CIRCLE('',#36776,14.9875296363);
#12620=CIRCLE('',#36777,0.3);
#12621=CIRCLE('',#36778,14.6875296363);
#12622=CIRCLE('',#36781,16.1875296363);
#12623=CIRCLE('',#36782,16.1875296363);
#12624=CIRCLE('',#36783,16.1875296363);
#12625=CIRCLE('',#36785,16.1875296363);
#12626=CIRCLE('',#36789,0.3);
#12627=CIRCLE('',#36794,0.3);
#12628=CIRCLE('',#36798,0.3);
#12629=CIRCLE('',#36799,0.3);
#12630=CIRCLE('',#36801,0.3);
#12631=CIRCLE('',#36802,0.3);
#12632=CIRCLE('',#36804,0.300000000000001);
#12633=CIRCLE('',#36805,15.6875296363);
#12634=CIRCLE('',#36809,0.599999999902816);
#12635=CIRCLE('',#36811,0.3);
#12636=CIRCLE('',#36812,0.3);
#12637=CIRCLE('',#36814,7.84541841273);
#12638=CIRCLE('',#36815,7.84541841273);
#12639=CIRCLE('',#36817,0.3);
#12640=CIRCLE('',#36818,0.3);
#12641=CIRCLE('',#36821,0.3);
#12642=CIRCLE('',#36823,0.3);
#12643=CIRCLE('',#36824,0.3);
#12644=CIRCLE('',#36826,14.6875296363);
#12645=CIRCLE('',#36827,14.6875296363);
#12646=CIRCLE('',#36829,0.3);
#12647=CIRCLE('',#36830,0.3);
#12648=CIRCLE('',#36832,4.89295371933);
#12649=CIRCLE('',#36833,0.3);
#12650=CIRCLE('',#36834,5.19295371933);
#12651=CIRCLE('',#36835,0.3);
#12652=CIRCLE('',#36837,0.6);
#12653=CIRCLE('',#36838,0.3);
#12654=CIRCLE('',#36839,0.3);
#12655=CIRCLE('',#36841,0.3);
#12656=CIRCLE('',#36843,0.6);
#12657=CIRCLE('',#36844,0.3);
#12658=CIRCLE('',#36845,0.299999999999999);
#12659=CIRCLE('',#36847,6.64541841273);
#12660=CIRCLE('',#36848,6.34541841273);
#12661=CIRCLE('',#36849,0.3);
#12662=CIRCLE('',#36851,0.6);
#12663=CIRCLE('',#36852,0.3);
#12664=CIRCLE('',#36853,0.3);
#12665=CIRCLE('',#36855,0.6);
#12666=CIRCLE('',#36856,0.3);
#12667=CIRCLE('',#36857,0.3);
#12668=CIRCLE('',#36860,6.34541841273);
#12669=CIRCLE('',#36861,0.3);
#12670=CIRCLE('',#36862,6.64541841273);
#12671=CIRCLE('',#36863,0.3);
#12672=CIRCLE('',#36867,0.6);
#12673=CIRCLE('',#36868,0.3);
#12674=CIRCLE('',#36869,0.3);
#12675=CIRCLE('',#36876,5.19295371933);
#12676=CIRCLE('',#36877,0.3);
#12677=CIRCLE('',#36878,4.89295371933);
#12678=CIRCLE('',#36880,0.3);
#12679=CIRCLE('',#36881,0.6);
#12680=CIRCLE('',#36882,0.300000000000002);
#12681=CIRCLE('',#36884,0.3);
#12682=CIRCLE('',#36885,0.300000000000002);
#12683=CIRCLE('',#36886,0.6);
#12684=CIRCLE('',#36895,4.89295371933);
#12685=CIRCLE('',#36896,0.3);
#12686=CIRCLE('',#36897,5.19295371933);
#12687=CIRCLE('',#36898,0.3);
#12688=CIRCLE('',#36899,4.89295371933);
#12689=CIRCLE('',#36901,0.6);
#12690=CIRCLE('',#36902,0.3);
#12691=CIRCLE('',#36903,0.3);
#12692=CIRCLE('',#36905,0.3);
#12693=CIRCLE('',#36907,0.6);
#12694=CIRCLE('',#36908,0.3);
#12695=CIRCLE('',#36909,0.3);
#12696=CIRCLE('',#36911,6.64541841273);
#12697=CIRCLE('',#36912,6.34541841273);
#12698=CIRCLE('',#36913,0.3);
#12699=CIRCLE('',#36915,0.6);
#12700=CIRCLE('',#36916,0.300000000000002);
#12701=CIRCLE('',#36917,0.3);
#12702=CIRCLE('',#36919,0.6);
#12703=CIRCLE('',#36920,0.3);
#12704=CIRCLE('',#36921,0.300000000000002);
#12705=CIRCLE('',#36924,0.299999999999996);
#12706=CIRCLE('',#36927,6.04541841273);
#12707=CIRCLE('',#36928,6.34541841273);
#12708=CIRCLE('',#36929,0.300000000000002);
#12709=CIRCLE('',#36931,0.3);
#12710=CIRCLE('',#36932,0.3);
#12711=CIRCLE('',#36934,5.19295371933);
#12712=CIRCLE('',#36935,5.49295371933);
#12713=CIRCLE('',#36937,0.3);
#12714=CIRCLE('',#36938,0.300000000000002);
#12715=CIRCLE('',#36940,0.3);
#12716=CIRCLE('',#36941,0.300000000000002);
#12717=CIRCLE('',#36943,0.3);
#12718=CIRCLE('',#36944,0.3);
#12719=CIRCLE('',#36947,5.49295371933);
#12720=CIRCLE('',#36948,5.19295371933);
#12721=CIRCLE('',#36949,0.299999999999998);
#12722=CIRCLE('',#36951,0.3);
#12723=CIRCLE('',#36952,0.3);
#12724=CIRCLE('',#36953,0.6);
#12725=CIRCLE('',#36955,7.84541841273);
#12726=CIRCLE('',#36956,0.3);
#12727=CIRCLE('',#36957,7.54541841273);
#12728=CIRCLE('',#36959,0.3);
#12729=CIRCLE('',#36960,0.6);
#12730=CIRCLE('',#36961,0.3);
#12731=CIRCLE('',#36963,0.3);
#12732=CIRCLE('',#36964,0.3);
#12733=CIRCLE('',#36965,0.6);
#12734=CIRCLE('',#36967,0.3);
#12735=CIRCLE('',#36968,0.3);
#12736=CIRCLE('',#36970,12.5256279976);
#12737=CIRCLE('',#36972,0.3);
#12738=CIRCLE('',#36974,12.8256279976);
#12739=CIRCLE('',#36976,0.3);
#12740=CIRCLE('',#36977,0.3);
#12741=CIRCLE('',#36979,5.49295371933);
#12742=CIRCLE('',#36980,5.19295371933);
#12743=CIRCLE('',#36982,15.8875296363);
#12744=CIRCLE('',#36983,0.385778366608001);
#12745=CIRCLE('',#36985,15.8875296363);
#12746=CIRCLE('',#36986,0.299999999999999);
#12747=CIRCLE('',#36987,0.3);
#12748=CIRCLE('',#36989,15.3875296363);
#12749=CIRCLE('',#36990,0.3);
#12750=CIRCLE('',#36991,15.6875296363);
#12751=CIRCLE('',#36992,0.3);
#12752=CIRCLE('',#36994,15.8875296363);
#12753=CIRCLE('',#36995,0.300000000000006);
#12754=CIRCLE('',#36997,0.685778366608001);
#12755=CIRCLE('',#36998,0.3);
#12756=CIRCLE('',#36999,0.985778366608001);
#12757=CIRCLE('',#37001,0.300000000000012);
#12758=CIRCLE('',#37002,0.3);
#12759=CIRCLE('',#37004,0.3);
#12760=CIRCLE('',#37006,3.);
#12761=CIRCLE('',#37008,2.7);
#12762=CIRCLE('',#37009,3.);
#12763=CIRCLE('',#37014,0.299999999999996);
#12764=CIRCLE('',#37017,0.3);
#12765=CIRCLE('',#37020,0.3);
#12766=CIRCLE('',#37022,0.3);
#12767=CIRCLE('',#37023,0.3);
#12768=CIRCLE('',#37024,0.3);
#12769=CIRCLE('',#37026,0.3);
#12770=CIRCLE('',#37028,0.300000000000014);
#12771=CIRCLE('',#37032,0.3);
#12772=CIRCLE('',#37035,0.299999999999999);
#12773=CIRCLE('',#37036,0.3);
#12774=CIRCLE('',#37038,0.3);
#12775=CIRCLE('',#37040,0.3);
#12776=CIRCLE('',#37041,8.14541841273);
#12777=CIRCLE('',#37042,7.86257590088);
#12778=CIRCLE('',#37044,0.282842511848);
#12779=CIRCLE('',#37045,0.3);
#12780=CIRCLE('',#37047,0.3);
#12781=CIRCLE('',#37049,0.3);
#12782=CIRCLE('',#37051,0.282842712475);
#12783=CIRCLE('',#37052,0.3);
#12784=CIRCLE('',#37054,14.3875296363);
#12785=CIRCLE('',#37055,14.670372344);
#12786=CIRCLE('',#37058,0.300000000000002);
#12787=CIRCLE('',#37062,0.3);
#12788=CIRCLE('',#37065,0.3);
#12789=CIRCLE('',#37067,6.34541841273);
#12790=CIRCLE('',#37081,0.3);
#12791=CIRCLE('',#37083,6.34541841273);
#12792=CIRCLE('',#37085,0.3);
#12793=CIRCLE('',#37087,0.3);
#12794=CIRCLE('',#37090,0.3);
#12795=CIRCLE('',#37092,6.04541841273);
#12796=CIRCLE('',#37094,0.300000000000002);
#12797=CIRCLE('',#37096,0.300000000000002);
#12798=CIRCLE('',#37099,6.04541841273);
#12799=CIRCLE('',#37102,0.3);
#12800=CIRCLE('',#37103,0.3);
#12801=CIRCLE('',#37104,0.3);
#12802=CIRCLE('',#37109,0.685778366608001);
#12803=CIRCLE('',#37111,0.3);
#12804=CIRCLE('',#37120,0.6);
#12805=CIRCLE('',#37121,0.300000000000002);
#12806=CIRCLE('',#37123,0.3);
#12807=CIRCLE('',#37124,0.3);
#12808=CIRCLE('',#37125,0.3);
#12809=CIRCLE('',#37128,7.84541841273);
#12810=CIRCLE('',#37130,8.14541841273);
#12811=CIRCLE('',#37132,0.3);
#12812=CIRCLE('',#37133,0.3);
#12813=CIRCLE('',#37135,0.3);
#12814=CIRCLE('',#37136,0.6);
#12815=CIRCLE('',#37138,0.3);
#12816=CIRCLE('',#37139,13.3462109523);
#12817=CIRCLE('',#37141,0.3);
#12818=CIRCLE('',#37142,0.6);
#12819=CIRCLE('',#37144,0.3);
#12820=CIRCLE('',#37146,0.3);
#12821=CIRCLE('',#37147,0.3);
#12822=CIRCLE('',#37148,0.300000000000001);
#12823=CIRCLE('',#37150,14.6875296363);
#12824=CIRCLE('',#37151,14.3875296363);
#12825=CIRCLE('',#37153,0.3);
#12826=CIRCLE('',#37155,14.6875296363);
#12827=CIRCLE('',#37156,14.3875296363);
#12828=CIRCLE('',#37161,0.3);
#12829=CIRCLE('',#37163,0.3);
#12830=CIRCLE('',#37169,0.299999999999999);
#12831=CIRCLE('',#37171,0.3);
#12832=CIRCLE('',#37172,0.6);
#12833=CIRCLE('',#37174,0.3);
#12834=CIRCLE('',#37175,7.54541841273);
#12835=CIRCLE('',#37177,0.3);
#12836=CIRCLE('',#37178,0.6);
#12837=CIRCLE('',#37180,0.3);
#12838=CIRCLE('',#37181,0.3);
#12839=CIRCLE('',#37183,0.6);
#12840=CIRCLE('',#37184,0.3);
#12841=CIRCLE('',#37186,0.300000000000002);
#12842=CIRCLE('',#37187,0.6);
#12843=CIRCLE('',#37189,14.9875296363);
#12844=CIRCLE('',#37191,0.299999999999999);
#12845=CIRCLE('',#37192,0.6);
#12846=CIRCLE('',#37194,0.299999999999998);
#12847=CIRCLE('',#37195,13.216744254);
#12848=CIRCLE('',#37200,0.300000000000002);
#12849=CIRCLE('',#37206,15.8875296363);
#12850=CIRCLE('',#37208,0.999999999999999);
#12851=CIRCLE('',#37210,0.825178907983792);
#12852=CIRCLE('',#37212,14.6875296363);
#12853=CIRCLE('',#37213,0.299999999999999);
#12854=CIRCLE('',#37214,14.9875296363);
#12855=CIRCLE('',#37216,0.3);
#12856=CIRCLE('',#37217,0.300000000000002);
#12857=CIRCLE('',#37218,0.6);
#12858=CIRCLE('',#37220,0.300000000000002);
#12859=CIRCLE('',#37222,0.3);
#12860=CIRCLE('',#37223,0.3);
#12861=CIRCLE('',#37224,0.6);
#12862=CIRCLE('',#37226,7.84541841273);
#12863=CIRCLE('',#37227,0.3);
#12864=CIRCLE('',#37228,7.54541841273);
#12865=CIRCLE('',#37230,0.3);
#12866=CIRCLE('',#37231,0.299999999999999);
#12867=CIRCLE('',#37232,0.6);
#12868=CIRCLE('',#37237,14.6875296363);
#12869=CIRCLE('',#37239,0.999999999999999);
#12870=CIRCLE('',#37241,14.6875296363);
#12871=CIRCLE('',#37243,0.3);
#12872=CIRCLE('',#37245,14.6875296363);
#12873=CIRCLE('',#37247,0.3);
#12874=CIRCLE('',#37250,0.3);
#12875=CIRCLE('',#37252,7.84541841273);
#12876=CIRCLE('',#37254,0.3);
#12877=CIRCLE('',#37257,0.3);
#12878=CIRCLE('',#37259,0.3);
#12879=CIRCLE('',#37260,0.3);
#12880=CIRCLE('',#37262,14.3875296363);
#12881=CIRCLE('',#37263,0.3);
#12882=CIRCLE('',#37265,0.699999999999999);
#12883=CIRCLE('',#37266,0.3);
#12884=CIRCLE('',#37268,0.300000000000001);
#12885=CIRCLE('',#37269,0.3);
#12886=CIRCLE('',#37271,14.3875296363);
#12887=CIRCLE('',#37273,0.3);
#12888=CIRCLE('',#37274,0.3);
#12889=CIRCLE('',#37276,14.3875296363);
#12890=CIRCLE('',#37278,0.300000000000002);
#12891=CIRCLE('',#37281,0.3);
#12892=CIRCLE('',#37283,8.14541841273);
#12893=CIRCLE('',#37285,0.3);
#12894=CIRCLE('',#37288,0.3);
#12895=CIRCLE('',#37290,0.6);
#12896=CIRCLE('',#37291,0.299999999999999);
#12897=CIRCLE('',#37293,13.216744254);
#12898=CIRCLE('',#37294,0.299999999999999);
#12899=CIRCLE('',#37296,0.6);
#12900=CIRCLE('',#37299,0.3);
#12901=CIRCLE('',#37300,0.3);
#12902=CIRCLE('',#37303,13.516744254);
#12903=CIRCLE('',#37304,13.516744254);
#12904=CIRCLE('',#37306,0.3);
#12905=CIRCLE('',#37308,0.3);
#12906=CIRCLE('',#37310,0.3);
#12907=CIRCLE('',#37313,0.3);
#12908=CIRCLE('',#37314,0.3);
#12909=CIRCLE('',#37316,13.516744254);
#12910=CIRCLE('',#37317,13.516744254);
#12911=CIRCLE('',#37319,0.3);
#12912=CIRCLE('',#37320,0.3);
#12913=CIRCLE('',#37322,0.861212043428353);
#12914=CIRCLE('',#37324,0.3);
#12915=CIRCLE('',#37325,0.300000000000002);
#12916=CIRCLE('',#37327,0.299999999999999);
#12917=CIRCLE('',#37329,0.3);
#12918=CIRCLE('',#37330,13.816744254);
#12919=CIRCLE('',#37332,0.3);
#12920=CIRCLE('',#37334,0.3);
#12921=CIRCLE('',#37336,0.3);
#12922=CIRCLE('',#37337,0.3);
#12923=CIRCLE('',#37338,0.6);
#12924=CIRCLE('',#37340,0.300000000000001);
#12925=CIRCLE('',#37341,14.6875296363);
#12926=CIRCLE('',#37342,14.9875296363);
#12927=CIRCLE('',#37344,0.299999999999999);
#12928=CIRCLE('',#37345,0.6);
#12929=CIRCLE('',#37347,0.300000000000001);
#12930=CIRCLE('',#37348,14.6875296363);
#12931=CIRCLE('',#37349,14.9875296363);
#12932=CIRCLE('',#37351,0.3);
#12933=CIRCLE('',#37352,0.6);
#12934=CIRCLE('',#37354,0.3);
#12935=CIRCLE('',#37356,0.299999999999999);
#12936=CIRCLE('',#37358,0.299999999999999);
#12937=CIRCLE('',#37359,13.816744254);
#12938=CIRCLE('',#37361,0.3);
#12939=CIRCLE('',#37363,0.300000000000007);
#12940=CIRCLE('',#37365,15.3875296363);
#12941=CIRCLE('',#37366,2.7);
#12942=CIRCLE('',#37369,0.3);
#12943=CIRCLE('',#37370,0.3);
#12944=CIRCLE('',#37372,13.6462109523);
#12945=CIRCLE('',#37373,13.6462109523);
#12946=CIRCLE('',#37375,0.3);
#12947=CIRCLE('',#37376,0.3);
#12948=CIRCLE('',#37379,0.300000000000001);
#12949=CIRCLE('',#37380,0.3);
#12950=CIRCLE('',#37382,0.3);
#12951=CIRCLE('',#37383,0.29999999999957);
#12952=CIRCLE('',#37385,0.3);
#12953=CIRCLE('',#37386,0.3);
#12954=CIRCLE('',#37388,0.3);
#12955=CIRCLE('',#37390,0.3);
#12956=CIRCLE('',#37391,13.9462109523);
#12957=CIRCLE('',#37393,0.3);
#12958=CIRCLE('',#37395,0.3);
#12959=CIRCLE('',#37397,0.3);
#12960=CIRCLE('',#37398,0.6);
#12961=CIRCLE('',#37399,1.);
#12962=CIRCLE('',#37401,14.6875296363);
#12963=CIRCLE('',#37402,14.9875296363);
#12964=CIRCLE('',#37404,0.3);
#12965=CIRCLE('',#37405,3.);
#12966=CIRCLE('',#37407,15.8875296363);
#12967=CIRCLE('',#37408,16.1875296363);
#12968=CIRCLE('',#37411,0.299999999999998);
#12969=CIRCLE('',#37413,7.84541841273);
#12970=CIRCLE('',#37414,0.299999999999989);
#12971=CIRCLE('',#37415,8.14541841273);
#12972=CIRCLE('',#37418,14.3875296363);
#12973=CIRCLE('',#37419,0.300000000000001);
#12974=CIRCLE('',#37420,14.6875296363);
#12975=CIRCLE('',#37422,0.3);
#12976=CIRCLE('',#37425,0.3);
#12977=CIRCLE('',#37427,7.84541841273);
#12978=CIRCLE('',#37429,0.3);
#12979=CIRCLE('',#37432,0.3);
#12980=CIRCLE('',#37434,14.6875296363);
#12981=CIRCLE('',#37436,0.3);
#12982=CIRCLE('',#37438,0.3);
#12983=CIRCLE('',#37439,0.3);
#12984=CIRCLE('',#37441,0.3);
#12985=CIRCLE('',#37443,0.3);
#12986=CIRCLE('',#37444,7.54541841273);
#12987=CIRCLE('',#37445,0.3);
#12988=CIRCLE('',#37447,0.3);
#12989=CIRCLE('',#37449,0.300000000000002);
#12990=CIRCLE('',#37450,0.300000000000002);
#12991=CIRCLE('',#37452,0.3);
#12992=CIRCLE('',#37454,0.300000000000001);
#12993=CIRCLE('',#37455,14.9875296363);
#12994=CIRCLE('',#37456,0.3);
#12995=CIRCLE('',#37458,0.6);
#12996=CIRCLE('',#37460,0.299999999999999);
#12997=CIRCLE('',#37461,0.3);
#12998=CIRCLE('',#37462,0.3);
#12999=CIRCLE('',#37464,0.6);
#13000=CIRCLE('',#37466,0.6);
#13001=CIRCLE('',#37468,0.6);
#13002=CIRCLE('',#37469,1.);
#13003=CIRCLE('',#37471,12.2256279976);
#13004=CIRCLE('',#37472,0.3);
#13005=CIRCLE('',#37473,12.5256279976);
#13006=CIRCLE('',#37477,14.6875296363);
#13007=CIRCLE('',#37478,0.3);
#13008=CIRCLE('',#37479,14.9875296363);
#13009=CIRCLE('',#37481,0.3);
#13010=CIRCLE('',#37482,0.3);
#13011=CIRCLE('',#37485,3.00001824423103);
#13012=CIRCLE('',#37487,16.1875296363);
#13013=CIRCLE('',#37489,16.1875296363);
#13014=CIRCLE('',#37490,16.1875296363);
#13015=CIRCLE('',#37491,16.1875296363);
#13016=CIRCLE('',#37493,0.3);
#13017=CIRCLE('',#37494,0.3);
#13018=CIRCLE('',#37498,0.3);
#13019=CIRCLE('',#37503,0.3);
#13020=CIRCLE('',#37506,0.3);
#13021=CIRCLE('',#37507,0.3);
#13022=CIRCLE('',#37509,0.3);
#13023=CIRCLE('',#37510,0.3);
#13024=CIRCLE('',#37512,15.6875296363);
#13025=CIRCLE('',#37513,0.300000000000001);
#13026=CIRCLE('',#37515,15.6875296363);
#13027=CIRCLE('',#37516,15.6875296363);
#13028=CIRCLE('',#37517,15.6875296363);
#13029=CIRCLE('',#37519,0.3);
#13030=CIRCLE('',#37521,0.599999999902816);
#13031=CIRCLE('',#37523,0.3);
#13032=CIRCLE('',#37524,0.3);
#13033=CIRCLE('',#37526,7.84541841273);
#13034=CIRCLE('',#37527,7.84541841273);
#13035=CIRCLE('',#37529,0.3);
#13036=CIRCLE('',#37530,0.3);
#13037=CIRCLE('',#37533,0.3);
#13038=CIRCLE('',#37535,0.3);
#13039=CIRCLE('',#37536,0.3);
#13040=CIRCLE('',#37538,14.6875296363);
#13041=CIRCLE('',#37539,14.6875296363);
#13042=CIRCLE('',#37541,0.3);
#13043=CIRCLE('',#37542,0.3);
#13044=CIRCLE('',#37544,0.3);
#13045=CIRCLE('',#37545,5.19295371933);
#13046=CIRCLE('',#37546,0.3);
#13047=CIRCLE('',#37547,4.89295371933);
#13048=CIRCLE('',#37549,0.3);
#13049=CIRCLE('',#37550,0.3);
#13050=CIRCLE('',#37551,0.6);
#13051=CIRCLE('',#37553,0.3);
#13052=CIRCLE('',#37555,0.299999999999999);
#13053=CIRCLE('',#37556,0.3);
#13054=CIRCLE('',#37557,0.6);
#13055=CIRCLE('',#37559,0.3);
#13056=CIRCLE('',#37560,6.34541841273);
#13057=CIRCLE('',#37561,6.64541841273);
#13058=CIRCLE('',#37563,0.3);
#13059=CIRCLE('',#37564,0.3);
#13060=CIRCLE('',#37565,0.6);
#13061=CIRCLE('',#37567,0.3);
#13062=CIRCLE('',#37568,0.3);
#13063=CIRCLE('',#37569,0.6);
#13064=CIRCLE('',#37572,0.3);
#13065=CIRCLE('',#37573,6.64541841273);
#13066=CIRCLE('',#37574,0.3);
#13067=CIRCLE('',#37575,6.34541841273);
#13068=CIRCLE('',#37579,0.3);
#13069=CIRCLE('',#37580,0.3);
#13070=CIRCLE('',#37581,0.6);
#13071=CIRCLE('',#37587,4.89295371933);
#13072=CIRCLE('',#37588,0.3);
#13073=CIRCLE('',#37589,5.19295371933);
#13074=CIRCLE('',#37591,0.300000000000002);
#13075=CIRCLE('',#37592,0.6);
#13076=CIRCLE('',#37593,0.3);
#13077=CIRCLE('',#37595,0.6);
#13078=CIRCLE('',#37596,0.300000000000002);
#13079=CIRCLE('',#37597,0.3);
#13080=CIRCLE('',#37606,4.89295371933);
#13081=CIRCLE('',#37607,0.3);
#13082=CIRCLE('',#37608,5.19295371933);
#13083=CIRCLE('',#37609,0.3);
#13084=CIRCLE('',#37610,4.89295371933);
#13085=CIRCLE('',#37612,0.3);
#13086=CIRCLE('',#37613,0.3);
#13087=CIRCLE('',#37614,0.6);
#13088=CIRCLE('',#37616,0.3);
#13089=CIRCLE('',#37618,0.3);
#13090=CIRCLE('',#37619,0.3);
#13091=CIRCLE('',#37620,0.6);
#13092=CIRCLE('',#37622,0.3);
#13093=CIRCLE('',#37623,6.34541841273);
#13094=CIRCLE('',#37624,6.64541841273);
#13095=CIRCLE('',#37626,0.3);
#13096=CIRCLE('',#37627,0.300000000000002);
#13097=CIRCLE('',#37628,0.6);
#13098=CIRCLE('',#37630,0.300000000000002);
#13099=CIRCLE('',#37631,0.3);
#13100=CIRCLE('',#37632,0.6);
#13101=CIRCLE('',#37636,0.300000000000002);
#13102=CIRCLE('',#37638,6.34541841273);
#13103=CIRCLE('',#37639,6.04541841273);
#13104=CIRCLE('',#37641,0.3);
#13105=CIRCLE('',#37642,0.3);
#13106=CIRCLE('',#37644,5.49295371933);
#13107=CIRCLE('',#37645,5.19295371933);
#13108=CIRCLE('',#37647,0.300000000000002);
#13109=CIRCLE('',#37648,0.3);
#13110=CIRCLE('',#37650,0.300000000000002);
#13111=CIRCLE('',#37651,0.3);
#13112=CIRCLE('',#37653,0.3);
#13113=CIRCLE('',#37654,0.3);
#13114=CIRCLE('',#37657,5.19295371933);
#13115=CIRCLE('',#37658,5.49295371933);
#13116=CIRCLE('',#37660,0.6);
#13117=CIRCLE('',#37661,0.3);
#13118=CIRCLE('',#37662,0.3);
#13119=CIRCLE('',#37664,7.54541841273);
#13120=CIRCLE('',#37665,0.3);
#13121=CIRCLE('',#37666,7.84541841273);
#13122=CIRCLE('',#37668,0.3);
#13123=CIRCLE('',#37669,0.6);
#13124=CIRCLE('',#37670,0.3);
#13125=CIRCLE('',#37672,0.6);
#13126=CIRCLE('',#37673,0.3);
#13127=CIRCLE('',#37674,0.3);
#13128=CIRCLE('',#37676,0.3);
#13129=CIRCLE('',#37677,0.3);
#13130=CIRCLE('',#37679,0.999999999999988);
#13131=CIRCLE('',#37681,12.5256279976);
#13132=CIRCLE('',#37683,0.3);
#13133=CIRCLE('',#37685,12.8256279976);
#13134=CIRCLE('',#37687,0.3);
#13135=CIRCLE('',#37688,0.3);
#13136=CIRCLE('',#37690,5.19295371933);
#13137=CIRCLE('',#37691,0.299999999999998);
#13138=CIRCLE('',#37692,5.49295371933);
#13139=CIRCLE('',#37694,0.385778366608001);
#13140=CIRCLE('',#37695,15.8875296363);
#13141=CIRCLE('',#37697,0.3);
#13142=CIRCLE('',#37698,0.299999999999999);
#13143=CIRCLE('',#37699,15.8875296363);
#13144=CIRCLE('',#37701,0.3);
#13145=CIRCLE('',#37702,0.3);
#13146=CIRCLE('',#37703,15.3875296363);
#13147=CIRCLE('',#37705,0.0999999999999999);
#13148=CIRCLE('',#37706,0.0999999999999999);
#13149=CIRCLE('',#37708,0.0999999999999999);
#13150=CIRCLE('',#37709,0.0999999999999999);
#13151=CIRCLE('',#37711,0.4);
#13152=CIRCLE('',#37712,0.0999999999999999);
#13153=CIRCLE('',#37714,0.0999999999999999);
#13154=CIRCLE('',#37716,0.4);
#13155=CIRCLE('',#37717,0.0999999999999999);
#13156=CIRCLE('',#37719,0.0999999999999999);
#13157=CIRCLE('',#37721,0.4);
#13158=CIRCLE('',#37723,0.4);
#13159=CIRCLE('',#37724,0.0999999999999999);
#13160=CIRCLE('',#37726,0.0999999999999999);
#13161=CIRCLE('',#37728,0.0999999999999999);
#13162=CIRCLE('',#37729,0.4);
#13163=CIRCLE('',#37731,0.0999999999999999);
#13164=CIRCLE('',#37733,0.0999999999999999);
#13165=CIRCLE('',#37734,0.4);
#13166=CIRCLE('',#37736,0.0999999999999999);
#13167=CIRCLE('',#37738,0.0999999999999999);
#13168=CIRCLE('',#37739,0.4);
#13169=CIRCLE('',#37741,0.0999999999999999);
#13170=CIRCLE('',#37743,0.4);
#13171=CIRCLE('',#37745,2.7);
#13172=CIRCLE('',#37746,0.6);
#13173=CIRCLE('',#37747,15.8875296363);
#13174=CIRCLE('',#37748,0.985778366608001);
#13175=CIRCLE('',#37751,0.3);
#13176=CIRCLE('',#37752,0.685778366608001);
#13177=CIRCLE('',#37753,0.3);
#13178=CIRCLE('',#37755,0.3);
#13179=CIRCLE('',#37756,0.300000000000006);
#13180=CIRCLE('',#37758,0.3);
#13181=CIRCLE('',#37760,3.);
#13182=CIRCLE('',#37762,3.);
#13183=CIRCLE('',#37770,0.3);
#13184=CIRCLE('',#37773,0.3);
#13185=CIRCLE('',#37775,0.300000000000002);
#13186=CIRCLE('',#37778,0.300000000000002);
#13187=CIRCLE('',#37780,15.3875296363);
#13188=CIRCLE('',#37781,0.300000000000003);
#13189=CIRCLE('',#37783,7.86257571140099);
#13190=CIRCLE('',#37784,0.282842712475);
#13191=CIRCLE('',#37785,0.282842712475);
#13192=CIRCLE('',#37786,14.6703723485088);
#13193=CIRCLE('',#37788,0.3);
#13194=CIRCLE('',#37789,0.3);
#13195=CIRCLE('',#37790,0.3);
#13196=CIRCLE('',#37792,0.3);
#13197=CIRCLE('',#37797,0.3);
#13198=CIRCLE('',#37799,0.3);
#13199=CIRCLE('',#37800,0.299999999999999);
#13200=CIRCLE('',#37802,0.3);
#13201=CIRCLE('',#37804,8.14541841273);
#13202=CIRCLE('',#37805,0.3);
#13203=CIRCLE('',#37807,0.3);
#13204=CIRCLE('',#37809,0.3);
#13205=CIRCLE('',#37811,0.3);
#13206=CIRCLE('',#37813,0.3);
#13207=CIRCLE('',#37815,14.3875296363);
#13208=CIRCLE('',#37821,0.3);
#13209=CIRCLE('',#37824,0.3);
#13210=CIRCLE('',#37826,6.34541841273);
#13211=CIRCLE('',#37840,0.3);
#13212=CIRCLE('',#37842,6.34541841273);
#13213=CIRCLE('',#37844,0.3);
#13214=CIRCLE('',#37846,0.3);
#13215=CIRCLE('',#37849,0.3);
#13216=CIRCLE('',#37851,6.04541841273);
#13217=CIRCLE('',#37853,0.300000000000002);
#13218=CIRCLE('',#37855,0.300000000000002);
#13219=CIRCLE('',#37858,6.04541841273);
#13220=CIRCLE('',#37861,0.3);
#13221=CIRCLE('',#37862,0.3);
#13222=CIRCLE('',#37863,0.3);
#13223=CIRCLE('',#37868,0.685778366608001);
#13224=CIRCLE('',#37870,0.3);
#13225=CIRCLE('',#37873,0.3);
#13226=CIRCLE('',#37880,0.3);
#13227=CIRCLE('',#37881,0.3);
#13228=CIRCLE('',#37882,0.3);
#13229=CIRCLE('',#37885,7.84541841273);
#13230=CIRCLE('',#37887,8.14541841273);
#13231=CIRCLE('',#37889,0.3);
#13232=CIRCLE('',#37890,0.3);
#13233=CIRCLE('',#37892,0.6);
#13234=CIRCLE('',#37893,0.3);
#13235=CIRCLE('',#37895,13.3462109523);
#13236=CIRCLE('',#37896,0.3);
#13237=CIRCLE('',#37898,0.6);
#13238=CIRCLE('',#37899,0.3);
#13239=CIRCLE('',#37901,0.3);
#13240=CIRCLE('',#37903,14.3875296363);
#13241=CIRCLE('',#37904,14.3875296363);
#13242=CIRCLE('',#37906,0.3);
#13243=CIRCLE('',#37907,0.3);
#13244=CIRCLE('',#37908,0.300000000000001);
#13245=CIRCLE('',#37910,14.6875296363);
#13246=CIRCLE('',#37912,0.3);
#13247=CIRCLE('',#37913,1.);
#13248=CIRCLE('',#37915,14.6875296363);
#13249=CIRCLE('',#37921,0.3);
#13250=CIRCLE('',#37923,0.3);
#13251=CIRCLE('',#37929,0.299999999999999);
#13252=CIRCLE('',#37931,0.6);
#13253=CIRCLE('',#37932,0.3);
#13254=CIRCLE('',#37934,7.54541841273);
#13255=CIRCLE('',#37935,0.3);
#13256=CIRCLE('',#37937,0.6);
#13257=CIRCLE('',#37938,0.3);
#13258=CIRCLE('',#37940,0.3);
#13259=CIRCLE('',#37941,0.3);
#13260=CIRCLE('',#37943,0.3);
#13261=CIRCLE('',#37944,0.6);
#13262=CIRCLE('',#37946,0.6);
#13263=CIRCLE('',#37947,0.3);
#13264=CIRCLE('',#37949,14.9875296363);
#13265=CIRCLE('',#37951,0.6);
#13266=CIRCLE('',#37952,0.299999999999999);
#13267=CIRCLE('',#37954,13.216744254);
#13268=CIRCLE('',#37966,15.8875296363);
#13269=CIRCLE('',#37968,15.3875296363);
#13270=CIRCLE('',#37970,0.0999999999999999);
#13271=CIRCLE('',#37971,0.0999999999999999);
#13272=CIRCLE('',#37973,0.0999999999999999);
#13273=CIRCLE('',#37976,0.0999999999999999);
#13274=CIRCLE('',#37978,0.4);
#13275=CIRCLE('',#37980,0.0999999999999999);
#13276=CIRCLE('',#37981,0.4);
#13277=CIRCLE('',#37983,0.0999999999999999);
#13278=CIRCLE('',#37985,0.4);
#13279=CIRCLE('',#37986,0.0999999999999999);
#13280=CIRCLE('',#37990,0.0999999999999999);
#13281=CIRCLE('',#37992,0.4);
#13282=CIRCLE('',#37994,0.6);
#13283=CIRCLE('',#37995,7.54541841273);
#13284=CIRCLE('',#37996,0.6);
#13285=CIRCLE('',#37997,0.6);
#13286=CIRCLE('',#37998,14.9875296363);
#13287=CIRCLE('',#38000,0.999999999999999);
#13288=CIRCLE('',#38002,0.825178907983792);
#13289=CIRCLE('',#38004,0.299999999999999);
#13290=CIRCLE('',#38005,14.6875296363);
#13291=CIRCLE('',#38007,0.300000000000002);
#13292=CIRCLE('',#38008,0.3);
#13293=CIRCLE('',#38010,0.300000000000002);
#13294=CIRCLE('',#38012,0.3);
#13295=CIRCLE('',#38013,0.3);
#13296=CIRCLE('',#38015,0.3);
#13297=CIRCLE('',#38016,7.84541841273);
#13298=CIRCLE('',#38018,0.299999999999999);
#13299=CIRCLE('',#38019,0.3);
#13300=CIRCLE('',#38024,14.6875296363);
#13301=CIRCLE('',#38026,0.999999999999999);
#13302=CIRCLE('',#38028,14.6875296363);
#13303=CIRCLE('',#38030,0.3);
#13304=CIRCLE('',#38032,14.6875296363);
#13305=CIRCLE('',#38034,0.3);
#13306=CIRCLE('',#38037,0.3);
#13307=CIRCLE('',#38039,7.84541841273);
#13308=CIRCLE('',#38041,0.3);
#13309=CIRCLE('',#38044,0.3);
#13310=CIRCLE('',#38046,0.3);
#13311=CIRCLE('',#38047,0.3);
#13312=CIRCLE('',#38049,0.3);
#13313=CIRCLE('',#38050,14.3875296363);
#13314=CIRCLE('',#38052,0.3);
#13315=CIRCLE('',#38053,0.699999999999999);
#13316=CIRCLE('',#38055,0.3);
#13317=CIRCLE('',#38056,0.300000000000001);
#13318=CIRCLE('',#38058,14.3875296363);
#13319=CIRCLE('',#38060,0.3);
#13320=CIRCLE('',#38061,0.3);
#13321=CIRCLE('',#38063,0.300000000000002);
#13322=CIRCLE('',#38064,14.3875296363);
#13323=CIRCLE('',#38066,0.300000000000002);
#13324=CIRCLE('',#38068,0.299999999999998);
#13325=CIRCLE('',#38070,0.3);
#13326=CIRCLE('',#38072,0.299999999999994);
#13327=CIRCLE('',#38073,8.14541841273);
#13328=CIRCLE('',#38075,0.299999999999999);
#13329=CIRCLE('',#38078,0.3);
#13330=CIRCLE('',#38080,0.299999999999999);
#13331=CIRCLE('',#38081,0.6);
#13332=CIRCLE('',#38083,0.299999999999999);
#13333=CIRCLE('',#38084,13.216744254);
#13334=CIRCLE('',#38086,0.6);
#13335=CIRCLE('',#38090,13.016744254);
#13336=CIRCLE('',#38091,0.3);
#13337=CIRCLE('',#38092,13.316744254);
#13338=CIRCLE('',#38093,0.3);
#13339=CIRCLE('',#38095,25.7066723663);
#13340=CIRCLE('',#38096,25.7066723663);
#13341=CIRCLE('',#38098,0.300005627369098);
#13342=CIRCLE('',#38099,0.3);
#13343=CIRCLE('',#38101,12.2773059952);
#13344=CIRCLE('',#38102,12.2773059952);
#13345=CIRCLE('',#38104,25.2066723663);
#13346=CIRCLE('',#38105,0.5);
#13347=CIRCLE('',#38107,0.5);
#13348=CIRCLE('',#38108,11.7773059952);
#13349=CIRCLE('',#38110,25.2066723663);
#13350=CIRCLE('',#38111,4.5);
#13351=CIRCLE('',#38112,4.5);
#13352=CIRCLE('',#38113,11.7773059952);
#13353=CIRCLE('',#38115,5.);
#13354=CIRCLE('',#38116,0.5);
#13355=CIRCLE('',#38118,5.);
#13356=CIRCLE('',#38120,25.7066723663);
#13357=CIRCLE('',#38122,25.7066723663);
#13358=CIRCLE('',#38124,5.);
#13359=CIRCLE('',#38125,0.5);
#13360=CIRCLE('',#38127,5.);
#13361=CIRCLE('',#38129,0.300005627369097);
#13362=CIRCLE('',#38130,0.3);
#13363=CIRCLE('',#38132,12.2773059952);
#13364=CIRCLE('',#38134,12.2773059952);
#13365=CIRCLE('',#38136,13.616744254);
#13366=CIRCLE('',#38137,2.7);
#13367=CIRCLE('',#38138,15.3875296363);
#13368=CIRCLE('',#38140,0.3);
#13369=CIRCLE('',#38143,0.3);
#13370=CIRCLE('',#38144,13.316744254);
#13371=CIRCLE('',#38145,0.3);
#13372=CIRCLE('',#38147,0.3);
#13373=CIRCLE('',#38149,0.3);
#13374=CIRCLE('',#38151,13.316744254);
#13375=CIRCLE('',#38153,0.299999999999999);
#13376=CIRCLE('',#38155,0.3);
#13377=CIRCLE('',#38157,0.3);
#13378=CIRCLE('',#38160,13.616744254);
#13379=CIRCLE('',#38161,15.3875296363);
#13380=CIRCLE('',#38162,2.7);
#13381=CIRCLE('',#38164,0.3);
#13382=CIRCLE('',#38167,0.3);
#13383=CIRCLE('',#38168,0.3);
#13384=CIRCLE('',#38170,0.3);
#13385=CIRCLE('',#38172,13.316744254);
#13386=CIRCLE('',#38174,0.3);
#13387=CIRCLE('',#38176,0.300000000000001);
#13388=CIRCLE('',#38178,0.3);
#13389=CIRCLE('',#38180,0.3);
#13390=CIRCLE('',#38184,0.3);
#13391=CIRCLE('',#38186,13.7462109523);
#13392=CIRCLE('',#38187,2.8);
#13393=CIRCLE('',#38188,13.7462109523);
#13394=CIRCLE('',#38189,15.8875296363);
#13395=CIRCLE('',#38190,2.7);
#13396=CIRCLE('',#38191,15.8875296363);
#13397=CIRCLE('',#38193,0.3);
#13398=CIRCLE('',#38194,0.3);
#13399=CIRCLE('',#38196,0.3);
#13400=CIRCLE('',#38198,13.4462109523);
#13401=CIRCLE('',#38199,0.3);
#13402=CIRCLE('',#38201,13.4462109523);
#13403=CIRCLE('',#38203,2.5);
#13404=CIRCLE('',#38204,0.3);
#13405=CIRCLE('',#38206,2.5);
#13406=CIRCLE('',#38208,13.4462109523);
#13407=CIRCLE('',#38209,0.3);
#13408=CIRCLE('',#38211,13.4462109523);
#13409=CIRCLE('',#38213,0.3);
#13410=CIRCLE('',#38215,0.3);
#13411=CIRCLE('',#38217,0.3);
#13412=CIRCLE('',#38220,15.6875296363);
#13413=CIRCLE('',#38221,3.);
#13414=CIRCLE('',#38222,16.1875296363);
#13415=CIRCLE('',#38223,3.);
#13416=CIRCLE('',#38224,16.1875296363);
#13417=CIRCLE('',#38225,3.);
#13418=CIRCLE('',#38227,0.3);
#13419=CIRCLE('',#38228,0.300000000000001);
#13420=CIRCLE('',#38230,0.3);
#13421=CIRCLE('',#38231,0.6);
#13422=CIRCLE('',#38233,0.3);
#13423=CIRCLE('',#38234,13.016744254);
#13424=CIRCLE('',#38236,0.299999999999999);
#13425=CIRCLE('',#38237,0.6);
#13426=CIRCLE('',#38239,0.3);
#13427=CIRCLE('',#38241,0.3);
#13428=CIRCLE('',#38242,0.299999999999999);
#13429=CIRCLE('',#38244,0.6);
#13430=CIRCLE('',#38246,0.300000000000001);
#13431=CIRCLE('',#38247,0.6);
#13432=CIRCLE('',#38249,0.3);
#13433=CIRCLE('',#38251,0.3);
#13434=CIRCLE('',#38252,0.3);
#13435=CIRCLE('',#38254,0.3);
#13436=CIRCLE('',#38255,0.6);
#13437=CIRCLE('',#38257,0.3);
#13438=CIRCLE('',#38258,13.1462109523);
#13439=CIRCLE('',#38260,0.3);
#13440=CIRCLE('',#38261,2.2);
#13441=CIRCLE('',#38263,0.3);
#13442=CIRCLE('',#38264,13.1462109523);
#13443=CIRCLE('',#38266,0.3);
#13444=CIRCLE('',#38267,0.6);
#13445=CIRCLE('',#38269,0.3);
#13446=CIRCLE('',#38271,15.8875296363);
#13447=CIRCLE('',#38272,15.8875296363);
#13448=CIRCLE('',#38273,15.3875296363);
#13449=CIRCLE('',#38275,0.3);
#13450=CIRCLE('',#38276,0.3);
#13451=CIRCLE('',#38277,0.3);
#13452=CIRCLE('',#38279,0.299999999999999);
#13453=CIRCLE('',#38280,0.3);
#13454=CIRCLE('',#38281,0.299999999999998);
#13455=CIRCLE('',#38282,0.3);
#13456=CIRCLE('',#38284,16.1875296363);
#13457=CIRCLE('',#38285,0.3);
#13458=CIRCLE('',#38286,0.300000118306239);
#13459=CIRCLE('',#38291,16.1875296363);
#13460=CIRCLE('',#38292,0.3);
#13461=CIRCLE('',#38295,3.);
#13462=CIRCLE('',#38296,0.3);
#13463=CIRCLE('',#38299,0.3);
#13464=CIRCLE('',#38300,0.300000000000001);
#13465=CIRCLE('',#38301,0.3);
#13466=CIRCLE('',#38302,0.3);
#13467=CIRCLE('',#38304,0.3);
#13468=CIRCLE('',#38305,0.299999999999999);
#13469=CIRCLE('',#38306,0.299999999999999);
#13470=CIRCLE('',#38308,16.1875296363);
#13471=CIRCLE('',#38309,0.300000000015482);
#13472=CIRCLE('',#38310,0.3);
#13473=CIRCLE('',#38313,16.1875296363);
#13474=CIRCLE('',#38318,0.300000000000004);
#13475=CIRCLE('',#38319,0.3);
#13476=CIRCLE('',#38320,3.);
#13477=CIRCLE('',#38323,0.3);
#13478=CIRCLE('',#38325,3.);
#13479=CIRCLE('',#38328,0.3);
#13480=CIRCLE('',#38329,0.3);
#13481=CIRCLE('',#38330,0.299999999999999);
#13482=CIRCLE('',#38332,0.3);
#13483=CIRCLE('',#38333,0.299999999999998);
#13484=CIRCLE('',#38334,0.3);
#13485=CIRCLE('',#38335,0.3);
#13486=CIRCLE('',#38337,15.6875296363);
#13487=CIRCLE('',#38339,0.30000000000005);
#13488=CIRCLE('',#38340,15.6875296363);
#13489=CIRCLE('',#38344,15.6875296363);
#13490=CIRCLE('',#38349,4.64715395326);
#13491=CIRCLE('',#38350,4.64715395326);
#13492=CIRCLE('',#38351,4.64715395326);
#13493=CIRCLE('',#38352,0.3);
#13494=CIRCLE('',#38353,4.35610046976);
#13495=CIRCLE('',#38354,0.3);
#13496=CIRCLE('',#38356,8.85);
#13497=CIRCLE('',#38357,7.28184557105);
#13498=CIRCLE('',#38361,7.28184557105);
#13499=CIRCLE('',#38364,8.85);
#13500=CIRCLE('',#38369,1.2046272227);
#13501=CIRCLE('',#38371,1.2046272227);
#13502=CIRCLE('',#38373,1.8);
#13503=CIRCLE('',#38374,7.35);
#13504=CIRCLE('',#38375,1.8);
#13505=CIRCLE('',#38376,8.85);
#13506=CIRCLE('',#38377,10.8);
#13507=CIRCLE('',#38378,1.8);
#13508=CIRCLE('',#38379,1.8);
#13509=CIRCLE('',#38380,13.5204936174);
#13510=CIRCLE('',#38381,1.8);
#13511=CIRCLE('',#38382,14.05);
#13512=CIRCLE('',#38383,1.8);
#13513=CIRCLE('',#38384,13.5204936174);
#13514=CIRCLE('',#38385,1.8);
#13515=CIRCLE('',#38386,1.8);
#13516=CIRCLE('',#38387,10.8);
#13517=CIRCLE('',#38388,8.85);
#13518=CIRCLE('',#38389,1.8);
#13519=CIRCLE('',#38390,7.35);
#13520=CIRCLE('',#38391,1.8);
#13521=CIRCLE('',#38393,4.19792065612);
#13522=CIRCLE('',#38395,0.3);
#13523=CIRCLE('',#38396,0.3);
#13524=CIRCLE('',#38397,0.3);
#13525=CIRCLE('',#38398,0.3);
#13526=CIRCLE('',#38399,8.85);
#13527=CIRCLE('',#38400,8.85);
#13528=CIRCLE('',#38401,8.85);
#13529=CIRCLE('',#38404,1.5);
#13530=CIRCLE('',#38406,2.54997399005);
#13531=CIRCLE('',#38408,8.85);
#13532=CIRCLE('',#38413,8.85);
#13533=CIRCLE('',#38415,8.85);
#13534=CIRCLE('',#38417,2.55);
#13535=CIRCLE('',#38421,8.85);
#13536=CIRCLE('',#38423,2.55);
#13537=CIRCLE('',#38425,8.85);
#13538=CIRCLE('',#38429,8.85);
#13539=CIRCLE('',#38431,8.85);
#13540=CIRCLE('',#38433,2.54997399005);
#13541=CIRCLE('',#38438,8.85);
#13542=CIRCLE('',#38440,7.35);
#13543=CIRCLE('',#38442,7.35);
#13544=CIRCLE('',#38446,8.85);
#13545=CIRCLE('',#38447,1.8);
#13546=CIRCLE('',#38448,1.8);
#13547=CIRCLE('',#38452,8.85);
#13548=CIRCLE('',#38454,1.8);
#13549=CIRCLE('',#38457,1.8);
#13550=CIRCLE('',#38459,1.5);
#13551=CIRCLE('',#38461,8.85);
#13552=CIRCLE('',#38464,2.54997399005);
#13553=CIRCLE('',#38468,2.54997399005);
#13554=CIRCLE('',#38471,8.85);
#13555=CIRCLE('',#38473,8.85);
#13556=CIRCLE('',#38475,2.55);
#13557=CIRCLE('',#38478,8.85);
#13558=CIRCLE('',#38480,2.55);
#13559=CIRCLE('',#38483,0.3);
#13560=CIRCLE('',#38484,0.3);
#13561=CIRCLE('',#38486,12.3);
#13562=CIRCLE('',#38487,0.3);
#13563=CIRCLE('',#38488,0.3);
#13564=CIRCLE('',#38489,15.55);
#13565=CIRCLE('',#38490,0.3);
#13566=CIRCLE('',#38491,0.3);
#13567=CIRCLE('',#38492,15.0204936174);
#13568=CIRCLE('',#38493,0.3);
#13569=CIRCLE('',#38494,0.3);
#13570=CIRCLE('',#38495,15.55);
#13571=CIRCLE('',#38496,0.3);
#13572=CIRCLE('',#38497,0.3);
#13573=CIRCLE('',#38498,15.0204936174);
#13574=CIRCLE('',#38499,0.3);
#13575=CIRCLE('',#38500,0.3);
#13576=CIRCLE('',#38501,15.55);
#13577=CIRCLE('',#38502,0.3);
#13578=CIRCLE('',#38503,0.3);
#13579=CIRCLE('',#38504,12.3);
#13580=CIRCLE('',#38505,10.35);
#13581=CIRCLE('',#38506,0.6);
#13582=CIRCLE('',#38507,0.6);
#13583=CIRCLE('',#38508,0.6);
#13584=CIRCLE('',#38509,0.6);
#13585=CIRCLE('',#38511,12.3);
#13586=CIRCLE('',#38514,10.35);
#13587=CIRCLE('',#38517,12.3);
#13588=CIRCLE('',#38519,0.3);
#13589=CIRCLE('',#38522,0.3);
#13590=CIRCLE('',#38524,15.55);
#13591=CIRCLE('',#38526,0.3);
#13592=CIRCLE('',#38528,0.3);
#13593=CIRCLE('',#38530,15.0204936174);
#13594=CIRCLE('',#38532,0.3);
#13595=CIRCLE('',#38535,0.3);
#13596=CIRCLE('',#38537,15.55);
#13597=CIRCLE('',#38539,0.3);
#13598=CIRCLE('',#38542,0.3);
#13599=CIRCLE('',#38544,15.0204936174);
#13600=CIRCLE('',#38546,0.3);
#13601=CIRCLE('',#38548,0.3);
#13602=CIRCLE('',#38550,15.55);
#13603=CIRCLE('',#38552,0.3);
#13604=CIRCLE('',#38555,0.3);
#13605=CIRCLE('',#38557,8.85);
#13606=CIRCLE('',#38561,8.85);
#13607=CIRCLE('',#38563,8.85);
#13608=CIRCLE('',#38566,8.85);
#13609=CIRCLE('',#38567,8.85);
#13610=CIRCLE('',#38571,0.3);
#13611=CIRCLE('',#38572,0.300000000000002);
#13612=CIRCLE('',#38575,0.300000000000002);
#13613=CIRCLE('',#38578,0.3);
#13614=CIRCLE('',#38579,0.3);
#13615=CIRCLE('',#38582,0.3);
#13616=CIRCLE('',#38584,0.3);
#13617=CIRCLE('',#38585,0.300092356025301);
#13618=CIRCLE('',#38587,0.3);
#13619=CIRCLE('',#38589,0.3);
#13620=CIRCLE('',#38592,4.47840533247);
#13621=CIRCLE('',#38593,0.300092357885528);
#13622=CIRCLE('',#38595,0.3);
#13623=CIRCLE('',#38597,0.3);
#13624=CIRCLE('',#38599,0.3);
#13625=VERTEX_POINT('',#49111);
#13626=VERTEX_POINT('',#49112);
#13627=VERTEX_POINT('',#49114);
#13628=VERTEX_POINT('',#49119);
#13629=VERTEX_POINT('',#49120);
#13630=VERTEX_POINT('',#49126);
#13631=VERTEX_POINT('',#49132);
#13632=VERTEX_POINT('',#49133);
#13633=VERTEX_POINT('',#49135);
#13634=VERTEX_POINT('',#49137);
#13635=VERTEX_POINT('',#49141);
#13636=VERTEX_POINT('',#49142);
#13637=VERTEX_POINT('',#49144);
#13638=VERTEX_POINT('',#49146);
#13639=VERTEX_POINT('',#49148);
#13640=VERTEX_POINT('',#49150);
#13641=VERTEX_POINT('',#49152);
#13642=VERTEX_POINT('',#49154);
#13643=VERTEX_POINT('',#49156);
#13644=VERTEX_POINT('',#49158);
#13645=VERTEX_POINT('',#49160);
#13646=VERTEX_POINT('',#49162);
#13647=VERTEX_POINT('',#49164);
#13648=VERTEX_POINT('',#49166);
#13649=VERTEX_POINT('',#49168);
#13650=VERTEX_POINT('',#49170);
#13651=VERTEX_POINT('',#49172);
#13652=VERTEX_POINT('',#49174);
#13653=VERTEX_POINT('',#49176);
#13654=VERTEX_POINT('',#49178);
#13655=VERTEX_POINT('',#49180);
#13656=VERTEX_POINT('',#49182);
#13657=VERTEX_POINT('',#49184);
#13658=VERTEX_POINT('',#49186);
#13659=VERTEX_POINT('',#49188);
#13660=VERTEX_POINT('',#49190);
#13661=VERTEX_POINT('',#49192);
#13662=VERTEX_POINT('',#49194);
#13663=VERTEX_POINT('',#49196);
#13664=VERTEX_POINT('',#49198);
#13665=VERTEX_POINT('',#49200);
#13666=VERTEX_POINT('',#49202);
#13667=VERTEX_POINT('',#49204);
#13668=VERTEX_POINT('',#49206);
#13669=VERTEX_POINT('',#49208);
#13670=VERTEX_POINT('',#49210);
#13671=VERTEX_POINT('',#49212);
#13672=VERTEX_POINT('',#49214);
#13673=VERTEX_POINT('',#49216);
#13674=VERTEX_POINT('',#49218);
#13675=VERTEX_POINT('',#49221);
#13676=VERTEX_POINT('',#49222);
#13677=VERTEX_POINT('',#49224);
#13678=VERTEX_POINT('',#49232);
#13679=VERTEX_POINT('',#49239);
#13680=VERTEX_POINT('',#49251);
#13681=VERTEX_POINT('',#49258);
#13682=VERTEX_POINT('',#49270);
#13683=VERTEX_POINT('',#49272);
#13684=VERTEX_POINT('',#49274);
#13685=VERTEX_POINT('',#49284);
#13686=VERTEX_POINT('',#49285);
#13687=VERTEX_POINT('',#49287);
#13688=VERTEX_POINT('',#49289);
#13689=VERTEX_POINT('',#49292);
#13690=VERTEX_POINT('',#49294);
#13691=VERTEX_POINT('',#49296);
#13692=VERTEX_POINT('',#49299);
#13693=VERTEX_POINT('',#49300);
#13694=VERTEX_POINT('',#49302);
#13695=VERTEX_POINT('',#49304);
#13696=VERTEX_POINT('',#49323);
#13697=VERTEX_POINT('',#49330);
#13698=VERTEX_POINT('',#49346);
#13699=VERTEX_POINT('',#49353);
#13700=VERTEX_POINT('',#49358);
#13701=VERTEX_POINT('',#49360);
#13702=VERTEX_POINT('',#49384);
#13703=VERTEX_POINT('',#49385);
#13704=VERTEX_POINT('',#49387);
#13705=VERTEX_POINT('',#49397);
#13706=VERTEX_POINT('',#49399);
#13707=VERTEX_POINT('',#49454);
#13708=VERTEX_POINT('',#49458);
#13709=VERTEX_POINT('',#49459);
#13710=VERTEX_POINT('',#49461);
#13711=VERTEX_POINT('',#49463);
#13712=VERTEX_POINT('',#49484);
#13713=VERTEX_POINT('',#49486);
#13714=VERTEX_POINT('',#49523);
#13715=VERTEX_POINT('',#49525);
#13716=VERTEX_POINT('',#49537);
#13717=VERTEX_POINT('',#49541);
#13718=VERTEX_POINT('',#49543);
#13719=VERTEX_POINT('',#49545);
#13720=VERTEX_POINT('',#49623);
#13721=VERTEX_POINT('',#49625);
#13722=VERTEX_POINT('',#49669);
#13723=VERTEX_POINT('',#49671);
#13724=VERTEX_POINT('',#49758);
#13725=VERTEX_POINT('',#49760);
#13726=VERTEX_POINT('',#49821);
#13727=VERTEX_POINT('',#49823);
#13728=VERTEX_POINT('',#49830);
#13729=VERTEX_POINT('',#49843);
#13730=VERTEX_POINT('',#49885);
#13731=VERTEX_POINT('',#49887);
#13732=VERTEX_POINT('',#49950);
#13733=VERTEX_POINT('',#49952);
#13734=VERTEX_POINT('',#49976);
#13735=VERTEX_POINT('',#49978);
#13736=VERTEX_POINT('',#50021);
#13737=VERTEX_POINT('',#50023);
#13738=VERTEX_POINT('',#50025);
#13739=VERTEX_POINT('',#50085);
#13740=VERTEX_POINT('',#50119);
#13741=VERTEX_POINT('',#50121);
#13742=VERTEX_POINT('',#50126);
#13743=VERTEX_POINT('',#50183);
#13744=VERTEX_POINT('',#50185);
#13745=VERTEX_POINT('',#50293);
#13746=VERTEX_POINT('',#50295);
#13747=VERTEX_POINT('',#50370);
#13748=VERTEX_POINT('',#50372);
#13749=VERTEX_POINT('',#50374);
#13750=VERTEX_POINT('',#50403);
#13751=VERTEX_POINT('',#50567);
#13752=VERTEX_POINT('',#50569);
#13753=VERTEX_POINT('',#50636);
#13754=VERTEX_POINT('',#50638);
#13755=VERTEX_POINT('',#50640);
#13756=VERTEX_POINT('',#50783);
#13757=VERTEX_POINT('',#50874);
#13758=VERTEX_POINT('',#50876);
#13759=VERTEX_POINT('',#50878);
#13760=VERTEX_POINT('',#50923);
#13761=VERTEX_POINT('',#50924);
#13762=VERTEX_POINT('',#50926);
#13763=VERTEX_POINT('',#50928);
#13764=VERTEX_POINT('',#50935);
#13765=VERTEX_POINT('',#50939);
#13766=VERTEX_POINT('',#50943);
#13767=VERTEX_POINT('',#50947);
#13768=VERTEX_POINT('',#50951);
#13769=VERTEX_POINT('',#50955);
#13770=VERTEX_POINT('',#50959);
#13771=VERTEX_POINT('',#50963);
#13772=VERTEX_POINT('',#50967);
#13773=VERTEX_POINT('',#50971);
#13774=VERTEX_POINT('',#50975);
#13775=VERTEX_POINT('',#50979);
#13776=VERTEX_POINT('',#50983);
#13777=VERTEX_POINT('',#50987);
#13778=VERTEX_POINT('',#50991);
#13779=VERTEX_POINT('',#50995);
#13780=VERTEX_POINT('',#50999);
#13781=VERTEX_POINT('',#51003);
#13782=VERTEX_POINT('',#51007);
#13783=VERTEX_POINT('',#51011);
#13784=VERTEX_POINT('',#51015);
#13785=VERTEX_POINT('',#51019);
#13786=VERTEX_POINT('',#51023);
#13787=VERTEX_POINT('',#51027);
#13788=VERTEX_POINT('',#51031);
#13789=VERTEX_POINT('',#51035);
#13790=VERTEX_POINT('',#51039);
#13791=VERTEX_POINT('',#51043);
#13792=VERTEX_POINT('',#51047);
#13793=VERTEX_POINT('',#51051);
#13794=VERTEX_POINT('',#51055);
#13795=VERTEX_POINT('',#51059);
#13796=VERTEX_POINT('',#51063);
#13797=VERTEX_POINT('',#51067);
#13798=VERTEX_POINT('',#51071);
#13799=VERTEX_POINT('',#51075);
#13800=VERTEX_POINT('',#51079);
#13801=VERTEX_POINT('',#51083);
#13802=VERTEX_POINT('',#51087);
#13803=VERTEX_POINT('',#51089);
#13804=VERTEX_POINT('',#51095);
#13805=VERTEX_POINT('',#51099);
#13806=VERTEX_POINT('',#51103);
#13807=VERTEX_POINT('',#51107);
#13808=VERTEX_POINT('',#51111);
#13809=VERTEX_POINT('',#51115);
#13810=VERTEX_POINT('',#51119);
#13811=VERTEX_POINT('',#51123);
#13812=VERTEX_POINT('',#51127);
#13813=VERTEX_POINT('',#51131);
#13814=VERTEX_POINT('',#51135);
#13815=VERTEX_POINT('',#51139);
#13816=VERTEX_POINT('',#51143);
#13817=VERTEX_POINT('',#51147);
#13818=VERTEX_POINT('',#51151);
#13819=VERTEX_POINT('',#51155);
#13820=VERTEX_POINT('',#51159);
#13821=VERTEX_POINT('',#51163);
#13822=VERTEX_POINT('',#51167);
#13823=VERTEX_POINT('',#51171);
#13824=VERTEX_POINT('',#51175);
#13825=VERTEX_POINT('',#51179);
#13826=VERTEX_POINT('',#51183);
#13827=VERTEX_POINT('',#51187);
#13828=VERTEX_POINT('',#51191);
#13829=VERTEX_POINT('',#51195);
#13830=VERTEX_POINT('',#51199);
#13831=VERTEX_POINT('',#51203);
#13832=VERTEX_POINT('',#51207);
#13833=VERTEX_POINT('',#51211);
#13834=VERTEX_POINT('',#51215);
#13835=VERTEX_POINT('',#51219);
#13836=VERTEX_POINT('',#51223);
#13837=VERTEX_POINT('',#51227);
#13838=VERTEX_POINT('',#51231);
#13839=VERTEX_POINT('',#51235);
#13840=VERTEX_POINT('',#51243);
#13841=VERTEX_POINT('',#51244);
#13842=VERTEX_POINT('',#51246);
#13843=VERTEX_POINT('',#51248);
#13844=VERTEX_POINT('',#51263);
#13845=VERTEX_POINT('',#51264);
#13846=VERTEX_POINT('',#51266);
#13847=VERTEX_POINT('',#51277);
#13848=VERTEX_POINT('',#51329);
#13849=VERTEX_POINT('',#51330);
#13850=VERTEX_POINT('',#51333);
#13851=VERTEX_POINT('',#51348);
#13852=VERTEX_POINT('',#51355);
#13853=VERTEX_POINT('',#51357);
#13854=VERTEX_POINT('',#51392);
#13855=VERTEX_POINT('',#51457);
#13856=VERTEX_POINT('',#51526);
#13857=VERTEX_POINT('',#51527);
#13858=VERTEX_POINT('',#51529);
#13859=VERTEX_POINT('',#51531);
#13860=VERTEX_POINT('',#51594);
#13861=VERTEX_POINT('',#51595);
#13862=VERTEX_POINT('',#51597);
#13863=VERTEX_POINT('',#51665);
#13864=VERTEX_POINT('',#51691);
#13865=VERTEX_POINT('',#51692);
#13866=VERTEX_POINT('',#51760);
#13867=VERTEX_POINT('',#51818);
#13868=VERTEX_POINT('',#51819);
#13869=VERTEX_POINT('',#51824);
#13870=VERTEX_POINT('',#51826);
#13871=VERTEX_POINT('',#51865);
#13872=VERTEX_POINT('',#51867);
#13873=VERTEX_POINT('',#51954);
#13874=VERTEX_POINT('',#51956);
#13875=VERTEX_POINT('',#52042);
#13876=VERTEX_POINT('',#52081);
#13877=VERTEX_POINT('',#52083);
#13878=VERTEX_POINT('',#52140);
#13879=VERTEX_POINT('',#52288);
#13880=VERTEX_POINT('',#52290);
#13881=VERTEX_POINT('',#52479);
#13882=VERTEX_POINT('',#52560);
#13883=VERTEX_POINT('',#52726);
#13884=VERTEX_POINT('',#52792);
#13885=VERTEX_POINT('',#52942);
#13886=VERTEX_POINT('',#53005);
#13887=VERTEX_POINT('',#53098);
#13888=VERTEX_POINT('',#53236);
#13889=VERTEX_POINT('',#53276);
#13890=VERTEX_POINT('',#53278);
#13891=VERTEX_POINT('',#53328);
#13892=VERTEX_POINT('',#53456);
#13893=VERTEX_POINT('',#53458);
#13894=VERTEX_POINT('',#53575);
#13895=VERTEX_POINT('',#53724);
#13896=VERTEX_POINT('',#53726);
#13897=VERTEX_POINT('',#53838);
#13898=VERTEX_POINT('',#53882);
#13899=VERTEX_POINT('',#54080);
#13900=VERTEX_POINT('',#54106);
#13901=VERTEX_POINT('',#54805);
#13902=VERTEX_POINT('',#54807);
#13903=VERTEX_POINT('',#54811);
#13904=VERTEX_POINT('',#54815);
#13905=VERTEX_POINT('',#54819);
#13906=VERTEX_POINT('',#54823);
#13907=VERTEX_POINT('',#54827);
#13908=VERTEX_POINT('',#54831);
#13909=VERTEX_POINT('',#54835);
#13910=VERTEX_POINT('',#54839);
#13911=VERTEX_POINT('',#54843);
#13912=VERTEX_POINT('',#54847);
#13913=VERTEX_POINT('',#54851);
#13914=VERTEX_POINT('',#54855);
#13915=VERTEX_POINT('',#54859);
#13916=VERTEX_POINT('',#54863);
#13917=VERTEX_POINT('',#54867);
#13918=VERTEX_POINT('',#54871);
#13919=VERTEX_POINT('',#54875);
#13920=VERTEX_POINT('',#54879);
#13921=VERTEX_POINT('',#54883);
#13922=VERTEX_POINT('',#54887);
#13923=VERTEX_POINT('',#54891);
#13924=VERTEX_POINT('',#54895);
#13925=VERTEX_POINT('',#54899);
#13926=VERTEX_POINT('',#54903);
#13927=VERTEX_POINT('',#54907);
#13928=VERTEX_POINT('',#54911);
#13929=VERTEX_POINT('',#54915);
#13930=VERTEX_POINT('',#54919);
#13931=VERTEX_POINT('',#54923);
#13932=VERTEX_POINT('',#54927);
#13933=VERTEX_POINT('',#54931);
#13934=VERTEX_POINT('',#54935);
#13935=VERTEX_POINT('',#54939);
#13936=VERTEX_POINT('',#54943);
#13937=VERTEX_POINT('',#54947);
#13938=VERTEX_POINT('',#54951);
#13939=VERTEX_POINT('',#54955);
#13940=VERTEX_POINT('',#54959);
#13941=VERTEX_POINT('',#54965);
#13942=VERTEX_POINT('',#54967);
#13943=VERTEX_POINT('',#54969);
#13944=VERTEX_POINT('',#54971);
#13945=VERTEX_POINT('',#54973);
#13946=VERTEX_POINT('',#54975);
#13947=VERTEX_POINT('',#54977);
#13948=VERTEX_POINT('',#54979);
#13949=VERTEX_POINT('',#54981);
#13950=VERTEX_POINT('',#54984);
#13951=VERTEX_POINT('',#54986);
#13952=VERTEX_POINT('',#54988);
#13953=VERTEX_POINT('',#54990);
#13954=VERTEX_POINT('',#54992);
#13955=VERTEX_POINT('',#54994);
#13956=VERTEX_POINT('',#54996);
#13957=VERTEX_POINT('',#54998);
#13958=VERTEX_POINT('',#55002);
#13959=VERTEX_POINT('',#55004);
#13960=VERTEX_POINT('',#55008);
#13961=VERTEX_POINT('',#55012);
#13962=VERTEX_POINT('',#55016);
#13963=VERTEX_POINT('',#55020);
#13964=VERTEX_POINT('',#55026);
#13965=VERTEX_POINT('',#55028);
#13966=VERTEX_POINT('',#55034);
#13967=VERTEX_POINT('',#55038);
#13968=VERTEX_POINT('',#55042);
#13969=VERTEX_POINT('',#55046);
#13970=VERTEX_POINT('',#55050);
#13971=VERTEX_POINT('',#55054);
#13972=VERTEX_POINT('',#55058);
#13973=VERTEX_POINT('',#55062);
#13974=VERTEX_POINT('',#55066);
#13975=VERTEX_POINT('',#55083);
#13976=VERTEX_POINT('',#55085);
#13977=VERTEX_POINT('',#55121);
#13978=VERTEX_POINT('',#55134);
#13979=VERTEX_POINT('',#55149);
#13980=VERTEX_POINT('',#55151);
#13981=VERTEX_POINT('',#55205);
#13982=VERTEX_POINT('',#55283);
#13983=VERTEX_POINT('',#55309);
#13984=VERTEX_POINT('',#55363);
#13985=VERTEX_POINT('',#55408);
#13986=VERTEX_POINT('',#55529);
#13987=VERTEX_POINT('',#55629);
#13988=VERTEX_POINT('',#55630);
#13989=VERTEX_POINT('',#55737);
#13990=VERTEX_POINT('',#55739);
#13991=VERTEX_POINT('',#55849);
#13992=VERTEX_POINT('',#55850);
#13993=VERTEX_POINT('',#55931);
#13994=VERTEX_POINT('',#55932);
#13995=VERTEX_POINT('',#56069);
#13996=VERTEX_POINT('',#56119);
#13997=VERTEX_POINT('',#56139);
#13998=VERTEX_POINT('',#56155);
#13999=VERTEX_POINT('',#56159);
#14000=VERTEX_POINT('',#56163);
#14001=VERTEX_POINT('',#56165);
#14002=VERTEX_POINT('',#56190);
#14003=VERTEX_POINT('',#56192);
#14004=VERTEX_POINT('',#56223);
#14005=VERTEX_POINT('',#56225);
#14006=VERTEX_POINT('',#56235);
#14007=VERTEX_POINT('',#56327);
#14008=VERTEX_POINT('',#56331);
#14009=VERTEX_POINT('',#56360);
#14010=VERTEX_POINT('',#56364);
#14011=VERTEX_POINT('',#56424);
#14012=VERTEX_POINT('',#56468);
#14013=VERTEX_POINT('',#56522);
#14014=VERTEX_POINT('',#56579);
#14015=VERTEX_POINT('',#56620);
#14016=VERTEX_POINT('',#56680);
#14017=VERTEX_POINT('',#56745);
#14018=VERTEX_POINT('',#56874);
#14019=VERTEX_POINT('',#56934);
#14020=VERTEX_POINT('',#56994);
#14021=VERTEX_POINT('',#57033);
#14022=VERTEX_POINT('',#57075);
#14023=VERTEX_POINT('',#57146);
#14024=VERTEX_POINT('',#57218);
#14025=VERTEX_POINT('',#57323);
#14026=VERTEX_POINT('',#57582);
#14027=VERTEX_POINT('',#57596);
#14028=VERTEX_POINT('',#57601);
#14029=VERTEX_POINT('',#57666);
#14030=VERTEX_POINT('',#57686);
#14031=VERTEX_POINT('',#57701);
#14032=VERTEX_POINT('',#57716);
#14033=VERTEX_POINT('',#57731);
#14034=VERTEX_POINT('',#57751);
#14035=VERTEX_POINT('',#57766);
#14036=VERTEX_POINT('',#57781);
#14037=VERTEX_POINT('',#57796);
#14038=VERTEX_POINT('',#57811);
#14039=VERTEX_POINT('',#57831);
#14040=VERTEX_POINT('',#57846);
#14041=VERTEX_POINT('',#57863);
#14042=VERTEX_POINT('',#57864);
#14043=VERTEX_POINT('',#57866);
#14044=VERTEX_POINT('',#57868);
#14045=VERTEX_POINT('',#57870);
#14046=VERTEX_POINT('',#57872);
#14047=VERTEX_POINT('',#57874);
#14048=VERTEX_POINT('',#57878);
#14049=VERTEX_POINT('',#57879);
#14050=VERTEX_POINT('',#57884);
#14051=VERTEX_POINT('',#57888);
#14052=VERTEX_POINT('',#57892);
#14053=VERTEX_POINT('',#57896);
#14054=VERTEX_POINT('',#57900);
#14055=VERTEX_POINT('',#57908);
#14056=VERTEX_POINT('',#57909);
#14057=VERTEX_POINT('',#58115);
#14058=VERTEX_POINT('',#58117);
#14059=VERTEX_POINT('',#58308);
#14060=VERTEX_POINT('',#58400);
#14061=VERTEX_POINT('',#58489);
#14062=VERTEX_POINT('',#58557);
#14063=VERTEX_POINT('',#58625);
#14064=VERTEX_POINT('',#58693);
#14065=VERTEX_POINT('',#58761);
#14066=VERTEX_POINT('',#58950);
#14067=VERTEX_POINT('',#58951);
#14068=VERTEX_POINT('',#59016);
#14069=VERTEX_POINT('',#59138);
#14070=VERTEX_POINT('',#59281);
#14071=VERTEX_POINT('',#59283);
#14072=VERTEX_POINT('',#59324);
#14073=VERTEX_POINT('',#59326);
#14074=VERTEX_POINT('',#59382);
#14075=VERTEX_POINT('',#59535);
#14076=VERTEX_POINT('',#59536);
#14077=VERTEX_POINT('',#59538);
#14078=VERTEX_POINT('',#59591);
#14079=VERTEX_POINT('',#59593);
#14080=VERTEX_POINT('',#59634);
#14081=VERTEX_POINT('',#59636);
#14082=VERTEX_POINT('',#59782);
#14083=VERTEX_POINT('',#59910);
#14084=VERTEX_POINT('',#60126);
#14085=VERTEX_POINT('',#60127);
#14086=VERTEX_POINT('',#60192);
#14087=VERTEX_POINT('',#60269);
#14088=VERTEX_POINT('',#60367);
#14089=VERTEX_POINT('',#60369);
#14090=VERTEX_POINT('',#60461);
#14091=VERTEX_POINT('',#60609);
#14092=VERTEX_POINT('',#60610);
#14093=VERTEX_POINT('',#60699);
#14094=VERTEX_POINT('',#60794);
#14095=VERTEX_POINT('',#60862);
#14096=VERTEX_POINT('',#60936);
#14097=VERTEX_POINT('',#61010);
#14098=VERTEX_POINT('',#61078);
#14099=VERTEX_POINT('',#61173);
#14100=VERTEX_POINT('',#61271);
#14101=VERTEX_POINT('',#61447);
#14102=VERTEX_POINT('',#61651);
#14103=VERTEX_POINT('',#61652);
#14104=VERTEX_POINT('',#61801);
#14105=VERTEX_POINT('',#61827);
#14106=VERTEX_POINT('',#61892);
#14107=VERTEX_POINT('',#61894);
#14108=VERTEX_POINT('',#61947);
#14109=VERTEX_POINT('',#61949);
#14110=VERTEX_POINT('',#62089);
#14111=VERTEX_POINT('',#62272);
#14112=VERTEX_POINT('',#62273);
#14113=VERTEX_POINT('',#62422);
#14114=VERTEX_POINT('',#62478);
#14115=VERTEX_POINT('',#62609);
#14116=VERTEX_POINT('',#62761);
#14117=VERTEX_POINT('',#62763);
#14118=VERTEX_POINT('',#62810);
#14119=VERTEX_POINT('',#62812);
#14120=VERTEX_POINT('',#62887);
#14121=VERTEX_POINT('',#62888);
#14122=VERTEX_POINT('',#62950);
#14123=VERTEX_POINT('',#63036);
#14124=VERTEX_POINT('',#63137);
#14125=VERTEX_POINT('',#63139);
#14126=VERTEX_POINT('',#63246);
#14127=VERTEX_POINT('',#63450);
#14128=VERTEX_POINT('',#63452);
#14129=VERTEX_POINT('',#63491);
#14130=VERTEX_POINT('',#63493);
#14131=VERTEX_POINT('',#63607);
#14132=VERTEX_POINT('',#63741);
#14133=VERTEX_POINT('',#63967);
#14134=VERTEX_POINT('',#64078);
#14135=VERTEX_POINT('',#64204);
#14136=VERTEX_POINT('',#64405);
#14137=VERTEX_POINT('',#64615);
#14138=VERTEX_POINT('',#64861);
#14139=VERTEX_POINT('',#64972);
#14140=VERTEX_POINT('',#65029);
#14141=VERTEX_POINT('',#65099);
#14142=VERTEX_POINT('',#65161);
#14143=VERTEX_POINT('',#65186);
#14144=VERTEX_POINT('',#65220);
#14145=VERTEX_POINT('',#65487);
#14146=VERTEX_POINT('',#65494);
#14147=VERTEX_POINT('',#65562);
#14148=VERTEX_POINT('',#65569);
#14149=VERTEX_POINT('',#65673);
#14150=VERTEX_POINT('',#65735);
#14151=VERTEX_POINT('',#65815);
#14152=VERTEX_POINT('',#65926);
#14153=VERTEX_POINT('',#66080);
#14154=VERTEX_POINT('',#66148);
#14155=VERTEX_POINT('',#66340);
#14156=VERTEX_POINT('',#66517);
#14157=VERTEX_POINT('',#66628);
#14158=VERTEX_POINT('',#66685);
#14159=VERTEX_POINT('',#67043);
#14160=VERTEX_POINT('',#67045);
#14161=VERTEX_POINT('',#67143);
#14162=VERTEX_POINT('',#67145);
#14163=VERTEX_POINT('',#67263);
#14164=VERTEX_POINT('',#67371);
#14165=VERTEX_POINT('',#67515);
#14166=VERTEX_POINT('',#67755);
#14167=VERTEX_POINT('',#67878);
#14168=VERTEX_POINT('',#67917);
#14169=VERTEX_POINT('',#67976);
#14170=VERTEX_POINT('',#68068);
#14171=VERTEX_POINT('',#68120);
#14172=VERTEX_POINT('',#68124);
#14173=VERTEX_POINT('',#68183);
#14174=VERTEX_POINT('',#68245);
#14175=VERTEX_POINT('',#68323);
#14176=VERTEX_POINT('',#68380);
#14177=VERTEX_POINT('',#68795);
#14178=VERTEX_POINT('',#68797);
#14179=VERTEX_POINT('',#68883);
#14180=VERTEX_POINT('',#68885);
#14181=VERTEX_POINT('',#69006);
#14182=VERTEX_POINT('',#69068);
#14183=VERTEX_POINT('',#69180);
#14184=VERTEX_POINT('',#69245);
#14185=VERTEX_POINT('',#69320);
#14186=VERTEX_POINT('',#69385);
#14187=VERTEX_POINT('',#69460);
#14188=VERTEX_POINT('',#69522);
#14189=VERTEX_POINT('',#69652);
#14190=VERTEX_POINT('',#69747);
#14191=VERTEX_POINT('',#69903);
#14192=VERTEX_POINT('',#70010);
#14193=VERTEX_POINT('',#70314);
#14194=VERTEX_POINT('',#70535);
#14195=VERTEX_POINT('',#70709);
#14196=VERTEX_POINT('',#70766);
#14197=VERTEX_POINT('',#70962);
#14198=VERTEX_POINT('',#71165);
#14199=VERTEX_POINT('',#71742);
#14200=VERTEX_POINT('',#71743);
#14201=VERTEX_POINT('',#71919);
#14202=VERTEX_POINT('',#71966);
#14203=VERTEX_POINT('',#71968);
#14204=VERTEX_POINT('',#72030);
#14205=VERTEX_POINT('',#72092);
#14206=VERTEX_POINT('',#72094);
#14207=VERTEX_POINT('',#72141);
#14208=VERTEX_POINT('',#72314);
#14209=VERTEX_POINT('',#72395);
#14210=VERTEX_POINT('',#72396);
#14211=VERTEX_POINT('',#72398);
#14212=VERTEX_POINT('',#72439);
#14213=VERTEX_POINT('',#72483);
#14214=VERTEX_POINT('',#72560);
#14215=VERTEX_POINT('',#72607);
#14216=VERTEX_POINT('',#72645);
#14217=VERTEX_POINT('',#72647);
#14218=VERTEX_POINT('',#72776);
#14219=VERTEX_POINT('',#72778);
#14220=VERTEX_POINT('',#72781);
#14221=VERTEX_POINT('',#72782);
#14222=VERTEX_POINT('',#72789);
#14223=VERTEX_POINT('',#72805);
#14224=VERTEX_POINT('',#72812);
#14225=VERTEX_POINT('',#72819);
#14226=VERTEX_POINT('',#72835);
#14227=VERTEX_POINT('',#72842);
#14228=VERTEX_POINT('',#72844);
#14229=VERTEX_POINT('',#72851);
#14230=VERTEX_POINT('',#72859);
#14231=VERTEX_POINT('',#72861);
#14232=VERTEX_POINT('',#72863);
#14233=VERTEX_POINT('',#72864);
#14234=VERTEX_POINT('',#72871);
#14235=VERTEX_POINT('',#72873);
#14236=VERTEX_POINT('',#72880);
#14237=VERTEX_POINT('',#72887);
#14238=VERTEX_POINT('',#72889);
#14239=VERTEX_POINT('',#72896);
#14240=VERTEX_POINT('',#72903);
#14241=VERTEX_POINT('',#72917);
#14242=VERTEX_POINT('',#72923);
#14243=VERTEX_POINT('',#72982);
#14244=VERTEX_POINT('',#72984);
#14245=VERTEX_POINT('',#73007);
#14246=VERTEX_POINT('',#73066);
#14247=VERTEX_POINT('',#73141);
#14248=VERTEX_POINT('',#73215);
#14249=VERTEX_POINT('',#73274);
#14250=VERTEX_POINT('',#73349);
#14251=VERTEX_POINT('',#73424);
#14252=VERTEX_POINT('',#73617);
#14253=VERTEX_POINT('',#73619);
#14254=VERTEX_POINT('',#73731);
#14255=VERTEX_POINT('',#73833);
#14256=VERTEX_POINT('',#73908);
#14257=VERTEX_POINT('',#74019);
#14258=VERTEX_POINT('',#74121);
#14259=VERTEX_POINT('',#74143);
#14260=VERTEX_POINT('',#74202);
#14261=VERTEX_POINT('',#74277);
#14262=VERTEX_POINT('',#74303);
#14263=VERTEX_POINT('',#74304);
#14264=VERTEX_POINT('',#74309);
#14265=VERTEX_POINT('',#74313);
#14266=VERTEX_POINT('',#74315);
#14267=VERTEX_POINT('',#74319);
#14268=VERTEX_POINT('',#74336);
#14269=VERTEX_POINT('',#74337);
#14270=VERTEX_POINT('',#74342);
#14271=VERTEX_POINT('',#74346);
#14272=VERTEX_POINT('',#74348);
#14273=VERTEX_POINT('',#74352);
#14274=VERTEX_POINT('',#74369);
#14275=VERTEX_POINT('',#74370);
#14276=VERTEX_POINT('',#74372);
#14277=VERTEX_POINT('',#74374);
#14278=VERTEX_POINT('',#74376);
#14279=VERTEX_POINT('',#74380);
#14280=VERTEX_POINT('',#74381);
#14281=VERTEX_POINT('',#74383);
#14282=VERTEX_POINT('',#74385);
#14283=VERTEX_POINT('',#74389);
#14284=VERTEX_POINT('',#74390);
#14285=VERTEX_POINT('',#74392);
#14286=VERTEX_POINT('',#74394);
#14287=VERTEX_POINT('',#74396);
#14288=VERTEX_POINT('',#74400);
#14289=VERTEX_POINT('',#74401);
#14290=VERTEX_POINT('',#74403);
#14291=VERTEX_POINT('',#74409);
#14292=VERTEX_POINT('',#74411);
#14293=VERTEX_POINT('',#74413);
#14294=VERTEX_POINT('',#74415);
#14295=VERTEX_POINT('',#74421);
#14296=VERTEX_POINT('',#74423);
#14297=VERTEX_POINT('',#74425);
#14298=VERTEX_POINT('',#74427);
#14299=VERTEX_POINT('',#74433);
#14300=VERTEX_POINT('',#74435);
#14301=VERTEX_POINT('',#74437);
#14302=VERTEX_POINT('',#74439);
#14303=VERTEX_POINT('',#74445);
#14304=VERTEX_POINT('',#74448);
#14305=VERTEX_POINT('',#74449);
#14306=VERTEX_POINT('',#74451);
#14307=VERTEX_POINT('',#74453);
#14308=VERTEX_POINT('',#74455);
#14309=VERTEX_POINT('',#74457);
#14310=VERTEX_POINT('',#74460);
#14311=VERTEX_POINT('',#74461);
#14312=VERTEX_POINT('',#74463);
#14313=VERTEX_POINT('',#74465);
#14314=VERTEX_POINT('',#74467);
#14315=VERTEX_POINT('',#74469);
#14316=VERTEX_POINT('',#74471);
#14317=VERTEX_POINT('',#74474);
#14318=VERTEX_POINT('',#74475);
#14319=VERTEX_POINT('',#74477);
#14320=VERTEX_POINT('',#74479);
#14321=VERTEX_POINT('',#74481);
#14322=VERTEX_POINT('',#74485);
#14323=VERTEX_POINT('',#74486);
#14324=VERTEX_POINT('',#74488);
#14325=VERTEX_POINT('',#74490);
#14326=VERTEX_POINT('',#74492);
#14327=VERTEX_POINT('',#74494);
#14328=VERTEX_POINT('',#74496);
#14329=VERTEX_POINT('',#74499);
#14330=VERTEX_POINT('',#74500);
#14331=VERTEX_POINT('',#74502);
#14332=VERTEX_POINT('',#74504);
#14333=VERTEX_POINT('',#74506);
#14334=VERTEX_POINT('',#74508);
#14335=VERTEX_POINT('',#74510);
#14336=VERTEX_POINT('',#74512);
#14337=VERTEX_POINT('',#74516);
#14338=VERTEX_POINT('',#74517);
#14339=VERTEX_POINT('',#74519);
#14340=VERTEX_POINT('',#74521);
#14341=VERTEX_POINT('',#74523);
#14342=VERTEX_POINT('',#74525);
#14343=VERTEX_POINT('',#74527);
#14344=VERTEX_POINT('',#74531);
#14345=VERTEX_POINT('',#74535);
#14346=VERTEX_POINT('',#74539);
#14347=VERTEX_POINT('',#74541);
#14348=VERTEX_POINT('',#74543);
#14349=VERTEX_POINT('',#74550);
#14350=VERTEX_POINT('',#74552);
#14351=VERTEX_POINT('',#74556);
#14352=VERTEX_POINT('',#74560);
#14353=VERTEX_POINT('',#74561);
#14354=VERTEX_POINT('',#74563);
#14355=VERTEX_POINT('',#74565);
#14356=VERTEX_POINT('',#74567);
#14357=VERTEX_POINT('',#74569);
#14358=VERTEX_POINT('',#74571);
#14359=VERTEX_POINT('',#74573);
#14360=VERTEX_POINT('',#74575);
#14361=VERTEX_POINT('',#74577);
#14362=VERTEX_POINT('',#74579);
#14363=VERTEX_POINT('',#74581);
#14364=VERTEX_POINT('',#74583);
#14365=VERTEX_POINT('',#74585);
#14366=VERTEX_POINT('',#74587);
#14367=VERTEX_POINT('',#74590);
#14368=VERTEX_POINT('',#74592);
#14369=VERTEX_POINT('',#74594);
#14370=VERTEX_POINT('',#74598);
#14371=VERTEX_POINT('',#74611);
#14372=VERTEX_POINT('',#74619);
#14373=VERTEX_POINT('',#74623);
#14374=VERTEX_POINT('',#74625);
#14375=VERTEX_POINT('',#74627);
#14376=VERTEX_POINT('',#74629);
#14377=VERTEX_POINT('',#74640);
#14378=VERTEX_POINT('',#74642);
#14379=VERTEX_POINT('',#74653);
#14380=VERTEX_POINT('',#74657);
#14381=VERTEX_POINT('',#74670);
#14382=VERTEX_POINT('',#74678);
#14383=VERTEX_POINT('',#74682);
#14384=VERTEX_POINT('',#74683);
#14385=VERTEX_POINT('',#74685);
#14386=VERTEX_POINT('',#74687);
#14387=VERTEX_POINT('',#74689);
#14388=VERTEX_POINT('',#74691);
#14389=VERTEX_POINT('',#74693);
#14390=VERTEX_POINT('',#74695);
#14391=VERTEX_POINT('',#74697);
#14392=VERTEX_POINT('',#74699);
#14393=VERTEX_POINT('',#74701);
#14394=VERTEX_POINT('',#74703);
#14395=VERTEX_POINT('',#74705);
#14396=VERTEX_POINT('',#74707);
#14397=VERTEX_POINT('',#74710);
#14398=VERTEX_POINT('',#74712);
#14399=VERTEX_POINT('',#74714);
#14400=VERTEX_POINT('',#74718);
#14401=VERTEX_POINT('',#74731);
#14402=VERTEX_POINT('',#74739);
#14403=VERTEX_POINT('',#74743);
#14404=VERTEX_POINT('',#74745);
#14405=VERTEX_POINT('',#74747);
#14406=VERTEX_POINT('',#74749);
#14407=VERTEX_POINT('',#74760);
#14408=VERTEX_POINT('',#74762);
#14409=VERTEX_POINT('',#74773);
#14410=VERTEX_POINT('',#74777);
#14411=VERTEX_POINT('',#74790);
#14412=VERTEX_POINT('',#74800);
#14413=VERTEX_POINT('',#74802);
#14414=VERTEX_POINT('',#74804);
#14415=VERTEX_POINT('',#74806);
#14416=VERTEX_POINT('',#74810);
#14417=VERTEX_POINT('',#74812);
#14418=VERTEX_POINT('',#74816);
#14419=VERTEX_POINT('',#74818);
#14420=VERTEX_POINT('',#74820);
#14421=VERTEX_POINT('',#74822);
#14422=VERTEX_POINT('',#74826);
#14423=VERTEX_POINT('',#74830);
#14424=VERTEX_POINT('',#74831);
#14425=VERTEX_POINT('',#74833);
#14426=VERTEX_POINT('',#74835);
#14427=VERTEX_POINT('',#74840);
#14428=VERTEX_POINT('',#74844);
#14429=VERTEX_POINT('',#74846);
#14430=VERTEX_POINT('',#74848);
#14431=VERTEX_POINT('',#74852);
#14432=VERTEX_POINT('',#74854);
#14433=VERTEX_POINT('',#74858);
#14434=VERTEX_POINT('',#74862);
#14435=VERTEX_POINT('',#74864);
#14436=VERTEX_POINT('',#74868);
#14437=VERTEX_POINT('',#74872);
#14438=VERTEX_POINT('',#74874);
#14439=VERTEX_POINT('',#74880);
#14440=VERTEX_POINT('',#74890);
#14441=VERTEX_POINT('',#74892);
#14442=VERTEX_POINT('',#74896);
#14443=VERTEX_POINT('',#74900);
#14444=VERTEX_POINT('',#74902);
#14445=VERTEX_POINT('',#74906);
#14446=VERTEX_POINT('',#74908);
#14447=VERTEX_POINT('',#74912);
#14448=VERTEX_POINT('',#74916);
#14449=VERTEX_POINT('',#74920);
#14450=VERTEX_POINT('',#74922);
#14451=VERTEX_POINT('',#74925);
#14452=VERTEX_POINT('',#74927);
#14453=VERTEX_POINT('',#74931);
#14454=VERTEX_POINT('',#74935);
#14455=VERTEX_POINT('',#74939);
#14456=VERTEX_POINT('',#74943);
#14457=VERTEX_POINT('',#74947);
#14458=VERTEX_POINT('',#74951);
#14459=VERTEX_POINT('',#74955);
#14460=VERTEX_POINT('',#74959);
#14461=VERTEX_POINT('',#74965);
#14462=VERTEX_POINT('',#74967);
#14463=VERTEX_POINT('',#74971);
#14464=VERTEX_POINT('',#74975);
#14465=VERTEX_POINT('',#74977);
#14466=VERTEX_POINT('',#74981);
#14467=VERTEX_POINT('',#74983);
#14468=VERTEX_POINT('',#74987);
#14469=VERTEX_POINT('',#74991);
#14470=VERTEX_POINT('',#74995);
#14471=VERTEX_POINT('',#74996);
#14472=VERTEX_POINT('',#74998);
#14473=VERTEX_POINT('',#75002);
#14474=VERTEX_POINT('',#75004);
#14475=VERTEX_POINT('',#75011);
#14476=VERTEX_POINT('',#75015);
#14477=VERTEX_POINT('',#75016);
#14478=VERTEX_POINT('',#75018);
#14479=VERTEX_POINT('',#75020);
#14480=VERTEX_POINT('',#75023);
#14481=VERTEX_POINT('',#75025);
#14482=VERTEX_POINT('',#75029);
#14483=VERTEX_POINT('',#75033);
#14484=VERTEX_POINT('',#75034);
#14485=VERTEX_POINT('',#75036);
#14486=VERTEX_POINT('',#75039);
#14487=VERTEX_POINT('',#75041);
#14488=VERTEX_POINT('',#75045);
#14489=VERTEX_POINT('',#75053);
#14490=VERTEX_POINT('',#75059);
#14491=VERTEX_POINT('',#75063);
#14492=VERTEX_POINT('',#75065);
#14493=VERTEX_POINT('',#75067);
#14494=VERTEX_POINT('',#75069);
#14495=VERTEX_POINT('',#75071);
#14496=VERTEX_POINT('',#75073);
#14497=VERTEX_POINT('',#75077);
#14498=VERTEX_POINT('',#75081);
#14499=VERTEX_POINT('',#75083);
#14500=VERTEX_POINT('',#75085);
#14501=VERTEX_POINT('',#75087);
#14502=VERTEX_POINT('',#75089);
#14503=VERTEX_POINT('',#75093);
#14504=VERTEX_POINT('',#75095);
#14505=VERTEX_POINT('',#75121);
#14506=VERTEX_POINT('',#75130);
#14507=VERTEX_POINT('',#75137);
#14508=VERTEX_POINT('',#75145);
#14509=VERTEX_POINT('',#75155);
#14510=VERTEX_POINT('',#75162);
#14511=VERTEX_POINT('',#75172);
#14512=VERTEX_POINT('',#75184);
#14513=VERTEX_POINT('',#75191);
#14514=VERTEX_POINT('',#75195);
#14515=VERTEX_POINT('',#75196);
#14516=VERTEX_POINT('',#75198);
#14517=VERTEX_POINT('',#75200);
#14518=VERTEX_POINT('',#75202);
#14519=VERTEX_POINT('',#75204);
#14520=VERTEX_POINT('',#75206);
#14521=VERTEX_POINT('',#75208);
#14522=VERTEX_POINT('',#75210);
#14523=VERTEX_POINT('',#75213);
#14524=VERTEX_POINT('',#75215);
#14525=VERTEX_POINT('',#75220);
#14526=VERTEX_POINT('',#75225);
#14527=VERTEX_POINT('',#75229);
#14528=VERTEX_POINT('',#75242);
#14529=VERTEX_POINT('',#75256);
#14530=VERTEX_POINT('',#75257);
#14531=VERTEX_POINT('',#75262);
#14532=VERTEX_POINT('',#75263);
#14533=VERTEX_POINT('',#75265);
#14534=VERTEX_POINT('',#75267);
#14535=VERTEX_POINT('',#75271);
#14536=VERTEX_POINT('',#75272);
#14537=VERTEX_POINT('',#75274);
#14538=VERTEX_POINT('',#75276);
#14539=VERTEX_POINT('',#75280);
#14540=VERTEX_POINT('',#75281);
#14541=VERTEX_POINT('',#75283);
#14542=VERTEX_POINT('',#75285);
#14543=VERTEX_POINT('',#75289);
#14544=VERTEX_POINT('',#75290);
#14545=VERTEX_POINT('',#75292);
#14546=VERTEX_POINT('',#75294);
#14547=VERTEX_POINT('',#75298);
#14548=VERTEX_POINT('',#75299);
#14549=VERTEX_POINT('',#75310);
#14550=VERTEX_POINT('',#75311);
#14551=VERTEX_POINT('',#75313);
#14552=VERTEX_POINT('',#75323);
#14553=VERTEX_POINT('',#75325);
#14554=VERTEX_POINT('',#75329);
#14555=VERTEX_POINT('',#75330);
#14556=VERTEX_POINT('',#75332);
#14557=VERTEX_POINT('',#75334);
#14558=VERTEX_POINT('',#75336);
#14559=VERTEX_POINT('',#75365);
#14560=VERTEX_POINT('',#75369);
#14561=VERTEX_POINT('',#75370);
#14562=VERTEX_POINT('',#75373);
#14563=VERTEX_POINT('',#75375);
#14564=VERTEX_POINT('',#75377);
#14565=VERTEX_POINT('',#75379);
#14566=VERTEX_POINT('',#75381);
#14567=VERTEX_POINT('',#75384);
#14568=VERTEX_POINT('',#75386);
#14569=VERTEX_POINT('',#75388);
#14570=VERTEX_POINT('',#75390);
#14571=VERTEX_POINT('',#75392);
#14572=VERTEX_POINT('',#75395);
#14573=VERTEX_POINT('',#75397);
#14574=VERTEX_POINT('',#75399);
#14575=VERTEX_POINT('',#75401);
#14576=VERTEX_POINT('',#75414);
#14577=VERTEX_POINT('',#75440);
#14578=VERTEX_POINT('',#75444);
#14579=VERTEX_POINT('',#75446);
#14580=VERTEX_POINT('',#75450);
#14581=VERTEX_POINT('',#75452);
#14582=VERTEX_POINT('',#75456);
#14583=VERTEX_POINT('',#75457);
#14584=VERTEX_POINT('',#75459);
#14585=VERTEX_POINT('',#75461);
#14586=VERTEX_POINT('',#75465);
#14587=VERTEX_POINT('',#75466);
#14588=VERTEX_POINT('',#75468);
#14589=VERTEX_POINT('',#75470);
#14590=VERTEX_POINT('',#75474);
#14591=VERTEX_POINT('',#75475);
#14592=VERTEX_POINT('',#75491);
#14593=VERTEX_POINT('',#75493);
#14594=VERTEX_POINT('',#75495);
#14595=VERTEX_POINT('',#75507);
#14596=VERTEX_POINT('',#75508);
#14597=VERTEX_POINT('',#75511);
#14598=VERTEX_POINT('',#75513);
#14599=VERTEX_POINT('',#75544);
#14600=VERTEX_POINT('',#75546);
#14601=VERTEX_POINT('',#75548);
#14602=VERTEX_POINT('',#75550);
#14603=VERTEX_POINT('',#75552);
#14604=VERTEX_POINT('',#75555);
#14605=VERTEX_POINT('',#75557);
#14606=VERTEX_POINT('',#75570);
#14607=VERTEX_POINT('',#75583);
#14608=VERTEX_POINT('',#75596);
#14609=VERTEX_POINT('',#75598);
#14610=VERTEX_POINT('',#75601);
#14611=VERTEX_POINT('',#75603);
#14612=VERTEX_POINT('',#75605);
#14613=VERTEX_POINT('',#75607);
#14614=VERTEX_POINT('',#75609);
#14615=VERTEX_POINT('',#75613);
#14616=VERTEX_POINT('',#75616);
#14617=VERTEX_POINT('',#75618);
#14618=VERTEX_POINT('',#75622);
#14619=VERTEX_POINT('',#75626);
#14620=VERTEX_POINT('',#75630);
#14621=VERTEX_POINT('',#75634);
#14622=VERTEX_POINT('',#75638);
#14623=VERTEX_POINT('',#75642);
#14624=VERTEX_POINT('',#75646);
#14625=VERTEX_POINT('',#75652);
#14626=VERTEX_POINT('',#75656);
#14627=VERTEX_POINT('',#75660);
#14628=VERTEX_POINT('',#75663);
#14629=VERTEX_POINT('',#75664);
#14630=VERTEX_POINT('',#75669);
#14631=VERTEX_POINT('',#75696);
#14632=VERTEX_POINT('',#75734);
#14633=VERTEX_POINT('',#75772);
#14634=VERTEX_POINT('',#75804);
#14635=VERTEX_POINT('',#75806);
#14636=VERTEX_POINT('',#75854);
#14637=VERTEX_POINT('',#75855);
#14638=VERTEX_POINT('',#75868);
#14639=VERTEX_POINT('',#75872);
#14640=VERTEX_POINT('',#75873);
#14641=VERTEX_POINT('',#75895);
#14642=VERTEX_POINT('',#75924);
#14643=VERTEX_POINT('',#75926);
#14644=VERTEX_POINT('',#75980);
#14645=VERTEX_POINT('',#75982);
#14646=VERTEX_POINT('',#76020);
#14647=VERTEX_POINT('',#76058);
#14648=VERTEX_POINT('',#76073);
#14649=VERTEX_POINT('',#76077);
#14650=VERTEX_POINT('',#76081);
#14651=VERTEX_POINT('',#76085);
#14652=VERTEX_POINT('',#76087);
#14653=VERTEX_POINT('',#76089);
#14654=VERTEX_POINT('',#76091);
#14655=VERTEX_POINT('',#76095);
#14656=VERTEX_POINT('',#76098);
#14657=VERTEX_POINT('',#76101);
#14658=VERTEX_POINT('',#76106);
#14659=VERTEX_POINT('',#76108);
#14660=VERTEX_POINT('',#76112);
#14661=VERTEX_POINT('',#76114);
#14662=VERTEX_POINT('',#76121);
#14663=VERTEX_POINT('',#76125);
#14664=VERTEX_POINT('',#76127);
#14665=VERTEX_POINT('',#76131);
#14666=VERTEX_POINT('',#76133);
#14667=VERTEX_POINT('',#76137);
#14668=VERTEX_POINT('',#76139);
#14669=VERTEX_POINT('',#76143);
#14670=VERTEX_POINT('',#76145);
#14671=VERTEX_POINT('',#76147);
#14672=VERTEX_POINT('',#76149);
#14673=VERTEX_POINT('',#76151);
#14674=VERTEX_POINT('',#76153);
#14675=VERTEX_POINT('',#76155);
#14676=VERTEX_POINT('',#76159);
#14677=VERTEX_POINT('',#76160);
#14678=VERTEX_POINT('',#76163);
#14679=VERTEX_POINT('',#76165);
#14680=VERTEX_POINT('',#76167);
#14681=VERTEX_POINT('',#76169);
#14682=VERTEX_POINT('',#76171);
#14683=VERTEX_POINT('',#76176);
#14684=VERTEX_POINT('',#76177);
#14685=VERTEX_POINT('',#76179);
#14686=VERTEX_POINT('',#76181);
#14687=VERTEX_POINT('',#76185);
#14688=VERTEX_POINT('',#76186);
#14689=VERTEX_POINT('',#76220);
#14690=VERTEX_POINT('',#76236);
#14691=VERTEX_POINT('',#76271);
#14692=VERTEX_POINT('',#76272);
#14693=VERTEX_POINT('',#76328);
#14694=VERTEX_POINT('',#76347);
#14695=VERTEX_POINT('',#76368);
#14696=VERTEX_POINT('',#76370);
#14697=VERTEX_POINT('',#76409);
#14698=VERTEX_POINT('',#76410);
#14699=VERTEX_POINT('',#76466);
#14700=VERTEX_POINT('',#76476);
#14701=VERTEX_POINT('',#76517);
#14702=VERTEX_POINT('',#76518);
#14703=VERTEX_POINT('',#76551);
#14704=VERTEX_POINT('',#76552);
#14705=VERTEX_POINT('',#76560);
#14706=VERTEX_POINT('',#76564);
#14707=VERTEX_POINT('',#76571);
#14708=VERTEX_POINT('',#76573);
#14709=VERTEX_POINT('',#76600);
#14710=VERTEX_POINT('',#76601);
#14711=VERTEX_POINT('',#76608);
#14712=VERTEX_POINT('',#76618);
#14713=VERTEX_POINT('',#76632);
#14714=VERTEX_POINT('',#76634);
#14715=VERTEX_POINT('',#76678);
#14716=VERTEX_POINT('',#76680);
#14717=VERTEX_POINT('',#76689);
#14718=VERTEX_POINT('',#76691);
#14719=VERTEX_POINT('',#76705);
#14720=VERTEX_POINT('',#76712);
#14721=VERTEX_POINT('',#76720);
#14722=VERTEX_POINT('',#76727);
#14723=VERTEX_POINT('',#76734);
#14724=VERTEX_POINT('',#76750);
#14725=VERTEX_POINT('',#76775);
#14726=VERTEX_POINT('',#76782);
#14727=VERTEX_POINT('',#76784);
#14728=VERTEX_POINT('',#76786);
#14729=VERTEX_POINT('',#76806);
#14730=VERTEX_POINT('',#76808);
#14731=VERTEX_POINT('',#76810);
#14732=VERTEX_POINT('',#76812);
#14733=VERTEX_POINT('',#76821);
#14734=VERTEX_POINT('',#76834);
#14735=VERTEX_POINT('',#76837);
#14736=VERTEX_POINT('',#76842);
#14737=VERTEX_POINT('',#76852);
#14738=VERTEX_POINT('',#76854);
#14739=VERTEX_POINT('',#76861);
#14740=VERTEX_POINT('',#76877);
#14741=VERTEX_POINT('',#76891);
#14742=VERTEX_POINT('',#76892);
#14743=VERTEX_POINT('',#76908);
#14744=VERTEX_POINT('',#76915);
#14745=VERTEX_POINT('',#76917);
#14746=VERTEX_POINT('',#76919);
#14747=VERTEX_POINT('',#76921);
#14748=VERTEX_POINT('',#76923);
#14749=VERTEX_POINT('',#76925);
#14750=VERTEX_POINT('',#76950);
#14751=VERTEX_POINT('',#76951);
#14752=VERTEX_POINT('',#76961);
#14753=VERTEX_POINT('',#76979);
#14754=VERTEX_POINT('',#76981);
#14755=VERTEX_POINT('',#76994);
#14756=VERTEX_POINT('',#77009);
#14757=VERTEX_POINT('',#77012);
#14758=VERTEX_POINT('',#77013);
#14759=VERTEX_POINT('',#77015);
#14760=VERTEX_POINT('',#77017);
#14761=VERTEX_POINT('',#77019);
#14762=VERTEX_POINT('',#77021);
#14763=VERTEX_POINT('',#77023);
#14764=VERTEX_POINT('',#77030);
#14765=VERTEX_POINT('',#77046);
#14766=VERTEX_POINT('',#77072);
#14767=VERTEX_POINT('',#77113);
#14768=VERTEX_POINT('',#77134);
#14769=VERTEX_POINT('',#77135);
#14770=VERTEX_POINT('',#77153);
#14771=VERTEX_POINT('',#77163);
#14772=VERTEX_POINT('',#77165);
#14773=VERTEX_POINT('',#77167);
#14774=VERTEX_POINT('',#77182);
#14775=VERTEX_POINT('',#77196);
#14776=VERTEX_POINT('',#77278);
#14777=VERTEX_POINT('',#77280);
#14778=VERTEX_POINT('',#77295);
#14779=VERTEX_POINT('',#77316);
#14780=VERTEX_POINT('',#77339);
#14781=VERTEX_POINT('',#77377);
#14782=VERTEX_POINT('',#77406);
#14783=VERTEX_POINT('',#77444);
#14784=VERTEX_POINT('',#77462);
#14785=VERTEX_POINT('',#77466);
#14786=VERTEX_POINT('',#77501);
#14787=VERTEX_POINT('',#77502);
#14788=VERTEX_POINT('',#77538);
#14789=VERTEX_POINT('',#77539);
#14790=VERTEX_POINT('',#77552);
#14791=VERTEX_POINT('',#77556);
#14792=VERTEX_POINT('',#77562);
#14793=VERTEX_POINT('',#77589);
#14794=VERTEX_POINT('',#77615);
#14795=VERTEX_POINT('',#77653);
#14796=VERTEX_POINT('',#77718);
#14797=VERTEX_POINT('',#77720);
#14798=VERTEX_POINT('',#77749);
#14799=VERTEX_POINT('',#77758);
#14800=VERTEX_POINT('',#77762);
#14801=VERTEX_POINT('',#77766);
#14802=VERTEX_POINT('',#77770);
#14803=VERTEX_POINT('',#77774);
#14804=VERTEX_POINT('',#77807);
#14805=VERTEX_POINT('',#77966);
#14806=VERTEX_POINT('',#77967);
#14807=VERTEX_POINT('',#77972);
#14808=VERTEX_POINT('',#77976);
#14809=VERTEX_POINT('',#77980);
#14810=VERTEX_POINT('',#77984);
#14811=VERTEX_POINT('',#77999);
#14812=VERTEX_POINT('',#78037);
#14813=VERTEX_POINT('',#78072);
#14814=VERTEX_POINT('',#78139);
#14815=VERTEX_POINT('',#78141);
#14816=VERTEX_POINT('',#78143);
#14817=VERTEX_POINT('',#78147);
#14818=VERTEX_POINT('',#78149);
#14819=VERTEX_POINT('',#78151);
#14820=VERTEX_POINT('',#78153);
#14821=VERTEX_POINT('',#78157);
#14822=VERTEX_POINT('',#78159);
#14823=VERTEX_POINT('',#78161);
#14824=VERTEX_POINT('',#78163);
#14825=VERTEX_POINT('',#78167);
#14826=VERTEX_POINT('',#78169);
#14827=VERTEX_POINT('',#78171);
#14828=VERTEX_POINT('',#78175);
#14829=VERTEX_POINT('',#78177);
#14830=VERTEX_POINT('',#78179);
#14831=VERTEX_POINT('',#78183);
#14832=VERTEX_POINT('',#78185);
#14833=VERTEX_POINT('',#78187);
#14834=VERTEX_POINT('',#78189);
#14835=VERTEX_POINT('',#78193);
#14836=VERTEX_POINT('',#78195);
#14837=VERTEX_POINT('',#78197);
#14838=VERTEX_POINT('',#78199);
#14839=VERTEX_POINT('',#78203);
#14840=VERTEX_POINT('',#78205);
#14841=VERTEX_POINT('',#78207);
#14842=VERTEX_POINT('',#78213);
#14843=VERTEX_POINT('',#78217);
#14844=VERTEX_POINT('',#78219);
#14845=VERTEX_POINT('',#78224);
#14846=VERTEX_POINT('',#78226);
#14847=VERTEX_POINT('',#78229);
#14848=VERTEX_POINT('',#78231);
#14849=VERTEX_POINT('',#78234);
#14850=VERTEX_POINT('',#78237);
#14851=VERTEX_POINT('',#78240);
#14852=VERTEX_POINT('',#78242);
#14853=VERTEX_POINT('',#78248);
#14854=VERTEX_POINT('',#78252);
#14855=VERTEX_POINT('',#78254);
#14856=VERTEX_POINT('',#78262);
#14857=VERTEX_POINT('',#78268);
#14858=VERTEX_POINT('',#78276);
#14859=VERTEX_POINT('',#78278);
#14860=VERTEX_POINT('',#78280);
#14861=VERTEX_POINT('',#78282);
#14862=VERTEX_POINT('',#78284);
#14863=VERTEX_POINT('',#78286);
#14864=VERTEX_POINT('',#78288);
#14865=VERTEX_POINT('',#78292);
#14866=VERTEX_POINT('',#78301);
#14867=VERTEX_POINT('',#78305);
#14868=VERTEX_POINT('',#78333);
#14869=VERTEX_POINT('',#78335);
#14870=VERTEX_POINT('',#78339);
#14871=VERTEX_POINT('',#78341);
#14872=VERTEX_POINT('',#78349);
#14873=VERTEX_POINT('',#78355);
#14874=VERTEX_POINT('',#78359);
#14875=VERTEX_POINT('',#78365);
#14876=VERTEX_POINT('',#78367);
#14877=VERTEX_POINT('',#78369);
#14878=VERTEX_POINT('',#78371);
#14879=VERTEX_POINT('',#78373);
#14880=VERTEX_POINT('',#78375);
#14881=VERTEX_POINT('',#78377);
#14882=VERTEX_POINT('',#78381);
#14883=VERTEX_POINT('',#78385);
#14884=VERTEX_POINT('',#78389);
#14885=VERTEX_POINT('',#78393);
#14886=VERTEX_POINT('',#78397);
#14887=VERTEX_POINT('',#78401);
#14888=VERTEX_POINT('',#78405);
#14889=VERTEX_POINT('',#78414);
#14890=VERTEX_POINT('',#78438);
#14891=VERTEX_POINT('',#78440);
#14892=VERTEX_POINT('',#78448);
#14893=VERTEX_POINT('',#78454);
#14894=VERTEX_POINT('',#78462);
#14895=VERTEX_POINT('',#78464);
#14896=VERTEX_POINT('',#78466);
#14897=VERTEX_POINT('',#78468);
#14898=VERTEX_POINT('',#78470);
#14899=VERTEX_POINT('',#78472);
#14900=VERTEX_POINT('',#78474);
#14901=VERTEX_POINT('',#78478);
#14902=VERTEX_POINT('',#78487);
#14903=VERTEX_POINT('',#78491);
#14904=VERTEX_POINT('',#78519);
#14905=VERTEX_POINT('',#78521);
#14906=VERTEX_POINT('',#78525);
#14907=VERTEX_POINT('',#78527);
#14908=VERTEX_POINT('',#78531);
#14909=VERTEX_POINT('',#78541);
#14910=VERTEX_POINT('',#78543);
#14911=VERTEX_POINT('',#78545);
#14912=VERTEX_POINT('',#78547);
#14913=VERTEX_POINT('',#78549);
#14914=VERTEX_POINT('',#78551);
#14915=VERTEX_POINT('',#78553);
#14916=VERTEX_POINT('',#78555);
#14917=VERTEX_POINT('',#78559);
#14918=VERTEX_POINT('',#78563);
#14919=VERTEX_POINT('',#78569);
#14920=VERTEX_POINT('',#78573);
#14921=VERTEX_POINT('',#78575);
#14922=VERTEX_POINT('',#78579);
#14923=VERTEX_POINT('',#78583);
#14924=VERTEX_POINT('',#78589);
#14925=VERTEX_POINT('',#78598);
#14926=VERTEX_POINT('',#78625);
#14927=VERTEX_POINT('',#78626);
#14928=VERTEX_POINT('',#78633);
#14929=VERTEX_POINT('',#78635);
#14930=VERTEX_POINT('',#78637);
#14931=VERTEX_POINT('',#78639);
#14932=VERTEX_POINT('',#78648);
#14933=VERTEX_POINT('',#78649);
#14934=VERTEX_POINT('',#78651);
#14935=VERTEX_POINT('',#78653);
#14936=VERTEX_POINT('',#78655);
#14937=VERTEX_POINT('',#78657);
#14938=VERTEX_POINT('',#78661);
#14939=VERTEX_POINT('',#78662);
#14940=VERTEX_POINT('',#78664);
#14941=VERTEX_POINT('',#78666);
#14942=VERTEX_POINT('',#78668);
#14943=VERTEX_POINT('',#78670);
#14944=VERTEX_POINT('',#78674);
#14945=VERTEX_POINT('',#78675);
#14946=VERTEX_POINT('',#78677);
#14947=VERTEX_POINT('',#78684);
#14948=VERTEX_POINT('',#78686);
#14949=VERTEX_POINT('',#78688);
#14950=VERTEX_POINT('',#78692);
#14951=VERTEX_POINT('',#78693);
#14952=VERTEX_POINT('',#78695);
#14953=VERTEX_POINT('',#78702);
#14954=VERTEX_POINT('',#78704);
#14955=VERTEX_POINT('',#78711);
#14956=VERTEX_POINT('',#78715);
#14957=VERTEX_POINT('',#78716);
#14958=VERTEX_POINT('',#78718);
#14959=VERTEX_POINT('',#78725);
#14960=VERTEX_POINT('',#78727);
#14961=VERTEX_POINT('',#78948);
#14962=VERTEX_POINT('',#78994);
#14963=VERTEX_POINT('',#78995);
#14964=VERTEX_POINT('',#78999);
#14965=VERTEX_POINT('',#79067);
#14966=VERTEX_POINT('',#79137);
#14967=VERTEX_POINT('',#79138);
#14968=VERTEX_POINT('',#79187);
#14969=VERTEX_POINT('',#79191);
#14970=VERTEX_POINT('',#79253);
#14971=VERTEX_POINT('',#79254);
#14972=VERTEX_POINT('',#79352);
#14973=VERTEX_POINT('',#79376);
#14974=VERTEX_POINT('',#79379);
#14975=VERTEX_POINT('',#79380);
#14976=VERTEX_POINT('',#79382);
#14977=VERTEX_POINT('',#79392);
#14978=VERTEX_POINT('',#79406);
#14979=VERTEX_POINT('',#79429);
#14980=VERTEX_POINT('',#79431);
#14981=VERTEX_POINT('',#79476);
#14982=VERTEX_POINT('',#79502);
#14983=VERTEX_POINT('',#79547);
#14984=VERTEX_POINT('',#79588);
#14985=VERTEX_POINT('',#79618);
#14986=VERTEX_POINT('',#79659);
#14987=VERTEX_POINT('',#79661);
#14988=VERTEX_POINT('',#79685);
#14989=VERTEX_POINT('',#79698);
#14990=VERTEX_POINT('',#79752);
#14991=VERTEX_POINT('',#79755);
#14992=VERTEX_POINT('',#79759);
#14993=VERTEX_POINT('',#79760);
#14994=VERTEX_POINT('',#79762);
#14995=VERTEX_POINT('',#79764);
#14996=VERTEX_POINT('',#79766);
#14997=VERTEX_POINT('',#79768);
#14998=VERTEX_POINT('',#79770);
#14999=VERTEX_POINT('',#79772);
#15000=VERTEX_POINT('',#79776);
#15001=VERTEX_POINT('',#79778);
#15002=VERTEX_POINT('',#79782);
#15003=VERTEX_POINT('',#79786);
#15004=VERTEX_POINT('',#79798);
#15005=VERTEX_POINT('',#79802);
#15006=VERTEX_POINT('',#79814);
#15007=VERTEX_POINT('',#79818);
#15008=VERTEX_POINT('',#79822);
#15009=VERTEX_POINT('',#79832);
#15010=VERTEX_POINT('',#79858);
#15011=VERTEX_POINT('',#79868);
#15012=VERTEX_POINT('',#79875);
#15013=VERTEX_POINT('',#79877);
#15014=VERTEX_POINT('',#79881);
#15015=VERTEX_POINT('',#79882);
#15016=VERTEX_POINT('',#79884);
#15017=VERTEX_POINT('',#79962);
#15018=VERTEX_POINT('',#79966);
#15019=VERTEX_POINT('',#79970);
#15020=VERTEX_POINT('',#79974);
#15021=VERTEX_POINT('',#79978);
#15022=VERTEX_POINT('',#80017);
#15023=VERTEX_POINT('',#80030);
#15024=VERTEX_POINT('',#80086);
#15025=VERTEX_POINT('',#80088);
#15026=VERTEX_POINT('',#80090);
#15027=VERTEX_POINT('',#80129);
#15028=VERTEX_POINT('',#80131);
#15029=VERTEX_POINT('',#80197);
#15030=VERTEX_POINT('',#80209);
#15031=VERTEX_POINT('',#80210);
#15032=VERTEX_POINT('',#80223);
#15033=VERTEX_POINT('',#80235);
#15034=VERTEX_POINT('',#80237);
#15035=VERTEX_POINT('',#80241);
#15036=VERTEX_POINT('',#80245);
#15037=VERTEX_POINT('',#80249);
#15038=VERTEX_POINT('',#80253);
#15039=VERTEX_POINT('',#80257);
#15040=VERTEX_POINT('',#80261);
#15041=VERTEX_POINT('',#80320);
#15042=VERTEX_POINT('',#80324);
#15043=VERTEX_POINT('',#80325);
#15044=VERTEX_POINT('',#80330);
#15045=VERTEX_POINT('',#80332);
#15046=VERTEX_POINT('',#80336);
#15047=VERTEX_POINT('',#80340);
#15048=VERTEX_POINT('',#80342);
#15049=VERTEX_POINT('',#80344);
#15050=VERTEX_POINT('',#80346);
#15051=VERTEX_POINT('',#80459);
#15052=VERTEX_POINT('',#80463);
#15053=VERTEX_POINT('',#80464);
#15054=VERTEX_POINT('',#80471);
#15055=VERTEX_POINT('',#80475);
#15056=VERTEX_POINT('',#80476);
#15057=VERTEX_POINT('',#80478);
#15058=VERTEX_POINT('',#80480);
#15059=VERTEX_POINT('',#80482);
#15060=VERTEX_POINT('',#80484);
#15061=VERTEX_POINT('',#80486);
#15062=VERTEX_POINT('',#80488);
#15063=VERTEX_POINT('',#80490);
#15064=VERTEX_POINT('',#80492);
#15065=VERTEX_POINT('',#80494);
#15066=VERTEX_POINT('',#80496);
#15067=VERTEX_POINT('',#80498);
#15068=VERTEX_POINT('',#80500);
#15069=VERTEX_POINT('',#80502);
#15070=VERTEX_POINT('',#80504);
#15071=VERTEX_POINT('',#80506);
#15072=VERTEX_POINT('',#80508);
#15073=VERTEX_POINT('',#80510);
#15074=VERTEX_POINT('',#80512);
#15075=VERTEX_POINT('',#80514);
#15076=VERTEX_POINT('',#80516);
#15077=VERTEX_POINT('',#80518);
#15078=VERTEX_POINT('',#80520);
#15079=VERTEX_POINT('',#80523);
#15080=VERTEX_POINT('',#80525);
#15081=VERTEX_POINT('',#80527);
#15082=VERTEX_POINT('',#80529);
#15083=VERTEX_POINT('',#80531);
#15084=VERTEX_POINT('',#80533);
#15085=VERTEX_POINT('',#80535);
#15086=VERTEX_POINT('',#80537);
#15087=VERTEX_POINT('',#80543);
#15088=VERTEX_POINT('',#80545);
#15089=VERTEX_POINT('',#80549);
#15090=VERTEX_POINT('',#80551);
#15091=VERTEX_POINT('',#80555);
#15092=VERTEX_POINT('',#80557);
#15093=VERTEX_POINT('',#80559);
#15094=VERTEX_POINT('',#80562);
#15095=VERTEX_POINT('',#80567);
#15096=VERTEX_POINT('',#80569);
#15097=VERTEX_POINT('',#80580);
#15098=VERTEX_POINT('',#80582);
#15099=VERTEX_POINT('',#80591);
#15100=VERTEX_POINT('',#80593);
#15101=VERTEX_POINT('',#80597);
#15102=VERTEX_POINT('',#80601);
#15103=VERTEX_POINT('',#80605);
#15104=VERTEX_POINT('',#80609);
#15105=VERTEX_POINT('',#80613);
#15106=VERTEX_POINT('',#80615);
#15107=VERTEX_POINT('',#80625);
#15108=VERTEX_POINT('',#80629);
#15109=VERTEX_POINT('',#80633);
#15110=VERTEX_POINT('',#80637);
#15111=VERTEX_POINT('',#80639);
#15112=VERTEX_POINT('',#80643);
#15113=VERTEX_POINT('',#80647);
#15114=VERTEX_POINT('',#80651);
#15115=VERTEX_POINT('',#80655);
#15116=VERTEX_POINT('',#80659);
#15117=VERTEX_POINT('',#80663);
#15118=VERTEX_POINT('',#80667);
#15119=VERTEX_POINT('',#80671);
#15120=VERTEX_POINT('',#80675);
#15121=VERTEX_POINT('',#80679);
#15122=VERTEX_POINT('',#80683);
#15123=VERTEX_POINT('',#80685);
#15124=VERTEX_POINT('',#80689);
#15125=VERTEX_POINT('',#80691);
#15126=VERTEX_POINT('',#80695);
#15127=VERTEX_POINT('',#80699);
#15128=VERTEX_POINT('',#80703);
#15129=VERTEX_POINT('',#80705);
#15130=VERTEX_POINT('',#80709);
#15131=VERTEX_POINT('',#80711);
#15132=VERTEX_POINT('',#80715);
#15133=VERTEX_POINT('',#80721);
#15134=VERTEX_POINT('',#80722);
#15135=VERTEX_POINT('',#80729);
#15136=VERTEX_POINT('',#80731);
#15137=VERTEX_POINT('',#80738);
#15138=VERTEX_POINT('',#80740);
#15139=VERTEX_POINT('',#80744);
#15140=VERTEX_POINT('',#80746);
#15141=VERTEX_POINT('',#80750);
#15142=VERTEX_POINT('',#80752);
#15143=VERTEX_POINT('',#80764);
#15144=VERTEX_POINT('',#80775);
#15145=VERTEX_POINT('',#80779);
#15146=VERTEX_POINT('',#80781);
#15147=VERTEX_POINT('',#80785);
#15148=VERTEX_POINT('',#80791);
#15149=VERTEX_POINT('',#80881);
#15150=VERTEX_POINT('',#80887);
#15151=VERTEX_POINT('',#80889);
#15152=VERTEX_POINT('',#80893);
#15153=VERTEX_POINT('',#80897);
#15154=VERTEX_POINT('',#80899);
#15155=VERTEX_POINT('',#80903);
#15156=VERTEX_POINT('',#81648);
#15157=VERTEX_POINT('',#81652);
#15158=VERTEX_POINT('',#81656);
#15159=VERTEX_POINT('',#81660);
#15160=VERTEX_POINT('',#81664);
#15161=VERTEX_POINT('',#81668);
#15162=VERTEX_POINT('',#81672);
#15163=VERTEX_POINT('',#81676);
#15164=VERTEX_POINT('',#81680);
#15165=VERTEX_POINT('',#81684);
#15166=VERTEX_POINT('',#81690);
#15167=VERTEX_POINT('',#81692);
#15168=VERTEX_POINT('',#81698);
#15169=VERTEX_POINT('',#81700);
#15170=VERTEX_POINT('',#81704);
#15171=VERTEX_POINT('',#81708);
#15172=VERTEX_POINT('',#81714);
#15173=VERTEX_POINT('',#81716);
#15174=VERTEX_POINT('',#81722);
#15175=VERTEX_POINT('',#81724);
#15176=VERTEX_POINT('',#81728);
#15177=VERTEX_POINT('',#81734);
#15178=VERTEX_POINT('',#81738);
#15179=VERTEX_POINT('',#81740);
#15180=VERTEX_POINT('',#81811);
#15181=VERTEX_POINT('',#81815);
#15182=VERTEX_POINT('',#81817);
#15183=VERTEX_POINT('',#81821);
#15184=VERTEX_POINT('',#81823);
#15185=VERTEX_POINT('',#81825);
#15186=VERTEX_POINT('',#81827);
#15187=VERTEX_POINT('',#81829);
#15188=VERTEX_POINT('',#81831);
#15189=VERTEX_POINT('',#81833);
#15190=VERTEX_POINT('',#81835);
#15191=VERTEX_POINT('',#81837);
#15192=VERTEX_POINT('',#81840);
#15193=VERTEX_POINT('',#81889);
#15194=VERTEX_POINT('',#81893);
#15195=VERTEX_POINT('',#81895);
#15196=VERTEX_POINT('',#82014);
#15197=VERTEX_POINT('',#82016);
#15198=VERTEX_POINT('',#82020);
#15199=VERTEX_POINT('',#82024);
#15200=VERTEX_POINT('',#82028);
#15201=VERTEX_POINT('',#82032);
#15202=VERTEX_POINT('',#82036);
#15203=VERTEX_POINT('',#82040);
#15204=VERTEX_POINT('',#82044);
#15205=VERTEX_POINT('',#82048);
#15206=VERTEX_POINT('',#82052);
#15207=VERTEX_POINT('',#82056);
#15208=VERTEX_POINT('',#82060);
#15209=VERTEX_POINT('',#82064);
#15210=VERTEX_POINT('',#82068);
#15211=VERTEX_POINT('',#82074);
#15212=VERTEX_POINT('',#82081);
#15213=VERTEX_POINT('',#82086);
#15214=VERTEX_POINT('',#82090);
#15215=VERTEX_POINT('',#82096);
#15216=VERTEX_POINT('',#82103);
#15217=VERTEX_POINT('',#82108);
#15218=VERTEX_POINT('',#82114);
#15219=VERTEX_POINT('',#82119);
#15220=VERTEX_POINT('',#82121);
#15221=VERTEX_POINT('',#82123);
#15222=VERTEX_POINT('',#82127);
#15223=VERTEX_POINT('',#82131);
#15224=VERTEX_POINT('',#82135);
#15225=VERTEX_POINT('',#82137);
#15226=VERTEX_POINT('',#82141);
#15227=VERTEX_POINT('',#82145);
#15228=VERTEX_POINT('',#82147);
#15229=VERTEX_POINT('',#82153);
#15230=VERTEX_POINT('',#82157);
#15231=VERTEX_POINT('',#82163);
#15232=VERTEX_POINT('',#82197);
#15233=VERTEX_POINT('',#82203);
#15234=VERTEX_POINT('',#82205);
#15235=VERTEX_POINT('',#82211);
#15236=VERTEX_POINT('',#82215);
#15237=VERTEX_POINT('',#82217);
#15238=VERTEX_POINT('',#82219);
#15239=VERTEX_POINT('',#82227);
#15240=VERTEX_POINT('',#82231);
#15241=VERTEX_POINT('',#82235);
#15242=VERTEX_POINT('',#82237);
#15243=VERTEX_POINT('',#82241);
#15244=VERTEX_POINT('',#82243);
#15245=VERTEX_POINT('',#82247);
#15246=VERTEX_POINT('',#82249);
#15247=VERTEX_POINT('',#82253);
#15248=VERTEX_POINT('',#82255);
#15249=VERTEX_POINT('',#82264);
#15250=VERTEX_POINT('',#82270);
#15251=VERTEX_POINT('',#82275);
#15252=VERTEX_POINT('',#82276);
#15253=VERTEX_POINT('',#82278);
#15254=VERTEX_POINT('',#82280);
#15255=VERTEX_POINT('',#82284);
#15256=VERTEX_POINT('',#82286);
#15257=VERTEX_POINT('',#82298);
#15258=VERTEX_POINT('',#82299);
#15259=VERTEX_POINT('',#82301);
#15260=VERTEX_POINT('',#82303);
#15261=VERTEX_POINT('',#82440);
#15262=VERTEX_POINT('',#82442);
#15263=VERTEX_POINT('',#82446);
#15264=VERTEX_POINT('',#82447);
#15265=VERTEX_POINT('',#82449);
#15266=VERTEX_POINT('',#82451);
#15267=VERTEX_POINT('',#82455);
#15268=VERTEX_POINT('',#82457);
#15269=VERTEX_POINT('',#82461);
#15270=VERTEX_POINT('',#82463);
#15271=VERTEX_POINT('',#82466);
#15272=VERTEX_POINT('',#82468);
#15273=VERTEX_POINT('',#82470);
#15274=VERTEX_POINT('',#82472);
#15275=VERTEX_POINT('',#82474);
#15276=VERTEX_POINT('',#82476);
#15277=VERTEX_POINT('',#82478);
#15278=VERTEX_POINT('',#82545);
#15279=VERTEX_POINT('',#82547);
#15280=VERTEX_POINT('',#82603);
#15281=VERTEX_POINT('',#82614);
#15282=VERTEX_POINT('',#82620);
#15283=VERTEX_POINT('',#82624);
#15284=VERTEX_POINT('',#82628);
#15285=VERTEX_POINT('',#82632);
#15286=VERTEX_POINT('',#82636);
#15287=VERTEX_POINT('',#82640);
#15288=VERTEX_POINT('',#82646);
#15289=VERTEX_POINT('',#82648);
#15290=VERTEX_POINT('',#82668);
#15291=VERTEX_POINT('',#82726);
#15292=VERTEX_POINT('',#82730);
#15293=VERTEX_POINT('',#82769);
#15294=VERTEX_POINT('',#82911);
#15295=VERTEX_POINT('',#82917);
#15296=VERTEX_POINT('',#82921);
#15297=VERTEX_POINT('',#82925);
#15298=VERTEX_POINT('',#82929);
#15299=VERTEX_POINT('',#83027);
#15300=VERTEX_POINT('',#83029);
#15301=VERTEX_POINT('',#83167);
#15302=VERTEX_POINT('',#83177);
#15303=VERTEX_POINT('',#83310);
#15304=VERTEX_POINT('',#83311);
#15305=VERTEX_POINT('',#83313);
#15306=VERTEX_POINT('',#83318);
#15307=VERTEX_POINT('',#83320);
#15308=VERTEX_POINT('',#83325);
#15309=VERTEX_POINT('',#83327);
#15310=VERTEX_POINT('',#83358);
#15311=VERTEX_POINT('',#83360);
#15312=VERTEX_POINT('',#83395);
#15313=VERTEX_POINT('',#83428);
#15314=VERTEX_POINT('',#83429);
#15315=VERTEX_POINT('',#83432);
#15316=VERTEX_POINT('',#83436);
#15317=VERTEX_POINT('',#83437);
#15318=VERTEX_POINT('',#83439);
#15319=VERTEX_POINT('',#83441);
#15320=VERTEX_POINT('',#83452);
#15321=VERTEX_POINT('',#83454);
#15322=VERTEX_POINT('',#83456);
#15323=VERTEX_POINT('',#83458);
#15324=VERTEX_POINT('',#83472);
#15325=VERTEX_POINT('',#83475);
#15326=VERTEX_POINT('',#83476);
#15327=VERTEX_POINT('',#83478);
#15328=VERTEX_POINT('',#83480);
#15329=VERTEX_POINT('',#83484);
#15330=VERTEX_POINT('',#83486);
#15331=VERTEX_POINT('',#83490);
#15332=VERTEX_POINT('',#83491);
#15333=VERTEX_POINT('',#83499);
#15334=VERTEX_POINT('',#83500);
#15335=VERTEX_POINT('',#83502);
#15336=VERTEX_POINT('',#83504);
#15337=VERTEX_POINT('',#83508);
#15338=VERTEX_POINT('',#83510);
#15339=VERTEX_POINT('',#83514);
#15340=VERTEX_POINT('',#83516);
#15341=VERTEX_POINT('',#83523);
#15342=VERTEX_POINT('',#83524);
#15343=VERTEX_POINT('',#83526);
#15344=VERTEX_POINT('',#83528);
#15345=VERTEX_POINT('',#83530);
#15346=VERTEX_POINT('',#83532);
#15347=VERTEX_POINT('',#83534);
#15348=VERTEX_POINT('',#83536);
#15349=VERTEX_POINT('',#83538);
#15350=VERTEX_POINT('',#83540);
#15351=VERTEX_POINT('',#83542);
#15352=VERTEX_POINT('',#83544);
#15353=VERTEX_POINT('',#83546);
#15354=VERTEX_POINT('',#83548);
#15355=VERTEX_POINT('',#83559);
#15356=VERTEX_POINT('',#83561);
#15357=VERTEX_POINT('',#83572);
#15358=VERTEX_POINT('',#83574);
#15359=VERTEX_POINT('',#83576);
#15360=VERTEX_POINT('',#83578);
#15361=VERTEX_POINT('',#83589);
#15362=VERTEX_POINT('',#83591);
#15363=VERTEX_POINT('',#83602);
#15364=VERTEX_POINT('',#83604);
#15365=VERTEX_POINT('',#83606);
#15366=VERTEX_POINT('',#83608);
#15367=VERTEX_POINT('',#83619);
#15368=VERTEX_POINT('',#83621);
#15369=VERTEX_POINT('',#83632);
#15370=VERTEX_POINT('',#83634);
#15371=VERTEX_POINT('',#83636);
#15372=VERTEX_POINT('',#83638);
#15373=VERTEX_POINT('',#83640);
#15374=VERTEX_POINT('',#83642);
#15375=VERTEX_POINT('',#83644);
#15376=VERTEX_POINT('',#83646);
#15377=VERTEX_POINT('',#83648);
#15378=VERTEX_POINT('',#83651);
#15379=VERTEX_POINT('',#83653);
#15380=VERTEX_POINT('',#83664);
#15381=VERTEX_POINT('',#83666);
#15382=VERTEX_POINT('',#83677);
#15383=VERTEX_POINT('',#83679);
#15384=VERTEX_POINT('',#83690);
#15385=VERTEX_POINT('',#83692);
#15386=VERTEX_POINT('',#83703);
#15387=VERTEX_POINT('',#83705);
#15388=VERTEX_POINT('',#83716);
#15389=VERTEX_POINT('',#83718);
#15390=VERTEX_POINT('',#83729);
#15391=VERTEX_POINT('',#83731);
#15392=VERTEX_POINT('',#83742);
#15393=VERTEX_POINT('',#83755);
#15394=VERTEX_POINT('',#83757);
#15395=VERTEX_POINT('',#83759);
#15396=VERTEX_POINT('',#83770);
#15397=VERTEX_POINT('',#83772);
#15398=VERTEX_POINT('',#83783);
#15399=VERTEX_POINT('',#83785);
#15400=VERTEX_POINT('',#83796);
#15401=VERTEX_POINT('',#83798);
#15402=VERTEX_POINT('',#83809);
#15403=VERTEX_POINT('',#83811);
#15404=VERTEX_POINT('',#83822);
#15405=VERTEX_POINT('',#83824);
#15406=VERTEX_POINT('',#83835);
#15407=VERTEX_POINT('',#83837);
#15408=VERTEX_POINT('',#83848);
#15409=VERTEX_POINT('',#83850);
#15410=VERTEX_POINT('',#83863);
#15411=VERTEX_POINT('',#83865);
#15412=VERTEX_POINT('',#83869);
#15413=VERTEX_POINT('',#83871);
#15414=VERTEX_POINT('',#83875);
#15415=VERTEX_POINT('',#83877);
#15416=VERTEX_POINT('',#83884);
#15417=VERTEX_POINT('',#83885);
#15418=VERTEX_POINT('',#83887);
#15419=VERTEX_POINT('',#83889);
#15420=VERTEX_POINT('',#83893);
#15421=VERTEX_POINT('',#83894);
#15422=VERTEX_POINT('',#83899);
#15423=VERTEX_POINT('',#83901);
#15424=VERTEX_POINT('',#83908);
#15425=VERTEX_POINT('',#83910);
#15426=VERTEX_POINT('',#83918);
#15427=VERTEX_POINT('',#83919);
#15428=VERTEX_POINT('',#83921);
#15429=VERTEX_POINT('',#83923);
#15430=VERTEX_POINT('',#83927);
#15431=VERTEX_POINT('',#83929);
#15432=VERTEX_POINT('',#83933);
#15433=VERTEX_POINT('',#83935);
#15434=VERTEX_POINT('',#83963);
#15435=VERTEX_POINT('',#83964);
#15436=VERTEX_POINT('',#83972);
#15437=VERTEX_POINT('',#83974);
#15438=VERTEX_POINT('',#83976);
#15439=VERTEX_POINT('',#83980);
#15440=VERTEX_POINT('',#83987);
#15441=VERTEX_POINT('',#83994);
#15442=VERTEX_POINT('',#83996);
#15443=VERTEX_POINT('',#84053);
#15444=VERTEX_POINT('',#84130);
#15445=VERTEX_POINT('',#84134);
#15446=VERTEX_POINT('',#84136);
#15447=VERTEX_POINT('',#84178);
#15448=VERTEX_POINT('',#84242);
#15449=VERTEX_POINT('',#84276);
#15450=VERTEX_POINT('',#84333);
#15451=VERTEX_POINT('',#84414);
#15452=VERTEX_POINT('',#84422);
#15453=VERTEX_POINT('',#84423);
#15454=VERTEX_POINT('',#84428);
#15455=VERTEX_POINT('',#84430);
#15456=VERTEX_POINT('',#84434);
#15457=VERTEX_POINT('',#84436);
#15458=VERTEX_POINT('',#84440);
#15459=VERTEX_POINT('',#84441);
#15460=VERTEX_POINT('',#84470);
#15461=VERTEX_POINT('',#84472);
#15462=VERTEX_POINT('',#84478);
#15463=VERTEX_POINT('',#84484);
#15464=VERTEX_POINT('',#84486);
#15465=VERTEX_POINT('',#84488);
#15466=VERTEX_POINT('',#84492);
#15467=VERTEX_POINT('',#84494);
#15468=VERTEX_POINT('',#84501);
#15469=VERTEX_POINT('',#84561);
#15470=VERTEX_POINT('',#84584);
#15471=VERTEX_POINT('',#84588);
#15472=VERTEX_POINT('',#84589);
#15473=VERTEX_POINT('',#84669);
#15474=VERTEX_POINT('',#84733);
#15475=VERTEX_POINT('',#84764);
#15476=VERTEX_POINT('',#84821);
#15477=VERTEX_POINT('',#84902);
#15478=VERTEX_POINT('',#84910);
#15479=VERTEX_POINT('',#84912);
#15480=VERTEX_POINT('',#84916);
#15481=VERTEX_POINT('',#84918);
#15482=VERTEX_POINT('',#84922);
#15483=VERTEX_POINT('',#84924);
#15484=VERTEX_POINT('',#84931);
#15485=VERTEX_POINT('',#84932);
#15486=VERTEX_POINT('',#84934);
#15487=VERTEX_POINT('',#84936);
#15488=VERTEX_POINT('',#84940);
#15489=VERTEX_POINT('',#84941);
#15490=VERTEX_POINT('',#84946);
#15491=VERTEX_POINT('',#84948);
#15492=VERTEX_POINT('',#84955);
#15493=VERTEX_POINT('',#84957);
#15494=VERTEX_POINT('',#84997);
#15495=VERTEX_POINT('',#85007);
#15496=VERTEX_POINT('',#85008);
#15497=VERTEX_POINT('',#85010);
#15498=VERTEX_POINT('',#85012);
#15499=VERTEX_POINT('',#85014);
#15500=VERTEX_POINT('',#85016);
#15501=VERTEX_POINT('',#85018);
#15502=VERTEX_POINT('',#85020);
#15503=VERTEX_POINT('',#85022);
#15504=VERTEX_POINT('',#85024);
#15505=VERTEX_POINT('',#85026);
#15506=VERTEX_POINT('',#85028);
#15507=VERTEX_POINT('',#85039);
#15508=VERTEX_POINT('',#85043);
#15509=VERTEX_POINT('',#85076);
#15510=VERTEX_POINT('',#85080);
#15511=VERTEX_POINT('',#85117);
#15512=VERTEX_POINT('',#85121);
#15513=VERTEX_POINT('',#85189);
#15514=VERTEX_POINT('',#85190);
#15515=VERTEX_POINT('',#85209);
#15516=VERTEX_POINT('',#85211);
#15517=VERTEX_POINT('',#85213);
#15518=VERTEX_POINT('',#85217);
#15519=VERTEX_POINT('',#85218);
#15520=VERTEX_POINT('',#85221);
#15521=VERTEX_POINT('',#85225);
#15522=VERTEX_POINT('',#85275);
#15523=VERTEX_POINT('',#85279);
#15524=VERTEX_POINT('',#85280);
#15525=VERTEX_POINT('',#85282);
#15526=VERTEX_POINT('',#85284);
#15527=VERTEX_POINT('',#85302);
#15528=VERTEX_POINT('',#85303);
#15529=VERTEX_POINT('',#85305);
#15530=VERTEX_POINT('',#85307);
#15531=VERTEX_POINT('',#85311);
#15532=VERTEX_POINT('',#85312);
#15533=VERTEX_POINT('',#85317);
#15534=VERTEX_POINT('',#85319);
#15535=VERTEX_POINT('',#85323);
#15536=VERTEX_POINT('',#85324);
#15537=VERTEX_POINT('',#85329);
#15538=VERTEX_POINT('',#85331);
#15539=VERTEX_POINT('',#85333);
#15540=VERTEX_POINT('',#85389);
#15541=VERTEX_POINT('',#85393);
#15542=VERTEX_POINT('',#85394);
#15543=VERTEX_POINT('',#85397);
#15544=VERTEX_POINT('',#85401);
#15545=VERTEX_POINT('',#85402);
#15546=VERTEX_POINT('',#85456);
#15547=VERTEX_POINT('',#85462);
#15548=VERTEX_POINT('',#85468);
#15549=VERTEX_POINT('',#85470);
#15550=VERTEX_POINT('',#85474);
#15551=VERTEX_POINT('',#85476);
#15552=VERTEX_POINT('',#85480);
#15553=VERTEX_POINT('',#85485);
#15554=VERTEX_POINT('',#85489);
#15555=VERTEX_POINT('',#85494);
#15556=VERTEX_POINT('',#85498);
#15557=VERTEX_POINT('',#85504);
#15558=VERTEX_POINT('',#85510);
#15559=VERTEX_POINT('',#85556);
#15560=VERTEX_POINT('',#85560);
#15561=VERTEX_POINT('',#85561);
#15562=VERTEX_POINT('',#85563);
#15563=VERTEX_POINT('',#85565);
#15564=VERTEX_POINT('',#85567);
#15565=VERTEX_POINT('',#85569);
#15566=VERTEX_POINT('',#85613);
#15567=VERTEX_POINT('',#85617);
#15568=VERTEX_POINT('',#85619);
#15569=VERTEX_POINT('',#85623);
#15570=VERTEX_POINT('',#85624);
#15571=VERTEX_POINT('',#85629);
#15572=VERTEX_POINT('',#85631);
#15573=VERTEX_POINT('',#85635);
#15574=VERTEX_POINT('',#85637);
#15575=VERTEX_POINT('',#85641);
#15576=VERTEX_POINT('',#85642);
#15577=VERTEX_POINT('',#85683);
#15578=VERTEX_POINT('',#85685);
#15579=VERTEX_POINT('',#85689);
#15580=VERTEX_POINT('',#85690);
#15581=VERTEX_POINT('',#85697);
#15582=VERTEX_POINT('',#85703);
#15583=VERTEX_POINT('',#85707);
#15584=VERTEX_POINT('',#85711);
#15585=VERTEX_POINT('',#85712);
#15586=VERTEX_POINT('',#85724);
#15587=VERTEX_POINT('',#85725);
#15588=VERTEX_POINT('',#85823);
#15589=VERTEX_POINT('',#85824);
#15590=VERTEX_POINT('',#85826);
#15591=VERTEX_POINT('',#85903);
#15592=VERTEX_POINT('',#85961);
#15593=VERTEX_POINT('',#85963);
#15594=VERTEX_POINT('',#86022);
#15595=VERTEX_POINT('',#86026);
#15596=VERTEX_POINT('',#86028);
#15597=VERTEX_POINT('',#86075);
#15598=VERTEX_POINT('',#86079);
#15599=VERTEX_POINT('',#86080);
#15600=VERTEX_POINT('',#86196);
#15601=VERTEX_POINT('',#86197);
#15602=VERTEX_POINT('',#86204);
#15603=VERTEX_POINT('',#86205);
#15604=VERTEX_POINT('',#86212);
#15605=VERTEX_POINT('',#86214);
#15606=VERTEX_POINT('',#86220);
#15607=VERTEX_POINT('',#86222);
#15608=VERTEX_POINT('',#86228);
#15609=VERTEX_POINT('',#86230);
#15610=VERTEX_POINT('',#86236);
#15611=VERTEX_POINT('',#86238);
#15612=VERTEX_POINT('',#86244);
#15613=VERTEX_POINT('',#86246);
#15614=VERTEX_POINT('',#86252);
#15615=VERTEX_POINT('',#86254);
#15616=VERTEX_POINT('',#86260);
#15617=VERTEX_POINT('',#86261);
#15618=VERTEX_POINT('',#86263);
#15619=VERTEX_POINT('',#86273);
#15620=VERTEX_POINT('',#86274);
#15621=VERTEX_POINT('',#86281);
#15622=VERTEX_POINT('',#86283);
#15623=VERTEX_POINT('',#86341);
#15624=VERTEX_POINT('',#86348);
#15625=VERTEX_POINT('',#86427);
#15626=VERTEX_POINT('',#86429);
#15627=VERTEX_POINT('',#86433);
#15628=VERTEX_POINT('',#86434);
#15629=VERTEX_POINT('',#86436);
#15630=VERTEX_POINT('',#86438);
#15631=VERTEX_POINT('',#86442);
#15632=VERTEX_POINT('',#86443);
#15633=VERTEX_POINT('',#86445);
#15634=VERTEX_POINT('',#86447);
#15635=VERTEX_POINT('',#86506);
#15636=VERTEX_POINT('',#86508);
#15637=VERTEX_POINT('',#86567);
#15638=VERTEX_POINT('',#86569);
#15639=VERTEX_POINT('',#86571);
#15640=VERTEX_POINT('',#86573);
#15641=VERTEX_POINT('',#86575);
#15642=VERTEX_POINT('',#86619);
#15643=VERTEX_POINT('',#86620);
#15644=VERTEX_POINT('',#86622);
#15645=VERTEX_POINT('',#86624);
#15646=VERTEX_POINT('',#86626);
#15647=VERTEX_POINT('',#86630);
#15648=VERTEX_POINT('',#86632);
#15649=VERTEX_POINT('',#86675);
#15650=VERTEX_POINT('',#86677);
#15651=VERTEX_POINT('',#86679);
#15652=VERTEX_POINT('',#86681);
#15653=VERTEX_POINT('',#86685);
#15654=VERTEX_POINT('',#86687);
#15655=VERTEX_POINT('',#86730);
#15656=VERTEX_POINT('',#86732);
#15657=VERTEX_POINT('',#86734);
#15658=VERTEX_POINT('',#86736);
#15659=VERTEX_POINT('',#86748);
#15660=VERTEX_POINT('',#86752);
#15661=VERTEX_POINT('',#86756);
#15662=VERTEX_POINT('',#86758);
#15663=VERTEX_POINT('',#86762);
#15664=VERTEX_POINT('',#86764);
#15665=VERTEX_POINT('',#86766);
#15666=VERTEX_POINT('',#86768);
#15667=VERTEX_POINT('',#86770);
#15668=VERTEX_POINT('',#86774);
#15669=VERTEX_POINT('',#86776);
#15670=VERTEX_POINT('',#86780);
#15671=VERTEX_POINT('',#86782);
#15672=VERTEX_POINT('',#86786);
#15673=VERTEX_POINT('',#86788);
#15674=VERTEX_POINT('',#86792);
#15675=VERTEX_POINT('',#86794);
#15676=VERTEX_POINT('',#86798);
#15677=VERTEX_POINT('',#86799);
#15678=VERTEX_POINT('',#86809);
#15679=VERTEX_POINT('',#86811);
#15680=VERTEX_POINT('',#86818);
#15681=VERTEX_POINT('',#86819);
#15682=VERTEX_POINT('',#86821);
#15683=VERTEX_POINT('',#86826);
#15684=VERTEX_POINT('',#86827);
#15685=VERTEX_POINT('',#86829);
#15686=VERTEX_POINT('',#86831);
#15687=VERTEX_POINT('',#86835);
#15688=VERTEX_POINT('',#86837);
#15689=VERTEX_POINT('',#86841);
#15690=VERTEX_POINT('',#86843);
#15691=VERTEX_POINT('',#86847);
#15692=VERTEX_POINT('',#86849);
#15693=VERTEX_POINT('',#86853);
#15694=VERTEX_POINT('',#86855);
#15695=VERTEX_POINT('',#86859);
#15696=VERTEX_POINT('',#86861);
#15697=VERTEX_POINT('',#86865);
#15698=VERTEX_POINT('',#86867);
#15699=VERTEX_POINT('',#86874);
#15700=VERTEX_POINT('',#86875);
#15701=VERTEX_POINT('',#86877);
#15702=VERTEX_POINT('',#86879);
#15703=VERTEX_POINT('',#86918);
#15704=VERTEX_POINT('',#86920);
#15705=VERTEX_POINT('',#86928);
#15706=VERTEX_POINT('',#86967);
#15707=VERTEX_POINT('',#86969);
#15708=VERTEX_POINT('',#87008);
#15709=VERTEX_POINT('',#87070);
#15710=VERTEX_POINT('',#87072);
#15711=VERTEX_POINT('',#87076);
#15712=VERTEX_POINT('',#87078);
#15713=VERTEX_POINT('',#87082);
#15714=VERTEX_POINT('',#87084);
#15715=VERTEX_POINT('',#87126);
#15716=VERTEX_POINT('',#87128);
#15717=VERTEX_POINT('',#87167);
#15718=VERTEX_POINT('',#87233);
#15719=VERTEX_POINT('',#87237);
#15720=VERTEX_POINT('',#87239);
#15721=VERTEX_POINT('',#87241);
#15722=VERTEX_POINT('',#87243);
#15723=VERTEX_POINT('',#87247);
#15724=VERTEX_POINT('',#87249);
#15725=VERTEX_POINT('',#87253);
#15726=VERTEX_POINT('',#87255);
#15727=VERTEX_POINT('',#87259);
#15728=VERTEX_POINT('',#87261);
#15729=VERTEX_POINT('',#87265);
#15730=VERTEX_POINT('',#87267);
#15731=VERTEX_POINT('',#87271);
#15732=VERTEX_POINT('',#87273);
#15733=VERTEX_POINT('',#87277);
#15734=VERTEX_POINT('',#87279);
#15735=VERTEX_POINT('',#87286);
#15736=VERTEX_POINT('',#87287);
#15737=VERTEX_POINT('',#87289);
#15738=VERTEX_POINT('',#87291);
#15739=VERTEX_POINT('',#87373);
#15740=VERTEX_POINT('',#87375);
#15741=VERTEX_POINT('',#87439);
#15742=VERTEX_POINT('',#87440);
#15743=VERTEX_POINT('',#87442);
#15744=VERTEX_POINT('',#87543);
#15745=VERTEX_POINT('',#87547);
#15746=VERTEX_POINT('',#87551);
#15747=VERTEX_POINT('',#87553);
#15748=VERTEX_POINT('',#87629);
#15749=VERTEX_POINT('',#87633);
#15750=VERTEX_POINT('',#87637);
#15751=VERTEX_POINT('',#87644);
#15752=VERTEX_POINT('',#87646);
#15753=VERTEX_POINT('',#87650);
#15754=VERTEX_POINT('',#87652);
#15755=VERTEX_POINT('',#87656);
#15756=VERTEX_POINT('',#87658);
#15757=VERTEX_POINT('',#87662);
#15758=VERTEX_POINT('',#87664);
#15759=VERTEX_POINT('',#87668);
#15760=VERTEX_POINT('',#87670);
#15761=VERTEX_POINT('',#87674);
#15762=VERTEX_POINT('',#87678);
#15763=VERTEX_POINT('',#87679);
#15764=VERTEX_POINT('',#87686);
#15765=VERTEX_POINT('',#87687);
#15766=VERTEX_POINT('',#87726);
#15767=VERTEX_POINT('',#87727);
#15768=VERTEX_POINT('',#87729);
#15769=VERTEX_POINT('',#87731);
#15770=VERTEX_POINT('',#87735);
#15771=VERTEX_POINT('',#87737);
#15772=VERTEX_POINT('',#87798);
#15773=VERTEX_POINT('',#87799);
#15774=VERTEX_POINT('',#87803);
#15775=VERTEX_POINT('',#87804);
#15776=VERTEX_POINT('',#87809);
#15777=VERTEX_POINT('',#87810);
#15778=VERTEX_POINT('',#87812);
#15779=VERTEX_POINT('',#87814);
#15780=VERTEX_POINT('',#87818);
#15781=VERTEX_POINT('',#87910);
#15782=VERTEX_POINT('',#87914);
#15783=VERTEX_POINT('',#87973);
#15784=VERTEX_POINT('',#87978);
#15785=VERTEX_POINT('',#87980);
#15786=VERTEX_POINT('',#88080);
#15787=VERTEX_POINT('',#88182);
#15788=VERTEX_POINT('',#88232);
#15789=VERTEX_POINT('',#88235);
#15790=VERTEX_POINT('',#88238);
#15791=VERTEX_POINT('',#88243);
#15792=VERTEX_POINT('',#88245);
#15793=VERTEX_POINT('',#88304);
#15794=VERTEX_POINT('',#88314);
#15795=VERTEX_POINT('',#88357);
#15796=VERTEX_POINT('',#88359);
#15797=VERTEX_POINT('',#88361);
#15798=VERTEX_POINT('',#88363);
#15799=VERTEX_POINT('',#88389);
#15800=VERTEX_POINT('',#88391);
#15801=VERTEX_POINT('',#88397);
#15802=VERTEX_POINT('',#88400);
#15803=VERTEX_POINT('',#88417);
#15804=VERTEX_POINT('',#88430);
#15805=VERTEX_POINT('',#88434);
#15806=VERTEX_POINT('',#88440);
#15807=VERTEX_POINT('',#88450);
#15808=VERTEX_POINT('',#88452);
#15809=VERTEX_POINT('',#88459);
#15810=VERTEX_POINT('',#88463);
#15811=VERTEX_POINT('',#88467);
#15812=VERTEX_POINT('',#88498);
#15813=VERTEX_POINT('',#88502);
#15814=VERTEX_POINT('',#88506);
#15815=VERTEX_POINT('',#88510);
#15816=VERTEX_POINT('',#88518);
#15817=VERTEX_POINT('',#88585);
#15818=VERTEX_POINT('',#88590);
#15819=VERTEX_POINT('',#88592);
#15820=VERTEX_POINT('',#88828);
#15821=VERTEX_POINT('',#88832);
#15822=VERTEX_POINT('',#88833);
#15823=VERTEX_POINT('',#88835);
#15824=VERTEX_POINT('',#88846);
#15825=VERTEX_POINT('',#88848);
#15826=VERTEX_POINT('',#88852);
#15827=VERTEX_POINT('',#88856);
#15828=VERTEX_POINT('',#88860);
#15829=VERTEX_POINT('',#88864);
#15830=VERTEX_POINT('',#88868);
#15831=VERTEX_POINT('',#88871);
#15832=VERTEX_POINT('',#88874);
#15833=VERTEX_POINT('',#88876);
#15834=VERTEX_POINT('',#88957);
#15835=VERTEX_POINT('',#88959);
#15836=VERTEX_POINT('',#88973);
#15837=VERTEX_POINT('',#89093);
#15838=VERTEX_POINT('',#89160);
#15839=VERTEX_POINT('',#89164);
#15840=VERTEX_POINT('',#89168);
#15841=VERTEX_POINT('',#89172);
#15842=VERTEX_POINT('',#89176);
#15843=VERTEX_POINT('',#89233);
#15844=VERTEX_POINT('',#89315);
#15845=VERTEX_POINT('',#89319);
#15846=VERTEX_POINT('',#89325);
#15847=VERTEX_POINT('',#89329);
#15848=VERTEX_POINT('',#89368);
#15849=VERTEX_POINT('',#89369);
#15850=VERTEX_POINT('',#89437);
#15851=VERTEX_POINT('',#89494);
#15852=VERTEX_POINT('',#89543);
#15853=VERTEX_POINT('',#89575);
#15854=VERTEX_POINT('',#89628);
#15855=VERTEX_POINT('',#89639);
#15856=VERTEX_POINT('',#89705);
#15857=VERTEX_POINT('',#89707);
#15858=VERTEX_POINT('',#89786);
#15859=VERTEX_POINT('',#89788);
#15860=VERTEX_POINT('',#89792);
#15861=VERTEX_POINT('',#89794);
#15862=VERTEX_POINT('',#89798);
#15863=VERTEX_POINT('',#89800);
#15864=VERTEX_POINT('',#89804);
#15865=VERTEX_POINT('',#89806);
#15866=VERTEX_POINT('',#89810);
#15867=VERTEX_POINT('',#89812);
#15868=VERTEX_POINT('',#89816);
#15869=VERTEX_POINT('',#89818);
#15870=VERTEX_POINT('',#89857);
#15871=VERTEX_POINT('',#89964);
#15872=VERTEX_POINT('',#89966);
#15873=VERTEX_POINT('',#89970);
#15874=VERTEX_POINT('',#89976);
#15875=VERTEX_POINT('',#89980);
#15876=VERTEX_POINT('',#89984);
#15877=VERTEX_POINT('',#89988);
#15878=VERTEX_POINT('',#89992);
#15879=VERTEX_POINT('',#89996);
#15880=VERTEX_POINT('',#90000);
#15881=VERTEX_POINT('',#90004);
#15882=VERTEX_POINT('',#90010);
#15883=VERTEX_POINT('',#90014);
#15884=VERTEX_POINT('',#90018);
#15885=VERTEX_POINT('',#90022);
#15886=VERTEX_POINT('',#90028);
#15887=VERTEX_POINT('',#90032);
#15888=VERTEX_POINT('',#90092);
#15889=VERTEX_POINT('',#90152);
#15890=VERTEX_POINT('',#90214);
#15891=VERTEX_POINT('',#90218);
#15892=VERTEX_POINT('',#90222);
#15893=VERTEX_POINT('',#90229);
#15894=VERTEX_POINT('',#90230);
#15895=VERTEX_POINT('',#90232);
#15896=VERTEX_POINT('',#90234);
#15897=VERTEX_POINT('',#90236);
#15898=VERTEX_POINT('',#90303);
#15899=VERTEX_POINT('',#90304);
#15900=VERTEX_POINT('',#90307);
#15901=VERTEX_POINT('',#90311);
#15902=VERTEX_POINT('',#90313);
#15903=VERTEX_POINT('',#90389);
#15904=VERTEX_POINT('',#90390);
#15905=VERTEX_POINT('',#90406);
#15906=VERTEX_POINT('',#90408);
#15907=VERTEX_POINT('',#90412);
#15908=VERTEX_POINT('',#90413);
#15909=VERTEX_POINT('',#90448);
#15910=VERTEX_POINT('',#90450);
#15911=VERTEX_POINT('',#90454);
#15912=VERTEX_POINT('',#90456);
#15913=VERTEX_POINT('',#90460);
#15914=VERTEX_POINT('',#90462);
#15915=VERTEX_POINT('',#90466);
#15916=VERTEX_POINT('',#90468);
#15917=VERTEX_POINT('',#90472);
#15918=VERTEX_POINT('',#90474);
#15919=VERTEX_POINT('',#90476);
#15920=VERTEX_POINT('',#90486);
#15921=VERTEX_POINT('',#90490);
#15922=VERTEX_POINT('',#90491);
#15923=VERTEX_POINT('',#90494);
#15924=VERTEX_POINT('',#90498);
#15925=VERTEX_POINT('',#90499);
#15926=VERTEX_POINT('',#90502);
#15927=VERTEX_POINT('',#90508);
#15928=VERTEX_POINT('',#90514);
#15929=VERTEX_POINT('',#90515);
#15930=VERTEX_POINT('',#90520);
#15931=VERTEX_POINT('',#90521);
#15932=VERTEX_POINT('',#90526);
#15933=VERTEX_POINT('',#90531);
#15934=VERTEX_POINT('',#90535);
#15935=VERTEX_POINT('',#90540);
#15936=VERTEX_POINT('',#90544);
#15937=VERTEX_POINT('',#90550);
#15938=VERTEX_POINT('',#90556);
#15939=VERTEX_POINT('',#90560);
#15940=VERTEX_POINT('',#90564);
#15941=VERTEX_POINT('',#90565);
#15942=VERTEX_POINT('',#90567);
#15943=VERTEX_POINT('',#90569);
#15944=VERTEX_POINT('',#90613);
#15945=VERTEX_POINT('',#90615);
#15946=VERTEX_POINT('',#90617);
#15947=VERTEX_POINT('',#90621);
#15948=VERTEX_POINT('',#90623);
#15949=VERTEX_POINT('',#90627);
#15950=VERTEX_POINT('',#90629);
#15951=VERTEX_POINT('',#90633);
#15952=VERTEX_POINT('',#90635);
#15953=VERTEX_POINT('',#90639);
#15954=VERTEX_POINT('',#90641);
#15955=VERTEX_POINT('',#90645);
#15956=VERTEX_POINT('',#90647);
#15957=VERTEX_POINT('',#90651);
#15958=VERTEX_POINT('',#90652);
#15959=VERTEX_POINT('',#90657);
#15960=VERTEX_POINT('',#90659);
#15961=VERTEX_POINT('',#90665);
#15962=VERTEX_POINT('',#90671);
#15963=VERTEX_POINT('',#90675);
#15964=VERTEX_POINT('',#90714);
#15965=VERTEX_POINT('',#90848);
#15966=VERTEX_POINT('',#90913);
#15967=VERTEX_POINT('',#90914);
#15968=VERTEX_POINT('',#90916);
#15969=VERTEX_POINT('',#90918);
#15970=VERTEX_POINT('',#91060);
#15971=VERTEX_POINT('',#91116);
#15972=VERTEX_POINT('',#91118);
#15973=VERTEX_POINT('',#91122);
#15974=VERTEX_POINT('',#91181);
#15975=VERTEX_POINT('',#91183);
#15976=VERTEX_POINT('',#91253);
#15977=VERTEX_POINT('',#91313);
#15978=VERTEX_POINT('',#91319);
#15979=VERTEX_POINT('',#91321);
#15980=VERTEX_POINT('',#91327);
#15981=VERTEX_POINT('',#91329);
#15982=VERTEX_POINT('',#91335);
#15983=VERTEX_POINT('',#91336);
#15984=VERTEX_POINT('',#91343);
#15985=VERTEX_POINT('',#91344);
#15986=VERTEX_POINT('',#91351);
#15987=VERTEX_POINT('',#91353);
#15988=VERTEX_POINT('',#91359);
#15989=VERTEX_POINT('',#91361);
#15990=VERTEX_POINT('',#91367);
#15991=VERTEX_POINT('',#91369);
#15992=VERTEX_POINT('',#91375);
#15993=VERTEX_POINT('',#91377);
#15994=VERTEX_POINT('',#91383);
#15995=VERTEX_POINT('',#91384);
#15996=VERTEX_POINT('',#91386);
#15997=VERTEX_POINT('',#91431);
#15998=VERTEX_POINT('',#91489);
#15999=VERTEX_POINT('',#91491);
#16000=VERTEX_POINT('',#91549);
#16001=VERTEX_POINT('',#91550);
#16002=VERTEX_POINT('',#91599);
#16003=VERTEX_POINT('',#91601);
#16004=VERTEX_POINT('',#91605);
#16005=VERTEX_POINT('',#91607);
#16006=VERTEX_POINT('',#91611);
#16007=VERTEX_POINT('',#91612);
#16008=VERTEX_POINT('',#91617);
#16009=VERTEX_POINT('',#91621);
#16010=VERTEX_POINT('',#91662);
#16011=VERTEX_POINT('',#91664);
#16012=VERTEX_POINT('',#91666);
#16013=VERTEX_POINT('',#91668);
#16014=VERTEX_POINT('',#91670);
#16015=VERTEX_POINT('',#91672);
#16016=VERTEX_POINT('',#91731);
#16017=VERTEX_POINT('',#91733);
#16018=VERTEX_POINT('',#91792);
#16019=VERTEX_POINT('',#91796);
#16020=VERTEX_POINT('',#91798);
#16021=VERTEX_POINT('',#91802);
#16022=VERTEX_POINT('',#91804);
#16023=VERTEX_POINT('',#91806);
#16024=VERTEX_POINT('',#91810);
#16025=VERTEX_POINT('',#91812);
#16026=VERTEX_POINT('',#91852);
#16027=VERTEX_POINT('',#91854);
#16028=VERTEX_POINT('',#91856);
#16029=VERTEX_POINT('',#91858);
#16030=VERTEX_POINT('',#91862);
#16031=VERTEX_POINT('',#91864);
#16032=VERTEX_POINT('',#91904);
#16033=VERTEX_POINT('',#91909);
#16034=VERTEX_POINT('',#91914);
#16035=VERTEX_POINT('',#91916);
#16036=VERTEX_POINT('',#91923);
#16037=VERTEX_POINT('',#91927);
#16038=VERTEX_POINT('',#91931);
#16039=VERTEX_POINT('',#91932);
#16040=VERTEX_POINT('',#91935);
#16041=VERTEX_POINT('',#91937);
#16042=VERTEX_POINT('',#91945);
#16043=VERTEX_POINT('',#91947);
#16044=VERTEX_POINT('',#91990);
#16045=VERTEX_POINT('',#91994);
#16046=VERTEX_POINT('',#91996);
#16047=VERTEX_POINT('',#91998);
#16048=VERTEX_POINT('',#92000);
#16049=VERTEX_POINT('',#92002);
#16050=VERTEX_POINT('',#92006);
#16051=VERTEX_POINT('',#92008);
#16052=VERTEX_POINT('',#92012);
#16053=VERTEX_POINT('',#92013);
#16054=VERTEX_POINT('',#92018);
#16055=VERTEX_POINT('',#92020);
#16056=VERTEX_POINT('',#92024);
#16057=VERTEX_POINT('',#92025);
#16058=VERTEX_POINT('',#92030);
#16059=VERTEX_POINT('',#92062);
#16060=VERTEX_POINT('',#92066);
#16061=VERTEX_POINT('',#92068);
#16062=VERTEX_POINT('',#92075);
#16063=VERTEX_POINT('',#92077);
#16064=VERTEX_POINT('',#92079);
#16065=VERTEX_POINT('',#92083);
#16066=VERTEX_POINT('',#92084);
#16067=VERTEX_POINT('',#92086);
#16068=VERTEX_POINT('',#92088);
#16069=VERTEX_POINT('',#92092);
#16070=VERTEX_POINT('',#92093);
#16071=VERTEX_POINT('',#92098);
#16072=VERTEX_POINT('',#92099);
#16073=VERTEX_POINT('',#92104);
#16074=VERTEX_POINT('',#92105);
#16075=VERTEX_POINT('',#92110);
#16076=VERTEX_POINT('',#92111);
#16077=VERTEX_POINT('',#92116);
#16078=VERTEX_POINT('',#92118);
#16079=VERTEX_POINT('',#92122);
#16080=VERTEX_POINT('',#92123);
#16081=VERTEX_POINT('',#92131);
#16082=VERTEX_POINT('',#92132);
#16083=VERTEX_POINT('',#92134);
#16084=VERTEX_POINT('',#92136);
#16085=VERTEX_POINT('',#92169);
#16086=VERTEX_POINT('',#92171);
#16087=VERTEX_POINT('',#92178);
#16088=VERTEX_POINT('',#92218);
#16089=VERTEX_POINT('',#92220);
#16090=VERTEX_POINT('',#92259);
#16091=VERTEX_POINT('',#92318);
#16092=VERTEX_POINT('',#92320);
#16093=VERTEX_POINT('',#92324);
#16094=VERTEX_POINT('',#92325);
#16095=VERTEX_POINT('',#92330);
#16096=VERTEX_POINT('',#92332);
#16097=VERTEX_POINT('',#92374);
#16098=VERTEX_POINT('',#92376);
#16099=VERTEX_POINT('',#92415);
#16100=VERTEX_POINT('',#92481);
#16101=VERTEX_POINT('',#92485);
#16102=VERTEX_POINT('',#92487);
#16103=VERTEX_POINT('',#92489);
#16104=VERTEX_POINT('',#92491);
#16105=VERTEX_POINT('',#92495);
#16106=VERTEX_POINT('',#92496);
#16107=VERTEX_POINT('',#92501);
#16108=VERTEX_POINT('',#92502);
#16109=VERTEX_POINT('',#92507);
#16110=VERTEX_POINT('',#92508);
#16111=VERTEX_POINT('',#92513);
#16112=VERTEX_POINT('',#92514);
#16113=VERTEX_POINT('',#92519);
#16114=VERTEX_POINT('',#92521);
#16115=VERTEX_POINT('',#92525);
#16116=VERTEX_POINT('',#92526);
#16117=VERTEX_POINT('',#92534);
#16118=VERTEX_POINT('',#92535);
#16119=VERTEX_POINT('',#92612);
#16120=VERTEX_POINT('',#92614);
#16121=VERTEX_POINT('',#92675);
#16122=VERTEX_POINT('',#92677);
#16123=VERTEX_POINT('',#92681);
#16124=VERTEX_POINT('',#92682);
#16125=VERTEX_POINT('',#92756);
#16126=VERTEX_POINT('',#92758);
#16127=VERTEX_POINT('',#92828);
#16128=VERTEX_POINT('',#92832);
#16129=VERTEX_POINT('',#92833);
#16130=VERTEX_POINT('',#92949);
#16131=VERTEX_POINT('',#92953);
#16132=VERTEX_POINT('',#92957);
#16133=VERTEX_POINT('',#92964);
#16134=VERTEX_POINT('',#92965);
#16135=VERTEX_POINT('',#93027);
#16136=VERTEX_POINT('',#93029);
#16137=VERTEX_POINT('',#93033);
#16138=VERTEX_POINT('',#93035);
#16139=VERTEX_POINT('',#93039);
#16140=VERTEX_POINT('',#93040);
#16141=VERTEX_POINT('',#93045);
#16142=VERTEX_POINT('',#93047);
#16143=VERTEX_POINT('',#93051);
#16144=VERTEX_POINT('',#93055);
#16145=VERTEX_POINT('',#93059);
#16146=VERTEX_POINT('',#93165);
#16147=VERTEX_POINT('',#93217);
#16148=VERTEX_POINT('',#93218);
#16149=VERTEX_POINT('',#93220);
#16150=VERTEX_POINT('',#93222);
#16151=VERTEX_POINT('',#93226);
#16152=VERTEX_POINT('',#93228);
#16153=VERTEX_POINT('',#93232);
#16154=VERTEX_POINT('',#93233);
#16155=VERTEX_POINT('',#93237);
#16156=VERTEX_POINT('',#93239);
#16157=VERTEX_POINT('',#93243);
#16158=VERTEX_POINT('',#93245);
#16159=VERTEX_POINT('',#93249);
#16160=VERTEX_POINT('',#93251);
#16161=VERTEX_POINT('',#93255);
#16162=VERTEX_POINT('',#93257);
#16163=VERTEX_POINT('',#93261);
#16164=VERTEX_POINT('',#93265);
#16165=VERTEX_POINT('',#93269);
#16166=VERTEX_POINT('',#93273);
#16167=VERTEX_POINT('',#93279);
#16168=VERTEX_POINT('',#93283);
#16169=VERTEX_POINT('',#93287);
#16170=VERTEX_POINT('',#93291);
#16171=VERTEX_POINT('',#93295);
#16172=VERTEX_POINT('',#93299);
#16173=VERTEX_POINT('',#93303);
#16174=VERTEX_POINT('',#93307);
#16175=VERTEX_POINT('',#93314);
#16176=VERTEX_POINT('',#93316);
#16177=VERTEX_POINT('',#93319);
#16178=VERTEX_POINT('',#93524);
#16179=VERTEX_POINT('',#93526);
#16180=VERTEX_POINT('',#93530);
#16181=VERTEX_POINT('',#93532);
#16182=VERTEX_POINT('',#93630);
#16183=VERTEX_POINT('',#93750);
#16184=VERTEX_POINT('',#93823);
#16185=VERTEX_POINT('',#93825);
#16186=VERTEX_POINT('',#93840);
#16187=VERTEX_POINT('',#93844);
#16188=VERTEX_POINT('',#93846);
#16189=VERTEX_POINT('',#93848);
#16190=VERTEX_POINT('',#93850);
#16191=VERTEX_POINT('',#93852);
#16192=VERTEX_POINT('',#93856);
#16193=VERTEX_POINT('',#93859);
#16194=VERTEX_POINT('',#93865);
#16195=VERTEX_POINT('',#93994);
#16196=VERTEX_POINT('',#94018);
#16197=VERTEX_POINT('',#94020);
#16198=VERTEX_POINT('',#94024);
#16199=VERTEX_POINT('',#94025);
#16200=VERTEX_POINT('',#94063);
#16201=VERTEX_POINT('',#94065);
#16202=VERTEX_POINT('',#94072);
#16203=VERTEX_POINT('',#94076);
#16204=VERTEX_POINT('',#94080);
#16205=VERTEX_POINT('',#94111);
#16206=VERTEX_POINT('',#94115);
#16207=VERTEX_POINT('',#94119);
#16208=VERTEX_POINT('',#94123);
#16209=VERTEX_POINT('',#94131);
#16210=VERTEX_POINT('',#94213);
#16211=VERTEX_POINT('',#94218);
#16212=VERTEX_POINT('',#94219);
#16213=VERTEX_POINT('',#94409);
#16214=VERTEX_POINT('',#94410);
#16215=VERTEX_POINT('',#94412);
#16216=VERTEX_POINT('',#94423);
#16217=VERTEX_POINT('',#94424);
#16218=VERTEX_POINT('',#94429);
#16219=VERTEX_POINT('',#94433);
#16220=VERTEX_POINT('',#94437);
#16221=VERTEX_POINT('',#94441);
#16222=VERTEX_POINT('',#94446);
#16223=VERTEX_POINT('',#94450);
#16224=VERTEX_POINT('',#94453);
#16225=VERTEX_POINT('',#94456);
#16226=VERTEX_POINT('',#94623);
#16227=VERTEX_POINT('',#94690);
#16228=VERTEX_POINT('',#94809);
#16229=VERTEX_POINT('',#94830);
#16230=VERTEX_POINT('',#94834);
#16231=VERTEX_POINT('',#94838);
#16232=VERTEX_POINT('',#94842);
#16233=VERTEX_POINT('',#94846);
#16234=VERTEX_POINT('',#94903);
#16235=VERTEX_POINT('',#94915);
#16236=VERTEX_POINT('',#94919);
#16237=VERTEX_POINT('',#94925);
#16238=VERTEX_POINT('',#94929);
#16239=VERTEX_POINT('',#94968);
#16240=VERTEX_POINT('',#94970);
#16241=VERTEX_POINT('',#95056);
#16242=VERTEX_POINT('',#95113);
#16243=VERTEX_POINT('',#95196);
#16244=VERTEX_POINT('',#95248);
#16245=VERTEX_POINT('',#95250);
#16246=VERTEX_POINT('',#95254);
#16247=VERTEX_POINT('',#95260);
#16248=VERTEX_POINT('',#95266);
#16249=VERTEX_POINT('',#95270);
#16250=VERTEX_POINT('',#95274);
#16251=VERTEX_POINT('',#95282);
#16252=VERTEX_POINT('',#95288);
#16253=VERTEX_POINT('',#95290);
#16254=VERTEX_POINT('',#95292);
#16255=VERTEX_POINT('',#95294);
#16256=VERTEX_POINT('',#95296);
#16257=VERTEX_POINT('',#95298);
#16258=VERTEX_POINT('',#95302);
#16259=VERTEX_POINT('',#95303);
#16260=VERTEX_POINT('',#95379);
#16261=VERTEX_POINT('',#95411);
#16262=VERTEX_POINT('',#95542);
#16263=VERTEX_POINT('',#95546);
#16264=VERTEX_POINT('',#95550);
#16265=VERTEX_POINT('',#95554);
#16266=VERTEX_POINT('',#95558);
#16267=VERTEX_POINT('',#95562);
#16268=VERTEX_POINT('',#95601);
#16269=VERTEX_POINT('',#95692);
#16270=VERTEX_POINT('',#95694);
#16271=VERTEX_POINT('',#95698);
#16272=VERTEX_POINT('',#95704);
#16273=VERTEX_POINT('',#95708);
#16274=VERTEX_POINT('',#95712);
#16275=VERTEX_POINT('',#95716);
#16276=VERTEX_POINT('',#95720);
#16277=VERTEX_POINT('',#95724);
#16278=VERTEX_POINT('',#95728);
#16279=VERTEX_POINT('',#95732);
#16280=VERTEX_POINT('',#95738);
#16281=VERTEX_POINT('',#95742);
#16282=VERTEX_POINT('',#95746);
#16283=VERTEX_POINT('',#95750);
#16284=VERTEX_POINT('',#95756);
#16285=VERTEX_POINT('',#95760);
#16286=VERTEX_POINT('',#95766);
#16287=VERTEX_POINT('',#95772);
#16288=VERTEX_POINT('',#95780);
#16289=VERTEX_POINT('',#95784);
#16290=VERTEX_POINT('',#95788);
#16291=VERTEX_POINT('',#95796);
#16292=VERTEX_POINT('',#95797);
#16293=VERTEX_POINT('',#95799);
#16294=VERTEX_POINT('',#95801);
#16295=VERTEX_POINT('',#95805);
#16296=VERTEX_POINT('',#95806);
#16297=VERTEX_POINT('',#95808);
#16298=VERTEX_POINT('',#95810);
#16299=VERTEX_POINT('',#95814);
#16300=VERTEX_POINT('',#95816);
#16301=VERTEX_POINT('',#95820);
#16302=VERTEX_POINT('',#95822);
#16303=VERTEX_POINT('',#95826);
#16304=VERTEX_POINT('',#95882);
#16305=VERTEX_POINT('',#95947);
#16306=VERTEX_POINT('',#95951);
#16307=VERTEX_POINT('',#95952);
#16308=VERTEX_POINT('',#95955);
#16309=VERTEX_POINT('',#95959);
#16310=VERTEX_POINT('',#95963);
#16311=VERTEX_POINT('',#95967);
#16312=VERTEX_POINT('',#95975);
#16313=VERTEX_POINT('',#95979);
#16314=VERTEX_POINT('',#95983);
#16315=VERTEX_POINT('',#95987);
#16316=VERTEX_POINT('',#95989);
#16317=VERTEX_POINT('',#96082);
#16318=VERTEX_POINT('',#96083);
#16319=VERTEX_POINT('',#96085);
#16320=VERTEX_POINT('',#96087);
#16321=VERTEX_POINT('',#96089);
#16322=VERTEX_POINT('',#96093);
#16323=VERTEX_POINT('',#96094);
#16324=VERTEX_POINT('',#96123);
#16325=VERTEX_POINT('',#96127);
#16326=VERTEX_POINT('',#96128);
#16327=VERTEX_POINT('',#96133);
#16328=VERTEX_POINT('',#96135);
#16329=VERTEX_POINT('',#96141);
#16330=VERTEX_POINT('',#96145);
#16331=VERTEX_POINT('',#96149);
#16332=VERTEX_POINT('',#96187);
#16333=VERTEX_POINT('',#96193);
#16334=VERTEX_POINT('',#96197);
#16335=VERTEX_POINT('',#96201);
#16336=VERTEX_POINT('',#96202);
#16337=VERTEX_POINT('',#96204);
#16338=VERTEX_POINT('',#96206);
#16339=VERTEX_POINT('',#96208);
#16340=VERTEX_POINT('',#96212);
#16341=VERTEX_POINT('',#96222);
#16342=VERTEX_POINT('',#96226);
#16343=VERTEX_POINT('',#96227);
#16344=VERTEX_POINT('',#96232);
#16345=VERTEX_POINT('',#96239);
#16346=VERTEX_POINT('',#96245);
#16347=VERTEX_POINT('',#96256);
#16348=VERTEX_POINT('',#96272);
#16349=VERTEX_POINT('',#96278);
#16350=VERTEX_POINT('',#96282);
#16351=VERTEX_POINT('',#96286);
#16352=VERTEX_POINT('',#96287);
#16353=VERTEX_POINT('',#96289);
#16354=VERTEX_POINT('',#96291);
#16355=VERTEX_POINT('',#96295);
#16356=VERTEX_POINT('',#96330);
#16357=VERTEX_POINT('',#96334);
#16358=VERTEX_POINT('',#96335);
#16359=VERTEX_POINT('',#96337);
#16360=VERTEX_POINT('',#96339);
#16361=VERTEX_POINT('',#96342);
#16362=VERTEX_POINT('',#96344);
#16363=VERTEX_POINT('',#96348);
#16364=VERTEX_POINT('',#96350);
#16365=VERTEX_POINT('',#96356);
#16366=VERTEX_POINT('',#96360);
#16367=VERTEX_POINT('',#96364);
#16368=VERTEX_POINT('',#96368);
#16369=VERTEX_POINT('',#96372);
#16370=VERTEX_POINT('',#96376);
#16371=VERTEX_POINT('',#96380);
#16372=VERTEX_POINT('',#96402);
#16373=VERTEX_POINT('',#96408);
#16374=VERTEX_POINT('',#96412);
#16375=VERTEX_POINT('',#96416);
#16376=VERTEX_POINT('',#96417);
#16377=VERTEX_POINT('',#96419);
#16378=VERTEX_POINT('',#96421);
#16379=VERTEX_POINT('',#96423);
#16380=VERTEX_POINT('',#96425);
#16381=VERTEX_POINT('',#96429);
#16382=VERTEX_POINT('',#96431);
#16383=VERTEX_POINT('',#96435);
#16384=VERTEX_POINT('',#96439);
#16385=VERTEX_POINT('',#96443);
#16386=VERTEX_POINT('',#96447);
#16387=VERTEX_POINT('',#96451);
#16388=VERTEX_POINT('',#96453);
#16389=VERTEX_POINT('',#96459);
#16390=VERTEX_POINT('',#96463);
#16391=VERTEX_POINT('',#96467);
#16392=VERTEX_POINT('',#96469);
#16393=VERTEX_POINT('',#96473);
#16394=VERTEX_POINT('',#96477);
#16395=VERTEX_POINT('',#96481);
#16396=VERTEX_POINT('',#96485);
#16397=VERTEX_POINT('',#96489);
#16398=VERTEX_POINT('',#96493);
#16399=VERTEX_POINT('',#96501);
#16400=VERTEX_POINT('',#96504);
#16401=VERTEX_POINT('',#96507);
#16402=VERTEX_POINT('',#96509);
#16403=VERTEX_POINT('',#96511);
#16404=VERTEX_POINT('',#96597);
#16405=VERTEX_POINT('',#96599);
#16406=VERTEX_POINT('',#96613);
#16407=VERTEX_POINT('',#96675);
#16408=VERTEX_POINT('',#96687);
#16409=VERTEX_POINT('',#96694);
#16410=VERTEX_POINT('',#96700);
#16411=VERTEX_POINT('',#96701);
#16412=VERTEX_POINT('',#96703);
#16413=VERTEX_POINT('',#96708);
#16414=VERTEX_POINT('',#96711);
#16415=VERTEX_POINT('',#96796);
#16416=VERTEX_POINT('',#96798);
#16417=VERTEX_POINT('',#96837);
#16418=VERTEX_POINT('',#96894);
#16419=VERTEX_POINT('',#96946);
#16420=VERTEX_POINT('',#96948);
#16421=VERTEX_POINT('',#97003);
#16422=VERTEX_POINT('',#97005);
#16423=VERTEX_POINT('',#97060);
#16424=VERTEX_POINT('',#97063);
#16425=VERTEX_POINT('',#97066);
#16426=VERTEX_POINT('',#97067);
#16427=VERTEX_POINT('',#97069);
#16428=VERTEX_POINT('',#97076);
#16429=VERTEX_POINT('',#97133);
#16430=VERTEX_POINT('',#97183);
#16431=VERTEX_POINT('',#97240);
#16432=VERTEX_POINT('',#97332);
#16433=VERTEX_POINT('',#97333);
#16434=VERTEX_POINT('',#97335);
#16435=VERTEX_POINT('',#97337);
#16436=VERTEX_POINT('',#97339);
#16437=VERTEX_POINT('',#97341);
#16438=VERTEX_POINT('',#97345);
#16439=VERTEX_POINT('',#97346);
#16440=VERTEX_POINT('',#97348);
#16441=VERTEX_POINT('',#97350);
#16442=VERTEX_POINT('',#97352);
#16443=VERTEX_POINT('',#97356);
#16444=VERTEX_POINT('',#97358);
#16445=VERTEX_POINT('',#97362);
#16446=VERTEX_POINT('',#97366);
#16447=VERTEX_POINT('',#97370);
#16448=VERTEX_POINT('',#97374);
#16449=VERTEX_POINT('',#97375);
#16450=VERTEX_POINT('',#97377);
#16451=VERTEX_POINT('',#97379);
#16452=VERTEX_POINT('',#97383);
#16453=VERTEX_POINT('',#97384);
#16454=VERTEX_POINT('',#97389);
#16455=VERTEX_POINT('',#97393);
#16456=VERTEX_POINT('',#97397);
#16457=VERTEX_POINT('',#97400);
#16458=VERTEX_POINT('',#97404);
#16459=VERTEX_POINT('',#97406);
#16460=VERTEX_POINT('',#97408);
#16461=VERTEX_POINT('',#97410);
#16462=VERTEX_POINT('',#97412);
#16463=VERTEX_POINT('',#97414);
#16464=VERTEX_POINT('',#97416);
#16465=VERTEX_POINT('',#97418);
#16466=VERTEX_POINT('',#97420);
#16467=VERTEX_POINT('',#97422);
#16468=VERTEX_POINT('',#97424);
#16469=VERTEX_POINT('',#97426);
#16470=VERTEX_POINT('',#97428);
#16471=VERTEX_POINT('',#97430);
#16472=VERTEX_POINT('',#97432);
#16473=VERTEX_POINT('',#97434);
#16474=VERTEX_POINT('',#97436);
#16475=VERTEX_POINT('',#97438);
#16476=VERTEX_POINT('',#97440);
#16477=VERTEX_POINT('',#97442);
#16478=VERTEX_POINT('',#97444);
#16479=VERTEX_POINT('',#97446);
#16480=VERTEX_POINT('',#97448);
#16481=VERTEX_POINT('',#97450);
#16482=VERTEX_POINT('',#97452);
#16483=VERTEX_POINT('',#97454);
#16484=VERTEX_POINT('',#97456);
#16485=VERTEX_POINT('',#97458);
#16486=VERTEX_POINT('',#97462);
#16487=VERTEX_POINT('',#97463);
#16488=VERTEX_POINT('',#97479);
#16489=VERTEX_POINT('',#97481);
#16490=VERTEX_POINT('',#97483);
#16491=VERTEX_POINT('',#97485);
#16492=VERTEX_POINT('',#97487);
#16493=VERTEX_POINT('',#97489);
#16494=VERTEX_POINT('',#97491);
#16495=VERTEX_POINT('',#97493);
#16496=VERTEX_POINT('',#97495);
#16497=VERTEX_POINT('',#97497);
#16498=VERTEX_POINT('',#97499);
#16499=VERTEX_POINT('',#97503);
#16500=VERTEX_POINT('',#97507);
#16501=VERTEX_POINT('',#97508);
#16502=VERTEX_POINT('',#97511);
#16503=VERTEX_POINT('',#97513);
#16504=VERTEX_POINT('',#97518);
#16505=VERTEX_POINT('',#97519);
#16506=VERTEX_POINT('',#97557);
#16507=VERTEX_POINT('',#97561);
#16508=VERTEX_POINT('',#97562);
#16509=VERTEX_POINT('',#97564);
#16510=VERTEX_POINT('',#97566);
#16511=VERTEX_POINT('',#97568);
#16512=VERTEX_POINT('',#97570);
#16513=VERTEX_POINT('',#97574);
#16514=VERTEX_POINT('',#97578);
#16515=VERTEX_POINT('',#97582);
#16516=VERTEX_POINT('',#97595);
#16517=VERTEX_POINT('',#97601);
#16518=VERTEX_POINT('',#97602);
#16519=VERTEX_POINT('',#97604);
#16520=VERTEX_POINT('',#97608);
#16521=VERTEX_POINT('',#97610);
#16522=VERTEX_POINT('',#97612);
#16523=VERTEX_POINT('',#97616);
#16524=VERTEX_POINT('',#97620);
#16525=VERTEX_POINT('',#97635);
#16526=VERTEX_POINT('',#97636);
#16527=VERTEX_POINT('',#97638);
#16528=VERTEX_POINT('',#97640);
#16529=VERTEX_POINT('',#97642);
#16530=VERTEX_POINT('',#97646);
#16531=VERTEX_POINT('',#97650);
#16532=VERTEX_POINT('',#97663);
#16533=VERTEX_POINT('',#97669);
#16534=VERTEX_POINT('',#97670);
#16535=VERTEX_POINT('',#97672);
#16536=VERTEX_POINT('',#97676);
#16537=VERTEX_POINT('',#97678);
#16538=VERTEX_POINT('',#97680);
#16539=VERTEX_POINT('',#97682);
#16540=VERTEX_POINT('',#97686);
#16541=VERTEX_POINT('',#97690);
#16542=VERTEX_POINT('',#97703);
#16543=VERTEX_POINT('',#97709);
#16544=VERTEX_POINT('',#97710);
#16545=VERTEX_POINT('',#97714);
#16546=VERTEX_POINT('',#97715);
#16547=VERTEX_POINT('',#97725);
#16548=VERTEX_POINT('',#97726);
#16549=VERTEX_POINT('',#97728);
#16550=VERTEX_POINT('',#97730);
#16551=VERTEX_POINT('',#97738);
#16552=VERTEX_POINT('',#97739);
#16553=VERTEX_POINT('',#97744);
#16554=VERTEX_POINT('',#97748);
#16555=VERTEX_POINT('',#97754);
#16556=VERTEX_POINT('',#97756);
#16557=VERTEX_POINT('',#97758);
#16558=VERTEX_POINT('',#97797);
#16559=VERTEX_POINT('',#97798);
#16560=VERTEX_POINT('',#97800);
#16561=VERTEX_POINT('',#97804);
#16562=VERTEX_POINT('',#97806);
#16563=VERTEX_POINT('',#97810);
#16564=VERTEX_POINT('',#97821);
#16565=VERTEX_POINT('',#97825);
#16566=VERTEX_POINT('',#97826);
#16567=VERTEX_POINT('',#97831);
#16568=VERTEX_POINT('',#97832);
#16569=VERTEX_POINT('',#97834);
#16570=VERTEX_POINT('',#97836);
#16571=VERTEX_POINT('',#97840);
#16572=VERTEX_POINT('',#97851);
#16573=VERTEX_POINT('',#97855);
#16574=VERTEX_POINT('',#97857);
#16575=VERTEX_POINT('',#97861);
#16576=VERTEX_POINT('',#97865);
#16577=VERTEX_POINT('',#97866);
#16578=VERTEX_POINT('',#97868);
#16579=VERTEX_POINT('',#97872);
#16580=VERTEX_POINT('',#97883);
#16581=VERTEX_POINT('',#97887);
#16582=VERTEX_POINT('',#97889);
#16583=VERTEX_POINT('',#97893);
#16584=VERTEX_POINT('',#97894);
#16585=VERTEX_POINT('',#97896);
#16586=VERTEX_POINT('',#97900);
#16587=VERTEX_POINT('',#97901);
#16588=VERTEX_POINT('',#97915);
#16589=VERTEX_POINT('',#97917);
#16590=VERTEX_POINT('',#97921);
#16591=VERTEX_POINT('',#97923);
#16592=VERTEX_POINT('',#97927);
#16593=VERTEX_POINT('',#97928);
#16594=VERTEX_POINT('',#97930);
#16595=VERTEX_POINT('',#97932);
#16596=VERTEX_POINT('',#97934);
#16597=VERTEX_POINT('',#97936);
#16598=VERTEX_POINT('',#97938);
#16599=VERTEX_POINT('',#97940);
#16600=VERTEX_POINT('',#97942);
#16601=VERTEX_POINT('',#97944);
#16602=VERTEX_POINT('',#97946);
#16603=VERTEX_POINT('',#97948);
#16604=VERTEX_POINT('',#97950);
#16605=VERTEX_POINT('',#97952);
#16606=VERTEX_POINT('',#97954);
#16607=VERTEX_POINT('',#97956);
#16608=VERTEX_POINT('',#97958);
#16609=VERTEX_POINT('',#97960);
#16610=VERTEX_POINT('',#97962);
#16611=VERTEX_POINT('',#97964);
#16612=VERTEX_POINT('',#97966);
#16613=VERTEX_POINT('',#97968);
#16614=VERTEX_POINT('',#97970);
#16615=VERTEX_POINT('',#97972);
#16616=VERTEX_POINT('',#97974);
#16617=VERTEX_POINT('',#97976);
#16618=VERTEX_POINT('',#97980);
#16619=VERTEX_POINT('',#97982);
#16620=VERTEX_POINT('',#97984);
#16621=VERTEX_POINT('',#97986);
#16622=VERTEX_POINT('',#97990);
#16623=VERTEX_POINT('',#97992);
#16624=VERTEX_POINT('',#97996);
#16625=VERTEX_POINT('',#98000);
#16626=VERTEX_POINT('',#98004);
#16627=VERTEX_POINT('',#98008);
#16628=VERTEX_POINT('',#98012);
#16629=VERTEX_POINT('',#98016);
#16630=VERTEX_POINT('',#98020);
#16631=VERTEX_POINT('',#98024);
#16632=VERTEX_POINT('',#98028);
#16633=VERTEX_POINT('',#98032);
#16634=VERTEX_POINT('',#98036);
#16635=VERTEX_POINT('',#98040);
#16636=VERTEX_POINT('',#98044);
#16637=VERTEX_POINT('',#98048);
#16638=VERTEX_POINT('',#98052);
#16639=VERTEX_POINT('',#98056);
#16640=VERTEX_POINT('',#98060);
#16641=VERTEX_POINT('',#98064);
#16642=VERTEX_POINT('',#98068);
#16643=VERTEX_POINT('',#98072);
#16644=VERTEX_POINT('',#98076);
#16645=VERTEX_POINT('',#98080);
#16646=VERTEX_POINT('',#98084);
#16647=VERTEX_POINT('',#98088);
#16648=VERTEX_POINT('',#98094);
#16649=VERTEX_POINT('',#98100);
#16650=VERTEX_POINT('',#98106);
#16651=VERTEX_POINT('',#98112);
#16652=VERTEX_POINT('',#98115);
#16653=VERTEX_POINT('',#98122);
#16654=VERTEX_POINT('',#98128);
#16655=VERTEX_POINT('',#98134);
#16656=VERTEX_POINT('',#98140);
#16657=VERTEX_POINT('',#98181);
#16658=VERTEX_POINT('',#98183);
#16659=VERTEX_POINT('',#98202);
#16660=VERTEX_POINT('',#98243);
#16661=VERTEX_POINT('',#98259);
#16662=VERTEX_POINT('',#98263);
#16663=EDGE_CURVE('',#13625,#13626,#11317,.T.);
#16664=EDGE_CURVE('',#13625,#13627,#7637,.T.);
#16665=EDGE_CURVE('',#13627,#13627,#11318,.T.);
#16666=EDGE_CURVE('',#13626,#13625,#11319,.T.);
#16667=EDGE_CURVE('',#13628,#13629,#11320,.T.);
#16668=EDGE_CURVE('',#13628,#13626,#7638,.T.);
#16669=EDGE_CURVE('',#13629,#13628,#11321,.T.);
#16670=EDGE_CURVE('',#13629,#13630,#7639,.T.);
#16671=EDGE_CURVE('',#13630,#13630,#11322,.T.);
#16672=EDGE_CURVE('',#13631,#13632,#7640,.T.);
#16673=EDGE_CURVE('',#13631,#13633,#11323,.T.);
#16674=EDGE_CURVE('',#13633,#13634,#7641,.T.);
#16675=EDGE_CURVE('',#13632,#13634,#11324,.T.);
#16676=EDGE_CURVE('',#13635,#13636,#7642,.T.);
#16677=EDGE_CURVE('',#13636,#13637,#11325,.T.);
#16678=EDGE_CURVE('',#13637,#13638,#11326,.T.);
#16679=EDGE_CURVE('',#13638,#13639,#11327,.T.);
#16680=EDGE_CURVE('',#13639,#13640,#7643,.T.);
#16681=EDGE_CURVE('',#13640,#13641,#11328,.T.);
#16682=EDGE_CURVE('',#13641,#13642,#7644,.T.);
#16683=EDGE_CURVE('',#13642,#13643,#11329,.T.);
#16684=EDGE_CURVE('',#13643,#13644,#7645,.T.);
#16685=EDGE_CURVE('',#13644,#13645,#11330,.T.);
#16686=EDGE_CURVE('',#13645,#13646,#11331,.T.);
#16687=EDGE_CURVE('',#13646,#13647,#11332,.T.);
#16688=EDGE_CURVE('',#13647,#13648,#7646,.T.);
#16689=EDGE_CURVE('',#13648,#13649,#11333,.T.);
#16690=EDGE_CURVE('',#13649,#13650,#7647,.T.);
#16691=EDGE_CURVE('',#13650,#13651,#11334,.T.);
#16692=EDGE_CURVE('',#13651,#13652,#7648,.T.);
#16693=EDGE_CURVE('',#13652,#13653,#11335,.T.);
#16694=EDGE_CURVE('',#13653,#13654,#11336,.T.);
#16695=EDGE_CURVE('',#13654,#13655,#11337,.T.);
#16696=EDGE_CURVE('',#13655,#13656,#7649,.T.);
#16697=EDGE_CURVE('',#13656,#13657,#11338,.T.);
#16698=EDGE_CURVE('',#13657,#13658,#11339,.T.);
#16699=EDGE_CURVE('',#13658,#13659,#11340,.T.);
#16700=EDGE_CURVE('',#13659,#13660,#7650,.T.);
#16701=EDGE_CURVE('',#13660,#13661,#11341,.T.);
#16702=EDGE_CURVE('',#13661,#13662,#7651,.T.);
#16703=EDGE_CURVE('',#13662,#13663,#11342,.T.);
#16704=EDGE_CURVE('',#13663,#13664,#7652,.T.);
#16705=EDGE_CURVE('',#13664,#13665,#11343,.T.);
#16706=EDGE_CURVE('',#13665,#13666,#11344,.T.);
#16707=EDGE_CURVE('',#13666,#13667,#11345,.T.);
#16708=EDGE_CURVE('',#13667,#13668,#7653,.T.);
#16709=EDGE_CURVE('',#13668,#13669,#11346,.T.);
#16710=EDGE_CURVE('',#13669,#13670,#7654,.T.);
#16711=EDGE_CURVE('',#13670,#13671,#11347,.T.);
#16712=EDGE_CURVE('',#13671,#13672,#7655,.T.);
#16713=EDGE_CURVE('',#13672,#13673,#11348,.T.);
#16714=EDGE_CURVE('',#13673,#13674,#11349,.T.);
#16715=EDGE_CURVE('',#13674,#13635,#11350,.T.);
#16716=EDGE_CURVE('',#13675,#13676,#11351,.T.);
#16717=EDGE_CURVE('',#13677,#13676,#1332,.T.);
#16718=EDGE_CURVE('',#13678,#13677,#1333,.T.);
#16719=EDGE_CURVE('',#13679,#13678,#1334,.T.);
#16720=EDGE_CURVE('',#13679,#13680,#1335,.T.);
#16721=EDGE_CURVE('',#13681,#13680,#1336,.T.);
#16722=EDGE_CURVE('',#13681,#13682,#11352,.T.);
#16723=EDGE_CURVE('',#13683,#13682,#7656,.T.);
#16724=EDGE_CURVE('',#13683,#13684,#11353,.T.);
#16725=EDGE_CURVE('',#13675,#13684,#1337,.T.);
#16726=EDGE_CURVE('',#13685,#13686,#11354,.T.);
#16727=EDGE_CURVE('',#13687,#13686,#11355,.T.);
#16728=EDGE_CURVE('',#13688,#13687,#11356,.T.);
#16729=EDGE_CURVE('',#13688,#13632,#7657,.T.);
#16730=EDGE_CURVE('',#13689,#13634,#11357,.T.);
#16731=EDGE_CURVE('',#13689,#13690,#11358,.T.);
#16732=EDGE_CURVE('',#13691,#13690,#11359,.T.);
#16733=EDGE_CURVE('',#13685,#13691,#7658,.T.);
#16734=EDGE_CURVE('',#13692,#13693,#7659,.T.);
#16735=EDGE_CURVE('',#13694,#13693,#11360,.T.);
#16736=EDGE_CURVE('',#13694,#13695,#1338,.T.);
#16737=EDGE_CURVE('',#13696,#13695,#1339,.T.);
#16738=EDGE_CURVE('',#13696,#13697,#1340,.T.);
#16739=EDGE_CURVE('',#13697,#13698,#1341,.T.);
#16740=EDGE_CURVE('',#13698,#13699,#1342,.T.);
#16741=EDGE_CURVE('',#13700,#13699,#11361,.T.);
#16742=EDGE_CURVE('',#13700,#13701,#1343,.T.);
#16743=EDGE_CURVE('',#13692,#13701,#11362,.T.);
#16744=EDGE_CURVE('',#13702,#13703,#7660,.T.);
#16745=EDGE_CURVE('',#13703,#13704,#1344,.T.);
#16746=EDGE_CURVE('',#13705,#13704,#7661,.T.);
#16747=EDGE_CURVE('',#13706,#13705,#1345,.T.);
#16748=EDGE_CURVE('',#13702,#13706,#1346,.T.);
#16749=EDGE_CURVE('',#13631,#13707,#11363,.T.);
#16750=EDGE_CURVE('',#13633,#13707,#11364,.T.);
#16751=EDGE_CURVE('',#13708,#13709,#7662,.T.);
#16752=EDGE_CURVE('',#13709,#13710,#7663,.T.);
#16753=EDGE_CURVE('',#13711,#13710,#7664,.T.);
#16754=EDGE_CURVE('',#13708,#13711,#7665,.T.);
#16755=EDGE_CURVE('',#13684,#13712,#7666,.T.);
#16756=EDGE_CURVE('',#13713,#13712,#1347,.T.);
#16757=EDGE_CURVE('',#13675,#13713,#7667,.T.);
#16758=EDGE_CURVE('',#13683,#13714,#7668,.T.);
#16759=EDGE_CURVE('',#13715,#13714,#1348,.T.);
#16760=EDGE_CURVE('',#13712,#13715,#449,.T.);
#16761=EDGE_CURVE('',#13682,#13716,#7669,.T.);
#16762=EDGE_CURVE('',#13714,#13716,#7670,.T.);
#16763=EDGE_CURVE('',#13681,#13717,#7671,.T.);
#16764=EDGE_CURVE('',#13718,#13717,#450,.T.);
#16765=EDGE_CURVE('',#13719,#13718,#1349,.T.);
#16766=EDGE_CURVE('',#13716,#13719,#451,.T.);
#16767=EDGE_CURVE('',#13680,#13720,#7672,.T.);
#16768=EDGE_CURVE('',#13721,#13720,#1350,.T.);
#16769=EDGE_CURVE('',#13722,#13721,#452,.T.);
#16770=EDGE_CURVE('',#13723,#13722,#1351,.T.);
#16771=EDGE_CURVE('',#13717,#13723,#11365,.T.);
#16772=EDGE_CURVE('',#13679,#13724,#7673,.T.);
#16773=EDGE_CURVE('',#13725,#13724,#1352,.T.);
#16774=EDGE_CURVE('',#13720,#13725,#1353,.T.);
#16775=EDGE_CURVE('',#13678,#13726,#7674,.T.);
#16776=EDGE_CURVE('',#13727,#13726,#1354,.T.);
#16777=EDGE_CURVE('',#13728,#13727,#1355,.T.);
#16778=EDGE_CURVE('',#13729,#13728,#1356,.T.);
#16779=EDGE_CURVE('',#13724,#13729,#453,.T.);
#16780=EDGE_CURVE('',#13677,#13730,#7675,.T.);
#16781=EDGE_CURVE('',#13730,#13731,#1357,.T.);
#16782=EDGE_CURVE('',#13726,#13731,#1358,.T.);
#16783=EDGE_CURVE('',#13676,#13732,#7676,.T.);
#16784=EDGE_CURVE('',#13733,#13732,#1359,.T.);
#16785=EDGE_CURVE('',#13733,#13730,#1360,.T.);
#16786=EDGE_CURVE('',#13734,#13713,#454,.T.);
#16787=EDGE_CURVE('',#13735,#13734,#1361,.T.);
#16788=EDGE_CURVE('',#13732,#13735,#1362,.T.);
#16789=EDGE_CURVE('',#13701,#13736,#7677,.T.);
#16790=EDGE_CURVE('',#13736,#13737,#455,.T.);
#16791=EDGE_CURVE('',#13737,#13738,#1363,.T.);
#16792=EDGE_CURVE('',#13692,#13738,#7678,.T.);
#16793=EDGE_CURVE('',#13700,#13739,#7679,.T.);
#16794=EDGE_CURVE('',#13739,#13736,#1364,.T.);
#16795=EDGE_CURVE('',#13699,#13740,#7680,.T.);
#16796=EDGE_CURVE('',#13740,#13741,#1365,.T.);
#16797=EDGE_CURVE('',#13741,#13742,#1366,.T.);
#16798=EDGE_CURVE('',#13742,#13739,#456,.T.);
#16799=EDGE_CURVE('',#13698,#13743,#7681,.T.);
#16800=EDGE_CURVE('',#13744,#13743,#1367,.T.);
#16801=EDGE_CURVE('',#13744,#13740,#1368,.T.);
#16802=EDGE_CURVE('',#13697,#13745,#7682,.T.);
#16803=EDGE_CURVE('',#13745,#13746,#1369,.T.);
#16804=EDGE_CURVE('',#13743,#13746,#1370,.T.);
#16805=EDGE_CURVE('',#13696,#13747,#7683,.T.);
#16806=EDGE_CURVE('',#13747,#13748,#457,.T.);
#16807=EDGE_CURVE('',#13748,#13749,#1371,.T.);
#16808=EDGE_CURVE('',#13749,#13750,#1372,.T.);
#16809=EDGE_CURVE('',#13750,#13745,#1373,.T.);
#16810=EDGE_CURVE('',#13695,#13751,#7684,.T.);
#16811=EDGE_CURVE('',#13751,#13752,#1374,.T.);
#16812=EDGE_CURVE('',#13752,#13747,#1375,.T.);
#16813=EDGE_CURVE('',#13694,#13753,#7685,.T.);
#16814=EDGE_CURVE('',#13753,#13754,#11366,.T.);
#16815=EDGE_CURVE('',#13754,#13755,#1376,.T.);
#16816=EDGE_CURVE('',#13755,#13756,#458,.T.);
#16817=EDGE_CURVE('',#13756,#13751,#1377,.T.);
#16818=EDGE_CURVE('',#13693,#13757,#7686,.T.);
#16819=EDGE_CURVE('',#13757,#13758,#459,.T.);
#16820=EDGE_CURVE('',#13758,#13759,#1378,.T.);
#16821=EDGE_CURVE('',#13759,#13753,#460,.T.);
#16822=EDGE_CURVE('',#13738,#13757,#7687,.T.);
#16823=EDGE_CURVE('',#13760,#13761,#11367,.T.);
#16824=EDGE_CURVE('',#13761,#13762,#7688,.T.);
#16825=EDGE_CURVE('',#13763,#13762,#11368,.T.);
#16826=EDGE_CURVE('',#13760,#13763,#7689,.T.);
#16827=EDGE_CURVE('',#13665,#13763,#11369,.T.);
#16828=EDGE_CURVE('',#13666,#13762,#11370,.T.);
#16829=EDGE_CURVE('',#13664,#13764,#11371,.T.);
#16830=EDGE_CURVE('',#13764,#13763,#11372,.T.);
#16831=EDGE_CURVE('',#13765,#13764,#7690,.T.);
#16832=EDGE_CURVE('',#13765,#13760,#11373,.T.);
#16833=EDGE_CURVE('',#13663,#13766,#11374,.T.);
#16834=EDGE_CURVE('',#13766,#13764,#7691,.T.);
#16835=EDGE_CURVE('',#13766,#13767,#7692,.T.);
#16836=EDGE_CURVE('',#13767,#13765,#7693,.T.);
#16837=EDGE_CURVE('',#13662,#13768,#11375,.T.);
#16838=EDGE_CURVE('',#13768,#13766,#11376,.T.);
#16839=EDGE_CURVE('',#13768,#13769,#7694,.T.);
#16840=EDGE_CURVE('',#13769,#13767,#11377,.T.);
#16841=EDGE_CURVE('',#13661,#13770,#11378,.T.);
#16842=EDGE_CURVE('',#13770,#13768,#7695,.T.);
#16843=EDGE_CURVE('',#13770,#13771,#7696,.T.);
#16844=EDGE_CURVE('',#13771,#13769,#7697,.T.);
#16845=EDGE_CURVE('',#13660,#13772,#11379,.T.);
#16846=EDGE_CURVE('',#13772,#13770,#11380,.T.);
#16847=EDGE_CURVE('',#13772,#13773,#7698,.T.);
#16848=EDGE_CURVE('',#13773,#13771,#11381,.T.);
#16849=EDGE_CURVE('',#13659,#13774,#11382,.T.);
#16850=EDGE_CURVE('',#13774,#13772,#7699,.T.);
#16851=EDGE_CURVE('',#13775,#13774,#7700,.T.);
#16852=EDGE_CURVE('',#13775,#13773,#7701,.T.);
#16853=EDGE_CURVE('',#13658,#13776,#11383,.T.);
#16854=EDGE_CURVE('',#13776,#13774,#11384,.T.);
#16855=EDGE_CURVE('',#13777,#13776,#7702,.T.);
#16856=EDGE_CURVE('',#13777,#13775,#11385,.T.);
#16857=EDGE_CURVE('',#13657,#13778,#11386,.T.);
#16858=EDGE_CURVE('',#13778,#13776,#11387,.T.);
#16859=EDGE_CURVE('',#13779,#13778,#7703,.T.);
#16860=EDGE_CURVE('',#13779,#13777,#11388,.T.);
#16861=EDGE_CURVE('',#13656,#13780,#11389,.T.);
#16862=EDGE_CURVE('',#13780,#13778,#11390,.T.);
#16863=EDGE_CURVE('',#13781,#13780,#7704,.T.);
#16864=EDGE_CURVE('',#13781,#13779,#11391,.T.);
#16865=EDGE_CURVE('',#13655,#13782,#11392,.T.);
#16866=EDGE_CURVE('',#13782,#13780,#7705,.T.);
#16867=EDGE_CURVE('',#13783,#13782,#7706,.T.);
#16868=EDGE_CURVE('',#13783,#13781,#7707,.T.);
#16869=EDGE_CURVE('',#13654,#13784,#11393,.T.);
#16870=EDGE_CURVE('',#13784,#13782,#11394,.T.);
#16871=EDGE_CURVE('',#13785,#13784,#7708,.T.);
#16872=EDGE_CURVE('',#13785,#13783,#11395,.T.);
#16873=EDGE_CURVE('',#13653,#13786,#11396,.T.);
#16874=EDGE_CURVE('',#13786,#13784,#11397,.T.);
#16875=EDGE_CURVE('',#13787,#13786,#7709,.T.);
#16876=EDGE_CURVE('',#13787,#13785,#11398,.T.);
#16877=EDGE_CURVE('',#13652,#13788,#11399,.T.);
#16878=EDGE_CURVE('',#13788,#13786,#11400,.T.);
#16879=EDGE_CURVE('',#13789,#13788,#7710,.T.);
#16880=EDGE_CURVE('',#13789,#13787,#11401,.T.);
#16881=EDGE_CURVE('',#13651,#13790,#11402,.T.);
#16882=EDGE_CURVE('',#13790,#13788,#7711,.T.);
#16883=EDGE_CURVE('',#13790,#13791,#7712,.T.);
#16884=EDGE_CURVE('',#13791,#13789,#7713,.T.);
#16885=EDGE_CURVE('',#13650,#13792,#11403,.T.);
#16886=EDGE_CURVE('',#13792,#13790,#11404,.T.);
#16887=EDGE_CURVE('',#13792,#13793,#7714,.T.);
#16888=EDGE_CURVE('',#13793,#13791,#11405,.T.);
#16889=EDGE_CURVE('',#13649,#13794,#11406,.T.);
#16890=EDGE_CURVE('',#13794,#13792,#7715,.T.);
#16891=EDGE_CURVE('',#13794,#13795,#7716,.T.);
#16892=EDGE_CURVE('',#13795,#13793,#7717,.T.);
#16893=EDGE_CURVE('',#13648,#13796,#11407,.T.);
#16894=EDGE_CURVE('',#13796,#13794,#11408,.T.);
#16895=EDGE_CURVE('',#13796,#13797,#7718,.T.);
#16896=EDGE_CURVE('',#13797,#13795,#11409,.T.);
#16897=EDGE_CURVE('',#13647,#13798,#11410,.T.);
#16898=EDGE_CURVE('',#13798,#13796,#7719,.T.);
#16899=EDGE_CURVE('',#13799,#13798,#7720,.T.);
#16900=EDGE_CURVE('',#13799,#13797,#7721,.T.);
#16901=EDGE_CURVE('',#13646,#13800,#11411,.T.);
#16902=EDGE_CURVE('',#13800,#13798,#11412,.T.);
#16903=EDGE_CURVE('',#13801,#13800,#7722,.T.);
#16904=EDGE_CURVE('',#13801,#13799,#11413,.T.);
#16905=EDGE_CURVE('',#13802,#13801,#11414,.T.);
#16906=EDGE_CURVE('',#13803,#13800,#11415,.T.);
#16907=EDGE_CURVE('',#13802,#13803,#7723,.T.);
#16908=EDGE_CURVE('',#13645,#13803,#11416,.T.);
#16909=EDGE_CURVE('',#13644,#13804,#11417,.T.);
#16910=EDGE_CURVE('',#13804,#13803,#11418,.T.);
#16911=EDGE_CURVE('',#13805,#13804,#7724,.T.);
#16912=EDGE_CURVE('',#13805,#13802,#11419,.T.);
#16913=EDGE_CURVE('',#13643,#13806,#11420,.T.);
#16914=EDGE_CURVE('',#13806,#13804,#7725,.T.);
#16915=EDGE_CURVE('',#13806,#13807,#7726,.T.);
#16916=EDGE_CURVE('',#13807,#13805,#7727,.T.);
#16917=EDGE_CURVE('',#13642,#13808,#11421,.T.);
#16918=EDGE_CURVE('',#13808,#13806,#11422,.T.);
#16919=EDGE_CURVE('',#13808,#13809,#7728,.T.);
#16920=EDGE_CURVE('',#13809,#13807,#11423,.T.);
#16921=EDGE_CURVE('',#13641,#13810,#11424,.T.);
#16922=EDGE_CURVE('',#13810,#13808,#7729,.T.);
#16923=EDGE_CURVE('',#13810,#13811,#7730,.T.);
#16924=EDGE_CURVE('',#13811,#13809,#7731,.T.);
#16925=EDGE_CURVE('',#13640,#13812,#11425,.T.);
#16926=EDGE_CURVE('',#13812,#13810,#11426,.T.);
#16927=EDGE_CURVE('',#13812,#13813,#7732,.T.);
#16928=EDGE_CURVE('',#13813,#13811,#11427,.T.);
#16929=EDGE_CURVE('',#13639,#13814,#11428,.T.);
#16930=EDGE_CURVE('',#13814,#13812,#7733,.T.);
#16931=EDGE_CURVE('',#13815,#13814,#7734,.T.);
#16932=EDGE_CURVE('',#13815,#13813,#7735,.T.);
#16933=EDGE_CURVE('',#13638,#13816,#11429,.T.);
#16934=EDGE_CURVE('',#13816,#13814,#11430,.T.);
#16935=EDGE_CURVE('',#13817,#13816,#7736,.T.);
#16936=EDGE_CURVE('',#13817,#13815,#11431,.T.);
#16937=EDGE_CURVE('',#13637,#13818,#11432,.T.);
#16938=EDGE_CURVE('',#13818,#13816,#11433,.T.);
#16939=EDGE_CURVE('',#13819,#13818,#7737,.T.);
#16940=EDGE_CURVE('',#13819,#13817,#11434,.T.);
#16941=EDGE_CURVE('',#13636,#13820,#11435,.T.);
#16942=EDGE_CURVE('',#13820,#13818,#11436,.T.);
#16943=EDGE_CURVE('',#13821,#13820,#7738,.T.);
#16944=EDGE_CURVE('',#13821,#13819,#11437,.T.);
#16945=EDGE_CURVE('',#13635,#13822,#11438,.T.);
#16946=EDGE_CURVE('',#13822,#13820,#7739,.T.);
#16947=EDGE_CURVE('',#13823,#13822,#7740,.T.);
#16948=EDGE_CURVE('',#13823,#13821,#7741,.T.);
#16949=EDGE_CURVE('',#13674,#13824,#11439,.T.);
#16950=EDGE_CURVE('',#13824,#13822,#11440,.T.);
#16951=EDGE_CURVE('',#13825,#13824,#7742,.T.);
#16952=EDGE_CURVE('',#13825,#13823,#11441,.T.);
#16953=EDGE_CURVE('',#13673,#13826,#11442,.T.);
#16954=EDGE_CURVE('',#13826,#13824,#11443,.T.);
#16955=EDGE_CURVE('',#13827,#13826,#7743,.T.);
#16956=EDGE_CURVE('',#13827,#13825,#11444,.T.);
#16957=EDGE_CURVE('',#13672,#13828,#11445,.T.);
#16958=EDGE_CURVE('',#13828,#13826,#11446,.T.);
#16959=EDGE_CURVE('',#13829,#13828,#7744,.T.);
#16960=EDGE_CURVE('',#13829,#13827,#11447,.T.);
#16961=EDGE_CURVE('',#13671,#13830,#11448,.T.);
#16962=EDGE_CURVE('',#13830,#13828,#7745,.T.);
#16963=EDGE_CURVE('',#13830,#13831,#7746,.T.);
#16964=EDGE_CURVE('',#13831,#13829,#7747,.T.);
#16965=EDGE_CURVE('',#13670,#13832,#11449,.T.);
#16966=EDGE_CURVE('',#13832,#13830,#11450,.T.);
#16967=EDGE_CURVE('',#13832,#13833,#7748,.T.);
#16968=EDGE_CURVE('',#13833,#13831,#11451,.T.);
#16969=EDGE_CURVE('',#13669,#13834,#11452,.T.);
#16970=EDGE_CURVE('',#13834,#13832,#7749,.T.);
#16971=EDGE_CURVE('',#13834,#13835,#7750,.T.);
#16972=EDGE_CURVE('',#13835,#13833,#7751,.T.);
#16973=EDGE_CURVE('',#13762,#13836,#11453,.T.);
#16974=EDGE_CURVE('',#13667,#13836,#11454,.T.);
#16975=EDGE_CURVE('',#13761,#13837,#11455,.T.);
#16976=EDGE_CURVE('',#13837,#13836,#7752,.T.);
#16977=EDGE_CURVE('',#13668,#13838,#11456,.T.);
#16978=EDGE_CURVE('',#13838,#13834,#11457,.T.);
#16979=EDGE_CURVE('',#13838,#13839,#7753,.T.);
#16980=EDGE_CURVE('',#13839,#13835,#11458,.T.);
#16981=EDGE_CURVE('',#13836,#13838,#7754,.T.);
#16982=EDGE_CURVE('',#13837,#13839,#7755,.T.);
#16983=EDGE_CURVE('',#13840,#13841,#7756,.T.);
#16984=EDGE_CURVE('',#13842,#13841,#7757,.T.);
#16985=EDGE_CURVE('',#13843,#13842,#7758,.T.);
#16986=EDGE_CURVE('',#13840,#13843,#7759,.T.);
#16987=EDGE_CURVE('',#13844,#13845,#7760,.T.);
#16988=EDGE_CURVE('',#13846,#13845,#1379,.T.);
#16989=EDGE_CURVE('',#13847,#13846,#7761,.T.);
#16990=EDGE_CURVE('',#13844,#13847,#1380,.T.);
#16991=EDGE_CURVE('',#13848,#13849,#7762,.T.);
#16992=EDGE_CURVE('',#13849,#13845,#7763,.T.);
#16993=EDGE_CURVE('',#13850,#13844,#461,.T.);
#16994=EDGE_CURVE('',#13848,#13850,#7764,.T.);
#16995=EDGE_CURVE('',#13846,#13851,#1381,.T.);
#16996=EDGE_CURVE('',#13852,#13851,#7765,.T.);
#16997=EDGE_CURVE('',#13853,#13852,#1382,.T.);
#16998=EDGE_CURVE('',#13847,#13853,#11459,.T.);
#16999=EDGE_CURVE('',#13851,#13854,#1383,.T.);
#17000=EDGE_CURVE('',#13855,#13854,#7766,.T.);
#17001=EDGE_CURVE('',#13852,#13855,#1384,.T.);
#17002=EDGE_CURVE('',#13854,#13703,#1385,.T.);
#17003=EDGE_CURVE('',#13855,#13702,#1386,.T.);
#17004=EDGE_CURVE('',#13856,#13857,#7767,.T.);
#17005=EDGE_CURVE('',#13858,#13857,#11460,.T.);
#17006=EDGE_CURVE('',#13859,#13858,#7768,.T.);
#17007=EDGE_CURVE('',#13856,#13859,#1387,.T.);
#17008=EDGE_CURVE('',#13860,#13861,#7769,.T.);
#17009=EDGE_CURVE('',#13861,#13862,#1388,.T.);
#17010=EDGE_CURVE('',#13863,#13862,#7770,.T.);
#17011=EDGE_CURVE('',#13860,#13863,#1389,.T.);
#17012=EDGE_CURVE('',#13864,#13865,#7771,.T.);
#17013=EDGE_CURVE('',#13865,#13861,#11461,.T.);
#17014=EDGE_CURVE('',#13864,#13860,#1390,.T.);
#17015=EDGE_CURVE('',#13865,#13704,#1391,.T.);
#17016=EDGE_CURVE('',#13866,#13864,#1392,.T.);
#17017=EDGE_CURVE('',#13705,#13866,#1393,.T.);
#17018=EDGE_CURVE('',#13867,#13868,#7772,.T.);
#17019=EDGE_CURVE('',#13868,#13710,#7773,.T.);
#17020=EDGE_CURVE('',#13867,#13709,#7774,.T.);
#17021=EDGE_CURVE('',#13869,#13843,#7775,.T.);
#17022=EDGE_CURVE('',#13842,#13870,#7776,.T.);
#17023=EDGE_CURVE('',#13869,#13870,#7777,.T.);
#17024=EDGE_CURVE('',#13712,#13871,#11462,.T.);
#17025=EDGE_CURVE('',#13872,#13871,#1394,.T.);
#17026=EDGE_CURVE('',#13713,#13872,#11463,.T.);
#17027=EDGE_CURVE('',#13714,#13873,#11464,.T.);
#17028=EDGE_CURVE('',#13874,#13873,#1395,.T.);
#17029=EDGE_CURVE('',#13715,#13874,#11465,.T.);
#17030=EDGE_CURVE('',#13871,#13874,#1396,.T.);
#17031=EDGE_CURVE('',#13716,#13875,#11466,.T.);
#17032=EDGE_CURVE('',#13873,#13875,#7778,.T.);
#17033=EDGE_CURVE('',#13717,#13876,#11467,.T.);
#17034=EDGE_CURVE('',#13877,#13876,#11468,.T.);
#17035=EDGE_CURVE('',#13718,#13877,#11469,.T.);
#17036=EDGE_CURVE('',#13878,#13877,#1397,.T.);
#17037=EDGE_CURVE('',#13719,#13878,#11470,.T.);
#17038=EDGE_CURVE('',#13875,#13878,#462,.T.);
#17039=EDGE_CURVE('',#13722,#13879,#11471,.T.);
#17040=EDGE_CURVE('',#13880,#13879,#1398,.T.);
#17041=EDGE_CURVE('',#13723,#13880,#11472,.T.);
#17042=EDGE_CURVE('',#13721,#13881,#11473,.T.);
#17043=EDGE_CURVE('',#13879,#13881,#1399,.T.);
#17044=EDGE_CURVE('',#13720,#13882,#11474,.T.);
#17045=EDGE_CURVE('',#13881,#13882,#1400,.T.);
#17046=EDGE_CURVE('',#13876,#13880,#1401,.T.);
#17047=EDGE_CURVE('',#13725,#13883,#11475,.T.);
#17048=EDGE_CURVE('',#13882,#13883,#1402,.T.);
#17049=EDGE_CURVE('',#13724,#13884,#11476,.T.);
#17050=EDGE_CURVE('',#13883,#13884,#1403,.T.);
#17051=EDGE_CURVE('',#13729,#13885,#11477,.T.);
#17052=EDGE_CURVE('',#13884,#13885,#1404,.T.);
#17053=EDGE_CURVE('',#13728,#13886,#11478,.T.);
#17054=EDGE_CURVE('',#13885,#13886,#1405,.T.);
#17055=EDGE_CURVE('',#13727,#13887,#11479,.T.);
#17056=EDGE_CURVE('',#13886,#13887,#1406,.T.);
#17057=EDGE_CURVE('',#13726,#13888,#11480,.T.);
#17058=EDGE_CURVE('',#13887,#13888,#1407,.T.);
#17059=EDGE_CURVE('',#13888,#13731,#1408,.T.);
#17060=EDGE_CURVE('',#13730,#13889,#7779,.T.);
#17061=EDGE_CURVE('',#13890,#13889,#1409,.T.);
#17062=EDGE_CURVE('',#13887,#13890,#7780,.T.);
#17063=EDGE_CURVE('',#13733,#13891,#1410,.T.);
#17064=EDGE_CURVE('',#13891,#13892,#463,.T.);
#17065=EDGE_CURVE('',#13892,#13893,#7781,.T.);
#17066=EDGE_CURVE('',#13889,#13893,#1411,.T.);
#17067=EDGE_CURVE('',#13732,#13891,#11481,.T.);
#17068=EDGE_CURVE('',#13894,#13872,#464,.T.);
#17069=EDGE_CURVE('',#13734,#13894,#11482,.T.);
#17070=EDGE_CURVE('',#13892,#13894,#1412,.T.);
#17071=EDGE_CURVE('',#13735,#13892,#11483,.T.);
#17072=EDGE_CURVE('',#13736,#13895,#11484,.T.);
#17073=EDGE_CURVE('',#13895,#13896,#1413,.T.);
#17074=EDGE_CURVE('',#13737,#13896,#11485,.T.);
#17075=EDGE_CURVE('',#13896,#13848,#1414,.T.);
#17076=EDGE_CURVE('',#13738,#13848,#11486,.T.);
#17077=EDGE_CURVE('',#13739,#13897,#11487,.T.);
#17078=EDGE_CURVE('',#13897,#13895,#1415,.T.);
#17079=EDGE_CURVE('',#13740,#13898,#11488,.T.);
#17080=EDGE_CURVE('',#13898,#13856,#465,.T.);
#17081=EDGE_CURVE('',#13741,#13856,#11489,.T.);
#17082=EDGE_CURVE('',#13742,#13859,#11490,.T.);
#17083=EDGE_CURVE('',#13859,#13897,#466,.T.);
#17084=EDGE_CURVE('',#13744,#13898,#1416,.T.);
#17085=EDGE_CURVE('',#13743,#13899,#7782,.T.);
#17086=EDGE_CURVE('',#13899,#13857,#1417,.T.);
#17087=EDGE_CURVE('',#13862,#13899,#1418,.T.);
#17088=EDGE_CURVE('',#13900,#13746,#1419,.T.);
#17089=EDGE_CURVE('',#13863,#13900,#1420,.T.);
#17090=EDGE_CURVE('',#13745,#13900,#11491,.T.);
#17091=EDGE_CURVE('',#13750,#13863,#11492,.T.);
#17092=EDGE_CURVE('',#13749,#13860,#11493,.T.);
#17093=EDGE_CURVE('',#13748,#13864,#11494,.T.);
#17094=EDGE_CURVE('',#13747,#13866,#11495,.T.);
#17095=EDGE_CURVE('',#13752,#13705,#11496,.T.);
#17096=EDGE_CURVE('',#13751,#13706,#11497,.T.);
#17097=EDGE_CURVE('',#13756,#13702,#11498,.T.);
#17098=EDGE_CURVE('',#13755,#13855,#11499,.T.);
#17099=EDGE_CURVE('',#13754,#13852,#11500,.T.);
#17100=EDGE_CURVE('',#13753,#13853,#11501,.T.);
#17101=EDGE_CURVE('',#13757,#13850,#11502,.T.);
#17102=EDGE_CURVE('',#13758,#13844,#11503,.T.);
#17103=EDGE_CURVE('',#13759,#13847,#11504,.T.);
#17104=EDGE_CURVE('',#13760,#13901,#11505,.T.);
#17105=EDGE_CURVE('',#13901,#13902,#11506,.T.);
#17106=EDGE_CURVE('',#13761,#13902,#11507,.T.);
#17107=EDGE_CURVE('',#13765,#13903,#11508,.T.);
#17108=EDGE_CURVE('',#13903,#13901,#11509,.T.);
#17109=EDGE_CURVE('',#13767,#13904,#11510,.T.);
#17110=EDGE_CURVE('',#13904,#13903,#7783,.T.);
#17111=EDGE_CURVE('',#13769,#13905,#11511,.T.);
#17112=EDGE_CURVE('',#13905,#13904,#11512,.T.);
#17113=EDGE_CURVE('',#13771,#13906,#11513,.T.);
#17114=EDGE_CURVE('',#13906,#13905,#7784,.T.);
#17115=EDGE_CURVE('',#13773,#13907,#11514,.T.);
#17116=EDGE_CURVE('',#13907,#13906,#11515,.T.);
#17117=EDGE_CURVE('',#13775,#13908,#11516,.T.);
#17118=EDGE_CURVE('',#13908,#13907,#7785,.T.);
#17119=EDGE_CURVE('',#13777,#13909,#11517,.T.);
#17120=EDGE_CURVE('',#13909,#13908,#11518,.T.);
#17121=EDGE_CURVE('',#13779,#13910,#11519,.T.);
#17122=EDGE_CURVE('',#13910,#13909,#11520,.T.);
#17123=EDGE_CURVE('',#13781,#13911,#11521,.T.);
#17124=EDGE_CURVE('',#13911,#13910,#11522,.T.);
#17125=EDGE_CURVE('',#13783,#13912,#11523,.T.);
#17126=EDGE_CURVE('',#13912,#13911,#7786,.T.);
#17127=EDGE_CURVE('',#13785,#13913,#11524,.T.);
#17128=EDGE_CURVE('',#13913,#13912,#11525,.T.);
#17129=EDGE_CURVE('',#13787,#13914,#11526,.T.);
#17130=EDGE_CURVE('',#13914,#13913,#11527,.T.);
#17131=EDGE_CURVE('',#13789,#13915,#11528,.T.);
#17132=EDGE_CURVE('',#13915,#13914,#11529,.T.);
#17133=EDGE_CURVE('',#13791,#13916,#11530,.T.);
#17134=EDGE_CURVE('',#13916,#13915,#7787,.T.);
#17135=EDGE_CURVE('',#13793,#13917,#11531,.T.);
#17136=EDGE_CURVE('',#13917,#13916,#11532,.T.);
#17137=EDGE_CURVE('',#13795,#13918,#11533,.T.);
#17138=EDGE_CURVE('',#13918,#13917,#7788,.T.);
#17139=EDGE_CURVE('',#13797,#13919,#11534,.T.);
#17140=EDGE_CURVE('',#13919,#13918,#11535,.T.);
#17141=EDGE_CURVE('',#13799,#13920,#11536,.T.);
#17142=EDGE_CURVE('',#13920,#13919,#7789,.T.);
#17143=EDGE_CURVE('',#13801,#13921,#11537,.T.);
#17144=EDGE_CURVE('',#13921,#13920,#11538,.T.);
#17145=EDGE_CURVE('',#13802,#13922,#11539,.T.);
#17146=EDGE_CURVE('',#13922,#13921,#11540,.T.);
#17147=EDGE_CURVE('',#13805,#13923,#11541,.T.);
#17148=EDGE_CURVE('',#13923,#13922,#11542,.T.);
#17149=EDGE_CURVE('',#13807,#13924,#11543,.T.);
#17150=EDGE_CURVE('',#13924,#13923,#7790,.T.);
#17151=EDGE_CURVE('',#13809,#13925,#11544,.T.);
#17152=EDGE_CURVE('',#13925,#13924,#11545,.T.);
#17153=EDGE_CURVE('',#13811,#13926,#11546,.T.);
#17154=EDGE_CURVE('',#13926,#13925,#7791,.T.);
#17155=EDGE_CURVE('',#13813,#13927,#11547,.T.);
#17156=EDGE_CURVE('',#13927,#13926,#11548,.T.);
#17157=EDGE_CURVE('',#13815,#13928,#11549,.T.);
#17158=EDGE_CURVE('',#13928,#13927,#7792,.T.);
#17159=EDGE_CURVE('',#13817,#13929,#11550,.T.);
#17160=EDGE_CURVE('',#13929,#13928,#11551,.T.);
#17161=EDGE_CURVE('',#13819,#13930,#11552,.T.);
#17162=EDGE_CURVE('',#13930,#13929,#11553,.T.);
#17163=EDGE_CURVE('',#13821,#13931,#11554,.T.);
#17164=EDGE_CURVE('',#13931,#13930,#11555,.T.);
#17165=EDGE_CURVE('',#13823,#13932,#11556,.T.);
#17166=EDGE_CURVE('',#13932,#13931,#7793,.T.);
#17167=EDGE_CURVE('',#13825,#13933,#11557,.T.);
#17168=EDGE_CURVE('',#13933,#13932,#11558,.T.);
#17169=EDGE_CURVE('',#13827,#13934,#11559,.T.);
#17170=EDGE_CURVE('',#13934,#13933,#11560,.T.);
#17171=EDGE_CURVE('',#13829,#13935,#11561,.T.);
#17172=EDGE_CURVE('',#13935,#13934,#11562,.T.);
#17173=EDGE_CURVE('',#13831,#13936,#11563,.T.);
#17174=EDGE_CURVE('',#13936,#13935,#7794,.T.);
#17175=EDGE_CURVE('',#13833,#13937,#11564,.T.);
#17176=EDGE_CURVE('',#13937,#13936,#11565,.T.);
#17177=EDGE_CURVE('',#13835,#13938,#11566,.T.);
#17178=EDGE_CURVE('',#13938,#13937,#7795,.T.);
#17179=EDGE_CURVE('',#13902,#13939,#11567,.T.);
#17180=EDGE_CURVE('',#13837,#13939,#11568,.T.);
#17181=EDGE_CURVE('',#13839,#13940,#11569,.T.);
#17182=EDGE_CURVE('',#13940,#13938,#11570,.T.);
#17183=EDGE_CURVE('',#13939,#13940,#7796,.T.);
#17184=EDGE_CURVE('',#13941,#13708,#7797,.T.);
#17185=EDGE_CURVE('',#13942,#13941,#11571,.T.);
#17186=EDGE_CURVE('',#13942,#13943,#7798,.T.);
#17187=EDGE_CURVE('',#13944,#13943,#11572,.T.);
#17188=EDGE_CURVE('',#13944,#13945,#7799,.T.);
#17189=EDGE_CURVE('',#13946,#13945,#11573,.T.);
#17190=EDGE_CURVE('',#13947,#13946,#7800,.T.);
#17191=EDGE_CURVE('',#13948,#13947,#11574,.T.);
#17192=EDGE_CURVE('',#13949,#13948,#7801,.T.);
#17193=EDGE_CURVE('',#13840,#13949,#11575,.T.);
#17194=EDGE_CURVE('',#13950,#13869,#11576,.T.);
#17195=EDGE_CURVE('',#13950,#13951,#7802,.T.);
#17196=EDGE_CURVE('',#13952,#13951,#11577,.T.);
#17197=EDGE_CURVE('',#13952,#13953,#7803,.T.);
#17198=EDGE_CURVE('',#13953,#13954,#11578,.T.);
#17199=EDGE_CURVE('',#13955,#13954,#7804,.T.);
#17200=EDGE_CURVE('',#13956,#13955,#11579,.T.);
#17201=EDGE_CURVE('',#13957,#13956,#7805,.T.);
#17202=EDGE_CURVE('',#13867,#13957,#11580,.T.);
#17203=EDGE_CURVE('',#13954,#13958,#7806,.T.);
#17204=EDGE_CURVE('',#13953,#13959,#7807,.T.);
#17205=EDGE_CURVE('',#13959,#13958,#11581,.T.);
#17206=EDGE_CURVE('',#13960,#13711,#7808,.T.);
#17207=EDGE_CURVE('',#13941,#13960,#7809,.T.);
#17208=EDGE_CURVE('',#13961,#13958,#7810,.T.);
#17209=EDGE_CURVE('',#13955,#13961,#7811,.T.);
#17210=EDGE_CURVE('',#13961,#13962,#11582,.T.);
#17211=EDGE_CURVE('',#13956,#13962,#7812,.T.);
#17212=EDGE_CURVE('',#13963,#13962,#7813,.T.);
#17213=EDGE_CURVE('',#13957,#13963,#7814,.T.);
#17214=EDGE_CURVE('',#13963,#13868,#11583,.T.);
#17215=EDGE_CURVE('',#13942,#13964,#7815,.T.);
#17216=EDGE_CURVE('',#13964,#13965,#7816,.T.);
#17217=EDGE_CURVE('',#13943,#13965,#7817,.T.);
#17218=EDGE_CURVE('',#13960,#13964,#11584,.T.);
#17219=EDGE_CURVE('',#13965,#13966,#11585,.T.);
#17220=EDGE_CURVE('',#13944,#13966,#7818,.T.);
#17221=EDGE_CURVE('',#13966,#13967,#7819,.T.);
#17222=EDGE_CURVE('',#13945,#13967,#7820,.T.);
#17223=EDGE_CURVE('',#13967,#13968,#11586,.T.);
#17224=EDGE_CURVE('',#13946,#13968,#7821,.T.);
#17225=EDGE_CURVE('',#13952,#13969,#7822,.T.);
#17226=EDGE_CURVE('',#13969,#13959,#7823,.T.);
#17227=EDGE_CURVE('',#13970,#13969,#11587,.T.);
#17228=EDGE_CURVE('',#13951,#13970,#7824,.T.);
#17229=EDGE_CURVE('',#13950,#13971,#7825,.T.);
#17230=EDGE_CURVE('',#13971,#13970,#7826,.T.);
#17231=EDGE_CURVE('',#13972,#13841,#11588,.T.);
#17232=EDGE_CURVE('',#13949,#13972,#7827,.T.);
#17233=EDGE_CURVE('',#13948,#13973,#7828,.T.);
#17234=EDGE_CURVE('',#13972,#13973,#7829,.T.);
#17235=EDGE_CURVE('',#13974,#13973,#11589,.T.);
#17236=EDGE_CURVE('',#13947,#13974,#7830,.T.);
#17237=EDGE_CURVE('',#13974,#13968,#7831,.T.);
#17238=EDGE_CURVE('',#13874,#13975,#7832,.T.);
#17239=EDGE_CURVE('',#13976,#13975,#1421,.T.);
#17240=EDGE_CURVE('',#13894,#13976,#7833,.T.);
#17241=EDGE_CURVE('',#13873,#13977,#7834,.T.);
#17242=EDGE_CURVE('',#13977,#13975,#1422,.T.);
#17243=EDGE_CURVE('',#13878,#13978,#7835,.T.);
#17244=EDGE_CURVE('',#13977,#13978,#7836,.T.);
#17245=EDGE_CURVE('',#13880,#13979,#7837,.T.);
#17246=EDGE_CURVE('',#13980,#13979,#1423,.T.);
#17247=EDGE_CURVE('',#13877,#13980,#7838,.T.);
#17248=EDGE_CURVE('',#13980,#13978,#1424,.T.);
#17249=EDGE_CURVE('',#13879,#13981,#7839,.T.);
#17250=EDGE_CURVE('',#13979,#13981,#1425,.T.);
#17251=EDGE_CURVE('',#13881,#13982,#7840,.T.);
#17252=EDGE_CURVE('',#13981,#13982,#1426,.T.);
#17253=EDGE_CURVE('',#13883,#13983,#7841,.T.);
#17254=EDGE_CURVE('',#13982,#13983,#1427,.T.);
#17255=EDGE_CURVE('',#13885,#13984,#7842,.T.);
#17256=EDGE_CURVE('',#13984,#13983,#1428,.T.);
#17257=EDGE_CURVE('',#13886,#13985,#7843,.T.);
#17258=EDGE_CURVE('',#13984,#13985,#11590,.T.);
#17259=EDGE_CURVE('',#13985,#13890,#1429,.T.);
#17260=EDGE_CURVE('',#13870,#13971,#11591,.T.);
#17261=EDGE_CURVE('',#13976,#13893,#11592,.T.);
#17262=EDGE_CURVE('',#13858,#13986,#1430,.T.);
#17263=EDGE_CURVE('',#13896,#13986,#7844,.T.);
#17264=EDGE_CURVE('',#13849,#13986,#1431,.T.);
#17265=EDGE_CURVE('',#13987,#13988,#1432,.T.);
#17266=EDGE_CURVE('',#13987,#13989,#11593,.T.);
#17267=EDGE_CURVE('',#13989,#13990,#1433,.T.);
#17268=EDGE_CURVE('',#13990,#13988,#1434,.T.);
#17269=EDGE_CURVE('',#13991,#13992,#11594,.T.);
#17270=EDGE_CURVE('',#13992,#13989,#1435,.T.);
#17271=EDGE_CURVE('',#13991,#13987,#1436,.T.);
#17272=EDGE_CURVE('',#13993,#13994,#11595,.T.);
#17273=EDGE_CURVE('',#13994,#13992,#1437,.T.);
#17274=EDGE_CURVE('',#13993,#13991,#1438,.T.);
#17275=EDGE_CURVE('',#13707,#13994,#1439,.T.);
#17276=EDGE_CURVE('',#13633,#13993,#467,.T.);
#17277=EDGE_CURVE('',#13689,#13988,#7845,.T.);
#17278=EDGE_CURVE('',#13995,#13988,#1440,.T.);
#17279=EDGE_CURVE('',#13996,#13995,#1441,.T.);
#17280=EDGE_CURVE('',#13997,#13996,#1442,.T.);
#17281=EDGE_CURVE('',#13998,#13997,#468,.T.);
#17282=EDGE_CURVE('',#13998,#13690,#7846,.T.);
#17283=EDGE_CURVE('',#13999,#13998,#11596,.T.);
#17284=EDGE_CURVE('',#13999,#13691,#7847,.T.);
#17285=EDGE_CURVE('',#14000,#13999,#469,.T.);
#17286=EDGE_CURVE('',#14001,#14000,#1443,.T.);
#17287=EDGE_CURVE('',#13685,#14001,#7848,.T.);
#17288=EDGE_CURVE('',#14002,#14001,#470,.T.);
#17289=EDGE_CURVE('',#14003,#14002,#1444,.T.);
#17290=EDGE_CURVE('',#13686,#14003,#7849,.T.);
#17291=EDGE_CURVE('',#14004,#14003,#471,.T.);
#17292=EDGE_CURVE('',#14005,#14004,#1445,.T.);
#17293=EDGE_CURVE('',#14005,#14006,#1446,.T.);
#17294=EDGE_CURVE('',#14006,#14007,#472,.T.);
#17295=EDGE_CURVE('',#13687,#14007,#7850,.T.);
#17296=EDGE_CURVE('',#14007,#14008,#1447,.T.);
#17297=EDGE_CURVE('',#14008,#14009,#473,.T.);
#17298=EDGE_CURVE('',#13688,#14009,#7851,.T.);
#17299=EDGE_CURVE('',#14009,#14010,#1448,.T.);
#17300=EDGE_CURVE('',#14010,#13631,#474,.T.);
#17301=EDGE_CURVE('',#14010,#14011,#11597,.T.);
#17302=EDGE_CURVE('',#14011,#13707,#1449,.T.);
#17303=EDGE_CURVE('',#14009,#14012,#475,.T.);
#17304=EDGE_CURVE('',#14012,#14011,#1450,.T.);
#17305=EDGE_CURVE('',#14008,#14013,#476,.T.);
#17306=EDGE_CURVE('',#14013,#14012,#477,.T.);
#17307=EDGE_CURVE('',#14007,#14014,#11598,.T.);
#17308=EDGE_CURVE('',#14014,#14013,#1451,.T.);
#17309=EDGE_CURVE('',#14006,#14015,#11599,.T.);
#17310=EDGE_CURVE('',#14015,#14014,#1452,.T.);
#17311=EDGE_CURVE('',#14016,#14015,#1453,.T.);
#17312=EDGE_CURVE('',#14005,#14016,#11600,.T.);
#17313=EDGE_CURVE('',#14004,#14017,#11601,.T.);
#17314=EDGE_CURVE('',#14016,#14017,#1454,.T.);
#17315=EDGE_CURVE('',#14003,#14018,#11602,.T.);
#17316=EDGE_CURVE('',#14017,#14018,#1455,.T.);
#17317=EDGE_CURVE('',#14002,#14019,#478,.T.);
#17318=EDGE_CURVE('',#14018,#14019,#1456,.T.);
#17319=EDGE_CURVE('',#14001,#14020,#479,.T.);
#17320=EDGE_CURVE('',#14019,#14020,#480,.T.);
#17321=EDGE_CURVE('',#14000,#14021,#11603,.T.);
#17322=EDGE_CURVE('',#14020,#14021,#1457,.T.);
#17323=EDGE_CURVE('',#13999,#14022,#11604,.T.);
#17324=EDGE_CURVE('',#14021,#14022,#1458,.T.);
#17325=EDGE_CURVE('',#13998,#14022,#11605,.T.);
#17326=EDGE_CURVE('',#13997,#14023,#11606,.T.);
#17327=EDGE_CURVE('',#14022,#14023,#1459,.T.);
#17328=EDGE_CURVE('',#13996,#14024,#11607,.T.);
#17329=EDGE_CURVE('',#14023,#14024,#1460,.T.);
#17330=EDGE_CURVE('',#13995,#14025,#11608,.T.);
#17331=EDGE_CURVE('',#14024,#14025,#1461,.T.);
#17332=EDGE_CURVE('',#14025,#13990,#1462,.T.);
#17333=EDGE_CURVE('',#13990,#14026,#1463,.T.);
#17334=EDGE_CURVE('',#14026,#14027,#1464,.T.);
#17335=EDGE_CURVE('',#14027,#14028,#1465,.T.);
#17336=EDGE_CURVE('',#14025,#14028,#7852,.T.);
#17337=EDGE_CURVE('',#13989,#14029,#7853,.T.);
#17338=EDGE_CURVE('',#14027,#14029,#1466,.T.);
#17339=EDGE_CURVE('',#13992,#14030,#7854,.T.);
#17340=EDGE_CURVE('',#14029,#14030,#11609,.T.);
#17341=EDGE_CURVE('',#13994,#14031,#7855,.T.);
#17342=EDGE_CURVE('',#14030,#14031,#11610,.T.);
#17343=EDGE_CURVE('',#14011,#14032,#7856,.T.);
#17344=EDGE_CURVE('',#14032,#14031,#11611,.T.);
#17345=EDGE_CURVE('',#14013,#14033,#7857,.T.);
#17346=EDGE_CURVE('',#14033,#14032,#1467,.T.);
#17347=EDGE_CURVE('',#14015,#14034,#7858,.T.);
#17348=EDGE_CURVE('',#14033,#14034,#481,.T.);
#17349=EDGE_CURVE('',#14016,#14035,#7859,.T.);
#17350=EDGE_CURVE('',#14034,#14035,#11612,.T.);
#17351=EDGE_CURVE('',#14017,#14036,#7860,.T.);
#17352=EDGE_CURVE('',#14036,#14035,#11613,.T.);
#17353=EDGE_CURVE('',#14019,#14037,#7861,.T.);
#17354=EDGE_CURVE('',#14037,#14036,#482,.T.);
#17355=EDGE_CURVE('',#14021,#14038,#7862,.T.);
#17356=EDGE_CURVE('',#14037,#14038,#1468,.T.);
#17357=EDGE_CURVE('',#14023,#14039,#7863,.T.);
#17358=EDGE_CURVE('',#14038,#14039,#11614,.T.);
#17359=EDGE_CURVE('',#14024,#14040,#7864,.T.);
#17360=EDGE_CURVE('',#14040,#14039,#11615,.T.);
#17361=EDGE_CURVE('',#14028,#14040,#11616,.T.);
#17362=EDGE_CURVE('',#14041,#14042,#11617,.T.);
#17363=EDGE_CURVE('',#14043,#14041,#11618,.T.);
#17364=EDGE_CURVE('',#14044,#14043,#11619,.T.);
#17365=EDGE_CURVE('',#14045,#14044,#11620,.T.);
#17366=EDGE_CURVE('',#14045,#14046,#11621,.T.);
#17367=EDGE_CURVE('',#14046,#14047,#11622,.T.);
#17368=EDGE_CURVE('',#14047,#14042,#11623,.T.);
#17369=EDGE_CURVE('',#14048,#14049,#11624,.T.);
#17370=EDGE_CURVE('',#14043,#14048,#7865,.T.);
#17371=EDGE_CURVE('',#14041,#14049,#7866,.T.);
#17372=EDGE_CURVE('',#14044,#14050,#7867,.T.);
#17373=EDGE_CURVE('',#14050,#14048,#11625,.T.);
#17374=EDGE_CURVE('',#14045,#14051,#7868,.T.);
#17375=EDGE_CURVE('',#14051,#14050,#11626,.T.);
#17376=EDGE_CURVE('',#14051,#14052,#11627,.T.);
#17377=EDGE_CURVE('',#14046,#14052,#7869,.T.);
#17378=EDGE_CURVE('',#14052,#14053,#11628,.T.);
#17379=EDGE_CURVE('',#14047,#14053,#7870,.T.);
#17380=EDGE_CURVE('',#14053,#14054,#11629,.T.);
#17381=EDGE_CURVE('',#14042,#14054,#7871,.T.);
#17382=EDGE_CURVE('',#14054,#14049,#11630,.T.);
#17383=EDGE_CURVE('',#14055,#14056,#1469,.T.);
#17384=EDGE_CURVE('',#14056,#14057,#483,.T.);
#17385=EDGE_CURVE('',#14057,#14058,#1470,.T.);
#17386=EDGE_CURVE('',#14058,#14059,#1471,.T.);
#17387=EDGE_CURVE('',#14059,#14060,#1472,.T.);
#17388=EDGE_CURVE('',#14060,#14061,#1473,.T.);
#17389=EDGE_CURVE('',#14061,#14062,#1474,.T.);
#17390=EDGE_CURVE('',#14062,#14063,#1475,.T.);
#17391=EDGE_CURVE('',#14063,#14064,#1476,.T.);
#17392=EDGE_CURVE('',#14064,#14065,#1477,.T.);
#17393=EDGE_CURVE('',#14065,#14055,#1478,.T.);
#17394=EDGE_CURVE('',#14066,#14067,#1479,.T.);
#17395=EDGE_CURVE('',#14068,#14066,#1480,.T.);
#17396=EDGE_CURVE('',#14069,#14068,#1481,.T.);
#17397=EDGE_CURVE('',#14070,#14069,#484,.T.);
#17398=EDGE_CURVE('',#14071,#14070,#1482,.T.);
#17399=EDGE_CURVE('',#14072,#14071,#7872,.T.);
#17400=EDGE_CURVE('',#14073,#14072,#1483,.T.);
#17401=EDGE_CURVE('',#14074,#14073,#485,.T.);
#17402=EDGE_CURVE('',#14067,#14074,#1484,.T.);
#17403=EDGE_CURVE('',#14075,#14076,#486,.T.);
#17404=EDGE_CURVE('',#14077,#14075,#1485,.T.);
#17405=EDGE_CURVE('',#14078,#14077,#7873,.T.);
#17406=EDGE_CURVE('',#14079,#14078,#1486,.T.);
#17407=EDGE_CURVE('',#14080,#14079,#487,.T.);
#17408=EDGE_CURVE('',#14081,#14080,#1487,.T.);
#17409=EDGE_CURVE('',#14082,#14081,#1488,.T.);
#17410=EDGE_CURVE('',#14083,#14082,#1489,.T.);
#17411=EDGE_CURVE('',#14076,#14083,#1490,.T.);
#17412=EDGE_CURVE('',#14084,#14085,#1491,.T.);
#17413=EDGE_CURVE('',#14086,#14084,#1492,.T.);
#17414=EDGE_CURVE('',#14087,#14086,#1493,.T.);
#17415=EDGE_CURVE('',#14088,#14087,#488,.T.);
#17416=EDGE_CURVE('',#14089,#14088,#1494,.T.);
#17417=EDGE_CURVE('',#14090,#14089,#1495,.T.);
#17418=EDGE_CURVE('',#14085,#14090,#1496,.T.);
#17419=EDGE_CURVE('',#14091,#14092,#1497,.T.);
#17420=EDGE_CURVE('',#14093,#14091,#1498,.T.);
#17421=EDGE_CURVE('',#14094,#14093,#1499,.T.);
#17422=EDGE_CURVE('',#14095,#14094,#1500,.T.);
#17423=EDGE_CURVE('',#14096,#14095,#1501,.T.);
#17424=EDGE_CURVE('',#14097,#14096,#1502,.T.);
#17425=EDGE_CURVE('',#14098,#14097,#1503,.T.);
#17426=EDGE_CURVE('',#14099,#14098,#1504,.T.);
#17427=EDGE_CURVE('',#14100,#14099,#1505,.T.);
#17428=EDGE_CURVE('',#14101,#14100,#489,.T.);
#17429=EDGE_CURVE('',#14092,#14101,#1506,.T.);
#17430=EDGE_CURVE('',#14102,#14103,#1507,.T.);
#17431=EDGE_CURVE('',#14103,#14104,#1508,.T.);
#17432=EDGE_CURVE('',#14104,#14105,#1509,.T.);
#17433=EDGE_CURVE('',#14105,#14106,#7874,.T.);
#17434=EDGE_CURVE('',#14106,#14107,#1510,.T.);
#17435=EDGE_CURVE('',#14107,#14108,#490,.T.);
#17436=EDGE_CURVE('',#14108,#14109,#1511,.T.);
#17437=EDGE_CURVE('',#14109,#14110,#1512,.T.);
#17438=EDGE_CURVE('',#14110,#14102,#1513,.T.);
#17439=EDGE_CURVE('',#14111,#14112,#1514,.T.);
#17440=EDGE_CURVE('',#14112,#14113,#1515,.T.);
#17441=EDGE_CURVE('',#14113,#14114,#1516,.T.);
#17442=EDGE_CURVE('',#14114,#14115,#1517,.T.);
#17443=EDGE_CURVE('',#14115,#14116,#491,.T.);
#17444=EDGE_CURVE('',#14116,#14117,#1518,.T.);
#17445=EDGE_CURVE('',#14117,#14118,#7875,.T.);
#17446=EDGE_CURVE('',#14118,#14119,#1519,.T.);
#17447=EDGE_CURVE('',#14119,#14111,#1520,.T.);
#17448=EDGE_CURVE('',#14120,#14121,#1521,.T.);
#17449=EDGE_CURVE('',#14121,#14122,#1522,.T.);
#17450=EDGE_CURVE('',#14122,#14123,#1523,.T.);
#17451=EDGE_CURVE('',#14123,#14124,#492,.T.);
#17452=EDGE_CURVE('',#14124,#14125,#1524,.T.);
#17453=EDGE_CURVE('',#14125,#14126,#1525,.T.);
#17454=EDGE_CURVE('',#14126,#14120,#1526,.T.);
#17455=EDGE_CURVE('',#14127,#14075,#493,.T.);
#17456=EDGE_CURVE('',#14128,#14076,#494,.T.);
#17457=EDGE_CURVE('',#14127,#14128,#495,.T.);
#17458=EDGE_CURVE('',#14119,#14129,#496,.T.);
#17459=EDGE_CURVE('',#14129,#14130,#497,.T.);
#17460=EDGE_CURVE('',#14111,#14130,#498,.T.);
#17461=EDGE_CURVE('',#14129,#14127,#7876,.T.);
#17462=EDGE_CURVE('',#14130,#14128,#7877,.T.);
#17463=EDGE_CURVE('',#14131,#14083,#499,.T.);
#17464=EDGE_CURVE('',#14128,#14131,#1527,.T.);
#17465=EDGE_CURVE('',#14130,#14132,#1528,.T.);
#17466=EDGE_CURVE('',#14112,#14132,#500,.T.);
#17467=EDGE_CURVE('',#14132,#14131,#7878,.T.);
#17468=EDGE_CURVE('',#14133,#14082,#501,.T.);
#17469=EDGE_CURVE('',#14131,#14133,#1529,.T.);
#17470=EDGE_CURVE('',#14132,#14134,#1530,.T.);
#17471=EDGE_CURVE('',#14113,#14134,#502,.T.);
#17472=EDGE_CURVE('',#14134,#14133,#7879,.T.);
#17473=EDGE_CURVE('',#14135,#14081,#503,.T.);
#17474=EDGE_CURVE('',#14133,#14135,#1531,.T.);
#17475=EDGE_CURVE('',#14134,#14136,#1532,.T.);
#17476=EDGE_CURVE('',#14114,#14136,#504,.T.);
#17477=EDGE_CURVE('',#14136,#14135,#7880,.T.);
#17478=EDGE_CURVE('',#14137,#14080,#505,.T.);
#17479=EDGE_CURVE('',#14135,#14137,#1533,.T.);
#17480=EDGE_CURVE('',#14136,#14138,#1534,.T.);
#17481=EDGE_CURVE('',#14115,#14138,#506,.T.);
#17482=EDGE_CURVE('',#14138,#14137,#7881,.T.);
#17483=EDGE_CURVE('',#14139,#14079,#507,.T.);
#17484=EDGE_CURVE('',#14137,#14139,#508,.T.);
#17485=EDGE_CURVE('',#14138,#14140,#509,.T.);
#17486=EDGE_CURVE('',#14116,#14140,#510,.T.);
#17487=EDGE_CURVE('',#14140,#14139,#7882,.T.);
#17488=EDGE_CURVE('',#14141,#14078,#511,.T.);
#17489=EDGE_CURVE('',#14139,#14141,#1535,.T.);
#17490=EDGE_CURVE('',#14140,#14142,#1536,.T.);
#17491=EDGE_CURVE('',#14117,#14142,#512,.T.);
#17492=EDGE_CURVE('',#14142,#14141,#7883,.T.);
#17493=EDGE_CURVE('',#14143,#14077,#1537,.T.);
#17494=EDGE_CURVE('',#14141,#14143,#7884,.T.);
#17495=EDGE_CURVE('',#14142,#14144,#7885,.T.);
#17496=EDGE_CURVE('',#14118,#14144,#1538,.T.);
#17497=EDGE_CURVE('',#14144,#14143,#7886,.T.);
#17498=EDGE_CURVE('',#14143,#14127,#1539,.T.);
#17499=EDGE_CURVE('',#14144,#14129,#1540,.T.);
#17500=EDGE_CURVE('',#14145,#14086,#1541,.T.);
#17501=EDGE_CURVE('',#14146,#14084,#513,.T.);
#17502=EDGE_CURVE('',#14145,#14146,#1542,.T.);
#17503=EDGE_CURVE('',#14125,#14147,#1543,.T.);
#17504=EDGE_CURVE('',#14147,#14148,#1544,.T.);
#17505=EDGE_CURVE('',#14126,#14148,#514,.T.);
#17506=EDGE_CURVE('',#14147,#14145,#7887,.T.);
#17507=EDGE_CURVE('',#14148,#14146,#7888,.T.);
#17508=EDGE_CURVE('',#14149,#14085,#515,.T.);
#17509=EDGE_CURVE('',#14146,#14149,#1545,.T.);
#17510=EDGE_CURVE('',#14148,#14150,#1546,.T.);
#17511=EDGE_CURVE('',#14120,#14150,#1547,.T.);
#17512=EDGE_CURVE('',#14150,#14149,#7889,.T.);
#17513=EDGE_CURVE('',#14151,#14090,#516,.T.);
#17514=EDGE_CURVE('',#14149,#14151,#1548,.T.);
#17515=EDGE_CURVE('',#14150,#14152,#1549,.T.);
#17516=EDGE_CURVE('',#14121,#14152,#517,.T.);
#17517=EDGE_CURVE('',#14152,#14151,#7890,.T.);
#17518=EDGE_CURVE('',#14153,#14089,#518,.T.);
#17519=EDGE_CURVE('',#14151,#14153,#1550,.T.);
#17520=EDGE_CURVE('',#14152,#14154,#1551,.T.);
#17521=EDGE_CURVE('',#14122,#14154,#1552,.T.);
#17522=EDGE_CURVE('',#14154,#14153,#7891,.T.);
#17523=EDGE_CURVE('',#14155,#14088,#519,.T.);
#17524=EDGE_CURVE('',#14153,#14155,#1553,.T.);
#17525=EDGE_CURVE('',#14154,#14156,#1554,.T.);
#17526=EDGE_CURVE('',#14123,#14156,#520,.T.);
#17527=EDGE_CURVE('',#14156,#14155,#7892,.T.);
#17528=EDGE_CURVE('',#14157,#14087,#521,.T.);
#17529=EDGE_CURVE('',#14155,#14157,#522,.T.);
#17530=EDGE_CURVE('',#14156,#14158,#523,.T.);
#17531=EDGE_CURVE('',#14124,#14158,#524,.T.);
#17532=EDGE_CURVE('',#14158,#14157,#7893,.T.);
#17533=EDGE_CURVE('',#14157,#14145,#1555,.T.);
#17534=EDGE_CURVE('',#14158,#14147,#1556,.T.);
#17535=EDGE_CURVE('',#14159,#14068,#525,.T.);
#17536=EDGE_CURVE('',#14160,#14066,#526,.T.);
#17537=EDGE_CURVE('',#14159,#14160,#1557,.T.);
#17538=EDGE_CURVE('',#14109,#14161,#527,.T.);
#17539=EDGE_CURVE('',#14161,#14162,#1558,.T.);
#17540=EDGE_CURVE('',#14110,#14162,#528,.T.);
#17541=EDGE_CURVE('',#14161,#14159,#7894,.T.);
#17542=EDGE_CURVE('',#14162,#14160,#7895,.T.);
#17543=EDGE_CURVE('',#14163,#14067,#529,.T.);
#17544=EDGE_CURVE('',#14160,#14163,#1559,.T.);
#17545=EDGE_CURVE('',#14162,#14164,#1560,.T.);
#17546=EDGE_CURVE('',#14102,#14164,#530,.T.);
#17547=EDGE_CURVE('',#14164,#14163,#7896,.T.);
#17548=EDGE_CURVE('',#14165,#14074,#531,.T.);
#17549=EDGE_CURVE('',#14163,#14165,#1561,.T.);
#17550=EDGE_CURVE('',#14164,#14166,#1562,.T.);
#17551=EDGE_CURVE('',#14103,#14166,#532,.T.);
#17552=EDGE_CURVE('',#14166,#14165,#7897,.T.);
#17553=EDGE_CURVE('',#14167,#14073,#533,.T.);
#17554=EDGE_CURVE('',#14165,#14167,#534,.T.);
#17555=EDGE_CURVE('',#14166,#14168,#535,.T.);
#17556=EDGE_CURVE('',#14104,#14168,#536,.T.);
#17557=EDGE_CURVE('',#14168,#14167,#7898,.T.);
#17558=EDGE_CURVE('',#14169,#14072,#1563,.T.);
#17559=EDGE_CURVE('',#14167,#14169,#1564,.T.);
#17560=EDGE_CURVE('',#14168,#14170,#1565,.T.);
#17561=EDGE_CURVE('',#14105,#14170,#1566,.T.);
#17562=EDGE_CURVE('',#14170,#14169,#7899,.T.);
#17563=EDGE_CURVE('',#14171,#14071,#537,.T.);
#17564=EDGE_CURVE('',#14169,#14171,#7900,.T.);
#17565=EDGE_CURVE('',#14170,#14172,#7901,.T.);
#17566=EDGE_CURVE('',#14106,#14172,#538,.T.);
#17567=EDGE_CURVE('',#14172,#14171,#7902,.T.);
#17568=EDGE_CURVE('',#14173,#14070,#539,.T.);
#17569=EDGE_CURVE('',#14171,#14173,#1567,.T.);
#17570=EDGE_CURVE('',#14172,#14174,#1568,.T.);
#17571=EDGE_CURVE('',#14107,#14174,#540,.T.);
#17572=EDGE_CURVE('',#14174,#14173,#7903,.T.);
#17573=EDGE_CURVE('',#14175,#14069,#541,.T.);
#17574=EDGE_CURVE('',#14173,#14175,#542,.T.);
#17575=EDGE_CURVE('',#14174,#14176,#543,.T.);
#17576=EDGE_CURVE('',#14108,#14176,#544,.T.);
#17577=EDGE_CURVE('',#14176,#14175,#7904,.T.);
#17578=EDGE_CURVE('',#14175,#14159,#1569,.T.);
#17579=EDGE_CURVE('',#14176,#14161,#1570,.T.);
#17580=EDGE_CURVE('',#14064,#14177,#545,.T.);
#17581=EDGE_CURVE('',#14177,#14178,#1571,.T.);
#17582=EDGE_CURVE('',#14065,#14178,#546,.T.);
#17583=EDGE_CURVE('',#14179,#14093,#547,.T.);
#17584=EDGE_CURVE('',#14180,#14091,#548,.T.);
#17585=EDGE_CURVE('',#14179,#14180,#1572,.T.);
#17586=EDGE_CURVE('',#14180,#14178,#7905,.T.);
#17587=EDGE_CURVE('',#14179,#14177,#7906,.T.);
#17588=EDGE_CURVE('',#14063,#14181,#549,.T.);
#17589=EDGE_CURVE('',#14181,#14177,#1573,.T.);
#17590=EDGE_CURVE('',#14182,#14094,#550,.T.);
#17591=EDGE_CURVE('',#14182,#14179,#1574,.T.);
#17592=EDGE_CURVE('',#14182,#14181,#7907,.T.);
#17593=EDGE_CURVE('',#14062,#14183,#551,.T.);
#17594=EDGE_CURVE('',#14183,#14181,#1575,.T.);
#17595=EDGE_CURVE('',#14184,#14095,#552,.T.);
#17596=EDGE_CURVE('',#14184,#14182,#1576,.T.);
#17597=EDGE_CURVE('',#14184,#14183,#7908,.T.);
#17598=EDGE_CURVE('',#14061,#14185,#553,.T.);
#17599=EDGE_CURVE('',#14185,#14183,#1577,.T.);
#17600=EDGE_CURVE('',#14186,#14096,#554,.T.);
#17601=EDGE_CURVE('',#14186,#14184,#1578,.T.);
#17602=EDGE_CURVE('',#14186,#14185,#7909,.T.);
#17603=EDGE_CURVE('',#14060,#14187,#555,.T.);
#17604=EDGE_CURVE('',#14187,#14185,#1579,.T.);
#17605=EDGE_CURVE('',#14188,#14097,#556,.T.);
#17606=EDGE_CURVE('',#14188,#14186,#1580,.T.);
#17607=EDGE_CURVE('',#14188,#14187,#7910,.T.);
#17608=EDGE_CURVE('',#14059,#14189,#557,.T.);
#17609=EDGE_CURVE('',#14189,#14187,#1581,.T.);
#17610=EDGE_CURVE('',#14190,#14098,#558,.T.);
#17611=EDGE_CURVE('',#14190,#14188,#1582,.T.);
#17612=EDGE_CURVE('',#14190,#14189,#7911,.T.);
#17613=EDGE_CURVE('',#14058,#14191,#559,.T.);
#17614=EDGE_CURVE('',#14191,#14189,#1583,.T.);
#17615=EDGE_CURVE('',#14192,#14099,#560,.T.);
#17616=EDGE_CURVE('',#14192,#14190,#1584,.T.);
#17617=EDGE_CURVE('',#14192,#14191,#7912,.T.);
#17618=EDGE_CURVE('',#14057,#14193,#561,.T.);
#17619=EDGE_CURVE('',#14193,#14191,#1585,.T.);
#17620=EDGE_CURVE('',#14194,#14100,#562,.T.);
#17621=EDGE_CURVE('',#14194,#14192,#1586,.T.);
#17622=EDGE_CURVE('',#14194,#14193,#7913,.T.);
#17623=EDGE_CURVE('',#14056,#14195,#563,.T.);
#17624=EDGE_CURVE('',#14195,#14193,#564,.T.);
#17625=EDGE_CURVE('',#14196,#14101,#565,.T.);
#17626=EDGE_CURVE('',#14196,#14194,#566,.T.);
#17627=EDGE_CURVE('',#14196,#14195,#7914,.T.);
#17628=EDGE_CURVE('',#14055,#14197,#567,.T.);
#17629=EDGE_CURVE('',#14197,#14195,#1587,.T.);
#17630=EDGE_CURVE('',#14198,#14092,#568,.T.);
#17631=EDGE_CURVE('',#14198,#14196,#1588,.T.);
#17632=EDGE_CURVE('',#14198,#14197,#7915,.T.);
#17633=EDGE_CURVE('',#14178,#14197,#1589,.T.);
#17634=EDGE_CURVE('',#14180,#14198,#1590,.T.);
#17635=EDGE_CURVE('',#14199,#14200,#1591,.T.);
#17636=EDGE_CURVE('',#14200,#14201,#1592,.T.);
#17637=EDGE_CURVE('',#14201,#14202,#7916,.T.);
#17638=EDGE_CURVE('',#14202,#14203,#1593,.T.);
#17639=EDGE_CURVE('',#14203,#14204,#1594,.T.);
#17640=EDGE_CURVE('',#14204,#14205,#7917,.T.);
#17641=EDGE_CURVE('',#14205,#14206,#1595,.T.);
#17642=EDGE_CURVE('',#14206,#14207,#1596,.T.);
#17643=EDGE_CURVE('',#14207,#14208,#1597,.T.);
#17644=EDGE_CURVE('',#14208,#14199,#1598,.T.);
#17645=EDGE_CURVE('',#14209,#14210,#7918,.T.);
#17646=EDGE_CURVE('',#14211,#14209,#1599,.T.);
#17647=EDGE_CURVE('',#14212,#14211,#1600,.T.);
#17648=EDGE_CURVE('',#14213,#14212,#1601,.T.);
#17649=EDGE_CURVE('',#14214,#14213,#1602,.T.);
#17650=EDGE_CURVE('',#14215,#14214,#1603,.T.);
#17651=EDGE_CURVE('',#14216,#14215,#7919,.T.);
#17652=EDGE_CURVE('',#14217,#14216,#1604,.T.);
#17653=EDGE_CURVE('',#14210,#14217,#1605,.T.);
#17654=EDGE_CURVE('',#14218,#14218,#11631,.T.);
#17655=EDGE_CURVE('',#14219,#14219,#11632,.T.);
#17656=EDGE_CURVE('',#14220,#14221,#1606,.T.);
#17657=EDGE_CURVE('',#14222,#14220,#1607,.T.);
#17658=EDGE_CURVE('',#14223,#14222,#1608,.T.);
#17659=EDGE_CURVE('',#14224,#14223,#1609,.T.);
#17660=EDGE_CURVE('',#14225,#14224,#1610,.T.);
#17661=EDGE_CURVE('',#14226,#14225,#1611,.T.);
#17662=EDGE_CURVE('',#14227,#14226,#7920,.T.);
#17663=EDGE_CURVE('',#14228,#14227,#1612,.T.);
#17664=EDGE_CURVE('',#14229,#14228,#1613,.T.);
#17665=EDGE_CURVE('',#14221,#14229,#7921,.T.);
#17666=EDGE_CURVE('',#14230,#14230,#11633,.T.);
#17667=EDGE_CURVE('',#14231,#14231,#11634,.T.);
#17668=EDGE_CURVE('',#14232,#14233,#1614,.T.);
#17669=EDGE_CURVE('',#14233,#14234,#7922,.T.);
#17670=EDGE_CURVE('',#14234,#14235,#1615,.T.);
#17671=EDGE_CURVE('',#14235,#14236,#1616,.T.);
#17672=EDGE_CURVE('',#14236,#14237,#7923,.T.);
#17673=EDGE_CURVE('',#14237,#14238,#1617,.T.);
#17674=EDGE_CURVE('',#14238,#14239,#1618,.T.);
#17675=EDGE_CURVE('',#14239,#14240,#1619,.T.);
#17676=EDGE_CURVE('',#14240,#14232,#1620,.T.);
#17677=EDGE_CURVE('',#14241,#14241,#11635,.T.);
#17678=EDGE_CURVE('',#14241,#14219,#11636,.T.);
#17679=EDGE_CURVE('',#14230,#14241,#7924,.T.);
#17680=EDGE_CURVE('',#14242,#14242,#11637,.T.);
#17681=EDGE_CURVE('',#14242,#14218,#11638,.T.);
#17682=EDGE_CURVE('',#14231,#14242,#7925,.T.);
#17683=EDGE_CURVE('',#14243,#14211,#569,.T.);
#17684=EDGE_CURVE('',#14244,#14209,#570,.T.);
#17685=EDGE_CURVE('',#14243,#14244,#1621,.T.);
#17686=EDGE_CURVE('',#14233,#14244,#7926,.T.);
#17687=EDGE_CURVE('',#14232,#14243,#7927,.T.);
#17688=EDGE_CURVE('',#14245,#14210,#11639,.T.);
#17689=EDGE_CURVE('',#14244,#14245,#7928,.T.);
#17690=EDGE_CURVE('',#14234,#14245,#7929,.T.);
#17691=EDGE_CURVE('',#14246,#14217,#571,.T.);
#17692=EDGE_CURVE('',#14245,#14246,#1622,.T.);
#17693=EDGE_CURVE('',#14235,#14246,#7930,.T.);
#17694=EDGE_CURVE('',#14247,#14216,#572,.T.);
#17695=EDGE_CURVE('',#14246,#14247,#1623,.T.);
#17696=EDGE_CURVE('',#14236,#14247,#7931,.T.);
#17697=EDGE_CURVE('',#14248,#14215,#573,.T.);
#17698=EDGE_CURVE('',#14247,#14248,#7932,.T.);
#17699=EDGE_CURVE('',#14237,#14248,#7933,.T.);
#17700=EDGE_CURVE('',#14249,#14214,#574,.T.);
#17701=EDGE_CURVE('',#14248,#14249,#1624,.T.);
#17702=EDGE_CURVE('',#14238,#14249,#7934,.T.);
#17703=EDGE_CURVE('',#14250,#14213,#575,.T.);
#17704=EDGE_CURVE('',#14249,#14250,#1625,.T.);
#17705=EDGE_CURVE('',#14239,#14250,#7935,.T.);
#17706=EDGE_CURVE('',#14251,#14212,#576,.T.);
#17707=EDGE_CURVE('',#14250,#14251,#1626,.T.);
#17708=EDGE_CURVE('',#14240,#14251,#7936,.T.);
#17709=EDGE_CURVE('',#14251,#14243,#1627,.T.);
#17710=EDGE_CURVE('',#14200,#14252,#577,.T.);
#17711=EDGE_CURVE('',#14252,#14253,#1628,.T.);
#17712=EDGE_CURVE('',#14201,#14253,#578,.T.);
#17713=EDGE_CURVE('',#14220,#14252,#7937,.T.);
#17714=EDGE_CURVE('',#14221,#14253,#7938,.T.);
#17715=EDGE_CURVE('',#14199,#14254,#579,.T.);
#17716=EDGE_CURVE('',#14254,#14252,#1629,.T.);
#17717=EDGE_CURVE('',#14222,#14254,#7939,.T.);
#17718=EDGE_CURVE('',#14208,#14255,#580,.T.);
#17719=EDGE_CURVE('',#14255,#14254,#1630,.T.);
#17720=EDGE_CURVE('',#14223,#14255,#7940,.T.);
#17721=EDGE_CURVE('',#14207,#14256,#581,.T.);
#17722=EDGE_CURVE('',#14256,#14255,#1631,.T.);
#17723=EDGE_CURVE('',#14224,#14256,#7941,.T.);
#17724=EDGE_CURVE('',#14206,#14257,#582,.T.);
#17725=EDGE_CURVE('',#14257,#14256,#1632,.T.);
#17726=EDGE_CURVE('',#14225,#14257,#7942,.T.);
#17727=EDGE_CURVE('',#14205,#14258,#583,.T.);
#17728=EDGE_CURVE('',#14258,#14257,#1633,.T.);
#17729=EDGE_CURVE('',#14226,#14258,#7943,.T.);
#17730=EDGE_CURVE('',#14204,#14259,#584,.T.);
#17731=EDGE_CURVE('',#14259,#14258,#7944,.T.);
#17732=EDGE_CURVE('',#14227,#14259,#7945,.T.);
#17733=EDGE_CURVE('',#14203,#14260,#585,.T.);
#17734=EDGE_CURVE('',#14260,#14259,#1634,.T.);
#17735=EDGE_CURVE('',#14228,#14260,#7946,.T.);
#17736=EDGE_CURVE('',#14202,#14261,#586,.T.);
#17737=EDGE_CURVE('',#14261,#14260,#1635,.T.);
#17738=EDGE_CURVE('',#14229,#14261,#7947,.T.);
#17739=EDGE_CURVE('',#14253,#14261,#7948,.T.);
#17740=EDGE_CURVE('',#14262,#14263,#1636,.T.);
#17741=EDGE_CURVE('',#14264,#14263,#7949,.T.);
#17742=EDGE_CURVE('',#14262,#14264,#11640,.T.);
#17743=EDGE_CURVE('',#14262,#14265,#7950,.T.);
#17744=EDGE_CURVE('',#14266,#14264,#7951,.T.);
#17745=EDGE_CURVE('',#14265,#14266,#11641,.T.);
#17746=EDGE_CURVE('',#14267,#14263,#7952,.T.);
#17747=EDGE_CURVE('',#14266,#14267,#7953,.T.);
#17748=EDGE_CURVE('',#14265,#14267,#1637,.T.);
#17749=EDGE_CURVE('',#14268,#14269,#1638,.T.);
#17750=EDGE_CURVE('',#14268,#14270,#11642,.T.);
#17751=EDGE_CURVE('',#14270,#14269,#7954,.T.);
#17752=EDGE_CURVE('',#14271,#14270,#7955,.T.);
#17753=EDGE_CURVE('',#14271,#14272,#7956,.T.);
#17754=EDGE_CURVE('',#14272,#14269,#7957,.T.);
#17755=EDGE_CURVE('',#14273,#14268,#7958,.T.);
#17756=EDGE_CURVE('',#14273,#14271,#11643,.T.);
#17757=EDGE_CURVE('',#14273,#14272,#1639,.T.);
#17758=EDGE_CURVE('',#14274,#14275,#11644,.T.);
#17759=EDGE_CURVE('',#14275,#14276,#7959,.T.);
#17760=EDGE_CURVE('',#14277,#14276,#11645,.T.);
#17761=EDGE_CURVE('',#14278,#14277,#11646,.T.);
#17762=EDGE_CURVE('',#14274,#14278,#7960,.T.);
#17763=EDGE_CURVE('',#14279,#14280,#11647,.T.);
#17764=EDGE_CURVE('',#14281,#14279,#7961,.T.);
#17765=EDGE_CURVE('',#14281,#14282,#11648,.T.);
#17766=EDGE_CURVE('',#14282,#14280,#7962,.T.);
#17767=EDGE_CURVE('',#14283,#14284,#7963,.T.);
#17768=EDGE_CURVE('',#14284,#14285,#7964,.T.);
#17769=EDGE_CURVE('',#14285,#14286,#7965,.T.);
#17770=EDGE_CURVE('',#14287,#14286,#7966,.T.);
#17771=EDGE_CURVE('',#14283,#14287,#7967,.T.);
#17772=EDGE_CURVE('',#14288,#14289,#7968,.T.);
#17773=EDGE_CURVE('',#14290,#14289,#1640,.T.);
#17774=EDGE_CURVE('',#14291,#14290,#7969,.T.);
#17775=EDGE_CURVE('',#14292,#14291,#11649,.T.);
#17776=EDGE_CURVE('',#14292,#14293,#7970,.T.);
#17777=EDGE_CURVE('',#14293,#14294,#1641,.T.);
#17778=EDGE_CURVE('',#14294,#14295,#7971,.T.);
#17779=EDGE_CURVE('',#14295,#14296,#11650,.T.);
#17780=EDGE_CURVE('',#14296,#14297,#7972,.T.);
#17781=EDGE_CURVE('',#14297,#14298,#1642,.T.);
#17782=EDGE_CURVE('',#14298,#14299,#7973,.T.);
#17783=EDGE_CURVE('',#14300,#14299,#11651,.T.);
#17784=EDGE_CURVE('',#14301,#14300,#7974,.T.);
#17785=EDGE_CURVE('',#14302,#14301,#1643,.T.);
#17786=EDGE_CURVE('',#14302,#14303,#7975,.T.);
#17787=EDGE_CURVE('',#14288,#14303,#11652,.T.);
#17788=EDGE_CURVE('',#14304,#14305,#7976,.T.);
#17789=EDGE_CURVE('',#14304,#14306,#11653,.T.);
#17790=EDGE_CURVE('',#14306,#14307,#11654,.T.);
#17791=EDGE_CURVE('',#14308,#14307,#11655,.T.);
#17792=EDGE_CURVE('',#14308,#14309,#7977,.T.);
#17793=EDGE_CURVE('',#14309,#14305,#11656,.T.);
#17794=EDGE_CURVE('',#14310,#14311,#11657,.T.);
#17795=EDGE_CURVE('',#14310,#14312,#11658,.T.);
#17796=EDGE_CURVE('',#14313,#14312,#7978,.T.);
#17797=EDGE_CURVE('',#14314,#14313,#7979,.T.);
#17798=EDGE_CURVE('',#14314,#14315,#11659,.T.);
#17799=EDGE_CURVE('',#14316,#14315,#7980,.T.);
#17800=EDGE_CURVE('',#14316,#14311,#7981,.T.);
#17801=EDGE_CURVE('',#14317,#14318,#7982,.T.);
#17802=EDGE_CURVE('',#14318,#14319,#7983,.T.);
#17803=EDGE_CURVE('',#14320,#14319,#11660,.T.);
#17804=EDGE_CURVE('',#14320,#14321,#11661,.T.);
#17805=EDGE_CURVE('',#14283,#14321,#7984,.T.);
#17806=EDGE_CURVE('',#14287,#14317,#11662,.T.);
#17807=EDGE_CURVE('',#14322,#14323,#11663,.T.);
#17808=EDGE_CURVE('',#14323,#14324,#11664,.T.);
#17809=EDGE_CURVE('',#14324,#14325,#7985,.T.);
#17810=EDGE_CURVE('',#14325,#14326,#7986,.T.);
#17811=EDGE_CURVE('',#14326,#14327,#11665,.T.);
#17812=EDGE_CURVE('',#14328,#14327,#7987,.T.);
#17813=EDGE_CURVE('',#14328,#14322,#11666,.T.);
#17814=EDGE_CURVE('',#14329,#14330,#7988,.T.);
#17815=EDGE_CURVE('',#14330,#14331,#11667,.T.);
#17816=EDGE_CURVE('',#14331,#14332,#11668,.T.);
#17817=EDGE_CURVE('',#14332,#14333,#11669,.T.);
#17818=EDGE_CURVE('',#14333,#14334,#11670,.T.);
#17819=EDGE_CURVE('',#14335,#14334,#11671,.T.);
#17820=EDGE_CURVE('',#14335,#14336,#11672,.T.);
#17821=EDGE_CURVE('',#14282,#14336,#7989,.T.);
#17822=EDGE_CURVE('',#14281,#14329,#11673,.T.);
#17823=EDGE_CURVE('',#14337,#14338,#11674,.T.);
#17824=EDGE_CURVE('',#14339,#14338,#11675,.T.);
#17825=EDGE_CURVE('',#14339,#14340,#7990,.T.);
#17826=EDGE_CURVE('',#14340,#14341,#11676,.T.);
#17827=EDGE_CURVE('',#14342,#14341,#7991,.T.);
#17828=EDGE_CURVE('',#14343,#14342,#7992,.T.);
#17829=EDGE_CURVE('',#14337,#14343,#11677,.T.);
#17830=EDGE_CURVE('',#14286,#14344,#11678,.T.);
#17831=EDGE_CURVE('',#14317,#14344,#7993,.T.);
#17832=EDGE_CURVE('',#14285,#14345,#587,.T.);
#17833=EDGE_CURVE('',#14344,#14345,#7994,.T.);
#17834=EDGE_CURVE('',#14284,#14346,#7995,.T.);
#17835=EDGE_CURVE('',#14347,#14346,#588,.T.);
#17836=EDGE_CURVE('',#14348,#14347,#1644,.T.);
#17837=EDGE_CURVE('',#14348,#14349,#11679,.T.);
#17838=EDGE_CURVE('',#14350,#14349,#7996,.T.);
#17839=EDGE_CURVE('',#14345,#14350,#7997,.T.);
#17840=EDGE_CURVE('',#14321,#14351,#7998,.T.);
#17841=EDGE_CURVE('',#14346,#14351,#7999,.T.);
#17842=EDGE_CURVE('',#14352,#14353,#8000,.T.);
#17843=EDGE_CURVE('',#14353,#14354,#11680,.T.);
#17844=EDGE_CURVE('',#14355,#14354,#8001,.T.);
#17845=EDGE_CURVE('',#14355,#14356,#11681,.T.);
#17846=EDGE_CURVE('',#14357,#14356,#8002,.T.);
#17847=EDGE_CURVE('',#14357,#14358,#11682,.T.);
#17848=EDGE_CURVE('',#14358,#14359,#8003,.T.);
#17849=EDGE_CURVE('',#14359,#14360,#11683,.T.);
#17850=EDGE_CURVE('',#14360,#14361,#8004,.T.);
#17851=EDGE_CURVE('',#14361,#14362,#11684,.T.);
#17852=EDGE_CURVE('',#14363,#14362,#8005,.T.);
#17853=EDGE_CURVE('',#14363,#14364,#11685,.T.);
#17854=EDGE_CURVE('',#14364,#14365,#8006,.T.);
#17855=EDGE_CURVE('',#14365,#14366,#11686,.T.);
#17856=EDGE_CURVE('',#14366,#14288,#8007,.T.);
#17857=EDGE_CURVE('',#14367,#14303,#8008,.T.);
#17858=EDGE_CURVE('',#14367,#14368,#11687,.T.);
#17859=EDGE_CURVE('',#14369,#14368,#8009,.T.);
#17860=EDGE_CURVE('',#14369,#14352,#11688,.T.);
#17861=EDGE_CURVE('',#14302,#14370,#8010,.T.);
#17862=EDGE_CURVE('',#14370,#14367,#8011,.T.);
#17863=EDGE_CURVE('',#14301,#14371,#8012,.T.);
#17864=EDGE_CURVE('',#14370,#14371,#1645,.T.);
#17865=EDGE_CURVE('',#14371,#14372,#8013,.T.);
#17866=EDGE_CURVE('',#14300,#14372,#8014,.T.);
#17867=EDGE_CURVE('',#14299,#14373,#8015,.T.);
#17868=EDGE_CURVE('',#14373,#14374,#11689,.T.);
#17869=EDGE_CURVE('',#14375,#14374,#8016,.T.);
#17870=EDGE_CURVE('',#14376,#14375,#1646,.T.);
#17871=EDGE_CURVE('',#14376,#14377,#11690,.T.);
#17872=EDGE_CURVE('',#14378,#14377,#1647,.T.);
#17873=EDGE_CURVE('',#14378,#14379,#8017,.T.);
#17874=EDGE_CURVE('',#14379,#14372,#11691,.T.);
#17875=EDGE_CURVE('',#14298,#14380,#8018,.T.);
#17876=EDGE_CURVE('',#14380,#14373,#8019,.T.);
#17877=EDGE_CURVE('',#14297,#14381,#8020,.T.);
#17878=EDGE_CURVE('',#14381,#14380,#1648,.T.);
#17879=EDGE_CURVE('',#14382,#14296,#8021,.T.);
#17880=EDGE_CURVE('',#14382,#14381,#8022,.T.);
#17881=EDGE_CURVE('',#14383,#14384,#8023,.T.);
#17882=EDGE_CURVE('',#14385,#14384,#11692,.T.);
#17883=EDGE_CURVE('',#14386,#14385,#8024,.T.);
#17884=EDGE_CURVE('',#14386,#14387,#11693,.T.);
#17885=EDGE_CURVE('',#14388,#14387,#8025,.T.);
#17886=EDGE_CURVE('',#14389,#14388,#11694,.T.);
#17887=EDGE_CURVE('',#14389,#14390,#8026,.T.);
#17888=EDGE_CURVE('',#14390,#14391,#11695,.T.);
#17889=EDGE_CURVE('',#14391,#14392,#8027,.T.);
#17890=EDGE_CURVE('',#14393,#14392,#11696,.T.);
#17891=EDGE_CURVE('',#14394,#14393,#8028,.T.);
#17892=EDGE_CURVE('',#14394,#14395,#11697,.T.);
#17893=EDGE_CURVE('',#14395,#14396,#8029,.T.);
#17894=EDGE_CURVE('',#14396,#14382,#11698,.T.);
#17895=EDGE_CURVE('',#14397,#14295,#8030,.T.);
#17896=EDGE_CURVE('',#14397,#14398,#11699,.T.);
#17897=EDGE_CURVE('',#14399,#14398,#8031,.T.);
#17898=EDGE_CURVE('',#14399,#14383,#11700,.T.);
#17899=EDGE_CURVE('',#14294,#14400,#8032,.T.);
#17900=EDGE_CURVE('',#14400,#14397,#8033,.T.);
#17901=EDGE_CURVE('',#14293,#14401,#8034,.T.);
#17902=EDGE_CURVE('',#14401,#14400,#1649,.T.);
#17903=EDGE_CURVE('',#14402,#14401,#8035,.T.);
#17904=EDGE_CURVE('',#14292,#14402,#8036,.T.);
#17905=EDGE_CURVE('',#14291,#14403,#8037,.T.);
#17906=EDGE_CURVE('',#14403,#14404,#11701,.T.);
#17907=EDGE_CURVE('',#14405,#14404,#8038,.T.);
#17908=EDGE_CURVE('',#14406,#14405,#1650,.T.);
#17909=EDGE_CURVE('',#14406,#14407,#11702,.T.);
#17910=EDGE_CURVE('',#14408,#14407,#1651,.T.);
#17911=EDGE_CURVE('',#14408,#14409,#8039,.T.);
#17912=EDGE_CURVE('',#14409,#14402,#11703,.T.);
#17913=EDGE_CURVE('',#14290,#14410,#8040,.T.);
#17914=EDGE_CURVE('',#14403,#14410,#8041,.T.);
#17915=EDGE_CURVE('',#14410,#14411,#1652,.T.);
#17916=EDGE_CURVE('',#14289,#14411,#8042,.T.);
#17917=EDGE_CURVE('',#14366,#14411,#8043,.T.);
#17918=EDGE_CURVE('',#14305,#14412,#8044,.T.);
#17919=EDGE_CURVE('',#14309,#14413,#8045,.T.);
#17920=EDGE_CURVE('',#14413,#14414,#11704,.T.);
#17921=EDGE_CURVE('',#14414,#14415,#11705,.T.);
#17922=EDGE_CURVE('',#14415,#14412,#11706,.T.);
#17923=EDGE_CURVE('',#14308,#14416,#8046,.T.);
#17924=EDGE_CURVE('',#14417,#14416,#8047,.T.);
#17925=EDGE_CURVE('',#14413,#14417,#8048,.T.);
#17926=EDGE_CURVE('',#14307,#14418,#8049,.T.);
#17927=EDGE_CURVE('',#14419,#14418,#11707,.T.);
#17928=EDGE_CURVE('',#14420,#14419,#11708,.T.);
#17929=EDGE_CURVE('',#14421,#14420,#11709,.T.);
#17930=EDGE_CURVE('',#14416,#14421,#11710,.T.);
#17931=EDGE_CURVE('',#14306,#14422,#8050,.T.);
#17932=EDGE_CURVE('',#14422,#14418,#11711,.T.);
#17933=EDGE_CURVE('',#14423,#14424,#11712,.T.);
#17934=EDGE_CURVE('',#14425,#14423,#11713,.T.);
#17935=EDGE_CURVE('',#14426,#14425,#11714,.T.);
#17936=EDGE_CURVE('',#14422,#14426,#11715,.T.);
#17937=EDGE_CURVE('',#14304,#14424,#8051,.T.);
#17938=EDGE_CURVE('',#14427,#14412,#8052,.T.);
#17939=EDGE_CURVE('',#14424,#14427,#8053,.T.);
#17940=EDGE_CURVE('',#14316,#14428,#8054,.T.);
#17941=EDGE_CURVE('',#14428,#14429,#8055,.T.);
#17942=EDGE_CURVE('',#14429,#14430,#8056,.T.);
#17943=EDGE_CURVE('',#14430,#14311,#8057,.T.);
#17944=EDGE_CURVE('',#14315,#14431,#8058,.T.);
#17945=EDGE_CURVE('',#14432,#14431,#8059,.T.);
#17946=EDGE_CURVE('',#14428,#14432,#8060,.T.);
#17947=EDGE_CURVE('',#14314,#14433,#8061,.T.);
#17948=EDGE_CURVE('',#14433,#14431,#11716,.T.);
#17949=EDGE_CURVE('',#14313,#14434,#8062,.T.);
#17950=EDGE_CURVE('',#14434,#14435,#8063,.T.);
#17951=EDGE_CURVE('',#14435,#14433,#8064,.T.);
#17952=EDGE_CURVE('',#14312,#14436,#8065,.T.);
#17953=EDGE_CURVE('',#14434,#14436,#8066,.T.);
#17954=EDGE_CURVE('',#14437,#14310,#8067,.T.);
#17955=EDGE_CURVE('',#14438,#14437,#11717,.T.);
#17956=EDGE_CURVE('',#14436,#14438,#11718,.T.);
#17957=EDGE_CURVE('',#14437,#14430,#11719,.T.);
#17958=EDGE_CURVE('',#14320,#14439,#8068,.T.);
#17959=EDGE_CURVE('',#14439,#14351,#11720,.T.);
#17960=EDGE_CURVE('',#14439,#14348,#11721,.T.);
#17961=EDGE_CURVE('',#14319,#14349,#8069,.T.);
#17962=EDGE_CURVE('',#14318,#14350,#8070,.T.);
#17963=EDGE_CURVE('',#14440,#14328,#8071,.T.);
#17964=EDGE_CURVE('',#14440,#14441,#11722,.T.);
#17965=EDGE_CURVE('',#14441,#14322,#8072,.T.);
#17966=EDGE_CURVE('',#14327,#14442,#8073,.T.);
#17967=EDGE_CURVE('',#14442,#14440,#8074,.T.);
#17968=EDGE_CURVE('',#14326,#14443,#8075,.T.);
#17969=EDGE_CURVE('',#14443,#14444,#11723,.T.);
#17970=EDGE_CURVE('',#14444,#14442,#11724,.T.);
#17971=EDGE_CURVE('',#14325,#14445,#8076,.T.);
#17972=EDGE_CURVE('',#14445,#14446,#8077,.T.);
#17973=EDGE_CURVE('',#14446,#14443,#8078,.T.);
#17974=EDGE_CURVE('',#14324,#14447,#8079,.T.);
#17975=EDGE_CURVE('',#14447,#14445,#8080,.T.);
#17976=EDGE_CURVE('',#14448,#14447,#11725,.T.);
#17977=EDGE_CURVE('',#14448,#14323,#8081,.T.);
#17978=EDGE_CURVE('',#14449,#14449,#11726,.T.);
#17979=EDGE_CURVE('',#14449,#14450,#8082,.T.);
#17980=EDGE_CURVE('',#14450,#14448,#11727,.T.);
#17981=EDGE_CURVE('',#14441,#14451,#11728,.T.);
#17982=EDGE_CURVE('',#14451,#14452,#11729,.T.);
#17983=EDGE_CURVE('',#14452,#14450,#11730,.T.);
#17984=EDGE_CURVE('',#14329,#14453,#8083,.T.);
#17985=EDGE_CURVE('',#14279,#14453,#11731,.T.);
#17986=EDGE_CURVE('',#14336,#14454,#8084,.T.);
#17987=EDGE_CURVE('',#14280,#14454,#8085,.T.);
#17988=EDGE_CURVE('',#14455,#14454,#11732,.T.);
#17989=EDGE_CURVE('',#14335,#14455,#8086,.T.);
#17990=EDGE_CURVE('',#14455,#14456,#11733,.T.);
#17991=EDGE_CURVE('',#14334,#14456,#8087,.T.);
#17992=EDGE_CURVE('',#14457,#14456,#11734,.T.);
#17993=EDGE_CURVE('',#14333,#14457,#8088,.T.);
#17994=EDGE_CURVE('',#14458,#14457,#11735,.T.);
#17995=EDGE_CURVE('',#14332,#14458,#8089,.T.);
#17996=EDGE_CURVE('',#14331,#14459,#8090,.T.);
#17997=EDGE_CURVE('',#14459,#14458,#11736,.T.);
#17998=EDGE_CURVE('',#14460,#14459,#11737,.T.);
#17999=EDGE_CURVE('',#14330,#14460,#8091,.T.);
#18000=EDGE_CURVE('',#14453,#14460,#8092,.T.);
#18001=EDGE_CURVE('',#14343,#14461,#8093,.T.);
#18002=EDGE_CURVE('',#14462,#14461,#11738,.T.);
#18003=EDGE_CURVE('',#14462,#14337,#8094,.T.);
#18004=EDGE_CURVE('',#14461,#14463,#8095,.T.);
#18005=EDGE_CURVE('',#14342,#14463,#8096,.T.);
#18006=EDGE_CURVE('',#14341,#14464,#8097,.T.);
#18007=EDGE_CURVE('',#14465,#14464,#8098,.T.);
#18008=EDGE_CURVE('',#14463,#14465,#8099,.T.);
#18009=EDGE_CURVE('',#14340,#14466,#8100,.T.);
#18010=EDGE_CURVE('',#14466,#14467,#11739,.T.);
#18011=EDGE_CURVE('',#14467,#14464,#11740,.T.);
#18012=EDGE_CURVE('',#14339,#14468,#8101,.T.);
#18013=EDGE_CURVE('',#14466,#14468,#8102,.T.);
#18014=EDGE_CURVE('',#14468,#14469,#11741,.T.);
#18015=EDGE_CURVE('',#14469,#14338,#8103,.T.);
#18016=EDGE_CURVE('',#14470,#14471,#11742,.T.);
#18017=EDGE_CURVE('',#14472,#14470,#11743,.T.);
#18018=EDGE_CURVE('',#14469,#14472,#11744,.T.);
#18019=EDGE_CURVE('',#14471,#14462,#11745,.T.);
#18020=EDGE_CURVE('',#14471,#14473,#8104,.T.);
#18021=EDGE_CURVE('',#14474,#14473,#11746,.T.);
#18022=EDGE_CURVE('',#14473,#14474,#11747,.T.);
#18023=EDGE_CURVE('',#14379,#14368,#8105,.T.);
#18024=EDGE_CURVE('',#14378,#14475,#8106,.T.);
#18025=EDGE_CURVE('',#14475,#14369,#8107,.T.);
#18026=EDGE_CURVE('',#14476,#14477,#8108,.T.);
#18027=EDGE_CURVE('',#14476,#14478,#8109,.T.);
#18028=EDGE_CURVE('',#14479,#14478,#8110,.T.);
#18029=EDGE_CURVE('',#14357,#14479,#8111,.T.);
#18030=EDGE_CURVE('',#14480,#14356,#8112,.T.);
#18031=EDGE_CURVE('',#14481,#14480,#8113,.T.);
#18032=EDGE_CURVE('',#14477,#14481,#8114,.T.);
#18033=EDGE_CURVE('',#14482,#14479,#11748,.T.);
#18034=EDGE_CURVE('',#14358,#14482,#8115,.T.);
#18035=EDGE_CURVE('',#14483,#14484,#8116,.T.);
#18036=EDGE_CURVE('',#14484,#14485,#8117,.T.);
#18037=EDGE_CURVE('',#14485,#14359,#8118,.T.);
#18038=EDGE_CURVE('',#14482,#14486,#8119,.T.);
#18039=EDGE_CURVE('',#14487,#14486,#8120,.T.);
#18040=EDGE_CURVE('',#14487,#14483,#8121,.T.);
#18041=EDGE_CURVE('',#14488,#14405,#8122,.T.);
#18042=EDGE_CURVE('',#14365,#14404,#8123,.T.);
#18043=EDGE_CURVE('',#14488,#14364,#8124,.T.);
#18044=EDGE_CURVE('',#14374,#14396,#8125,.T.);
#18045=EDGE_CURVE('',#14489,#14395,#8126,.T.);
#18046=EDGE_CURVE('',#14375,#14489,#8127,.T.);
#18047=EDGE_CURVE('',#14398,#14409,#8128,.T.);
#18048=EDGE_CURVE('',#14490,#14399,#8129,.T.);
#18049=EDGE_CURVE('',#14490,#14408,#8130,.T.);
#18050=EDGE_CURVE('',#14387,#14491,#8131,.T.);
#18051=EDGE_CURVE('',#14492,#14491,#8132,.T.);
#18052=EDGE_CURVE('',#14492,#14493,#8133,.T.);
#18053=EDGE_CURVE('',#14494,#14493,#8134,.T.);
#18054=EDGE_CURVE('',#14494,#14495,#8135,.T.);
#18055=EDGE_CURVE('',#14496,#14495,#8136,.T.);
#18056=EDGE_CURVE('',#14388,#14496,#8137,.T.);
#18057=EDGE_CURVE('',#14496,#14497,#11749,.T.);
#18058=EDGE_CURVE('',#14389,#14497,#8138,.T.);
#18059=EDGE_CURVE('',#14497,#14498,#8139,.T.);
#18060=EDGE_CURVE('',#14499,#14498,#8140,.T.);
#18061=EDGE_CURVE('',#14499,#14500,#8141,.T.);
#18062=EDGE_CURVE('',#14501,#14500,#8142,.T.);
#18063=EDGE_CURVE('',#14501,#14502,#8143,.T.);
#18064=EDGE_CURVE('',#14390,#14502,#8144,.T.);
#18065=EDGE_CURVE('',#14503,#14407,#8145,.T.);
#18066=EDGE_CURVE('',#14504,#14406,#8146,.T.);
#18067=EDGE_CURVE('',#14504,#14503,#11750,.T.);
#18068=EDGE_CURVE('',#14503,#14490,#1653,.T.);
#18069=EDGE_CURVE('',#14504,#14488,#1654,.T.);
#18070=EDGE_CURVE('',#14505,#14415,#8147,.T.);
#18071=EDGE_CURVE('',#14505,#14427,#1655,.T.);
#18072=EDGE_CURVE('',#14506,#14421,#1656,.T.);
#18073=EDGE_CURVE('',#14506,#14507,#589,.T.);
#18074=EDGE_CURVE('',#14507,#14423,#1657,.T.);
#18075=EDGE_CURVE('',#14508,#14414,#8148,.T.);
#18076=EDGE_CURVE('',#14417,#14508,#1658,.T.);
#18077=EDGE_CURVE('',#14420,#14509,#1659,.T.);
#18078=EDGE_CURVE('',#14419,#14509,#8149,.T.);
#18079=EDGE_CURVE('',#14426,#14510,#8150,.T.);
#18080=EDGE_CURVE('',#14510,#14425,#1660,.T.);
#18081=EDGE_CURVE('',#14438,#14511,#1661,.T.);
#18082=EDGE_CURVE('',#14429,#14511,#590,.T.);
#18083=EDGE_CURVE('',#14435,#14432,#591,.T.);
#18084=EDGE_CURVE('',#14444,#14512,#8151,.T.);
#18085=EDGE_CURVE('',#14451,#14512,#592,.T.);
#18086=EDGE_CURVE('',#14446,#14452,#593,.T.);
#18087=EDGE_CURVE('',#14449,#14513,#11751,.T.);
#18088=EDGE_CURVE('',#14513,#14513,#11752,.T.);
#18089=EDGE_CURVE('',#14514,#14515,#11753,.T.);
#18090=EDGE_CURVE('',#14516,#14514,#11754,.T.);
#18091=EDGE_CURVE('',#14517,#14516,#11755,.T.);
#18092=EDGE_CURVE('',#14517,#14518,#11756,.T.);
#18093=EDGE_CURVE('',#14519,#14518,#11757,.T.);
#18094=EDGE_CURVE('',#14520,#14519,#8152,.T.);
#18095=EDGE_CURVE('',#14521,#14520,#11758,.T.);
#18096=EDGE_CURVE('',#14521,#14522,#11759,.T.);
#18097=EDGE_CURVE('',#14522,#14515,#8153,.T.);
#18098=EDGE_CURVE('',#14523,#14523,#11760,.T.);
#18099=EDGE_CURVE('',#14524,#14524,#11761,.T.);
#18100=EDGE_CURVE('',#14470,#14465,#594,.T.);
#18101=EDGE_CURVE('',#14467,#14525,#8154,.T.);
#18102=EDGE_CURVE('',#14525,#14472,#595,.T.);
#18103=EDGE_CURVE('',#14474,#14526,#11762,.T.);
#18104=EDGE_CURVE('',#14526,#14526,#11763,.T.);
#18105=EDGE_CURVE('',#14377,#14527,#8155,.T.);
#18106=EDGE_CURVE('',#14527,#14475,#1662,.T.);
#18107=EDGE_CURVE('',#14528,#14527,#11764,.T.);
#18108=EDGE_CURVE('',#14489,#14528,#1663,.T.);
#18109=EDGE_CURVE('',#14395,#14369,#11765,.T.);
#18110=EDGE_CURVE('',#14529,#14530,#8156,.T.);
#18111=EDGE_CURVE('',#14529,#14481,#11766,.T.);
#18112=EDGE_CURVE('',#14480,#14530,#11767,.T.);
#18113=EDGE_CURVE('',#14531,#14532,#11768,.T.);
#18114=EDGE_CURVE('',#14533,#14532,#8157,.T.);
#18115=EDGE_CURVE('',#14533,#14534,#11769,.T.);
#18116=EDGE_CURVE('',#14534,#14531,#8158,.T.);
#18117=EDGE_CURVE('',#14535,#14536,#8159,.T.);
#18118=EDGE_CURVE('',#14536,#14537,#11770,.T.);
#18119=EDGE_CURVE('',#14538,#14537,#8160,.T.);
#18120=EDGE_CURVE('',#14538,#14535,#11771,.T.);
#18121=EDGE_CURVE('',#14539,#14540,#8161,.T.);
#18122=EDGE_CURVE('',#14539,#14541,#11772,.T.);
#18123=EDGE_CURVE('',#14541,#14542,#8162,.T.);
#18124=EDGE_CURVE('',#14542,#14540,#11773,.T.);
#18125=EDGE_CURVE('',#14543,#14544,#11774,.T.);
#18126=EDGE_CURVE('',#14545,#14544,#8163,.T.);
#18127=EDGE_CURVE('',#14546,#14545,#11775,.T.);
#18128=EDGE_CURVE('',#14546,#14543,#8164,.T.);
#18129=EDGE_CURVE('',#14547,#14548,#8165,.T.);
#18130=EDGE_CURVE('',#14548,#14502,#11776,.T.);
#18131=EDGE_CURVE('',#14501,#14547,#11777,.T.);
#18132=EDGE_CURVE('',#14476,#14487,#8166,.T.);
#18133=EDGE_CURVE('',#14477,#14483,#8167,.T.);
#18134=EDGE_CURVE('',#14486,#14478,#11778,.T.);
#18135=EDGE_CURVE('',#14549,#14550,#8168,.T.);
#18136=EDGE_CURVE('',#14551,#14550,#1664,.T.);
#18137=EDGE_CURVE('',#14552,#14551,#11779,.T.);
#18138=EDGE_CURVE('',#14552,#14553,#8169,.T.);
#18139=EDGE_CURVE('',#14549,#14553,#11780,.T.);
#18140=EDGE_CURVE('',#14554,#14555,#11781,.T.);
#18141=EDGE_CURVE('',#14554,#14556,#11782,.T.);
#18142=EDGE_CURVE('',#14556,#14557,#8170,.T.);
#18143=EDGE_CURVE('',#14558,#14557,#1665,.T.);
#18144=EDGE_CURVE('',#14559,#14558,#8171,.T.);
#18145=EDGE_CURVE('',#14559,#14555,#11783,.T.);
#18146=EDGE_CURVE('',#14560,#14561,#8172,.T.);
#18147=EDGE_CURVE('',#14484,#14560,#11784,.T.);
#18148=EDGE_CURVE('',#14562,#14529,#8173,.T.);
#18149=EDGE_CURVE('',#14563,#14562,#11785,.T.);
#18150=EDGE_CURVE('',#14563,#14564,#8174,.T.);
#18151=EDGE_CURVE('',#14565,#14564,#11786,.T.);
#18152=EDGE_CURVE('',#14565,#14566,#8175,.T.);
#18153=EDGE_CURVE('',#14566,#14532,#11787,.T.);
#18154=EDGE_CURVE('',#14531,#14567,#11788,.T.);
#18155=EDGE_CURVE('',#14568,#14567,#8176,.T.);
#18156=EDGE_CURVE('',#14569,#14568,#11789,.T.);
#18157=EDGE_CURVE('',#14569,#14570,#8177,.T.);
#18158=EDGE_CURVE('',#14571,#14570,#11790,.T.);
#18159=EDGE_CURVE('',#14571,#14535,#8178,.T.);
#18160=EDGE_CURVE('',#14538,#14572,#8179,.T.);
#18161=EDGE_CURVE('',#14572,#14573,#11791,.T.);
#18162=EDGE_CURVE('',#14573,#14574,#11792,.T.);
#18163=EDGE_CURVE('',#14575,#14574,#1666,.T.);
#18164=EDGE_CURVE('',#14575,#14576,#1667,.T.);
#18165=EDGE_CURVE('',#14561,#14576,#1668,.T.);
#18166=EDGE_CURVE('',#14560,#14577,#8180,.T.);
#18167=EDGE_CURVE('',#14577,#14485,#11793,.T.);
#18168=EDGE_CURVE('',#14578,#14555,#8181,.T.);
#18169=EDGE_CURVE('',#14578,#14579,#11794,.T.);
#18170=EDGE_CURVE('',#14579,#14554,#8182,.T.);
#18171=EDGE_CURVE('',#14549,#14580,#8183,.T.);
#18172=EDGE_CURVE('',#14553,#14581,#8184,.T.);
#18173=EDGE_CURVE('',#14581,#14580,#11795,.T.);
#18174=EDGE_CURVE('',#14582,#14583,#8185,.T.);
#18175=EDGE_CURVE('',#14583,#14584,#11796,.T.);
#18176=EDGE_CURVE('',#14585,#14584,#8186,.T.);
#18177=EDGE_CURVE('',#14585,#14582,#11797,.T.);
#18178=EDGE_CURVE('',#14586,#14587,#11798,.T.);
#18179=EDGE_CURVE('',#14588,#14587,#8187,.T.);
#18180=EDGE_CURVE('',#14589,#14588,#11799,.T.);
#18181=EDGE_CURVE('',#14589,#14586,#8188,.T.);
#18182=EDGE_CURVE('',#14590,#14591,#8189,.T.);
#18183=EDGE_CURVE('',#14590,#14492,#11800,.T.);
#18184=EDGE_CURVE('',#14491,#14591,#11801,.T.);
#18185=EDGE_CURVE('',#14364,#14399,#11802,.T.);
#18186=EDGE_CURVE('',#14376,#14528,#8190,.T.);
#18187=EDGE_CURVE('',#14495,#14498,#11803,.T.);
#18188=EDGE_CURVE('',#14499,#14494,#8191,.T.);
#18189=EDGE_CURVE('',#14500,#14493,#8192,.T.);
#18190=EDGE_CURVE('',#14592,#14585,#8193,.T.);
#18191=EDGE_CURVE('',#14593,#14592,#11804,.T.);
#18192=EDGE_CURVE('',#14593,#14594,#1669,.T.);
#18193=EDGE_CURVE('',#14582,#14594,#8194,.T.);
#18194=EDGE_CURVE('',#14595,#14596,#8195,.T.);
#18195=EDGE_CURVE('',#14595,#14587,#11805,.T.);
#18196=EDGE_CURVE('',#14586,#14597,#11806,.T.);
#18197=EDGE_CURVE('',#14597,#14598,#8196,.T.);
#18198=EDGE_CURVE('',#14598,#14596,#1670,.T.);
#18199=EDGE_CURVE('',#14543,#14599,#11807,.T.);
#18200=EDGE_CURVE('',#14600,#14599,#8197,.T.);
#18201=EDGE_CURVE('',#14601,#14600,#11808,.T.);
#18202=EDGE_CURVE('',#14602,#14601,#8198,.T.);
#18203=EDGE_CURVE('',#14603,#14602,#11809,.T.);
#18204=EDGE_CURVE('',#14603,#14547,#8199,.T.);
#18205=EDGE_CURVE('',#14590,#14604,#8200,.T.);
#18206=EDGE_CURVE('',#14604,#14605,#1671,.T.);
#18207=EDGE_CURVE('',#14606,#14605,#1672,.T.);
#18208=EDGE_CURVE('',#14606,#14607,#1673,.T.);
#18209=EDGE_CURVE('',#14608,#14607,#11810,.T.);
#18210=EDGE_CURVE('',#14609,#14608,#11811,.T.);
#18211=EDGE_CURVE('',#14541,#14609,#8201,.T.);
#18212=EDGE_CURVE('',#14610,#14539,#8202,.T.);
#18213=EDGE_CURVE('',#14611,#14610,#11812,.T.);
#18214=EDGE_CURVE('',#14612,#14611,#8203,.T.);
#18215=EDGE_CURVE('',#14613,#14612,#11813,.T.);
#18216=EDGE_CURVE('',#14613,#14614,#8204,.T.);
#18217=EDGE_CURVE('',#14614,#14544,#11814,.T.);
#18218=EDGE_CURVE('',#14615,#14615,#11815,.T.);
#18219=EDGE_CURVE('',#14616,#14515,#8205,.T.);
#18220=EDGE_CURVE('',#14616,#14617,#11816,.T.);
#18221=EDGE_CURVE('',#14617,#14514,#8206,.T.);
#18222=EDGE_CURVE('',#14617,#14618,#11817,.T.);
#18223=EDGE_CURVE('',#14618,#14516,#8207,.T.);
#18224=EDGE_CURVE('',#14618,#14619,#11818,.T.);
#18225=EDGE_CURVE('',#14619,#14517,#8208,.T.);
#18226=EDGE_CURVE('',#14620,#14518,#8209,.T.);
#18227=EDGE_CURVE('',#14620,#14619,#11819,.T.);
#18228=EDGE_CURVE('',#14620,#14621,#11820,.T.);
#18229=EDGE_CURVE('',#14621,#14519,#8210,.T.);
#18230=EDGE_CURVE('',#14622,#14621,#8211,.T.);
#18231=EDGE_CURVE('',#14622,#14520,#8212,.T.);
#18232=EDGE_CURVE('',#14623,#14622,#11821,.T.);
#18233=EDGE_CURVE('',#14623,#14521,#8213,.T.);
#18234=EDGE_CURVE('',#14623,#14624,#11822,.T.);
#18235=EDGE_CURVE('',#14624,#14522,#8214,.T.);
#18236=EDGE_CURVE('',#14624,#14616,#8215,.T.);
#18237=EDGE_CURVE('',#14523,#14625,#8216,.T.);
#18238=EDGE_CURVE('',#14625,#14625,#11823,.T.);
#18239=EDGE_CURVE('',#14626,#14626,#11824,.T.);
#18240=EDGE_CURVE('',#14626,#14524,#8217,.T.);
#18241=EDGE_CURVE('',#14627,#14627,#11825,.T.);
#18242=EDGE_CURVE('',#14628,#14629,#11826,.T.);
#18243=EDGE_CURVE('',#14573,#14629,#8218,.T.);
#18244=EDGE_CURVE('',#14572,#14628,#8219,.T.);
#18245=EDGE_CURVE('',#14630,#14629,#11827,.T.);
#18246=EDGE_CURVE('',#14574,#14630,#8220,.T.);
#18247=EDGE_CURVE('',#14575,#14631,#8221,.T.);
#18248=EDGE_CURVE('',#14631,#14630,#1674,.T.);
#18249=EDGE_CURVE('',#14631,#14632,#1675,.T.);
#18250=EDGE_CURVE('',#14576,#14632,#8222,.T.);
#18251=EDGE_CURVE('',#14633,#14632,#1676,.T.);
#18252=EDGE_CURVE('',#14561,#14633,#8223,.T.);
#18253=EDGE_CURVE('',#14557,#14634,#8224,.T.);
#18254=EDGE_CURVE('',#14635,#14634,#1677,.T.);
#18255=EDGE_CURVE('',#14558,#14635,#8225,.T.);
#18256=EDGE_CURVE('',#14636,#14637,#1678,.T.);
#18257=EDGE_CURVE('',#14551,#14636,#8226,.T.);
#18258=EDGE_CURVE('',#14550,#14637,#8227,.T.);
#18259=EDGE_CURVE('',#14636,#14638,#11828,.T.);
#18260=EDGE_CURVE('',#14552,#14638,#8228,.T.);
#18261=EDGE_CURVE('',#14639,#14640,#11829,.T.);
#18262=EDGE_CURVE('',#14593,#14640,#8229,.T.);
#18263=EDGE_CURVE('',#14592,#14639,#8230,.T.);
#18264=EDGE_CURVE('',#14594,#14641,#8231,.T.);
#18265=EDGE_CURVE('',#14640,#14641,#1679,.T.);
#18266=EDGE_CURVE('',#14596,#14642,#8232,.T.);
#18267=EDGE_CURVE('',#14598,#14643,#8233,.T.);
#18268=EDGE_CURVE('',#14643,#14642,#1680,.T.);
#18269=EDGE_CURVE('',#14604,#14644,#8234,.T.);
#18270=EDGE_CURVE('',#14644,#14645,#1681,.T.);
#18271=EDGE_CURVE('',#14605,#14645,#8235,.T.);
#18272=EDGE_CURVE('',#14606,#14646,#8236,.T.);
#18273=EDGE_CURVE('',#14646,#14645,#1682,.T.);
#18274=EDGE_CURVE('',#14646,#14647,#1683,.T.);
#18275=EDGE_CURVE('',#14647,#14607,#8237,.T.);
#18276=EDGE_CURVE('',#14648,#14647,#11830,.T.);
#18277=EDGE_CURVE('',#14648,#14608,#8238,.T.);
#18278=EDGE_CURVE('',#14649,#14648,#11831,.T.);
#18279=EDGE_CURVE('',#14609,#14649,#8239,.T.);
#18280=EDGE_CURVE('',#14650,#14650,#11832,.T.);
#18281=EDGE_CURVE('',#14650,#14615,#8240,.T.);
#18282=EDGE_CURVE('',#14651,#14275,#11833,.T.);
#18283=EDGE_CURVE('',#14652,#14274,#8241,.T.);
#18284=EDGE_CURVE('',#14653,#14652,#11834,.T.);
#18285=EDGE_CURVE('',#14653,#14654,#11835,.T.);
#18286=EDGE_CURVE('',#14654,#14651,#8242,.T.);
#18287=EDGE_CURVE('',#14655,#14655,#11836,.T.);
#18288=EDGE_CURVE('',#14656,#14656,#11837,.T.);
#18289=EDGE_CURVE('',#14627,#14657,#8243,.T.);
#18290=EDGE_CURVE('',#14657,#14657,#11838,.T.);
#18291=EDGE_CURVE('',#14651,#14658,#8244,.T.);
#18292=EDGE_CURVE('',#14658,#14659,#11839,.T.);
#18293=EDGE_CURVE('',#14659,#14276,#11840,.T.);
#18294=EDGE_CURVE('',#14660,#14278,#8245,.T.);
#18295=EDGE_CURVE('',#14661,#14660,#1684,.T.);
#18296=EDGE_CURVE('',#14662,#14661,#8246,.T.);
#18297=EDGE_CURVE('',#14652,#14662,#8247,.T.);
#18298=EDGE_CURVE('',#14663,#14662,#11841,.T.);
#18299=EDGE_CURVE('',#14664,#14663,#11842,.T.);
#18300=EDGE_CURVE('',#14653,#14664,#8248,.T.);
#18301=EDGE_CURVE('',#14664,#14665,#11843,.T.);
#18302=EDGE_CURVE('',#14665,#14666,#11844,.T.);
#18303=EDGE_CURVE('',#14654,#14666,#8249,.T.);
#18304=EDGE_CURVE('',#14666,#14667,#8250,.T.);
#18305=EDGE_CURVE('',#14667,#14668,#8251,.T.);
#18306=EDGE_CURVE('',#14668,#14658,#8252,.T.);
#18307=EDGE_CURVE('',#14655,#14669,#8253,.T.);
#18308=EDGE_CURVE('',#14670,#14669,#11845,.T.);
#18309=EDGE_CURVE('',#14671,#14670,#11846,.T.);
#18310=EDGE_CURVE('',#14672,#14671,#11847,.T.);
#18311=EDGE_CURVE('',#14673,#14672,#11848,.T.);
#18312=EDGE_CURVE('',#14674,#14673,#11849,.T.);
#18313=EDGE_CURVE('',#14675,#14674,#11850,.T.);
#18314=EDGE_CURVE('',#14669,#14675,#11851,.T.);
#18315=EDGE_CURVE('',#14676,#14677,#11852,.T.);
#18316=EDGE_CURVE('',#14677,#14656,#8254,.T.);
#18317=EDGE_CURVE('',#14677,#14678,#11853,.T.);
#18318=EDGE_CURVE('',#14678,#14679,#11854,.T.);
#18319=EDGE_CURVE('',#14679,#14680,#11855,.T.);
#18320=EDGE_CURVE('',#14680,#14681,#11856,.T.);
#18321=EDGE_CURVE('',#14681,#14682,#11857,.T.);
#18322=EDGE_CURVE('',#14682,#14676,#11858,.T.);
#18323=EDGE_CURVE('',#14683,#14684,#11859,.T.);
#18324=EDGE_CURVE('',#14685,#14683,#8255,.T.);
#18325=EDGE_CURVE('',#14685,#14686,#11860,.T.);
#18326=EDGE_CURVE('',#14684,#14686,#8256,.T.);
#18327=EDGE_CURVE('',#14687,#14688,#8257,.T.);
#18328=EDGE_CURVE('',#14687,#14684,#11861,.T.);
#18329=EDGE_CURVE('',#14688,#14686,#11862,.T.);
#18330=EDGE_CURVE('',#14689,#14688,#1685,.T.);
#18331=EDGE_CURVE('',#14689,#14690,#8258,.T.);
#18332=EDGE_CURVE('',#14690,#14687,#1686,.T.);
#18333=EDGE_CURVE('',#14691,#14692,#8259,.T.);
#18334=EDGE_CURVE('',#14690,#14692,#1687,.T.);
#18335=EDGE_CURVE('',#14689,#14691,#1688,.T.);
#18336=EDGE_CURVE('',#14693,#14692,#1689,.T.);
#18337=EDGE_CURVE('',#14694,#14691,#1690,.T.);
#18338=EDGE_CURVE('',#14693,#14694,#8260,.T.);
#18339=EDGE_CURVE('',#14693,#14695,#11863,.T.);
#18340=EDGE_CURVE('',#14694,#14696,#11864,.T.);
#18341=EDGE_CURVE('',#14695,#14696,#8261,.T.);
#18342=EDGE_CURVE('',#14697,#14698,#8262,.T.);
#18343=EDGE_CURVE('',#14695,#14698,#1691,.T.);
#18344=EDGE_CURVE('',#14696,#14697,#1692,.T.);
#18345=EDGE_CURVE('',#14699,#14698,#1693,.T.);
#18346=EDGE_CURVE('',#14700,#14697,#1694,.T.);
#18347=EDGE_CURVE('',#14700,#14699,#8263,.T.);
#18348=EDGE_CURVE('',#14701,#14702,#8264,.T.);
#18349=EDGE_CURVE('',#14699,#14702,#1695,.T.);
#18350=EDGE_CURVE('',#14700,#14701,#1696,.T.);
#18351=EDGE_CURVE('',#14703,#14704,#8265,.T.);
#18352=EDGE_CURVE('',#14704,#14702,#11865,.T.);
#18353=EDGE_CURVE('',#14701,#14703,#11866,.T.);
#18354=EDGE_CURVE('',#14683,#14704,#11867,.T.);
#18355=EDGE_CURVE('',#14685,#14703,#11868,.T.);
#18356=EDGE_CURVE('',#14705,#14659,#596,.T.);
#18357=EDGE_CURVE('',#14705,#14277,#597,.T.);
#18358=EDGE_CURVE('',#14706,#14668,#1697,.T.);
#18359=EDGE_CURVE('',#14707,#14706,#11869,.T.);
#18360=EDGE_CURVE('',#14707,#14708,#11870,.T.);
#18361=EDGE_CURVE('',#14708,#14660,#1698,.T.);
#18362=EDGE_CURVE('',#14661,#14663,#1699,.T.);
#18363=EDGE_CURVE('',#14709,#14710,#1700,.T.);
#18364=EDGE_CURVE('',#14710,#14711,#8266,.T.);
#18365=EDGE_CURVE('',#14663,#14711,#1701,.T.);
#18366=EDGE_CURVE('',#14709,#14708,#8267,.T.);
#18367=EDGE_CURVE('',#14712,#14711,#1702,.T.);
#18368=EDGE_CURVE('',#14713,#14712,#11871,.T.);
#18369=EDGE_CURVE('',#14713,#14714,#1703,.T.);
#18370=EDGE_CURVE('',#14665,#14714,#1704,.T.);
#18371=EDGE_CURVE('',#14667,#14665,#1705,.T.);
#18372=EDGE_CURVE('',#14715,#14706,#8268,.T.);
#18373=EDGE_CURVE('',#14716,#14714,#8269,.T.);
#18374=EDGE_CURVE('',#14715,#14716,#1706,.T.);
#18375=EDGE_CURVE('',#14717,#14671,#598,.T.);
#18376=EDGE_CURVE('',#14717,#14718,#11872,.T.);
#18377=EDGE_CURVE('',#14674,#14718,#1707,.T.);
#18378=EDGE_CURVE('',#14673,#14719,#1708,.T.);
#18379=EDGE_CURVE('',#14720,#14719,#599,.T.);
#18380=EDGE_CURVE('',#14720,#14672,#1709,.T.);
#18381=EDGE_CURVE('',#14721,#14674,#1710,.T.);
#18382=EDGE_CURVE('',#14722,#14721,#1711,.T.);
#18383=EDGE_CURVE('',#14723,#14722,#1712,.T.);
#18384=EDGE_CURVE('',#14723,#14724,#1713,.T.);
#18385=EDGE_CURVE('',#14675,#14724,#600,.T.);
#18386=EDGE_CURVE('',#14670,#14675,#1714,.T.);
#18387=EDGE_CURVE('',#14725,#14670,#1715,.T.);
#18388=EDGE_CURVE('',#14725,#14726,#11873,.T.);
#18389=EDGE_CURVE('',#14727,#14726,#8270,.T.);
#18390=EDGE_CURVE('',#14727,#14728,#11874,.T.);
#18391=EDGE_CURVE('',#14671,#14728,#601,.T.);
#18392=EDGE_CURVE('',#14676,#14678,#1716,.T.);
#18393=EDGE_CURVE('',#14682,#14729,#602,.T.);
#18394=EDGE_CURVE('',#14730,#14729,#11875,.T.);
#18395=EDGE_CURVE('',#14730,#14731,#8271,.T.);
#18396=EDGE_CURVE('',#14732,#14731,#11876,.T.);
#18397=EDGE_CURVE('',#14732,#14676,#1717,.T.);
#18398=EDGE_CURVE('',#14679,#14733,#1718,.T.);
#18399=EDGE_CURVE('',#14734,#14733,#11877,.T.);
#18400=EDGE_CURVE('',#14734,#14682,#603,.T.);
#18401=EDGE_CURVE('',#14735,#14681,#1719,.T.);
#18402=EDGE_CURVE('',#14735,#14736,#604,.T.);
#18403=EDGE_CURVE('',#14680,#14736,#1720,.T.);
#18404=EDGE_CURVE('',#14678,#14737,#605,.T.);
#18405=EDGE_CURVE('',#14738,#14737,#1721,.T.);
#18406=EDGE_CURVE('',#14738,#14739,#1722,.T.);
#18407=EDGE_CURVE('',#14739,#14740,#1723,.T.);
#18408=EDGE_CURVE('',#14740,#14679,#1724,.T.);
#18409=EDGE_CURVE('',#14741,#14742,#1725,.T.);
#18410=EDGE_CURVE('',#14742,#14743,#1726,.T.);
#18411=EDGE_CURVE('',#14743,#14744,#11878,.T.);
#18412=EDGE_CURVE('',#14744,#14745,#11879,.T.);
#18413=EDGE_CURVE('',#14745,#14746,#8272,.T.);
#18414=EDGE_CURVE('',#14747,#14746,#11880,.T.);
#18415=EDGE_CURVE('',#14748,#14747,#11881,.T.);
#18416=EDGE_CURVE('',#14748,#14749,#1727,.T.);
#18417=EDGE_CURVE('',#14741,#14749,#1728,.T.);
#18418=EDGE_CURVE('',#14750,#14751,#1729,.T.);
#18419=EDGE_CURVE('',#14752,#14751,#1730,.T.);
#18420=EDGE_CURVE('',#14753,#14752,#11882,.T.);
#18421=EDGE_CURVE('',#14753,#14754,#1731,.T.);
#18422=EDGE_CURVE('',#14755,#14754,#1732,.T.);
#18423=EDGE_CURVE('',#14756,#14755,#11883,.T.);
#18424=EDGE_CURVE('',#14756,#14750,#11884,.T.);
#18425=EDGE_CURVE('',#14757,#14758,#11885,.T.);
#18426=EDGE_CURVE('',#14758,#14759,#11886,.T.);
#18427=EDGE_CURVE('',#14760,#14759,#8273,.T.);
#18428=EDGE_CURVE('',#14761,#14760,#11887,.T.);
#18429=EDGE_CURVE('',#14762,#14761,#11888,.T.);
#18430=EDGE_CURVE('',#14763,#14762,#1733,.T.);
#18431=EDGE_CURVE('',#14764,#14763,#1734,.T.);
#18432=EDGE_CURVE('',#14764,#14765,#1735,.T.);
#18433=EDGE_CURVE('',#14757,#14765,#1736,.T.);
#18434=EDGE_CURVE('',#14766,#14709,#11889,.T.);
#18435=EDGE_CURVE('',#14766,#14707,#8274,.T.);
#18436=EDGE_CURVE('',#14766,#14715,#11890,.T.);
#18437=EDGE_CURVE('',#14767,#14710,#1737,.T.);
#18438=EDGE_CURVE('',#14767,#14712,#8275,.T.);
#18439=EDGE_CURVE('',#14768,#14769,#1738,.T.);
#18440=EDGE_CURVE('',#14770,#14769,#1739,.T.);
#18441=EDGE_CURVE('',#14771,#14770,#11891,.T.);
#18442=EDGE_CURVE('',#14771,#14772,#11892,.T.);
#18443=EDGE_CURVE('',#14772,#14773,#1740,.T.);
#18444=EDGE_CURVE('',#14774,#14773,#1741,.T.);
#18445=EDGE_CURVE('',#14768,#14774,#11893,.T.);
#18446=EDGE_CURVE('',#14775,#14767,#11894,.T.);
#18447=EDGE_CURVE('',#14775,#14716,#1742,.T.);
#18448=EDGE_CURVE('',#14775,#14713,#8276,.T.);
#18449=EDGE_CURVE('',#14776,#14718,#8277,.T.);
#18450=EDGE_CURVE('',#14777,#14776,#1743,.T.);
#18451=EDGE_CURVE('',#14777,#14721,#8278,.T.);
#18452=EDGE_CURVE('',#14778,#14776,#11895,.T.);
#18453=EDGE_CURVE('',#14778,#14717,#8279,.T.);
#18454=EDGE_CURVE('',#14779,#14728,#8280,.T.);
#18455=EDGE_CURVE('',#14778,#14779,#1744,.T.);
#18456=EDGE_CURVE('',#14780,#14722,#8281,.T.);
#18457=EDGE_CURVE('',#14780,#14777,#1745,.T.);
#18458=EDGE_CURVE('',#14781,#14723,#8282,.T.);
#18459=EDGE_CURVE('',#14781,#14780,#1746,.T.);
#18460=EDGE_CURVE('',#14781,#14782,#1747,.T.);
#18461=EDGE_CURVE('',#14782,#14724,#8283,.T.);
#18462=EDGE_CURVE('',#14783,#14782,#1748,.T.);
#18463=EDGE_CURVE('',#14783,#14725,#8284,.T.);
#18464=EDGE_CURVE('',#14783,#14784,#11896,.T.);
#18465=EDGE_CURVE('',#14784,#14726,#8285,.T.);
#18466=EDGE_CURVE('',#14785,#14784,#8286,.T.);
#18467=EDGE_CURVE('',#14785,#14727,#8287,.T.);
#18468=EDGE_CURVE('',#14785,#14779,#11897,.T.);
#18469=EDGE_CURVE('',#14786,#14787,#1749,.T.);
#18470=EDGE_CURVE('',#14787,#14737,#8288,.T.);
#18471=EDGE_CURVE('',#14786,#14732,#8289,.T.);
#18472=EDGE_CURVE('',#14788,#14789,#1750,.T.);
#18473=EDGE_CURVE('',#14789,#14729,#8290,.T.);
#18474=EDGE_CURVE('',#14788,#14734,#8291,.T.);
#18475=EDGE_CURVE('',#14790,#14789,#11898,.T.);
#18476=EDGE_CURVE('',#14790,#14730,#8292,.T.);
#18477=EDGE_CURVE('',#14790,#14791,#8293,.T.);
#18478=EDGE_CURVE('',#14791,#14731,#8294,.T.);
#18479=EDGE_CURVE('',#14786,#14791,#11899,.T.);
#18480=EDGE_CURVE('',#14788,#14792,#11900,.T.);
#18481=EDGE_CURVE('',#14792,#14733,#8295,.T.);
#18482=EDGE_CURVE('',#14793,#14792,#1751,.T.);
#18483=EDGE_CURVE('',#14793,#14740,#8296,.T.);
#18484=EDGE_CURVE('',#14794,#14787,#1752,.T.);
#18485=EDGE_CURVE('',#14794,#14738,#8297,.T.);
#18486=EDGE_CURVE('',#14794,#14795,#1753,.T.);
#18487=EDGE_CURVE('',#14795,#14739,#8298,.T.);
#18488=EDGE_CURVE('',#14795,#14793,#1754,.T.);
#18489=EDGE_CURVE('',#14741,#14796,#8299,.T.);
#18490=EDGE_CURVE('',#14796,#14797,#1755,.T.);
#18491=EDGE_CURVE('',#14742,#14797,#8300,.T.);
#18492=EDGE_CURVE('',#14797,#14798,#1756,.T.);
#18493=EDGE_CURVE('',#14743,#14798,#8301,.T.);
#18494=EDGE_CURVE('',#14798,#14799,#11901,.T.);
#18495=EDGE_CURVE('',#14799,#14744,#8302,.T.);
#18496=EDGE_CURVE('',#14800,#14745,#8303,.T.);
#18497=EDGE_CURVE('',#14799,#14800,#11902,.T.);
#18498=EDGE_CURVE('',#14800,#14801,#8304,.T.);
#18499=EDGE_CURVE('',#14746,#14801,#8305,.T.);
#18500=EDGE_CURVE('',#14802,#14747,#8306,.T.);
#18501=EDGE_CURVE('',#14802,#14801,#11903,.T.);
#18502=EDGE_CURVE('',#14803,#14802,#11904,.T.);
#18503=EDGE_CURVE('',#14803,#14748,#8307,.T.);
#18504=EDGE_CURVE('',#14803,#14804,#1757,.T.);
#18505=EDGE_CURVE('',#14749,#14804,#8308,.T.);
#18506=EDGE_CURVE('',#14796,#14804,#1758,.T.);
#18507=EDGE_CURVE('',#14751,#14769,#8309,.T.);
#18508=EDGE_CURVE('',#14750,#14770,#8310,.T.);
#18509=EDGE_CURVE('',#14752,#14768,#8311,.T.);
#18510=EDGE_CURVE('',#14753,#14774,#8312,.T.);
#18511=EDGE_CURVE('',#14754,#14773,#8313,.T.);
#18512=EDGE_CURVE('',#14755,#14772,#8314,.T.);
#18513=EDGE_CURVE('',#14756,#14771,#8315,.T.);
#18514=EDGE_CURVE('',#14805,#14806,#11905,.T.);
#18515=EDGE_CURVE('',#14758,#14805,#8316,.T.);
#18516=EDGE_CURVE('',#14757,#14806,#8317,.T.);
#18517=EDGE_CURVE('',#14805,#14807,#11906,.T.);
#18518=EDGE_CURVE('',#14759,#14807,#8318,.T.);
#18519=EDGE_CURVE('',#14808,#14807,#8319,.T.);
#18520=EDGE_CURVE('',#14760,#14808,#8320,.T.);
#18521=EDGE_CURVE('',#14808,#14809,#11907,.T.);
#18522=EDGE_CURVE('',#14761,#14809,#8321,.T.);
#18523=EDGE_CURVE('',#14810,#14809,#11908,.T.);
#18524=EDGE_CURVE('',#14762,#14810,#8322,.T.);
#18525=EDGE_CURVE('',#14811,#14810,#1759,.T.);
#18526=EDGE_CURVE('',#14763,#14811,#8323,.T.);
#18527=EDGE_CURVE('',#14812,#14811,#1760,.T.);
#18528=EDGE_CURVE('',#14764,#14812,#8324,.T.);
#18529=EDGE_CURVE('',#14812,#14813,#1761,.T.);
#18530=EDGE_CURVE('',#14765,#14813,#8325,.T.);
#18531=EDGE_CURVE('',#14806,#14813,#1762,.T.);
#18532=EDGE_CURVE('',#14649,#14542,#8326,.T.);
#18533=EDGE_CURVE('',#14628,#14537,#8327,.T.);
#18534=EDGE_CURVE('',#14584,#14639,#8328,.T.);
#18535=EDGE_CURVE('',#14581,#14638,#8329,.T.);
#18536=EDGE_CURVE('',#14814,#14556,#8330,.T.);
#18537=EDGE_CURVE('',#14814,#14815,#8331,.T.);
#18538=EDGE_CURVE('',#14816,#14815,#8332,.T.);
#18539=EDGE_CURVE('',#14816,#14634,#8333,.T.);
#18540=EDGE_CURVE('',#14817,#14633,#8334,.T.);
#18541=EDGE_CURVE('',#14817,#14818,#8335,.T.);
#18542=EDGE_CURVE('',#14818,#14819,#8336,.T.);
#18543=EDGE_CURVE('',#14820,#14819,#8337,.T.);
#18544=EDGE_CURVE('',#14577,#14820,#8338,.T.);
#18545=EDGE_CURVE('',#14580,#14821,#8339,.T.);
#18546=EDGE_CURVE('',#14821,#14822,#8340,.T.);
#18547=EDGE_CURVE('',#14822,#14823,#8341,.T.);
#18548=EDGE_CURVE('',#14824,#14823,#8342,.T.);
#18549=EDGE_CURVE('',#14824,#14637,#8343,.T.);
#18550=EDGE_CURVE('',#14825,#14635,#8344,.T.);
#18551=EDGE_CURVE('',#14825,#14826,#8345,.T.);
#18552=EDGE_CURVE('',#14826,#14827,#8346,.T.);
#18553=EDGE_CURVE('',#14827,#14559,#8347,.T.);
#18554=EDGE_CURVE('',#14828,#14597,#8348,.T.);
#18555=EDGE_CURVE('',#14829,#14828,#8349,.T.);
#18556=EDGE_CURVE('',#14830,#14829,#8350,.T.);
#18557=EDGE_CURVE('',#14830,#14643,#8351,.T.);
#18558=EDGE_CURVE('',#14831,#14641,#8352,.T.);
#18559=EDGE_CURVE('',#14831,#14832,#8353,.T.);
#18560=EDGE_CURVE('',#14833,#14832,#8354,.T.);
#18561=EDGE_CURVE('',#14834,#14833,#8355,.T.);
#18562=EDGE_CURVE('',#14583,#14834,#8356,.T.);
#18563=EDGE_CURVE('',#14591,#14835,#8357,.T.);
#18564=EDGE_CURVE('',#14835,#14836,#8358,.T.);
#18565=EDGE_CURVE('',#14837,#14836,#8359,.T.);
#18566=EDGE_CURVE('',#14838,#14837,#8360,.T.);
#18567=EDGE_CURVE('',#14838,#14644,#8361,.T.);
#18568=EDGE_CURVE('',#14839,#14642,#8362,.T.);
#18569=EDGE_CURVE('',#14839,#14840,#8363,.T.);
#18570=EDGE_CURVE('',#14841,#14840,#8364,.T.);
#18571=EDGE_CURVE('',#14841,#14595,#8365,.T.);
#18572=EDGE_CURVE('',#14835,#14386,#11909,.T.);
#18573=EDGE_CURVE('',#14548,#14842,#8366,.T.);
#18574=EDGE_CURVE('',#14391,#14842,#11910,.T.);
#18575=EDGE_CURVE('',#14843,#14830,#11911,.T.);
#18576=EDGE_CURVE('',#14843,#14844,#8367,.T.);
#18577=EDGE_CURVE('',#14831,#14844,#11912,.T.);
#18578=EDGE_CURVE('',#14383,#14834,#11913,.T.);
#18579=EDGE_CURVE('',#14821,#14363,#11914,.T.);
#18580=EDGE_CURVE('',#14845,#14824,#11915,.T.);
#18581=EDGE_CURVE('',#14846,#14845,#8368,.T.);
#18582=EDGE_CURVE('',#14825,#14846,#11916,.T.);
#18583=EDGE_CURVE('',#14847,#14816,#11917,.T.);
#18584=EDGE_CURVE('',#14848,#14847,#8369,.T.);
#18585=EDGE_CURVE('',#14817,#14848,#11918,.T.);
#18586=EDGE_CURVE('',#14536,#14849,#8370,.T.);
#18587=EDGE_CURVE('',#14352,#14849,#11919,.T.);
#18588=EDGE_CURVE('',#14850,#14394,#11920,.T.);
#18589=EDGE_CURVE('',#14540,#14850,#8371,.T.);
#18590=EDGE_CURVE('',#14851,#14838,#11921,.T.);
#18591=EDGE_CURVE('',#14851,#14852,#8372,.T.);
#18592=EDGE_CURVE('',#14839,#14852,#11922,.T.);
#18593=EDGE_CURVE('',#14360,#14820,#11923,.T.);
#18594=EDGE_CURVE('',#14853,#14355,#11924,.T.);
#18595=EDGE_CURVE('',#14530,#14853,#8373,.T.);
#18596=EDGE_CURVE('',#14854,#14837,#11925,.T.);
#18597=EDGE_CURVE('',#14855,#14836,#11926,.T.);
#18598=EDGE_CURVE('',#14854,#14855,#8374,.T.);
#18599=EDGE_CURVE('',#14836,#14385,#11927,.T.);
#18600=EDGE_CURVE('',#14855,#14385,#11928,.T.);
#18601=EDGE_CURVE('',#14856,#14837,#11929,.T.);
#18602=EDGE_CURVE('',#14851,#14856,#8375,.T.);
#18603=EDGE_CURVE('',#14854,#14856,#11930,.T.);
#18604=EDGE_CURVE('',#14857,#14384,#11931,.T.);
#18605=EDGE_CURVE('',#14855,#14857,#11932,.T.);
#18606=EDGE_CURVE('',#14384,#14833,#11933,.T.);
#18607=EDGE_CURVE('',#14857,#14833,#11934,.T.);
#18608=EDGE_CURVE('',#14857,#14858,#8376,.T.);
#18609=EDGE_CURVE('',#14858,#14859,#8377,.T.);
#18610=EDGE_CURVE('',#14859,#14860,#8378,.T.);
#18611=EDGE_CURVE('',#14860,#14861,#11935,.T.);
#18612=EDGE_CURVE('',#14861,#14862,#11936,.T.);
#18613=EDGE_CURVE('',#14862,#14863,#11937,.T.);
#18614=EDGE_CURVE('',#14863,#14864,#8379,.T.);
#18615=EDGE_CURVE('',#14864,#14854,#8380,.T.);
#18616=EDGE_CURVE('',#14864,#14865,#11938,.T.);
#18617=EDGE_CURVE('',#14865,#14856,#8381,.T.);
#18618=EDGE_CURVE('',#14864,#14840,#11939,.T.);
#18619=EDGE_CURVE('',#14840,#14865,#11940,.T.);
#18620=EDGE_CURVE('',#14858,#14832,#11941,.T.);
#18621=EDGE_CURVE('',#14832,#14866,#11942,.T.);
#18622=EDGE_CURVE('',#14858,#14866,#11943,.T.);
#18623=EDGE_CURVE('',#14866,#14867,#8382,.T.);
#18624=EDGE_CURVE('',#14859,#14867,#11944,.T.);
#18625=EDGE_CURVE('',#14867,#14829,#11945,.T.);
#18626=EDGE_CURVE('',#14859,#14829,#11946,.T.);
#18627=EDGE_CURVE('',#14860,#14828,#11947,.T.);
#18628=EDGE_CURVE('',#14828,#14589,#11948,.T.);
#18629=EDGE_CURVE('',#14861,#14589,#11949,.T.);
#18630=EDGE_CURVE('',#14862,#14588,#11950,.T.);
#18631=EDGE_CURVE('',#14588,#14841,#11951,.T.);
#18632=EDGE_CURVE('',#14863,#14841,#11952,.T.);
#18633=EDGE_CURVE('',#14852,#14865,#8383,.T.);
#18634=EDGE_CURVE('',#14844,#14866,#8384,.T.);
#18635=EDGE_CURVE('',#14843,#14867,#8385,.T.);
#18636=EDGE_CURVE('',#14850,#14868,#8386,.T.);
#18637=EDGE_CURVE('',#14869,#14868,#8387,.T.);
#18638=EDGE_CURVE('',#14610,#14869,#8388,.T.);
#18639=EDGE_CURVE('',#14870,#14869,#11953,.T.);
#18640=EDGE_CURVE('',#14871,#14868,#11954,.T.);
#18641=EDGE_CURVE('',#14870,#14871,#8389,.T.);
#18642=EDGE_CURVE('',#14868,#14393,#11955,.T.);
#18643=EDGE_CURVE('',#14871,#14393,#11956,.T.);
#18644=EDGE_CURVE('',#14611,#14872,#8390,.T.);
#18645=EDGE_CURVE('',#14872,#14869,#11957,.T.);
#18646=EDGE_CURVE('',#14870,#14872,#11958,.T.);
#18647=EDGE_CURVE('',#14873,#14392,#11959,.T.);
#18648=EDGE_CURVE('',#14871,#14873,#11960,.T.);
#18649=EDGE_CURVE('',#14842,#14874,#8391,.T.);
#18650=EDGE_CURVE('',#14392,#14874,#11961,.T.);
#18651=EDGE_CURVE('',#14873,#14874,#11962,.T.);
#18652=EDGE_CURVE('',#14873,#14875,#8392,.T.);
#18653=EDGE_CURVE('',#14875,#14876,#8393,.T.);
#18654=EDGE_CURVE('',#14876,#14877,#8394,.T.);
#18655=EDGE_CURVE('',#14877,#14878,#11963,.T.);
#18656=EDGE_CURVE('',#14878,#14879,#11964,.T.);
#18657=EDGE_CURVE('',#14879,#14880,#11965,.T.);
#18658=EDGE_CURVE('',#14880,#14881,#8395,.T.);
#18659=EDGE_CURVE('',#14881,#14870,#8396,.T.);
#18660=EDGE_CURVE('',#14881,#14882,#11966,.T.);
#18661=EDGE_CURVE('',#14882,#14872,#8397,.T.);
#18662=EDGE_CURVE('',#14881,#14883,#11967,.T.);
#18663=EDGE_CURVE('',#14883,#14882,#11968,.T.);
#18664=EDGE_CURVE('',#14874,#14884,#8398,.T.);
#18665=EDGE_CURVE('',#14875,#14884,#11969,.T.);
#18666=EDGE_CURVE('',#14884,#14885,#11970,.T.);
#18667=EDGE_CURVE('',#14875,#14885,#11971,.T.);
#18668=EDGE_CURVE('',#14885,#14886,#8399,.T.);
#18669=EDGE_CURVE('',#14876,#14886,#11972,.T.);
#18670=EDGE_CURVE('',#14886,#14887,#11973,.T.);
#18671=EDGE_CURVE('',#14876,#14887,#11974,.T.);
#18672=EDGE_CURVE('',#14887,#14888,#8400,.T.);
#18673=EDGE_CURVE('',#14877,#14888,#11975,.T.);
#18674=EDGE_CURVE('',#14888,#14546,#11976,.T.);
#18675=EDGE_CURVE('',#14878,#14546,#11977,.T.);
#18676=EDGE_CURVE('',#14879,#14545,#11978,.T.);
#18677=EDGE_CURVE('',#14545,#14889,#11979,.T.);
#18678=EDGE_CURVE('',#14880,#14889,#11980,.T.);
#18679=EDGE_CURVE('',#14889,#14883,#8401,.T.);
#18680=EDGE_CURVE('',#14612,#14882,#8402,.T.);
#18681=EDGE_CURVE('',#14613,#14883,#8403,.T.);
#18682=EDGE_CURVE('',#14603,#14884,#8404,.T.);
#18683=EDGE_CURVE('',#14602,#14885,#8405,.T.);
#18684=EDGE_CURVE('',#14601,#14886,#8406,.T.);
#18685=EDGE_CURVE('',#14600,#14887,#8407,.T.);
#18686=EDGE_CURVE('',#14888,#14599,#8408,.T.);
#18687=EDGE_CURVE('',#14889,#14614,#8409,.T.);
#18688=EDGE_CURVE('',#14818,#14890,#11981,.T.);
#18689=EDGE_CURVE('',#14890,#14891,#8410,.T.);
#18690=EDGE_CURVE('',#14819,#14891,#11982,.T.);
#18691=EDGE_CURVE('',#14819,#14361,#11983,.T.);
#18692=EDGE_CURVE('',#14361,#14891,#11984,.T.);
#18693=EDGE_CURVE('',#14848,#14892,#8411,.T.);
#18694=EDGE_CURVE('',#14892,#14818,#11985,.T.);
#18695=EDGE_CURVE('',#14892,#14890,#11986,.T.);
#18696=EDGE_CURVE('',#14891,#14893,#11987,.T.);
#18697=EDGE_CURVE('',#14362,#14893,#11988,.T.);
#18698=EDGE_CURVE('',#14362,#14822,#11989,.T.);
#18699=EDGE_CURVE('',#14822,#14893,#11990,.T.);
#18700=EDGE_CURVE('',#14894,#14890,#8412,.T.);
#18701=EDGE_CURVE('',#14895,#14894,#8413,.T.);
#18702=EDGE_CURVE('',#14896,#14895,#11991,.T.);
#18703=EDGE_CURVE('',#14897,#14896,#11992,.T.);
#18704=EDGE_CURVE('',#14898,#14897,#11993,.T.);
#18705=EDGE_CURVE('',#14899,#14898,#8414,.T.);
#18706=EDGE_CURVE('',#14900,#14899,#8415,.T.);
#18707=EDGE_CURVE('',#14893,#14900,#8416,.T.);
#18708=EDGE_CURVE('',#14901,#14894,#11994,.T.);
#18709=EDGE_CURVE('',#14901,#14892,#8417,.T.);
#18710=EDGE_CURVE('',#14815,#14894,#11995,.T.);
#18711=EDGE_CURVE('',#14815,#14901,#11996,.T.);
#18712=EDGE_CURVE('',#14823,#14900,#11997,.T.);
#18713=EDGE_CURVE('',#14902,#14900,#11998,.T.);
#18714=EDGE_CURVE('',#14823,#14902,#11999,.T.);
#18715=EDGE_CURVE('',#14903,#14899,#12000,.T.);
#18716=EDGE_CURVE('',#14902,#14903,#8418,.T.);
#18717=EDGE_CURVE('',#14826,#14899,#12001,.T.);
#18718=EDGE_CURVE('',#14903,#14826,#12002,.T.);
#18719=EDGE_CURVE('',#14827,#14898,#12003,.T.);
#18720=EDGE_CURVE('',#14578,#14897,#12004,.T.);
#18721=EDGE_CURVE('',#14827,#14578,#12005,.T.);
#18722=EDGE_CURVE('',#14579,#14896,#12006,.T.);
#18723=EDGE_CURVE('',#14814,#14895,#12007,.T.);
#18724=EDGE_CURVE('',#14579,#14814,#12008,.T.);
#18725=EDGE_CURVE('',#14847,#14901,#8419,.T.);
#18726=EDGE_CURVE('',#14845,#14902,#8420,.T.);
#18727=EDGE_CURVE('',#14846,#14903,#8421,.T.);
#18728=EDGE_CURVE('',#14571,#14904,#8422,.T.);
#18729=EDGE_CURVE('',#14904,#14905,#8423,.T.);
#18730=EDGE_CURVE('',#14849,#14905,#8424,.T.);
#18731=EDGE_CURVE('',#14904,#14906,#12009,.T.);
#18732=EDGE_CURVE('',#14906,#14907,#8425,.T.);
#18733=EDGE_CURVE('',#14905,#14907,#12010,.T.);
#18734=EDGE_CURVE('',#14570,#14908,#8426,.T.);
#18735=EDGE_CURVE('',#14908,#14904,#12011,.T.);
#18736=EDGE_CURVE('',#14908,#14906,#12012,.T.);
#18737=EDGE_CURVE('',#14905,#14353,#12013,.T.);
#18738=EDGE_CURVE('',#14353,#14907,#12014,.T.);
#18739=EDGE_CURVE('',#14909,#14906,#8427,.T.);
#18740=EDGE_CURVE('',#14910,#14909,#8428,.T.);
#18741=EDGE_CURVE('',#14911,#14910,#12015,.T.);
#18742=EDGE_CURVE('',#14912,#14911,#12016,.T.);
#18743=EDGE_CURVE('',#14913,#14912,#12017,.T.);
#18744=EDGE_CURVE('',#14914,#14913,#8429,.T.);
#18745=EDGE_CURVE('',#14915,#14914,#8430,.T.);
#18746=EDGE_CURVE('',#14916,#14915,#8431,.T.);
#18747=EDGE_CURVE('',#14907,#14916,#12018,.T.);
#18748=EDGE_CURVE('',#14917,#14909,#12019,.T.);
#18749=EDGE_CURVE('',#14917,#14908,#8432,.T.);
#18750=EDGE_CURVE('',#14918,#14909,#12020,.T.);
#18751=EDGE_CURVE('',#14918,#14917,#12021,.T.);
#18752=EDGE_CURVE('',#14354,#14916,#12022,.T.);
#18753=EDGE_CURVE('',#14919,#14916,#12023,.T.);
#18754=EDGE_CURVE('',#14354,#14919,#12024,.T.);
#18755=EDGE_CURVE('',#14920,#14915,#12025,.T.);
#18756=EDGE_CURVE('',#14921,#14914,#12026,.T.);
#18757=EDGE_CURVE('',#14920,#14921,#8433,.T.);
#18758=EDGE_CURVE('',#14922,#14915,#12027,.T.);
#18759=EDGE_CURVE('',#14922,#14920,#12028,.T.);
#18760=EDGE_CURVE('',#14923,#14914,#12029,.T.);
#18761=EDGE_CURVE('',#14921,#14923,#12030,.T.);
#18762=EDGE_CURVE('',#14919,#14922,#8434,.T.);
#18763=EDGE_CURVE('',#14924,#14913,#12031,.T.);
#18764=EDGE_CURVE('',#14923,#14924,#8435,.T.);
#18765=EDGE_CURVE('',#14533,#14912,#12032,.T.);
#18766=EDGE_CURVE('',#14924,#14533,#12033,.T.);
#18767=EDGE_CURVE('',#14534,#14911,#12034,.T.);
#18768=EDGE_CURVE('',#14925,#14910,#12035,.T.);
#18769=EDGE_CURVE('',#14534,#14925,#12036,.T.);
#18770=EDGE_CURVE('',#14925,#14918,#8436,.T.);
#18771=EDGE_CURVE('',#14569,#14917,#8437,.T.);
#18772=EDGE_CURVE('',#14568,#14918,#8438,.T.);
#18773=EDGE_CURVE('',#14853,#14919,#8439,.T.);
#18774=EDGE_CURVE('',#14564,#14921,#8440,.T.);
#18775=EDGE_CURVE('',#14563,#14920,#8441,.T.);
#18776=EDGE_CURVE('',#14562,#14922,#8442,.T.);
#18777=EDGE_CURVE('',#14565,#14923,#8443,.T.);
#18778=EDGE_CURVE('',#14924,#14566,#8444,.T.);
#18779=EDGE_CURVE('',#14925,#14567,#8445,.T.);
#18780=EDGE_CURVE('',#14926,#14927,#1763,.T.);
#18781=EDGE_CURVE('',#14928,#14926,#606,.T.);
#18782=EDGE_CURVE('',#14928,#14929,#12037,.T.);
#18783=EDGE_CURVE('',#14929,#14930,#607,.T.);
#18784=EDGE_CURVE('',#14930,#14931,#1764,.T.);
#18785=EDGE_CURVE('',#14927,#14931,#12038,.T.);
#18786=EDGE_CURVE('',#14932,#14933,#608,.T.);
#18787=EDGE_CURVE('',#14934,#14932,#12039,.T.);
#18788=EDGE_CURVE('',#14934,#14935,#12040,.T.);
#18789=EDGE_CURVE('',#14935,#14936,#12041,.T.);
#18790=EDGE_CURVE('',#14936,#14937,#12042,.T.);
#18791=EDGE_CURVE('',#14933,#14937,#12043,.T.);
#18792=EDGE_CURVE('',#14938,#14939,#12044,.T.);
#18793=EDGE_CURVE('',#14939,#14940,#12045,.T.);
#18794=EDGE_CURVE('',#14941,#14940,#12046,.T.);
#18795=EDGE_CURVE('',#14942,#14941,#12047,.T.);
#18796=EDGE_CURVE('',#14943,#14942,#12048,.T.);
#18797=EDGE_CURVE('',#14943,#14938,#12049,.T.);
#18798=EDGE_CURVE('',#14944,#14945,#12050,.T.);
#18799=EDGE_CURVE('',#14945,#14946,#1765,.T.);
#18800=EDGE_CURVE('',#14947,#14946,#12051,.T.);
#18801=EDGE_CURVE('',#14948,#14947,#12052,.T.);
#18802=EDGE_CURVE('',#14949,#14948,#12053,.T.);
#18803=EDGE_CURVE('',#14949,#14944,#12054,.T.);
#18804=EDGE_CURVE('',#14950,#14951,#609,.T.);
#18805=EDGE_CURVE('',#14951,#14952,#1766,.T.);
#18806=EDGE_CURVE('',#14953,#14952,#12055,.T.);
#18807=EDGE_CURVE('',#14954,#14953,#1767,.T.);
#18808=EDGE_CURVE('',#14955,#14954,#610,.T.);
#18809=EDGE_CURVE('',#14955,#14950,#12056,.T.);
#18810=EDGE_CURVE('',#14956,#14957,#12057,.T.);
#18811=EDGE_CURVE('',#14958,#14957,#1768,.T.);
#18812=EDGE_CURVE('',#14959,#14958,#12058,.T.);
#18813=EDGE_CURVE('',#14960,#14959,#1769,.T.);
#18814=EDGE_CURVE('',#14961,#14960,#1770,.T.);
#18815=EDGE_CURVE('',#14961,#14956,#12059,.T.);
#18816=EDGE_CURVE('',#14962,#14963,#8446,.T.);
#18817=EDGE_CURVE('',#14962,#14963,#12060,.T.);
#18818=EDGE_CURVE('',#14964,#14962,#1771,.T.);
#18819=EDGE_CURVE('',#14964,#14965,#8447,.T.);
#18820=EDGE_CURVE('',#14963,#14965,#1772,.T.);
#18821=EDGE_CURVE('',#14966,#14967,#8448,.T.);
#18822=EDGE_CURVE('',#14965,#14966,#12061,.T.);
#18823=EDGE_CURVE('',#14967,#14964,#12062,.T.);
#18824=EDGE_CURVE('',#14957,#14967,#1773,.T.);
#18825=EDGE_CURVE('',#14956,#14957,#8449,.T.);
#18826=EDGE_CURVE('',#14966,#14956,#1774,.T.);
#18827=EDGE_CURVE('',#14968,#14964,#12063,.T.);
#18828=EDGE_CURVE('',#14968,#14962,#12064,.T.);
#18829=EDGE_CURVE('',#14969,#14967,#12065,.T.);
#18830=EDGE_CURVE('',#14969,#14968,#12066,.T.);
#18831=EDGE_CURVE('',#14958,#14969,#1775,.T.);
#18832=EDGE_CURVE('',#14970,#14971,#1776,.T.);
#18833=EDGE_CURVE('',#14971,#14972,#12067,.T.);
#18834=EDGE_CURVE('',#14972,#14961,#1777,.T.);
#18835=EDGE_CURVE('',#14960,#14973,#12068,.T.);
#18836=EDGE_CURVE('',#14968,#14970,#12069,.T.);
#18837=EDGE_CURVE('',#14974,#14975,#12070,.T.);
#18838=EDGE_CURVE('',#14976,#14974,#1778,.T.);
#18839=EDGE_CURVE('',#14977,#14976,#12071,.T.);
#18840=EDGE_CURVE('',#14950,#14977,#1779,.T.);
#18841=EDGE_CURVE('',#14978,#14955,#1780,.T.);
#18842=EDGE_CURVE('',#14979,#14978,#12072,.T.);
#18843=EDGE_CURVE('',#14980,#14979,#12073,.T.);
#18844=EDGE_CURVE('',#14944,#14980,#1781,.T.);
#18845=EDGE_CURVE('',#14981,#14949,#1782,.T.);
#18846=EDGE_CURVE('',#14982,#14981,#12074,.T.);
#18847=EDGE_CURVE('',#14938,#14982,#1783,.T.);
#18848=EDGE_CURVE('',#14983,#14943,#1784,.T.);
#18849=EDGE_CURVE('',#14984,#14983,#12075,.T.);
#18850=EDGE_CURVE('',#14935,#14984,#1785,.T.);
#18851=EDGE_CURVE('',#14985,#14934,#1786,.T.);
#18852=EDGE_CURVE('',#14986,#14985,#12076,.T.);
#18853=EDGE_CURVE('',#14987,#14986,#12077,.T.);
#18854=EDGE_CURVE('',#14929,#14987,#1787,.T.);
#18855=EDGE_CURVE('',#14988,#14928,#1788,.T.);
#18856=EDGE_CURVE('',#14989,#14988,#12078,.T.);
#18857=EDGE_CURVE('',#14975,#14989,#1789,.T.);
#18858=EDGE_CURVE('',#14971,#14963,#12079,.T.);
#18859=EDGE_CURVE('',#14971,#14965,#12080,.T.);
#18860=EDGE_CURVE('',#14972,#14966,#12081,.T.);
#18861=EDGE_CURVE('',#14990,#14990,#12082,.T.);
#18862=EDGE_CURVE('',#14990,#14991,#8450,.T.);
#18863=EDGE_CURVE('',#14991,#14991,#12083,.T.);
#18864=EDGE_CURVE('',#14992,#14993,#12084,.T.);
#18865=EDGE_CURVE('',#14994,#14993,#8451,.T.);
#18866=EDGE_CURVE('',#14995,#14994,#12085,.T.);
#18867=EDGE_CURVE('',#14996,#14995,#8452,.T.);
#18868=EDGE_CURVE('',#14997,#14996,#12086,.T.);
#18869=EDGE_CURVE('',#14998,#14997,#8453,.T.);
#18870=EDGE_CURVE('',#14999,#14998,#12087,.T.);
#18871=EDGE_CURVE('',#14992,#14999,#8454,.T.);
#18872=EDGE_CURVE('',#14999,#15000,#12088,.T.);
#18873=EDGE_CURVE('',#15001,#15000,#8455,.T.);
#18874=EDGE_CURVE('',#14992,#15001,#611,.T.);
#18875=EDGE_CURVE('',#14998,#15002,#12089,.T.);
#18876=EDGE_CURVE('',#15000,#15002,#12090,.T.);
#18877=EDGE_CURVE('',#14997,#15003,#12091,.T.);
#18878=EDGE_CURVE('',#15002,#15003,#8456,.T.);
#18879=EDGE_CURVE('',#14996,#15004,#12092,.T.);
#18880=EDGE_CURVE('',#15003,#15004,#12093,.T.);
#18881=EDGE_CURVE('',#14995,#15005,#12094,.T.);
#18882=EDGE_CURVE('',#15004,#15005,#8457,.T.);
#18883=EDGE_CURVE('',#14994,#15006,#12095,.T.);
#18884=EDGE_CURVE('',#15005,#15006,#12096,.T.);
#18885=EDGE_CURVE('',#14993,#15007,#12097,.T.);
#18886=EDGE_CURVE('',#15006,#15007,#8458,.T.);
#18887=EDGE_CURVE('',#14993,#15008,#1790,.T.);
#18888=EDGE_CURVE('',#15009,#14992,#1791,.T.);
#18889=EDGE_CURVE('',#15010,#15009,#1792,.T.);
#18890=EDGE_CURVE('',#15011,#15010,#1793,.T.);
#18891=EDGE_CURVE('',#15011,#15012,#12098,.T.);
#18892=EDGE_CURVE('',#15012,#15013,#12099,.T.);
#18893=EDGE_CURVE('',#15008,#15013,#12100,.T.);
#18894=EDGE_CURVE('',#15014,#15015,#8459,.T.);
#18895=EDGE_CURVE('',#15015,#15016,#8460,.T.);
#18896=EDGE_CURVE('',#15016,#15001,#1794,.T.);
#18897=EDGE_CURVE('',#15000,#15014,#8461,.T.);
#18898=EDGE_CURVE('',#15009,#15016,#612,.T.);
#18899=EDGE_CURVE('',#15002,#15017,#8462,.T.);
#18900=EDGE_CURVE('',#15017,#15014,#12101,.T.);
#18901=EDGE_CURVE('',#15018,#15017,#8463,.T.);
#18902=EDGE_CURVE('',#15018,#15003,#8464,.T.);
#18903=EDGE_CURVE('',#15019,#15018,#12102,.T.);
#18904=EDGE_CURVE('',#15019,#15004,#8465,.T.);
#18905=EDGE_CURVE('',#15020,#15019,#8466,.T.);
#18906=EDGE_CURVE('',#15020,#15005,#8467,.T.);
#18907=EDGE_CURVE('',#15021,#15020,#12103,.T.);
#18908=EDGE_CURVE('',#15021,#15006,#8468,.T.);
#18909=EDGE_CURVE('',#15008,#15022,#613,.T.);
#18910=EDGE_CURVE('',#15007,#15022,#1795,.T.);
#18911=EDGE_CURVE('',#15022,#15023,#1796,.T.);
#18912=EDGE_CURVE('',#15023,#15024,#8469,.T.);
#18913=EDGE_CURVE('',#15024,#15025,#8470,.T.);
#18914=EDGE_CURVE('',#15026,#15025,#8471,.T.);
#18915=EDGE_CURVE('',#15026,#15021,#8472,.T.);
#18916=EDGE_CURVE('',#15010,#15027,#614,.T.);
#18917=EDGE_CURVE('',#15028,#15027,#1797,.T.);
#18918=EDGE_CURVE('',#15011,#15028,#615,.T.);
#18919=EDGE_CURVE('',#15027,#15016,#1798,.T.);
#18920=EDGE_CURVE('',#15029,#15012,#12104,.T.);
#18921=EDGE_CURVE('',#15029,#15011,#1799,.T.);
#18922=EDGE_CURVE('',#15030,#15031,#12105,.T.);
#18923=EDGE_CURVE('',#15031,#15013,#8473,.T.);
#18924=EDGE_CURVE('',#15030,#15012,#8474,.T.);
#18925=EDGE_CURVE('',#15013,#15032,#12106,.T.);
#18926=EDGE_CURVE('',#15008,#15032,#1800,.T.);
#18927=EDGE_CURVE('',#15014,#15033,#12107,.T.);
#18928=EDGE_CURVE('',#15033,#15034,#8475,.T.);
#18929=EDGE_CURVE('',#15015,#15034,#12108,.T.);
#18930=EDGE_CURVE('',#15015,#15035,#12109,.T.);
#18931=EDGE_CURVE('',#15035,#15027,#8476,.T.);
#18932=EDGE_CURVE('',#15017,#15036,#12110,.T.);
#18933=EDGE_CURVE('',#15036,#15033,#12111,.T.);
#18934=EDGE_CURVE('',#15018,#15037,#12112,.T.);
#18935=EDGE_CURVE('',#15037,#15036,#8477,.T.);
#18936=EDGE_CURVE('',#15019,#15038,#12113,.T.);
#18937=EDGE_CURVE('',#15038,#15037,#12114,.T.);
#18938=EDGE_CURVE('',#15020,#15039,#12115,.T.);
#18939=EDGE_CURVE('',#15039,#15038,#8478,.T.);
#18940=EDGE_CURVE('',#15021,#15040,#12116,.T.);
#18941=EDGE_CURVE('',#15040,#15039,#12117,.T.);
#18942=EDGE_CURVE('',#15032,#15023,#12118,.T.);
#18943=EDGE_CURVE('',#15041,#15024,#12119,.T.);
#18944=EDGE_CURVE('',#15032,#15041,#8479,.T.);
#18945=EDGE_CURVE('',#15042,#15043,#8480,.T.);
#18946=EDGE_CURVE('',#15043,#15025,#12120,.T.);
#18947=EDGE_CURVE('',#15042,#15024,#12121,.T.);
#18948=EDGE_CURVE('',#15044,#15026,#12122,.T.);
#18949=EDGE_CURVE('',#15025,#15045,#12123,.T.);
#18950=EDGE_CURVE('',#15044,#15045,#8481,.T.);
#18951=EDGE_CURVE('',#15026,#15046,#12124,.T.);
#18952=EDGE_CURVE('',#15046,#15040,#8482,.T.);
#18953=EDGE_CURVE('',#15035,#15047,#8483,.T.);
#18954=EDGE_CURVE('',#15047,#15048,#8484,.T.);
#18955=EDGE_CURVE('',#15048,#15049,#8485,.T.);
#18956=EDGE_CURVE('',#15049,#15050,#8486,.T.);
#18957=EDGE_CURVE('',#15050,#15028,#1801,.T.);
#18958=EDGE_CURVE('',#15029,#15050,#12125,.T.);
#18959=EDGE_CURVE('',#15051,#15029,#8487,.T.);
#18960=EDGE_CURVE('',#15051,#15030,#12126,.T.);
#18961=EDGE_CURVE('',#15052,#15053,#12127,.T.);
#18962=EDGE_CURVE('',#15053,#15031,#12128,.T.);
#18963=EDGE_CURVE('',#15052,#15030,#12129,.T.);
#18964=EDGE_CURVE('',#15031,#15041,#12130,.T.);
#18965=EDGE_CURVE('',#15034,#15054,#12131,.T.);
#18966=EDGE_CURVE('',#15035,#15054,#12132,.T.);
#18967=EDGE_CURVE('',#15055,#15056,#8488,.T.);
#18968=EDGE_CURVE('',#15057,#15055,#12133,.T.);
#18969=EDGE_CURVE('',#15058,#15057,#8489,.T.);
#18970=EDGE_CURVE('',#15059,#15058,#8490,.T.);
#18971=EDGE_CURVE('',#15060,#15059,#8491,.T.);
#18972=EDGE_CURVE('',#15061,#15060,#12134,.T.);
#18973=EDGE_CURVE('',#15062,#15061,#8492,.T.);
#18974=EDGE_CURVE('',#15063,#15062,#8493,.T.);
#18975=EDGE_CURVE('',#15064,#15063,#8494,.T.);
#18976=EDGE_CURVE('',#15065,#15064,#12135,.T.);
#18977=EDGE_CURVE('',#15066,#15065,#8495,.T.);
#18978=EDGE_CURVE('',#15067,#15066,#12136,.T.);
#18979=EDGE_CURVE('',#15068,#15067,#8496,.T.);
#18980=EDGE_CURVE('',#15069,#15068,#12137,.T.);
#18981=EDGE_CURVE('',#15070,#15069,#8497,.T.);
#18982=EDGE_CURVE('',#15071,#15070,#12138,.T.);
#18983=EDGE_CURVE('',#15072,#15071,#8498,.T.);
#18984=EDGE_CURVE('',#15073,#15072,#12139,.T.);
#18985=EDGE_CURVE('',#15074,#15073,#12140,.T.);
#18986=EDGE_CURVE('',#15075,#15074,#8499,.T.);
#18987=EDGE_CURVE('',#15076,#15075,#12141,.T.);
#18988=EDGE_CURVE('',#15077,#15076,#8500,.T.);
#18989=EDGE_CURVE('',#15078,#15077,#12142,.T.);
#18990=EDGE_CURVE('',#15054,#15078,#8501,.T.);
#18991=EDGE_CURVE('',#15079,#15046,#12143,.T.);
#18992=EDGE_CURVE('',#15080,#15079,#8502,.T.);
#18993=EDGE_CURVE('',#15081,#15080,#12144,.T.);
#18994=EDGE_CURVE('',#15082,#15081,#8503,.T.);
#18995=EDGE_CURVE('',#15083,#15082,#12145,.T.);
#18996=EDGE_CURVE('',#15084,#15083,#12146,.T.);
#18997=EDGE_CURVE('',#15085,#15084,#8504,.T.);
#18998=EDGE_CURVE('',#15086,#15085,#12147,.T.);
#18999=EDGE_CURVE('',#15056,#15086,#8505,.T.);
#19000=EDGE_CURVE('',#15042,#15041,#12148,.T.);
#19001=EDGE_CURVE('',#14978,#15087,#12149,.T.);
#19002=EDGE_CURVE('',#15088,#15087,#12150,.T.);
#19003=EDGE_CURVE('',#14979,#15088,#12151,.T.);
#19004=EDGE_CURVE('',#15089,#15087,#12152,.T.);
#19005=EDGE_CURVE('',#15090,#15089,#8506,.T.);
#19006=EDGE_CURVE('',#15043,#15090,#12153,.T.);
#19007=EDGE_CURVE('',#15053,#15042,#12154,.T.);
#19008=EDGE_CURVE('',#15091,#15052,#12155,.T.);
#19009=EDGE_CURVE('',#15092,#15091,#8507,.T.);
#19010=EDGE_CURVE('',#15093,#15092,#12156,.T.);
#19011=EDGE_CURVE('',#15088,#15093,#8508,.T.);
#19012=EDGE_CURVE('',#15094,#15094,#12157,.T.);
#19013=EDGE_CURVE('',#15090,#15045,#12158,.T.);
#19014=EDGE_CURVE('',#15045,#15095,#8509,.T.);
#19015=EDGE_CURVE('',#15096,#15095,#8510,.T.);
#19016=EDGE_CURVE('',#15096,#15044,#8511,.T.);
#19017=EDGE_CURVE('',#15044,#15079,#12159,.T.);
#19018=EDGE_CURVE('',#15091,#15049,#12160,.T.);
#19019=EDGE_CURVE('',#15092,#15048,#12161,.T.);
#19020=EDGE_CURVE('',#15049,#15051,#12162,.T.);
#19021=EDGE_CURVE('',#15047,#15097,#12163,.T.);
#19022=EDGE_CURVE('',#15097,#15098,#8512,.T.);
#19023=EDGE_CURVE('',#15098,#15048,#12164,.T.);
#19024=EDGE_CURVE('',#15047,#15078,#12165,.T.);
#19025=EDGE_CURVE('',#15091,#15051,#12166,.T.);
#19026=EDGE_CURVE('',#15099,#15086,#12167,.T.);
#19027=EDGE_CURVE('',#15100,#15099,#8513,.T.);
#19028=EDGE_CURVE('',#15056,#15100,#616,.T.);
#19029=EDGE_CURVE('',#15101,#15085,#12168,.T.);
#19030=EDGE_CURVE('',#15099,#15101,#12169,.T.);
#19031=EDGE_CURVE('',#15102,#15084,#12170,.T.);
#19032=EDGE_CURVE('',#15101,#15102,#8514,.T.);
#19033=EDGE_CURVE('',#15103,#15083,#12171,.T.);
#19034=EDGE_CURVE('',#15102,#15103,#12172,.T.);
#19035=EDGE_CURVE('',#15104,#15082,#12173,.T.);
#19036=EDGE_CURVE('',#15103,#15104,#12174,.T.);
#19037=EDGE_CURVE('',#15105,#15082,#12175,.T.);
#19038=EDGE_CURVE('',#15106,#15081,#12176,.T.);
#19039=EDGE_CURVE('',#15105,#15106,#8515,.T.);
#19040=EDGE_CURVE('',#15096,#15080,#12177,.T.);
#19041=EDGE_CURVE('',#15106,#15096,#12178,.T.);
#19042=EDGE_CURVE('',#15097,#15077,#12179,.T.);
#19043=EDGE_CURVE('',#15107,#15076,#12180,.T.);
#19044=EDGE_CURVE('',#15097,#15107,#8516,.T.);
#19045=EDGE_CURVE('',#15108,#15075,#12181,.T.);
#19046=EDGE_CURVE('',#15107,#15108,#12182,.T.);
#19047=EDGE_CURVE('',#15109,#15074,#12183,.T.);
#19048=EDGE_CURVE('',#15108,#15109,#8517,.T.);
#19049=EDGE_CURVE('',#15110,#15074,#12184,.T.);
#19050=EDGE_CURVE('',#15111,#15073,#12185,.T.);
#19051=EDGE_CURVE('',#15110,#15111,#12186,.T.);
#19052=EDGE_CURVE('',#15112,#15072,#12187,.T.);
#19053=EDGE_CURVE('',#15111,#15112,#12188,.T.);
#19054=EDGE_CURVE('',#15113,#15071,#12189,.T.);
#19055=EDGE_CURVE('',#15112,#15113,#8518,.T.);
#19056=EDGE_CURVE('',#15114,#15070,#12190,.T.);
#19057=EDGE_CURVE('',#15113,#15114,#12191,.T.);
#19058=EDGE_CURVE('',#15115,#15069,#12192,.T.);
#19059=EDGE_CURVE('',#15114,#15115,#8519,.T.);
#19060=EDGE_CURVE('',#15116,#15068,#12193,.T.);
#19061=EDGE_CURVE('',#15115,#15116,#12194,.T.);
#19062=EDGE_CURVE('',#15117,#15067,#12195,.T.);
#19063=EDGE_CURVE('',#15116,#15117,#8520,.T.);
#19064=EDGE_CURVE('',#15118,#15066,#12196,.T.);
#19065=EDGE_CURVE('',#15117,#15118,#12197,.T.);
#19066=EDGE_CURVE('',#15119,#15065,#12198,.T.);
#19067=EDGE_CURVE('',#15118,#15119,#8521,.T.);
#19068=EDGE_CURVE('',#15120,#15064,#12199,.T.);
#19069=EDGE_CURVE('',#15119,#15120,#12200,.T.);
#19070=EDGE_CURVE('',#15121,#15063,#12201,.T.);
#19071=EDGE_CURVE('',#15120,#15121,#8522,.T.);
#19072=EDGE_CURVE('',#15122,#15063,#12202,.T.);
#19073=EDGE_CURVE('',#15123,#15062,#12203,.T.);
#19074=EDGE_CURVE('',#15122,#15123,#8523,.T.);
#19075=EDGE_CURVE('',#15124,#15062,#12204,.T.);
#19076=EDGE_CURVE('',#15125,#15061,#12205,.T.);
#19077=EDGE_CURVE('',#15124,#15125,#8524,.T.);
#19078=EDGE_CURVE('',#15126,#15060,#12206,.T.);
#19079=EDGE_CURVE('',#15125,#15126,#12207,.T.);
#19080=EDGE_CURVE('',#15127,#15059,#12208,.T.);
#19081=EDGE_CURVE('',#15126,#15127,#8525,.T.);
#19082=EDGE_CURVE('',#15128,#15059,#12209,.T.);
#19083=EDGE_CURVE('',#15129,#15058,#12210,.T.);
#19084=EDGE_CURVE('',#15128,#15129,#8526,.T.);
#19085=EDGE_CURVE('',#15130,#15058,#12211,.T.);
#19086=EDGE_CURVE('',#15131,#15057,#12212,.T.);
#19087=EDGE_CURVE('',#15130,#15131,#8527,.T.);
#19088=EDGE_CURVE('',#15132,#15055,#12213,.T.);
#19089=EDGE_CURVE('',#15131,#15132,#12214,.T.);
#19090=EDGE_CURVE('',#15132,#15100,#8528,.T.);
#19091=EDGE_CURVE('',#15133,#15134,#12215,.T.);
#19092=EDGE_CURVE('',#15134,#15133,#12216,.T.);
#19093=EDGE_CURVE('',#15133,#15094,#12217,.T.);
#19094=EDGE_CURVE('',#15093,#15098,#12218,.T.);
#19095=EDGE_CURVE('',#14981,#15135,#12219,.T.);
#19096=EDGE_CURVE('',#15136,#15135,#12220,.T.);
#19097=EDGE_CURVE('',#14982,#15136,#12221,.T.);
#19098=EDGE_CURVE('',#15110,#15135,#8529,.T.);
#19099=EDGE_CURVE('',#15111,#15136,#8530,.T.);
#19100=EDGE_CURVE('',#14983,#15137,#12222,.T.);
#19101=EDGE_CURVE('',#15138,#15137,#12223,.T.);
#19102=EDGE_CURVE('',#14984,#15138,#12224,.T.);
#19103=EDGE_CURVE('',#15137,#15139,#8531,.T.);
#19104=EDGE_CURVE('',#15140,#15139,#12225,.T.);
#19105=EDGE_CURVE('',#15140,#15138,#8532,.T.);
#19106=EDGE_CURVE('',#14976,#15141,#12226,.T.);
#19107=EDGE_CURVE('',#15142,#15141,#12227,.T.);
#19108=EDGE_CURVE('',#14977,#15142,#1802,.T.);
#19109=EDGE_CURVE('',#15103,#15141,#8533,.T.);
#19110=EDGE_CURVE('',#15104,#15142,#8534,.T.);
#19111=EDGE_CURVE('',#14988,#15143,#1803,.T.);
#19112=EDGE_CURVE('',#15144,#15143,#12228,.T.);
#19113=EDGE_CURVE('',#14989,#15144,#12229,.T.);
#19114=EDGE_CURVE('',#15145,#15143,#8535,.T.);
#19115=EDGE_CURVE('',#15146,#15145,#12230,.T.);
#19116=EDGE_CURVE('',#15144,#15146,#8536,.T.);
#19117=EDGE_CURVE('',#15147,#15088,#12231,.T.);
#19118=EDGE_CURVE('',#14979,#15147,#12232,.T.);
#19119=EDGE_CURVE('',#15147,#15098,#8537,.T.);
#19120=EDGE_CURVE('',#14978,#15148,#1804,.T.);
#19121=EDGE_CURVE('',#15087,#15148,#12233,.T.);
#19122=EDGE_CURVE('',#15095,#15148,#12234,.T.);
#19123=EDGE_CURVE('',#15089,#15095,#12235,.T.);
#19124=EDGE_CURVE('',#15148,#14953,#1805,.T.);
#19125=EDGE_CURVE('',#15106,#14953,#8538,.T.);
#19126=EDGE_CURVE('',#15149,#15147,#12236,.T.);
#19127=EDGE_CURVE('',#14980,#15149,#12237,.T.);
#19128=EDGE_CURVE('',#15107,#15149,#8539,.T.);
#19129=EDGE_CURVE('',#15099,#15150,#8540,.T.);
#19130=EDGE_CURVE('',#15151,#15150,#8541,.T.);
#19131=EDGE_CURVE('',#15100,#15151,#8542,.T.);
#19132=EDGE_CURVE('',#15101,#15152,#8543,.T.);
#19133=EDGE_CURVE('',#15150,#15152,#12238,.T.);
#19134=EDGE_CURVE('',#14975,#15153,#12239,.T.);
#19135=EDGE_CURVE('',#15154,#15153,#12240,.T.);
#19136=EDGE_CURVE('',#14974,#15154,#12241,.T.);
#19137=EDGE_CURVE('',#15153,#15155,#8544,.T.);
#19138=EDGE_CURVE('',#15152,#15155,#8545,.T.);
#19139=EDGE_CURVE('',#15102,#15154,#8546,.T.);
#19140=EDGE_CURVE('',#15153,#15144,#1806,.T.);
#19141=EDGE_CURVE('',#15155,#15146,#12242,.T.);
#19142=EDGE_CURVE('',#15141,#15154,#1807,.T.);
#19143=EDGE_CURVE('',#15104,#15105,#12243,.T.);
#19144=EDGE_CURVE('',#15105,#14952,#8547,.T.);
#19145=EDGE_CURVE('',#14946,#15149,#1808,.T.);
#19146=EDGE_CURVE('',#15108,#14946,#8548,.T.);
#19147=EDGE_CURVE('',#15109,#14947,#8549,.T.);
#19148=EDGE_CURVE('',#15109,#15110,#12244,.T.);
#19149=EDGE_CURVE('',#14940,#15136,#1809,.T.);
#19150=EDGE_CURVE('',#15112,#14940,#8550,.T.);
#19151=EDGE_CURVE('',#15137,#14941,#1810,.T.);
#19152=EDGE_CURVE('',#14941,#15156,#8551,.T.);
#19153=EDGE_CURVE('',#15139,#15156,#12245,.T.);
#19154=EDGE_CURVE('',#15113,#15157,#8552,.T.);
#19155=EDGE_CURVE('',#15156,#15157,#8553,.T.);
#19156=EDGE_CURVE('',#15114,#15158,#8554,.T.);
#19157=EDGE_CURVE('',#15157,#15158,#12246,.T.);
#19158=EDGE_CURVE('',#15115,#15159,#8555,.T.);
#19159=EDGE_CURVE('',#15158,#15159,#8556,.T.);
#19160=EDGE_CURVE('',#15116,#15160,#8557,.T.);
#19161=EDGE_CURVE('',#15159,#15160,#12247,.T.);
#19162=EDGE_CURVE('',#15161,#15117,#8558,.T.);
#19163=EDGE_CURVE('',#15160,#15161,#8559,.T.);
#19164=EDGE_CURVE('',#15162,#15118,#8560,.T.);
#19165=EDGE_CURVE('',#15161,#15162,#12248,.T.);
#19166=EDGE_CURVE('',#15163,#15119,#8561,.T.);
#19167=EDGE_CURVE('',#15162,#15163,#8562,.T.);
#19168=EDGE_CURVE('',#15164,#15120,#8563,.T.);
#19169=EDGE_CURVE('',#15163,#15164,#12249,.T.);
#19170=EDGE_CURVE('',#15121,#15165,#8564,.T.);
#19171=EDGE_CURVE('',#15164,#15165,#8565,.T.);
#19172=EDGE_CURVE('',#15121,#15122,#12250,.T.);
#19173=EDGE_CURVE('',#15123,#15166,#8566,.T.);
#19174=EDGE_CURVE('',#15167,#15166,#8567,.T.);
#19175=EDGE_CURVE('',#15122,#15167,#8568,.T.);
#19176=EDGE_CURVE('',#15123,#15124,#12251,.T.);
#19177=EDGE_CURVE('',#15168,#15125,#8569,.T.);
#19178=EDGE_CURVE('',#15169,#15168,#8570,.T.);
#19179=EDGE_CURVE('',#15124,#15169,#8571,.T.);
#19180=EDGE_CURVE('',#15170,#15126,#8572,.T.);
#19181=EDGE_CURVE('',#15168,#15170,#12252,.T.);
#19182=EDGE_CURVE('',#15127,#15171,#8573,.T.);
#19183=EDGE_CURVE('',#15170,#15171,#8574,.T.);
#19184=EDGE_CURVE('',#15127,#15128,#12253,.T.);
#19185=EDGE_CURVE('',#15129,#15172,#8575,.T.);
#19186=EDGE_CURVE('',#15173,#15172,#8576,.T.);
#19187=EDGE_CURVE('',#15128,#15173,#8577,.T.);
#19188=EDGE_CURVE('',#15129,#15130,#12254,.T.);
#19189=EDGE_CURVE('',#15174,#15131,#8578,.T.);
#19190=EDGE_CURVE('',#15175,#15174,#8579,.T.);
#19191=EDGE_CURVE('',#15130,#15175,#8580,.T.);
#19192=EDGE_CURVE('',#15176,#15132,#8581,.T.);
#19193=EDGE_CURVE('',#15174,#15176,#12255,.T.);
#19194=EDGE_CURVE('',#15176,#15151,#8582,.T.);
#19195=EDGE_CURVE('',#15177,#15177,#12256,.T.);
#19196=EDGE_CURVE('',#15177,#15134,#8583,.T.);
#19197=EDGE_CURVE('',#15139,#15178,#12257,.T.);
#19198=EDGE_CURVE('',#15179,#15178,#12258,.T.);
#19199=EDGE_CURVE('',#15140,#15179,#12259,.T.);
#19200=EDGE_CURVE('',#14937,#15138,#1811,.T.);
#19201=EDGE_CURVE('',#15180,#15140,#12260,.T.);
#19202=EDGE_CURVE('',#15180,#14937,#8584,.T.);
#19203=EDGE_CURVE('',#14986,#15181,#12261,.T.);
#19204=EDGE_CURVE('',#15182,#15181,#12262,.T.);
#19205=EDGE_CURVE('',#14987,#15182,#12263,.T.);
#19206=EDGE_CURVE('',#15181,#15183,#8585,.T.);
#19207=EDGE_CURVE('',#15183,#15184,#12264,.T.);
#19208=EDGE_CURVE('',#15184,#15185,#8586,.T.);
#19209=EDGE_CURVE('',#15185,#15186,#12265,.T.);
#19210=EDGE_CURVE('',#15186,#15187,#12266,.T.);
#19211=EDGE_CURVE('',#15187,#15188,#12267,.T.);
#19212=EDGE_CURVE('',#15188,#15189,#8587,.T.);
#19213=EDGE_CURVE('',#15189,#15190,#12268,.T.);
#19214=EDGE_CURVE('',#15190,#15191,#8588,.T.);
#19215=EDGE_CURVE('',#15191,#15182,#12269,.T.);
#19216=EDGE_CURVE('',#15192,#15192,#12270,.T.);
#19217=EDGE_CURVE('',#15143,#14927,#1812,.T.);
#19218=EDGE_CURVE('',#15193,#14927,#8589,.T.);
#19219=EDGE_CURVE('',#15145,#15193,#12271,.T.);
#19220=EDGE_CURVE('',#15188,#15194,#12272,.T.);
#19221=EDGE_CURVE('',#15194,#15195,#12273,.T.);
#19222=EDGE_CURVE('',#15188,#15195,#12274,.T.);
#19223=EDGE_CURVE('',#15135,#14947,#1813,.T.);
#19224=EDGE_CURVE('',#14952,#15142,#1814,.T.);
#19225=EDGE_CURVE('',#15196,#15151,#617,.T.);
#19226=EDGE_CURVE('',#15150,#15197,#12275,.T.);
#19227=EDGE_CURVE('',#15196,#15197,#8590,.T.);
#19228=EDGE_CURVE('',#15152,#15198,#12276,.T.);
#19229=EDGE_CURVE('',#15197,#15198,#12277,.T.);
#19230=EDGE_CURVE('',#15155,#15199,#12278,.T.);
#19231=EDGE_CURVE('',#15198,#15199,#8591,.T.);
#19232=EDGE_CURVE('',#15146,#15200,#12279,.T.);
#19233=EDGE_CURVE('',#15199,#15200,#12280,.T.);
#19234=EDGE_CURVE('',#15156,#15201,#12281,.T.);
#19235=EDGE_CURVE('',#15178,#15201,#12282,.T.);
#19236=EDGE_CURVE('',#15157,#15202,#12283,.T.);
#19237=EDGE_CURVE('',#15201,#15202,#8592,.T.);
#19238=EDGE_CURVE('',#15158,#15203,#12284,.T.);
#19239=EDGE_CURVE('',#15202,#15203,#12285,.T.);
#19240=EDGE_CURVE('',#15159,#15204,#12286,.T.);
#19241=EDGE_CURVE('',#15203,#15204,#8593,.T.);
#19242=EDGE_CURVE('',#15160,#15205,#12287,.T.);
#19243=EDGE_CURVE('',#15204,#15205,#12288,.T.);
#19244=EDGE_CURVE('',#15161,#15206,#12289,.T.);
#19245=EDGE_CURVE('',#15205,#15206,#8594,.T.);
#19246=EDGE_CURVE('',#15162,#15207,#12290,.T.);
#19247=EDGE_CURVE('',#15206,#15207,#12291,.T.);
#19248=EDGE_CURVE('',#15163,#15208,#12292,.T.);
#19249=EDGE_CURVE('',#15207,#15208,#8595,.T.);
#19250=EDGE_CURVE('',#15164,#15209,#12293,.T.);
#19251=EDGE_CURVE('',#15208,#15209,#12294,.T.);
#19252=EDGE_CURVE('',#15165,#15210,#12295,.T.);
#19253=EDGE_CURVE('',#15209,#15210,#8596,.T.);
#19254=EDGE_CURVE('',#15165,#15167,#12296,.T.);
#19255=EDGE_CURVE('',#15166,#15211,#12297,.T.);
#19256=EDGE_CURVE('',#15210,#15211,#8597,.T.);
#19257=EDGE_CURVE('',#15167,#15210,#12298,.T.);
#19258=EDGE_CURVE('',#15166,#15169,#12299,.T.);
#19259=EDGE_CURVE('',#15168,#15212,#12300,.T.);
#19260=EDGE_CURVE('',#15211,#15212,#8598,.T.);
#19261=EDGE_CURVE('',#15169,#15211,#12301,.T.);
#19262=EDGE_CURVE('',#15170,#15213,#12302,.T.);
#19263=EDGE_CURVE('',#15212,#15213,#12303,.T.);
#19264=EDGE_CURVE('',#15171,#15214,#12304,.T.);
#19265=EDGE_CURVE('',#15213,#15214,#8599,.T.);
#19266=EDGE_CURVE('',#15171,#15173,#12305,.T.);
#19267=EDGE_CURVE('',#15172,#15215,#12306,.T.);
#19268=EDGE_CURVE('',#15214,#15215,#8600,.T.);
#19269=EDGE_CURVE('',#15173,#15214,#12307,.T.);
#19270=EDGE_CURVE('',#15172,#15175,#12308,.T.);
#19271=EDGE_CURVE('',#15174,#15216,#12309,.T.);
#19272=EDGE_CURVE('',#15215,#15216,#8601,.T.);
#19273=EDGE_CURVE('',#15175,#15215,#12310,.T.);
#19274=EDGE_CURVE('',#15176,#15217,#12311,.T.);
#19275=EDGE_CURVE('',#15216,#15217,#12312,.T.);
#19276=EDGE_CURVE('',#15217,#15196,#8602,.T.);
#19277=EDGE_CURVE('',#15218,#15218,#12313,.T.);
#19278=EDGE_CURVE('',#15180,#15179,#12314,.T.);
#19279=EDGE_CURVE('',#15219,#15219,#12315,.T.);
#19280=EDGE_CURVE('',#15219,#15220,#8603,.T.);
#19281=EDGE_CURVE('',#15221,#15220,#12316,.T.);
#19282=EDGE_CURVE('',#15220,#15221,#12317,.T.);
#19283=EDGE_CURVE('',#15222,#15180,#8604,.T.);
#19284=EDGE_CURVE('',#15222,#14933,#8605,.T.);
#19285=EDGE_CURVE('',#15223,#15223,#12318,.T.);
#19286=EDGE_CURVE('',#15223,#15192,#12319,.T.);
#19287=EDGE_CURVE('',#15184,#15224,#12320,.T.);
#19288=EDGE_CURVE('',#15224,#15225,#8606,.T.);
#19289=EDGE_CURVE('',#15185,#15225,#12321,.T.);
#19290=EDGE_CURVE('',#15183,#15226,#12322,.T.);
#19291=EDGE_CURVE('',#15226,#15224,#12323,.T.);
#19292=EDGE_CURVE('',#15189,#15227,#12324,.T.);
#19293=EDGE_CURVE('',#15227,#15228,#12325,.T.);
#19294=EDGE_CURVE('',#15190,#15228,#12326,.T.);
#19295=EDGE_CURVE('',#15195,#15227,#8607,.T.);
#19296=EDGE_CURVE('',#15187,#15229,#12327,.T.);
#19297=EDGE_CURVE('',#15229,#15194,#12328,.T.);
#19298=EDGE_CURVE('',#14986,#15230,#12329,.T.);
#19299=EDGE_CURVE('',#15181,#15230,#12330,.T.);
#19300=EDGE_CURVE('',#15230,#15226,#8608,.T.);
#19301=EDGE_CURVE('',#15231,#15182,#12331,.T.);
#19302=EDGE_CURVE('',#14987,#15231,#1815,.T.);
#19303=EDGE_CURVE('',#15191,#15232,#12332,.T.);
#19304=EDGE_CURVE('',#15232,#15231,#12333,.T.);
#19305=EDGE_CURVE('',#15228,#15232,#8609,.T.);
#19306=EDGE_CURVE('',#15185,#15233,#12334,.T.);
#19307=EDGE_CURVE('',#15233,#15234,#12335,.T.);
#19308=EDGE_CURVE('',#15186,#15234,#12336,.T.);
#19309=EDGE_CURVE('',#15234,#15229,#12337,.T.);
#19310=EDGE_CURVE('',#15235,#14931,#8610,.T.);
#19311=EDGE_CURVE('',#15193,#15235,#8611,.T.);
#19312=EDGE_CURVE('',#15221,#15236,#12338,.T.);
#19313=EDGE_CURVE('',#15237,#15236,#12339,.T.);
#19314=EDGE_CURVE('',#15238,#15237,#12340,.T.);
#19315=EDGE_CURVE('',#15236,#15238,#12341,.T.);
#19316=EDGE_CURVE('',#15239,#15239,#12342,.T.);
#19317=EDGE_CURVE('',#15239,#15218,#8612,.T.);
#19318=EDGE_CURVE('',#15240,#15179,#8613,.T.);
#19319=EDGE_CURVE('',#15222,#15240,#12343,.T.);
#19320=EDGE_CURVE('',#15241,#15222,#12344,.T.);
#19321=EDGE_CURVE('',#15242,#15240,#12345,.T.);
#19322=EDGE_CURVE('',#15241,#15242,#12346,.T.);
#19323=EDGE_CURVE('',#15243,#15241,#8614,.T.);
#19324=EDGE_CURVE('',#15244,#15242,#8615,.T.);
#19325=EDGE_CURVE('',#15243,#15244,#12347,.T.);
#19326=EDGE_CURVE('',#15245,#15243,#12348,.T.);
#19327=EDGE_CURVE('',#15246,#15244,#12349,.T.);
#19328=EDGE_CURVE('',#15245,#15246,#12350,.T.);
#19329=EDGE_CURVE('',#15247,#15245,#8616,.T.);
#19330=EDGE_CURVE('',#15248,#15246,#8617,.T.);
#19331=EDGE_CURVE('',#15247,#15248,#12351,.T.);
#19332=EDGE_CURVE('',#15225,#15233,#12352,.T.);
#19333=EDGE_CURVE('',#15245,#15224,#8618,.T.);
#19334=EDGE_CURVE('',#15243,#15226,#8619,.T.);
#19335=EDGE_CURVE('',#14985,#15249,#12353,.T.);
#19336=EDGE_CURVE('',#15230,#15249,#12354,.T.);
#19337=EDGE_CURVE('',#15241,#15249,#8620,.T.);
#19338=EDGE_CURVE('',#15219,#15250,#12355,.T.);
#19339=EDGE_CURVE('',#15250,#15250,#12356,.T.);
#19340=EDGE_CURVE('',#15251,#15252,#12357,.T.);
#19341=EDGE_CURVE('',#15252,#15253,#12358,.T.);
#19342=EDGE_CURVE('',#15254,#15253,#12359,.T.);
#19343=EDGE_CURVE('',#15251,#15254,#12360,.T.);
#19344=EDGE_CURVE('',#15255,#15194,#8621,.T.);
#19345=EDGE_CURVE('',#15255,#15256,#12361,.T.);
#19346=EDGE_CURVE('',#15256,#15195,#8622,.T.);
#19347=EDGE_CURVE('',#15257,#15258,#12362,.T.);
#19348=EDGE_CURVE('',#15258,#15259,#12363,.T.);
#19349=EDGE_CURVE('',#15260,#15259,#12364,.T.);
#19350=EDGE_CURVE('',#15257,#15260,#12365,.T.);
#19351=EDGE_CURVE('',#15253,#15258,#8623,.T.);
#19352=EDGE_CURVE('',#15254,#15257,#8624,.T.);
#19353=EDGE_CURVE('',#15249,#14933,#1816,.T.);
#19354=EDGE_CURVE('',#15223,#15250,#8625,.T.);
#19355=EDGE_CURVE('',#15259,#15261,#8626,.T.);
#19356=EDGE_CURVE('',#15262,#15261,#12366,.T.);
#19357=EDGE_CURVE('',#15260,#15262,#8627,.T.);
#19358=EDGE_CURVE('',#15263,#15264,#12367,.T.);
#19359=EDGE_CURVE('',#15264,#15265,#12368,.T.);
#19360=EDGE_CURVE('',#15266,#15265,#12369,.T.);
#19361=EDGE_CURVE('',#15263,#15266,#12370,.T.);
#19362=EDGE_CURVE('',#15267,#15263,#8628,.T.);
#19363=EDGE_CURVE('',#15268,#15266,#8629,.T.);
#19364=EDGE_CURVE('',#15267,#15268,#12371,.T.);
#19365=EDGE_CURVE('',#15200,#15269,#12372,.T.);
#19366=EDGE_CURVE('',#15269,#15270,#8630,.T.);
#19367=EDGE_CURVE('',#15270,#15268,#12373,.T.);
#19368=EDGE_CURVE('',#15265,#15271,#8631,.T.);
#19369=EDGE_CURVE('',#15271,#15272,#12374,.T.);
#19370=EDGE_CURVE('',#15272,#15273,#8632,.T.);
#19371=EDGE_CURVE('',#15273,#15274,#12375,.T.);
#19372=EDGE_CURVE('',#15274,#15275,#8633,.T.);
#19373=EDGE_CURVE('',#15275,#15276,#12376,.T.);
#19374=EDGE_CURVE('',#15276,#15277,#8634,.T.);
#19375=EDGE_CURVE('',#15277,#15248,#12377,.T.);
#19376=EDGE_CURVE('',#15145,#15269,#12378,.T.);
#19377=EDGE_CURVE('',#15193,#15269,#12379,.T.);
#19378=EDGE_CURVE('',#15235,#15270,#12380,.T.);
#19379=EDGE_CURVE('',#15235,#15267,#12381,.T.);
#19380=EDGE_CURVE('',#14931,#15231,#1817,.T.);
#19381=EDGE_CURVE('',#15267,#15232,#8635,.T.);
#19382=EDGE_CURVE('',#15263,#15228,#8636,.T.);
#19383=EDGE_CURVE('',#15264,#15227,#8637,.T.);
#19384=EDGE_CURVE('',#15264,#15278,#8638,.T.);
#19385=EDGE_CURVE('',#15279,#15256,#1818,.T.);
#19386=EDGE_CURVE('',#15280,#15279,#1819,.T.);
#19387=EDGE_CURVE('',#15281,#15280,#8639,.T.);
#19388=EDGE_CURVE('',#15278,#15281,#8640,.T.);
#19389=EDGE_CURVE('',#15278,#15271,#12382,.T.);
#19390=EDGE_CURVE('',#15278,#15282,#12383,.T.);
#19391=EDGE_CURVE('',#15282,#15272,#12384,.T.);
#19392=EDGE_CURVE('',#15282,#15283,#8641,.T.);
#19393=EDGE_CURVE('',#15283,#15273,#12385,.T.);
#19394=EDGE_CURVE('',#15283,#15284,#12386,.T.);
#19395=EDGE_CURVE('',#15284,#15274,#12387,.T.);
#19396=EDGE_CURVE('',#15284,#15285,#8642,.T.);
#19397=EDGE_CURVE('',#15285,#15275,#12388,.T.);
#19398=EDGE_CURVE('',#15285,#15286,#12389,.T.);
#19399=EDGE_CURVE('',#15286,#15276,#12390,.T.);
#19400=EDGE_CURVE('',#15286,#15287,#8643,.T.);
#19401=EDGE_CURVE('',#15287,#15277,#12391,.T.);
#19402=EDGE_CURVE('',#15287,#15247,#12392,.T.);
#19403=EDGE_CURVE('',#15287,#15288,#8644,.T.);
#19404=EDGE_CURVE('',#15289,#15288,#1820,.T.);
#19405=EDGE_CURVE('',#15247,#15289,#8645,.T.);
#19406=EDGE_CURVE('',#15252,#15286,#8646,.T.);
#19407=EDGE_CURVE('',#15290,#15252,#8647,.T.);
#19408=EDGE_CURVE('',#15288,#15290,#1821,.T.);
#19409=EDGE_CURVE('',#15253,#15285,#8648,.T.);
#19410=EDGE_CURVE('',#15284,#15258,#8649,.T.);
#19411=EDGE_CURVE('',#15283,#15259,#8650,.T.);
#19412=EDGE_CURVE('',#15282,#15261,#8651,.T.);
#19413=EDGE_CURVE('',#15261,#15281,#12393,.T.);
#19414=EDGE_CURVE('',#15291,#15281,#12394,.T.);
#19415=EDGE_CURVE('',#15262,#15291,#12395,.T.);
#19416=EDGE_CURVE('',#15292,#15280,#618,.T.);
#19417=EDGE_CURVE('',#15291,#15292,#8652,.T.);
#19418=EDGE_CURVE('',#15293,#15279,#619,.T.);
#19419=EDGE_CURVE('',#15292,#15293,#1822,.T.);
#19420=EDGE_CURVE('',#15293,#15255,#1823,.T.);
#19421=EDGE_CURVE('',#15294,#15255,#12396,.T.);
#19422=EDGE_CURVE('',#15293,#15294,#12397,.T.);
#19423=EDGE_CURVE('',#15229,#15294,#8653,.T.);
#19424=EDGE_CURVE('',#15234,#15295,#8654,.T.);
#19425=EDGE_CURVE('',#15295,#15294,#12398,.T.);
#19426=EDGE_CURVE('',#15233,#15296,#8655,.T.);
#19427=EDGE_CURVE('',#15296,#15295,#12399,.T.);
#19428=EDGE_CURVE('',#15225,#15297,#8656,.T.);
#19429=EDGE_CURVE('',#15296,#15297,#12400,.T.);
#19430=EDGE_CURVE('',#15298,#15289,#1824,.T.);
#19431=EDGE_CURVE('',#15297,#15298,#1825,.T.);
#19432=EDGE_CURVE('',#15299,#15298,#620,.T.);
#19433=EDGE_CURVE('',#15300,#15289,#621,.T.);
#19434=EDGE_CURVE('',#15299,#15300,#1826,.T.);
#19435=EDGE_CURVE('',#15296,#15299,#1827,.T.);
#19436=EDGE_CURVE('',#15299,#15295,#12401,.T.);
#19437=EDGE_CURVE('',#15300,#15301,#1828,.T.);
#19438=EDGE_CURVE('',#15301,#15302,#1829,.T.);
#19439=EDGE_CURVE('',#15302,#15292,#12402,.T.);
#19440=EDGE_CURVE('',#15301,#15288,#622,.T.);
#19441=EDGE_CURVE('',#15302,#15290,#623,.T.);
#19442=EDGE_CURVE('',#15302,#15251,#8657,.T.);
#19443=EDGE_CURVE('',#15303,#15304,#12403,.T.);
#19444=EDGE_CURVE('',#15304,#15305,#1830,.T.);
#19445=EDGE_CURVE('',#15306,#15305,#12404,.T.);
#19446=EDGE_CURVE('',#15307,#15306,#1831,.T.);
#19447=EDGE_CURVE('',#15307,#15308,#12405,.T.);
#19448=EDGE_CURVE('',#15309,#15308,#1832,.T.);
#19449=EDGE_CURVE('',#15310,#15309,#12406,.T.);
#19450=EDGE_CURVE('',#15311,#15310,#1833,.T.);
#19451=EDGE_CURVE('',#15311,#15312,#12407,.T.);
#19452=EDGE_CURVE('',#15303,#15312,#1834,.T.);
#19453=EDGE_CURVE('',#15313,#15314,#12408,.T.);
#19454=EDGE_CURVE('',#15314,#15313,#12409,.T.);
#19455=EDGE_CURVE('',#15314,#15315,#8658,.T.);
#19456=EDGE_CURVE('',#15315,#15315,#12410,.T.);
#19457=EDGE_CURVE('',#15316,#15317,#12411,.T.);
#19458=EDGE_CURVE('',#15317,#15318,#8659,.T.);
#19459=EDGE_CURVE('',#15318,#15319,#1835,.T.);
#19460=EDGE_CURVE('',#15319,#15320,#8660,.T.);
#19461=EDGE_CURVE('',#15320,#15321,#12412,.T.);
#19462=EDGE_CURVE('',#15322,#15321,#8661,.T.);
#19463=EDGE_CURVE('',#15323,#15322,#1836,.T.);
#19464=EDGE_CURVE('',#15316,#15323,#8662,.T.);
#19465=EDGE_CURVE('',#15305,#15306,#12413,.T.);
#19466=EDGE_CURVE('',#15324,#15324,#12414,.T.);
#19467=EDGE_CURVE('',#15325,#15326,#8663,.T.);
#19468=EDGE_CURVE('',#15327,#15326,#12415,.T.);
#19469=EDGE_CURVE('',#15328,#15327,#8664,.T.);
#19470=EDGE_CURVE('',#15328,#15325,#12416,.T.);
#19471=EDGE_CURVE('',#15329,#15328,#8665,.T.);
#19472=EDGE_CURVE('',#15330,#15327,#8666,.T.);
#19473=EDGE_CURVE('',#15329,#15330,#8667,.T.);
#19474=EDGE_CURVE('',#15331,#15332,#8668,.T.);
#19475=EDGE_CURVE('',#15332,#15326,#8669,.T.);
#19476=EDGE_CURVE('',#15331,#15325,#8670,.T.);
#19477=EDGE_CURVE('',#15332,#15330,#12417,.T.);
#19478=EDGE_CURVE('',#15331,#15329,#12418,.T.);
#19479=EDGE_CURVE('',#15333,#15334,#8671,.T.);
#19480=EDGE_CURVE('',#15335,#15333,#12419,.T.);
#19481=EDGE_CURVE('',#15335,#15336,#8672,.T.);
#19482=EDGE_CURVE('',#15336,#15334,#12420,.T.);
#19483=EDGE_CURVE('',#15337,#15335,#8673,.T.);
#19484=EDGE_CURVE('',#15337,#15338,#8674,.T.);
#19485=EDGE_CURVE('',#15338,#15336,#8675,.T.);
#19486=EDGE_CURVE('',#15339,#15334,#8676,.T.);
#19487=EDGE_CURVE('',#15340,#15339,#8677,.T.);
#19488=EDGE_CURVE('',#15340,#15333,#8678,.T.);
#19489=EDGE_CURVE('',#15340,#15337,#12421,.T.);
#19490=EDGE_CURVE('',#15339,#15338,#12422,.T.);
#19491=EDGE_CURVE('',#15341,#15342,#12423,.T.);
#19492=EDGE_CURVE('',#15342,#15343,#8679,.T.);
#19493=EDGE_CURVE('',#15343,#15344,#12424,.T.);
#19494=EDGE_CURVE('',#15344,#15345,#8680,.T.);
#19495=EDGE_CURVE('',#15346,#15345,#12425,.T.);
#19496=EDGE_CURVE('',#15347,#15346,#8681,.T.);
#19497=EDGE_CURVE('',#15347,#15348,#12426,.T.);
#19498=EDGE_CURVE('',#15348,#15349,#8682,.T.);
#19499=EDGE_CURVE('',#15350,#15349,#12427,.T.);
#19500=EDGE_CURVE('',#15351,#15350,#8683,.T.);
#19501=EDGE_CURVE('',#15351,#15352,#12428,.T.);
#19502=EDGE_CURVE('',#15352,#15353,#8684,.T.);
#19503=EDGE_CURVE('',#15354,#15353,#1837,.T.);
#19504=EDGE_CURVE('',#15355,#15354,#12429,.T.);
#19505=EDGE_CURVE('',#15356,#15355,#1838,.T.);
#19506=EDGE_CURVE('',#15357,#15356,#8685,.T.);
#19507=EDGE_CURVE('',#15357,#15358,#12430,.T.);
#19508=EDGE_CURVE('',#15358,#15359,#8686,.T.);
#19509=EDGE_CURVE('',#15360,#15359,#1839,.T.);
#19510=EDGE_CURVE('',#15360,#15361,#12431,.T.);
#19511=EDGE_CURVE('',#15361,#15362,#1840,.T.);
#19512=EDGE_CURVE('',#15363,#15362,#8687,.T.);
#19513=EDGE_CURVE('',#15363,#15364,#12432,.T.);
#19514=EDGE_CURVE('',#15364,#15365,#8688,.T.);
#19515=EDGE_CURVE('',#15365,#15366,#1841,.T.);
#19516=EDGE_CURVE('',#15366,#15367,#12433,.T.);
#19517=EDGE_CURVE('',#15367,#15368,#1842,.T.);
#19518=EDGE_CURVE('',#15369,#15368,#8689,.T.);
#19519=EDGE_CURVE('',#15369,#15370,#12434,.T.);
#19520=EDGE_CURVE('',#15370,#15371,#8690,.T.);
#19521=EDGE_CURVE('',#15372,#15371,#12435,.T.);
#19522=EDGE_CURVE('',#15373,#15372,#8691,.T.);
#19523=EDGE_CURVE('',#15373,#15374,#12436,.T.);
#19524=EDGE_CURVE('',#15374,#15375,#8692,.T.);
#19525=EDGE_CURVE('',#15376,#15375,#12437,.T.);
#19526=EDGE_CURVE('',#15377,#15376,#8693,.T.);
#19527=EDGE_CURVE('',#15377,#15343,#12438,.T.);
#19528=EDGE_CURVE('',#15342,#15378,#12439,.T.);
#19529=EDGE_CURVE('',#15379,#15378,#1843,.T.);
#19530=EDGE_CURVE('',#15379,#15380,#8694,.T.);
#19531=EDGE_CURVE('',#15380,#15381,#1844,.T.);
#19532=EDGE_CURVE('',#15381,#15382,#12440,.T.);
#19533=EDGE_CURVE('',#15382,#15383,#1845,.T.);
#19534=EDGE_CURVE('',#15384,#15383,#8695,.T.);
#19535=EDGE_CURVE('',#15385,#15384,#1846,.T.);
#19536=EDGE_CURVE('',#15385,#15386,#12441,.T.);
#19537=EDGE_CURVE('',#15387,#15386,#1847,.T.);
#19538=EDGE_CURVE('',#15387,#15388,#8696,.T.);
#19539=EDGE_CURVE('',#15388,#15389,#1848,.T.);
#19540=EDGE_CURVE('',#15390,#15389,#12442,.T.);
#19541=EDGE_CURVE('',#15390,#15391,#1849,.T.);
#19542=EDGE_CURVE('',#15392,#15391,#8697,.T.);
#19543=EDGE_CURVE('',#15341,#15392,#1850,.T.);
#19544=EDGE_CURVE('',#15313,#15393,#8698,.T.);
#19545=EDGE_CURVE('',#15394,#15393,#12443,.T.);
#19546=EDGE_CURVE('',#15395,#15394,#1851,.T.);
#19547=EDGE_CURVE('',#15395,#15396,#8699,.T.);
#19548=EDGE_CURVE('',#15396,#15397,#1852,.T.);
#19549=EDGE_CURVE('',#15397,#15398,#12444,.T.);
#19550=EDGE_CURVE('',#15398,#15399,#1853,.T.);
#19551=EDGE_CURVE('',#15400,#15399,#8700,.T.);
#19552=EDGE_CURVE('',#15401,#15400,#1854,.T.);
#19553=EDGE_CURVE('',#15401,#15402,#12445,.T.);
#19554=EDGE_CURVE('',#15403,#15402,#1855,.T.);
#19555=EDGE_CURVE('',#15403,#15404,#8701,.T.);
#19556=EDGE_CURVE('',#15404,#15405,#1856,.T.);
#19557=EDGE_CURVE('',#15406,#15405,#12446,.T.);
#19558=EDGE_CURVE('',#15406,#15407,#1857,.T.);
#19559=EDGE_CURVE('',#15408,#15407,#8702,.T.);
#19560=EDGE_CURVE('',#15409,#15408,#1858,.T.);
#19561=EDGE_CURVE('',#15393,#15409,#12447,.T.);
#19562=EDGE_CURVE('',#15410,#15374,#8703,.T.);
#19563=EDGE_CURVE('',#15410,#15411,#8704,.T.);
#19564=EDGE_CURVE('',#15411,#15375,#8705,.T.);
#19565=EDGE_CURVE('',#15412,#15372,#8706,.T.);
#19566=EDGE_CURVE('',#15412,#15413,#8707,.T.);
#19567=EDGE_CURVE('',#15413,#15373,#8708,.T.);
#19568=EDGE_CURVE('',#15411,#15414,#12448,.T.);
#19569=EDGE_CURVE('',#15410,#15415,#12449,.T.);
#19570=EDGE_CURVE('',#15414,#15415,#8709,.T.);
#19571=EDGE_CURVE('',#15415,#15413,#12450,.T.);
#19572=EDGE_CURVE('',#15414,#15412,#12451,.T.);
#19573=EDGE_CURVE('',#15416,#15417,#8710,.T.);
#19574=EDGE_CURVE('',#15417,#15418,#12452,.T.);
#19575=EDGE_CURVE('',#15418,#15419,#8711,.T.);
#19576=EDGE_CURVE('',#15416,#15419,#12453,.T.);
#19577=EDGE_CURVE('',#15420,#15421,#8712,.T.);
#19578=EDGE_CURVE('',#15417,#15420,#12454,.T.);
#19579=EDGE_CURVE('',#15421,#15416,#12455,.T.);
#19580=EDGE_CURVE('',#15421,#15422,#12456,.T.);
#19581=EDGE_CURVE('',#15423,#15422,#8713,.T.);
#19582=EDGE_CURVE('',#15423,#15420,#12457,.T.);
#19583=EDGE_CURVE('',#15371,#15422,#8714,.T.);
#19584=EDGE_CURVE('',#15370,#15423,#8715,.T.);
#19585=EDGE_CURVE('',#15424,#15419,#12458,.T.);
#19586=EDGE_CURVE('',#15418,#15425,#12459,.T.);
#19587=EDGE_CURVE('',#15425,#15424,#8716,.T.);
#19588=EDGE_CURVE('',#15424,#15376,#8717,.T.);
#19589=EDGE_CURVE('',#15425,#15377,#8718,.T.);
#19590=EDGE_CURVE('',#15426,#15427,#12460,.T.);
#19591=EDGE_CURVE('',#15428,#15427,#8719,.T.);
#19592=EDGE_CURVE('',#15428,#15429,#12461,.T.);
#19593=EDGE_CURVE('',#15429,#15426,#8720,.T.);
#19594=EDGE_CURVE('',#15427,#15430,#8721,.T.);
#19595=EDGE_CURVE('',#15431,#15430,#8722,.T.);
#19596=EDGE_CURVE('',#15431,#15428,#8723,.T.);
#19597=EDGE_CURVE('',#15432,#15320,#12462,.T.);
#19598=EDGE_CURVE('',#15433,#15319,#12463,.T.);
#19599=EDGE_CURVE('',#15433,#15432,#8724,.T.);
#19600=EDGE_CURVE('',#15434,#15435,#12464,.T.);
#19601=EDGE_CURVE('',#15435,#15320,#12465,.T.);
#19602=EDGE_CURVE('',#15434,#15432,#12466,.T.);
#19603=EDGE_CURVE('',#15361,#15434,#8725,.T.);
#19604=EDGE_CURVE('',#15362,#15432,#8726,.T.);
#19605=EDGE_CURVE('',#15436,#15433,#8727,.T.);
#19606=EDGE_CURVE('',#15437,#15436,#624,.T.);
#19607=EDGE_CURVE('',#15438,#15437,#8728,.T.);
#19608=EDGE_CURVE('',#15363,#15438,#8729,.T.);
#19609=EDGE_CURVE('',#15439,#15437,#1859,.T.);
#19610=EDGE_CURVE('',#15440,#15439,#8730,.T.);
#19611=EDGE_CURVE('',#15440,#15438,#12467,.T.);
#19612=EDGE_CURVE('',#15439,#15365,#8731,.T.);
#19613=EDGE_CURVE('',#15440,#15364,#8732,.T.);
#19614=EDGE_CURVE('',#15430,#15441,#12468,.T.);
#19615=EDGE_CURVE('',#15442,#15441,#8733,.T.);
#19616=EDGE_CURVE('',#15442,#15431,#12469,.T.);
#19617=EDGE_CURVE('',#15443,#15436,#625,.T.);
#19618=EDGE_CURVE('',#15439,#15443,#1860,.T.);
#19619=EDGE_CURVE('',#15443,#15366,#8734,.T.);
#19620=EDGE_CURVE('',#15444,#15319,#12470,.T.);
#19621=EDGE_CURVE('',#15444,#15318,#12471,.T.);
#19622=EDGE_CURVE('',#15445,#15433,#12472,.T.);
#19623=EDGE_CURVE('',#15446,#15444,#1861,.T.);
#19624=EDGE_CURVE('',#15445,#15446,#1862,.T.);
#19625=EDGE_CURVE('',#15443,#15447,#8735,.T.);
#19626=EDGE_CURVE('',#15447,#15445,#1863,.T.);
#19627=EDGE_CURVE('',#15367,#15447,#8736,.T.);
#19628=EDGE_CURVE('',#15448,#15318,#1864,.T.);
#19629=EDGE_CURVE('',#15446,#15448,#12473,.T.);
#19630=EDGE_CURVE('',#15449,#15317,#12474,.T.);
#19631=EDGE_CURVE('',#15448,#15449,#8737,.T.);
#19632=EDGE_CURVE('',#15450,#15448,#1865,.T.);
#19633=EDGE_CURVE('',#15445,#15450,#626,.T.);
#19634=EDGE_CURVE('',#15451,#15450,#627,.T.);
#19635=EDGE_CURVE('',#15447,#15451,#628,.T.);
#19636=EDGE_CURVE('',#15368,#15451,#8738,.T.);
#19637=EDGE_CURVE('',#15369,#15449,#8739,.T.);
#19638=EDGE_CURVE('',#15452,#15453,#8740,.T.);
#19639=EDGE_CURVE('',#15426,#15453,#12475,.F.);
#19640=EDGE_CURVE('',#15429,#15452,#12476,.T.);
#19641=EDGE_CURVE('',#15454,#15452,#12477,.T.);
#19642=EDGE_CURVE('',#15454,#15455,#8741,.T.);
#19643=EDGE_CURVE('',#15453,#15455,#12478,.T.);
#19644=EDGE_CURVE('',#15456,#15454,#8742,.T.);
#19645=EDGE_CURVE('',#15456,#15457,#8743,.T.);
#19646=EDGE_CURVE('',#15455,#15457,#8744,.T.);
#19647=EDGE_CURVE('',#15458,#15459,#8745,.T.);
#19648=EDGE_CURVE('',#15458,#15322,#12479,.T.);
#19649=EDGE_CURVE('',#15459,#15321,#12480,.T.);
#19650=EDGE_CURVE('',#15460,#15459,#12481,.T.);
#19651=EDGE_CURVE('',#15461,#15321,#12482,.T.);
#19652=EDGE_CURVE('',#15460,#15461,#12483,.T.);
#19653=EDGE_CURVE('',#15360,#15460,#8746,.T.);
#19654=EDGE_CURVE('',#15461,#15435,#12484,.T.);
#19655=EDGE_CURVE('',#15442,#15462,#12485,.T.);
#19656=EDGE_CURVE('',#15462,#15456,#12486,.T.);
#19657=EDGE_CURVE('',#15359,#15459,#8747,.T.);
#19658=EDGE_CURVE('',#15358,#15463,#8748,.T.);
#19659=EDGE_CURVE('',#15463,#15464,#8749,.T.);
#19660=EDGE_CURVE('',#15464,#15465,#629,.T.);
#19661=EDGE_CURVE('',#15465,#15458,#8750,.T.);
#19662=EDGE_CURVE('',#15466,#15463,#12487,.T.);
#19663=EDGE_CURVE('',#15466,#15467,#8751,.T.);
#19664=EDGE_CURVE('',#15467,#15464,#12488,.T.);
#19665=EDGE_CURVE('',#15466,#15357,#8752,.T.);
#19666=EDGE_CURVE('',#15467,#15356,#8753,.T.);
#19667=EDGE_CURVE('',#15462,#15468,#8754,.T.);
#19668=EDGE_CURVE('',#15457,#15468,#12489,.T.);
#19669=EDGE_CURVE('',#15468,#15441,#12490,.T.);
#19670=EDGE_CURVE('',#15467,#15469,#630,.T.);
#19671=EDGE_CURVE('',#15469,#15465,#631,.T.);
#19672=EDGE_CURVE('',#15469,#15355,#8755,.T.);
#19673=EDGE_CURVE('',#15470,#15323,#12491,.T.);
#19674=EDGE_CURVE('',#15470,#15322,#632,.T.);
#19675=EDGE_CURVE('',#15471,#15472,#1866,.T.);
#19676=EDGE_CURVE('',#15472,#15470,#1867,.T.);
#19677=EDGE_CURVE('',#15471,#15458,#12492,.T.);
#19678=EDGE_CURVE('',#15473,#15471,#1868,.T.);
#19679=EDGE_CURVE('',#15469,#15473,#8756,.T.);
#19680=EDGE_CURVE('',#15354,#15473,#8757,.T.);
#19681=EDGE_CURVE('',#15472,#15474,#12493,.T.);
#19682=EDGE_CURVE('',#15474,#15323,#1869,.T.);
#19683=EDGE_CURVE('',#15474,#15475,#8758,.T.);
#19684=EDGE_CURVE('',#15475,#15316,#12494,.T.);
#19685=EDGE_CURVE('',#15471,#15476,#633,.T.);
#19686=EDGE_CURVE('',#15476,#15474,#1870,.T.);
#19687=EDGE_CURVE('',#15473,#15477,#634,.T.);
#19688=EDGE_CURVE('',#15477,#15476,#635,.T.);
#19689=EDGE_CURVE('',#15353,#15477,#8759,.T.);
#19690=EDGE_CURVE('',#15352,#15475,#8760,.T.);
#19691=EDGE_CURVE('',#15478,#15348,#8761,.T.);
#19692=EDGE_CURVE('',#15478,#15479,#8762,.T.);
#19693=EDGE_CURVE('',#15479,#15349,#8763,.T.);
#19694=EDGE_CURVE('',#15480,#15346,#8764,.T.);
#19695=EDGE_CURVE('',#15480,#15481,#8765,.T.);
#19696=EDGE_CURVE('',#15481,#15347,#8766,.T.);
#19697=EDGE_CURVE('',#15479,#15482,#12495,.T.);
#19698=EDGE_CURVE('',#15478,#15483,#12496,.T.);
#19699=EDGE_CURVE('',#15482,#15483,#8767,.T.);
#19700=EDGE_CURVE('',#15483,#15481,#12497,.T.);
#19701=EDGE_CURVE('',#15482,#15480,#12498,.T.);
#19702=EDGE_CURVE('',#15484,#15485,#8768,.T.);
#19703=EDGE_CURVE('',#15485,#15486,#12499,.T.);
#19704=EDGE_CURVE('',#15486,#15487,#8769,.T.);
#19705=EDGE_CURVE('',#15484,#15487,#12500,.T.);
#19706=EDGE_CURVE('',#15488,#15489,#8770,.T.);
#19707=EDGE_CURVE('',#15485,#15488,#12501,.T.);
#19708=EDGE_CURVE('',#15489,#15484,#12502,.T.);
#19709=EDGE_CURVE('',#15489,#15490,#12503,.T.);
#19710=EDGE_CURVE('',#15491,#15490,#8771,.T.);
#19711=EDGE_CURVE('',#15491,#15488,#12504,.T.);
#19712=EDGE_CURVE('',#15345,#15490,#8772,.T.);
#19713=EDGE_CURVE('',#15344,#15491,#8773,.T.);
#19714=EDGE_CURVE('',#15492,#15487,#12505,.T.);
#19715=EDGE_CURVE('',#15486,#15493,#12506,.T.);
#19716=EDGE_CURVE('',#15493,#15492,#8774,.T.);
#19717=EDGE_CURVE('',#15492,#15350,#8775,.T.);
#19718=EDGE_CURVE('',#15493,#15351,#8776,.T.);
#19719=EDGE_CURVE('',#15404,#15383,#8777,.T.);
#19720=EDGE_CURVE('',#15384,#15403,#8778,.T.);
#19721=EDGE_CURVE('',#15405,#15382,#8779,.T.);
#19722=EDGE_CURVE('',#15406,#15381,#8780,.T.);
#19723=EDGE_CURVE('',#15407,#15380,#8781,.T.);
#19724=EDGE_CURVE('',#15379,#15408,#8782,.T.);
#19725=EDGE_CURVE('',#15388,#15399,#8783,.T.);
#19726=EDGE_CURVE('',#15400,#15387,#8784,.T.);
#19727=EDGE_CURVE('',#15389,#15398,#8785,.T.);
#19728=EDGE_CURVE('',#15390,#15397,#8786,.T.);
#19729=EDGE_CURVE('',#15391,#15396,#8787,.T.);
#19730=EDGE_CURVE('',#15395,#15392,#8788,.T.);
#19731=EDGE_CURVE('',#15378,#15409,#8789,.T.);
#19732=EDGE_CURVE('',#15394,#15341,#8790,.T.);
#19733=EDGE_CURVE('',#15385,#15402,#8791,.T.);
#19734=EDGE_CURVE('',#15401,#15386,#8792,.T.);
#19735=EDGE_CURVE('',#15494,#15494,#12507,.T.);
#19736=EDGE_CURVE('',#15494,#15324,#8793,.T.);
#19737=EDGE_CURVE('',#15495,#15496,#12508,.T.);
#19738=EDGE_CURVE('',#15497,#15495,#8794,.T.);
#19739=EDGE_CURVE('',#15498,#15497,#12509,.T.);
#19740=EDGE_CURVE('',#15499,#15498,#8795,.T.);
#19741=EDGE_CURVE('',#15500,#15499,#12510,.T.);
#19742=EDGE_CURVE('',#15501,#15500,#8796,.T.);
#19743=EDGE_CURVE('',#15502,#15501,#12511,.T.);
#19744=EDGE_CURVE('',#15503,#15502,#8797,.T.);
#19745=EDGE_CURVE('',#15504,#15503,#12512,.T.);
#19746=EDGE_CURVE('',#15505,#15504,#8798,.T.);
#19747=EDGE_CURVE('',#15506,#15505,#12513,.T.);
#19748=EDGE_CURVE('',#15496,#15506,#8799,.T.);
#19749=EDGE_CURVE('',#15311,#15495,#8800,.T.);
#19750=EDGE_CURVE('',#15310,#15497,#8801,.T.);
#19751=EDGE_CURVE('',#15312,#15496,#8802,.T.);
#19752=EDGE_CURVE('',#15303,#15506,#8803,.T.);
#19753=EDGE_CURVE('',#15507,#15505,#8804,.T.);
#19754=EDGE_CURVE('',#15304,#15507,#12514,.T.);
#19755=EDGE_CURVE('',#15508,#15504,#8805,.T.);
#19756=EDGE_CURVE('',#15508,#15507,#1871,.T.);
#19757=EDGE_CURVE('',#15509,#15503,#8806,.T.);
#19758=EDGE_CURVE('',#15508,#15509,#12515,.T.);
#19759=EDGE_CURVE('',#15510,#15502,#8807,.T.);
#19760=EDGE_CURVE('',#15510,#15509,#1872,.T.);
#19761=EDGE_CURVE('',#15511,#15501,#8808,.T.);
#19762=EDGE_CURVE('',#15510,#15511,#12516,.T.);
#19763=EDGE_CURVE('',#15512,#15500,#8809,.T.);
#19764=EDGE_CURVE('',#15512,#15511,#1873,.T.);
#19765=EDGE_CURVE('',#15308,#15499,#8810,.T.);
#19766=EDGE_CURVE('',#15512,#15307,#12517,.T.);
#19767=EDGE_CURVE('',#15309,#15498,#8811,.T.);
#19768=EDGE_CURVE('',#15513,#15514,#1874,.T.);
#19769=EDGE_CURVE('',#15515,#15513,#12518,.T.);
#19770=EDGE_CURVE('',#15515,#15516,#8812,.T.);
#19771=EDGE_CURVE('',#15516,#15517,#12519,.T.);
#19772=EDGE_CURVE('',#15514,#15517,#8813,.T.);
#19773=EDGE_CURVE('',#15518,#15519,#8814,.T.);
#19774=EDGE_CURVE('',#15519,#15516,#12520,.T.);
#19775=EDGE_CURVE('',#15520,#15515,#12521,.T.);
#19776=EDGE_CURVE('',#15518,#15520,#636,.T.);
#19777=EDGE_CURVE('',#15521,#15518,#1875,.T.);
#19778=EDGE_CURVE('',#15521,#15522,#8815,.T.);
#19779=EDGE_CURVE('',#15522,#15519,#12522,.T.);
#19780=EDGE_CURVE('',#15523,#15524,#8816,.T.);
#19781=EDGE_CURVE('',#15523,#15525,#12523,.T.);
#19782=EDGE_CURVE('',#15525,#15526,#8817,.T.);
#19783=EDGE_CURVE('',#15526,#15524,#1876,.T.);
#19784=EDGE_CURVE('',#15527,#15528,#8818,.T.);
#19785=EDGE_CURVE('',#15527,#15529,#12524,.T.);
#19786=EDGE_CURVE('',#15529,#15530,#8819,.T.);
#19787=EDGE_CURVE('',#15530,#15528,#12525,.T.);
#19788=EDGE_CURVE('',#15531,#15532,#8820,.T.);
#19789=EDGE_CURVE('',#15532,#15527,#8821,.T.);
#19790=EDGE_CURVE('',#15528,#15531,#8822,.T.);
#19791=EDGE_CURVE('',#15531,#15533,#12526,.T.);
#19792=EDGE_CURVE('',#15533,#15534,#8823,.T.);
#19793=EDGE_CURVE('',#15534,#15532,#12527,.T.);
#19794=EDGE_CURVE('',#15535,#15536,#8824,.T.);
#19795=EDGE_CURVE('',#15536,#15534,#12528,.T.);
#19796=EDGE_CURVE('',#15533,#15535,#12529,.T.);
#19797=EDGE_CURVE('',#15535,#15537,#12530,.T.);
#19798=EDGE_CURVE('',#15537,#15538,#8825,.T.);
#19799=EDGE_CURVE('',#15538,#15539,#1877,.T.);
#19800=EDGE_CURVE('',#15539,#15540,#8826,.T.);
#19801=EDGE_CURVE('',#15540,#15536,#12531,.T.);
#19802=EDGE_CURVE('',#15541,#15542,#8827,.T.);
#19803=EDGE_CURVE('',#15541,#15540,#8828,.T.);
#19804=EDGE_CURVE('',#15539,#15543,#12532,.T.);
#19805=EDGE_CURVE('',#15543,#15542,#8829,.T.);
#19806=EDGE_CURVE('',#15544,#15545,#1878,.T.);
#19807=EDGE_CURVE('',#15517,#15544,#8830,.T.);
#19808=EDGE_CURVE('',#15546,#15517,#12533,.T.);
#19809=EDGE_CURVE('',#15546,#15545,#8831,.T.);
#19810=EDGE_CURVE('',#15546,#15516,#12534,.T.);
#19811=EDGE_CURVE('',#15547,#15546,#12535,.T.);
#19812=EDGE_CURVE('',#15547,#15519,#12536,.T.);
#19813=EDGE_CURVE('',#15547,#15522,#12537,.T.);
#19814=EDGE_CURVE('',#15548,#15547,#8832,.T.);
#19815=EDGE_CURVE('',#15549,#15522,#8833,.T.);
#19816=EDGE_CURVE('',#15548,#15549,#12538,.T.);
#19817=EDGE_CURVE('',#15550,#15548,#12539,.T.);
#19818=EDGE_CURVE('',#15551,#15549,#12540,.T.);
#19819=EDGE_CURVE('',#15550,#15551,#12541,.T.);
#19820=EDGE_CURVE('',#15552,#15550,#12542,.T.);
#19821=EDGE_CURVE('',#15525,#15551,#12543,.T.);
#19822=EDGE_CURVE('',#15552,#15525,#12544,.T.);
#19823=EDGE_CURVE('',#15553,#15552,#12545,.T.);
#19824=EDGE_CURVE('',#15553,#15523,#12546,.T.);
#19825=EDGE_CURVE('',#15554,#15553,#12547,.T.);
#19826=EDGE_CURVE('',#15529,#15523,#12548,.T.);
#19827=EDGE_CURVE('',#15554,#15529,#12549,.T.);
#19828=EDGE_CURVE('',#15555,#15554,#12550,.T.);
#19829=EDGE_CURVE('',#15555,#15527,#12551,.T.);
#19830=EDGE_CURVE('',#15556,#15555,#8834,.T.);
#19831=EDGE_CURVE('',#15556,#15532,#12552,.T.);
#19832=EDGE_CURVE('',#15556,#15534,#12553,.T.);
#19833=EDGE_CURVE('',#15557,#15556,#12554,.T.);
#19834=EDGE_CURVE('',#15557,#15536,#12555,.T.);
#19835=EDGE_CURVE('',#15557,#15540,#12556,.T.);
#19836=EDGE_CURVE('',#15558,#15541,#1879,.T.);
#19837=EDGE_CURVE('',#15558,#15557,#8835,.T.);
#19838=EDGE_CURVE('',#15559,#15558,#12557,.T.);
#19839=EDGE_CURVE('',#15545,#15559,#12558,.T.);
#19840=EDGE_CURVE('',#15560,#15561,#8836,.T.);
#19841=EDGE_CURVE('',#15561,#15562,#8837,.T.);
#19842=EDGE_CURVE('',#15563,#15562,#8838,.T.);
#19843=EDGE_CURVE('',#15564,#15563,#8839,.T.);
#19844=EDGE_CURVE('',#15565,#15564,#1880,.T.);
#19845=EDGE_CURVE('',#15566,#15565,#8840,.T.);
#19846=EDGE_CURVE('',#15560,#15566,#8841,.T.);
#19847=EDGE_CURVE('',#15567,#15560,#12559,.T.);
#19848=EDGE_CURVE('',#15567,#15568,#8842,.T.);
#19849=EDGE_CURVE('',#15568,#15561,#12560,.T.);
#19850=EDGE_CURVE('',#15569,#15570,#8843,.T.);
#19851=EDGE_CURVE('',#15570,#15568,#12561,.T.);
#19852=EDGE_CURVE('',#15569,#15567,#12562,.T.);
#19853=EDGE_CURVE('',#15571,#15569,#12563,.T.);
#19854=EDGE_CURVE('',#15571,#15572,#8844,.T.);
#19855=EDGE_CURVE('',#15572,#15570,#12564,.T.);
#19856=EDGE_CURVE('',#15573,#15571,#8845,.T.);
#19857=EDGE_CURVE('',#15574,#15573,#8846,.T.);
#19858=EDGE_CURVE('',#15574,#15572,#8847,.T.);
#19859=EDGE_CURVE('',#15575,#15576,#8848,.T.);
#19860=EDGE_CURVE('',#15575,#15574,#12565,.T.);
#19861=EDGE_CURVE('',#15576,#15573,#1881,.T.);
#19862=EDGE_CURVE('',#15577,#15563,#12566,.T.);
#19863=EDGE_CURVE('',#15562,#15578,#12567,.T.);
#19864=EDGE_CURVE('',#15577,#15578,#8849,.T.);
#19865=EDGE_CURVE('',#15579,#15580,#8850,.T.);
#19866=EDGE_CURVE('',#15580,#15562,#12568,.T.);
#19867=EDGE_CURVE('',#15579,#15561,#12569,.T.);
#19868=EDGE_CURVE('',#15579,#15568,#12570,.T.);
#19869=EDGE_CURVE('',#15581,#15579,#12571,.T.);
#19870=EDGE_CURVE('',#15581,#15570,#12572,.T.);
#19871=EDGE_CURVE('',#15581,#15572,#12573,.T.);
#19872=EDGE_CURVE('',#15582,#15581,#8851,.T.);
#19873=EDGE_CURVE('',#15582,#15574,#12574,.T.);
#19874=EDGE_CURVE('',#15583,#15582,#12575,.T.);
#19875=EDGE_CURVE('',#15583,#15575,#12576,.T.);
#19876=EDGE_CURVE('',#15584,#15585,#1882,.T.);
#19877=EDGE_CURVE('',#15584,#15583,#12577,.T.);
#19878=EDGE_CURVE('',#15585,#15575,#12578,.T.);
#19879=EDGE_CURVE('',#15580,#15578,#12579,.T.);
#19880=EDGE_CURVE('',#15586,#15587,#1883,.T.);
#19881=EDGE_CURVE('',#15578,#15587,#12580,.T.);
#19882=EDGE_CURVE('',#15580,#15586,#12581,.T.);
#19883=EDGE_CURVE('',#15588,#15589,#8852,.T.);
#19884=EDGE_CURVE('',#15590,#15588,#1884,.T.);
#19885=EDGE_CURVE('',#15590,#15591,#8853,.T.);
#19886=EDGE_CURVE('',#15589,#15591,#1885,.T.);
#19887=EDGE_CURVE('',#15591,#15592,#12582,.T.);
#19888=EDGE_CURVE('',#15593,#15592,#1886,.T.);
#19889=EDGE_CURVE('',#15594,#15593,#12583,.T.);
#19890=EDGE_CURVE('',#15594,#15591,#12584,.T.);
#19891=EDGE_CURVE('',#15592,#15595,#8854,.T.);
#19892=EDGE_CURVE('',#15595,#15596,#1887,.T.);
#19893=EDGE_CURVE('',#15597,#15596,#8855,.T.);
#19894=EDGE_CURVE('',#15597,#15592,#12585,.T.);
#19895=EDGE_CURVE('',#15598,#15599,#12586,.T.);
#19896=EDGE_CURVE('',#15595,#15598,#1888,.T.);
#19897=EDGE_CURVE('',#15595,#15590,#12587,.T.);
#19898=EDGE_CURVE('',#15590,#15599,#12588,.T.);
#19899=EDGE_CURVE('',#15599,#15588,#12589,.T.);
#19900=EDGE_CURVE('',#15600,#15601,#8856,.T.);
#19901=EDGE_CURVE('',#15588,#15600,#8857,.T.);
#19902=EDGE_CURVE('',#15601,#15589,#8858,.T.);
#19903=EDGE_CURVE('',#15594,#15589,#12590,.T.);
#19904=EDGE_CURVE('',#15602,#15603,#12591,.T.);
#19905=EDGE_CURVE('',#15602,#15594,#8859,.T.);
#19906=EDGE_CURVE('',#15603,#15593,#8860,.T.);
#19907=EDGE_CURVE('',#15597,#15593,#12592,.T.);
#19908=EDGE_CURVE('',#15604,#15597,#8861,.T.);
#19909=EDGE_CURVE('',#15596,#15605,#8862,.T.);
#19910=EDGE_CURVE('',#15604,#15605,#8863,.T.);
#19911=EDGE_CURVE('',#15596,#15598,#12593,.T.);
#19912=EDGE_CURVE('',#15598,#15606,#8864,.T.);
#19913=EDGE_CURVE('',#15599,#15607,#8865,.T.);
#19914=EDGE_CURVE('',#15606,#15607,#12594,.T.);
#19915=EDGE_CURVE('',#15607,#15600,#12595,.T.);
#19916=EDGE_CURVE('',#15601,#15608,#12596,.T.);
#19917=EDGE_CURVE('',#15609,#15608,#8866,.T.);
#19918=EDGE_CURVE('',#15600,#15609,#12597,.T.);
#19919=EDGE_CURVE('',#15601,#15602,#12598,.T.);
#19920=EDGE_CURVE('',#15603,#15610,#12599,.T.);
#19921=EDGE_CURVE('',#15611,#15610,#12600,.T.);
#19922=EDGE_CURVE('',#15602,#15611,#12601,.T.);
#19923=EDGE_CURVE('',#15603,#15604,#12602,.T.);
#19924=EDGE_CURVE('',#15605,#15612,#12603,.T.);
#19925=EDGE_CURVE('',#15613,#15612,#8867,.T.);
#19926=EDGE_CURVE('',#15604,#15613,#12604,.T.);
#19927=EDGE_CURVE('',#15605,#15606,#12605,.T.);
#19928=EDGE_CURVE('',#15607,#15614,#12606,.T.);
#19929=EDGE_CURVE('',#15615,#15614,#12607,.T.);
#19930=EDGE_CURVE('',#15606,#15615,#12608,.T.);
#19931=EDGE_CURVE('',#15614,#15609,#12609,.T.);
#19932=EDGE_CURVE('',#15616,#15617,#12610,.T.);
#19933=EDGE_CURVE('',#15617,#15618,#12611,.T.);
#19934=EDGE_CURVE('',#15616,#15618,#12612,.T.);
#19935=EDGE_CURVE('',#15608,#15611,#12613,.T.);
#19936=EDGE_CURVE('',#15610,#15613,#12614,.T.);
#19937=EDGE_CURVE('',#15612,#15615,#12615,.T.);
#19938=EDGE_CURVE('',#15619,#15620,#1889,.T.);
#19939=EDGE_CURVE('',#15621,#15619,#12616,.T.);
#19940=EDGE_CURVE('',#15621,#15622,#12617,.T.);
#19941=EDGE_CURVE('',#15622,#15620,#12618,.T.);
#19942=EDGE_CURVE('',#15623,#15565,#1890,.T.);
#19943=EDGE_CURVE('',#15624,#15564,#637,.T.);
#19944=EDGE_CURVE('',#15623,#15624,#1891,.T.);
#19945=EDGE_CURVE('',#15625,#15624,#12619,.T.);
#19946=EDGE_CURVE('',#15626,#15625,#12620,.T.);
#19947=EDGE_CURVE('',#15626,#15623,#12621,.T.);
#19948=EDGE_CURVE('',#15627,#15628,#8868,.T.);
#19949=EDGE_CURVE('',#15628,#15629,#8869,.T.);
#19950=EDGE_CURVE('',#15629,#15630,#8870,.T.);
#19951=EDGE_CURVE('',#15627,#15630,#8871,.T.);
#19952=EDGE_CURVE('',#15631,#15632,#12622,.T.);
#19953=EDGE_CURVE('',#15632,#15633,#8872,.T.);
#19954=EDGE_CURVE('',#15633,#15634,#1892,.T.);
#19955=EDGE_CURVE('',#15634,#15635,#12623,.T.);
#19956=EDGE_CURVE('',#15635,#15636,#1893,.T.);
#19957=EDGE_CURVE('',#15636,#15637,#8873,.T.);
#19958=EDGE_CURVE('',#15637,#15638,#12624,.T.);
#19959=EDGE_CURVE('',#15638,#15639,#8874,.T.);
#19960=EDGE_CURVE('',#15639,#15640,#638,.T.);
#19961=EDGE_CURVE('',#15640,#15641,#12625,.T.);
#19962=EDGE_CURVE('',#15641,#15577,#1894,.T.);
#19963=EDGE_CURVE('',#15587,#15631,#8875,.T.);
#19964=EDGE_CURVE('',#15642,#15643,#8876,.T.);
#19965=EDGE_CURVE('',#15643,#15644,#8877,.T.);
#19966=EDGE_CURVE('',#15644,#15645,#639,.T.);
#19967=EDGE_CURVE('',#15645,#15646,#8878,.T.);
#19968=EDGE_CURVE('',#15642,#15646,#8879,.T.);
#19969=EDGE_CURVE('',#15643,#15647,#12626,.T.);
#19970=EDGE_CURVE('',#15647,#15648,#8880,.T.);
#19971=EDGE_CURVE('',#15648,#15644,#1895,.T.);
#19972=EDGE_CURVE('',#15647,#15649,#8881,.T.);
#19973=EDGE_CURVE('',#15649,#15650,#8882,.T.);
#19974=EDGE_CURVE('',#15650,#15651,#640,.T.);
#19975=EDGE_CURVE('',#15651,#15652,#8883,.T.);
#19976=EDGE_CURVE('',#15652,#15648,#641,.T.);
#19977=EDGE_CURVE('',#15649,#15653,#12627,.T.);
#19978=EDGE_CURVE('',#15653,#15654,#8884,.T.);
#19979=EDGE_CURVE('',#15654,#15650,#1896,.T.);
#19980=EDGE_CURVE('',#15653,#15655,#8885,.T.);
#19981=EDGE_CURVE('',#15655,#15656,#8886,.T.);
#19982=EDGE_CURVE('',#15656,#15657,#8887,.T.);
#19983=EDGE_CURVE('',#15657,#15658,#1897,.T.);
#19984=EDGE_CURVE('',#15658,#15654,#642,.T.);
#19985=EDGE_CURVE('',#15655,#15627,#12628,.T.);
#19986=EDGE_CURVE('',#15630,#15656,#12629,.T.);
#19987=EDGE_CURVE('',#15545,#15659,#12630,.T.);
#19988=EDGE_CURVE('',#15544,#15659,#12631,.T.);
#19989=EDGE_CURVE('',#15559,#15660,#12632,.T.);
#19990=EDGE_CURVE('',#15659,#15660,#12633,.T.);
#19991=EDGE_CURVE('',#15661,#15544,#8888,.T.);
#19992=EDGE_CURVE('',#15662,#15659,#8889,.T.);
#19993=EDGE_CURVE('',#15661,#15662,#643,.T.);
#19994=EDGE_CURVE('',#15663,#15661,#8890,.T.);
#19995=EDGE_CURVE('',#15664,#15663,#12634,.T.);
#19996=EDGE_CURVE('',#15665,#15664,#8891,.T.);
#19997=EDGE_CURVE('',#15666,#15665,#8892,.T.);
#19998=EDGE_CURVE('',#15666,#15667,#8893,.T.);
#19999=EDGE_CURVE('',#15514,#15667,#8894,.T.);
#20000=EDGE_CURVE('',#15668,#15666,#12635,.T.);
#20001=EDGE_CURVE('',#15668,#15669,#8895,.T.);
#20002=EDGE_CURVE('',#15667,#15669,#12636,.T.);
#20003=EDGE_CURVE('',#15669,#15670,#12637,.T.);
#20004=EDGE_CURVE('',#15671,#15668,#12638,.T.);
#20005=EDGE_CURVE('',#15671,#15670,#8896,.T.);
#20006=EDGE_CURVE('',#15672,#15671,#12639,.T.);
#20007=EDGE_CURVE('',#15672,#15673,#8897,.T.);
#20008=EDGE_CURVE('',#15670,#15673,#12640,.T.);
#20009=EDGE_CURVE('',#15673,#15674,#8898,.T.);
#20010=EDGE_CURVE('',#15675,#15672,#8899,.T.);
#20011=EDGE_CURVE('',#15675,#15674,#8900,.T.);
#20012=EDGE_CURVE('',#15676,#15677,#8901,.T.);
#20013=EDGE_CURVE('',#15665,#15676,#12641,.T.);
#20014=EDGE_CURVE('',#15677,#15664,#1898,.T.);
#20015=EDGE_CURVE('',#15678,#15675,#12642,.T.);
#20016=EDGE_CURVE('',#15678,#15679,#8902,.T.);
#20017=EDGE_CURVE('',#15674,#15679,#12643,.T.);
#20018=EDGE_CURVE('',#15676,#15678,#12644,.T.);
#20019=EDGE_CURVE('',#15679,#15677,#12645,.T.);
#20020=EDGE_CURVE('',#15680,#15681,#8903,.T.);
#20021=EDGE_CURVE('',#15681,#15682,#12646,.T.);
#20022=EDGE_CURVE('',#15622,#15682,#8904,.T.);
#20023=EDGE_CURVE('',#15680,#15622,#12647,.T.);
#20024=EDGE_CURVE('',#15683,#15684,#12648,.T.);
#20025=EDGE_CURVE('',#15684,#15685,#12649,.T.);
#20026=EDGE_CURVE('',#15686,#15685,#12650,.T.);
#20027=EDGE_CURVE('',#15683,#15686,#12651,.T.);
#20028=EDGE_CURVE('',#15687,#15683,#12652,.T.);
#20029=EDGE_CURVE('',#15688,#15686,#12653,.T.);
#20030=EDGE_CURVE('',#15687,#15688,#12654,.T.);
#20031=EDGE_CURVE('',#15689,#15687,#8905,.T.);
#20032=EDGE_CURVE('',#15690,#15688,#8906,.T.);
#20033=EDGE_CURVE('',#15689,#15690,#12655,.T.);
#20034=EDGE_CURVE('',#15691,#15689,#12656,.T.);
#20035=EDGE_CURVE('',#15692,#15690,#12657,.T.);
#20036=EDGE_CURVE('',#15691,#15692,#12658,.T.);
#20037=EDGE_CURVE('',#15693,#15691,#12659,.T.);
#20038=EDGE_CURVE('',#15694,#15692,#12660,.T.);
#20039=EDGE_CURVE('',#15693,#15694,#12661,.T.);
#20040=EDGE_CURVE('',#15684,#15695,#12662,.T.);
#20041=EDGE_CURVE('',#15695,#15696,#12663,.T.);
#20042=EDGE_CURVE('',#15685,#15696,#12664,.T.);
#20043=EDGE_CURVE('',#15697,#15693,#12665,.T.);
#20044=EDGE_CURVE('',#15698,#15694,#12666,.T.);
#20045=EDGE_CURVE('',#15697,#15698,#12667,.T.);
#20046=EDGE_CURVE('',#15695,#15697,#8907,.T.);
#20047=EDGE_CURVE('',#15696,#15698,#8908,.T.);
#20048=EDGE_CURVE('',#15699,#15700,#12668,.T.);
#20049=EDGE_CURVE('',#15700,#15701,#12669,.T.);
#20050=EDGE_CURVE('',#15702,#15701,#12670,.T.);
#20051=EDGE_CURVE('',#15699,#15702,#12671,.T.);
#20052=EDGE_CURVE('',#15657,#15703,#644,.T.);
#20053=EDGE_CURVE('',#15703,#15704,#1899,.T.);
#20054=EDGE_CURVE('',#15658,#15704,#645,.T.);
#20055=EDGE_CURVE('',#15701,#15703,#12672,.T.);
#20056=EDGE_CURVE('',#15700,#15705,#12673,.T.);
#20057=EDGE_CURVE('',#15705,#15704,#12674,.T.);
#20058=EDGE_CURVE('',#15650,#15706,#646,.T.);
#20059=EDGE_CURVE('',#15706,#15707,#647,.T.);
#20060=EDGE_CURVE('',#15651,#15707,#648,.T.);
#20061=EDGE_CURVE('',#15654,#15708,#649,.T.);
#20062=EDGE_CURVE('',#15708,#15706,#1900,.T.);
#20063=EDGE_CURVE('',#15704,#15708,#650,.T.);
#20064=EDGE_CURVE('',#15705,#15709,#12675,.T.);
#20065=EDGE_CURVE('',#15709,#15710,#12676,.T.);
#20066=EDGE_CURVE('',#15707,#15710,#12677,.T.);
#20067=EDGE_CURVE('',#15711,#15699,#12678,.T.);
#20068=EDGE_CURVE('',#15712,#15702,#12679,.T.);
#20069=EDGE_CURVE('',#15711,#15712,#12680,.T.);
#20070=EDGE_CURVE('',#15709,#15713,#12681,.T.);
#20071=EDGE_CURVE('',#15713,#15714,#12682,.T.);
#20072=EDGE_CURVE('',#15710,#15714,#12683,.T.);
#20073=EDGE_CURVE('',#15713,#15711,#8909,.T.);
#20074=EDGE_CURVE('',#15714,#15712,#8910,.T.);
#20075=EDGE_CURVE('',#15644,#15715,#651,.T.);
#20076=EDGE_CURVE('',#15715,#15716,#652,.T.);
#20077=EDGE_CURVE('',#15645,#15716,#653,.T.);
#20078=EDGE_CURVE('',#15648,#15717,#654,.T.);
#20079=EDGE_CURVE('',#15717,#15715,#1901,.T.);
#20080=EDGE_CURVE('',#15652,#15718,#655,.T.);
#20081=EDGE_CURVE('',#15718,#15717,#656,.T.);
#20082=EDGE_CURVE('',#15718,#15719,#12684,.T.);
#20083=EDGE_CURVE('',#15719,#15720,#12685,.T.);
#20084=EDGE_CURVE('',#15721,#15720,#12686,.T.);
#20085=EDGE_CURVE('',#15722,#15721,#12687,.T.);
#20086=EDGE_CURVE('',#15722,#15716,#12688,.T.);
#20087=EDGE_CURVE('',#15723,#15722,#12689,.T.);
#20088=EDGE_CURVE('',#15724,#15721,#12690,.T.);
#20089=EDGE_CURVE('',#15723,#15724,#12691,.T.);
#20090=EDGE_CURVE('',#15725,#15723,#8911,.T.);
#20091=EDGE_CURVE('',#15726,#15724,#8912,.T.);
#20092=EDGE_CURVE('',#15725,#15726,#12692,.T.);
#20093=EDGE_CURVE('',#15727,#15725,#12693,.T.);
#20094=EDGE_CURVE('',#15728,#15726,#12694,.T.);
#20095=EDGE_CURVE('',#15727,#15728,#12695,.T.);
#20096=EDGE_CURVE('',#15729,#15727,#12696,.T.);
#20097=EDGE_CURVE('',#15730,#15728,#12697,.T.);
#20098=EDGE_CURVE('',#15729,#15730,#12698,.T.);
#20099=EDGE_CURVE('',#15719,#15731,#12699,.T.);
#20100=EDGE_CURVE('',#15731,#15732,#12700,.T.);
#20101=EDGE_CURVE('',#15720,#15732,#12701,.T.);
#20102=EDGE_CURVE('',#15733,#15729,#12702,.T.);
#20103=EDGE_CURVE('',#15734,#15730,#12703,.T.);
#20104=EDGE_CURVE('',#15733,#15734,#12704,.T.);
#20105=EDGE_CURVE('',#15731,#15733,#8913,.T.);
#20106=EDGE_CURVE('',#15732,#15734,#8914,.T.);
#20107=EDGE_CURVE('',#15735,#15736,#8915,.T.);
#20108=EDGE_CURVE('',#15736,#15737,#12705,.T.);
#20109=EDGE_CURVE('',#15738,#15737,#8916,.T.);
#20110=EDGE_CURVE('',#15735,#15738,#1902,.T.);
#20111=EDGE_CURVE('',#15618,#15739,#8917,.T.);
#20112=EDGE_CURVE('',#15740,#15739,#1903,.T.);
#20113=EDGE_CURVE('',#15616,#15740,#8918,.T.);
#20114=EDGE_CURVE('',#15741,#15742,#12706,.T.);
#20115=EDGE_CURVE('',#15743,#15741,#1904,.T.);
#20116=EDGE_CURVE('',#15743,#15744,#12707,.T.);
#20117=EDGE_CURVE('',#15744,#15742,#12708,.T.);
#20118=EDGE_CURVE('',#15745,#15743,#12709,.T.);
#20119=EDGE_CURVE('',#15745,#15741,#12710,.T.);
#20120=EDGE_CURVE('',#15746,#15745,#12711,.T.);
#20121=EDGE_CURVE('',#15747,#15741,#12712,.T.);
#20122=EDGE_CURVE('',#15746,#15747,#1905,.T.);
#20123=EDGE_CURVE('',#15744,#15748,#12713,.T.);
#20124=EDGE_CURVE('',#15748,#15742,#12714,.T.);
#20125=EDGE_CURVE('',#15749,#15746,#12715,.T.);
#20126=EDGE_CURVE('',#15749,#15747,#12716,.T.);
#20127=EDGE_CURVE('',#15750,#15738,#12717,.T.);
#20128=EDGE_CURVE('',#15735,#15750,#12718,.T.);
#20129=EDGE_CURVE('',#15748,#15749,#8919,.T.);
#20130=EDGE_CURVE('',#15742,#15747,#8920,.T.);
#20131=EDGE_CURVE('',#15751,#15735,#12719,.T.);
#20132=EDGE_CURVE('',#15752,#15750,#12720,.T.);
#20133=EDGE_CURVE('',#15752,#15751,#12721,.T.);
#20134=EDGE_CURVE('',#15681,#15753,#12722,.T.);
#20135=EDGE_CURVE('',#15753,#15754,#12723,.T.);
#20136=EDGE_CURVE('',#15682,#15754,#12724,.T.);
#20137=EDGE_CURVE('',#15753,#15755,#12725,.T.);
#20138=EDGE_CURVE('',#15755,#15756,#12726,.T.);
#20139=EDGE_CURVE('',#15754,#15756,#12727,.T.);
#20140=EDGE_CURVE('',#15757,#15626,#12728,.T.);
#20141=EDGE_CURVE('',#15758,#15625,#12729,.T.);
#20142=EDGE_CURVE('',#15757,#15758,#12730,.T.);
#20143=EDGE_CURVE('',#15755,#15759,#12731,.T.);
#20144=EDGE_CURVE('',#15759,#15760,#12732,.T.);
#20145=EDGE_CURVE('',#15756,#15760,#12733,.T.);
#20146=EDGE_CURVE('',#15761,#15740,#12734,.T.);
#20147=EDGE_CURVE('',#15761,#15739,#12735,.T.);
#20148=EDGE_CURVE('',#15762,#15763,#12736,.T.);
#20149=EDGE_CURVE('',#15763,#15621,#8921,.T.);
#20150=EDGE_CURVE('',#15762,#15619,#8922,.T.);
#20151=EDGE_CURVE('',#15621,#15680,#12737,.T.);
#20152=EDGE_CURVE('',#15764,#15765,#12738,.T.);
#20153=EDGE_CURVE('',#15765,#15763,#1906,.T.);
#20154=EDGE_CURVE('',#15764,#15762,#1907,.T.);
#20155=EDGE_CURVE('',#15766,#15767,#8923,.T.);
#20156=EDGE_CURVE('',#15768,#15766,#12739,.T.);
#20157=EDGE_CURVE('',#15768,#15769,#8924,.T.);
#20158=EDGE_CURVE('',#15767,#15769,#12740,.T.);
#20159=EDGE_CURVE('',#15739,#15770,#12741,.T.);
#20160=EDGE_CURVE('',#15771,#15770,#1908,.T.);
#20161=EDGE_CURVE('',#15761,#15771,#12742,.T.);
#20162=EDGE_CURVE('',#15772,#15773,#12743,.T.);
#20163=EDGE_CURVE('',#15772,#15773,#12744,.T.);
#20164=EDGE_CURVE('',#15774,#15775,#12745,.T.);
#20165=EDGE_CURVE('',#15775,#15638,#12746,.T.);
#20166=EDGE_CURVE('',#15774,#15637,#12747,.T.);
#20167=EDGE_CURVE('',#15776,#15777,#12748,.T.);
#20168=EDGE_CURVE('',#15777,#15778,#12749,.T.);
#20169=EDGE_CURVE('',#15779,#15778,#12750,.T.);
#20170=EDGE_CURVE('',#15776,#15779,#12751,.T.);
#20171=EDGE_CURVE('',#15631,#15780,#1909,.T.);
#20172=EDGE_CURVE('',#15780,#15781,#12752,.T.);
#20173=EDGE_CURVE('',#15781,#15632,#12753,.T.);
#20174=EDGE_CURVE('',#15782,#15774,#1910,.T.);
#20175=EDGE_CURVE('',#15782,#15783,#12754,.T.);
#20176=EDGE_CURVE('',#15783,#15781,#12755,.T.);
#20177=EDGE_CURVE('',#15774,#15781,#12756,.T.);
#20178=EDGE_CURVE('',#15542,#15784,#12757,.T.);
#20179=EDGE_CURVE('',#15785,#15784,#8925,.T.);
#20180=EDGE_CURVE('',#15541,#15785,#12758,.T.);
#20181=EDGE_CURVE('',#15558,#15785,#12759,.T.);
#20182=EDGE_CURVE('',#15660,#15785,#12760,.T.);
#20183=EDGE_CURVE('',#15775,#15776,#12761,.T.);
#20184=EDGE_CURVE('',#15638,#15779,#12762,.T.);
#20185=EDGE_CURVE('',#15779,#15660,#8926,.T.);
#20186=EDGE_CURVE('',#15784,#15639,#1911,.T.);
#20187=EDGE_CURVE('',#15786,#15772,#1912,.T.);
#20188=EDGE_CURVE('',#15772,#15634,#657,.T.);
#20189=EDGE_CURVE('',#15786,#15633,#658,.T.);
#20190=EDGE_CURVE('',#15773,#15635,#12763,.T.);
#20191=EDGE_CURVE('',#15773,#15787,#1913,.T.);
#20192=EDGE_CURVE('',#15787,#15636,#659,.T.);
#20193=EDGE_CURVE('',#15782,#15637,#12764,.T.);
#20194=EDGE_CURVE('',#15787,#15782,#8927,.T.);
#20195=EDGE_CURVE('',#15783,#15786,#8928,.T.);
#20196=EDGE_CURVE('',#15783,#15632,#12765,.T.);
#20197=EDGE_CURVE('',#15777,#15788,#12766,.T.);
#20198=EDGE_CURVE('',#15788,#15778,#12767,.T.);
#20199=EDGE_CURVE('',#15789,#15777,#12768,.T.);
#20200=EDGE_CURVE('',#15790,#15777,#8929,.T.);
#20201=EDGE_CURVE('',#15769,#15790,#12769,.T.);
#20202=EDGE_CURVE('',#15769,#15788,#8930,.T.);
#20203=EDGE_CURVE('',#15788,#15791,#8931,.T.);
#20204=EDGE_CURVE('',#15791,#15792,#12770,.T.);
#20205=EDGE_CURVE('',#15778,#15792,#8932,.T.);
#20206=EDGE_CURVE('',#15791,#15768,#8933,.T.);
#20207=EDGE_CURVE('',#15791,#15793,#1914,.T.);
#20208=EDGE_CURVE('',#15793,#15794,#660,.T.);
#20209=EDGE_CURVE('',#15792,#15794,#1915,.T.);
#20210=EDGE_CURVE('',#15795,#15768,#12771,.T.);
#20211=EDGE_CURVE('',#15796,#15795,#661,.T.);
#20212=EDGE_CURVE('',#15796,#15797,#8934,.T.);
#20213=EDGE_CURVE('',#15798,#15797,#1916,.T.);
#20214=EDGE_CURVE('',#15798,#15793,#8935,.T.);
#20215=EDGE_CURVE('',#15799,#15666,#12772,.T.);
#20216=EDGE_CURVE('',#15800,#15665,#12773,.T.);
#20217=EDGE_CURVE('',#15799,#15800,#8936,.T.);
#20218=EDGE_CURVE('',#15799,#15668,#12774,.T.);
#20219=EDGE_CURVE('',#15801,#15671,#12775,.T.);
#20220=EDGE_CURVE('',#15796,#15799,#12776,.T.);
#20221=EDGE_CURVE('',#15795,#15802,#1917,.T.);
#20222=EDGE_CURVE('',#15802,#15803,#1918,.T.);
#20223=EDGE_CURVE('',#15803,#15801,#12777,.T.);
#20224=EDGE_CURVE('',#15801,#15804,#12778,.T.);
#20225=EDGE_CURVE('',#15804,#15672,#12779,.T.);
#20226=EDGE_CURVE('',#15804,#15805,#8937,.T.);
#20227=EDGE_CURVE('',#15805,#15675,#12780,.T.);
#20228=EDGE_CURVE('',#15800,#15676,#12781,.T.);
#20229=EDGE_CURVE('',#15805,#15806,#12782,.T.);
#20230=EDGE_CURVE('',#15806,#15678,#12783,.T.);
#20231=EDGE_CURVE('',#15800,#15797,#12784,.T.);
#20232=EDGE_CURVE('',#15806,#15798,#12785,.T.);
#20233=EDGE_CURVE('',#15766,#15802,#12786,.T.);
#20234=EDGE_CURVE('',#15807,#15680,#8938,.T.);
#20235=EDGE_CURVE('',#15807,#15808,#8939,.T.);
#20236=EDGE_CURVE('',#15681,#15808,#8940,.T.);
#20237=EDGE_CURVE('',#15685,#15761,#8941,.T.);
#20238=EDGE_CURVE('',#15686,#15771,#8942,.T.);
#20239=EDGE_CURVE('',#15809,#15771,#12787,.T.);
#20240=EDGE_CURVE('',#15688,#15809,#8943,.T.);
#20241=EDGE_CURVE('',#15809,#15810,#8944,.T.);
#20242=EDGE_CURVE('',#15810,#15690,#8945,.T.);
#20243=EDGE_CURVE('',#15810,#15811,#12788,.T.);
#20244=EDGE_CURVE('',#15811,#15692,#8946,.T.);
#20245=EDGE_CURVE('',#15811,#15617,#12789,.T.);
#20246=EDGE_CURVE('',#15694,#15617,#8947,.T.);
#20247=EDGE_CURVE('',#15696,#15740,#8948,.T.);
#20248=EDGE_CURVE('',#15698,#15616,#8949,.T.);
#20249=EDGE_CURVE('',#15699,#15744,#8950,.T.);
#20250=EDGE_CURVE('',#15700,#15743,#8951,.T.);
#20251=EDGE_CURVE('',#15705,#15745,#8952,.T.);
#20252=EDGE_CURVE('',#15709,#15746,#8953,.T.);
#20253=EDGE_CURVE('',#15711,#15748,#8954,.T.);
#20254=EDGE_CURVE('',#15713,#15749,#8955,.T.);
#20255=EDGE_CURVE('',#15720,#15752,#8956,.T.);
#20256=EDGE_CURVE('',#15750,#15721,#8957,.T.);
#20257=EDGE_CURVE('',#15738,#15724,#8958,.T.);
#20258=EDGE_CURVE('',#15737,#15726,#8959,.T.);
#20259=EDGE_CURVE('',#15737,#15812,#12790,.T.);
#20260=EDGE_CURVE('',#15812,#15728,#8960,.T.);
#20261=EDGE_CURVE('',#15812,#15813,#12791,.T.);
#20262=EDGE_CURVE('',#15813,#15730,#8961,.T.);
#20263=EDGE_CURVE('',#15732,#15814,#8962,.T.);
#20264=EDGE_CURVE('',#15752,#15814,#12792,.T.);
#20265=EDGE_CURVE('',#15813,#15815,#12793,.T.);
#20266=EDGE_CURVE('',#15815,#15734,#8963,.T.);
#20267=EDGE_CURVE('',#15815,#15814,#8964,.T.);
#20268=EDGE_CURVE('',#15736,#15812,#12794,.T.);
#20269=EDGE_CURVE('',#15736,#15816,#12795,.T.);
#20270=EDGE_CURVE('',#15816,#15813,#1919,.T.);
#20271=EDGE_CURVE('',#15814,#15751,#12796,.T.);
#20272=EDGE_CURVE('',#15816,#15815,#12797,.T.);
#20273=EDGE_CURVE('',#15816,#15751,#8965,.T.);
#20274=EDGE_CURVE('',#15770,#15817,#8966,.T.);
#20275=EDGE_CURVE('',#15817,#15618,#12798,.T.);
#20276=EDGE_CURVE('',#15818,#15808,#12799,.T.);
#20277=EDGE_CURVE('',#15808,#15819,#12800,.T.);
#20278=EDGE_CURVE('',#15818,#15819,#12801,.T.);
#20279=EDGE_CURVE('',#15753,#15818,#8967,.T.);
#20280=EDGE_CURVE('',#15786,#15787,#12802,.T.);
#20281=EDGE_CURVE('',#15809,#15770,#12803,.T.);
#20282=EDGE_CURVE('',#15817,#15811,#1920,.T.);
#20283=EDGE_CURVE('',#15807,#15763,#662,.T.);
#20284=EDGE_CURVE('',#15765,#15807,#1921,.T.);
#20285=EDGE_CURVE('',#15817,#15810,#1922,.T.);
#20286=EDGE_CURVE('',#15765,#15819,#8968,.T.);
#20287=EDGE_CURVE('',#15820,#15790,#12804,.T.);
#20288=EDGE_CURVE('',#15767,#15820,#12805,.T.);
#20289=EDGE_CURVE('',#15821,#15822,#12806,.T.);
#20290=EDGE_CURVE('',#15822,#15823,#12807,.T.);
#20291=EDGE_CURVE('',#15821,#15823,#12808,.T.);
#20292=EDGE_CURVE('',#15755,#15822,#8969,.T.);
#20293=EDGE_CURVE('',#15759,#15821,#8970,.T.);
#20294=EDGE_CURVE('',#15818,#15822,#12809,.T.);
#20295=EDGE_CURVE('',#15819,#15823,#12810,.T.);
#20296=EDGE_CURVE('',#15824,#15560,#12811,.T.);
#20297=EDGE_CURVE('',#15825,#15566,#12812,.T.);
#20298=EDGE_CURVE('',#15824,#15825,#8971,.T.);
#20299=EDGE_CURVE('',#15826,#15567,#12813,.T.);
#20300=EDGE_CURVE('',#15826,#15824,#12814,.T.);
#20301=EDGE_CURVE('',#15827,#15569,#12815,.T.);
#20302=EDGE_CURVE('',#15827,#15826,#12816,.T.);
#20303=EDGE_CURVE('',#15828,#15571,#12817,.T.);
#20304=EDGE_CURVE('',#15828,#15827,#12818,.T.);
#20305=EDGE_CURVE('',#15829,#15573,#12819,.T.);
#20306=EDGE_CURVE('',#15829,#15828,#8972,.T.);
#20307=EDGE_CURVE('',#15830,#15566,#12820,.T.);
#20308=EDGE_CURVE('',#15825,#15830,#12821,.T.);
#20309=EDGE_CURVE('',#15825,#15831,#12822,.T.);
#20310=EDGE_CURVE('',#15830,#15832,#12823,.T.);
#20311=EDGE_CURVE('',#15833,#15832,#1923,.T.);
#20312=EDGE_CURVE('',#15825,#15833,#12824,.T.);
#20313=EDGE_CURVE('',#15576,#15829,#12825,.T.);
#20314=EDGE_CURVE('',#15834,#15576,#12826,.T.);
#20315=EDGE_CURVE('',#15835,#15829,#12827,.T.);
#20316=EDGE_CURVE('',#15834,#15835,#1924,.T.);
#20317=EDGE_CURVE('',#15830,#15623,#8973,.T.);
#20318=EDGE_CURVE('',#15832,#15626,#8974,.T.);
#20319=EDGE_CURVE('',#15585,#15834,#8975,.T.);
#20320=EDGE_CURVE('',#15836,#15757,#8976,.T.);
#20321=EDGE_CURVE('',#15836,#15832,#12828,.T.);
#20322=EDGE_CURVE('',#15833,#15836,#12829,.T.);
#20323=EDGE_CURVE('',#15821,#15836,#8977,.T.);
#20324=EDGE_CURVE('',#15823,#15833,#8978,.T.);
#20325=EDGE_CURVE('',#15759,#15757,#8979,.T.);
#20326=EDGE_CURVE('',#15760,#15758,#8980,.T.);
#20327=EDGE_CURVE('',#15837,#15513,#663,.T.);
#20328=EDGE_CURVE('',#15837,#15514,#1925,.T.);
#20329=EDGE_CURVE('',#15667,#15838,#12830,.T.);
#20330=EDGE_CURVE('',#15837,#15838,#8981,.T.);
#20331=EDGE_CURVE('',#15669,#15839,#12831,.T.);
#20332=EDGE_CURVE('',#15838,#15839,#12832,.T.);
#20333=EDGE_CURVE('',#15670,#15840,#12833,.T.);
#20334=EDGE_CURVE('',#15839,#15840,#12834,.T.);
#20335=EDGE_CURVE('',#15673,#15841,#12835,.T.);
#20336=EDGE_CURVE('',#15840,#15841,#12836,.T.);
#20337=EDGE_CURVE('',#15674,#15842,#12837,.T.);
#20338=EDGE_CURVE('',#15841,#15842,#8982,.T.);
#20339=EDGE_CURVE('',#15843,#15663,#12838,.T.);
#20340=EDGE_CURVE('',#15677,#15843,#1926,.T.);
#20341=EDGE_CURVE('',#15844,#15843,#12839,.T.);
#20342=EDGE_CURVE('',#15677,#15844,#12840,.T.);
#20343=EDGE_CURVE('',#15679,#15845,#12841,.T.);
#20344=EDGE_CURVE('',#15842,#15845,#12842,.T.);
#20345=EDGE_CURVE('',#15845,#15844,#12843,.T.);
#20346=EDGE_CURVE('',#15846,#15515,#12844,.T.);
#20347=EDGE_CURVE('',#15846,#15837,#12845,.T.);
#20348=EDGE_CURVE('',#15847,#15520,#12846,.T.);
#20349=EDGE_CURVE('',#15847,#15846,#12847,.T.);
#20350=EDGE_CURVE('',#15848,#15849,#664,.T.);
#20351=EDGE_CURVE('',#15849,#15640,#665,.T.);
#20352=EDGE_CURVE('',#15848,#15639,#666,.T.);
#20353=EDGE_CURVE('',#15542,#15848,#1927,.T.);
#20354=EDGE_CURVE('',#15543,#15850,#12848,.T.);
#20355=EDGE_CURVE('',#15850,#15849,#8983,.T.);
#20356=EDGE_CURVE('',#15851,#15563,#1928,.T.);
#20357=EDGE_CURVE('',#15851,#15641,#667,.T.);
#20358=EDGE_CURVE('',#15624,#15851,#8984,.T.);
#20359=EDGE_CURVE('',#15852,#15661,#1929,.T.);
#20360=EDGE_CURVE('',#15853,#15662,#1930,.T.);
#20361=EDGE_CURVE('',#15852,#15853,#668,.T.);
#20362=EDGE_CURVE('',#15843,#15852,#8985,.T.);
#20363=EDGE_CURVE('',#15849,#15851,#12849,.T.);
#20364=EDGE_CURVE('',#15854,#15524,#1931,.T.);
#20365=EDGE_CURVE('',#15855,#15526,#1932,.T.);
#20366=EDGE_CURVE('',#15855,#15854,#12850,.T.);
#20367=EDGE_CURVE('',#15538,#15856,#669,.T.);
#20368=EDGE_CURVE('',#15856,#15857,#1933,.T.);
#20369=EDGE_CURVE('',#15539,#15857,#1934,.T.);
#20370=EDGE_CURVE('',#15857,#15850,#12851,.T.);
#20371=EDGE_CURVE('',#15856,#15858,#12852,.T.);
#20372=EDGE_CURVE('',#15858,#15859,#12853,.T.);
#20373=EDGE_CURVE('',#15850,#15859,#12854,.T.);
#20374=EDGE_CURVE('',#15858,#15860,#12855,.T.);
#20375=EDGE_CURVE('',#15860,#15861,#12856,.T.);
#20376=EDGE_CURVE('',#15859,#15861,#12857,.T.);
#20377=EDGE_CURVE('',#15860,#15862,#8986,.T.);
#20378=EDGE_CURVE('',#15862,#15863,#12858,.T.);
#20379=EDGE_CURVE('',#15861,#15863,#8987,.T.);
#20380=EDGE_CURVE('',#15862,#15864,#12859,.T.);
#20381=EDGE_CURVE('',#15864,#15865,#12860,.T.);
#20382=EDGE_CURVE('',#15863,#15865,#12861,.T.);
#20383=EDGE_CURVE('',#15864,#15866,#12862,.T.);
#20384=EDGE_CURVE('',#15866,#15867,#12863,.T.);
#20385=EDGE_CURVE('',#15865,#15867,#12864,.T.);
#20386=EDGE_CURVE('',#15866,#15868,#12865,.T.);
#20387=EDGE_CURVE('',#15868,#15869,#12866,.T.);
#20388=EDGE_CURVE('',#15867,#15869,#12867,.T.);
#20389=EDGE_CURVE('',#15870,#15518,#670,.T.);
#20390=EDGE_CURVE('',#15870,#15847,#671,.T.);
#20391=EDGE_CURVE('',#15521,#15870,#1935,.T.);
#20392=EDGE_CURVE('',#15869,#15847,#8988,.T.);
#20393=EDGE_CURVE('',#15868,#15521,#8989,.T.);
#20394=EDGE_CURVE('',#15551,#15871,#8990,.T.);
#20395=EDGE_CURVE('',#15871,#15872,#12868,.T.);
#20396=EDGE_CURVE('',#15872,#15855,#8991,.T.);
#20397=EDGE_CURVE('',#15872,#15873,#12869,.T.);
#20398=EDGE_CURVE('',#15873,#15854,#8992,.T.);
#20399=EDGE_CURVE('',#15873,#15530,#12870,.T.);
#20400=EDGE_CURVE('',#15537,#15874,#12871,.T.);
#20401=EDGE_CURVE('',#15874,#15856,#8993,.T.);
#20402=EDGE_CURVE('',#15874,#15875,#12872,.T.);
#20403=EDGE_CURVE('',#15858,#15875,#8994,.T.);
#20404=EDGE_CURVE('',#15876,#15875,#12873,.T.);
#20405=EDGE_CURVE('',#15860,#15876,#8995,.T.);
#20406=EDGE_CURVE('',#15876,#15877,#8996,.T.);
#20407=EDGE_CURVE('',#15862,#15877,#8997,.T.);
#20408=EDGE_CURVE('',#15878,#15877,#12874,.T.);
#20409=EDGE_CURVE('',#15864,#15878,#8998,.T.);
#20410=EDGE_CURVE('',#15878,#15879,#12875,.T.);
#20411=EDGE_CURVE('',#15866,#15879,#8999,.T.);
#20412=EDGE_CURVE('',#15880,#15879,#12876,.T.);
#20413=EDGE_CURVE('',#15868,#15880,#9000,.T.);
#20414=EDGE_CURVE('',#15880,#15881,#9001,.T.);
#20415=EDGE_CURVE('',#15549,#15881,#9002,.T.);
#20416=EDGE_CURVE('',#15881,#15871,#12877,.T.);
#20417=EDGE_CURVE('',#15882,#15871,#12878,.T.);
#20418=EDGE_CURVE('',#15882,#15881,#12879,.T.);
#20419=EDGE_CURVE('',#15882,#15883,#12880,.T.);
#20420=EDGE_CURVE('',#15872,#15883,#12881,.T.);
#20421=EDGE_CURVE('',#15883,#15884,#12882,.T.);
#20422=EDGE_CURVE('',#15873,#15884,#12883,.T.);
#20423=EDGE_CURVE('',#15530,#15885,#12884,.T.);
#20424=EDGE_CURVE('',#15528,#15885,#12885,.T.);
#20425=EDGE_CURVE('',#15884,#15885,#12886,.T.);
#20426=EDGE_CURVE('',#15537,#15886,#12887,.T.);
#20427=EDGE_CURVE('',#15886,#15874,#12888,.T.);
#20428=EDGE_CURVE('',#15886,#15887,#12889,.T.);
#20429=EDGE_CURVE('',#15875,#15887,#1936,.T.);
#20430=EDGE_CURVE('',#15876,#15887,#12890,.T.);
#20431=EDGE_CURVE('',#15887,#15888,#9003,.T.);
#20432=EDGE_CURVE('',#15877,#15888,#1937,.T.);
#20433=EDGE_CURVE('',#15878,#15888,#12891,.T.);
#20434=EDGE_CURVE('',#15888,#15889,#12892,.T.);
#20435=EDGE_CURVE('',#15879,#15889,#1938,.T.);
#20436=EDGE_CURVE('',#15880,#15889,#12893,.T.);
#20437=EDGE_CURVE('',#15889,#15882,#9004,.T.);
#20438=EDGE_CURVE('',#15885,#15890,#9005,.T.);
#20439=EDGE_CURVE('',#15531,#15890,#12894,.T.);
#20440=EDGE_CURVE('',#15890,#15891,#12895,.T.);
#20441=EDGE_CURVE('',#15533,#15891,#12896,.T.);
#20442=EDGE_CURVE('',#15891,#15892,#12897,.T.);
#20443=EDGE_CURVE('',#15535,#15892,#12898,.T.);
#20444=EDGE_CURVE('',#15892,#15886,#12899,.T.);
#20445=EDGE_CURVE('',#15893,#15894,#9006,.T.);
#20446=EDGE_CURVE('',#15895,#15894,#12900,.T.);
#20447=EDGE_CURVE('',#15896,#15895,#9007,.T.);
#20448=EDGE_CURVE('',#15896,#15897,#12901,.T.);
#20449=EDGE_CURVE('',#15897,#15893,#1939,.T.);
#20450=EDGE_CURVE('',#15898,#15899,#672,.T.);
#20451=EDGE_CURVE('',#15899,#15896,#12902,.T.);
#20452=EDGE_CURVE('',#15900,#15895,#12903,.T.);
#20453=EDGE_CURVE('',#15898,#15900,#9008,.T.);
#20454=EDGE_CURVE('',#15901,#15900,#12904,.T.);
#20455=EDGE_CURVE('',#15902,#15901,#9009,.T.);
#20456=EDGE_CURVE('',#15902,#15898,#1940,.T.);
#20457=EDGE_CURVE('',#15903,#15904,#1941,.T.);
#20458=EDGE_CURVE('',#15905,#15903,#9010,.T.);
#20459=EDGE_CURVE('',#15906,#15905,#12905,.T.);
#20460=EDGE_CURVE('',#15906,#15904,#9011,.T.);
#20461=EDGE_CURVE('',#15907,#15908,#1942,.T.);
#20462=EDGE_CURVE('',#15909,#15907,#9012,.T.);
#20463=EDGE_CURVE('',#15910,#15909,#12906,.T.);
#20464=EDGE_CURVE('',#15910,#15908,#9013,.T.);
#20465=EDGE_CURVE('',#15908,#15911,#9014,.T.);
#20466=EDGE_CURVE('',#15912,#15910,#9015,.T.);
#20467=EDGE_CURVE('',#15911,#15912,#9016,.T.);
#20468=EDGE_CURVE('',#15913,#15912,#12907,.T.);
#20469=EDGE_CURVE('',#15914,#15913,#9017,.T.);
#20470=EDGE_CURVE('',#15911,#15914,#12908,.T.);
#20471=EDGE_CURVE('',#15914,#15915,#12909,.T.);
#20472=EDGE_CURVE('',#15916,#15913,#12910,.T.);
#20473=EDGE_CURVE('',#15915,#15916,#9018,.T.);
#20474=EDGE_CURVE('',#15917,#15916,#12911,.T.);
#20475=EDGE_CURVE('',#15918,#15917,#9019,.T.);
#20476=EDGE_CURVE('',#15919,#15918,#1943,.T.);
#20477=EDGE_CURVE('',#15920,#15919,#9020,.T.);
#20478=EDGE_CURVE('',#15915,#15920,#12912,.T.);
#20479=EDGE_CURVE('',#15921,#15922,#9021,.T.);
#20480=EDGE_CURVE('',#15918,#15921,#12913,.T.);
#20481=EDGE_CURVE('',#15923,#15917,#9022,.T.);
#20482=EDGE_CURVE('',#15923,#15922,#9023,.T.);
#20483=EDGE_CURVE('',#15924,#15925,#9024,.T.);
#20484=EDGE_CURVE('',#15924,#15894,#12914,.T.);
#20485=EDGE_CURVE('',#15894,#15926,#9025,.T.);
#20486=EDGE_CURVE('',#15926,#15925,#12915,.T.);
#20487=EDGE_CURVE('',#15924,#15895,#12916,.T.);
#20488=EDGE_CURVE('',#15927,#15900,#12917,.T.);
#20489=EDGE_CURVE('',#15927,#15924,#12918,.T.);
#20490=EDGE_CURVE('',#15927,#15901,#12919,.T.);
#20491=EDGE_CURVE('',#15928,#15929,#12920,.T.);
#20492=EDGE_CURVE('',#15929,#15901,#9026,.T.);
#20493=EDGE_CURVE('',#15928,#15927,#9027,.T.);
#20494=EDGE_CURVE('',#15930,#15931,#12921,.T.);
#20495=EDGE_CURVE('',#15931,#15929,#12922,.T.);
#20496=EDGE_CURVE('',#15930,#15928,#12923,.T.);
#20497=EDGE_CURVE('',#15932,#15905,#12924,.T.);
#20498=EDGE_CURVE('',#15905,#15931,#12925,.T.);
#20499=EDGE_CURVE('',#15932,#15930,#12926,.T.);
#20500=EDGE_CURVE('',#15933,#15906,#12927,.T.);
#20501=EDGE_CURVE('',#15933,#15932,#12928,.T.);
#20502=EDGE_CURVE('',#15934,#15909,#12929,.T.);
#20503=EDGE_CURVE('',#15909,#15906,#12930,.T.);
#20504=EDGE_CURVE('',#15934,#15933,#12931,.T.);
#20505=EDGE_CURVE('',#15935,#15910,#12932,.T.);
#20506=EDGE_CURVE('',#15935,#15934,#12933,.T.);
#20507=EDGE_CURVE('',#15936,#15912,#12934,.T.);
#20508=EDGE_CURVE('',#15936,#15935,#9028,.T.);
#20509=EDGE_CURVE('',#15936,#15913,#12935,.T.);
#20510=EDGE_CURVE('',#15937,#15916,#12936,.T.);
#20511=EDGE_CURVE('',#15937,#15936,#12937,.T.);
#20512=EDGE_CURVE('',#15937,#15917,#12938,.T.);
#20513=EDGE_CURVE('',#15938,#15937,#9029,.T.);
#20514=EDGE_CURVE('',#15938,#15923,#12939,.T.);
#20515=EDGE_CURVE('',#15925,#15939,#12940,.T.);
#20516=EDGE_CURVE('',#15939,#15938,#12941,.T.);
#20517=EDGE_CURVE('',#15940,#15941,#9030,.T.);
#20518=EDGE_CURVE('',#15941,#15942,#9031,.T.);
#20519=EDGE_CURVE('',#15942,#15943,#1944,.T.);
#20520=EDGE_CURVE('',#15943,#15944,#9032,.T.);
#20521=EDGE_CURVE('',#15944,#15945,#9033,.T.);
#20522=EDGE_CURVE('',#15946,#15945,#9034,.T.);
#20523=EDGE_CURVE('',#15940,#15946,#9035,.T.);
#20524=EDGE_CURVE('',#15947,#15946,#12942,.T.);
#20525=EDGE_CURVE('',#15948,#15947,#9036,.T.);
#20526=EDGE_CURVE('',#15948,#15940,#12943,.T.);
#20527=EDGE_CURVE('',#15949,#15948,#12944,.T.);
#20528=EDGE_CURVE('',#15950,#15947,#12945,.T.);
#20529=EDGE_CURVE('',#15949,#15950,#9037,.T.);
#20530=EDGE_CURVE('',#15951,#15950,#12946,.T.);
#20531=EDGE_CURVE('',#15952,#15951,#9038,.T.);
#20532=EDGE_CURVE('',#15952,#15949,#12947,.T.);
#20533=EDGE_CURVE('',#15953,#15951,#9039,.T.);
#20534=EDGE_CURVE('',#15953,#15954,#9040,.T.);
#20535=EDGE_CURVE('',#15954,#15952,#9041,.T.);
#20536=EDGE_CURVE('',#15955,#15954,#12948,.T.);
#20537=EDGE_CURVE('',#15956,#15953,#12949,.T.);
#20538=EDGE_CURVE('',#15956,#15955,#9042,.T.);
#20539=EDGE_CURVE('',#15957,#15958,#9043,.T.);
#20540=EDGE_CURVE('',#15945,#15958,#12950,.T.);
#20541=EDGE_CURVE('',#15957,#15944,#12951,.T.);
#20542=EDGE_CURVE('',#15959,#15946,#12952,.T.);
#20543=EDGE_CURVE('',#15960,#15945,#12953,.T.);
#20544=EDGE_CURVE('',#15959,#15960,#9044,.T.);
#20545=EDGE_CURVE('',#15959,#15947,#12954,.T.);
#20546=EDGE_CURVE('',#15961,#15950,#12955,.T.);
#20547=EDGE_CURVE('',#15961,#15959,#12956,.T.);
#20548=EDGE_CURVE('',#15961,#15951,#12957,.T.);
#20549=EDGE_CURVE('',#15962,#15953,#12958,.T.);
#20550=EDGE_CURVE('',#15962,#15961,#9045,.T.);
#20551=EDGE_CURVE('',#15963,#15956,#12959,.T.);
#20552=EDGE_CURVE('',#15963,#15962,#12960,.T.);
#20553=EDGE_CURVE('',#15585,#15964,#12961,.T.);
#20554=EDGE_CURVE('',#15584,#15964,#1945,.T.);
#20555=EDGE_CURVE('',#15964,#15956,#12962,.T.);
#20556=EDGE_CURVE('',#15584,#15963,#12963,.T.);
#20557=EDGE_CURVE('',#15960,#15958,#12964,.T.);
#20558=EDGE_CURVE('',#15586,#15965,#1946,.T.);
#20559=EDGE_CURVE('',#15587,#15965,#12965,.T.);
#20560=EDGE_CURVE('',#15960,#15586,#12966,.T.);
#20561=EDGE_CURVE('',#15958,#15965,#12967,.T.);
#20562=EDGE_CURVE('',#15966,#15967,#12968,.T.);
#20563=EDGE_CURVE('',#15968,#15967,#9046,.T.);
#20564=EDGE_CURVE('',#15968,#15969,#1947,.T.);
#20565=EDGE_CURVE('',#15969,#15966,#9047,.T.);
#20566=EDGE_CURVE('',#15970,#15967,#1948,.T.);
#20567=EDGE_CURVE('',#15970,#15971,#12969,.T.);
#20568=EDGE_CURVE('',#15971,#15972,#12970,.T.);
#20569=EDGE_CURVE('',#15967,#15972,#12971,.T.);
#20570=EDGE_CURVE('',#15973,#15972,#1949,.T.);
#20571=EDGE_CURVE('',#15973,#15974,#9048,.T.);
#20572=EDGE_CURVE('',#15975,#15974,#1950,.T.);
#20573=EDGE_CURVE('',#15972,#15975,#9049,.T.);
#20574=EDGE_CURVE('',#15968,#15976,#1951,.T.);
#20575=EDGE_CURVE('',#15975,#15968,#12972,.T.);
#20576=EDGE_CURVE('',#15975,#15977,#12973,.T.);
#20577=EDGE_CURVE('',#15977,#15976,#12974,.T.);
#20578=EDGE_CURVE('',#15976,#15969,#12975,.T.);
#20579=EDGE_CURVE('',#15978,#15966,#9050,.T.);
#20580=EDGE_CURVE('',#15969,#15979,#9051,.T.);
#20581=EDGE_CURVE('',#15979,#15978,#9052,.T.);
#20582=EDGE_CURVE('',#15970,#15966,#12976,.T.);
#20583=EDGE_CURVE('',#15980,#15971,#9053,.T.);
#20584=EDGE_CURVE('',#15981,#15970,#9054,.T.);
#20585=EDGE_CURVE('',#15981,#15980,#12977,.T.);
#20586=EDGE_CURVE('',#15973,#15971,#12978,.T.);
#20587=EDGE_CURVE('',#15982,#15983,#9055,.T.);
#20588=EDGE_CURVE('',#15974,#15983,#9056,.T.);
#20589=EDGE_CURVE('',#15982,#15973,#9057,.T.);
#20590=EDGE_CURVE('',#15974,#15977,#12979,.T.);
#20591=EDGE_CURVE('',#15984,#15985,#12980,.T.);
#20592=EDGE_CURVE('',#15976,#15985,#9058,.T.);
#20593=EDGE_CURVE('',#15977,#15984,#9059,.T.);
#20594=EDGE_CURVE('',#15985,#15979,#12981,.T.);
#20595=EDGE_CURVE('',#15979,#15986,#12982,.T.);
#20596=EDGE_CURVE('',#15986,#15987,#9060,.T.);
#20597=EDGE_CURVE('',#15978,#15987,#12983,.T.);
#20598=EDGE_CURVE('',#15978,#15981,#12984,.T.);
#20599=EDGE_CURVE('',#15981,#15988,#12985,.T.);
#20600=EDGE_CURVE('',#15988,#15989,#12986,.T.);
#20601=EDGE_CURVE('',#15980,#15989,#12987,.T.);
#20602=EDGE_CURVE('',#15980,#15982,#12988,.T.);
#20603=EDGE_CURVE('',#15982,#15990,#12989,.T.);
#20604=EDGE_CURVE('',#15990,#15991,#9061,.T.);
#20605=EDGE_CURVE('',#15983,#15991,#12990,.T.);
#20606=EDGE_CURVE('',#15983,#15984,#12991,.T.);
#20607=EDGE_CURVE('',#15984,#15992,#12992,.T.);
#20608=EDGE_CURVE('',#15992,#15993,#12993,.T.);
#20609=EDGE_CURVE('',#15985,#15993,#12994,.T.);
#20610=EDGE_CURVE('',#15993,#15986,#12995,.T.);
#20611=EDGE_CURVE('',#15994,#15995,#12996,.T.);
#20612=EDGE_CURVE('',#15996,#15995,#12997,.T.);
#20613=EDGE_CURVE('',#15994,#15996,#12998,.T.);
#20614=EDGE_CURVE('',#15987,#15988,#12999,.T.);
#20615=EDGE_CURVE('',#15989,#15990,#13000,.T.);
#20616=EDGE_CURVE('',#15991,#15992,#13001,.T.);
#20617=EDGE_CURVE('',#15997,#15619,#13002,.T.);
#20618=EDGE_CURVE('',#15997,#15620,#1952,.T.);
#20619=EDGE_CURVE('',#15998,#15620,#13003,.T.);
#20620=EDGE_CURVE('',#15999,#15998,#13004,.T.);
#20621=EDGE_CURVE('',#15999,#15997,#13005,.T.);
#20622=EDGE_CURVE('',#16000,#16001,#1953,.T.);
#20623=EDGE_CURVE('',#16001,#15943,#673,.T.);
#20624=EDGE_CURVE('',#16000,#15942,#1954,.T.);
#20625=EDGE_CURVE('',#16002,#16000,#13006,.T.);
#20626=EDGE_CURVE('',#16002,#16003,#13007,.T.);
#20627=EDGE_CURVE('',#16003,#16001,#13008,.T.);
#20628=EDGE_CURVE('',#15628,#16004,#13009,.T.);
#20629=EDGE_CURVE('',#16004,#16005,#9062,.T.);
#20630=EDGE_CURVE('',#16005,#15629,#13010,.T.);
#20631=EDGE_CURVE('',#16006,#16007,#9063,.T.);
#20632=EDGE_CURVE('',#16007,#16005,#9064,.T.);
#20633=EDGE_CURVE('',#16004,#16006,#9065,.T.);
#20634=EDGE_CURVE('',#15965,#16008,#9066,.T.);
#20635=EDGE_CURVE('',#15631,#16008,#13011,.T.);
#20636=EDGE_CURVE('',#16009,#15957,#1955,.T.);
#20637=EDGE_CURVE('',#16010,#16009,#13012,.T.);
#20638=EDGE_CURVE('',#16011,#16010,#674,.T.);
#20639=EDGE_CURVE('',#16012,#16011,#9067,.T.);
#20640=EDGE_CURVE('',#16013,#16012,#13013,.T.);
#20641=EDGE_CURVE('',#16014,#16013,#9068,.T.);
#20642=EDGE_CURVE('',#16015,#16014,#1956,.T.);
#20643=EDGE_CURVE('',#16016,#16015,#13014,.T.);
#20644=EDGE_CURVE('',#16017,#16016,#1957,.T.);
#20645=EDGE_CURVE('',#16018,#16017,#9069,.T.);
#20646=EDGE_CURVE('',#16008,#16018,#13015,.T.);
#20647=EDGE_CURVE('',#16019,#15642,#13016,.T.);
#20648=EDGE_CURVE('',#15646,#16020,#13017,.T.);
#20649=EDGE_CURVE('',#16019,#16020,#9070,.T.);
#20650=EDGE_CURVE('',#16020,#16021,#9071,.T.);
#20651=EDGE_CURVE('',#16021,#16022,#675,.T.);
#20652=EDGE_CURVE('',#16023,#16022,#9072,.T.);
#20653=EDGE_CURVE('',#16023,#16019,#9073,.T.);
#20654=EDGE_CURVE('',#16024,#16023,#13018,.T.);
#20655=EDGE_CURVE('',#16022,#16025,#1958,.T.);
#20656=EDGE_CURVE('',#16024,#16025,#9074,.T.);
#20657=EDGE_CURVE('',#16025,#16026,#676,.T.);
#20658=EDGE_CURVE('',#16026,#16027,#9075,.T.);
#20659=EDGE_CURVE('',#16027,#16028,#677,.T.);
#20660=EDGE_CURVE('',#16029,#16028,#9076,.T.);
#20661=EDGE_CURVE('',#16029,#16024,#9077,.T.);
#20662=EDGE_CURVE('',#16030,#16029,#13019,.T.);
#20663=EDGE_CURVE('',#16028,#16031,#1959,.T.);
#20664=EDGE_CURVE('',#16030,#16031,#9078,.T.);
#20665=EDGE_CURVE('',#16031,#16032,#1960,.T.);
#20666=EDGE_CURVE('',#16032,#16033,#1961,.T.);
#20667=EDGE_CURVE('',#16033,#16034,#9079,.T.);
#20668=EDGE_CURVE('',#16035,#16034,#9080,.T.);
#20669=EDGE_CURVE('',#16035,#16030,#9081,.T.);
#20670=EDGE_CURVE('',#16006,#16035,#13020,.T.);
#20671=EDGE_CURVE('',#16034,#16007,#13021,.T.);
#20672=EDGE_CURVE('',#15926,#16036,#13022,.T.);
#20673=EDGE_CURVE('',#15925,#16036,#13023,.T.);
#20674=EDGE_CURVE('',#16036,#16037,#13024,.T.);
#20675=EDGE_CURVE('',#15939,#16037,#13025,.T.);
#20676=EDGE_CURVE('',#16038,#16039,#13026,.T.);
#20677=EDGE_CURVE('',#16038,#16037,#9082,.T.);
#20678=EDGE_CURVE('',#16040,#16036,#9083,.T.);
#20679=EDGE_CURVE('',#16041,#16040,#1962,.T.);
#20680=EDGE_CURVE('',#16041,#15853,#13027,.T.);
#20681=EDGE_CURVE('',#15794,#16042,#13028,.T.);
#20682=EDGE_CURVE('',#16043,#16042,#1963,.T.);
#20683=EDGE_CURVE('',#16039,#16043,#9084,.T.);
#20684=EDGE_CURVE('',#16044,#16040,#13029,.T.);
#20685=EDGE_CURVE('',#16044,#15926,#9085,.T.);
#20686=EDGE_CURVE('',#15893,#16045,#9086,.T.);
#20687=EDGE_CURVE('',#16046,#16045,#9087,.T.);
#20688=EDGE_CURVE('',#16046,#16047,#9088,.T.);
#20689=EDGE_CURVE('',#16047,#16048,#9089,.T.);
#20690=EDGE_CURVE('',#16048,#16049,#13030,.T.);
#20691=EDGE_CURVE('',#16049,#16044,#9090,.T.);
#20692=EDGE_CURVE('',#16045,#16050,#13031,.T.);
#20693=EDGE_CURVE('',#16051,#16050,#9091,.T.);
#20694=EDGE_CURVE('',#16051,#16046,#13032,.T.);
#20695=EDGE_CURVE('',#16052,#16053,#9092,.T.);
#20696=EDGE_CURVE('',#16052,#16051,#13033,.T.);
#20697=EDGE_CURVE('',#16050,#16053,#13034,.T.);
#20698=EDGE_CURVE('',#16053,#16054,#13035,.T.);
#20699=EDGE_CURVE('',#16055,#16054,#9093,.T.);
#20700=EDGE_CURVE('',#16055,#16052,#13036,.T.);
#20701=EDGE_CURVE('',#16056,#16057,#9094,.T.);
#20702=EDGE_CURVE('',#16056,#16055,#9095,.T.);
#20703=EDGE_CURVE('',#16054,#16057,#9096,.T.);
#20704=EDGE_CURVE('',#16058,#16048,#1964,.T.);
#20705=EDGE_CURVE('',#16047,#16059,#13037,.T.);
#20706=EDGE_CURVE('',#16059,#16058,#9097,.T.);
#20707=EDGE_CURVE('',#16057,#16060,#13038,.T.);
#20708=EDGE_CURVE('',#16061,#16060,#9098,.T.);
#20709=EDGE_CURVE('',#16061,#16056,#13039,.T.);
#20710=EDGE_CURVE('',#16060,#16058,#13040,.T.);
#20711=EDGE_CURVE('',#16059,#16061,#13041,.T.);
#20712=EDGE_CURVE('',#16062,#15998,#13042,.T.);
#20713=EDGE_CURVE('',#15998,#16063,#9099,.T.);
#20714=EDGE_CURVE('',#16064,#16063,#13043,.T.);
#20715=EDGE_CURVE('',#16062,#16064,#9100,.T.);
#20716=EDGE_CURVE('',#16065,#16066,#13044,.T.);
#20717=EDGE_CURVE('',#16066,#16067,#13045,.T.);
#20718=EDGE_CURVE('',#16068,#16067,#13046,.T.);
#20719=EDGE_CURVE('',#16065,#16068,#13047,.T.);
#20720=EDGE_CURVE('',#16069,#16070,#13048,.T.);
#20721=EDGE_CURVE('',#16070,#16066,#13049,.T.);
#20722=EDGE_CURVE('',#16069,#16065,#13050,.T.);
#20723=EDGE_CURVE('',#16071,#16072,#13051,.T.);
#20724=EDGE_CURVE('',#16072,#16070,#9101,.T.);
#20725=EDGE_CURVE('',#16071,#16069,#9102,.T.);
#20726=EDGE_CURVE('',#16073,#16074,#13052,.T.);
#20727=EDGE_CURVE('',#16074,#16072,#13053,.T.);
#20728=EDGE_CURVE('',#16073,#16071,#13054,.T.);
#20729=EDGE_CURVE('',#16075,#16076,#13055,.T.);
#20730=EDGE_CURVE('',#16076,#16074,#13056,.T.);
#20731=EDGE_CURVE('',#16075,#16073,#13057,.T.);
#20732=EDGE_CURVE('',#16067,#16077,#13058,.T.);
#20733=EDGE_CURVE('',#16078,#16077,#13059,.T.);
#20734=EDGE_CURVE('',#16068,#16078,#13060,.T.);
#20735=EDGE_CURVE('',#16079,#16080,#13061,.T.);
#20736=EDGE_CURVE('',#16080,#16076,#13062,.T.);
#20737=EDGE_CURVE('',#16079,#16075,#13063,.T.);
#20738=EDGE_CURVE('',#16077,#16080,#9103,.T.);
#20739=EDGE_CURVE('',#16078,#16079,#9104,.T.);
#20740=EDGE_CURVE('',#16081,#16082,#13064,.T.);
#20741=EDGE_CURVE('',#16082,#16083,#13065,.T.);
#20742=EDGE_CURVE('',#16084,#16083,#13066,.T.);
#20743=EDGE_CURVE('',#16081,#16084,#13067,.T.);
#20744=EDGE_CURVE('',#16032,#16085,#678,.T.);
#20745=EDGE_CURVE('',#16085,#16086,#1965,.T.);
#20746=EDGE_CURVE('',#16033,#16086,#679,.T.);
#20747=EDGE_CURVE('',#16087,#16085,#13068,.T.);
#20748=EDGE_CURVE('',#16084,#16087,#13069,.T.);
#20749=EDGE_CURVE('',#16083,#16086,#13070,.T.);
#20750=EDGE_CURVE('',#16027,#16088,#680,.T.);
#20751=EDGE_CURVE('',#16088,#16089,#681,.T.);
#20752=EDGE_CURVE('',#16028,#16089,#682,.T.);
#20753=EDGE_CURVE('',#16089,#16090,#1966,.T.);
#20754=EDGE_CURVE('',#16031,#16090,#683,.T.);
#20755=EDGE_CURVE('',#16090,#16085,#1967,.T.);
#20756=EDGE_CURVE('',#16088,#16091,#13071,.T.);
#20757=EDGE_CURVE('',#16092,#16091,#13072,.T.);
#20758=EDGE_CURVE('',#16087,#16092,#13073,.T.);
#20759=EDGE_CURVE('',#16093,#16094,#13074,.T.);
#20760=EDGE_CURVE('',#16094,#16082,#13075,.T.);
#20761=EDGE_CURVE('',#16093,#16081,#13076,.T.);
#20762=EDGE_CURVE('',#16091,#16095,#13077,.T.);
#20763=EDGE_CURVE('',#16096,#16095,#13078,.T.);
#20764=EDGE_CURVE('',#16092,#16096,#13079,.T.);
#20765=EDGE_CURVE('',#16095,#16094,#9105,.T.);
#20766=EDGE_CURVE('',#16096,#16093,#9106,.T.);
#20767=EDGE_CURVE('',#16021,#16097,#684,.T.);
#20768=EDGE_CURVE('',#16097,#16098,#685,.T.);
#20769=EDGE_CURVE('',#16022,#16098,#686,.T.);
#20770=EDGE_CURVE('',#16098,#16099,#1968,.T.);
#20771=EDGE_CURVE('',#16025,#16099,#687,.T.);
#20772=EDGE_CURVE('',#16099,#16100,#688,.T.);
#20773=EDGE_CURVE('',#16026,#16100,#689,.T.);
#20774=EDGE_CURVE('',#16101,#16097,#13080,.T.);
#20775=EDGE_CURVE('',#16101,#16102,#13081,.T.);
#20776=EDGE_CURVE('',#16102,#16103,#13082,.T.);
#20777=EDGE_CURVE('',#16104,#16103,#13083,.T.);
#20778=EDGE_CURVE('',#16100,#16104,#13084,.T.);
#20779=EDGE_CURVE('',#16105,#16106,#13085,.T.);
#20780=EDGE_CURVE('',#16106,#16102,#13086,.T.);
#20781=EDGE_CURVE('',#16105,#16101,#13087,.T.);
#20782=EDGE_CURVE('',#16107,#16108,#13088,.T.);
#20783=EDGE_CURVE('',#16108,#16106,#9107,.T.);
#20784=EDGE_CURVE('',#16107,#16105,#9108,.T.);
#20785=EDGE_CURVE('',#16109,#16110,#13089,.T.);
#20786=EDGE_CURVE('',#16110,#16108,#13090,.T.);
#20787=EDGE_CURVE('',#16109,#16107,#13091,.T.);
#20788=EDGE_CURVE('',#16111,#16112,#13092,.T.);
#20789=EDGE_CURVE('',#16112,#16110,#13093,.T.);
#20790=EDGE_CURVE('',#16111,#16109,#13094,.T.);
#20791=EDGE_CURVE('',#16103,#16113,#13095,.T.);
#20792=EDGE_CURVE('',#16114,#16113,#13096,.T.);
#20793=EDGE_CURVE('',#16104,#16114,#13097,.T.);
#20794=EDGE_CURVE('',#16115,#16116,#13098,.T.);
#20795=EDGE_CURVE('',#16116,#16112,#13099,.T.);
#20796=EDGE_CURVE('',#16115,#16111,#13100,.T.);
#20797=EDGE_CURVE('',#16113,#16116,#9109,.T.);
#20798=EDGE_CURVE('',#16114,#16115,#9110,.T.);
#20799=EDGE_CURVE('',#16117,#16118,#1969,.T.);
#20800=EDGE_CURVE('',#16118,#16119,#9111,.T.);
#20801=EDGE_CURVE('',#16120,#16119,#1970,.T.);
#20802=EDGE_CURVE('',#16117,#16120,#9112,.T.);
#20803=EDGE_CURVE('',#15994,#16121,#9113,.T.);
#20804=EDGE_CURVE('',#16121,#16122,#13101,.T.);
#20805=EDGE_CURVE('',#15995,#16122,#9114,.T.);
#20806=EDGE_CURVE('',#16123,#16124,#1971,.T.);
#20807=EDGE_CURVE('',#16125,#16123,#13102,.T.);
#20808=EDGE_CURVE('',#16125,#16126,#1972,.T.);
#20809=EDGE_CURVE('',#16126,#16124,#13103,.T.);
#20810=EDGE_CURVE('',#16127,#16126,#13104,.T.);
#20811=EDGE_CURVE('',#16127,#16125,#13105,.T.);
#20812=EDGE_CURVE('',#16128,#16129,#1973,.T.);
#20813=EDGE_CURVE('',#16129,#16126,#13106,.T.);
#20814=EDGE_CURVE('',#16128,#16127,#13107,.T.);
#20815=EDGE_CURVE('',#16130,#16124,#13108,.T.);
#20816=EDGE_CURVE('',#16123,#16130,#13109,.T.);
#20817=EDGE_CURVE('',#16131,#16129,#13110,.T.);
#20818=EDGE_CURVE('',#16131,#16128,#13111,.T.);
#20819=EDGE_CURVE('',#16117,#16132,#13112,.T.);
#20820=EDGE_CURVE('',#16132,#16118,#13113,.T.);
#20821=EDGE_CURVE('',#16124,#16129,#9115,.T.);
#20822=EDGE_CURVE('',#16130,#16131,#9116,.T.);
#20823=EDGE_CURVE('',#16133,#16134,#1974,.T.);
#20824=EDGE_CURVE('',#16133,#16132,#13114,.T.);
#20825=EDGE_CURVE('',#16134,#16117,#13115,.T.);
#20826=EDGE_CURVE('',#16063,#16135,#13116,.T.);
#20827=EDGE_CURVE('',#16136,#16135,#13117,.T.);
#20828=EDGE_CURVE('',#16064,#16136,#13118,.T.);
#20829=EDGE_CURVE('',#16135,#16137,#13119,.T.);
#20830=EDGE_CURVE('',#16138,#16137,#13120,.T.);
#20831=EDGE_CURVE('',#16136,#16138,#13121,.T.);
#20832=EDGE_CURVE('',#16139,#16140,#13122,.T.);
#20833=EDGE_CURVE('',#16140,#16003,#13123,.T.);
#20834=EDGE_CURVE('',#16139,#16002,#13124,.T.);
#20835=EDGE_CURVE('',#16137,#16141,#13125,.T.);
#20836=EDGE_CURVE('',#16142,#16141,#13126,.T.);
#20837=EDGE_CURVE('',#16138,#16142,#13127,.T.);
#20838=EDGE_CURVE('',#16143,#16122,#13128,.T.);
#20839=EDGE_CURVE('',#16143,#16121,#13129,.T.);
#20840=EDGE_CURVE('',#16144,#15762,#13130,.T.);
#20841=EDGE_CURVE('',#16144,#15997,#9117,.T.);
#20842=EDGE_CURVE('',#16145,#15999,#9118,.T.);
#20843=EDGE_CURVE('',#16144,#16145,#13131,.T.);
#20844=EDGE_CURVE('',#15999,#16062,#13132,.T.);
#20845=EDGE_CURVE('',#15764,#16144,#1975,.T.);
#20846=EDGE_CURVE('',#16146,#16145,#1976,.T.);
#20847=EDGE_CURVE('',#15764,#16146,#13133,.T.);
#20848=EDGE_CURVE('',#16147,#16148,#13134,.T.);
#20849=EDGE_CURVE('',#16149,#16148,#9119,.T.);
#20850=EDGE_CURVE('',#16149,#16150,#13135,.T.);
#20851=EDGE_CURVE('',#16150,#16147,#9120,.T.);
#20852=EDGE_CURVE('',#16143,#16151,#13136,.T.);
#20853=EDGE_CURVE('',#16151,#16152,#13137,.T.);
#20854=EDGE_CURVE('',#16122,#16152,#13138,.T.);
#20855=EDGE_CURVE('',#16153,#16154,#13139,.T.);
#20856=EDGE_CURVE('',#16153,#16154,#13140,.T.);
#20857=EDGE_CURVE('',#16155,#16013,#13141,.T.);
#20858=EDGE_CURVE('',#16156,#16012,#13142,.T.);
#20859=EDGE_CURVE('',#16155,#16156,#13143,.T.);
#20860=EDGE_CURVE('',#16157,#16038,#13144,.T.);
#20861=EDGE_CURVE('',#16158,#16039,#13145,.T.);
#20862=EDGE_CURVE('',#16157,#16158,#13146,.T.);
#20863=EDGE_CURVE('',#15627,#16159,#13147,.T.);
#20864=EDGE_CURVE('',#16159,#16160,#9121,.T.);
#20865=EDGE_CURVE('',#15628,#16160,#13148,.T.);
#20866=EDGE_CURVE('',#15642,#16161,#13149,.T.);
#20867=EDGE_CURVE('',#16161,#16162,#9122,.T.);
#20868=EDGE_CURVE('',#15643,#16162,#13150,.T.);
#20869=EDGE_CURVE('',#16162,#16163,#13151,.T.);
#20870=EDGE_CURVE('',#15647,#16163,#13152,.T.);
#20871=EDGE_CURVE('',#16163,#16164,#9123,.T.);
#20872=EDGE_CURVE('',#15649,#16164,#13153,.T.);
#20873=EDGE_CURVE('',#16164,#16165,#13154,.T.);
#20874=EDGE_CURVE('',#15653,#16165,#13155,.T.);
#20875=EDGE_CURVE('',#16165,#16166,#9124,.T.);
#20876=EDGE_CURVE('',#15655,#16166,#13156,.T.);
#20877=EDGE_CURVE('',#16166,#16159,#13157,.T.);
#20878=EDGE_CURVE('',#16160,#16167,#13158,.T.);
#20879=EDGE_CURVE('',#16004,#16167,#13159,.T.);
#20880=EDGE_CURVE('',#16167,#16168,#9125,.T.);
#20881=EDGE_CURVE('',#16006,#16168,#13160,.T.);
#20882=EDGE_CURVE('',#16019,#16169,#13161,.T.);
#20883=EDGE_CURVE('',#16169,#16161,#13162,.T.);
#20884=EDGE_CURVE('',#16023,#16170,#13163,.T.);
#20885=EDGE_CURVE('',#16170,#16169,#9126,.T.);
#20886=EDGE_CURVE('',#16024,#16171,#13164,.T.);
#20887=EDGE_CURVE('',#16171,#16170,#13165,.T.);
#20888=EDGE_CURVE('',#16029,#16172,#13166,.T.);
#20889=EDGE_CURVE('',#16172,#16171,#9127,.T.);
#20890=EDGE_CURVE('',#16030,#16173,#13167,.T.);
#20891=EDGE_CURVE('',#16173,#16172,#13168,.T.);
#20892=EDGE_CURVE('',#16035,#16174,#13169,.T.);
#20893=EDGE_CURVE('',#16174,#16173,#9128,.T.);
#20894=EDGE_CURVE('',#16168,#16174,#13170,.T.);
#20895=EDGE_CURVE('',#16156,#16157,#13171,.T.);
#20896=EDGE_CURVE('',#16175,#16158,#9129,.T.);
#20897=EDGE_CURVE('',#16176,#16175,#13172,.T.);
#20898=EDGE_CURVE('',#16176,#15820,#9130,.T.);
#20899=EDGE_CURVE('',#15780,#16177,#13173,.T.);
#20900=EDGE_CURVE('',#16155,#16177,#13174,.T.);
#20901=EDGE_CURVE('',#16008,#15780,#1977,.T.);
#20902=EDGE_CURVE('',#16177,#16018,#1978,.T.);
#20903=EDGE_CURVE('',#16178,#16177,#13175,.T.);
#20904=EDGE_CURVE('',#16179,#16178,#13176,.T.);
#20905=EDGE_CURVE('',#16179,#16155,#13177,.T.);
#20906=EDGE_CURVE('',#15923,#16180,#13178,.T.);
#20907=EDGE_CURVE('',#16180,#16181,#9131,.T.);
#20908=EDGE_CURVE('',#15922,#16181,#13179,.T.);
#20909=EDGE_CURVE('',#15938,#16180,#13180,.T.);
#20910=EDGE_CURVE('',#16037,#16180,#13181,.T.);
#20911=EDGE_CURVE('',#16012,#16038,#13182,.T.);
#20912=EDGE_CURVE('',#16181,#16011,#1979,.T.);
#20913=EDGE_CURVE('',#16182,#16017,#690,.T.);
#20914=EDGE_CURVE('',#16153,#16016,#691,.T.);
#20915=EDGE_CURVE('',#16182,#16153,#1980,.T.);
#20916=EDGE_CURVE('',#16154,#16015,#692,.T.);
#20917=EDGE_CURVE('',#16183,#16014,#693,.T.);
#20918=EDGE_CURVE('',#16154,#16183,#1981,.T.);
#20919=EDGE_CURVE('',#16179,#16013,#13183,.T.);
#20920=EDGE_CURVE('',#16183,#16179,#9132,.T.);
#20921=EDGE_CURVE('',#16178,#16018,#13184,.T.);
#20922=EDGE_CURVE('',#16178,#16182,#9133,.T.);
#20923=EDGE_CURVE('',#16147,#16176,#13185,.T.);
#20924=EDGE_CURVE('',#16147,#15767,#9134,.T.);
#20925=EDGE_CURVE('',#15766,#16150,#9135,.T.);
#20926=EDGE_CURVE('',#16150,#16184,#13186,.T.);
#20927=EDGE_CURVE('',#16184,#16185,#1982,.T.);
#20928=EDGE_CURVE('',#16185,#15803,#9136,.T.);
#20929=EDGE_CURVE('',#16186,#15793,#13187,.T.);
#20930=EDGE_CURVE('',#16186,#16042,#13188,.T.);
#20931=EDGE_CURVE('',#16185,#16187,#13189,.T.);
#20932=EDGE_CURVE('',#16187,#16188,#13190,.T.);
#20933=EDGE_CURVE('',#16188,#16189,#9137,.T.);
#20934=EDGE_CURVE('',#16189,#16190,#13191,.T.);
#20935=EDGE_CURVE('',#16190,#16191,#13192,.T.);
#20936=EDGE_CURVE('',#16191,#16186,#9138,.T.);
#20937=EDGE_CURVE('',#16192,#16039,#13193,.T.);
#20938=EDGE_CURVE('',#16158,#16192,#13194,.T.);
#20939=EDGE_CURVE('',#16193,#16158,#13195,.T.);
#20940=EDGE_CURVE('',#16148,#16192,#9139,.T.);
#20941=EDGE_CURVE('',#16148,#16175,#13196,.T.);
#20942=EDGE_CURVE('',#16194,#16043,#1983,.T.);
#20943=EDGE_CURVE('',#16192,#16194,#9140,.T.);
#20944=EDGE_CURVE('',#16194,#16149,#9141,.T.);
#20945=EDGE_CURVE('',#16194,#16186,#1984,.T.);
#20946=EDGE_CURVE('',#16191,#16195,#1985,.T.);
#20947=EDGE_CURVE('',#16196,#16195,#9142,.T.);
#20948=EDGE_CURVE('',#16196,#16197,#694,.T.);
#20949=EDGE_CURVE('',#16197,#16149,#13197,.T.);
#20950=EDGE_CURVE('',#16198,#16199,#9143,.T.);
#20951=EDGE_CURVE('',#16199,#16047,#13198,.T.);
#20952=EDGE_CURVE('',#16198,#16046,#13199,.T.);
#20953=EDGE_CURVE('',#16198,#16051,#13200,.T.);
#20954=EDGE_CURVE('',#16197,#16184,#1986,.T.);
#20955=EDGE_CURVE('',#16196,#16198,#13201,.T.);
#20956=EDGE_CURVE('',#16187,#16052,#13202,.T.);
#20957=EDGE_CURVE('',#16188,#16055,#13203,.T.);
#20958=EDGE_CURVE('',#16189,#16056,#13204,.T.);
#20959=EDGE_CURVE('',#16199,#16059,#13205,.T.);
#20960=EDGE_CURVE('',#16190,#16061,#13206,.T.);
#20961=EDGE_CURVE('',#16199,#16195,#13207,.T.);
#20962=EDGE_CURVE('',#16064,#16200,#9144,.T.);
#20963=EDGE_CURVE('',#16201,#16200,#9145,.T.);
#20964=EDGE_CURVE('',#16201,#16062,#9146,.T.);
#20965=EDGE_CURVE('',#16066,#16151,#9147,.T.);
#20966=EDGE_CURVE('',#16067,#16143,#9148,.T.);
#20967=EDGE_CURVE('',#16070,#16202,#9149,.T.);
#20968=EDGE_CURVE('',#16202,#16151,#13208,.T.);
#20969=EDGE_CURVE('',#16203,#16072,#9150,.T.);
#20970=EDGE_CURVE('',#16202,#16203,#9151,.T.);
#20971=EDGE_CURVE('',#16204,#16074,#9152,.T.);
#20972=EDGE_CURVE('',#16203,#16204,#13209,.T.);
#20973=EDGE_CURVE('',#16076,#15996,#9153,.T.);
#20974=EDGE_CURVE('',#16204,#15996,#13210,.T.);
#20975=EDGE_CURVE('',#16077,#16121,#9154,.T.);
#20976=EDGE_CURVE('',#16080,#15994,#9155,.T.);
#20977=EDGE_CURVE('',#16084,#16125,#9156,.T.);
#20978=EDGE_CURVE('',#16081,#16123,#9157,.T.);
#20979=EDGE_CURVE('',#16087,#16127,#9158,.T.);
#20980=EDGE_CURVE('',#16092,#16128,#9159,.T.);
#20981=EDGE_CURVE('',#16093,#16130,#9160,.T.);
#20982=EDGE_CURVE('',#16096,#16131,#9161,.T.);
#20983=EDGE_CURVE('',#16132,#16102,#9162,.T.);
#20984=EDGE_CURVE('',#16103,#16133,#9163,.T.);
#20985=EDGE_CURVE('',#16118,#16106,#9164,.T.);
#20986=EDGE_CURVE('',#16119,#16108,#9165,.T.);
#20987=EDGE_CURVE('',#16205,#16110,#9166,.T.);
#20988=EDGE_CURVE('',#16119,#16205,#13211,.T.);
#20989=EDGE_CURVE('',#16206,#16112,#9167,.T.);
#20990=EDGE_CURVE('',#16205,#16206,#13212,.T.);
#20991=EDGE_CURVE('',#16133,#16207,#13213,.T.);
#20992=EDGE_CURVE('',#16113,#16207,#9168,.T.);
#20993=EDGE_CURVE('',#16208,#16116,#9169,.T.);
#20994=EDGE_CURVE('',#16206,#16208,#13214,.T.);
#20995=EDGE_CURVE('',#16208,#16207,#9170,.T.);
#20996=EDGE_CURVE('',#16120,#16205,#13215,.T.);
#20997=EDGE_CURVE('',#16209,#16206,#1987,.T.);
#20998=EDGE_CURVE('',#16120,#16209,#13216,.T.);
#20999=EDGE_CURVE('',#16207,#16134,#13217,.T.);
#21000=EDGE_CURVE('',#16209,#16208,#13218,.T.);
#21001=EDGE_CURVE('',#16209,#16134,#9171,.T.);
#21002=EDGE_CURVE('',#16210,#15995,#13219,.T.);
#21003=EDGE_CURVE('',#16152,#16210,#9172,.T.);
#21004=EDGE_CURVE('',#16211,#16212,#13220,.T.);
#21005=EDGE_CURVE('',#16200,#16212,#13221,.T.);
#21006=EDGE_CURVE('',#16211,#16200,#13222,.T.);
#21007=EDGE_CURVE('',#16136,#16211,#9173,.T.);
#21008=EDGE_CURVE('',#16182,#16183,#13223,.T.);
#21009=EDGE_CURVE('',#16202,#16152,#13224,.T.);
#21010=EDGE_CURVE('',#16210,#16204,#1988,.T.);
#21011=EDGE_CURVE('',#16201,#16145,#13225,.T.);
#21012=EDGE_CURVE('',#16146,#16201,#1989,.T.);
#21013=EDGE_CURVE('',#16210,#16203,#1990,.T.);
#21014=EDGE_CURVE('',#16146,#16212,#9174,.T.);
#21015=EDGE_CURVE('',#16213,#16214,#13226,.T.);
#21016=EDGE_CURVE('',#16215,#16214,#13227,.T.);
#21017=EDGE_CURVE('',#16213,#16215,#13228,.T.);
#21018=EDGE_CURVE('',#16142,#16213,#9175,.T.);
#21019=EDGE_CURVE('',#16138,#16215,#9176,.T.);
#21020=EDGE_CURVE('',#16211,#16215,#13229,.T.);
#21021=EDGE_CURVE('',#16212,#16214,#13230,.T.);
#21022=EDGE_CURVE('',#16216,#16217,#9177,.T.);
#21023=EDGE_CURVE('',#16217,#15941,#13231,.T.);
#21024=EDGE_CURVE('',#16216,#15940,#13232,.T.);
#21025=EDGE_CURVE('',#16218,#16216,#13233,.T.);
#21026=EDGE_CURVE('',#16218,#15948,#13234,.T.);
#21027=EDGE_CURVE('',#16219,#16218,#13235,.T.);
#21028=EDGE_CURVE('',#16219,#15949,#13236,.T.);
#21029=EDGE_CURVE('',#16220,#16219,#13237,.T.);
#21030=EDGE_CURVE('',#16220,#15952,#13238,.T.);
#21031=EDGE_CURVE('',#16221,#16220,#9178,.T.);
#21032=EDGE_CURVE('',#16221,#15954,#13239,.T.);
#21033=EDGE_CURVE('',#15835,#16221,#13240,.T.);
#21034=EDGE_CURVE('',#16214,#16222,#9179,.T.);
#21035=EDGE_CURVE('',#16217,#16222,#13241,.T.);
#21036=EDGE_CURVE('',#16217,#16223,#13242,.T.);
#21037=EDGE_CURVE('',#16223,#15941,#13243,.T.);
#21038=EDGE_CURVE('',#16217,#16224,#13244,.T.);
#21039=EDGE_CURVE('',#16222,#16225,#1991,.T.);
#21040=EDGE_CURVE('',#16223,#16225,#13245,.T.);
#21041=EDGE_CURVE('',#15955,#16221,#13246,.T.);
#21042=EDGE_CURVE('',#16226,#15835,#1992,.T.);
#21043=EDGE_CURVE('',#15834,#16226,#13247,.T.);
#21044=EDGE_CURVE('',#16226,#15955,#13248,.T.);
#21045=EDGE_CURVE('',#16223,#16000,#9180,.T.);
#21046=EDGE_CURVE('',#16225,#16002,#9181,.T.);
#21047=EDGE_CURVE('',#15964,#16226,#9182,.T.);
#21048=EDGE_CURVE('',#16227,#16225,#13249,.T.);
#21049=EDGE_CURVE('',#16227,#16139,#9183,.T.);
#21050=EDGE_CURVE('',#16222,#16227,#13250,.T.);
#21051=EDGE_CURVE('',#16213,#16227,#9184,.T.);
#21052=EDGE_CURVE('',#16142,#16139,#9185,.T.);
#21053=EDGE_CURVE('',#16141,#16140,#9186,.T.);
#21054=EDGE_CURVE('',#16228,#15893,#1993,.T.);
#21055=EDGE_CURVE('',#16228,#15897,#695,.T.);
#21056=EDGE_CURVE('',#16228,#16229,#9187,.T.);
#21057=EDGE_CURVE('',#16045,#16229,#13251,.T.);
#21058=EDGE_CURVE('',#16229,#16230,#13252,.T.);
#21059=EDGE_CURVE('',#16050,#16230,#13253,.T.);
#21060=EDGE_CURVE('',#16230,#16231,#13254,.T.);
#21061=EDGE_CURVE('',#16053,#16231,#13255,.T.);
#21062=EDGE_CURVE('',#16231,#16232,#13256,.T.);
#21063=EDGE_CURVE('',#16054,#16232,#13257,.T.);
#21064=EDGE_CURVE('',#16232,#16233,#9188,.T.);
#21065=EDGE_CURVE('',#16057,#16233,#13258,.T.);
#21066=EDGE_CURVE('',#16058,#16234,#1994,.T.);
#21067=EDGE_CURVE('',#16234,#16049,#13259,.T.);
#21068=EDGE_CURVE('',#16058,#16235,#13260,.T.);
#21069=EDGE_CURVE('',#16235,#16234,#13261,.T.);
#21070=EDGE_CURVE('',#16233,#16236,#13262,.T.);
#21071=EDGE_CURVE('',#16060,#16236,#13263,.T.);
#21072=EDGE_CURVE('',#16236,#16235,#13264,.T.);
#21073=EDGE_CURVE('',#16237,#16228,#13265,.T.);
#21074=EDGE_CURVE('',#16237,#15896,#13266,.T.);
#21075=EDGE_CURVE('',#16238,#16237,#13267,.T.);
#21076=EDGE_CURVE('',#16238,#15899,#696,.T.);
#21077=EDGE_CURVE('',#16239,#16011,#697,.T.);
#21078=EDGE_CURVE('',#16240,#16010,#698,.T.);
#21079=EDGE_CURVE('',#16239,#16240,#699,.T.);
#21080=EDGE_CURVE('',#15922,#16239,#1995,.T.);
#21081=EDGE_CURVE('',#16241,#16240,#9189,.T.);
#21082=EDGE_CURVE('',#15921,#16241,#700,.T.);
#21083=EDGE_CURVE('',#16242,#16009,#701,.T.);
#21084=EDGE_CURVE('',#16242,#15944,#1996,.T.);
#21085=EDGE_CURVE('',#16001,#16242,#9190,.T.);
#21086=EDGE_CURVE('',#16243,#16041,#702,.T.);
#21087=EDGE_CURVE('',#16243,#16044,#1997,.T.);
#21088=EDGE_CURVE('',#16234,#16243,#9191,.T.);
#21089=EDGE_CURVE('',#16240,#16242,#13268,.T.);
#21090=EDGE_CURVE('',#16243,#15852,#13269,.T.);
#21091=EDGE_CURVE('',#15629,#16244,#13270,.T.);
#21092=EDGE_CURVE('',#16244,#16245,#9192,.T.);
#21093=EDGE_CURVE('',#15630,#16245,#13271,.T.);
#21094=EDGE_CURVE('',#15716,#16246,#9193,.T.);
#21095=EDGE_CURVE('',#15646,#16246,#13272,.T.);
#21096=EDGE_CURVE('',#15707,#15718,#9194,.T.);
#21097=EDGE_CURVE('',#15656,#16247,#13273,.T.);
#21098=EDGE_CURVE('',#16247,#15703,#9195,.T.);
#21099=EDGE_CURVE('',#16245,#16247,#13274,.T.);
#21100=EDGE_CURVE('',#16005,#16248,#13275,.T.);
#21101=EDGE_CURVE('',#16248,#16244,#13276,.T.);
#21102=EDGE_CURVE('',#16007,#16249,#13277,.T.);
#21103=EDGE_CURVE('',#16249,#16248,#9196,.T.);
#21104=EDGE_CURVE('',#16246,#16250,#13278,.T.);
#21105=EDGE_CURVE('',#16020,#16250,#13279,.T.);
#21106=EDGE_CURVE('',#16250,#16097,#9197,.T.);
#21107=EDGE_CURVE('',#16100,#16088,#9198,.T.);
#21108=EDGE_CURVE('',#16086,#16251,#9199,.T.);
#21109=EDGE_CURVE('',#16034,#16251,#13280,.T.);
#21110=EDGE_CURVE('',#16251,#16249,#13281,.T.);
#21111=EDGE_CURVE('',#16252,#16238,#9200,.T.);
#21112=EDGE_CURVE('',#16253,#16252,#13282,.T.);
#21113=EDGE_CURVE('',#16254,#16253,#13283,.T.);
#21114=EDGE_CURVE('',#16255,#16254,#13284,.T.);
#21115=EDGE_CURVE('',#16256,#16255,#9201,.T.);
#21116=EDGE_CURVE('',#16257,#16256,#13285,.T.);
#21117=EDGE_CURVE('',#16241,#16257,#13286,.T.);
#21118=EDGE_CURVE('',#16258,#16259,#13287,.T.);
#21119=EDGE_CURVE('',#16258,#15903,#1998,.T.);
#21120=EDGE_CURVE('',#16259,#15904,#1999,.T.);
#21121=EDGE_CURVE('',#15918,#16260,#2000,.T.);
#21122=EDGE_CURVE('',#16261,#16260,#2001,.T.);
#21123=EDGE_CURVE('',#15919,#16261,#703,.T.);
#21124=EDGE_CURVE('',#16260,#16241,#13288,.T.);
#21125=EDGE_CURVE('',#16262,#16257,#13289,.T.);
#21126=EDGE_CURVE('',#16261,#16262,#13290,.T.);
#21127=EDGE_CURVE('',#16263,#16256,#13291,.T.);
#21128=EDGE_CURVE('',#16262,#16263,#13292,.T.);
#21129=EDGE_CURVE('',#16264,#16255,#13293,.T.);
#21130=EDGE_CURVE('',#16263,#16264,#9202,.T.);
#21131=EDGE_CURVE('',#16265,#16254,#13294,.T.);
#21132=EDGE_CURVE('',#16264,#16265,#13295,.T.);
#21133=EDGE_CURVE('',#16266,#16253,#13296,.T.);
#21134=EDGE_CURVE('',#16265,#16266,#13297,.T.);
#21135=EDGE_CURVE('',#16267,#16252,#13298,.T.);
#21136=EDGE_CURVE('',#16266,#16267,#13299,.T.);
#21137=EDGE_CURVE('',#16268,#16238,#704,.T.);
#21138=EDGE_CURVE('',#16268,#15898,#705,.T.);
#21139=EDGE_CURVE('',#15902,#16268,#2002,.T.);
#21140=EDGE_CURVE('',#16267,#15902,#9203,.T.);
#21141=EDGE_CURVE('',#16269,#16258,#9204,.T.);
#21142=EDGE_CURVE('',#16270,#16269,#13300,.T.);
#21143=EDGE_CURVE('',#15931,#16270,#9205,.T.);
#21144=EDGE_CURVE('',#16271,#16259,#9206,.T.);
#21145=EDGE_CURVE('',#16269,#16271,#13301,.T.);
#21146=EDGE_CURVE('',#16271,#15907,#13302,.T.);
#21147=EDGE_CURVE('',#16272,#16261,#9207,.T.);
#21148=EDGE_CURVE('',#15920,#16272,#13303,.T.);
#21149=EDGE_CURVE('',#16262,#16273,#9208,.T.);
#21150=EDGE_CURVE('',#16272,#16273,#13304,.T.);
#21151=EDGE_CURVE('',#16263,#16274,#9209,.T.);
#21152=EDGE_CURVE('',#16274,#16273,#13305,.T.);
#21153=EDGE_CURVE('',#16264,#16275,#9210,.T.);
#21154=EDGE_CURVE('',#16274,#16275,#9211,.T.);
#21155=EDGE_CURVE('',#16265,#16276,#9212,.T.);
#21156=EDGE_CURVE('',#16276,#16275,#13306,.T.);
#21157=EDGE_CURVE('',#16266,#16277,#9213,.T.);
#21158=EDGE_CURVE('',#16276,#16277,#13307,.T.);
#21159=EDGE_CURVE('',#16267,#16278,#9214,.T.);
#21160=EDGE_CURVE('',#16278,#16277,#13308,.T.);
#21161=EDGE_CURVE('',#15929,#16279,#9215,.T.);
#21162=EDGE_CURVE('',#16278,#16279,#9216,.T.);
#21163=EDGE_CURVE('',#16279,#16270,#13309,.T.);
#21164=EDGE_CURVE('',#16280,#16279,#13310,.T.);
#21165=EDGE_CURVE('',#16280,#16270,#13311,.T.);
#21166=EDGE_CURVE('',#16269,#16281,#13312,.T.);
#21167=EDGE_CURVE('',#16280,#16281,#13313,.T.);
#21168=EDGE_CURVE('',#16271,#16282,#13314,.T.);
#21169=EDGE_CURVE('',#16281,#16282,#13315,.T.);
#21170=EDGE_CURVE('',#15908,#16283,#13316,.T.);
#21171=EDGE_CURVE('',#15907,#16283,#13317,.T.);
#21172=EDGE_CURVE('',#16282,#16283,#13318,.T.);
#21173=EDGE_CURVE('',#16284,#16272,#13319,.T.);
#21174=EDGE_CURVE('',#15920,#16284,#13320,.T.);
#21175=EDGE_CURVE('',#16273,#16285,#13321,.T.);
#21176=EDGE_CURVE('',#16284,#16285,#13322,.T.);
#21177=EDGE_CURVE('',#16274,#16285,#13323,.T.);
#21178=EDGE_CURVE('',#16275,#16286,#13324,.T.);
#21179=EDGE_CURVE('',#16285,#16286,#9217,.T.);
#21180=EDGE_CURVE('',#16276,#16286,#13325,.T.);
#21181=EDGE_CURVE('',#16277,#16287,#13326,.T.);
#21182=EDGE_CURVE('',#16286,#16287,#13327,.T.);
#21183=EDGE_CURVE('',#16278,#16287,#13328,.T.);
#21184=EDGE_CURVE('',#16287,#16280,#9218,.T.);
#21185=EDGE_CURVE('',#15911,#16288,#13329,.T.);
#21186=EDGE_CURVE('',#16283,#16288,#9219,.T.);
#21187=EDGE_CURVE('',#15914,#16289,#13330,.T.);
#21188=EDGE_CURVE('',#16288,#16289,#13331,.T.);
#21189=EDGE_CURVE('',#15915,#16290,#13332,.T.);
#21190=EDGE_CURVE('',#16289,#16290,#13333,.T.);
#21191=EDGE_CURVE('',#16290,#16284,#13334,.T.);
#21192=EDGE_CURVE('',#16291,#16292,#13335,.T.);
#21193=EDGE_CURVE('',#16291,#16293,#13336,.T.);
#21194=EDGE_CURVE('',#16293,#16294,#13337,.T.);
#21195=EDGE_CURVE('',#16292,#16294,#13338,.T.);
#21196=EDGE_CURVE('',#16295,#16296,#13339,.T.);
#21197=EDGE_CURVE('',#16297,#16295,#9220,.T.);
#21198=EDGE_CURVE('',#16298,#16297,#13340,.T.);
#21199=EDGE_CURVE('',#16298,#16296,#9221,.T.);
#21200=EDGE_CURVE('',#16299,#16296,#13341,.T.);
#21201=EDGE_CURVE('',#16300,#16298,#13342,.T.);
#21202=EDGE_CURVE('',#16300,#16299,#9222,.T.);
#21203=EDGE_CURVE('',#16299,#16301,#13343,.T.);
#21204=EDGE_CURVE('',#16302,#16300,#13344,.T.);
#21205=EDGE_CURVE('',#16302,#16301,#9223,.T.);
#21206=EDGE_CURVE('',#16296,#16303,#2003,.T.);
#21207=EDGE_CURVE('',#16304,#16303,#13345,.T.);
#21208=EDGE_CURVE('',#16295,#16304,#13346,.T.);
#21209=EDGE_CURVE('',#16299,#16303,#2004,.T.);
#21210=EDGE_CURVE('',#16301,#16305,#13347,.T.);
#21211=EDGE_CURVE('',#16303,#16305,#13348,.T.);
#21212=EDGE_CURVE('',#16306,#16307,#13349,.T.);
#21213=EDGE_CURVE('',#16307,#16304,#13350,.T.);
#21214=EDGE_CURVE('',#16305,#16308,#13351,.T.);
#21215=EDGE_CURVE('',#16308,#16306,#13352,.T.);
#21216=EDGE_CURVE('',#16309,#16295,#13353,.T.);
#21217=EDGE_CURVE('',#16309,#16307,#13354,.T.);
#21218=EDGE_CURVE('',#16310,#16309,#9224,.T.);
#21219=EDGE_CURVE('',#16297,#16310,#13355,.T.);
#21220=EDGE_CURVE('',#16311,#16306,#2005,.T.);
#21221=EDGE_CURVE('',#16311,#16309,#13356,.T.);
#21222=EDGE_CURVE('',#16312,#16311,#9225,.T.);
#21223=EDGE_CURVE('',#16312,#16310,#13357,.T.);
#21224=EDGE_CURVE('',#16301,#16313,#13358,.T.);
#21225=EDGE_CURVE('',#16313,#16308,#13359,.T.);
#21226=EDGE_CURVE('',#16314,#16302,#13360,.T.);
#21227=EDGE_CURVE('',#16314,#16313,#9226,.T.);
#21228=EDGE_CURVE('',#16311,#16315,#13361,.T.);
#21229=EDGE_CURVE('',#16316,#16315,#9227,.T.);
#21230=EDGE_CURVE('',#16312,#16316,#13362,.T.);
#21231=EDGE_CURVE('',#16315,#16306,#2006,.T.);
#21232=EDGE_CURVE('',#16313,#16315,#13363,.T.);
#21233=EDGE_CURVE('',#16314,#16316,#13364,.T.);
#21234=EDGE_CURVE('',#16317,#16318,#9228,.T.);
#21235=EDGE_CURVE('',#16319,#16317,#13365,.T.);
#21236=EDGE_CURVE('',#16320,#16319,#9229,.T.);
#21237=EDGE_CURVE('',#16321,#16320,#13366,.T.);
#21238=EDGE_CURVE('',#16318,#16321,#13367,.T.);
#21239=EDGE_CURVE('',#16322,#16323,#2007,.T.);
#21240=EDGE_CURVE('',#16320,#16322,#2008,.T.);
#21241=EDGE_CURVE('',#16319,#16324,#13368,.T.);
#21242=EDGE_CURVE('',#16323,#16324,#9230,.T.);
#21243=EDGE_CURVE('',#16325,#16326,#9231,.T.);
#21244=EDGE_CURVE('',#16323,#16325,#9232,.T.);
#21245=EDGE_CURVE('',#16326,#16324,#9233,.T.);
#21246=EDGE_CURVE('',#16317,#16327,#13369,.T.);
#21247=EDGE_CURVE('',#16328,#16327,#13370,.T.);
#21248=EDGE_CURVE('',#16319,#16328,#13371,.T.);
#21249=EDGE_CURVE('',#16324,#16328,#13372,.T.);
#21250=EDGE_CURVE('',#16326,#16329,#13373,.T.);
#21251=EDGE_CURVE('',#16329,#16328,#9234,.T.);
#21252=EDGE_CURVE('',#16330,#16327,#9235,.T.);
#21253=EDGE_CURVE('',#16329,#16330,#13374,.T.);
#21254=EDGE_CURVE('',#16331,#16318,#2009,.T.);
#21255=EDGE_CURVE('',#16332,#16331,#9236,.T.);
#21256=EDGE_CURVE('',#16317,#16332,#13375,.T.);
#21257=EDGE_CURVE('',#16327,#16332,#13376,.T.);
#21258=EDGE_CURVE('',#16330,#16333,#13377,.T.);
#21259=EDGE_CURVE('',#16333,#16332,#9237,.T.);
#21260=EDGE_CURVE('',#16334,#16331,#9238,.T.);
#21261=EDGE_CURVE('',#16333,#16334,#9239,.T.);
#21262=EDGE_CURVE('',#16335,#16336,#9240,.T.);
#21263=EDGE_CURVE('',#16337,#16335,#13378,.T.);
#21264=EDGE_CURVE('',#16338,#16337,#9241,.T.);
#21265=EDGE_CURVE('',#16339,#16338,#13379,.T.);
#21266=EDGE_CURVE('',#16336,#16339,#13380,.T.);
#21267=EDGE_CURVE('',#16338,#16340,#2010,.T.);
#21268=EDGE_CURVE('',#16337,#16341,#13381,.T.);
#21269=EDGE_CURVE('',#16340,#16341,#9242,.T.);
#21270=EDGE_CURVE('',#16342,#16343,#9243,.T.);
#21271=EDGE_CURVE('',#16340,#16342,#9244,.T.);
#21272=EDGE_CURVE('',#16341,#16343,#9245,.T.);
#21273=EDGE_CURVE('',#16337,#16344,#13382,.T.);
#21274=EDGE_CURVE('',#16341,#16344,#13383,.T.);
#21275=EDGE_CURVE('',#16343,#16293,#13384,.T.);
#21276=EDGE_CURVE('',#16344,#16293,#9246,.T.);
#21277=EDGE_CURVE('',#16344,#16345,#13385,.T.);
#21278=EDGE_CURVE('',#16294,#16345,#9247,.T.);
#21279=EDGE_CURVE('',#16335,#16345,#13386,.T.);
#21280=EDGE_CURVE('',#16346,#16336,#2011,.T.);
#21281=EDGE_CURVE('',#16347,#16346,#2012,.T.);
#21282=EDGE_CURVE('',#16348,#16347,#9248,.T.);
#21283=EDGE_CURVE('',#16335,#16348,#13387,.T.);
#21284=EDGE_CURVE('',#16345,#16348,#13388,.T.);
#21285=EDGE_CURVE('',#16294,#16349,#13389,.T.);
#21286=EDGE_CURVE('',#16349,#16348,#9249,.T.);
#21287=EDGE_CURVE('',#16350,#16347,#9250,.T.);
#21288=EDGE_CURVE('',#16349,#16350,#9251,.T.);
#21289=EDGE_CURVE('',#16351,#16352,#9252,.T.);
#21290=EDGE_CURVE('',#16352,#16353,#9253,.T.);
#21291=EDGE_CURVE('',#16354,#16353,#9254,.T.);
#21292=EDGE_CURVE('',#16354,#16351,#9255,.T.);
#21293=EDGE_CURVE('',#16353,#16355,#2013,.T.);
#21294=EDGE_CURVE('',#16356,#16355,#9256,.T.);
#21295=EDGE_CURVE('',#16354,#16356,#13390,.T.);
#21296=EDGE_CURVE('',#16357,#16358,#9257,.T.);
#21297=EDGE_CURVE('',#16358,#16359,#13391,.T.);
#21298=EDGE_CURVE('',#16359,#16360,#13392,.T.);
#21299=EDGE_CURVE('',#16360,#16356,#13393,.T.);
#21300=EDGE_CURVE('',#16355,#16361,#13394,.T.);
#21301=EDGE_CURVE('',#16361,#16362,#13395,.T.);
#21302=EDGE_CURVE('',#16362,#16357,#13396,.T.);
#21303=EDGE_CURVE('',#16363,#16351,#13397,.T.);
#21304=EDGE_CURVE('',#16364,#16354,#13398,.T.);
#21305=EDGE_CURVE('',#16364,#16363,#9258,.T.);
#21306=EDGE_CURVE('',#16364,#16356,#13399,.T.);
#21307=EDGE_CURVE('',#16365,#16364,#13400,.T.);
#21308=EDGE_CURVE('',#16365,#16360,#13401,.T.);
#21309=EDGE_CURVE('',#16365,#16366,#9259,.T.);
#21310=EDGE_CURVE('',#16366,#16363,#13402,.T.);
#21311=EDGE_CURVE('',#16367,#16365,#13403,.T.);
#21312=EDGE_CURVE('',#16367,#16359,#13404,.T.);
#21313=EDGE_CURVE('',#16367,#16368,#9260,.T.);
#21314=EDGE_CURVE('',#16368,#16366,#13405,.T.);
#21315=EDGE_CURVE('',#16369,#16367,#13406,.T.);
#21316=EDGE_CURVE('',#16369,#16358,#13407,.T.);
#21317=EDGE_CURVE('',#16370,#16369,#9261,.T.);
#21318=EDGE_CURVE('',#16370,#16368,#13408,.T.);
#21319=EDGE_CURVE('',#16357,#16371,#2014,.T.);
#21320=EDGE_CURVE('',#16371,#16372,#9262,.T.);
#21321=EDGE_CURVE('',#16372,#16358,#13409,.T.);
#21322=EDGE_CURVE('',#16372,#16369,#13410,.T.);
#21323=EDGE_CURVE('',#16373,#16370,#13411,.T.);
#21324=EDGE_CURVE('',#16373,#16372,#9263,.T.);
#21325=EDGE_CURVE('',#16371,#16374,#9264,.T.);
#21326=EDGE_CURVE('',#16374,#16373,#9265,.T.);
#21327=EDGE_CURVE('',#16375,#16376,#13412,.T.);
#21328=EDGE_CURVE('',#16377,#16376,#13413,.T.);
#21329=EDGE_CURVE('',#16377,#16378,#13414,.T.);
#21330=EDGE_CURVE('',#16379,#16378,#13415,.T.);
#21331=EDGE_CURVE('',#16379,#16380,#13416,.T.);
#21332=EDGE_CURVE('',#16375,#16380,#13417,.T.);
#21333=EDGE_CURVE('',#16381,#16325,#13418,.T.);
#21334=EDGE_CURVE('',#16382,#16326,#13419,.T.);
#21335=EDGE_CURVE('',#16381,#16382,#9266,.T.);
#21336=EDGE_CURVE('',#16383,#16329,#13420,.T.);
#21337=EDGE_CURVE('',#16382,#16383,#13421,.T.);
#21338=EDGE_CURVE('',#16384,#16330,#13422,.T.);
#21339=EDGE_CURVE('',#16383,#16384,#13423,.T.);
#21340=EDGE_CURVE('',#16385,#16333,#13424,.T.);
#21341=EDGE_CURVE('',#16384,#16385,#13425,.T.);
#21342=EDGE_CURVE('',#16386,#16334,#13426,.T.);
#21343=EDGE_CURVE('',#16385,#16386,#9267,.T.);
#21344=EDGE_CURVE('',#16387,#16342,#13427,.T.);
#21345=EDGE_CURVE('',#16388,#16343,#13428,.T.);
#21346=EDGE_CURVE('',#16387,#16388,#9268,.T.);
#21347=EDGE_CURVE('',#16388,#16291,#13429,.T.);
#21348=EDGE_CURVE('',#16389,#16349,#13430,.T.);
#21349=EDGE_CURVE('',#16292,#16389,#13431,.T.);
#21350=EDGE_CURVE('',#16390,#16350,#13432,.T.);
#21351=EDGE_CURVE('',#16389,#16390,#9269,.T.);
#21352=EDGE_CURVE('',#16351,#16391,#13433,.T.);
#21353=EDGE_CURVE('',#16391,#16392,#9270,.T.);
#21354=EDGE_CURVE('',#16352,#16392,#13434,.T.);
#21355=EDGE_CURVE('',#16363,#16393,#13435,.T.);
#21356=EDGE_CURVE('',#16393,#16391,#13436,.T.);
#21357=EDGE_CURVE('',#16366,#16394,#13437,.T.);
#21358=EDGE_CURVE('',#16394,#16393,#13438,.T.);
#21359=EDGE_CURVE('',#16368,#16395,#13439,.T.);
#21360=EDGE_CURVE('',#16395,#16394,#13440,.T.);
#21361=EDGE_CURVE('',#16370,#16396,#13441,.T.);
#21362=EDGE_CURVE('',#16396,#16395,#13442,.T.);
#21363=EDGE_CURVE('',#16373,#16397,#13443,.T.);
#21364=EDGE_CURVE('',#16397,#16396,#13444,.T.);
#21365=EDGE_CURVE('',#16374,#16398,#13445,.T.);
#21366=EDGE_CURVE('',#16398,#16397,#9271,.T.);
#21367=EDGE_CURVE('',#16392,#16390,#13446,.T.);
#21368=EDGE_CURVE('',#16381,#16398,#13447,.T.);
#21369=EDGE_CURVE('',#16387,#16386,#13448,.T.);
#21370=EDGE_CURVE('',#16399,#16350,#13449,.T.);
#21371=EDGE_CURVE('',#16390,#16399,#13450,.T.);
#21372=EDGE_CURVE('',#16400,#16390,#13451,.T.);
#21373=EDGE_CURVE('',#16392,#16401,#13452,.T.);
#21374=EDGE_CURVE('',#16402,#16401,#13453,.T.);
#21375=EDGE_CURVE('',#16403,#16402,#13454,.T.);
#21376=EDGE_CURVE('',#16352,#16402,#13455,.T.);
#21377=EDGE_CURVE('',#16401,#16399,#13456,.T.);
#21378=EDGE_CURVE('',#16404,#16347,#13457,.T.);
#21379=EDGE_CURVE('',#16405,#16346,#13458,.T.);
#21380=EDGE_CURVE('',#16404,#16405,#2015,.T.);
#21381=EDGE_CURVE('',#16399,#16404,#9272,.T.);
#21382=EDGE_CURVE('',#16401,#16406,#9273,.T.);
#21383=EDGE_CURVE('',#16353,#16406,#2016,.T.);
#21384=EDGE_CURVE('',#16406,#16407,#2017,.T.);
#21385=EDGE_CURVE('',#16355,#16407,#706,.T.);
#21386=EDGE_CURVE('',#16407,#16408,#13459,.T.);
#21387=EDGE_CURVE('',#16361,#16408,#13460,.T.);
#21388=EDGE_CURVE('',#16405,#16380,#9274,.T.);
#21389=EDGE_CURVE('',#16408,#16379,#9275,.T.);
#21390=EDGE_CURVE('',#16408,#16409,#13461,.T.);
#21391=EDGE_CURVE('',#16362,#16409,#13462,.T.);
#21392=EDGE_CURVE('',#16409,#16378,#9276,.T.);
#21393=EDGE_CURVE('',#16410,#16411,#13463,.T.);
#21394=EDGE_CURVE('',#16412,#16411,#13464,.T.);
#21395=EDGE_CURVE('',#16411,#16325,#13465,.T.);
#21396=EDGE_CURVE('',#16410,#16381,#13466,.T.);
#21397=EDGE_CURVE('',#16374,#16413,#13467,.T.);
#21398=EDGE_CURVE('',#16413,#16398,#13468,.T.);
#21399=EDGE_CURVE('',#16414,#16398,#13469,.T.);
#21400=EDGE_CURVE('',#16410,#16413,#13470,.T.);
#21401=EDGE_CURVE('',#16415,#16322,#13471,.T.);
#21402=EDGE_CURVE('',#16416,#16323,#13472,.T.);
#21403=EDGE_CURVE('',#16415,#16416,#2018,.T.);
#21404=EDGE_CURVE('',#16416,#16410,#9277,.T.);
#21405=EDGE_CURVE('',#16409,#16417,#13473,.T.);
#21406=EDGE_CURVE('',#16357,#16417,#707,.T.);
#21407=EDGE_CURVE('',#16417,#16418,#2019,.T.);
#21408=EDGE_CURVE('',#16371,#16418,#2020,.T.);
#21409=EDGE_CURVE('',#16418,#16413,#9278,.T.);
#21410=EDGE_CURVE('',#16415,#16377,#9279,.T.);
#21411=EDGE_CURVE('',#16419,#16336,#13474,.T.);
#21412=EDGE_CURVE('',#16420,#16339,#13475,.T.);
#21413=EDGE_CURVE('',#16419,#16420,#13476,.T.);
#21414=EDGE_CURVE('',#16405,#16419,#2021,.T.);
#21415=EDGE_CURVE('',#16420,#16375,#9280,.T.);
#21416=EDGE_CURVE('',#16421,#16321,#13477,.T.);
#21417=EDGE_CURVE('',#16422,#16320,#708,.T.);
#21418=EDGE_CURVE('',#16421,#16422,#13478,.T.);
#21419=EDGE_CURVE('',#16422,#16415,#2022,.T.);
#21420=EDGE_CURVE('',#16421,#16376,#9281,.T.);
#21421=EDGE_CURVE('',#16423,#16334,#13479,.T.);
#21422=EDGE_CURVE('',#16386,#16423,#13480,.T.);
#21423=EDGE_CURVE('',#16424,#16386,#13481,.T.);
#21424=EDGE_CURVE('',#16425,#16426,#13482,.T.);
#21425=EDGE_CURVE('',#16427,#16426,#13483,.T.);
#21426=EDGE_CURVE('',#16426,#16342,#13484,.T.);
#21427=EDGE_CURVE('',#16425,#16387,#13485,.T.);
#21428=EDGE_CURVE('',#16425,#16423,#13486,.T.);
#21429=EDGE_CURVE('',#16428,#16318,#13487,.T.);
#21430=EDGE_CURVE('',#16428,#16421,#13488,.T.);
#21431=EDGE_CURVE('',#16429,#16331,#2023,.T.);
#21432=EDGE_CURVE('',#16429,#16428,#2024,.T.);
#21433=EDGE_CURVE('',#16423,#16429,#9282,.T.);
#21434=EDGE_CURVE('',#16430,#16338,#709,.T.);
#21435=EDGE_CURVE('',#16420,#16430,#13489,.T.);
#21436=EDGE_CURVE('',#16431,#16340,#2025,.T.);
#21437=EDGE_CURVE('',#16430,#16431,#2026,.T.);
#21438=EDGE_CURVE('',#16431,#16425,#9283,.T.);
#21439=EDGE_CURVE('',#16432,#16433,#13490,.T.);
#21440=EDGE_CURVE('',#16433,#16434,#13491,.T.);
#21441=EDGE_CURVE('',#16434,#16435,#13492,.T.);
#21442=EDGE_CURVE('',#16436,#16435,#13493,.T.);
#21443=EDGE_CURVE('',#16437,#16436,#13494,.T.);
#21444=EDGE_CURVE('',#16437,#16432,#13495,.T.);
#21445=EDGE_CURVE('',#16438,#16439,#13496,.T.);
#21446=EDGE_CURVE('',#16439,#16440,#9284,.T.);
#21447=EDGE_CURVE('',#16440,#16441,#13497,.T.);
#21448=EDGE_CURVE('',#16441,#16442,#9285,.T.);
#21449=EDGE_CURVE('',#16442,#16438,#9286,.T.);
#21450=EDGE_CURVE('',#16443,#16442,#9287,.T.);
#21451=EDGE_CURVE('',#16443,#16444,#9288,.T.);
#21452=EDGE_CURVE('',#16444,#16438,#9289,.T.);
#21453=EDGE_CURVE('',#16445,#16441,#9290,.T.);
#21454=EDGE_CURVE('',#16445,#16443,#9291,.T.);
#21455=EDGE_CURVE('',#16446,#16440,#9292,.T.);
#21456=EDGE_CURVE('',#16446,#16445,#13498,.T.);
#21457=EDGE_CURVE('',#16447,#16439,#9293,.T.);
#21458=EDGE_CURVE('',#16447,#16446,#9294,.T.);
#21459=EDGE_CURVE('',#16448,#16449,#9295,.T.);
#21460=EDGE_CURVE('',#16450,#16448,#9296,.T.);
#21461=EDGE_CURVE('',#16450,#16451,#13499,.T.);
#21462=EDGE_CURVE('',#16449,#16451,#9297,.T.);
#21463=EDGE_CURVE('',#16452,#16453,#9298,.T.);
#21464=EDGE_CURVE('',#16453,#16450,#9299,.T.);
#21465=EDGE_CURVE('',#16452,#16448,#9300,.T.);
#21466=EDGE_CURVE('',#16454,#16449,#9301,.T.);
#21467=EDGE_CURVE('',#16454,#16452,#9302,.T.);
#21468=EDGE_CURVE('',#16455,#16451,#9303,.T.);
#21469=EDGE_CURVE('',#16455,#16454,#9304,.T.);
#21470=EDGE_CURVE('',#16456,#16456,#13500,.T.);
#21471=EDGE_CURVE('',#16456,#16457,#9305,.T.);
#21472=EDGE_CURVE('',#16457,#16457,#13501,.T.);
#21473=EDGE_CURVE('',#16433,#16458,#9306,.T.);
#21474=EDGE_CURVE('',#16459,#16458,#13502,.T.);
#21475=EDGE_CURVE('',#16460,#16459,#9307,.T.);
#21476=EDGE_CURVE('',#16460,#16461,#13503,.T.);
#21477=EDGE_CURVE('',#16462,#16461,#9308,.T.);
#21478=EDGE_CURVE('',#16463,#16462,#13504,.T.);
#21479=EDGE_CURVE('',#16464,#16463,#13505,.T.);
#21480=EDGE_CURVE('',#16464,#16465,#9309,.T.);
#21481=EDGE_CURVE('',#16465,#16466,#13506,.T.);
#21482=EDGE_CURVE('',#16467,#16466,#13507,.T.);
#21483=EDGE_CURVE('',#16467,#16468,#9310,.T.);
#21484=EDGE_CURVE('',#16468,#16469,#13508,.T.);
#21485=EDGE_CURVE('',#16470,#16469,#13509,.T.);
#21486=EDGE_CURVE('',#16471,#16470,#13510,.T.);
#21487=EDGE_CURVE('',#16471,#16472,#13511,.T.);
#21488=EDGE_CURVE('',#16472,#16473,#13512,.T.);
#21489=EDGE_CURVE('',#16474,#16473,#13513,.T.);
#21490=EDGE_CURVE('',#16474,#16475,#13514,.T.);
#21491=EDGE_CURVE('',#16476,#16475,#9311,.T.);
#21492=EDGE_CURVE('',#16476,#16477,#13515,.T.);
#21493=EDGE_CURVE('',#16477,#16478,#13516,.T.);
#21494=EDGE_CURVE('',#16478,#16479,#9312,.T.);
#21495=EDGE_CURVE('',#16480,#16479,#13517,.T.);
#21496=EDGE_CURVE('',#16481,#16480,#13518,.T.);
#21497=EDGE_CURVE('',#16481,#16482,#9313,.T.);
#21498=EDGE_CURVE('',#16482,#16483,#13519,.T.);
#21499=EDGE_CURVE('',#16483,#16484,#9314,.T.);
#21500=EDGE_CURVE('',#16485,#16484,#13520,.T.);
#21501=EDGE_CURVE('',#16485,#16434,#9315,.T.);
#21502=EDGE_CURVE('',#16486,#16487,#13521,.T.);
#21503=EDGE_CURVE('',#16487,#16437,#2027,.T.);
#21504=EDGE_CURVE('',#16436,#16486,#2028,.T.);
#21505=EDGE_CURVE('',#16488,#16445,#13522,.T.);
#21506=EDGE_CURVE('',#16488,#16489,#9316,.T.);
#21507=EDGE_CURVE('',#16490,#16489,#13523,.T.);
#21508=EDGE_CURVE('',#16490,#16491,#9317,.T.);
#21509=EDGE_CURVE('',#16491,#16492,#9318,.T.);
#21510=EDGE_CURVE('',#16492,#16493,#9319,.T.);
#21511=EDGE_CURVE('',#16494,#16493,#9320,.T.);
#21512=EDGE_CURVE('',#16494,#16495,#9321,.T.);
#21513=EDGE_CURVE('',#16496,#16495,#13524,.T.);
#21514=EDGE_CURVE('',#16497,#16496,#9322,.T.);
#21515=EDGE_CURVE('',#16498,#16497,#13525,.T.);
#21516=EDGE_CURVE('',#16445,#16498,#9323,.T.);
#21517=EDGE_CURVE('',#16447,#16453,#13526,.T.);
#21518=EDGE_CURVE('',#16455,#16499,#13527,.T.);
#21519=EDGE_CURVE('',#16499,#16444,#13528,.T.);
#21520=EDGE_CURVE('',#16500,#16501,#9324,.T.);
#21521=EDGE_CURVE('',#16495,#16500,#9325,.T.);
#21522=EDGE_CURVE('',#16494,#16502,#9326,.T.);
#21523=EDGE_CURVE('',#16503,#16502,#9327,.T.);
#21524=EDGE_CURVE('',#16491,#16503,#9328,.T.);
#21525=EDGE_CURVE('',#16490,#16501,#9329,.T.);
#21526=EDGE_CURVE('',#16504,#16505,#2029,.T.);
#21527=EDGE_CURVE('',#16505,#16504,#2030,.T.);
#21528=EDGE_CURVE('',#16505,#16506,#9330,.T.);
#21529=EDGE_CURVE('',#16506,#16506,#13529,.T.);
#21530=EDGE_CURVE('',#16507,#16508,#9331,.T.);
#21531=EDGE_CURVE('',#16507,#16509,#9332,.T.);
#21532=EDGE_CURVE('',#16509,#16510,#9333,.T.);
#21533=EDGE_CURVE('',#16510,#16511,#13530,.T.);
#21534=EDGE_CURVE('',#16512,#16511,#9334,.T.);
#21535=EDGE_CURVE('',#16512,#16508,#9335,.T.);
#21536=EDGE_CURVE('',#16512,#16513,#9336,.T.);
#21537=EDGE_CURVE('',#16508,#16513,#13531,.T.);
#21538=EDGE_CURVE('',#16513,#16514,#9337,.T.);
#21539=EDGE_CURVE('',#16514,#16511,#9338,.T.);
#21540=EDGE_CURVE('',#16515,#16514,#2031,.T.);
#21541=EDGE_CURVE('',#16510,#16515,#9339,.T.);
#21542=EDGE_CURVE('',#16515,#16516,#9340,.T.);
#21543=EDGE_CURVE('',#16509,#16516,#9341,.T.);
#21544=EDGE_CURVE('',#16507,#16516,#13532,.T.);
#21545=EDGE_CURVE('',#16517,#16518,#13533,.T.);
#21546=EDGE_CURVE('',#16518,#16519,#9342,.T.);
#21547=EDGE_CURVE('',#16519,#16517,#9343,.T.);
#21548=EDGE_CURVE('',#16520,#16518,#9344,.T.);
#21549=EDGE_CURVE('',#16521,#16520,#9345,.T.);
#21550=EDGE_CURVE('',#16521,#16522,#13534,.T.);
#21551=EDGE_CURVE('',#16522,#16519,#9346,.T.);
#21552=EDGE_CURVE('',#16517,#16523,#9347,.T.);
#21553=EDGE_CURVE('',#16523,#16522,#9348,.T.);
#21554=EDGE_CURVE('',#16521,#16524,#9349,.T.);
#21555=EDGE_CURVE('',#16524,#16523,#2032,.T.);
#21556=EDGE_CURVE('',#16520,#16524,#13535,.T.);
#21557=EDGE_CURVE('',#16525,#16526,#9350,.T.);
#21558=EDGE_CURVE('',#16527,#16526,#9351,.T.);
#21559=EDGE_CURVE('',#16528,#16527,#9352,.T.);
#21560=EDGE_CURVE('',#16528,#16529,#13536,.T.);
#21561=EDGE_CURVE('',#16525,#16529,#9353,.T.);
#21562=EDGE_CURVE('',#16530,#16525,#13537,.T.);
#21563=EDGE_CURVE('',#16529,#16530,#9354,.T.);
#21564=EDGE_CURVE('',#16531,#16528,#9355,.T.);
#21565=EDGE_CURVE('',#16530,#16531,#2033,.T.);
#21566=EDGE_CURVE('',#16527,#16532,#9356,.T.);
#21567=EDGE_CURVE('',#16532,#16531,#9357,.T.);
#21568=EDGE_CURVE('',#16526,#16532,#13538,.T.);
#21569=EDGE_CURVE('',#16533,#16534,#13539,.T.);
#21570=EDGE_CURVE('',#16535,#16534,#9358,.T.);
#21571=EDGE_CURVE('',#16535,#16533,#9359,.T.);
#21572=EDGE_CURVE('',#16534,#16536,#9360,.T.);
#21573=EDGE_CURVE('',#16536,#16537,#9361,.T.);
#21574=EDGE_CURVE('',#16537,#16538,#9362,.T.);
#21575=EDGE_CURVE('',#16538,#16539,#13540,.T.);
#21576=EDGE_CURVE('',#16535,#16539,#9363,.T.);
#21577=EDGE_CURVE('',#16539,#16540,#9364,.T.);
#21578=EDGE_CURVE('',#16540,#16533,#9365,.T.);
#21579=EDGE_CURVE('',#16541,#16540,#2034,.T.);
#21580=EDGE_CURVE('',#16541,#16538,#9366,.T.);
#21581=EDGE_CURVE('',#16542,#16541,#9367,.T.);
#21582=EDGE_CURVE('',#16537,#16542,#9368,.T.);
#21583=EDGE_CURVE('',#16542,#16536,#13541,.T.);
#21584=EDGE_CURVE('',#16543,#16544,#13542,.T.);
#21585=EDGE_CURVE('',#16543,#16544,#9369,.T.);
#21586=EDGE_CURVE('',#16545,#16546,#13543,.T.);
#21587=EDGE_CURVE('',#16546,#16545,#9370,.T.);
#21588=EDGE_CURVE('',#16546,#16482,#9371,.T.);
#21589=EDGE_CURVE('',#16483,#16545,#9372,.T.);
#21590=EDGE_CURVE('',#16543,#16461,#9373,.T.);
#21591=EDGE_CURVE('',#16460,#16544,#9374,.T.);
#21592=EDGE_CURVE('',#16547,#16548,#13544,.T.);
#21593=EDGE_CURVE('',#16549,#16547,#13545,.T.);
#21594=EDGE_CURVE('',#16550,#16549,#9375,.T.);
#21595=EDGE_CURVE('',#16548,#16550,#13546,.T.);
#21596=EDGE_CURVE('',#16461,#16460,#9376,.T.);
#21597=EDGE_CURVE('',#16482,#16483,#9377,.T.);
#21598=EDGE_CURVE('',#16551,#16552,#13547,.T.);
#21599=EDGE_CURVE('',#16551,#16547,#9378,.T.);
#21600=EDGE_CURVE('',#16548,#16552,#9379,.T.);
#21601=EDGE_CURVE('',#16552,#16553,#13548,.T.);
#21602=EDGE_CURVE('',#16550,#16553,#9380,.T.);
#21603=EDGE_CURVE('',#16549,#16554,#9381,.T.);
#21604=EDGE_CURVE('',#16553,#16554,#9382,.T.);
#21605=EDGE_CURVE('',#16554,#16551,#13549,.T.);
#21606=EDGE_CURVE('',#16555,#16555,#13550,.T.);
#21607=EDGE_CURVE('',#16555,#16556,#9383,.T.);
#21608=EDGE_CURVE('',#16556,#16557,#2035,.T.);
#21609=EDGE_CURVE('',#16557,#16556,#2036,.T.);
#21610=EDGE_CURVE('',#16558,#16559,#13551,.T.);
#21611=EDGE_CURVE('',#16560,#16559,#9384,.T.);
#21612=EDGE_CURVE('',#16560,#16558,#9385,.T.);
#21613=EDGE_CURVE('',#16559,#16561,#9386,.T.);
#21614=EDGE_CURVE('',#16561,#16562,#9387,.T.);
#21615=EDGE_CURVE('',#16560,#16562,#9388,.T.);
#21616=EDGE_CURVE('',#16563,#16561,#2037,.T.);
#21617=EDGE_CURVE('',#16564,#16563,#9389,.T.);
#21618=EDGE_CURVE('',#16564,#16562,#13552,.T.);
#21619=EDGE_CURVE('',#16565,#16566,#9390,.T.);
#21620=EDGE_CURVE('',#16566,#16564,#9391,.T.);
#21621=EDGE_CURVE('',#16563,#16565,#9392,.T.);
#21622=EDGE_CURVE('',#16567,#16568,#9393,.T.);
#21623=EDGE_CURVE('',#16569,#16567,#9394,.T.);
#21624=EDGE_CURVE('',#16570,#16569,#9395,.T.);
#21625=EDGE_CURVE('',#16568,#16570,#9396,.T.);
#21626=EDGE_CURVE('',#16571,#16567,#2038,.T.);
#21627=EDGE_CURVE('',#16571,#16572,#9397,.T.);
#21628=EDGE_CURVE('',#16572,#16569,#13553,.T.);
#21629=EDGE_CURVE('',#16573,#16572,#9398,.T.);
#21630=EDGE_CURVE('',#16574,#16571,#9399,.T.);
#21631=EDGE_CURVE('',#16573,#16574,#9400,.T.);
#21632=EDGE_CURVE('',#16574,#16575,#13554,.T.);
#21633=EDGE_CURVE('',#16575,#16573,#9401,.T.);
#21634=EDGE_CURVE('',#16576,#16577,#9402,.T.);
#21635=EDGE_CURVE('',#16578,#16576,#13555,.T.);
#21636=EDGE_CURVE('',#16577,#16578,#9403,.T.);
#21637=EDGE_CURVE('',#16578,#16579,#2039,.T.);
#21638=EDGE_CURVE('',#16579,#16580,#9404,.T.);
#21639=EDGE_CURVE('',#16580,#16577,#13556,.T.);
#21640=EDGE_CURVE('',#16581,#16579,#9405,.T.);
#21641=EDGE_CURVE('',#16581,#16582,#9406,.T.);
#21642=EDGE_CURVE('',#16580,#16582,#9407,.T.);
#21643=EDGE_CURVE('',#16583,#16584,#9408,.T.);
#21644=EDGE_CURVE('',#16583,#16585,#9409,.T.);
#21645=EDGE_CURVE('',#16584,#16585,#13557,.T.);
#21646=EDGE_CURVE('',#16586,#16587,#9410,.T.);
#21647=EDGE_CURVE('',#16585,#16586,#2040,.T.);
#21648=EDGE_CURVE('',#16583,#16587,#13558,.T.);
#21649=EDGE_CURVE('',#16587,#16588,#9411,.T.);
#21650=EDGE_CURVE('',#16589,#16588,#9412,.T.);
#21651=EDGE_CURVE('',#16589,#16586,#9413,.T.);
#21652=EDGE_CURVE('',#16590,#16500,#13559,.T.);
#21653=EDGE_CURVE('',#16591,#16501,#13560,.T.);
#21654=EDGE_CURVE('',#16590,#16591,#9414,.T.);
#21655=EDGE_CURVE('',#16592,#16593,#9415,.T.);
#21656=EDGE_CURVE('',#16593,#16594,#13561,.T.);
#21657=EDGE_CURVE('',#16594,#16595,#13562,.T.);
#21658=EDGE_CURVE('',#16595,#16596,#9416,.T.);
#21659=EDGE_CURVE('',#16597,#16596,#13563,.T.);
#21660=EDGE_CURVE('',#16597,#16598,#13564,.T.);
#21661=EDGE_CURVE('',#16599,#16598,#13565,.T.);
#21662=EDGE_CURVE('',#16599,#16600,#13566,.T.);
#21663=EDGE_CURVE('',#16600,#16601,#13567,.T.);
#21664=EDGE_CURVE('',#16601,#16602,#13568,.T.);
#21665=EDGE_CURVE('',#16602,#16603,#9417,.T.);
#21666=EDGE_CURVE('',#16604,#16603,#13569,.T.);
#21667=EDGE_CURVE('',#16604,#16605,#13570,.T.);
#21668=EDGE_CURVE('',#16606,#16605,#13571,.T.);
#21669=EDGE_CURVE('',#16606,#16607,#9418,.T.);
#21670=EDGE_CURVE('',#16607,#16608,#13572,.T.);
#21671=EDGE_CURVE('',#16608,#16609,#13573,.T.);
#21672=EDGE_CURVE('',#16609,#16610,#13574,.T.);
#21673=EDGE_CURVE('',#16611,#16610,#13575,.T.);
#21674=EDGE_CURVE('',#16611,#16612,#13576,.T.);
#21675=EDGE_CURVE('',#16613,#16612,#13577,.T.);
#21676=EDGE_CURVE('',#16614,#16613,#9419,.T.);
#21677=EDGE_CURVE('',#16614,#16615,#13578,.T.);
#21678=EDGE_CURVE('',#16615,#16616,#13579,.T.);
#21679=EDGE_CURVE('',#16616,#16617,#9420,.T.);
#21680=EDGE_CURVE('',#16617,#16592,#13580,.T.);
#21681=EDGE_CURVE('',#16432,#16590,#13581,.T.);
#21682=EDGE_CURVE('',#16591,#16618,#13582,.T.);
#21683=EDGE_CURVE('',#16618,#16619,#9421,.T.);
#21684=EDGE_CURVE('',#16619,#16620,#13583,.T.);
#21685=EDGE_CURVE('',#16620,#16621,#9422,.T.);
#21686=EDGE_CURVE('',#16621,#16435,#13584,.T.);
#21687=EDGE_CURVE('',#16622,#16594,#9423,.T.);
#21688=EDGE_CURVE('',#16593,#16623,#9424,.T.);
#21689=EDGE_CURVE('',#16623,#16622,#13585,.T.);
#21690=EDGE_CURVE('',#16624,#16592,#9425,.T.);
#21691=EDGE_CURVE('',#16624,#16623,#9426,.T.);
#21692=EDGE_CURVE('',#16625,#16624,#13586,.T.);
#21693=EDGE_CURVE('',#16625,#16617,#9427,.T.);
#21694=EDGE_CURVE('',#16616,#16626,#9428,.T.);
#21695=EDGE_CURVE('',#16626,#16625,#9429,.T.);
#21696=EDGE_CURVE('',#16627,#16615,#9430,.T.);
#21697=EDGE_CURVE('',#16627,#16626,#13587,.T.);
#21698=EDGE_CURVE('',#16628,#16614,#9431,.T.);
#21699=EDGE_CURVE('',#16627,#16628,#13588,.T.);
#21700=EDGE_CURVE('',#16613,#16629,#9432,.T.);
#21701=EDGE_CURVE('',#16629,#16628,#9433,.T.);
#21702=EDGE_CURVE('',#16630,#16629,#13589,.T.);
#21703=EDGE_CURVE('',#16612,#16630,#9434,.T.);
#21704=EDGE_CURVE('',#16631,#16630,#13590,.T.);
#21705=EDGE_CURVE('',#16611,#16631,#9435,.T.);
#21706=EDGE_CURVE('',#16632,#16631,#13591,.T.);
#21707=EDGE_CURVE('',#16632,#16610,#9436,.T.);
#21708=EDGE_CURVE('',#16633,#16609,#9437,.T.);
#21709=EDGE_CURVE('',#16632,#16633,#13592,.T.);
#21710=EDGE_CURVE('',#16634,#16608,#9438,.T.);
#21711=EDGE_CURVE('',#16634,#16633,#13593,.T.);
#21712=EDGE_CURVE('',#16635,#16607,#9439,.T.);
#21713=EDGE_CURVE('',#16634,#16635,#13594,.T.);
#21714=EDGE_CURVE('',#16636,#16635,#9440,.T.);
#21715=EDGE_CURVE('',#16606,#16636,#9441,.T.);
#21716=EDGE_CURVE('',#16637,#16636,#13595,.T.);
#21717=EDGE_CURVE('',#16605,#16637,#9442,.T.);
#21718=EDGE_CURVE('',#16604,#16638,#9443,.T.);
#21719=EDGE_CURVE('',#16638,#16637,#13596,.T.);
#21720=EDGE_CURVE('',#16639,#16638,#13597,.T.);
#21721=EDGE_CURVE('',#16603,#16639,#9444,.T.);
#21722=EDGE_CURVE('',#16640,#16602,#9445,.T.);
#21723=EDGE_CURVE('',#16640,#16639,#9446,.T.);
#21724=EDGE_CURVE('',#16641,#16601,#9447,.T.);
#21725=EDGE_CURVE('',#16640,#16641,#13598,.T.);
#21726=EDGE_CURVE('',#16642,#16600,#9448,.T.);
#21727=EDGE_CURVE('',#16642,#16641,#13599,.T.);
#21728=EDGE_CURVE('',#16599,#16643,#9449,.T.);
#21729=EDGE_CURVE('',#16642,#16643,#13600,.T.);
#21730=EDGE_CURVE('',#16644,#16643,#13601,.T.);
#21731=EDGE_CURVE('',#16598,#16644,#9450,.T.);
#21732=EDGE_CURVE('',#16597,#16645,#9451,.T.);
#21733=EDGE_CURVE('',#16645,#16644,#13602,.T.);
#21734=EDGE_CURVE('',#16646,#16645,#13603,.T.);
#21735=EDGE_CURVE('',#16596,#16646,#9452,.T.);
#21736=EDGE_CURVE('',#16647,#16595,#9453,.T.);
#21737=EDGE_CURVE('',#16647,#16646,#9454,.T.);
#21738=EDGE_CURVE('',#16647,#16622,#13604,.T.);
#21739=EDGE_CURVE('',#16581,#16648,#13605,.T.);
#21740=EDGE_CURVE('',#16582,#16648,#9455,.T.);
#21741=EDGE_CURVE('',#16576,#16648,#9456,.T.);
#21742=EDGE_CURVE('',#16649,#16575,#9457,.T.);
#21743=EDGE_CURVE('',#16570,#16649,#9458,.T.);
#21744=EDGE_CURVE('',#16649,#16568,#13606,.T.);
#21745=EDGE_CURVE('',#16565,#16650,#13607,.T.);
#21746=EDGE_CURVE('',#16650,#16566,#9459,.T.);
#21747=EDGE_CURVE('',#16650,#16558,#9460,.T.);
#21748=EDGE_CURVE('',#16499,#16651,#9461,.T.);
#21749=EDGE_CURVE('',#16651,#16651,#13608,.T.);
#21750=EDGE_CURVE('',#16652,#16589,#13609,.T.);
#21751=EDGE_CURVE('',#16584,#16652,#9462,.T.);
#21752=EDGE_CURVE('',#16652,#16588,#9463,.T.);
#21753=EDGE_CURVE('',#16501,#16653,#13610,.T.);
#21754=EDGE_CURVE('',#16618,#16653,#13611,.T.);
#21755=EDGE_CURVE('',#16489,#16653,#9464,.T.);
#21756=EDGE_CURVE('',#16653,#16654,#9465,.T.);
#21757=EDGE_CURVE('',#16619,#16654,#13612,.T.);
#21758=EDGE_CURVE('',#16488,#16654,#9466,.T.);
#21759=EDGE_CURVE('',#16654,#16655,#13613,.T.);
#21760=EDGE_CURVE('',#16620,#16655,#13614,.T.);
#21761=EDGE_CURVE('',#16445,#16655,#9467,.T.);
#21762=EDGE_CURVE('',#16655,#16656,#9468,.T.);
#21763=EDGE_CURVE('',#16621,#16656,#13615,.T.);
#21764=EDGE_CURVE('',#16498,#16656,#9469,.T.);
#21765=EDGE_CURVE('',#16436,#16657,#13616,.T.);
#21766=EDGE_CURVE('',#16657,#16658,#2041,.T.);
#21767=EDGE_CURVE('',#16486,#16658,#13617,.T.);
#21768=EDGE_CURVE('',#16435,#16657,#13618,.T.);
#21769=EDGE_CURVE('',#16656,#16657,#13619,.T.);
#21770=EDGE_CURVE('',#16497,#16658,#9470,.T.);
#21771=EDGE_CURVE('',#16658,#16659,#13620,.T.);
#21772=EDGE_CURVE('',#16487,#16659,#13621,.T.);
#21773=EDGE_CURVE('',#16496,#16659,#9471,.T.);
#21774=EDGE_CURVE('',#16659,#16660,#2042,.T.);
#21775=EDGE_CURVE('',#16437,#16660,#13622,.T.);
#21776=EDGE_CURVE('',#16660,#16432,#13623,.T.);
#21777=EDGE_CURVE('',#16660,#16500,#13624,.T.);
#21778=EDGE_CURVE('',#16661,#16503,#9472,.T.);
#21779=EDGE_CURVE('',#16492,#16661,#9473,.T.);
#21780=EDGE_CURVE('',#16661,#16662,#9474,.T.);
#21781=EDGE_CURVE('',#16493,#16662,#9475,.T.);
#21782=EDGE_CURVE('',#16662,#16502,#9476,.T.);
#21783=ORIENTED_EDGE('',*,*,#16663,.F.);
#21784=ORIENTED_EDGE('',*,*,#16664,.T.);
#21785=ORIENTED_EDGE('',*,*,#16665,.T.);
#21786=ORIENTED_EDGE('',*,*,#16664,.F.);
#21787=ORIENTED_EDGE('',*,*,#16666,.F.);
#21788=ORIENTED_EDGE('',*,*,#16667,.F.);
#21789=ORIENTED_EDGE('',*,*,#16668,.T.);
#21790=ORIENTED_EDGE('',*,*,#16666,.T.);
#21791=ORIENTED_EDGE('',*,*,#16663,.T.);
#21792=ORIENTED_EDGE('',*,*,#16668,.F.);
#21793=ORIENTED_EDGE('',*,*,#16669,.F.);
#21794=ORIENTED_EDGE('',*,*,#16665,.F.);
#21795=ORIENTED_EDGE('',*,*,#16667,.T.);
#21796=ORIENTED_EDGE('',*,*,#16670,.T.);
#21797=ORIENTED_EDGE('',*,*,#16671,.F.);
#21798=ORIENTED_EDGE('',*,*,#16670,.F.);
#21799=ORIENTED_EDGE('',*,*,#16669,.T.);
#21800=ORIENTED_EDGE('',*,*,#16671,.T.);
#21801=ORIENTED_EDGE('',*,*,#16672,.F.);
#21802=ORIENTED_EDGE('',*,*,#16673,.T.);
#21803=ORIENTED_EDGE('',*,*,#16674,.T.);
#21804=ORIENTED_EDGE('',*,*,#16675,.F.);
#21805=ORIENTED_EDGE('',*,*,#16676,.T.);
#21806=ORIENTED_EDGE('',*,*,#16677,.T.);
#21807=ORIENTED_EDGE('',*,*,#16678,.T.);
#21808=ORIENTED_EDGE('',*,*,#16679,.T.);
#21809=ORIENTED_EDGE('',*,*,#16680,.T.);
#21810=ORIENTED_EDGE('',*,*,#16681,.T.);
#21811=ORIENTED_EDGE('',*,*,#16682,.T.);
#21812=ORIENTED_EDGE('',*,*,#16683,.T.);
#21813=ORIENTED_EDGE('',*,*,#16684,.T.);
#21814=ORIENTED_EDGE('',*,*,#16685,.T.);
#21815=ORIENTED_EDGE('',*,*,#16686,.T.);
#21816=ORIENTED_EDGE('',*,*,#16687,.T.);
#21817=ORIENTED_EDGE('',*,*,#16688,.T.);
#21818=ORIENTED_EDGE('',*,*,#16689,.T.);
#21819=ORIENTED_EDGE('',*,*,#16690,.T.);
#21820=ORIENTED_EDGE('',*,*,#16691,.T.);
#21821=ORIENTED_EDGE('',*,*,#16692,.T.);
#21822=ORIENTED_EDGE('',*,*,#16693,.T.);
#21823=ORIENTED_EDGE('',*,*,#16694,.T.);
#21824=ORIENTED_EDGE('',*,*,#16695,.T.);
#21825=ORIENTED_EDGE('',*,*,#16696,.T.);
#21826=ORIENTED_EDGE('',*,*,#16697,.T.);
#21827=ORIENTED_EDGE('',*,*,#16698,.T.);
#21828=ORIENTED_EDGE('',*,*,#16699,.T.);
#21829=ORIENTED_EDGE('',*,*,#16700,.T.);
#21830=ORIENTED_EDGE('',*,*,#16701,.T.);
#21831=ORIENTED_EDGE('',*,*,#16702,.T.);
#21832=ORIENTED_EDGE('',*,*,#16703,.T.);
#21833=ORIENTED_EDGE('',*,*,#16704,.T.);
#21834=ORIENTED_EDGE('',*,*,#16705,.T.);
#21835=ORIENTED_EDGE('',*,*,#16706,.T.);
#21836=ORIENTED_EDGE('',*,*,#16707,.T.);
#21837=ORIENTED_EDGE('',*,*,#16708,.T.);
#21838=ORIENTED_EDGE('',*,*,#16709,.T.);
#21839=ORIENTED_EDGE('',*,*,#16710,.T.);
#21840=ORIENTED_EDGE('',*,*,#16711,.T.);
#21841=ORIENTED_EDGE('',*,*,#16712,.T.);
#21842=ORIENTED_EDGE('',*,*,#16713,.T.);
#21843=ORIENTED_EDGE('',*,*,#16714,.T.);
#21844=ORIENTED_EDGE('',*,*,#16715,.T.);
#21845=ORIENTED_EDGE('',*,*,#16716,.T.);
#21846=ORIENTED_EDGE('',*,*,#16717,.F.);
#21847=ORIENTED_EDGE('',*,*,#16718,.F.);
#21848=ORIENTED_EDGE('',*,*,#16719,.F.);
#21849=ORIENTED_EDGE('',*,*,#16720,.T.);
#21850=ORIENTED_EDGE('',*,*,#16721,.F.);
#21851=ORIENTED_EDGE('',*,*,#16722,.T.);
#21852=ORIENTED_EDGE('',*,*,#16723,.F.);
#21853=ORIENTED_EDGE('',*,*,#16724,.T.);
#21854=ORIENTED_EDGE('',*,*,#16725,.F.);
#21855=ORIENTED_EDGE('',*,*,#16726,.T.);
#21856=ORIENTED_EDGE('',*,*,#16727,.F.);
#21857=ORIENTED_EDGE('',*,*,#16728,.F.);
#21858=ORIENTED_EDGE('',*,*,#16729,.T.);
#21859=ORIENTED_EDGE('',*,*,#16675,.T.);
#21860=ORIENTED_EDGE('',*,*,#16730,.F.);
#21861=ORIENTED_EDGE('',*,*,#16731,.T.);
#21862=ORIENTED_EDGE('',*,*,#16732,.F.);
#21863=ORIENTED_EDGE('',*,*,#16733,.F.);
#21864=ORIENTED_EDGE('',*,*,#16734,.T.);
#21865=ORIENTED_EDGE('',*,*,#16735,.F.);
#21866=ORIENTED_EDGE('',*,*,#16736,.T.);
#21867=ORIENTED_EDGE('',*,*,#16737,.F.);
#21868=ORIENTED_EDGE('',*,*,#16738,.T.);
#21869=ORIENTED_EDGE('',*,*,#16739,.T.);
#21870=ORIENTED_EDGE('',*,*,#16740,.T.);
#21871=ORIENTED_EDGE('',*,*,#16741,.F.);
#21872=ORIENTED_EDGE('',*,*,#16742,.T.);
#21873=ORIENTED_EDGE('',*,*,#16743,.F.);
#21874=ORIENTED_EDGE('',*,*,#16744,.T.);
#21875=ORIENTED_EDGE('',*,*,#16745,.T.);
#21876=ORIENTED_EDGE('',*,*,#16746,.F.);
#21877=ORIENTED_EDGE('',*,*,#16747,.F.);
#21878=ORIENTED_EDGE('',*,*,#16748,.F.);
#21879=ORIENTED_EDGE('',*,*,#16749,.T.);
#21880=ORIENTED_EDGE('',*,*,#16750,.F.);
#21881=ORIENTED_EDGE('',*,*,#16673,.F.);
#21882=ORIENTED_EDGE('',*,*,#16751,.T.);
#21883=ORIENTED_EDGE('',*,*,#16752,.T.);
#21884=ORIENTED_EDGE('',*,*,#16753,.F.);
#21885=ORIENTED_EDGE('',*,*,#16754,.F.);
#21886=ORIENTED_EDGE('',*,*,#16755,.T.);
#21887=ORIENTED_EDGE('',*,*,#16756,.F.);
#21888=ORIENTED_EDGE('',*,*,#16757,.F.);
#21889=ORIENTED_EDGE('',*,*,#16725,.T.);
#21890=ORIENTED_EDGE('',*,*,#16758,.T.);
#21891=ORIENTED_EDGE('',*,*,#16759,.F.);
#21892=ORIENTED_EDGE('',*,*,#16760,.F.);
#21893=ORIENTED_EDGE('',*,*,#16755,.F.);
#21894=ORIENTED_EDGE('',*,*,#16724,.F.);
#21895=ORIENTED_EDGE('',*,*,#16761,.T.);
#21896=ORIENTED_EDGE('',*,*,#16762,.F.);
#21897=ORIENTED_EDGE('',*,*,#16758,.F.);
#21898=ORIENTED_EDGE('',*,*,#16723,.T.);
#21899=ORIENTED_EDGE('',*,*,#16763,.T.);
#21900=ORIENTED_EDGE('',*,*,#16764,.F.);
#21901=ORIENTED_EDGE('',*,*,#16765,.F.);
#21902=ORIENTED_EDGE('',*,*,#16766,.F.);
#21903=ORIENTED_EDGE('',*,*,#16761,.F.);
#21904=ORIENTED_EDGE('',*,*,#16722,.F.);
#21905=ORIENTED_EDGE('',*,*,#16767,.T.);
#21906=ORIENTED_EDGE('',*,*,#16768,.F.);
#21907=ORIENTED_EDGE('',*,*,#16769,.F.);
#21908=ORIENTED_EDGE('',*,*,#16770,.F.);
#21909=ORIENTED_EDGE('',*,*,#16771,.F.);
#21910=ORIENTED_EDGE('',*,*,#16763,.F.);
#21911=ORIENTED_EDGE('',*,*,#16721,.T.);
#21912=ORIENTED_EDGE('',*,*,#16720,.F.);
#21913=ORIENTED_EDGE('',*,*,#16772,.T.);
#21914=ORIENTED_EDGE('',*,*,#16773,.F.);
#21915=ORIENTED_EDGE('',*,*,#16774,.F.);
#21916=ORIENTED_EDGE('',*,*,#16767,.F.);
#21917=ORIENTED_EDGE('',*,*,#16775,.T.);
#21918=ORIENTED_EDGE('',*,*,#16776,.F.);
#21919=ORIENTED_EDGE('',*,*,#16777,.F.);
#21920=ORIENTED_EDGE('',*,*,#16778,.F.);
#21921=ORIENTED_EDGE('',*,*,#16779,.F.);
#21922=ORIENTED_EDGE('',*,*,#16772,.F.);
#21923=ORIENTED_EDGE('',*,*,#16719,.T.);
#21924=ORIENTED_EDGE('',*,*,#16780,.T.);
#21925=ORIENTED_EDGE('',*,*,#16781,.T.);
#21926=ORIENTED_EDGE('',*,*,#16782,.F.);
#21927=ORIENTED_EDGE('',*,*,#16775,.F.);
#21928=ORIENTED_EDGE('',*,*,#16718,.T.);
#21929=ORIENTED_EDGE('',*,*,#16783,.T.);
#21930=ORIENTED_EDGE('',*,*,#16784,.F.);
#21931=ORIENTED_EDGE('',*,*,#16785,.T.);
#21932=ORIENTED_EDGE('',*,*,#16780,.F.);
#21933=ORIENTED_EDGE('',*,*,#16717,.T.);
#21934=ORIENTED_EDGE('',*,*,#16757,.T.);
#21935=ORIENTED_EDGE('',*,*,#16786,.F.);
#21936=ORIENTED_EDGE('',*,*,#16787,.F.);
#21937=ORIENTED_EDGE('',*,*,#16788,.F.);
#21938=ORIENTED_EDGE('',*,*,#16783,.F.);
#21939=ORIENTED_EDGE('',*,*,#16716,.F.);
#21940=ORIENTED_EDGE('',*,*,#16743,.T.);
#21941=ORIENTED_EDGE('',*,*,#16789,.T.);
#21942=ORIENTED_EDGE('',*,*,#16790,.T.);
#21943=ORIENTED_EDGE('',*,*,#16791,.T.);
#21944=ORIENTED_EDGE('',*,*,#16792,.F.);
#21945=ORIENTED_EDGE('',*,*,#16742,.F.);
#21946=ORIENTED_EDGE('',*,*,#16793,.T.);
#21947=ORIENTED_EDGE('',*,*,#16794,.T.);
#21948=ORIENTED_EDGE('',*,*,#16789,.F.);
#21949=ORIENTED_EDGE('',*,*,#16741,.T.);
#21950=ORIENTED_EDGE('',*,*,#16795,.T.);
#21951=ORIENTED_EDGE('',*,*,#16796,.T.);
#21952=ORIENTED_EDGE('',*,*,#16797,.T.);
#21953=ORIENTED_EDGE('',*,*,#16798,.T.);
#21954=ORIENTED_EDGE('',*,*,#16793,.F.);
#21955=ORIENTED_EDGE('',*,*,#16740,.F.);
#21956=ORIENTED_EDGE('',*,*,#16799,.T.);
#21957=ORIENTED_EDGE('',*,*,#16800,.F.);
#21958=ORIENTED_EDGE('',*,*,#16801,.T.);
#21959=ORIENTED_EDGE('',*,*,#16795,.F.);
#21960=ORIENTED_EDGE('',*,*,#16739,.F.);
#21961=ORIENTED_EDGE('',*,*,#16802,.T.);
#21962=ORIENTED_EDGE('',*,*,#16803,.T.);
#21963=ORIENTED_EDGE('',*,*,#16804,.F.);
#21964=ORIENTED_EDGE('',*,*,#16799,.F.);
#21965=ORIENTED_EDGE('',*,*,#16738,.F.);
#21966=ORIENTED_EDGE('',*,*,#16805,.T.);
#21967=ORIENTED_EDGE('',*,*,#16806,.T.);
#21968=ORIENTED_EDGE('',*,*,#16807,.T.);
#21969=ORIENTED_EDGE('',*,*,#16808,.T.);
#21970=ORIENTED_EDGE('',*,*,#16809,.T.);
#21971=ORIENTED_EDGE('',*,*,#16802,.F.);
#21972=ORIENTED_EDGE('',*,*,#16810,.T.);
#21973=ORIENTED_EDGE('',*,*,#16811,.T.);
#21974=ORIENTED_EDGE('',*,*,#16812,.T.);
#21975=ORIENTED_EDGE('',*,*,#16805,.F.);
#21976=ORIENTED_EDGE('',*,*,#16737,.T.);
#21977=ORIENTED_EDGE('',*,*,#16736,.F.);
#21978=ORIENTED_EDGE('',*,*,#16813,.T.);
#21979=ORIENTED_EDGE('',*,*,#16814,.T.);
#21980=ORIENTED_EDGE('',*,*,#16815,.T.);
#21981=ORIENTED_EDGE('',*,*,#16816,.T.);
#21982=ORIENTED_EDGE('',*,*,#16817,.T.);
#21983=ORIENTED_EDGE('',*,*,#16810,.F.);
#21984=ORIENTED_EDGE('',*,*,#16735,.T.);
#21985=ORIENTED_EDGE('',*,*,#16818,.T.);
#21986=ORIENTED_EDGE('',*,*,#16819,.T.);
#21987=ORIENTED_EDGE('',*,*,#16820,.T.);
#21988=ORIENTED_EDGE('',*,*,#16821,.T.);
#21989=ORIENTED_EDGE('',*,*,#16813,.F.);
#21990=ORIENTED_EDGE('',*,*,#16734,.F.);
#21991=ORIENTED_EDGE('',*,*,#16792,.T.);
#21992=ORIENTED_EDGE('',*,*,#16822,.T.);
#21993=ORIENTED_EDGE('',*,*,#16818,.F.);
#21994=ORIENTED_EDGE('',*,*,#16823,.T.);
#21995=ORIENTED_EDGE('',*,*,#16824,.T.);
#21996=ORIENTED_EDGE('',*,*,#16825,.F.);
#21997=ORIENTED_EDGE('',*,*,#16826,.F.);
#21998=ORIENTED_EDGE('',*,*,#16827,.T.);
#21999=ORIENTED_EDGE('',*,*,#16825,.T.);
#22000=ORIENTED_EDGE('',*,*,#16828,.F.);
#22001=ORIENTED_EDGE('',*,*,#16706,.F.);
#22002=ORIENTED_EDGE('',*,*,#16829,.T.);
#22003=ORIENTED_EDGE('',*,*,#16830,.T.);
#22004=ORIENTED_EDGE('',*,*,#16827,.F.);
#22005=ORIENTED_EDGE('',*,*,#16705,.F.);
#22006=ORIENTED_EDGE('',*,*,#16831,.F.);
#22007=ORIENTED_EDGE('',*,*,#16832,.T.);
#22008=ORIENTED_EDGE('',*,*,#16826,.T.);
#22009=ORIENTED_EDGE('',*,*,#16830,.F.);
#22010=ORIENTED_EDGE('',*,*,#16833,.T.);
#22011=ORIENTED_EDGE('',*,*,#16834,.T.);
#22012=ORIENTED_EDGE('',*,*,#16829,.F.);
#22013=ORIENTED_EDGE('',*,*,#16704,.F.);
#22014=ORIENTED_EDGE('',*,*,#16835,.T.);
#22015=ORIENTED_EDGE('',*,*,#16836,.T.);
#22016=ORIENTED_EDGE('',*,*,#16831,.T.);
#22017=ORIENTED_EDGE('',*,*,#16834,.F.);
#22018=ORIENTED_EDGE('',*,*,#16837,.T.);
#22019=ORIENTED_EDGE('',*,*,#16838,.T.);
#22020=ORIENTED_EDGE('',*,*,#16833,.F.);
#22021=ORIENTED_EDGE('',*,*,#16703,.F.);
#22022=ORIENTED_EDGE('',*,*,#16838,.F.);
#22023=ORIENTED_EDGE('',*,*,#16839,.T.);
#22024=ORIENTED_EDGE('',*,*,#16840,.T.);
#22025=ORIENTED_EDGE('',*,*,#16835,.F.);
#22026=ORIENTED_EDGE('',*,*,#16841,.T.);
#22027=ORIENTED_EDGE('',*,*,#16842,.T.);
#22028=ORIENTED_EDGE('',*,*,#16837,.F.);
#22029=ORIENTED_EDGE('',*,*,#16702,.F.);
#22030=ORIENTED_EDGE('',*,*,#16843,.T.);
#22031=ORIENTED_EDGE('',*,*,#16844,.T.);
#22032=ORIENTED_EDGE('',*,*,#16839,.F.);
#22033=ORIENTED_EDGE('',*,*,#16842,.F.);
#22034=ORIENTED_EDGE('',*,*,#16845,.T.);
#22035=ORIENTED_EDGE('',*,*,#16846,.T.);
#22036=ORIENTED_EDGE('',*,*,#16841,.F.);
#22037=ORIENTED_EDGE('',*,*,#16701,.F.);
#22038=ORIENTED_EDGE('',*,*,#16846,.F.);
#22039=ORIENTED_EDGE('',*,*,#16847,.T.);
#22040=ORIENTED_EDGE('',*,*,#16848,.T.);
#22041=ORIENTED_EDGE('',*,*,#16843,.F.);
#22042=ORIENTED_EDGE('',*,*,#16849,.T.);
#22043=ORIENTED_EDGE('',*,*,#16850,.T.);
#22044=ORIENTED_EDGE('',*,*,#16845,.F.);
#22045=ORIENTED_EDGE('',*,*,#16700,.F.);
#22046=ORIENTED_EDGE('',*,*,#16850,.F.);
#22047=ORIENTED_EDGE('',*,*,#16851,.F.);
#22048=ORIENTED_EDGE('',*,*,#16852,.T.);
#22049=ORIENTED_EDGE('',*,*,#16847,.F.);
#22050=ORIENTED_EDGE('',*,*,#16853,.T.);
#22051=ORIENTED_EDGE('',*,*,#16854,.T.);
#22052=ORIENTED_EDGE('',*,*,#16849,.F.);
#22053=ORIENTED_EDGE('',*,*,#16699,.F.);
#22054=ORIENTED_EDGE('',*,*,#16855,.F.);
#22055=ORIENTED_EDGE('',*,*,#16856,.T.);
#22056=ORIENTED_EDGE('',*,*,#16851,.T.);
#22057=ORIENTED_EDGE('',*,*,#16854,.F.);
#22058=ORIENTED_EDGE('',*,*,#16857,.T.);
#22059=ORIENTED_EDGE('',*,*,#16858,.T.);
#22060=ORIENTED_EDGE('',*,*,#16853,.F.);
#22061=ORIENTED_EDGE('',*,*,#16698,.F.);
#22062=ORIENTED_EDGE('',*,*,#16859,.F.);
#22063=ORIENTED_EDGE('',*,*,#16860,.T.);
#22064=ORIENTED_EDGE('',*,*,#16855,.T.);
#22065=ORIENTED_EDGE('',*,*,#16858,.F.);
#22066=ORIENTED_EDGE('',*,*,#16861,.T.);
#22067=ORIENTED_EDGE('',*,*,#16862,.T.);
#22068=ORIENTED_EDGE('',*,*,#16857,.F.);
#22069=ORIENTED_EDGE('',*,*,#16697,.F.);
#22070=ORIENTED_EDGE('',*,*,#16863,.F.);
#22071=ORIENTED_EDGE('',*,*,#16864,.T.);
#22072=ORIENTED_EDGE('',*,*,#16859,.T.);
#22073=ORIENTED_EDGE('',*,*,#16862,.F.);
#22074=ORIENTED_EDGE('',*,*,#16865,.T.);
#22075=ORIENTED_EDGE('',*,*,#16866,.T.);
#22076=ORIENTED_EDGE('',*,*,#16861,.F.);
#22077=ORIENTED_EDGE('',*,*,#16696,.F.);
#22078=ORIENTED_EDGE('',*,*,#16866,.F.);
#22079=ORIENTED_EDGE('',*,*,#16867,.F.);
#22080=ORIENTED_EDGE('',*,*,#16868,.T.);
#22081=ORIENTED_EDGE('',*,*,#16863,.T.);
#22082=ORIENTED_EDGE('',*,*,#16869,.T.);
#22083=ORIENTED_EDGE('',*,*,#16870,.T.);
#22084=ORIENTED_EDGE('',*,*,#16865,.F.);
#22085=ORIENTED_EDGE('',*,*,#16695,.F.);
#22086=ORIENTED_EDGE('',*,*,#16871,.F.);
#22087=ORIENTED_EDGE('',*,*,#16872,.T.);
#22088=ORIENTED_EDGE('',*,*,#16867,.T.);
#22089=ORIENTED_EDGE('',*,*,#16870,.F.);
#22090=ORIENTED_EDGE('',*,*,#16873,.T.);
#22091=ORIENTED_EDGE('',*,*,#16874,.T.);
#22092=ORIENTED_EDGE('',*,*,#16869,.F.);
#22093=ORIENTED_EDGE('',*,*,#16694,.F.);
#22094=ORIENTED_EDGE('',*,*,#16875,.F.);
#22095=ORIENTED_EDGE('',*,*,#16876,.T.);
#22096=ORIENTED_EDGE('',*,*,#16871,.T.);
#22097=ORIENTED_EDGE('',*,*,#16874,.F.);
#22098=ORIENTED_EDGE('',*,*,#16877,.T.);
#22099=ORIENTED_EDGE('',*,*,#16878,.T.);
#22100=ORIENTED_EDGE('',*,*,#16873,.F.);
#22101=ORIENTED_EDGE('',*,*,#16693,.F.);
#22102=ORIENTED_EDGE('',*,*,#16879,.F.);
#22103=ORIENTED_EDGE('',*,*,#16880,.T.);
#22104=ORIENTED_EDGE('',*,*,#16875,.T.);
#22105=ORIENTED_EDGE('',*,*,#16878,.F.);
#22106=ORIENTED_EDGE('',*,*,#16881,.T.);
#22107=ORIENTED_EDGE('',*,*,#16882,.T.);
#22108=ORIENTED_EDGE('',*,*,#16877,.F.);
#22109=ORIENTED_EDGE('',*,*,#16692,.F.);
#22110=ORIENTED_EDGE('',*,*,#16883,.T.);
#22111=ORIENTED_EDGE('',*,*,#16884,.T.);
#22112=ORIENTED_EDGE('',*,*,#16879,.T.);
#22113=ORIENTED_EDGE('',*,*,#16882,.F.);
#22114=ORIENTED_EDGE('',*,*,#16885,.T.);
#22115=ORIENTED_EDGE('',*,*,#16886,.T.);
#22116=ORIENTED_EDGE('',*,*,#16881,.F.);
#22117=ORIENTED_EDGE('',*,*,#16691,.F.);
#22118=ORIENTED_EDGE('',*,*,#16886,.F.);
#22119=ORIENTED_EDGE('',*,*,#16887,.T.);
#22120=ORIENTED_EDGE('',*,*,#16888,.T.);
#22121=ORIENTED_EDGE('',*,*,#16883,.F.);
#22122=ORIENTED_EDGE('',*,*,#16889,.T.);
#22123=ORIENTED_EDGE('',*,*,#16890,.T.);
#22124=ORIENTED_EDGE('',*,*,#16885,.F.);
#22125=ORIENTED_EDGE('',*,*,#16690,.F.);
#22126=ORIENTED_EDGE('',*,*,#16890,.F.);
#22127=ORIENTED_EDGE('',*,*,#16891,.T.);
#22128=ORIENTED_EDGE('',*,*,#16892,.T.);
#22129=ORIENTED_EDGE('',*,*,#16887,.F.);
#22130=ORIENTED_EDGE('',*,*,#16893,.T.);
#22131=ORIENTED_EDGE('',*,*,#16894,.T.);
#22132=ORIENTED_EDGE('',*,*,#16889,.F.);
#22133=ORIENTED_EDGE('',*,*,#16689,.F.);
#22134=ORIENTED_EDGE('',*,*,#16894,.F.);
#22135=ORIENTED_EDGE('',*,*,#16895,.T.);
#22136=ORIENTED_EDGE('',*,*,#16896,.T.);
#22137=ORIENTED_EDGE('',*,*,#16891,.F.);
#22138=ORIENTED_EDGE('',*,*,#16897,.T.);
#22139=ORIENTED_EDGE('',*,*,#16898,.T.);
#22140=ORIENTED_EDGE('',*,*,#16893,.F.);
#22141=ORIENTED_EDGE('',*,*,#16688,.F.);
#22142=ORIENTED_EDGE('',*,*,#16898,.F.);
#22143=ORIENTED_EDGE('',*,*,#16899,.F.);
#22144=ORIENTED_EDGE('',*,*,#16900,.T.);
#22145=ORIENTED_EDGE('',*,*,#16895,.F.);
#22146=ORIENTED_EDGE('',*,*,#16901,.T.);
#22147=ORIENTED_EDGE('',*,*,#16902,.T.);
#22148=ORIENTED_EDGE('',*,*,#16897,.F.);
#22149=ORIENTED_EDGE('',*,*,#16687,.F.);
#22150=ORIENTED_EDGE('',*,*,#16903,.F.);
#22151=ORIENTED_EDGE('',*,*,#16904,.T.);
#22152=ORIENTED_EDGE('',*,*,#16899,.T.);
#22153=ORIENTED_EDGE('',*,*,#16902,.F.);
#22154=ORIENTED_EDGE('',*,*,#16905,.T.);
#22155=ORIENTED_EDGE('',*,*,#16903,.T.);
#22156=ORIENTED_EDGE('',*,*,#16906,.F.);
#22157=ORIENTED_EDGE('',*,*,#16907,.F.);
#22158=ORIENTED_EDGE('',*,*,#16908,.T.);
#22159=ORIENTED_EDGE('',*,*,#16906,.T.);
#22160=ORIENTED_EDGE('',*,*,#16901,.F.);
#22161=ORIENTED_EDGE('',*,*,#16686,.F.);
#22162=ORIENTED_EDGE('',*,*,#16909,.T.);
#22163=ORIENTED_EDGE('',*,*,#16910,.T.);
#22164=ORIENTED_EDGE('',*,*,#16908,.F.);
#22165=ORIENTED_EDGE('',*,*,#16685,.F.);
#22166=ORIENTED_EDGE('',*,*,#16911,.F.);
#22167=ORIENTED_EDGE('',*,*,#16912,.T.);
#22168=ORIENTED_EDGE('',*,*,#16907,.T.);
#22169=ORIENTED_EDGE('',*,*,#16910,.F.);
#22170=ORIENTED_EDGE('',*,*,#16913,.T.);
#22171=ORIENTED_EDGE('',*,*,#16914,.T.);
#22172=ORIENTED_EDGE('',*,*,#16909,.F.);
#22173=ORIENTED_EDGE('',*,*,#16684,.F.);
#22174=ORIENTED_EDGE('',*,*,#16915,.T.);
#22175=ORIENTED_EDGE('',*,*,#16916,.T.);
#22176=ORIENTED_EDGE('',*,*,#16911,.T.);
#22177=ORIENTED_EDGE('',*,*,#16914,.F.);
#22178=ORIENTED_EDGE('',*,*,#16917,.T.);
#22179=ORIENTED_EDGE('',*,*,#16918,.T.);
#22180=ORIENTED_EDGE('',*,*,#16913,.F.);
#22181=ORIENTED_EDGE('',*,*,#16683,.F.);
#22182=ORIENTED_EDGE('',*,*,#16918,.F.);
#22183=ORIENTED_EDGE('',*,*,#16919,.T.);
#22184=ORIENTED_EDGE('',*,*,#16920,.T.);
#22185=ORIENTED_EDGE('',*,*,#16915,.F.);
#22186=ORIENTED_EDGE('',*,*,#16921,.T.);
#22187=ORIENTED_EDGE('',*,*,#16922,.T.);
#22188=ORIENTED_EDGE('',*,*,#16917,.F.);
#22189=ORIENTED_EDGE('',*,*,#16682,.F.);
#22190=ORIENTED_EDGE('',*,*,#16923,.T.);
#22191=ORIENTED_EDGE('',*,*,#16924,.T.);
#22192=ORIENTED_EDGE('',*,*,#16919,.F.);
#22193=ORIENTED_EDGE('',*,*,#16922,.F.);
#22194=ORIENTED_EDGE('',*,*,#16925,.T.);
#22195=ORIENTED_EDGE('',*,*,#16926,.T.);
#22196=ORIENTED_EDGE('',*,*,#16921,.F.);
#22197=ORIENTED_EDGE('',*,*,#16681,.F.);
#22198=ORIENTED_EDGE('',*,*,#16926,.F.);
#22199=ORIENTED_EDGE('',*,*,#16927,.T.);
#22200=ORIENTED_EDGE('',*,*,#16928,.T.);
#22201=ORIENTED_EDGE('',*,*,#16923,.F.);
#22202=ORIENTED_EDGE('',*,*,#16929,.T.);
#22203=ORIENTED_EDGE('',*,*,#16930,.T.);
#22204=ORIENTED_EDGE('',*,*,#16925,.F.);
#22205=ORIENTED_EDGE('',*,*,#16680,.F.);
#22206=ORIENTED_EDGE('',*,*,#16930,.F.);
#22207=ORIENTED_EDGE('',*,*,#16931,.F.);
#22208=ORIENTED_EDGE('',*,*,#16932,.T.);
#22209=ORIENTED_EDGE('',*,*,#16927,.F.);
#22210=ORIENTED_EDGE('',*,*,#16933,.T.);
#22211=ORIENTED_EDGE('',*,*,#16934,.T.);
#22212=ORIENTED_EDGE('',*,*,#16929,.F.);
#22213=ORIENTED_EDGE('',*,*,#16679,.F.);
#22214=ORIENTED_EDGE('',*,*,#16935,.F.);
#22215=ORIENTED_EDGE('',*,*,#16936,.T.);
#22216=ORIENTED_EDGE('',*,*,#16931,.T.);
#22217=ORIENTED_EDGE('',*,*,#16934,.F.);
#22218=ORIENTED_EDGE('',*,*,#16937,.T.);
#22219=ORIENTED_EDGE('',*,*,#16938,.T.);
#22220=ORIENTED_EDGE('',*,*,#16933,.F.);
#22221=ORIENTED_EDGE('',*,*,#16678,.F.);
#22222=ORIENTED_EDGE('',*,*,#16939,.F.);
#22223=ORIENTED_EDGE('',*,*,#16940,.T.);
#22224=ORIENTED_EDGE('',*,*,#16935,.T.);
#22225=ORIENTED_EDGE('',*,*,#16938,.F.);
#22226=ORIENTED_EDGE('',*,*,#16941,.T.);
#22227=ORIENTED_EDGE('',*,*,#16942,.T.);
#22228=ORIENTED_EDGE('',*,*,#16937,.F.);
#22229=ORIENTED_EDGE('',*,*,#16677,.F.);
#22230=ORIENTED_EDGE('',*,*,#16943,.F.);
#22231=ORIENTED_EDGE('',*,*,#16944,.T.);
#22232=ORIENTED_EDGE('',*,*,#16939,.T.);
#22233=ORIENTED_EDGE('',*,*,#16942,.F.);
#22234=ORIENTED_EDGE('',*,*,#16945,.T.);
#22235=ORIENTED_EDGE('',*,*,#16946,.T.);
#22236=ORIENTED_EDGE('',*,*,#16941,.F.);
#22237=ORIENTED_EDGE('',*,*,#16676,.F.);
#22238=ORIENTED_EDGE('',*,*,#16947,.F.);
#22239=ORIENTED_EDGE('',*,*,#16948,.T.);
#22240=ORIENTED_EDGE('',*,*,#16943,.T.);
#22241=ORIENTED_EDGE('',*,*,#16946,.F.);
#22242=ORIENTED_EDGE('',*,*,#16949,.T.);
#22243=ORIENTED_EDGE('',*,*,#16950,.T.);
#22244=ORIENTED_EDGE('',*,*,#16945,.F.);
#22245=ORIENTED_EDGE('',*,*,#16715,.F.);
#22246=ORIENTED_EDGE('',*,*,#16951,.F.);
#22247=ORIENTED_EDGE('',*,*,#16952,.T.);
#22248=ORIENTED_EDGE('',*,*,#16947,.T.);
#22249=ORIENTED_EDGE('',*,*,#16950,.F.);
#22250=ORIENTED_EDGE('',*,*,#16953,.T.);
#22251=ORIENTED_EDGE('',*,*,#16954,.T.);
#22252=ORIENTED_EDGE('',*,*,#16949,.F.);
#22253=ORIENTED_EDGE('',*,*,#16714,.F.);
#22254=ORIENTED_EDGE('',*,*,#16955,.F.);
#22255=ORIENTED_EDGE('',*,*,#16956,.T.);
#22256=ORIENTED_EDGE('',*,*,#16951,.T.);
#22257=ORIENTED_EDGE('',*,*,#16954,.F.);
#22258=ORIENTED_EDGE('',*,*,#16957,.T.);
#22259=ORIENTED_EDGE('',*,*,#16958,.T.);
#22260=ORIENTED_EDGE('',*,*,#16953,.F.);
#22261=ORIENTED_EDGE('',*,*,#16713,.F.);
#22262=ORIENTED_EDGE('',*,*,#16959,.F.);
#22263=ORIENTED_EDGE('',*,*,#16960,.T.);
#22264=ORIENTED_EDGE('',*,*,#16955,.T.);
#22265=ORIENTED_EDGE('',*,*,#16958,.F.);
#22266=ORIENTED_EDGE('',*,*,#16961,.T.);
#22267=ORIENTED_EDGE('',*,*,#16962,.T.);
#22268=ORIENTED_EDGE('',*,*,#16957,.F.);
#22269=ORIENTED_EDGE('',*,*,#16712,.F.);
#22270=ORIENTED_EDGE('',*,*,#16963,.T.);
#22271=ORIENTED_EDGE('',*,*,#16964,.T.);
#22272=ORIENTED_EDGE('',*,*,#16959,.T.);
#22273=ORIENTED_EDGE('',*,*,#16962,.F.);
#22274=ORIENTED_EDGE('',*,*,#16965,.T.);
#22275=ORIENTED_EDGE('',*,*,#16966,.T.);
#22276=ORIENTED_EDGE('',*,*,#16961,.F.);
#22277=ORIENTED_EDGE('',*,*,#16711,.F.);
#22278=ORIENTED_EDGE('',*,*,#16966,.F.);
#22279=ORIENTED_EDGE('',*,*,#16967,.T.);
#22280=ORIENTED_EDGE('',*,*,#16968,.T.);
#22281=ORIENTED_EDGE('',*,*,#16963,.F.);
#22282=ORIENTED_EDGE('',*,*,#16969,.T.);
#22283=ORIENTED_EDGE('',*,*,#16970,.T.);
#22284=ORIENTED_EDGE('',*,*,#16965,.F.);
#22285=ORIENTED_EDGE('',*,*,#16710,.F.);
#22286=ORIENTED_EDGE('',*,*,#16970,.F.);
#22287=ORIENTED_EDGE('',*,*,#16971,.T.);
#22288=ORIENTED_EDGE('',*,*,#16972,.T.);
#22289=ORIENTED_EDGE('',*,*,#16967,.F.);
#22290=ORIENTED_EDGE('',*,*,#16828,.T.);
#22291=ORIENTED_EDGE('',*,*,#16973,.T.);
#22292=ORIENTED_EDGE('',*,*,#16974,.F.);
#22293=ORIENTED_EDGE('',*,*,#16707,.F.);
#22294=ORIENTED_EDGE('',*,*,#16824,.F.);
#22295=ORIENTED_EDGE('',*,*,#16975,.T.);
#22296=ORIENTED_EDGE('',*,*,#16976,.T.);
#22297=ORIENTED_EDGE('',*,*,#16973,.F.);
#22298=ORIENTED_EDGE('',*,*,#16977,.T.);
#22299=ORIENTED_EDGE('',*,*,#16978,.T.);
#22300=ORIENTED_EDGE('',*,*,#16969,.F.);
#22301=ORIENTED_EDGE('',*,*,#16709,.F.);
#22302=ORIENTED_EDGE('',*,*,#16978,.F.);
#22303=ORIENTED_EDGE('',*,*,#16979,.T.);
#22304=ORIENTED_EDGE('',*,*,#16980,.T.);
#22305=ORIENTED_EDGE('',*,*,#16971,.F.);
#22306=ORIENTED_EDGE('',*,*,#16974,.T.);
#22307=ORIENTED_EDGE('',*,*,#16981,.T.);
#22308=ORIENTED_EDGE('',*,*,#16977,.F.);
#22309=ORIENTED_EDGE('',*,*,#16708,.F.);
#22310=ORIENTED_EDGE('',*,*,#16981,.F.);
#22311=ORIENTED_EDGE('',*,*,#16976,.F.);
#22312=ORIENTED_EDGE('',*,*,#16982,.T.);
#22313=ORIENTED_EDGE('',*,*,#16979,.F.);
#22314=ORIENTED_EDGE('',*,*,#16983,.T.);
#22315=ORIENTED_EDGE('',*,*,#16984,.F.);
#22316=ORIENTED_EDGE('',*,*,#16985,.F.);
#22317=ORIENTED_EDGE('',*,*,#16986,.F.);
#22318=ORIENTED_EDGE('',*,*,#16987,.T.);
#22319=ORIENTED_EDGE('',*,*,#16988,.F.);
#22320=ORIENTED_EDGE('',*,*,#16989,.F.);
#22321=ORIENTED_EDGE('',*,*,#16990,.F.);
#22322=ORIENTED_EDGE('',*,*,#16991,.T.);
#22323=ORIENTED_EDGE('',*,*,#16992,.T.);
#22324=ORIENTED_EDGE('',*,*,#16987,.F.);
#22325=ORIENTED_EDGE('',*,*,#16993,.F.);
#22326=ORIENTED_EDGE('',*,*,#16994,.F.);
#22327=ORIENTED_EDGE('',*,*,#16989,.T.);
#22328=ORIENTED_EDGE('',*,*,#16995,.T.);
#22329=ORIENTED_EDGE('',*,*,#16996,.F.);
#22330=ORIENTED_EDGE('',*,*,#16997,.F.);
#22331=ORIENTED_EDGE('',*,*,#16998,.F.);
#22332=ORIENTED_EDGE('',*,*,#16996,.T.);
#22333=ORIENTED_EDGE('',*,*,#16999,.T.);
#22334=ORIENTED_EDGE('',*,*,#17000,.F.);
#22335=ORIENTED_EDGE('',*,*,#17001,.F.);
#22336=ORIENTED_EDGE('',*,*,#17000,.T.);
#22337=ORIENTED_EDGE('',*,*,#17002,.T.);
#22338=ORIENTED_EDGE('',*,*,#16744,.F.);
#22339=ORIENTED_EDGE('',*,*,#17003,.F.);
#22340=ORIENTED_EDGE('',*,*,#17004,.T.);
#22341=ORIENTED_EDGE('',*,*,#17005,.F.);
#22342=ORIENTED_EDGE('',*,*,#17006,.F.);
#22343=ORIENTED_EDGE('',*,*,#17007,.F.);
#22344=ORIENTED_EDGE('',*,*,#17008,.T.);
#22345=ORIENTED_EDGE('',*,*,#17009,.T.);
#22346=ORIENTED_EDGE('',*,*,#17010,.F.);
#22347=ORIENTED_EDGE('',*,*,#17011,.F.);
#22348=ORIENTED_EDGE('',*,*,#17012,.T.);
#22349=ORIENTED_EDGE('',*,*,#17013,.T.);
#22350=ORIENTED_EDGE('',*,*,#17008,.F.);
#22351=ORIENTED_EDGE('',*,*,#17014,.F.);
#22352=ORIENTED_EDGE('',*,*,#16746,.T.);
#22353=ORIENTED_EDGE('',*,*,#17015,.F.);
#22354=ORIENTED_EDGE('',*,*,#17012,.F.);
#22355=ORIENTED_EDGE('',*,*,#17016,.F.);
#22356=ORIENTED_EDGE('',*,*,#17017,.F.);
#22357=ORIENTED_EDGE('',*,*,#17018,.T.);
#22358=ORIENTED_EDGE('',*,*,#17019,.T.);
#22359=ORIENTED_EDGE('',*,*,#16752,.F.);
#22360=ORIENTED_EDGE('',*,*,#17020,.F.);
#22361=ORIENTED_EDGE('',*,*,#17021,.T.);
#22362=ORIENTED_EDGE('',*,*,#16985,.T.);
#22363=ORIENTED_EDGE('',*,*,#17022,.T.);
#22364=ORIENTED_EDGE('',*,*,#17023,.F.);
#22365=ORIENTED_EDGE('',*,*,#16756,.T.);
#22366=ORIENTED_EDGE('',*,*,#17024,.T.);
#22367=ORIENTED_EDGE('',*,*,#17025,.F.);
#22368=ORIENTED_EDGE('',*,*,#17026,.F.);
#22369=ORIENTED_EDGE('',*,*,#16759,.T.);
#22370=ORIENTED_EDGE('',*,*,#17027,.T.);
#22371=ORIENTED_EDGE('',*,*,#17028,.F.);
#22372=ORIENTED_EDGE('',*,*,#17029,.F.);
#22373=ORIENTED_EDGE('',*,*,#16760,.T.);
#22374=ORIENTED_EDGE('',*,*,#17029,.T.);
#22375=ORIENTED_EDGE('',*,*,#17030,.F.);
#22376=ORIENTED_EDGE('',*,*,#17024,.F.);
#22377=ORIENTED_EDGE('',*,*,#16762,.T.);
#22378=ORIENTED_EDGE('',*,*,#17031,.T.);
#22379=ORIENTED_EDGE('',*,*,#17032,.F.);
#22380=ORIENTED_EDGE('',*,*,#17027,.F.);
#22381=ORIENTED_EDGE('',*,*,#16764,.T.);
#22382=ORIENTED_EDGE('',*,*,#17033,.T.);
#22383=ORIENTED_EDGE('',*,*,#17034,.F.);
#22384=ORIENTED_EDGE('',*,*,#17035,.F.);
#22385=ORIENTED_EDGE('',*,*,#16765,.T.);
#22386=ORIENTED_EDGE('',*,*,#17035,.T.);
#22387=ORIENTED_EDGE('',*,*,#17036,.F.);
#22388=ORIENTED_EDGE('',*,*,#17037,.F.);
#22389=ORIENTED_EDGE('',*,*,#16766,.T.);
#22390=ORIENTED_EDGE('',*,*,#17037,.T.);
#22391=ORIENTED_EDGE('',*,*,#17038,.F.);
#22392=ORIENTED_EDGE('',*,*,#17031,.F.);
#22393=ORIENTED_EDGE('',*,*,#16770,.T.);
#22394=ORIENTED_EDGE('',*,*,#17039,.T.);
#22395=ORIENTED_EDGE('',*,*,#17040,.F.);
#22396=ORIENTED_EDGE('',*,*,#17041,.F.);
#22397=ORIENTED_EDGE('',*,*,#16769,.T.);
#22398=ORIENTED_EDGE('',*,*,#17042,.T.);
#22399=ORIENTED_EDGE('',*,*,#17043,.F.);
#22400=ORIENTED_EDGE('',*,*,#17039,.F.);
#22401=ORIENTED_EDGE('',*,*,#16768,.T.);
#22402=ORIENTED_EDGE('',*,*,#17044,.T.);
#22403=ORIENTED_EDGE('',*,*,#17045,.F.);
#22404=ORIENTED_EDGE('',*,*,#17042,.F.);
#22405=ORIENTED_EDGE('',*,*,#16771,.T.);
#22406=ORIENTED_EDGE('',*,*,#17041,.T.);
#22407=ORIENTED_EDGE('',*,*,#17046,.F.);
#22408=ORIENTED_EDGE('',*,*,#17033,.F.);
#22409=ORIENTED_EDGE('',*,*,#16774,.T.);
#22410=ORIENTED_EDGE('',*,*,#17047,.T.);
#22411=ORIENTED_EDGE('',*,*,#17048,.F.);
#22412=ORIENTED_EDGE('',*,*,#17044,.F.);
#22413=ORIENTED_EDGE('',*,*,#16773,.T.);
#22414=ORIENTED_EDGE('',*,*,#17049,.T.);
#22415=ORIENTED_EDGE('',*,*,#17050,.F.);
#22416=ORIENTED_EDGE('',*,*,#17047,.F.);
#22417=ORIENTED_EDGE('',*,*,#16779,.T.);
#22418=ORIENTED_EDGE('',*,*,#17051,.T.);
#22419=ORIENTED_EDGE('',*,*,#17052,.F.);
#22420=ORIENTED_EDGE('',*,*,#17049,.F.);
#22421=ORIENTED_EDGE('',*,*,#16778,.T.);
#22422=ORIENTED_EDGE('',*,*,#17053,.T.);
#22423=ORIENTED_EDGE('',*,*,#17054,.F.);
#22424=ORIENTED_EDGE('',*,*,#17051,.F.);
#22425=ORIENTED_EDGE('',*,*,#16777,.T.);
#22426=ORIENTED_EDGE('',*,*,#17055,.T.);
#22427=ORIENTED_EDGE('',*,*,#17056,.F.);
#22428=ORIENTED_EDGE('',*,*,#17053,.F.);
#22429=ORIENTED_EDGE('',*,*,#16776,.T.);
#22430=ORIENTED_EDGE('',*,*,#17057,.T.);
#22431=ORIENTED_EDGE('',*,*,#17058,.F.);
#22432=ORIENTED_EDGE('',*,*,#17055,.F.);
#22433=ORIENTED_EDGE('',*,*,#17058,.T.);
#22434=ORIENTED_EDGE('',*,*,#17059,.T.);
#22435=ORIENTED_EDGE('',*,*,#16781,.F.);
#22436=ORIENTED_EDGE('',*,*,#17060,.T.);
#22437=ORIENTED_EDGE('',*,*,#17061,.F.);
#22438=ORIENTED_EDGE('',*,*,#17062,.F.);
#22439=ORIENTED_EDGE('',*,*,#16782,.T.);
#22440=ORIENTED_EDGE('',*,*,#17059,.F.);
#22441=ORIENTED_EDGE('',*,*,#17057,.F.);
#22442=ORIENTED_EDGE('',*,*,#17063,.T.);
#22443=ORIENTED_EDGE('',*,*,#17064,.T.);
#22444=ORIENTED_EDGE('',*,*,#17065,.T.);
#22445=ORIENTED_EDGE('',*,*,#17066,.F.);
#22446=ORIENTED_EDGE('',*,*,#17060,.F.);
#22447=ORIENTED_EDGE('',*,*,#16785,.F.);
#22448=ORIENTED_EDGE('',*,*,#16784,.T.);
#22449=ORIENTED_EDGE('',*,*,#17067,.T.);
#22450=ORIENTED_EDGE('',*,*,#17063,.F.);
#22451=ORIENTED_EDGE('',*,*,#16786,.T.);
#22452=ORIENTED_EDGE('',*,*,#17026,.T.);
#22453=ORIENTED_EDGE('',*,*,#17068,.F.);
#22454=ORIENTED_EDGE('',*,*,#17069,.F.);
#22455=ORIENTED_EDGE('',*,*,#16787,.T.);
#22456=ORIENTED_EDGE('',*,*,#17069,.T.);
#22457=ORIENTED_EDGE('',*,*,#17070,.F.);
#22458=ORIENTED_EDGE('',*,*,#17071,.F.);
#22459=ORIENTED_EDGE('',*,*,#16788,.T.);
#22460=ORIENTED_EDGE('',*,*,#17071,.T.);
#22461=ORIENTED_EDGE('',*,*,#17064,.F.);
#22462=ORIENTED_EDGE('',*,*,#17067,.F.);
#22463=ORIENTED_EDGE('',*,*,#17072,.T.);
#22464=ORIENTED_EDGE('',*,*,#17073,.T.);
#22465=ORIENTED_EDGE('',*,*,#17074,.F.);
#22466=ORIENTED_EDGE('',*,*,#16790,.F.);
#22467=ORIENTED_EDGE('',*,*,#17074,.T.);
#22468=ORIENTED_EDGE('',*,*,#17075,.T.);
#22469=ORIENTED_EDGE('',*,*,#17076,.F.);
#22470=ORIENTED_EDGE('',*,*,#16791,.F.);
#22471=ORIENTED_EDGE('',*,*,#17077,.T.);
#22472=ORIENTED_EDGE('',*,*,#17078,.T.);
#22473=ORIENTED_EDGE('',*,*,#17072,.F.);
#22474=ORIENTED_EDGE('',*,*,#16794,.F.);
#22475=ORIENTED_EDGE('',*,*,#17079,.T.);
#22476=ORIENTED_EDGE('',*,*,#17080,.T.);
#22477=ORIENTED_EDGE('',*,*,#17081,.F.);
#22478=ORIENTED_EDGE('',*,*,#16796,.F.);
#22479=ORIENTED_EDGE('',*,*,#17081,.T.);
#22480=ORIENTED_EDGE('',*,*,#17007,.T.);
#22481=ORIENTED_EDGE('',*,*,#17082,.F.);
#22482=ORIENTED_EDGE('',*,*,#16797,.F.);
#22483=ORIENTED_EDGE('',*,*,#17082,.T.);
#22484=ORIENTED_EDGE('',*,*,#17083,.T.);
#22485=ORIENTED_EDGE('',*,*,#17077,.F.);
#22486=ORIENTED_EDGE('',*,*,#16798,.F.);
#22487=ORIENTED_EDGE('',*,*,#17084,.T.);
#22488=ORIENTED_EDGE('',*,*,#17079,.F.);
#22489=ORIENTED_EDGE('',*,*,#16801,.F.);
#22490=ORIENTED_EDGE('',*,*,#16800,.T.);
#22491=ORIENTED_EDGE('',*,*,#17085,.T.);
#22492=ORIENTED_EDGE('',*,*,#17086,.T.);
#22493=ORIENTED_EDGE('',*,*,#17004,.F.);
#22494=ORIENTED_EDGE('',*,*,#17080,.F.);
#22495=ORIENTED_EDGE('',*,*,#17084,.F.);
#22496=ORIENTED_EDGE('',*,*,#17010,.T.);
#22497=ORIENTED_EDGE('',*,*,#17087,.T.);
#22498=ORIENTED_EDGE('',*,*,#17085,.F.);
#22499=ORIENTED_EDGE('',*,*,#16804,.T.);
#22500=ORIENTED_EDGE('',*,*,#17088,.F.);
#22501=ORIENTED_EDGE('',*,*,#17089,.F.);
#22502=ORIENTED_EDGE('',*,*,#17090,.T.);
#22503=ORIENTED_EDGE('',*,*,#17088,.T.);
#22504=ORIENTED_EDGE('',*,*,#16803,.F.);
#22505=ORIENTED_EDGE('',*,*,#17091,.T.);
#22506=ORIENTED_EDGE('',*,*,#17089,.T.);
#22507=ORIENTED_EDGE('',*,*,#17090,.F.);
#22508=ORIENTED_EDGE('',*,*,#16809,.F.);
#22509=ORIENTED_EDGE('',*,*,#17092,.T.);
#22510=ORIENTED_EDGE('',*,*,#17011,.T.);
#22511=ORIENTED_EDGE('',*,*,#17091,.F.);
#22512=ORIENTED_EDGE('',*,*,#16808,.F.);
#22513=ORIENTED_EDGE('',*,*,#17093,.T.);
#22514=ORIENTED_EDGE('',*,*,#17014,.T.);
#22515=ORIENTED_EDGE('',*,*,#17092,.F.);
#22516=ORIENTED_EDGE('',*,*,#16807,.F.);
#22517=ORIENTED_EDGE('',*,*,#17094,.T.);
#22518=ORIENTED_EDGE('',*,*,#17016,.T.);
#22519=ORIENTED_EDGE('',*,*,#17093,.F.);
#22520=ORIENTED_EDGE('',*,*,#16806,.F.);
#22521=ORIENTED_EDGE('',*,*,#17095,.T.);
#22522=ORIENTED_EDGE('',*,*,#17017,.T.);
#22523=ORIENTED_EDGE('',*,*,#17094,.F.);
#22524=ORIENTED_EDGE('',*,*,#16812,.F.);
#22525=ORIENTED_EDGE('',*,*,#17096,.T.);
#22526=ORIENTED_EDGE('',*,*,#16747,.T.);
#22527=ORIENTED_EDGE('',*,*,#17095,.F.);
#22528=ORIENTED_EDGE('',*,*,#16811,.F.);
#22529=ORIENTED_EDGE('',*,*,#17097,.T.);
#22530=ORIENTED_EDGE('',*,*,#16748,.T.);
#22531=ORIENTED_EDGE('',*,*,#17096,.F.);
#22532=ORIENTED_EDGE('',*,*,#16817,.F.);
#22533=ORIENTED_EDGE('',*,*,#17098,.T.);
#22534=ORIENTED_EDGE('',*,*,#17003,.T.);
#22535=ORIENTED_EDGE('',*,*,#17097,.F.);
#22536=ORIENTED_EDGE('',*,*,#16816,.F.);
#22537=ORIENTED_EDGE('',*,*,#17099,.T.);
#22538=ORIENTED_EDGE('',*,*,#17001,.T.);
#22539=ORIENTED_EDGE('',*,*,#17098,.F.);
#22540=ORIENTED_EDGE('',*,*,#16815,.F.);
#22541=ORIENTED_EDGE('',*,*,#17100,.T.);
#22542=ORIENTED_EDGE('',*,*,#16997,.T.);
#22543=ORIENTED_EDGE('',*,*,#17099,.F.);
#22544=ORIENTED_EDGE('',*,*,#16814,.F.);
#22545=ORIENTED_EDGE('',*,*,#17101,.T.);
#22546=ORIENTED_EDGE('',*,*,#16993,.T.);
#22547=ORIENTED_EDGE('',*,*,#17102,.F.);
#22548=ORIENTED_EDGE('',*,*,#16819,.F.);
#22549=ORIENTED_EDGE('',*,*,#17102,.T.);
#22550=ORIENTED_EDGE('',*,*,#16990,.T.);
#22551=ORIENTED_EDGE('',*,*,#17103,.F.);
#22552=ORIENTED_EDGE('',*,*,#16820,.F.);
#22553=ORIENTED_EDGE('',*,*,#17103,.T.);
#22554=ORIENTED_EDGE('',*,*,#16998,.T.);
#22555=ORIENTED_EDGE('',*,*,#17100,.F.);
#22556=ORIENTED_EDGE('',*,*,#16821,.F.);
#22557=ORIENTED_EDGE('',*,*,#17076,.T.);
#22558=ORIENTED_EDGE('',*,*,#16994,.T.);
#22559=ORIENTED_EDGE('',*,*,#17101,.F.);
#22560=ORIENTED_EDGE('',*,*,#16822,.F.);
#22561=ORIENTED_EDGE('',*,*,#17104,.T.);
#22562=ORIENTED_EDGE('',*,*,#17105,.T.);
#22563=ORIENTED_EDGE('',*,*,#17106,.F.);
#22564=ORIENTED_EDGE('',*,*,#16823,.F.);
#22565=ORIENTED_EDGE('',*,*,#17107,.T.);
#22566=ORIENTED_EDGE('',*,*,#17108,.T.);
#22567=ORIENTED_EDGE('',*,*,#17104,.F.);
#22568=ORIENTED_EDGE('',*,*,#16832,.F.);
#22569=ORIENTED_EDGE('',*,*,#17109,.T.);
#22570=ORIENTED_EDGE('',*,*,#17110,.T.);
#22571=ORIENTED_EDGE('',*,*,#17107,.F.);
#22572=ORIENTED_EDGE('',*,*,#16836,.F.);
#22573=ORIENTED_EDGE('',*,*,#17111,.T.);
#22574=ORIENTED_EDGE('',*,*,#17112,.T.);
#22575=ORIENTED_EDGE('',*,*,#17109,.F.);
#22576=ORIENTED_EDGE('',*,*,#16840,.F.);
#22577=ORIENTED_EDGE('',*,*,#17113,.T.);
#22578=ORIENTED_EDGE('',*,*,#17114,.T.);
#22579=ORIENTED_EDGE('',*,*,#17111,.F.);
#22580=ORIENTED_EDGE('',*,*,#16844,.F.);
#22581=ORIENTED_EDGE('',*,*,#17115,.T.);
#22582=ORIENTED_EDGE('',*,*,#17116,.T.);
#22583=ORIENTED_EDGE('',*,*,#17113,.F.);
#22584=ORIENTED_EDGE('',*,*,#16848,.F.);
#22585=ORIENTED_EDGE('',*,*,#17117,.T.);
#22586=ORIENTED_EDGE('',*,*,#17118,.T.);
#22587=ORIENTED_EDGE('',*,*,#17115,.F.);
#22588=ORIENTED_EDGE('',*,*,#16852,.F.);
#22589=ORIENTED_EDGE('',*,*,#17119,.T.);
#22590=ORIENTED_EDGE('',*,*,#17120,.T.);
#22591=ORIENTED_EDGE('',*,*,#17117,.F.);
#22592=ORIENTED_EDGE('',*,*,#16856,.F.);
#22593=ORIENTED_EDGE('',*,*,#17121,.T.);
#22594=ORIENTED_EDGE('',*,*,#17122,.T.);
#22595=ORIENTED_EDGE('',*,*,#17119,.F.);
#22596=ORIENTED_EDGE('',*,*,#16860,.F.);
#22597=ORIENTED_EDGE('',*,*,#17123,.T.);
#22598=ORIENTED_EDGE('',*,*,#17124,.T.);
#22599=ORIENTED_EDGE('',*,*,#17121,.F.);
#22600=ORIENTED_EDGE('',*,*,#16864,.F.);
#22601=ORIENTED_EDGE('',*,*,#17125,.T.);
#22602=ORIENTED_EDGE('',*,*,#17126,.T.);
#22603=ORIENTED_EDGE('',*,*,#17123,.F.);
#22604=ORIENTED_EDGE('',*,*,#16868,.F.);
#22605=ORIENTED_EDGE('',*,*,#17127,.T.);
#22606=ORIENTED_EDGE('',*,*,#17128,.T.);
#22607=ORIENTED_EDGE('',*,*,#17125,.F.);
#22608=ORIENTED_EDGE('',*,*,#16872,.F.);
#22609=ORIENTED_EDGE('',*,*,#17129,.T.);
#22610=ORIENTED_EDGE('',*,*,#17130,.T.);
#22611=ORIENTED_EDGE('',*,*,#17127,.F.);
#22612=ORIENTED_EDGE('',*,*,#16876,.F.);
#22613=ORIENTED_EDGE('',*,*,#17131,.T.);
#22614=ORIENTED_EDGE('',*,*,#17132,.T.);
#22615=ORIENTED_EDGE('',*,*,#17129,.F.);
#22616=ORIENTED_EDGE('',*,*,#16880,.F.);
#22617=ORIENTED_EDGE('',*,*,#17133,.T.);
#22618=ORIENTED_EDGE('',*,*,#17134,.T.);
#22619=ORIENTED_EDGE('',*,*,#17131,.F.);
#22620=ORIENTED_EDGE('',*,*,#16884,.F.);
#22621=ORIENTED_EDGE('',*,*,#17135,.T.);
#22622=ORIENTED_EDGE('',*,*,#17136,.T.);
#22623=ORIENTED_EDGE('',*,*,#17133,.F.);
#22624=ORIENTED_EDGE('',*,*,#16888,.F.);
#22625=ORIENTED_EDGE('',*,*,#17137,.T.);
#22626=ORIENTED_EDGE('',*,*,#17138,.T.);
#22627=ORIENTED_EDGE('',*,*,#17135,.F.);
#22628=ORIENTED_EDGE('',*,*,#16892,.F.);
#22629=ORIENTED_EDGE('',*,*,#17139,.T.);
#22630=ORIENTED_EDGE('',*,*,#17140,.T.);
#22631=ORIENTED_EDGE('',*,*,#17137,.F.);
#22632=ORIENTED_EDGE('',*,*,#16896,.F.);
#22633=ORIENTED_EDGE('',*,*,#17141,.T.);
#22634=ORIENTED_EDGE('',*,*,#17142,.T.);
#22635=ORIENTED_EDGE('',*,*,#17139,.F.);
#22636=ORIENTED_EDGE('',*,*,#16900,.F.);
#22637=ORIENTED_EDGE('',*,*,#17143,.T.);
#22638=ORIENTED_EDGE('',*,*,#17144,.T.);
#22639=ORIENTED_EDGE('',*,*,#17141,.F.);
#22640=ORIENTED_EDGE('',*,*,#16904,.F.);
#22641=ORIENTED_EDGE('',*,*,#17145,.T.);
#22642=ORIENTED_EDGE('',*,*,#17146,.T.);
#22643=ORIENTED_EDGE('',*,*,#17143,.F.);
#22644=ORIENTED_EDGE('',*,*,#16905,.F.);
#22645=ORIENTED_EDGE('',*,*,#17147,.T.);
#22646=ORIENTED_EDGE('',*,*,#17148,.T.);
#22647=ORIENTED_EDGE('',*,*,#17145,.F.);
#22648=ORIENTED_EDGE('',*,*,#16912,.F.);
#22649=ORIENTED_EDGE('',*,*,#17149,.T.);
#22650=ORIENTED_EDGE('',*,*,#17150,.T.);
#22651=ORIENTED_EDGE('',*,*,#17147,.F.);
#22652=ORIENTED_EDGE('',*,*,#16916,.F.);
#22653=ORIENTED_EDGE('',*,*,#17151,.T.);
#22654=ORIENTED_EDGE('',*,*,#17152,.T.);
#22655=ORIENTED_EDGE('',*,*,#17149,.F.);
#22656=ORIENTED_EDGE('',*,*,#16920,.F.);
#22657=ORIENTED_EDGE('',*,*,#17153,.T.);
#22658=ORIENTED_EDGE('',*,*,#17154,.T.);
#22659=ORIENTED_EDGE('',*,*,#17151,.F.);
#22660=ORIENTED_EDGE('',*,*,#16924,.F.);
#22661=ORIENTED_EDGE('',*,*,#17155,.T.);
#22662=ORIENTED_EDGE('',*,*,#17156,.T.);
#22663=ORIENTED_EDGE('',*,*,#17153,.F.);
#22664=ORIENTED_EDGE('',*,*,#16928,.F.);
#22665=ORIENTED_EDGE('',*,*,#17157,.T.);
#22666=ORIENTED_EDGE('',*,*,#17158,.T.);
#22667=ORIENTED_EDGE('',*,*,#17155,.F.);
#22668=ORIENTED_EDGE('',*,*,#16932,.F.);
#22669=ORIENTED_EDGE('',*,*,#17159,.T.);
#22670=ORIENTED_EDGE('',*,*,#17160,.T.);
#22671=ORIENTED_EDGE('',*,*,#17157,.F.);
#22672=ORIENTED_EDGE('',*,*,#16936,.F.);
#22673=ORIENTED_EDGE('',*,*,#17161,.T.);
#22674=ORIENTED_EDGE('',*,*,#17162,.T.);
#22675=ORIENTED_EDGE('',*,*,#17159,.F.);
#22676=ORIENTED_EDGE('',*,*,#16940,.F.);
#22677=ORIENTED_EDGE('',*,*,#17163,.T.);
#22678=ORIENTED_EDGE('',*,*,#17164,.T.);
#22679=ORIENTED_EDGE('',*,*,#17161,.F.);
#22680=ORIENTED_EDGE('',*,*,#16944,.F.);
#22681=ORIENTED_EDGE('',*,*,#17165,.T.);
#22682=ORIENTED_EDGE('',*,*,#17166,.T.);
#22683=ORIENTED_EDGE('',*,*,#17163,.F.);
#22684=ORIENTED_EDGE('',*,*,#16948,.F.);
#22685=ORIENTED_EDGE('',*,*,#17167,.T.);
#22686=ORIENTED_EDGE('',*,*,#17168,.T.);
#22687=ORIENTED_EDGE('',*,*,#17165,.F.);
#22688=ORIENTED_EDGE('',*,*,#16952,.F.);
#22689=ORIENTED_EDGE('',*,*,#17169,.T.);
#22690=ORIENTED_EDGE('',*,*,#17170,.T.);
#22691=ORIENTED_EDGE('',*,*,#17167,.F.);
#22692=ORIENTED_EDGE('',*,*,#16956,.F.);
#22693=ORIENTED_EDGE('',*,*,#17171,.T.);
#22694=ORIENTED_EDGE('',*,*,#17172,.T.);
#22695=ORIENTED_EDGE('',*,*,#17169,.F.);
#22696=ORIENTED_EDGE('',*,*,#16960,.F.);
#22697=ORIENTED_EDGE('',*,*,#17173,.T.);
#22698=ORIENTED_EDGE('',*,*,#17174,.T.);
#22699=ORIENTED_EDGE('',*,*,#17171,.F.);
#22700=ORIENTED_EDGE('',*,*,#16964,.F.);
#22701=ORIENTED_EDGE('',*,*,#17175,.T.);
#22702=ORIENTED_EDGE('',*,*,#17176,.T.);
#22703=ORIENTED_EDGE('',*,*,#17173,.F.);
#22704=ORIENTED_EDGE('',*,*,#16968,.F.);
#22705=ORIENTED_EDGE('',*,*,#17177,.T.);
#22706=ORIENTED_EDGE('',*,*,#17178,.T.);
#22707=ORIENTED_EDGE('',*,*,#17175,.F.);
#22708=ORIENTED_EDGE('',*,*,#16972,.F.);
#22709=ORIENTED_EDGE('',*,*,#17106,.T.);
#22710=ORIENTED_EDGE('',*,*,#17179,.T.);
#22711=ORIENTED_EDGE('',*,*,#17180,.F.);
#22712=ORIENTED_EDGE('',*,*,#16975,.F.);
#22713=ORIENTED_EDGE('',*,*,#17181,.T.);
#22714=ORIENTED_EDGE('',*,*,#17182,.T.);
#22715=ORIENTED_EDGE('',*,*,#17177,.F.);
#22716=ORIENTED_EDGE('',*,*,#16980,.F.);
#22717=ORIENTED_EDGE('',*,*,#17180,.T.);
#22718=ORIENTED_EDGE('',*,*,#17183,.T.);
#22719=ORIENTED_EDGE('',*,*,#17181,.F.);
#22720=ORIENTED_EDGE('',*,*,#16982,.F.);
#22721=ORIENTED_EDGE('',*,*,#17168,.F.);
#22722=ORIENTED_EDGE('',*,*,#17170,.F.);
#22723=ORIENTED_EDGE('',*,*,#17172,.F.);
#22724=ORIENTED_EDGE('',*,*,#17174,.F.);
#22725=ORIENTED_EDGE('',*,*,#17176,.F.);
#22726=ORIENTED_EDGE('',*,*,#17178,.F.);
#22727=ORIENTED_EDGE('',*,*,#17182,.F.);
#22728=ORIENTED_EDGE('',*,*,#17183,.F.);
#22729=ORIENTED_EDGE('',*,*,#17179,.F.);
#22730=ORIENTED_EDGE('',*,*,#17105,.F.);
#22731=ORIENTED_EDGE('',*,*,#17108,.F.);
#22732=ORIENTED_EDGE('',*,*,#17110,.F.);
#22733=ORIENTED_EDGE('',*,*,#17112,.F.);
#22734=ORIENTED_EDGE('',*,*,#17114,.F.);
#22735=ORIENTED_EDGE('',*,*,#17116,.F.);
#22736=ORIENTED_EDGE('',*,*,#17118,.F.);
#22737=ORIENTED_EDGE('',*,*,#17120,.F.);
#22738=ORIENTED_EDGE('',*,*,#17122,.F.);
#22739=ORIENTED_EDGE('',*,*,#17124,.F.);
#22740=ORIENTED_EDGE('',*,*,#17126,.F.);
#22741=ORIENTED_EDGE('',*,*,#17128,.F.);
#22742=ORIENTED_EDGE('',*,*,#17130,.F.);
#22743=ORIENTED_EDGE('',*,*,#17132,.F.);
#22744=ORIENTED_EDGE('',*,*,#17134,.F.);
#22745=ORIENTED_EDGE('',*,*,#17136,.F.);
#22746=ORIENTED_EDGE('',*,*,#17138,.F.);
#22747=ORIENTED_EDGE('',*,*,#17140,.F.);
#22748=ORIENTED_EDGE('',*,*,#17142,.F.);
#22749=ORIENTED_EDGE('',*,*,#17144,.F.);
#22750=ORIENTED_EDGE('',*,*,#17146,.F.);
#22751=ORIENTED_EDGE('',*,*,#17148,.F.);
#22752=ORIENTED_EDGE('',*,*,#17150,.F.);
#22753=ORIENTED_EDGE('',*,*,#17152,.F.);
#22754=ORIENTED_EDGE('',*,*,#17154,.F.);
#22755=ORIENTED_EDGE('',*,*,#17156,.F.);
#22756=ORIENTED_EDGE('',*,*,#17158,.F.);
#22757=ORIENTED_EDGE('',*,*,#17160,.F.);
#22758=ORIENTED_EDGE('',*,*,#17162,.F.);
#22759=ORIENTED_EDGE('',*,*,#17164,.F.);
#22760=ORIENTED_EDGE('',*,*,#17166,.F.);
#22761=ORIENTED_EDGE('',*,*,#17020,.T.);
#22762=ORIENTED_EDGE('',*,*,#16751,.F.);
#22763=ORIENTED_EDGE('',*,*,#17184,.F.);
#22764=ORIENTED_EDGE('',*,*,#17185,.F.);
#22765=ORIENTED_EDGE('',*,*,#17186,.T.);
#22766=ORIENTED_EDGE('',*,*,#17187,.F.);
#22767=ORIENTED_EDGE('',*,*,#17188,.T.);
#22768=ORIENTED_EDGE('',*,*,#17189,.F.);
#22769=ORIENTED_EDGE('',*,*,#17190,.F.);
#22770=ORIENTED_EDGE('',*,*,#17191,.F.);
#22771=ORIENTED_EDGE('',*,*,#17192,.F.);
#22772=ORIENTED_EDGE('',*,*,#17193,.F.);
#22773=ORIENTED_EDGE('',*,*,#16986,.T.);
#22774=ORIENTED_EDGE('',*,*,#17021,.F.);
#22775=ORIENTED_EDGE('',*,*,#17194,.F.);
#22776=ORIENTED_EDGE('',*,*,#17195,.T.);
#22777=ORIENTED_EDGE('',*,*,#17196,.F.);
#22778=ORIENTED_EDGE('',*,*,#17197,.T.);
#22779=ORIENTED_EDGE('',*,*,#17198,.T.);
#22780=ORIENTED_EDGE('',*,*,#17199,.F.);
#22781=ORIENTED_EDGE('',*,*,#17200,.F.);
#22782=ORIENTED_EDGE('',*,*,#17201,.F.);
#22783=ORIENTED_EDGE('',*,*,#17202,.F.);
#22784=ORIENTED_EDGE('',*,*,#17203,.F.);
#22785=ORIENTED_EDGE('',*,*,#17198,.F.);
#22786=ORIENTED_EDGE('',*,*,#17204,.T.);
#22787=ORIENTED_EDGE('',*,*,#17205,.T.);
#22788=ORIENTED_EDGE('',*,*,#17184,.T.);
#22789=ORIENTED_EDGE('',*,*,#16754,.T.);
#22790=ORIENTED_EDGE('',*,*,#17206,.F.);
#22791=ORIENTED_EDGE('',*,*,#17207,.F.);
#22792=ORIENTED_EDGE('',*,*,#17199,.T.);
#22793=ORIENTED_EDGE('',*,*,#17203,.T.);
#22794=ORIENTED_EDGE('',*,*,#17208,.F.);
#22795=ORIENTED_EDGE('',*,*,#17209,.F.);
#22796=ORIENTED_EDGE('',*,*,#17210,.T.);
#22797=ORIENTED_EDGE('',*,*,#17211,.F.);
#22798=ORIENTED_EDGE('',*,*,#17200,.T.);
#22799=ORIENTED_EDGE('',*,*,#17209,.T.);
#22800=ORIENTED_EDGE('',*,*,#17201,.T.);
#22801=ORIENTED_EDGE('',*,*,#17211,.T.);
#22802=ORIENTED_EDGE('',*,*,#17212,.F.);
#22803=ORIENTED_EDGE('',*,*,#17213,.F.);
#22804=ORIENTED_EDGE('',*,*,#17214,.T.);
#22805=ORIENTED_EDGE('',*,*,#17018,.F.);
#22806=ORIENTED_EDGE('',*,*,#17202,.T.);
#22807=ORIENTED_EDGE('',*,*,#17213,.T.);
#22808=ORIENTED_EDGE('',*,*,#17215,.T.);
#22809=ORIENTED_EDGE('',*,*,#17216,.T.);
#22810=ORIENTED_EDGE('',*,*,#17217,.F.);
#22811=ORIENTED_EDGE('',*,*,#17186,.F.);
#22812=ORIENTED_EDGE('',*,*,#17218,.T.);
#22813=ORIENTED_EDGE('',*,*,#17215,.F.);
#22814=ORIENTED_EDGE('',*,*,#17185,.T.);
#22815=ORIENTED_EDGE('',*,*,#17207,.T.);
#22816=ORIENTED_EDGE('',*,*,#17219,.T.);
#22817=ORIENTED_EDGE('',*,*,#17220,.F.);
#22818=ORIENTED_EDGE('',*,*,#17187,.T.);
#22819=ORIENTED_EDGE('',*,*,#17217,.T.);
#22820=ORIENTED_EDGE('',*,*,#17220,.T.);
#22821=ORIENTED_EDGE('',*,*,#17221,.T.);
#22822=ORIENTED_EDGE('',*,*,#17222,.F.);
#22823=ORIENTED_EDGE('',*,*,#17188,.F.);
#22824=ORIENTED_EDGE('',*,*,#17222,.T.);
#22825=ORIENTED_EDGE('',*,*,#17223,.T.);
#22826=ORIENTED_EDGE('',*,*,#17224,.F.);
#22827=ORIENTED_EDGE('',*,*,#17189,.T.);
#22828=ORIENTED_EDGE('',*,*,#17225,.T.);
#22829=ORIENTED_EDGE('',*,*,#17226,.T.);
#22830=ORIENTED_EDGE('',*,*,#17204,.F.);
#22831=ORIENTED_EDGE('',*,*,#17197,.F.);
#22832=ORIENTED_EDGE('',*,*,#17227,.T.);
#22833=ORIENTED_EDGE('',*,*,#17225,.F.);
#22834=ORIENTED_EDGE('',*,*,#17196,.T.);
#22835=ORIENTED_EDGE('',*,*,#17228,.T.);
#22836=ORIENTED_EDGE('',*,*,#17228,.F.);
#22837=ORIENTED_EDGE('',*,*,#17195,.F.);
#22838=ORIENTED_EDGE('',*,*,#17229,.T.);
#22839=ORIENTED_EDGE('',*,*,#17230,.T.);
#22840=ORIENTED_EDGE('',*,*,#17231,.T.);
#22841=ORIENTED_EDGE('',*,*,#16983,.F.);
#22842=ORIENTED_EDGE('',*,*,#17193,.T.);
#22843=ORIENTED_EDGE('',*,*,#17232,.T.);
#22844=ORIENTED_EDGE('',*,*,#17192,.T.);
#22845=ORIENTED_EDGE('',*,*,#17233,.T.);
#22846=ORIENTED_EDGE('',*,*,#17234,.F.);
#22847=ORIENTED_EDGE('',*,*,#17232,.F.);
#22848=ORIENTED_EDGE('',*,*,#17235,.T.);
#22849=ORIENTED_EDGE('',*,*,#17233,.F.);
#22850=ORIENTED_EDGE('',*,*,#17191,.T.);
#22851=ORIENTED_EDGE('',*,*,#17236,.T.);
#22852=ORIENTED_EDGE('',*,*,#17190,.T.);
#22853=ORIENTED_EDGE('',*,*,#17224,.T.);
#22854=ORIENTED_EDGE('',*,*,#17237,.F.);
#22855=ORIENTED_EDGE('',*,*,#17236,.F.);
#22856=ORIENTED_EDGE('',*,*,#17068,.T.);
#22857=ORIENTED_EDGE('',*,*,#17025,.T.);
#22858=ORIENTED_EDGE('',*,*,#17030,.T.);
#22859=ORIENTED_EDGE('',*,*,#17238,.T.);
#22860=ORIENTED_EDGE('',*,*,#17239,.F.);
#22861=ORIENTED_EDGE('',*,*,#17240,.F.);
#22862=ORIENTED_EDGE('',*,*,#17028,.T.);
#22863=ORIENTED_EDGE('',*,*,#17241,.T.);
#22864=ORIENTED_EDGE('',*,*,#17242,.T.);
#22865=ORIENTED_EDGE('',*,*,#17238,.F.);
#22866=ORIENTED_EDGE('',*,*,#17032,.T.);
#22867=ORIENTED_EDGE('',*,*,#17038,.T.);
#22868=ORIENTED_EDGE('',*,*,#17243,.T.);
#22869=ORIENTED_EDGE('',*,*,#17244,.F.);
#22870=ORIENTED_EDGE('',*,*,#17241,.F.);
#22871=ORIENTED_EDGE('',*,*,#17034,.T.);
#22872=ORIENTED_EDGE('',*,*,#17046,.T.);
#22873=ORIENTED_EDGE('',*,*,#17245,.T.);
#22874=ORIENTED_EDGE('',*,*,#17246,.F.);
#22875=ORIENTED_EDGE('',*,*,#17247,.F.);
#22876=ORIENTED_EDGE('',*,*,#17036,.T.);
#22877=ORIENTED_EDGE('',*,*,#17247,.T.);
#22878=ORIENTED_EDGE('',*,*,#17248,.T.);
#22879=ORIENTED_EDGE('',*,*,#17243,.F.);
#22880=ORIENTED_EDGE('',*,*,#17040,.T.);
#22881=ORIENTED_EDGE('',*,*,#17249,.T.);
#22882=ORIENTED_EDGE('',*,*,#17250,.F.);
#22883=ORIENTED_EDGE('',*,*,#17245,.F.);
#22884=ORIENTED_EDGE('',*,*,#17043,.T.);
#22885=ORIENTED_EDGE('',*,*,#17251,.T.);
#22886=ORIENTED_EDGE('',*,*,#17252,.F.);
#22887=ORIENTED_EDGE('',*,*,#17249,.F.);
#22888=ORIENTED_EDGE('',*,*,#17045,.T.);
#22889=ORIENTED_EDGE('',*,*,#17048,.T.);
#22890=ORIENTED_EDGE('',*,*,#17253,.T.);
#22891=ORIENTED_EDGE('',*,*,#17254,.F.);
#22892=ORIENTED_EDGE('',*,*,#17251,.F.);
#22893=ORIENTED_EDGE('',*,*,#17050,.T.);
#22894=ORIENTED_EDGE('',*,*,#17052,.T.);
#22895=ORIENTED_EDGE('',*,*,#17255,.T.);
#22896=ORIENTED_EDGE('',*,*,#17256,.T.);
#22897=ORIENTED_EDGE('',*,*,#17253,.F.);
#22898=ORIENTED_EDGE('',*,*,#17054,.T.);
#22899=ORIENTED_EDGE('',*,*,#17257,.T.);
#22900=ORIENTED_EDGE('',*,*,#17258,.F.);
#22901=ORIENTED_EDGE('',*,*,#17255,.F.);
#22902=ORIENTED_EDGE('',*,*,#17056,.T.);
#22903=ORIENTED_EDGE('',*,*,#17062,.T.);
#22904=ORIENTED_EDGE('',*,*,#17259,.F.);
#22905=ORIENTED_EDGE('',*,*,#17257,.F.);
#22906=ORIENTED_EDGE('',*,*,#17260,.T.);
#22907=ORIENTED_EDGE('',*,*,#17229,.F.);
#22908=ORIENTED_EDGE('',*,*,#17194,.T.);
#22909=ORIENTED_EDGE('',*,*,#17023,.T.);
#22910=ORIENTED_EDGE('',*,*,#17070,.T.);
#22911=ORIENTED_EDGE('',*,*,#17240,.T.);
#22912=ORIENTED_EDGE('',*,*,#17261,.T.);
#22913=ORIENTED_EDGE('',*,*,#17065,.F.);
#22914=ORIENTED_EDGE('',*,*,#17006,.T.);
#22915=ORIENTED_EDGE('',*,*,#17262,.T.);
#22916=ORIENTED_EDGE('',*,*,#17263,.F.);
#22917=ORIENTED_EDGE('',*,*,#17073,.F.);
#22918=ORIENTED_EDGE('',*,*,#17078,.F.);
#22919=ORIENTED_EDGE('',*,*,#17083,.F.);
#22920=ORIENTED_EDGE('',*,*,#17263,.T.);
#22921=ORIENTED_EDGE('',*,*,#17264,.F.);
#22922=ORIENTED_EDGE('',*,*,#16991,.F.);
#22923=ORIENTED_EDGE('',*,*,#17075,.F.);
#22924=ORIENTED_EDGE('',*,*,#17265,.F.);
#22925=ORIENTED_EDGE('',*,*,#17266,.T.);
#22926=ORIENTED_EDGE('',*,*,#17267,.T.);
#22927=ORIENTED_EDGE('',*,*,#17268,.T.);
#22928=ORIENTED_EDGE('',*,*,#17269,.T.);
#22929=ORIENTED_EDGE('',*,*,#17270,.T.);
#22930=ORIENTED_EDGE('',*,*,#17266,.F.);
#22931=ORIENTED_EDGE('',*,*,#17271,.F.);
#22932=ORIENTED_EDGE('',*,*,#17272,.T.);
#22933=ORIENTED_EDGE('',*,*,#17273,.T.);
#22934=ORIENTED_EDGE('',*,*,#17269,.F.);
#22935=ORIENTED_EDGE('',*,*,#17274,.F.);
#22936=ORIENTED_EDGE('',*,*,#16750,.T.);
#22937=ORIENTED_EDGE('',*,*,#17275,.T.);
#22938=ORIENTED_EDGE('',*,*,#17272,.F.);
#22939=ORIENTED_EDGE('',*,*,#17276,.F.);
#22940=ORIENTED_EDGE('',*,*,#16730,.T.);
#22941=ORIENTED_EDGE('',*,*,#16674,.F.);
#22942=ORIENTED_EDGE('',*,*,#17276,.T.);
#22943=ORIENTED_EDGE('',*,*,#17274,.T.);
#22944=ORIENTED_EDGE('',*,*,#17271,.T.);
#22945=ORIENTED_EDGE('',*,*,#17265,.T.);
#22946=ORIENTED_EDGE('',*,*,#17277,.F.);
#22947=ORIENTED_EDGE('',*,*,#17277,.T.);
#22948=ORIENTED_EDGE('',*,*,#17278,.F.);
#22949=ORIENTED_EDGE('',*,*,#17279,.F.);
#22950=ORIENTED_EDGE('',*,*,#17280,.F.);
#22951=ORIENTED_EDGE('',*,*,#17281,.F.);
#22952=ORIENTED_EDGE('',*,*,#17282,.T.);
#22953=ORIENTED_EDGE('',*,*,#16731,.F.);
#22954=ORIENTED_EDGE('',*,*,#16732,.T.);
#22955=ORIENTED_EDGE('',*,*,#17282,.F.);
#22956=ORIENTED_EDGE('',*,*,#17283,.F.);
#22957=ORIENTED_EDGE('',*,*,#17284,.T.);
#22958=ORIENTED_EDGE('',*,*,#17284,.F.);
#22959=ORIENTED_EDGE('',*,*,#17285,.F.);
#22960=ORIENTED_EDGE('',*,*,#17286,.F.);
#22961=ORIENTED_EDGE('',*,*,#17287,.F.);
#22962=ORIENTED_EDGE('',*,*,#16733,.T.);
#22963=ORIENTED_EDGE('',*,*,#17287,.T.);
#22964=ORIENTED_EDGE('',*,*,#17288,.F.);
#22965=ORIENTED_EDGE('',*,*,#17289,.F.);
#22966=ORIENTED_EDGE('',*,*,#17290,.F.);
#22967=ORIENTED_EDGE('',*,*,#16726,.F.);
#22968=ORIENTED_EDGE('',*,*,#16727,.T.);
#22969=ORIENTED_EDGE('',*,*,#17290,.T.);
#22970=ORIENTED_EDGE('',*,*,#17291,.F.);
#22971=ORIENTED_EDGE('',*,*,#17292,.F.);
#22972=ORIENTED_EDGE('',*,*,#17293,.T.);
#22973=ORIENTED_EDGE('',*,*,#17294,.T.);
#22974=ORIENTED_EDGE('',*,*,#17295,.F.);
#22975=ORIENTED_EDGE('',*,*,#16728,.T.);
#22976=ORIENTED_EDGE('',*,*,#17295,.T.);
#22977=ORIENTED_EDGE('',*,*,#17296,.T.);
#22978=ORIENTED_EDGE('',*,*,#17297,.T.);
#22979=ORIENTED_EDGE('',*,*,#17298,.F.);
#22980=ORIENTED_EDGE('',*,*,#16729,.F.);
#22981=ORIENTED_EDGE('',*,*,#17298,.T.);
#22982=ORIENTED_EDGE('',*,*,#17299,.T.);
#22983=ORIENTED_EDGE('',*,*,#17300,.T.);
#22984=ORIENTED_EDGE('',*,*,#16672,.T.);
#22985=ORIENTED_EDGE('',*,*,#17301,.T.);
#22986=ORIENTED_EDGE('',*,*,#17302,.T.);
#22987=ORIENTED_EDGE('',*,*,#16749,.F.);
#22988=ORIENTED_EDGE('',*,*,#17300,.F.);
#22989=ORIENTED_EDGE('',*,*,#17303,.T.);
#22990=ORIENTED_EDGE('',*,*,#17304,.T.);
#22991=ORIENTED_EDGE('',*,*,#17301,.F.);
#22992=ORIENTED_EDGE('',*,*,#17299,.F.);
#22993=ORIENTED_EDGE('',*,*,#17305,.T.);
#22994=ORIENTED_EDGE('',*,*,#17306,.T.);
#22995=ORIENTED_EDGE('',*,*,#17303,.F.);
#22996=ORIENTED_EDGE('',*,*,#17297,.F.);
#22997=ORIENTED_EDGE('',*,*,#17307,.T.);
#22998=ORIENTED_EDGE('',*,*,#17308,.T.);
#22999=ORIENTED_EDGE('',*,*,#17305,.F.);
#23000=ORIENTED_EDGE('',*,*,#17296,.F.);
#23001=ORIENTED_EDGE('',*,*,#17309,.T.);
#23002=ORIENTED_EDGE('',*,*,#17310,.T.);
#23003=ORIENTED_EDGE('',*,*,#17307,.F.);
#23004=ORIENTED_EDGE('',*,*,#17294,.F.);
#23005=ORIENTED_EDGE('',*,*,#17311,.T.);
#23006=ORIENTED_EDGE('',*,*,#17309,.F.);
#23007=ORIENTED_EDGE('',*,*,#17293,.F.);
#23008=ORIENTED_EDGE('',*,*,#17312,.T.);
#23009=ORIENTED_EDGE('',*,*,#17312,.F.);
#23010=ORIENTED_EDGE('',*,*,#17292,.T.);
#23011=ORIENTED_EDGE('',*,*,#17313,.T.);
#23012=ORIENTED_EDGE('',*,*,#17314,.F.);
#23013=ORIENTED_EDGE('',*,*,#17291,.T.);
#23014=ORIENTED_EDGE('',*,*,#17315,.T.);
#23015=ORIENTED_EDGE('',*,*,#17316,.F.);
#23016=ORIENTED_EDGE('',*,*,#17313,.F.);
#23017=ORIENTED_EDGE('',*,*,#17289,.T.);
#23018=ORIENTED_EDGE('',*,*,#17317,.T.);
#23019=ORIENTED_EDGE('',*,*,#17318,.F.);
#23020=ORIENTED_EDGE('',*,*,#17315,.F.);
#23021=ORIENTED_EDGE('',*,*,#17288,.T.);
#23022=ORIENTED_EDGE('',*,*,#17319,.T.);
#23023=ORIENTED_EDGE('',*,*,#17320,.F.);
#23024=ORIENTED_EDGE('',*,*,#17317,.F.);
#23025=ORIENTED_EDGE('',*,*,#17286,.T.);
#23026=ORIENTED_EDGE('',*,*,#17321,.T.);
#23027=ORIENTED_EDGE('',*,*,#17322,.F.);
#23028=ORIENTED_EDGE('',*,*,#17319,.F.);
#23029=ORIENTED_EDGE('',*,*,#17285,.T.);
#23030=ORIENTED_EDGE('',*,*,#17323,.T.);
#23031=ORIENTED_EDGE('',*,*,#17324,.F.);
#23032=ORIENTED_EDGE('',*,*,#17321,.F.);
#23033=ORIENTED_EDGE('',*,*,#17283,.T.);
#23034=ORIENTED_EDGE('',*,*,#17325,.T.);
#23035=ORIENTED_EDGE('',*,*,#17323,.F.);
#23036=ORIENTED_EDGE('',*,*,#17281,.T.);
#23037=ORIENTED_EDGE('',*,*,#17326,.T.);
#23038=ORIENTED_EDGE('',*,*,#17327,.F.);
#23039=ORIENTED_EDGE('',*,*,#17325,.F.);
#23040=ORIENTED_EDGE('',*,*,#17280,.T.);
#23041=ORIENTED_EDGE('',*,*,#17328,.T.);
#23042=ORIENTED_EDGE('',*,*,#17329,.F.);
#23043=ORIENTED_EDGE('',*,*,#17326,.F.);
#23044=ORIENTED_EDGE('',*,*,#17279,.T.);
#23045=ORIENTED_EDGE('',*,*,#17330,.T.);
#23046=ORIENTED_EDGE('',*,*,#17331,.F.);
#23047=ORIENTED_EDGE('',*,*,#17328,.F.);
#23048=ORIENTED_EDGE('',*,*,#17268,.F.);
#23049=ORIENTED_EDGE('',*,*,#17332,.F.);
#23050=ORIENTED_EDGE('',*,*,#17330,.F.);
#23051=ORIENTED_EDGE('',*,*,#17278,.T.);
#23052=ORIENTED_EDGE('',*,*,#17332,.T.);
#23053=ORIENTED_EDGE('',*,*,#17333,.T.);
#23054=ORIENTED_EDGE('',*,*,#17334,.T.);
#23055=ORIENTED_EDGE('',*,*,#17335,.T.);
#23056=ORIENTED_EDGE('',*,*,#17336,.F.);
#23057=ORIENTED_EDGE('',*,*,#17337,.T.);
#23058=ORIENTED_EDGE('',*,*,#17338,.F.);
#23059=ORIENTED_EDGE('',*,*,#17334,.F.);
#23060=ORIENTED_EDGE('',*,*,#17333,.F.);
#23061=ORIENTED_EDGE('',*,*,#17267,.F.);
#23062=ORIENTED_EDGE('',*,*,#17339,.T.);
#23063=ORIENTED_EDGE('',*,*,#17340,.F.);
#23064=ORIENTED_EDGE('',*,*,#17337,.F.);
#23065=ORIENTED_EDGE('',*,*,#17270,.F.);
#23066=ORIENTED_EDGE('',*,*,#17341,.T.);
#23067=ORIENTED_EDGE('',*,*,#17342,.F.);
#23068=ORIENTED_EDGE('',*,*,#17339,.F.);
#23069=ORIENTED_EDGE('',*,*,#17273,.F.);
#23070=ORIENTED_EDGE('',*,*,#17343,.T.);
#23071=ORIENTED_EDGE('',*,*,#17344,.T.);
#23072=ORIENTED_EDGE('',*,*,#17341,.F.);
#23073=ORIENTED_EDGE('',*,*,#17275,.F.);
#23074=ORIENTED_EDGE('',*,*,#17302,.F.);
#23075=ORIENTED_EDGE('',*,*,#17345,.T.);
#23076=ORIENTED_EDGE('',*,*,#17346,.T.);
#23077=ORIENTED_EDGE('',*,*,#17343,.F.);
#23078=ORIENTED_EDGE('',*,*,#17304,.F.);
#23079=ORIENTED_EDGE('',*,*,#17306,.F.);
#23080=ORIENTED_EDGE('',*,*,#17347,.T.);
#23081=ORIENTED_EDGE('',*,*,#17348,.F.);
#23082=ORIENTED_EDGE('',*,*,#17345,.F.);
#23083=ORIENTED_EDGE('',*,*,#17308,.F.);
#23084=ORIENTED_EDGE('',*,*,#17310,.F.);
#23085=ORIENTED_EDGE('',*,*,#17349,.T.);
#23086=ORIENTED_EDGE('',*,*,#17350,.F.);
#23087=ORIENTED_EDGE('',*,*,#17347,.F.);
#23088=ORIENTED_EDGE('',*,*,#17311,.F.);
#23089=ORIENTED_EDGE('',*,*,#17314,.T.);
#23090=ORIENTED_EDGE('',*,*,#17351,.T.);
#23091=ORIENTED_EDGE('',*,*,#17352,.T.);
#23092=ORIENTED_EDGE('',*,*,#17349,.F.);
#23093=ORIENTED_EDGE('',*,*,#17316,.T.);
#23094=ORIENTED_EDGE('',*,*,#17318,.T.);
#23095=ORIENTED_EDGE('',*,*,#17353,.T.);
#23096=ORIENTED_EDGE('',*,*,#17354,.T.);
#23097=ORIENTED_EDGE('',*,*,#17351,.F.);
#23098=ORIENTED_EDGE('',*,*,#17320,.T.);
#23099=ORIENTED_EDGE('',*,*,#17322,.T.);
#23100=ORIENTED_EDGE('',*,*,#17355,.T.);
#23101=ORIENTED_EDGE('',*,*,#17356,.F.);
#23102=ORIENTED_EDGE('',*,*,#17353,.F.);
#23103=ORIENTED_EDGE('',*,*,#17324,.T.);
#23104=ORIENTED_EDGE('',*,*,#17327,.T.);
#23105=ORIENTED_EDGE('',*,*,#17357,.T.);
#23106=ORIENTED_EDGE('',*,*,#17358,.F.);
#23107=ORIENTED_EDGE('',*,*,#17355,.F.);
#23108=ORIENTED_EDGE('',*,*,#17329,.T.);
#23109=ORIENTED_EDGE('',*,*,#17359,.T.);
#23110=ORIENTED_EDGE('',*,*,#17360,.T.);
#23111=ORIENTED_EDGE('',*,*,#17357,.F.);
#23112=ORIENTED_EDGE('',*,*,#17331,.T.);
#23113=ORIENTED_EDGE('',*,*,#17336,.T.);
#23114=ORIENTED_EDGE('',*,*,#17361,.T.);
#23115=ORIENTED_EDGE('',*,*,#17359,.F.);
#23116=ORIENTED_EDGE('',*,*,#17362,.F.);
#23117=ORIENTED_EDGE('',*,*,#17363,.F.);
#23118=ORIENTED_EDGE('',*,*,#17364,.F.);
#23119=ORIENTED_EDGE('',*,*,#17365,.F.);
#23120=ORIENTED_EDGE('',*,*,#17366,.T.);
#23121=ORIENTED_EDGE('',*,*,#17367,.T.);
#23122=ORIENTED_EDGE('',*,*,#17368,.T.);
#23123=ORIENTED_EDGE('',*,*,#17013,.F.);
#23124=ORIENTED_EDGE('',*,*,#17015,.T.);
#23125=ORIENTED_EDGE('',*,*,#16745,.F.);
#23126=ORIENTED_EDGE('',*,*,#17002,.F.);
#23127=ORIENTED_EDGE('',*,*,#16999,.F.);
#23128=ORIENTED_EDGE('',*,*,#16995,.F.);
#23129=ORIENTED_EDGE('',*,*,#16988,.T.);
#23130=ORIENTED_EDGE('',*,*,#16992,.F.);
#23131=ORIENTED_EDGE('',*,*,#17264,.T.);
#23132=ORIENTED_EDGE('',*,*,#17262,.F.);
#23133=ORIENTED_EDGE('',*,*,#17005,.T.);
#23134=ORIENTED_EDGE('',*,*,#17086,.F.);
#23135=ORIENTED_EDGE('',*,*,#17087,.F.);
#23136=ORIENTED_EDGE('',*,*,#17009,.F.);
#23137=ORIENTED_EDGE('',*,*,#17354,.F.);
#23138=ORIENTED_EDGE('',*,*,#17356,.T.);
#23139=ORIENTED_EDGE('',*,*,#17358,.T.);
#23140=ORIENTED_EDGE('',*,*,#17360,.F.);
#23141=ORIENTED_EDGE('',*,*,#17361,.F.);
#23142=ORIENTED_EDGE('',*,*,#17335,.F.);
#23143=ORIENTED_EDGE('',*,*,#17338,.T.);
#23144=ORIENTED_EDGE('',*,*,#17340,.T.);
#23145=ORIENTED_EDGE('',*,*,#17342,.T.);
#23146=ORIENTED_EDGE('',*,*,#17344,.F.);
#23147=ORIENTED_EDGE('',*,*,#17346,.F.);
#23148=ORIENTED_EDGE('',*,*,#17348,.T.);
#23149=ORIENTED_EDGE('',*,*,#17350,.T.);
#23150=ORIENTED_EDGE('',*,*,#17352,.F.);
#23151=ORIENTED_EDGE('',*,*,#17250,.T.);
#23152=ORIENTED_EDGE('',*,*,#17252,.T.);
#23153=ORIENTED_EDGE('',*,*,#17254,.T.);
#23154=ORIENTED_EDGE('',*,*,#17256,.F.);
#23155=ORIENTED_EDGE('',*,*,#17258,.T.);
#23156=ORIENTED_EDGE('',*,*,#17259,.T.);
#23157=ORIENTED_EDGE('',*,*,#17061,.T.);
#23158=ORIENTED_EDGE('',*,*,#17066,.T.);
#23159=ORIENTED_EDGE('',*,*,#17261,.F.);
#23160=ORIENTED_EDGE('',*,*,#17239,.T.);
#23161=ORIENTED_EDGE('',*,*,#17242,.F.);
#23162=ORIENTED_EDGE('',*,*,#17244,.T.);
#23163=ORIENTED_EDGE('',*,*,#17248,.F.);
#23164=ORIENTED_EDGE('',*,*,#17246,.T.);
#23165=ORIENTED_EDGE('',*,*,#17369,.F.);
#23166=ORIENTED_EDGE('',*,*,#17370,.F.);
#23167=ORIENTED_EDGE('',*,*,#17363,.T.);
#23168=ORIENTED_EDGE('',*,*,#17371,.T.);
#23169=ORIENTED_EDGE('',*,*,#17372,.F.);
#23170=ORIENTED_EDGE('',*,*,#17364,.T.);
#23171=ORIENTED_EDGE('',*,*,#17370,.T.);
#23172=ORIENTED_EDGE('',*,*,#17373,.F.);
#23173=ORIENTED_EDGE('',*,*,#17374,.F.);
#23174=ORIENTED_EDGE('',*,*,#17365,.T.);
#23175=ORIENTED_EDGE('',*,*,#17372,.T.);
#23176=ORIENTED_EDGE('',*,*,#17375,.F.);
#23177=ORIENTED_EDGE('',*,*,#17376,.T.);
#23178=ORIENTED_EDGE('',*,*,#17377,.F.);
#23179=ORIENTED_EDGE('',*,*,#17366,.F.);
#23180=ORIENTED_EDGE('',*,*,#17374,.T.);
#23181=ORIENTED_EDGE('',*,*,#17378,.T.);
#23182=ORIENTED_EDGE('',*,*,#17379,.F.);
#23183=ORIENTED_EDGE('',*,*,#17367,.F.);
#23184=ORIENTED_EDGE('',*,*,#17377,.T.);
#23185=ORIENTED_EDGE('',*,*,#17368,.F.);
#23186=ORIENTED_EDGE('',*,*,#17379,.T.);
#23187=ORIENTED_EDGE('',*,*,#17380,.T.);
#23188=ORIENTED_EDGE('',*,*,#17381,.F.);
#23189=ORIENTED_EDGE('',*,*,#17382,.T.);
#23190=ORIENTED_EDGE('',*,*,#17371,.F.);
#23191=ORIENTED_EDGE('',*,*,#17362,.T.);
#23192=ORIENTED_EDGE('',*,*,#17381,.T.);
#23193=ORIENTED_EDGE('',*,*,#16753,.T.);
#23194=ORIENTED_EDGE('',*,*,#17019,.F.);
#23195=ORIENTED_EDGE('',*,*,#17214,.F.);
#23196=ORIENTED_EDGE('',*,*,#17212,.T.);
#23197=ORIENTED_EDGE('',*,*,#17210,.F.);
#23198=ORIENTED_EDGE('',*,*,#17208,.T.);
#23199=ORIENTED_EDGE('',*,*,#17205,.F.);
#23200=ORIENTED_EDGE('',*,*,#17226,.F.);
#23201=ORIENTED_EDGE('',*,*,#17227,.F.);
#23202=ORIENTED_EDGE('',*,*,#17230,.F.);
#23203=ORIENTED_EDGE('',*,*,#17260,.F.);
#23204=ORIENTED_EDGE('',*,*,#17022,.F.);
#23205=ORIENTED_EDGE('',*,*,#16984,.T.);
#23206=ORIENTED_EDGE('',*,*,#17231,.F.);
#23207=ORIENTED_EDGE('',*,*,#17234,.T.);
#23208=ORIENTED_EDGE('',*,*,#17235,.F.);
#23209=ORIENTED_EDGE('',*,*,#17237,.T.);
#23210=ORIENTED_EDGE('',*,*,#17223,.F.);
#23211=ORIENTED_EDGE('',*,*,#17221,.F.);
#23212=ORIENTED_EDGE('',*,*,#17219,.F.);
#23213=ORIENTED_EDGE('',*,*,#17216,.F.);
#23214=ORIENTED_EDGE('',*,*,#17218,.F.);
#23215=ORIENTED_EDGE('',*,*,#17206,.T.);
#23216=ORIENTED_EDGE('',*,*,#17380,.F.);
#23217=ORIENTED_EDGE('',*,*,#17378,.F.);
#23218=ORIENTED_EDGE('',*,*,#17376,.F.);
#23219=ORIENTED_EDGE('',*,*,#17375,.T.);
#23220=ORIENTED_EDGE('',*,*,#17373,.T.);
#23221=ORIENTED_EDGE('',*,*,#17369,.T.);
#23222=ORIENTED_EDGE('',*,*,#17382,.F.);
#23223=ORIENTED_EDGE('',*,*,#17383,.T.);
#23224=ORIENTED_EDGE('',*,*,#17384,.T.);
#23225=ORIENTED_EDGE('',*,*,#17385,.T.);
#23226=ORIENTED_EDGE('',*,*,#17386,.T.);
#23227=ORIENTED_EDGE('',*,*,#17387,.T.);
#23228=ORIENTED_EDGE('',*,*,#17388,.T.);
#23229=ORIENTED_EDGE('',*,*,#17389,.T.);
#23230=ORIENTED_EDGE('',*,*,#17390,.T.);
#23231=ORIENTED_EDGE('',*,*,#17391,.T.);
#23232=ORIENTED_EDGE('',*,*,#17392,.T.);
#23233=ORIENTED_EDGE('',*,*,#17393,.T.);
#23234=ORIENTED_EDGE('',*,*,#17394,.F.);
#23235=ORIENTED_EDGE('',*,*,#17395,.F.);
#23236=ORIENTED_EDGE('',*,*,#17396,.F.);
#23237=ORIENTED_EDGE('',*,*,#17397,.F.);
#23238=ORIENTED_EDGE('',*,*,#17398,.F.);
#23239=ORIENTED_EDGE('',*,*,#17399,.F.);
#23240=ORIENTED_EDGE('',*,*,#17400,.F.);
#23241=ORIENTED_EDGE('',*,*,#17401,.F.);
#23242=ORIENTED_EDGE('',*,*,#17402,.F.);
#23243=ORIENTED_EDGE('',*,*,#17403,.F.);
#23244=ORIENTED_EDGE('',*,*,#17404,.F.);
#23245=ORIENTED_EDGE('',*,*,#17405,.F.);
#23246=ORIENTED_EDGE('',*,*,#17406,.F.);
#23247=ORIENTED_EDGE('',*,*,#17407,.F.);
#23248=ORIENTED_EDGE('',*,*,#17408,.F.);
#23249=ORIENTED_EDGE('',*,*,#17409,.F.);
#23250=ORIENTED_EDGE('',*,*,#17410,.F.);
#23251=ORIENTED_EDGE('',*,*,#17411,.F.);
#23252=ORIENTED_EDGE('',*,*,#17412,.F.);
#23253=ORIENTED_EDGE('',*,*,#17413,.F.);
#23254=ORIENTED_EDGE('',*,*,#17414,.F.);
#23255=ORIENTED_EDGE('',*,*,#17415,.F.);
#23256=ORIENTED_EDGE('',*,*,#17416,.F.);
#23257=ORIENTED_EDGE('',*,*,#17417,.F.);
#23258=ORIENTED_EDGE('',*,*,#17418,.F.);
#23259=ORIENTED_EDGE('',*,*,#17419,.F.);
#23260=ORIENTED_EDGE('',*,*,#17420,.F.);
#23261=ORIENTED_EDGE('',*,*,#17421,.F.);
#23262=ORIENTED_EDGE('',*,*,#17422,.F.);
#23263=ORIENTED_EDGE('',*,*,#17423,.F.);
#23264=ORIENTED_EDGE('',*,*,#17424,.F.);
#23265=ORIENTED_EDGE('',*,*,#17425,.F.);
#23266=ORIENTED_EDGE('',*,*,#17426,.F.);
#23267=ORIENTED_EDGE('',*,*,#17427,.F.);
#23268=ORIENTED_EDGE('',*,*,#17428,.F.);
#23269=ORIENTED_EDGE('',*,*,#17429,.F.);
#23270=ORIENTED_EDGE('',*,*,#17430,.T.);
#23271=ORIENTED_EDGE('',*,*,#17431,.T.);
#23272=ORIENTED_EDGE('',*,*,#17432,.T.);
#23273=ORIENTED_EDGE('',*,*,#17433,.T.);
#23274=ORIENTED_EDGE('',*,*,#17434,.T.);
#23275=ORIENTED_EDGE('',*,*,#17435,.T.);
#23276=ORIENTED_EDGE('',*,*,#17436,.T.);
#23277=ORIENTED_EDGE('',*,*,#17437,.T.);
#23278=ORIENTED_EDGE('',*,*,#17438,.T.);
#23279=ORIENTED_EDGE('',*,*,#17439,.T.);
#23280=ORIENTED_EDGE('',*,*,#17440,.T.);
#23281=ORIENTED_EDGE('',*,*,#17441,.T.);
#23282=ORIENTED_EDGE('',*,*,#17442,.T.);
#23283=ORIENTED_EDGE('',*,*,#17443,.T.);
#23284=ORIENTED_EDGE('',*,*,#17444,.T.);
#23285=ORIENTED_EDGE('',*,*,#17445,.T.);
#23286=ORIENTED_EDGE('',*,*,#17446,.T.);
#23287=ORIENTED_EDGE('',*,*,#17447,.T.);
#23288=ORIENTED_EDGE('',*,*,#17448,.T.);
#23289=ORIENTED_EDGE('',*,*,#17449,.T.);
#23290=ORIENTED_EDGE('',*,*,#17450,.T.);
#23291=ORIENTED_EDGE('',*,*,#17451,.T.);
#23292=ORIENTED_EDGE('',*,*,#17452,.T.);
#23293=ORIENTED_EDGE('',*,*,#17453,.T.);
#23294=ORIENTED_EDGE('',*,*,#17454,.T.);
#23295=ORIENTED_EDGE('',*,*,#17455,.T.);
#23296=ORIENTED_EDGE('',*,*,#17403,.T.);
#23297=ORIENTED_EDGE('',*,*,#17456,.F.);
#23298=ORIENTED_EDGE('',*,*,#17457,.F.);
#23299=ORIENTED_EDGE('',*,*,#17458,.T.);
#23300=ORIENTED_EDGE('',*,*,#17459,.T.);
#23301=ORIENTED_EDGE('',*,*,#17460,.F.);
#23302=ORIENTED_EDGE('',*,*,#17447,.F.);
#23303=ORIENTED_EDGE('',*,*,#17459,.F.);
#23304=ORIENTED_EDGE('',*,*,#17461,.T.);
#23305=ORIENTED_EDGE('',*,*,#17457,.T.);
#23306=ORIENTED_EDGE('',*,*,#17462,.F.);
#23307=ORIENTED_EDGE('',*,*,#17456,.T.);
#23308=ORIENTED_EDGE('',*,*,#17411,.T.);
#23309=ORIENTED_EDGE('',*,*,#17463,.F.);
#23310=ORIENTED_EDGE('',*,*,#17464,.F.);
#23311=ORIENTED_EDGE('',*,*,#17460,.T.);
#23312=ORIENTED_EDGE('',*,*,#17465,.T.);
#23313=ORIENTED_EDGE('',*,*,#17466,.F.);
#23314=ORIENTED_EDGE('',*,*,#17439,.F.);
#23315=ORIENTED_EDGE('',*,*,#17465,.F.);
#23316=ORIENTED_EDGE('',*,*,#17462,.T.);
#23317=ORIENTED_EDGE('',*,*,#17464,.T.);
#23318=ORIENTED_EDGE('',*,*,#17467,.F.);
#23319=ORIENTED_EDGE('',*,*,#17463,.T.);
#23320=ORIENTED_EDGE('',*,*,#17410,.T.);
#23321=ORIENTED_EDGE('',*,*,#17468,.F.);
#23322=ORIENTED_EDGE('',*,*,#17469,.F.);
#23323=ORIENTED_EDGE('',*,*,#17466,.T.);
#23324=ORIENTED_EDGE('',*,*,#17470,.T.);
#23325=ORIENTED_EDGE('',*,*,#17471,.F.);
#23326=ORIENTED_EDGE('',*,*,#17440,.F.);
#23327=ORIENTED_EDGE('',*,*,#17470,.F.);
#23328=ORIENTED_EDGE('',*,*,#17467,.T.);
#23329=ORIENTED_EDGE('',*,*,#17469,.T.);
#23330=ORIENTED_EDGE('',*,*,#17472,.F.);
#23331=ORIENTED_EDGE('',*,*,#17468,.T.);
#23332=ORIENTED_EDGE('',*,*,#17409,.T.);
#23333=ORIENTED_EDGE('',*,*,#17473,.F.);
#23334=ORIENTED_EDGE('',*,*,#17474,.F.);
#23335=ORIENTED_EDGE('',*,*,#17471,.T.);
#23336=ORIENTED_EDGE('',*,*,#17475,.T.);
#23337=ORIENTED_EDGE('',*,*,#17476,.F.);
#23338=ORIENTED_EDGE('',*,*,#17441,.F.);
#23339=ORIENTED_EDGE('',*,*,#17475,.F.);
#23340=ORIENTED_EDGE('',*,*,#17472,.T.);
#23341=ORIENTED_EDGE('',*,*,#17474,.T.);
#23342=ORIENTED_EDGE('',*,*,#17477,.F.);
#23343=ORIENTED_EDGE('',*,*,#17473,.T.);
#23344=ORIENTED_EDGE('',*,*,#17408,.T.);
#23345=ORIENTED_EDGE('',*,*,#17478,.F.);
#23346=ORIENTED_EDGE('',*,*,#17479,.F.);
#23347=ORIENTED_EDGE('',*,*,#17476,.T.);
#23348=ORIENTED_EDGE('',*,*,#17480,.T.);
#23349=ORIENTED_EDGE('',*,*,#17481,.F.);
#23350=ORIENTED_EDGE('',*,*,#17442,.F.);
#23351=ORIENTED_EDGE('',*,*,#17480,.F.);
#23352=ORIENTED_EDGE('',*,*,#17477,.T.);
#23353=ORIENTED_EDGE('',*,*,#17479,.T.);
#23354=ORIENTED_EDGE('',*,*,#17482,.F.);
#23355=ORIENTED_EDGE('',*,*,#17478,.T.);
#23356=ORIENTED_EDGE('',*,*,#17407,.T.);
#23357=ORIENTED_EDGE('',*,*,#17483,.F.);
#23358=ORIENTED_EDGE('',*,*,#17484,.F.);
#23359=ORIENTED_EDGE('',*,*,#17481,.T.);
#23360=ORIENTED_EDGE('',*,*,#17485,.T.);
#23361=ORIENTED_EDGE('',*,*,#17486,.F.);
#23362=ORIENTED_EDGE('',*,*,#17443,.F.);
#23363=ORIENTED_EDGE('',*,*,#17485,.F.);
#23364=ORIENTED_EDGE('',*,*,#17482,.T.);
#23365=ORIENTED_EDGE('',*,*,#17484,.T.);
#23366=ORIENTED_EDGE('',*,*,#17487,.F.);
#23367=ORIENTED_EDGE('',*,*,#17483,.T.);
#23368=ORIENTED_EDGE('',*,*,#17406,.T.);
#23369=ORIENTED_EDGE('',*,*,#17488,.F.);
#23370=ORIENTED_EDGE('',*,*,#17489,.F.);
#23371=ORIENTED_EDGE('',*,*,#17486,.T.);
#23372=ORIENTED_EDGE('',*,*,#17490,.T.);
#23373=ORIENTED_EDGE('',*,*,#17491,.F.);
#23374=ORIENTED_EDGE('',*,*,#17444,.F.);
#23375=ORIENTED_EDGE('',*,*,#17490,.F.);
#23376=ORIENTED_EDGE('',*,*,#17487,.T.);
#23377=ORIENTED_EDGE('',*,*,#17489,.T.);
#23378=ORIENTED_EDGE('',*,*,#17492,.F.);
#23379=ORIENTED_EDGE('',*,*,#17488,.T.);
#23380=ORIENTED_EDGE('',*,*,#17405,.T.);
#23381=ORIENTED_EDGE('',*,*,#17493,.F.);
#23382=ORIENTED_EDGE('',*,*,#17494,.F.);
#23383=ORIENTED_EDGE('',*,*,#17491,.T.);
#23384=ORIENTED_EDGE('',*,*,#17495,.T.);
#23385=ORIENTED_EDGE('',*,*,#17496,.F.);
#23386=ORIENTED_EDGE('',*,*,#17445,.F.);
#23387=ORIENTED_EDGE('',*,*,#17495,.F.);
#23388=ORIENTED_EDGE('',*,*,#17492,.T.);
#23389=ORIENTED_EDGE('',*,*,#17494,.T.);
#23390=ORIENTED_EDGE('',*,*,#17497,.F.);
#23391=ORIENTED_EDGE('',*,*,#17493,.T.);
#23392=ORIENTED_EDGE('',*,*,#17404,.T.);
#23393=ORIENTED_EDGE('',*,*,#17455,.F.);
#23394=ORIENTED_EDGE('',*,*,#17498,.F.);
#23395=ORIENTED_EDGE('',*,*,#17496,.T.);
#23396=ORIENTED_EDGE('',*,*,#17499,.T.);
#23397=ORIENTED_EDGE('',*,*,#17458,.F.);
#23398=ORIENTED_EDGE('',*,*,#17446,.F.);
#23399=ORIENTED_EDGE('',*,*,#17499,.F.);
#23400=ORIENTED_EDGE('',*,*,#17497,.T.);
#23401=ORIENTED_EDGE('',*,*,#17498,.T.);
#23402=ORIENTED_EDGE('',*,*,#17461,.F.);
#23403=ORIENTED_EDGE('',*,*,#17500,.T.);
#23404=ORIENTED_EDGE('',*,*,#17413,.T.);
#23405=ORIENTED_EDGE('',*,*,#17501,.F.);
#23406=ORIENTED_EDGE('',*,*,#17502,.F.);
#23407=ORIENTED_EDGE('',*,*,#17503,.T.);
#23408=ORIENTED_EDGE('',*,*,#17504,.T.);
#23409=ORIENTED_EDGE('',*,*,#17505,.F.);
#23410=ORIENTED_EDGE('',*,*,#17453,.F.);
#23411=ORIENTED_EDGE('',*,*,#17504,.F.);
#23412=ORIENTED_EDGE('',*,*,#17506,.T.);
#23413=ORIENTED_EDGE('',*,*,#17502,.T.);
#23414=ORIENTED_EDGE('',*,*,#17507,.F.);
#23415=ORIENTED_EDGE('',*,*,#17501,.T.);
#23416=ORIENTED_EDGE('',*,*,#17412,.T.);
#23417=ORIENTED_EDGE('',*,*,#17508,.F.);
#23418=ORIENTED_EDGE('',*,*,#17509,.F.);
#23419=ORIENTED_EDGE('',*,*,#17505,.T.);
#23420=ORIENTED_EDGE('',*,*,#17510,.T.);
#23421=ORIENTED_EDGE('',*,*,#17511,.F.);
#23422=ORIENTED_EDGE('',*,*,#17454,.F.);
#23423=ORIENTED_EDGE('',*,*,#17510,.F.);
#23424=ORIENTED_EDGE('',*,*,#17507,.T.);
#23425=ORIENTED_EDGE('',*,*,#17509,.T.);
#23426=ORIENTED_EDGE('',*,*,#17512,.F.);
#23427=ORIENTED_EDGE('',*,*,#17508,.T.);
#23428=ORIENTED_EDGE('',*,*,#17418,.T.);
#23429=ORIENTED_EDGE('',*,*,#17513,.F.);
#23430=ORIENTED_EDGE('',*,*,#17514,.F.);
#23431=ORIENTED_EDGE('',*,*,#17511,.T.);
#23432=ORIENTED_EDGE('',*,*,#17515,.T.);
#23433=ORIENTED_EDGE('',*,*,#17516,.F.);
#23434=ORIENTED_EDGE('',*,*,#17448,.F.);
#23435=ORIENTED_EDGE('',*,*,#17515,.F.);
#23436=ORIENTED_EDGE('',*,*,#17512,.T.);
#23437=ORIENTED_EDGE('',*,*,#17514,.T.);
#23438=ORIENTED_EDGE('',*,*,#17517,.F.);
#23439=ORIENTED_EDGE('',*,*,#17513,.T.);
#23440=ORIENTED_EDGE('',*,*,#17417,.T.);
#23441=ORIENTED_EDGE('',*,*,#17518,.F.);
#23442=ORIENTED_EDGE('',*,*,#17519,.F.);
#23443=ORIENTED_EDGE('',*,*,#17516,.T.);
#23444=ORIENTED_EDGE('',*,*,#17520,.T.);
#23445=ORIENTED_EDGE('',*,*,#17521,.F.);
#23446=ORIENTED_EDGE('',*,*,#17449,.F.);
#23447=ORIENTED_EDGE('',*,*,#17520,.F.);
#23448=ORIENTED_EDGE('',*,*,#17517,.T.);
#23449=ORIENTED_EDGE('',*,*,#17519,.T.);
#23450=ORIENTED_EDGE('',*,*,#17522,.F.);
#23451=ORIENTED_EDGE('',*,*,#17518,.T.);
#23452=ORIENTED_EDGE('',*,*,#17416,.T.);
#23453=ORIENTED_EDGE('',*,*,#17523,.F.);
#23454=ORIENTED_EDGE('',*,*,#17524,.F.);
#23455=ORIENTED_EDGE('',*,*,#17521,.T.);
#23456=ORIENTED_EDGE('',*,*,#17525,.T.);
#23457=ORIENTED_EDGE('',*,*,#17526,.F.);
#23458=ORIENTED_EDGE('',*,*,#17450,.F.);
#23459=ORIENTED_EDGE('',*,*,#17525,.F.);
#23460=ORIENTED_EDGE('',*,*,#17522,.T.);
#23461=ORIENTED_EDGE('',*,*,#17524,.T.);
#23462=ORIENTED_EDGE('',*,*,#17527,.F.);
#23463=ORIENTED_EDGE('',*,*,#17523,.T.);
#23464=ORIENTED_EDGE('',*,*,#17415,.T.);
#23465=ORIENTED_EDGE('',*,*,#17528,.F.);
#23466=ORIENTED_EDGE('',*,*,#17529,.F.);
#23467=ORIENTED_EDGE('',*,*,#17526,.T.);
#23468=ORIENTED_EDGE('',*,*,#17530,.T.);
#23469=ORIENTED_EDGE('',*,*,#17531,.F.);
#23470=ORIENTED_EDGE('',*,*,#17451,.F.);
#23471=ORIENTED_EDGE('',*,*,#17530,.F.);
#23472=ORIENTED_EDGE('',*,*,#17527,.T.);
#23473=ORIENTED_EDGE('',*,*,#17529,.T.);
#23474=ORIENTED_EDGE('',*,*,#17532,.F.);
#23475=ORIENTED_EDGE('',*,*,#17528,.T.);
#23476=ORIENTED_EDGE('',*,*,#17414,.T.);
#23477=ORIENTED_EDGE('',*,*,#17500,.F.);
#23478=ORIENTED_EDGE('',*,*,#17533,.F.);
#23479=ORIENTED_EDGE('',*,*,#17531,.T.);
#23480=ORIENTED_EDGE('',*,*,#17534,.T.);
#23481=ORIENTED_EDGE('',*,*,#17503,.F.);
#23482=ORIENTED_EDGE('',*,*,#17452,.F.);
#23483=ORIENTED_EDGE('',*,*,#17534,.F.);
#23484=ORIENTED_EDGE('',*,*,#17532,.T.);
#23485=ORIENTED_EDGE('',*,*,#17533,.T.);
#23486=ORIENTED_EDGE('',*,*,#17506,.F.);
#23487=ORIENTED_EDGE('',*,*,#17535,.T.);
#23488=ORIENTED_EDGE('',*,*,#17395,.T.);
#23489=ORIENTED_EDGE('',*,*,#17536,.F.);
#23490=ORIENTED_EDGE('',*,*,#17537,.F.);
#23491=ORIENTED_EDGE('',*,*,#17538,.T.);
#23492=ORIENTED_EDGE('',*,*,#17539,.T.);
#23493=ORIENTED_EDGE('',*,*,#17540,.F.);
#23494=ORIENTED_EDGE('',*,*,#17437,.F.);
#23495=ORIENTED_EDGE('',*,*,#17539,.F.);
#23496=ORIENTED_EDGE('',*,*,#17541,.T.);
#23497=ORIENTED_EDGE('',*,*,#17537,.T.);
#23498=ORIENTED_EDGE('',*,*,#17542,.F.);
#23499=ORIENTED_EDGE('',*,*,#17536,.T.);
#23500=ORIENTED_EDGE('',*,*,#17394,.T.);
#23501=ORIENTED_EDGE('',*,*,#17543,.F.);
#23502=ORIENTED_EDGE('',*,*,#17544,.F.);
#23503=ORIENTED_EDGE('',*,*,#17540,.T.);
#23504=ORIENTED_EDGE('',*,*,#17545,.T.);
#23505=ORIENTED_EDGE('',*,*,#17546,.F.);
#23506=ORIENTED_EDGE('',*,*,#17438,.F.);
#23507=ORIENTED_EDGE('',*,*,#17545,.F.);
#23508=ORIENTED_EDGE('',*,*,#17542,.T.);
#23509=ORIENTED_EDGE('',*,*,#17544,.T.);
#23510=ORIENTED_EDGE('',*,*,#17547,.F.);
#23511=ORIENTED_EDGE('',*,*,#17543,.T.);
#23512=ORIENTED_EDGE('',*,*,#17402,.T.);
#23513=ORIENTED_EDGE('',*,*,#17548,.F.);
#23514=ORIENTED_EDGE('',*,*,#17549,.F.);
#23515=ORIENTED_EDGE('',*,*,#17546,.T.);
#23516=ORIENTED_EDGE('',*,*,#17550,.T.);
#23517=ORIENTED_EDGE('',*,*,#17551,.F.);
#23518=ORIENTED_EDGE('',*,*,#17430,.F.);
#23519=ORIENTED_EDGE('',*,*,#17550,.F.);
#23520=ORIENTED_EDGE('',*,*,#17547,.T.);
#23521=ORIENTED_EDGE('',*,*,#17549,.T.);
#23522=ORIENTED_EDGE('',*,*,#17552,.F.);
#23523=ORIENTED_EDGE('',*,*,#17548,.T.);
#23524=ORIENTED_EDGE('',*,*,#17401,.T.);
#23525=ORIENTED_EDGE('',*,*,#17553,.F.);
#23526=ORIENTED_EDGE('',*,*,#17554,.F.);
#23527=ORIENTED_EDGE('',*,*,#17551,.T.);
#23528=ORIENTED_EDGE('',*,*,#17555,.T.);
#23529=ORIENTED_EDGE('',*,*,#17556,.F.);
#23530=ORIENTED_EDGE('',*,*,#17431,.F.);
#23531=ORIENTED_EDGE('',*,*,#17555,.F.);
#23532=ORIENTED_EDGE('',*,*,#17552,.T.);
#23533=ORIENTED_EDGE('',*,*,#17554,.T.);
#23534=ORIENTED_EDGE('',*,*,#17557,.F.);
#23535=ORIENTED_EDGE('',*,*,#17553,.T.);
#23536=ORIENTED_EDGE('',*,*,#17400,.T.);
#23537=ORIENTED_EDGE('',*,*,#17558,.F.);
#23538=ORIENTED_EDGE('',*,*,#17559,.F.);
#23539=ORIENTED_EDGE('',*,*,#17556,.T.);
#23540=ORIENTED_EDGE('',*,*,#17560,.T.);
#23541=ORIENTED_EDGE('',*,*,#17561,.F.);
#23542=ORIENTED_EDGE('',*,*,#17432,.F.);
#23543=ORIENTED_EDGE('',*,*,#17560,.F.);
#23544=ORIENTED_EDGE('',*,*,#17557,.T.);
#23545=ORIENTED_EDGE('',*,*,#17559,.T.);
#23546=ORIENTED_EDGE('',*,*,#17562,.F.);
#23547=ORIENTED_EDGE('',*,*,#17558,.T.);
#23548=ORIENTED_EDGE('',*,*,#17399,.T.);
#23549=ORIENTED_EDGE('',*,*,#17563,.F.);
#23550=ORIENTED_EDGE('',*,*,#17564,.F.);
#23551=ORIENTED_EDGE('',*,*,#17561,.T.);
#23552=ORIENTED_EDGE('',*,*,#17565,.T.);
#23553=ORIENTED_EDGE('',*,*,#17566,.F.);
#23554=ORIENTED_EDGE('',*,*,#17433,.F.);
#23555=ORIENTED_EDGE('',*,*,#17565,.F.);
#23556=ORIENTED_EDGE('',*,*,#17562,.T.);
#23557=ORIENTED_EDGE('',*,*,#17564,.T.);
#23558=ORIENTED_EDGE('',*,*,#17567,.F.);
#23559=ORIENTED_EDGE('',*,*,#17563,.T.);
#23560=ORIENTED_EDGE('',*,*,#17398,.T.);
#23561=ORIENTED_EDGE('',*,*,#17568,.F.);
#23562=ORIENTED_EDGE('',*,*,#17569,.F.);
#23563=ORIENTED_EDGE('',*,*,#17566,.T.);
#23564=ORIENTED_EDGE('',*,*,#17570,.T.);
#23565=ORIENTED_EDGE('',*,*,#17571,.F.);
#23566=ORIENTED_EDGE('',*,*,#17434,.F.);
#23567=ORIENTED_EDGE('',*,*,#17570,.F.);
#23568=ORIENTED_EDGE('',*,*,#17567,.T.);
#23569=ORIENTED_EDGE('',*,*,#17569,.T.);
#23570=ORIENTED_EDGE('',*,*,#17572,.F.);
#23571=ORIENTED_EDGE('',*,*,#17568,.T.);
#23572=ORIENTED_EDGE('',*,*,#17397,.T.);
#23573=ORIENTED_EDGE('',*,*,#17573,.F.);
#23574=ORIENTED_EDGE('',*,*,#17574,.F.);
#23575=ORIENTED_EDGE('',*,*,#17571,.T.);
#23576=ORIENTED_EDGE('',*,*,#17575,.T.);
#23577=ORIENTED_EDGE('',*,*,#17576,.F.);
#23578=ORIENTED_EDGE('',*,*,#17435,.F.);
#23579=ORIENTED_EDGE('',*,*,#17575,.F.);
#23580=ORIENTED_EDGE('',*,*,#17572,.T.);
#23581=ORIENTED_EDGE('',*,*,#17574,.T.);
#23582=ORIENTED_EDGE('',*,*,#17577,.F.);
#23583=ORIENTED_EDGE('',*,*,#17573,.T.);
#23584=ORIENTED_EDGE('',*,*,#17396,.T.);
#23585=ORIENTED_EDGE('',*,*,#17535,.F.);
#23586=ORIENTED_EDGE('',*,*,#17578,.F.);
#23587=ORIENTED_EDGE('',*,*,#17576,.T.);
#23588=ORIENTED_EDGE('',*,*,#17579,.T.);
#23589=ORIENTED_EDGE('',*,*,#17538,.F.);
#23590=ORIENTED_EDGE('',*,*,#17436,.F.);
#23591=ORIENTED_EDGE('',*,*,#17579,.F.);
#23592=ORIENTED_EDGE('',*,*,#17577,.T.);
#23593=ORIENTED_EDGE('',*,*,#17578,.T.);
#23594=ORIENTED_EDGE('',*,*,#17541,.F.);
#23595=ORIENTED_EDGE('',*,*,#17580,.T.);
#23596=ORIENTED_EDGE('',*,*,#17581,.T.);
#23597=ORIENTED_EDGE('',*,*,#17582,.F.);
#23598=ORIENTED_EDGE('',*,*,#17392,.F.);
#23599=ORIENTED_EDGE('',*,*,#17583,.T.);
#23600=ORIENTED_EDGE('',*,*,#17420,.T.);
#23601=ORIENTED_EDGE('',*,*,#17584,.F.);
#23602=ORIENTED_EDGE('',*,*,#17585,.F.);
#23603=ORIENTED_EDGE('',*,*,#17585,.T.);
#23604=ORIENTED_EDGE('',*,*,#17586,.T.);
#23605=ORIENTED_EDGE('',*,*,#17581,.F.);
#23606=ORIENTED_EDGE('',*,*,#17587,.F.);
#23607=ORIENTED_EDGE('',*,*,#17588,.T.);
#23608=ORIENTED_EDGE('',*,*,#17589,.T.);
#23609=ORIENTED_EDGE('',*,*,#17580,.F.);
#23610=ORIENTED_EDGE('',*,*,#17391,.F.);
#23611=ORIENTED_EDGE('',*,*,#17590,.T.);
#23612=ORIENTED_EDGE('',*,*,#17421,.T.);
#23613=ORIENTED_EDGE('',*,*,#17583,.F.);
#23614=ORIENTED_EDGE('',*,*,#17591,.F.);
#23615=ORIENTED_EDGE('',*,*,#17591,.T.);
#23616=ORIENTED_EDGE('',*,*,#17587,.T.);
#23617=ORIENTED_EDGE('',*,*,#17589,.F.);
#23618=ORIENTED_EDGE('',*,*,#17592,.F.);
#23619=ORIENTED_EDGE('',*,*,#17593,.T.);
#23620=ORIENTED_EDGE('',*,*,#17594,.T.);
#23621=ORIENTED_EDGE('',*,*,#17588,.F.);
#23622=ORIENTED_EDGE('',*,*,#17390,.F.);
#23623=ORIENTED_EDGE('',*,*,#17595,.T.);
#23624=ORIENTED_EDGE('',*,*,#17422,.T.);
#23625=ORIENTED_EDGE('',*,*,#17590,.F.);
#23626=ORIENTED_EDGE('',*,*,#17596,.F.);
#23627=ORIENTED_EDGE('',*,*,#17596,.T.);
#23628=ORIENTED_EDGE('',*,*,#17592,.T.);
#23629=ORIENTED_EDGE('',*,*,#17594,.F.);
#23630=ORIENTED_EDGE('',*,*,#17597,.F.);
#23631=ORIENTED_EDGE('',*,*,#17598,.T.);
#23632=ORIENTED_EDGE('',*,*,#17599,.T.);
#23633=ORIENTED_EDGE('',*,*,#17593,.F.);
#23634=ORIENTED_EDGE('',*,*,#17389,.F.);
#23635=ORIENTED_EDGE('',*,*,#17600,.T.);
#23636=ORIENTED_EDGE('',*,*,#17423,.T.);
#23637=ORIENTED_EDGE('',*,*,#17595,.F.);
#23638=ORIENTED_EDGE('',*,*,#17601,.F.);
#23639=ORIENTED_EDGE('',*,*,#17601,.T.);
#23640=ORIENTED_EDGE('',*,*,#17597,.T.);
#23641=ORIENTED_EDGE('',*,*,#17599,.F.);
#23642=ORIENTED_EDGE('',*,*,#17602,.F.);
#23643=ORIENTED_EDGE('',*,*,#17603,.T.);
#23644=ORIENTED_EDGE('',*,*,#17604,.T.);
#23645=ORIENTED_EDGE('',*,*,#17598,.F.);
#23646=ORIENTED_EDGE('',*,*,#17388,.F.);
#23647=ORIENTED_EDGE('',*,*,#17605,.T.);
#23648=ORIENTED_EDGE('',*,*,#17424,.T.);
#23649=ORIENTED_EDGE('',*,*,#17600,.F.);
#23650=ORIENTED_EDGE('',*,*,#17606,.F.);
#23651=ORIENTED_EDGE('',*,*,#17606,.T.);
#23652=ORIENTED_EDGE('',*,*,#17602,.T.);
#23653=ORIENTED_EDGE('',*,*,#17604,.F.);
#23654=ORIENTED_EDGE('',*,*,#17607,.F.);
#23655=ORIENTED_EDGE('',*,*,#17608,.T.);
#23656=ORIENTED_EDGE('',*,*,#17609,.T.);
#23657=ORIENTED_EDGE('',*,*,#17603,.F.);
#23658=ORIENTED_EDGE('',*,*,#17387,.F.);
#23659=ORIENTED_EDGE('',*,*,#17610,.T.);
#23660=ORIENTED_EDGE('',*,*,#17425,.T.);
#23661=ORIENTED_EDGE('',*,*,#17605,.F.);
#23662=ORIENTED_EDGE('',*,*,#17611,.F.);
#23663=ORIENTED_EDGE('',*,*,#17611,.T.);
#23664=ORIENTED_EDGE('',*,*,#17607,.T.);
#23665=ORIENTED_EDGE('',*,*,#17609,.F.);
#23666=ORIENTED_EDGE('',*,*,#17612,.F.);
#23667=ORIENTED_EDGE('',*,*,#17613,.T.);
#23668=ORIENTED_EDGE('',*,*,#17614,.T.);
#23669=ORIENTED_EDGE('',*,*,#17608,.F.);
#23670=ORIENTED_EDGE('',*,*,#17386,.F.);
#23671=ORIENTED_EDGE('',*,*,#17615,.T.);
#23672=ORIENTED_EDGE('',*,*,#17426,.T.);
#23673=ORIENTED_EDGE('',*,*,#17610,.F.);
#23674=ORIENTED_EDGE('',*,*,#17616,.F.);
#23675=ORIENTED_EDGE('',*,*,#17616,.T.);
#23676=ORIENTED_EDGE('',*,*,#17612,.T.);
#23677=ORIENTED_EDGE('',*,*,#17614,.F.);
#23678=ORIENTED_EDGE('',*,*,#17617,.F.);
#23679=ORIENTED_EDGE('',*,*,#17618,.T.);
#23680=ORIENTED_EDGE('',*,*,#17619,.T.);
#23681=ORIENTED_EDGE('',*,*,#17613,.F.);
#23682=ORIENTED_EDGE('',*,*,#17385,.F.);
#23683=ORIENTED_EDGE('',*,*,#17620,.T.);
#23684=ORIENTED_EDGE('',*,*,#17427,.T.);
#23685=ORIENTED_EDGE('',*,*,#17615,.F.);
#23686=ORIENTED_EDGE('',*,*,#17621,.F.);
#23687=ORIENTED_EDGE('',*,*,#17621,.T.);
#23688=ORIENTED_EDGE('',*,*,#17617,.T.);
#23689=ORIENTED_EDGE('',*,*,#17619,.F.);
#23690=ORIENTED_EDGE('',*,*,#17622,.F.);
#23691=ORIENTED_EDGE('',*,*,#17623,.T.);
#23692=ORIENTED_EDGE('',*,*,#17624,.T.);
#23693=ORIENTED_EDGE('',*,*,#17618,.F.);
#23694=ORIENTED_EDGE('',*,*,#17384,.F.);
#23695=ORIENTED_EDGE('',*,*,#17625,.T.);
#23696=ORIENTED_EDGE('',*,*,#17428,.T.);
#23697=ORIENTED_EDGE('',*,*,#17620,.F.);
#23698=ORIENTED_EDGE('',*,*,#17626,.F.);
#23699=ORIENTED_EDGE('',*,*,#17626,.T.);
#23700=ORIENTED_EDGE('',*,*,#17622,.T.);
#23701=ORIENTED_EDGE('',*,*,#17624,.F.);
#23702=ORIENTED_EDGE('',*,*,#17627,.F.);
#23703=ORIENTED_EDGE('',*,*,#17628,.T.);
#23704=ORIENTED_EDGE('',*,*,#17629,.T.);
#23705=ORIENTED_EDGE('',*,*,#17623,.F.);
#23706=ORIENTED_EDGE('',*,*,#17383,.F.);
#23707=ORIENTED_EDGE('',*,*,#17630,.T.);
#23708=ORIENTED_EDGE('',*,*,#17429,.T.);
#23709=ORIENTED_EDGE('',*,*,#17625,.F.);
#23710=ORIENTED_EDGE('',*,*,#17631,.F.);
#23711=ORIENTED_EDGE('',*,*,#17631,.T.);
#23712=ORIENTED_EDGE('',*,*,#17627,.T.);
#23713=ORIENTED_EDGE('',*,*,#17629,.F.);
#23714=ORIENTED_EDGE('',*,*,#17632,.F.);
#23715=ORIENTED_EDGE('',*,*,#17582,.T.);
#23716=ORIENTED_EDGE('',*,*,#17633,.T.);
#23717=ORIENTED_EDGE('',*,*,#17628,.F.);
#23718=ORIENTED_EDGE('',*,*,#17393,.F.);
#23719=ORIENTED_EDGE('',*,*,#17584,.T.);
#23720=ORIENTED_EDGE('',*,*,#17419,.T.);
#23721=ORIENTED_EDGE('',*,*,#17630,.F.);
#23722=ORIENTED_EDGE('',*,*,#17634,.F.);
#23723=ORIENTED_EDGE('',*,*,#17634,.T.);
#23724=ORIENTED_EDGE('',*,*,#17632,.T.);
#23725=ORIENTED_EDGE('',*,*,#17633,.F.);
#23726=ORIENTED_EDGE('',*,*,#17586,.F.);
#23727=ORIENTED_EDGE('',*,*,#17635,.T.);
#23728=ORIENTED_EDGE('',*,*,#17636,.T.);
#23729=ORIENTED_EDGE('',*,*,#17637,.T.);
#23730=ORIENTED_EDGE('',*,*,#17638,.T.);
#23731=ORIENTED_EDGE('',*,*,#17639,.T.);
#23732=ORIENTED_EDGE('',*,*,#17640,.T.);
#23733=ORIENTED_EDGE('',*,*,#17641,.T.);
#23734=ORIENTED_EDGE('',*,*,#17642,.T.);
#23735=ORIENTED_EDGE('',*,*,#17643,.T.);
#23736=ORIENTED_EDGE('',*,*,#17644,.T.);
#23737=ORIENTED_EDGE('',*,*,#17645,.F.);
#23738=ORIENTED_EDGE('',*,*,#17646,.F.);
#23739=ORIENTED_EDGE('',*,*,#17647,.F.);
#23740=ORIENTED_EDGE('',*,*,#17648,.F.);
#23741=ORIENTED_EDGE('',*,*,#17649,.F.);
#23742=ORIENTED_EDGE('',*,*,#17650,.F.);
#23743=ORIENTED_EDGE('',*,*,#17651,.F.);
#23744=ORIENTED_EDGE('',*,*,#17652,.F.);
#23745=ORIENTED_EDGE('',*,*,#17653,.F.);
#23746=ORIENTED_EDGE('',*,*,#17654,.F.);
#23747=ORIENTED_EDGE('',*,*,#17655,.F.);
#23748=ORIENTED_EDGE('',*,*,#17656,.F.);
#23749=ORIENTED_EDGE('',*,*,#17657,.F.);
#23750=ORIENTED_EDGE('',*,*,#17658,.F.);
#23751=ORIENTED_EDGE('',*,*,#17659,.F.);
#23752=ORIENTED_EDGE('',*,*,#17660,.F.);
#23753=ORIENTED_EDGE('',*,*,#17661,.F.);
#23754=ORIENTED_EDGE('',*,*,#17662,.F.);
#23755=ORIENTED_EDGE('',*,*,#17663,.F.);
#23756=ORIENTED_EDGE('',*,*,#17664,.F.);
#23757=ORIENTED_EDGE('',*,*,#17665,.F.);
#23758=ORIENTED_EDGE('',*,*,#17666,.T.);
#23759=ORIENTED_EDGE('',*,*,#17667,.T.);
#23760=ORIENTED_EDGE('',*,*,#17668,.T.);
#23761=ORIENTED_EDGE('',*,*,#17669,.T.);
#23762=ORIENTED_EDGE('',*,*,#17670,.T.);
#23763=ORIENTED_EDGE('',*,*,#17671,.T.);
#23764=ORIENTED_EDGE('',*,*,#17672,.T.);
#23765=ORIENTED_EDGE('',*,*,#17673,.T.);
#23766=ORIENTED_EDGE('',*,*,#17674,.T.);
#23767=ORIENTED_EDGE('',*,*,#17675,.T.);
#23768=ORIENTED_EDGE('',*,*,#17676,.T.);
#23769=ORIENTED_EDGE('',*,*,#17677,.F.);
#23770=ORIENTED_EDGE('',*,*,#17678,.T.);
#23771=ORIENTED_EDGE('',*,*,#17655,.T.);
#23772=ORIENTED_EDGE('',*,*,#17678,.F.);
#23773=ORIENTED_EDGE('',*,*,#17666,.F.);
#23774=ORIENTED_EDGE('',*,*,#17679,.T.);
#23775=ORIENTED_EDGE('',*,*,#17677,.T.);
#23776=ORIENTED_EDGE('',*,*,#17679,.F.);
#23777=ORIENTED_EDGE('',*,*,#17680,.F.);
#23778=ORIENTED_EDGE('',*,*,#17681,.T.);
#23779=ORIENTED_EDGE('',*,*,#17654,.T.);
#23780=ORIENTED_EDGE('',*,*,#17681,.F.);
#23781=ORIENTED_EDGE('',*,*,#17667,.F.);
#23782=ORIENTED_EDGE('',*,*,#17682,.T.);
#23783=ORIENTED_EDGE('',*,*,#17680,.T.);
#23784=ORIENTED_EDGE('',*,*,#17682,.F.);
#23785=ORIENTED_EDGE('',*,*,#17683,.T.);
#23786=ORIENTED_EDGE('',*,*,#17646,.T.);
#23787=ORIENTED_EDGE('',*,*,#17684,.F.);
#23788=ORIENTED_EDGE('',*,*,#17685,.F.);
#23789=ORIENTED_EDGE('',*,*,#17685,.T.);
#23790=ORIENTED_EDGE('',*,*,#17686,.F.);
#23791=ORIENTED_EDGE('',*,*,#17668,.F.);
#23792=ORIENTED_EDGE('',*,*,#17687,.T.);
#23793=ORIENTED_EDGE('',*,*,#17684,.T.);
#23794=ORIENTED_EDGE('',*,*,#17645,.T.);
#23795=ORIENTED_EDGE('',*,*,#17688,.F.);
#23796=ORIENTED_EDGE('',*,*,#17689,.F.);
#23797=ORIENTED_EDGE('',*,*,#17689,.T.);
#23798=ORIENTED_EDGE('',*,*,#17690,.F.);
#23799=ORIENTED_EDGE('',*,*,#17669,.F.);
#23800=ORIENTED_EDGE('',*,*,#17686,.T.);
#23801=ORIENTED_EDGE('',*,*,#17688,.T.);
#23802=ORIENTED_EDGE('',*,*,#17653,.T.);
#23803=ORIENTED_EDGE('',*,*,#17691,.F.);
#23804=ORIENTED_EDGE('',*,*,#17692,.F.);
#23805=ORIENTED_EDGE('',*,*,#17692,.T.);
#23806=ORIENTED_EDGE('',*,*,#17693,.F.);
#23807=ORIENTED_EDGE('',*,*,#17670,.F.);
#23808=ORIENTED_EDGE('',*,*,#17690,.T.);
#23809=ORIENTED_EDGE('',*,*,#17691,.T.);
#23810=ORIENTED_EDGE('',*,*,#17652,.T.);
#23811=ORIENTED_EDGE('',*,*,#17694,.F.);
#23812=ORIENTED_EDGE('',*,*,#17695,.F.);
#23813=ORIENTED_EDGE('',*,*,#17695,.T.);
#23814=ORIENTED_EDGE('',*,*,#17696,.F.);
#23815=ORIENTED_EDGE('',*,*,#17671,.F.);
#23816=ORIENTED_EDGE('',*,*,#17693,.T.);
#23817=ORIENTED_EDGE('',*,*,#17694,.T.);
#23818=ORIENTED_EDGE('',*,*,#17651,.T.);
#23819=ORIENTED_EDGE('',*,*,#17697,.F.);
#23820=ORIENTED_EDGE('',*,*,#17698,.F.);
#23821=ORIENTED_EDGE('',*,*,#17698,.T.);
#23822=ORIENTED_EDGE('',*,*,#17699,.F.);
#23823=ORIENTED_EDGE('',*,*,#17672,.F.);
#23824=ORIENTED_EDGE('',*,*,#17696,.T.);
#23825=ORIENTED_EDGE('',*,*,#17697,.T.);
#23826=ORIENTED_EDGE('',*,*,#17650,.T.);
#23827=ORIENTED_EDGE('',*,*,#17700,.F.);
#23828=ORIENTED_EDGE('',*,*,#17701,.F.);
#23829=ORIENTED_EDGE('',*,*,#17701,.T.);
#23830=ORIENTED_EDGE('',*,*,#17702,.F.);
#23831=ORIENTED_EDGE('',*,*,#17673,.F.);
#23832=ORIENTED_EDGE('',*,*,#17699,.T.);
#23833=ORIENTED_EDGE('',*,*,#17700,.T.);
#23834=ORIENTED_EDGE('',*,*,#17649,.T.);
#23835=ORIENTED_EDGE('',*,*,#17703,.F.);
#23836=ORIENTED_EDGE('',*,*,#17704,.F.);
#23837=ORIENTED_EDGE('',*,*,#17704,.T.);
#23838=ORIENTED_EDGE('',*,*,#17705,.F.);
#23839=ORIENTED_EDGE('',*,*,#17674,.F.);
#23840=ORIENTED_EDGE('',*,*,#17702,.T.);
#23841=ORIENTED_EDGE('',*,*,#17703,.T.);
#23842=ORIENTED_EDGE('',*,*,#17648,.T.);
#23843=ORIENTED_EDGE('',*,*,#17706,.F.);
#23844=ORIENTED_EDGE('',*,*,#17707,.F.);
#23845=ORIENTED_EDGE('',*,*,#17707,.T.);
#23846=ORIENTED_EDGE('',*,*,#17708,.F.);
#23847=ORIENTED_EDGE('',*,*,#17675,.F.);
#23848=ORIENTED_EDGE('',*,*,#17705,.T.);
#23849=ORIENTED_EDGE('',*,*,#17706,.T.);
#23850=ORIENTED_EDGE('',*,*,#17647,.T.);
#23851=ORIENTED_EDGE('',*,*,#17683,.F.);
#23852=ORIENTED_EDGE('',*,*,#17709,.F.);
#23853=ORIENTED_EDGE('',*,*,#17709,.T.);
#23854=ORIENTED_EDGE('',*,*,#17687,.F.);
#23855=ORIENTED_EDGE('',*,*,#17676,.F.);
#23856=ORIENTED_EDGE('',*,*,#17708,.T.);
#23857=ORIENTED_EDGE('',*,*,#17710,.T.);
#23858=ORIENTED_EDGE('',*,*,#17711,.T.);
#23859=ORIENTED_EDGE('',*,*,#17712,.F.);
#23860=ORIENTED_EDGE('',*,*,#17636,.F.);
#23861=ORIENTED_EDGE('',*,*,#17711,.F.);
#23862=ORIENTED_EDGE('',*,*,#17713,.F.);
#23863=ORIENTED_EDGE('',*,*,#17656,.T.);
#23864=ORIENTED_EDGE('',*,*,#17714,.T.);
#23865=ORIENTED_EDGE('',*,*,#17715,.T.);
#23866=ORIENTED_EDGE('',*,*,#17716,.T.);
#23867=ORIENTED_EDGE('',*,*,#17710,.F.);
#23868=ORIENTED_EDGE('',*,*,#17635,.F.);
#23869=ORIENTED_EDGE('',*,*,#17716,.F.);
#23870=ORIENTED_EDGE('',*,*,#17717,.F.);
#23871=ORIENTED_EDGE('',*,*,#17657,.T.);
#23872=ORIENTED_EDGE('',*,*,#17713,.T.);
#23873=ORIENTED_EDGE('',*,*,#17718,.T.);
#23874=ORIENTED_EDGE('',*,*,#17719,.T.);
#23875=ORIENTED_EDGE('',*,*,#17715,.F.);
#23876=ORIENTED_EDGE('',*,*,#17644,.F.);
#23877=ORIENTED_EDGE('',*,*,#17719,.F.);
#23878=ORIENTED_EDGE('',*,*,#17720,.F.);
#23879=ORIENTED_EDGE('',*,*,#17658,.T.);
#23880=ORIENTED_EDGE('',*,*,#17717,.T.);
#23881=ORIENTED_EDGE('',*,*,#17721,.T.);
#23882=ORIENTED_EDGE('',*,*,#17722,.T.);
#23883=ORIENTED_EDGE('',*,*,#17718,.F.);
#23884=ORIENTED_EDGE('',*,*,#17643,.F.);
#23885=ORIENTED_EDGE('',*,*,#17722,.F.);
#23886=ORIENTED_EDGE('',*,*,#17723,.F.);
#23887=ORIENTED_EDGE('',*,*,#17659,.T.);
#23888=ORIENTED_EDGE('',*,*,#17720,.T.);
#23889=ORIENTED_EDGE('',*,*,#17724,.T.);
#23890=ORIENTED_EDGE('',*,*,#17725,.T.);
#23891=ORIENTED_EDGE('',*,*,#17721,.F.);
#23892=ORIENTED_EDGE('',*,*,#17642,.F.);
#23893=ORIENTED_EDGE('',*,*,#17725,.F.);
#23894=ORIENTED_EDGE('',*,*,#17726,.F.);
#23895=ORIENTED_EDGE('',*,*,#17660,.T.);
#23896=ORIENTED_EDGE('',*,*,#17723,.T.);
#23897=ORIENTED_EDGE('',*,*,#17727,.T.);
#23898=ORIENTED_EDGE('',*,*,#17728,.T.);
#23899=ORIENTED_EDGE('',*,*,#17724,.F.);
#23900=ORIENTED_EDGE('',*,*,#17641,.F.);
#23901=ORIENTED_EDGE('',*,*,#17728,.F.);
#23902=ORIENTED_EDGE('',*,*,#17729,.F.);
#23903=ORIENTED_EDGE('',*,*,#17661,.T.);
#23904=ORIENTED_EDGE('',*,*,#17726,.T.);
#23905=ORIENTED_EDGE('',*,*,#17730,.T.);
#23906=ORIENTED_EDGE('',*,*,#17731,.T.);
#23907=ORIENTED_EDGE('',*,*,#17727,.F.);
#23908=ORIENTED_EDGE('',*,*,#17640,.F.);
#23909=ORIENTED_EDGE('',*,*,#17731,.F.);
#23910=ORIENTED_EDGE('',*,*,#17732,.F.);
#23911=ORIENTED_EDGE('',*,*,#17662,.T.);
#23912=ORIENTED_EDGE('',*,*,#17729,.T.);
#23913=ORIENTED_EDGE('',*,*,#17733,.T.);
#23914=ORIENTED_EDGE('',*,*,#17734,.T.);
#23915=ORIENTED_EDGE('',*,*,#17730,.F.);
#23916=ORIENTED_EDGE('',*,*,#17639,.F.);
#23917=ORIENTED_EDGE('',*,*,#17734,.F.);
#23918=ORIENTED_EDGE('',*,*,#17735,.F.);
#23919=ORIENTED_EDGE('',*,*,#17663,.T.);
#23920=ORIENTED_EDGE('',*,*,#17732,.T.);
#23921=ORIENTED_EDGE('',*,*,#17736,.T.);
#23922=ORIENTED_EDGE('',*,*,#17737,.T.);
#23923=ORIENTED_EDGE('',*,*,#17733,.F.);
#23924=ORIENTED_EDGE('',*,*,#17638,.F.);
#23925=ORIENTED_EDGE('',*,*,#17737,.F.);
#23926=ORIENTED_EDGE('',*,*,#17738,.F.);
#23927=ORIENTED_EDGE('',*,*,#17664,.T.);
#23928=ORIENTED_EDGE('',*,*,#17735,.T.);
#23929=ORIENTED_EDGE('',*,*,#17712,.T.);
#23930=ORIENTED_EDGE('',*,*,#17739,.T.);
#23931=ORIENTED_EDGE('',*,*,#17736,.F.);
#23932=ORIENTED_EDGE('',*,*,#17637,.F.);
#23933=ORIENTED_EDGE('',*,*,#17739,.F.);
#23934=ORIENTED_EDGE('',*,*,#17714,.F.);
#23935=ORIENTED_EDGE('',*,*,#17665,.T.);
#23936=ORIENTED_EDGE('',*,*,#17738,.T.);
#23937=ORIENTED_EDGE('',*,*,#17740,.T.);
#23938=ORIENTED_EDGE('',*,*,#17741,.F.);
#23939=ORIENTED_EDGE('',*,*,#17742,.F.);
#23940=ORIENTED_EDGE('',*,*,#17743,.F.);
#23941=ORIENTED_EDGE('',*,*,#17742,.T.);
#23942=ORIENTED_EDGE('',*,*,#17744,.F.);
#23943=ORIENTED_EDGE('',*,*,#17745,.F.);
#23944=ORIENTED_EDGE('',*,*,#17746,.F.);
#23945=ORIENTED_EDGE('',*,*,#17747,.F.);
#23946=ORIENTED_EDGE('',*,*,#17744,.T.);
#23947=ORIENTED_EDGE('',*,*,#17741,.T.);
#23948=ORIENTED_EDGE('',*,*,#17743,.T.);
#23949=ORIENTED_EDGE('',*,*,#17748,.T.);
#23950=ORIENTED_EDGE('',*,*,#17746,.T.);
#23951=ORIENTED_EDGE('',*,*,#17740,.F.);
#23952=ORIENTED_EDGE('',*,*,#17745,.T.);
#23953=ORIENTED_EDGE('',*,*,#17747,.T.);
#23954=ORIENTED_EDGE('',*,*,#17748,.F.);
#23955=ORIENTED_EDGE('',*,*,#17749,.F.);
#23956=ORIENTED_EDGE('',*,*,#17750,.T.);
#23957=ORIENTED_EDGE('',*,*,#17751,.T.);
#23958=ORIENTED_EDGE('',*,*,#17752,.F.);
#23959=ORIENTED_EDGE('',*,*,#17753,.T.);
#23960=ORIENTED_EDGE('',*,*,#17754,.T.);
#23961=ORIENTED_EDGE('',*,*,#17751,.F.);
#23962=ORIENTED_EDGE('',*,*,#17752,.T.);
#23963=ORIENTED_EDGE('',*,*,#17750,.F.);
#23964=ORIENTED_EDGE('',*,*,#17755,.F.);
#23965=ORIENTED_EDGE('',*,*,#17756,.T.);
#23966=ORIENTED_EDGE('',*,*,#17754,.F.);
#23967=ORIENTED_EDGE('',*,*,#17757,.F.);
#23968=ORIENTED_EDGE('',*,*,#17755,.T.);
#23969=ORIENTED_EDGE('',*,*,#17749,.T.);
#23970=ORIENTED_EDGE('',*,*,#17757,.T.);
#23971=ORIENTED_EDGE('',*,*,#17753,.F.);
#23972=ORIENTED_EDGE('',*,*,#17756,.F.);
#23973=ORIENTED_EDGE('',*,*,#17758,.T.);
#23974=ORIENTED_EDGE('',*,*,#17759,.T.);
#23975=ORIENTED_EDGE('',*,*,#17760,.F.);
#23976=ORIENTED_EDGE('',*,*,#17761,.F.);
#23977=ORIENTED_EDGE('',*,*,#17762,.F.);
#23978=ORIENTED_EDGE('',*,*,#17763,.F.);
#23979=ORIENTED_EDGE('',*,*,#17764,.F.);
#23980=ORIENTED_EDGE('',*,*,#17765,.T.);
#23981=ORIENTED_EDGE('',*,*,#17766,.T.);
#23982=ORIENTED_EDGE('',*,*,#17767,.T.);
#23983=ORIENTED_EDGE('',*,*,#17768,.T.);
#23984=ORIENTED_EDGE('',*,*,#17769,.T.);
#23985=ORIENTED_EDGE('',*,*,#17770,.F.);
#23986=ORIENTED_EDGE('',*,*,#17771,.F.);
#23987=ORIENTED_EDGE('',*,*,#17772,.T.);
#23988=ORIENTED_EDGE('',*,*,#17773,.F.);
#23989=ORIENTED_EDGE('',*,*,#17774,.F.);
#23990=ORIENTED_EDGE('',*,*,#17775,.F.);
#23991=ORIENTED_EDGE('',*,*,#17776,.T.);
#23992=ORIENTED_EDGE('',*,*,#17777,.T.);
#23993=ORIENTED_EDGE('',*,*,#17778,.T.);
#23994=ORIENTED_EDGE('',*,*,#17779,.T.);
#23995=ORIENTED_EDGE('',*,*,#17780,.T.);
#23996=ORIENTED_EDGE('',*,*,#17781,.T.);
#23997=ORIENTED_EDGE('',*,*,#17782,.T.);
#23998=ORIENTED_EDGE('',*,*,#17783,.F.);
#23999=ORIENTED_EDGE('',*,*,#17784,.F.);
#24000=ORIENTED_EDGE('',*,*,#17785,.F.);
#24001=ORIENTED_EDGE('',*,*,#17786,.T.);
#24002=ORIENTED_EDGE('',*,*,#17787,.F.);
#24003=ORIENTED_EDGE('',*,*,#17788,.F.);
#24004=ORIENTED_EDGE('',*,*,#17789,.T.);
#24005=ORIENTED_EDGE('',*,*,#17790,.T.);
#24006=ORIENTED_EDGE('',*,*,#17791,.F.);
#24007=ORIENTED_EDGE('',*,*,#17792,.T.);
#24008=ORIENTED_EDGE('',*,*,#17793,.T.);
#24009=ORIENTED_EDGE('',*,*,#17794,.F.);
#24010=ORIENTED_EDGE('',*,*,#17795,.T.);
#24011=ORIENTED_EDGE('',*,*,#17796,.F.);
#24012=ORIENTED_EDGE('',*,*,#17797,.F.);
#24013=ORIENTED_EDGE('',*,*,#17798,.T.);
#24014=ORIENTED_EDGE('',*,*,#17799,.F.);
#24015=ORIENTED_EDGE('',*,*,#17800,.T.);
#24016=ORIENTED_EDGE('',*,*,#17801,.T.);
#24017=ORIENTED_EDGE('',*,*,#17802,.T.);
#24018=ORIENTED_EDGE('',*,*,#17803,.F.);
#24019=ORIENTED_EDGE('',*,*,#17804,.T.);
#24020=ORIENTED_EDGE('',*,*,#17805,.F.);
#24021=ORIENTED_EDGE('',*,*,#17771,.T.);
#24022=ORIENTED_EDGE('',*,*,#17806,.T.);
#24023=ORIENTED_EDGE('',*,*,#17807,.T.);
#24024=ORIENTED_EDGE('',*,*,#17808,.T.);
#24025=ORIENTED_EDGE('',*,*,#17809,.T.);
#24026=ORIENTED_EDGE('',*,*,#17810,.T.);
#24027=ORIENTED_EDGE('',*,*,#17811,.T.);
#24028=ORIENTED_EDGE('',*,*,#17812,.F.);
#24029=ORIENTED_EDGE('',*,*,#17813,.T.);
#24030=ORIENTED_EDGE('',*,*,#17814,.T.);
#24031=ORIENTED_EDGE('',*,*,#17815,.T.);
#24032=ORIENTED_EDGE('',*,*,#17816,.T.);
#24033=ORIENTED_EDGE('',*,*,#17817,.T.);
#24034=ORIENTED_EDGE('',*,*,#17818,.T.);
#24035=ORIENTED_EDGE('',*,*,#17819,.F.);
#24036=ORIENTED_EDGE('',*,*,#17820,.T.);
#24037=ORIENTED_EDGE('',*,*,#17821,.F.);
#24038=ORIENTED_EDGE('',*,*,#17765,.F.);
#24039=ORIENTED_EDGE('',*,*,#17822,.T.);
#24040=ORIENTED_EDGE('',*,*,#17823,.T.);
#24041=ORIENTED_EDGE('',*,*,#17824,.F.);
#24042=ORIENTED_EDGE('',*,*,#17825,.T.);
#24043=ORIENTED_EDGE('',*,*,#17826,.T.);
#24044=ORIENTED_EDGE('',*,*,#17827,.F.);
#24045=ORIENTED_EDGE('',*,*,#17828,.F.);
#24046=ORIENTED_EDGE('',*,*,#17829,.F.);
#24047=ORIENTED_EDGE('',*,*,#17770,.T.);
#24048=ORIENTED_EDGE('',*,*,#17830,.T.);
#24049=ORIENTED_EDGE('',*,*,#17831,.F.);
#24050=ORIENTED_EDGE('',*,*,#17806,.F.);
#24051=ORIENTED_EDGE('',*,*,#17769,.F.);
#24052=ORIENTED_EDGE('',*,*,#17832,.T.);
#24053=ORIENTED_EDGE('',*,*,#17833,.F.);
#24054=ORIENTED_EDGE('',*,*,#17830,.F.);
#24055=ORIENTED_EDGE('',*,*,#17768,.F.);
#24056=ORIENTED_EDGE('',*,*,#17834,.T.);
#24057=ORIENTED_EDGE('',*,*,#17835,.F.);
#24058=ORIENTED_EDGE('',*,*,#17836,.F.);
#24059=ORIENTED_EDGE('',*,*,#17837,.T.);
#24060=ORIENTED_EDGE('',*,*,#17838,.F.);
#24061=ORIENTED_EDGE('',*,*,#17839,.F.);
#24062=ORIENTED_EDGE('',*,*,#17832,.F.);
#24063=ORIENTED_EDGE('',*,*,#17805,.T.);
#24064=ORIENTED_EDGE('',*,*,#17840,.T.);
#24065=ORIENTED_EDGE('',*,*,#17841,.F.);
#24066=ORIENTED_EDGE('',*,*,#17834,.F.);
#24067=ORIENTED_EDGE('',*,*,#17767,.F.);
#24068=ORIENTED_EDGE('',*,*,#17842,.T.);
#24069=ORIENTED_EDGE('',*,*,#17843,.T.);
#24070=ORIENTED_EDGE('',*,*,#17844,.F.);
#24071=ORIENTED_EDGE('',*,*,#17845,.T.);
#24072=ORIENTED_EDGE('',*,*,#17846,.F.);
#24073=ORIENTED_EDGE('',*,*,#17847,.T.);
#24074=ORIENTED_EDGE('',*,*,#17848,.T.);
#24075=ORIENTED_EDGE('',*,*,#17849,.T.);
#24076=ORIENTED_EDGE('',*,*,#17850,.T.);
#24077=ORIENTED_EDGE('',*,*,#17851,.T.);
#24078=ORIENTED_EDGE('',*,*,#17852,.F.);
#24079=ORIENTED_EDGE('',*,*,#17853,.T.);
#24080=ORIENTED_EDGE('',*,*,#17854,.T.);
#24081=ORIENTED_EDGE('',*,*,#17855,.T.);
#24082=ORIENTED_EDGE('',*,*,#17856,.T.);
#24083=ORIENTED_EDGE('',*,*,#17787,.T.);
#24084=ORIENTED_EDGE('',*,*,#17857,.F.);
#24085=ORIENTED_EDGE('',*,*,#17858,.T.);
#24086=ORIENTED_EDGE('',*,*,#17859,.F.);
#24087=ORIENTED_EDGE('',*,*,#17860,.T.);
#24088=ORIENTED_EDGE('',*,*,#17786,.F.);
#24089=ORIENTED_EDGE('',*,*,#17861,.T.);
#24090=ORIENTED_EDGE('',*,*,#17862,.T.);
#24091=ORIENTED_EDGE('',*,*,#17857,.T.);
#24092=ORIENTED_EDGE('',*,*,#17861,.F.);
#24093=ORIENTED_EDGE('',*,*,#17785,.T.);
#24094=ORIENTED_EDGE('',*,*,#17863,.T.);
#24095=ORIENTED_EDGE('',*,*,#17864,.F.);
#24096=ORIENTED_EDGE('',*,*,#17865,.F.);
#24097=ORIENTED_EDGE('',*,*,#17863,.F.);
#24098=ORIENTED_EDGE('',*,*,#17784,.T.);
#24099=ORIENTED_EDGE('',*,*,#17866,.T.);
#24100=ORIENTED_EDGE('',*,*,#17783,.T.);
#24101=ORIENTED_EDGE('',*,*,#17867,.T.);
#24102=ORIENTED_EDGE('',*,*,#17868,.T.);
#24103=ORIENTED_EDGE('',*,*,#17869,.F.);
#24104=ORIENTED_EDGE('',*,*,#17870,.F.);
#24105=ORIENTED_EDGE('',*,*,#17871,.T.);
#24106=ORIENTED_EDGE('',*,*,#17872,.F.);
#24107=ORIENTED_EDGE('',*,*,#17873,.T.);
#24108=ORIENTED_EDGE('',*,*,#17874,.T.);
#24109=ORIENTED_EDGE('',*,*,#17866,.F.);
#24110=ORIENTED_EDGE('',*,*,#17782,.F.);
#24111=ORIENTED_EDGE('',*,*,#17875,.T.);
#24112=ORIENTED_EDGE('',*,*,#17876,.T.);
#24113=ORIENTED_EDGE('',*,*,#17867,.F.);
#24114=ORIENTED_EDGE('',*,*,#17781,.F.);
#24115=ORIENTED_EDGE('',*,*,#17877,.T.);
#24116=ORIENTED_EDGE('',*,*,#17878,.T.);
#24117=ORIENTED_EDGE('',*,*,#17875,.F.);
#24118=ORIENTED_EDGE('',*,*,#17879,.F.);
#24119=ORIENTED_EDGE('',*,*,#17880,.T.);
#24120=ORIENTED_EDGE('',*,*,#17877,.F.);
#24121=ORIENTED_EDGE('',*,*,#17780,.F.);
#24122=ORIENTED_EDGE('',*,*,#17881,.T.);
#24123=ORIENTED_EDGE('',*,*,#17882,.F.);
#24124=ORIENTED_EDGE('',*,*,#17883,.F.);
#24125=ORIENTED_EDGE('',*,*,#17884,.T.);
#24126=ORIENTED_EDGE('',*,*,#17885,.F.);
#24127=ORIENTED_EDGE('',*,*,#17886,.F.);
#24128=ORIENTED_EDGE('',*,*,#17887,.T.);
#24129=ORIENTED_EDGE('',*,*,#17888,.T.);
#24130=ORIENTED_EDGE('',*,*,#17889,.T.);
#24131=ORIENTED_EDGE('',*,*,#17890,.F.);
#24132=ORIENTED_EDGE('',*,*,#17891,.F.);
#24133=ORIENTED_EDGE('',*,*,#17892,.T.);
#24134=ORIENTED_EDGE('',*,*,#17893,.T.);
#24135=ORIENTED_EDGE('',*,*,#17894,.T.);
#24136=ORIENTED_EDGE('',*,*,#17879,.T.);
#24137=ORIENTED_EDGE('',*,*,#17779,.F.);
#24138=ORIENTED_EDGE('',*,*,#17895,.F.);
#24139=ORIENTED_EDGE('',*,*,#17896,.T.);
#24140=ORIENTED_EDGE('',*,*,#17897,.F.);
#24141=ORIENTED_EDGE('',*,*,#17898,.T.);
#24142=ORIENTED_EDGE('',*,*,#17778,.F.);
#24143=ORIENTED_EDGE('',*,*,#17899,.T.);
#24144=ORIENTED_EDGE('',*,*,#17900,.T.);
#24145=ORIENTED_EDGE('',*,*,#17895,.T.);
#24146=ORIENTED_EDGE('',*,*,#17901,.T.);
#24147=ORIENTED_EDGE('',*,*,#17902,.T.);
#24148=ORIENTED_EDGE('',*,*,#17899,.F.);
#24149=ORIENTED_EDGE('',*,*,#17777,.F.);
#24150=ORIENTED_EDGE('',*,*,#17903,.T.);
#24151=ORIENTED_EDGE('',*,*,#17901,.F.);
#24152=ORIENTED_EDGE('',*,*,#17776,.F.);
#24153=ORIENTED_EDGE('',*,*,#17904,.T.);
#24154=ORIENTED_EDGE('',*,*,#17775,.T.);
#24155=ORIENTED_EDGE('',*,*,#17905,.T.);
#24156=ORIENTED_EDGE('',*,*,#17906,.T.);
#24157=ORIENTED_EDGE('',*,*,#17907,.F.);
#24158=ORIENTED_EDGE('',*,*,#17908,.F.);
#24159=ORIENTED_EDGE('',*,*,#17909,.T.);
#24160=ORIENTED_EDGE('',*,*,#17910,.F.);
#24161=ORIENTED_EDGE('',*,*,#17911,.T.);
#24162=ORIENTED_EDGE('',*,*,#17912,.T.);
#24163=ORIENTED_EDGE('',*,*,#17904,.F.);
#24164=ORIENTED_EDGE('',*,*,#17774,.T.);
#24165=ORIENTED_EDGE('',*,*,#17913,.T.);
#24166=ORIENTED_EDGE('',*,*,#17914,.F.);
#24167=ORIENTED_EDGE('',*,*,#17905,.F.);
#24168=ORIENTED_EDGE('',*,*,#17915,.F.);
#24169=ORIENTED_EDGE('',*,*,#17913,.F.);
#24170=ORIENTED_EDGE('',*,*,#17773,.T.);
#24171=ORIENTED_EDGE('',*,*,#17916,.T.);
#24172=ORIENTED_EDGE('',*,*,#17856,.F.);
#24173=ORIENTED_EDGE('',*,*,#17917,.T.);
#24174=ORIENTED_EDGE('',*,*,#17916,.F.);
#24175=ORIENTED_EDGE('',*,*,#17772,.F.);
#24176=ORIENTED_EDGE('',*,*,#17918,.F.);
#24177=ORIENTED_EDGE('',*,*,#17793,.F.);
#24178=ORIENTED_EDGE('',*,*,#17919,.T.);
#24179=ORIENTED_EDGE('',*,*,#17920,.T.);
#24180=ORIENTED_EDGE('',*,*,#17921,.T.);
#24181=ORIENTED_EDGE('',*,*,#17922,.T.);
#24182=ORIENTED_EDGE('',*,*,#17792,.F.);
#24183=ORIENTED_EDGE('',*,*,#17923,.T.);
#24184=ORIENTED_EDGE('',*,*,#17924,.F.);
#24185=ORIENTED_EDGE('',*,*,#17925,.F.);
#24186=ORIENTED_EDGE('',*,*,#17919,.F.);
#24187=ORIENTED_EDGE('',*,*,#17791,.T.);
#24188=ORIENTED_EDGE('',*,*,#17926,.T.);
#24189=ORIENTED_EDGE('',*,*,#17927,.F.);
#24190=ORIENTED_EDGE('',*,*,#17928,.F.);
#24191=ORIENTED_EDGE('',*,*,#17929,.F.);
#24192=ORIENTED_EDGE('',*,*,#17930,.F.);
#24193=ORIENTED_EDGE('',*,*,#17923,.F.);
#24194=ORIENTED_EDGE('',*,*,#17790,.F.);
#24195=ORIENTED_EDGE('',*,*,#17931,.T.);
#24196=ORIENTED_EDGE('',*,*,#17932,.T.);
#24197=ORIENTED_EDGE('',*,*,#17926,.F.);
#24198=ORIENTED_EDGE('',*,*,#17933,.F.);
#24199=ORIENTED_EDGE('',*,*,#17934,.F.);
#24200=ORIENTED_EDGE('',*,*,#17935,.F.);
#24201=ORIENTED_EDGE('',*,*,#17936,.F.);
#24202=ORIENTED_EDGE('',*,*,#17931,.F.);
#24203=ORIENTED_EDGE('',*,*,#17789,.F.);
#24204=ORIENTED_EDGE('',*,*,#17937,.T.);
#24205=ORIENTED_EDGE('',*,*,#17788,.T.);
#24206=ORIENTED_EDGE('',*,*,#17918,.T.);
#24207=ORIENTED_EDGE('',*,*,#17938,.F.);
#24208=ORIENTED_EDGE('',*,*,#17939,.F.);
#24209=ORIENTED_EDGE('',*,*,#17937,.F.);
#24210=ORIENTED_EDGE('',*,*,#17940,.T.);
#24211=ORIENTED_EDGE('',*,*,#17941,.T.);
#24212=ORIENTED_EDGE('',*,*,#17942,.T.);
#24213=ORIENTED_EDGE('',*,*,#17943,.T.);
#24214=ORIENTED_EDGE('',*,*,#17800,.F.);
#24215=ORIENTED_EDGE('',*,*,#17799,.T.);
#24216=ORIENTED_EDGE('',*,*,#17944,.T.);
#24217=ORIENTED_EDGE('',*,*,#17945,.F.);
#24218=ORIENTED_EDGE('',*,*,#17946,.F.);
#24219=ORIENTED_EDGE('',*,*,#17940,.F.);
#24220=ORIENTED_EDGE('',*,*,#17944,.F.);
#24221=ORIENTED_EDGE('',*,*,#17798,.F.);
#24222=ORIENTED_EDGE('',*,*,#17947,.T.);
#24223=ORIENTED_EDGE('',*,*,#17948,.T.);
#24224=ORIENTED_EDGE('',*,*,#17797,.T.);
#24225=ORIENTED_EDGE('',*,*,#17949,.T.);
#24226=ORIENTED_EDGE('',*,*,#17950,.T.);
#24227=ORIENTED_EDGE('',*,*,#17951,.T.);
#24228=ORIENTED_EDGE('',*,*,#17947,.F.);
#24229=ORIENTED_EDGE('',*,*,#17949,.F.);
#24230=ORIENTED_EDGE('',*,*,#17796,.T.);
#24231=ORIENTED_EDGE('',*,*,#17952,.T.);
#24232=ORIENTED_EDGE('',*,*,#17953,.F.);
#24233=ORIENTED_EDGE('',*,*,#17954,.F.);
#24234=ORIENTED_EDGE('',*,*,#17955,.F.);
#24235=ORIENTED_EDGE('',*,*,#17956,.F.);
#24236=ORIENTED_EDGE('',*,*,#17952,.F.);
#24237=ORIENTED_EDGE('',*,*,#17795,.F.);
#24238=ORIENTED_EDGE('',*,*,#17794,.T.);
#24239=ORIENTED_EDGE('',*,*,#17943,.F.);
#24240=ORIENTED_EDGE('',*,*,#17957,.F.);
#24241=ORIENTED_EDGE('',*,*,#17954,.T.);
#24242=ORIENTED_EDGE('',*,*,#17804,.F.);
#24243=ORIENTED_EDGE('',*,*,#17958,.T.);
#24244=ORIENTED_EDGE('',*,*,#17959,.T.);
#24245=ORIENTED_EDGE('',*,*,#17840,.F.);
#24246=ORIENTED_EDGE('',*,*,#17837,.F.);
#24247=ORIENTED_EDGE('',*,*,#17960,.F.);
#24248=ORIENTED_EDGE('',*,*,#17958,.F.);
#24249=ORIENTED_EDGE('',*,*,#17803,.T.);
#24250=ORIENTED_EDGE('',*,*,#17961,.T.);
#24251=ORIENTED_EDGE('',*,*,#17961,.F.);
#24252=ORIENTED_EDGE('',*,*,#17802,.F.);
#24253=ORIENTED_EDGE('',*,*,#17962,.T.);
#24254=ORIENTED_EDGE('',*,*,#17838,.T.);
#24255=ORIENTED_EDGE('',*,*,#17962,.F.);
#24256=ORIENTED_EDGE('',*,*,#17801,.F.);
#24257=ORIENTED_EDGE('',*,*,#17831,.T.);
#24258=ORIENTED_EDGE('',*,*,#17833,.T.);
#24259=ORIENTED_EDGE('',*,*,#17839,.T.);
#24260=ORIENTED_EDGE('',*,*,#17813,.F.);
#24261=ORIENTED_EDGE('',*,*,#17963,.F.);
#24262=ORIENTED_EDGE('',*,*,#17964,.T.);
#24263=ORIENTED_EDGE('',*,*,#17965,.T.);
#24264=ORIENTED_EDGE('',*,*,#17812,.T.);
#24265=ORIENTED_EDGE('',*,*,#17966,.T.);
#24266=ORIENTED_EDGE('',*,*,#17967,.T.);
#24267=ORIENTED_EDGE('',*,*,#17963,.T.);
#24268=ORIENTED_EDGE('',*,*,#17968,.T.);
#24269=ORIENTED_EDGE('',*,*,#17969,.T.);
#24270=ORIENTED_EDGE('',*,*,#17970,.T.);
#24271=ORIENTED_EDGE('',*,*,#17966,.F.);
#24272=ORIENTED_EDGE('',*,*,#17811,.F.);
#24273=ORIENTED_EDGE('',*,*,#17971,.T.);
#24274=ORIENTED_EDGE('',*,*,#17972,.T.);
#24275=ORIENTED_EDGE('',*,*,#17973,.T.);
#24276=ORIENTED_EDGE('',*,*,#17968,.F.);
#24277=ORIENTED_EDGE('',*,*,#17810,.F.);
#24278=ORIENTED_EDGE('',*,*,#17971,.F.);
#24279=ORIENTED_EDGE('',*,*,#17809,.F.);
#24280=ORIENTED_EDGE('',*,*,#17974,.T.);
#24281=ORIENTED_EDGE('',*,*,#17975,.T.);
#24282=ORIENTED_EDGE('',*,*,#17976,.T.);
#24283=ORIENTED_EDGE('',*,*,#17974,.F.);
#24284=ORIENTED_EDGE('',*,*,#17808,.F.);
#24285=ORIENTED_EDGE('',*,*,#17977,.F.);
#24286=ORIENTED_EDGE('',*,*,#17978,.T.);
#24287=ORIENTED_EDGE('',*,*,#17979,.T.);
#24288=ORIENTED_EDGE('',*,*,#17980,.T.);
#24289=ORIENTED_EDGE('',*,*,#17977,.T.);
#24290=ORIENTED_EDGE('',*,*,#17807,.F.);
#24291=ORIENTED_EDGE('',*,*,#17965,.F.);
#24292=ORIENTED_EDGE('',*,*,#17981,.T.);
#24293=ORIENTED_EDGE('',*,*,#17982,.T.);
#24294=ORIENTED_EDGE('',*,*,#17983,.T.);
#24295=ORIENTED_EDGE('',*,*,#17979,.F.);
#24296=ORIENTED_EDGE('',*,*,#17984,.F.);
#24297=ORIENTED_EDGE('',*,*,#17822,.F.);
#24298=ORIENTED_EDGE('',*,*,#17764,.T.);
#24299=ORIENTED_EDGE('',*,*,#17985,.T.);
#24300=ORIENTED_EDGE('',*,*,#17986,.T.);
#24301=ORIENTED_EDGE('',*,*,#17987,.F.);
#24302=ORIENTED_EDGE('',*,*,#17766,.F.);
#24303=ORIENTED_EDGE('',*,*,#17821,.T.);
#24304=ORIENTED_EDGE('',*,*,#17988,.T.);
#24305=ORIENTED_EDGE('',*,*,#17986,.F.);
#24306=ORIENTED_EDGE('',*,*,#17820,.F.);
#24307=ORIENTED_EDGE('',*,*,#17989,.T.);
#24308=ORIENTED_EDGE('',*,*,#17990,.F.);
#24309=ORIENTED_EDGE('',*,*,#17989,.F.);
#24310=ORIENTED_EDGE('',*,*,#17819,.T.);
#24311=ORIENTED_EDGE('',*,*,#17991,.T.);
#24312=ORIENTED_EDGE('',*,*,#17992,.T.);
#24313=ORIENTED_EDGE('',*,*,#17991,.F.);
#24314=ORIENTED_EDGE('',*,*,#17818,.F.);
#24315=ORIENTED_EDGE('',*,*,#17993,.T.);
#24316=ORIENTED_EDGE('',*,*,#17994,.T.);
#24317=ORIENTED_EDGE('',*,*,#17993,.F.);
#24318=ORIENTED_EDGE('',*,*,#17817,.F.);
#24319=ORIENTED_EDGE('',*,*,#17995,.T.);
#24320=ORIENTED_EDGE('',*,*,#17995,.F.);
#24321=ORIENTED_EDGE('',*,*,#17816,.F.);
#24322=ORIENTED_EDGE('',*,*,#17996,.T.);
#24323=ORIENTED_EDGE('',*,*,#17997,.T.);
#24324=ORIENTED_EDGE('',*,*,#17998,.T.);
#24325=ORIENTED_EDGE('',*,*,#17996,.F.);
#24326=ORIENTED_EDGE('',*,*,#17815,.F.);
#24327=ORIENTED_EDGE('',*,*,#17999,.T.);
#24328=ORIENTED_EDGE('',*,*,#17999,.F.);
#24329=ORIENTED_EDGE('',*,*,#17814,.F.);
#24330=ORIENTED_EDGE('',*,*,#17984,.T.);
#24331=ORIENTED_EDGE('',*,*,#18000,.T.);
#24332=ORIENTED_EDGE('',*,*,#17829,.T.);
#24333=ORIENTED_EDGE('',*,*,#18001,.T.);
#24334=ORIENTED_EDGE('',*,*,#18002,.F.);
#24335=ORIENTED_EDGE('',*,*,#18003,.T.);
#24336=ORIENTED_EDGE('',*,*,#18004,.F.);
#24337=ORIENTED_EDGE('',*,*,#18001,.F.);
#24338=ORIENTED_EDGE('',*,*,#17828,.T.);
#24339=ORIENTED_EDGE('',*,*,#18005,.T.);
#24340=ORIENTED_EDGE('',*,*,#17827,.T.);
#24341=ORIENTED_EDGE('',*,*,#18006,.T.);
#24342=ORIENTED_EDGE('',*,*,#18007,.F.);
#24343=ORIENTED_EDGE('',*,*,#18008,.F.);
#24344=ORIENTED_EDGE('',*,*,#18005,.F.);
#24345=ORIENTED_EDGE('',*,*,#18006,.F.);
#24346=ORIENTED_EDGE('',*,*,#17826,.F.);
#24347=ORIENTED_EDGE('',*,*,#18009,.T.);
#24348=ORIENTED_EDGE('',*,*,#18010,.T.);
#24349=ORIENTED_EDGE('',*,*,#18011,.T.);
#24350=ORIENTED_EDGE('',*,*,#18012,.T.);
#24351=ORIENTED_EDGE('',*,*,#18013,.F.);
#24352=ORIENTED_EDGE('',*,*,#18009,.F.);
#24353=ORIENTED_EDGE('',*,*,#17825,.F.);
#24354=ORIENTED_EDGE('',*,*,#18014,.F.);
#24355=ORIENTED_EDGE('',*,*,#18012,.F.);
#24356=ORIENTED_EDGE('',*,*,#17824,.T.);
#24357=ORIENTED_EDGE('',*,*,#18015,.F.);
#24358=ORIENTED_EDGE('',*,*,#18016,.F.);
#24359=ORIENTED_EDGE('',*,*,#18017,.F.);
#24360=ORIENTED_EDGE('',*,*,#18018,.F.);
#24361=ORIENTED_EDGE('',*,*,#18015,.T.);
#24362=ORIENTED_EDGE('',*,*,#17823,.F.);
#24363=ORIENTED_EDGE('',*,*,#18003,.F.);
#24364=ORIENTED_EDGE('',*,*,#18019,.F.);
#24365=ORIENTED_EDGE('',*,*,#18020,.T.);
#24366=ORIENTED_EDGE('',*,*,#18021,.F.);
#24367=ORIENTED_EDGE('',*,*,#18022,.F.);
#24368=ORIENTED_EDGE('',*,*,#18020,.F.);
#24369=ORIENTED_EDGE('',*,*,#17836,.T.);
#24370=ORIENTED_EDGE('',*,*,#17835,.T.);
#24371=ORIENTED_EDGE('',*,*,#17841,.T.);
#24372=ORIENTED_EDGE('',*,*,#17959,.F.);
#24373=ORIENTED_EDGE('',*,*,#17960,.T.);
#24374=ORIENTED_EDGE('',*,*,#17862,.F.);
#24375=ORIENTED_EDGE('',*,*,#17864,.T.);
#24376=ORIENTED_EDGE('',*,*,#17865,.T.);
#24377=ORIENTED_EDGE('',*,*,#17874,.F.);
#24378=ORIENTED_EDGE('',*,*,#18023,.T.);
#24379=ORIENTED_EDGE('',*,*,#17858,.F.);
#24380=ORIENTED_EDGE('',*,*,#18024,.T.);
#24381=ORIENTED_EDGE('',*,*,#18025,.T.);
#24382=ORIENTED_EDGE('',*,*,#17859,.T.);
#24383=ORIENTED_EDGE('',*,*,#18023,.F.);
#24384=ORIENTED_EDGE('',*,*,#17873,.F.);
#24385=ORIENTED_EDGE('',*,*,#18026,.F.);
#24386=ORIENTED_EDGE('',*,*,#18027,.T.);
#24387=ORIENTED_EDGE('',*,*,#18028,.F.);
#24388=ORIENTED_EDGE('',*,*,#18029,.F.);
#24389=ORIENTED_EDGE('',*,*,#17846,.T.);
#24390=ORIENTED_EDGE('',*,*,#18030,.F.);
#24391=ORIENTED_EDGE('',*,*,#18031,.F.);
#24392=ORIENTED_EDGE('',*,*,#18032,.F.);
#24393=ORIENTED_EDGE('',*,*,#18029,.T.);
#24394=ORIENTED_EDGE('',*,*,#18033,.F.);
#24395=ORIENTED_EDGE('',*,*,#18034,.F.);
#24396=ORIENTED_EDGE('',*,*,#17847,.F.);
#24397=ORIENTED_EDGE('',*,*,#18035,.T.);
#24398=ORIENTED_EDGE('',*,*,#18036,.T.);
#24399=ORIENTED_EDGE('',*,*,#18037,.T.);
#24400=ORIENTED_EDGE('',*,*,#17848,.F.);
#24401=ORIENTED_EDGE('',*,*,#18034,.T.);
#24402=ORIENTED_EDGE('',*,*,#18038,.T.);
#24403=ORIENTED_EDGE('',*,*,#18039,.F.);
#24404=ORIENTED_EDGE('',*,*,#18040,.T.);
#24405=ORIENTED_EDGE('',*,*,#18041,.T.);
#24406=ORIENTED_EDGE('',*,*,#17907,.T.);
#24407=ORIENTED_EDGE('',*,*,#18042,.F.);
#24408=ORIENTED_EDGE('',*,*,#17854,.F.);
#24409=ORIENTED_EDGE('',*,*,#18043,.F.);
#24410=ORIENTED_EDGE('',*,*,#17855,.F.);
#24411=ORIENTED_EDGE('',*,*,#18042,.T.);
#24412=ORIENTED_EDGE('',*,*,#17906,.F.);
#24413=ORIENTED_EDGE('',*,*,#17914,.T.);
#24414=ORIENTED_EDGE('',*,*,#17915,.T.);
#24415=ORIENTED_EDGE('',*,*,#17917,.F.);
#24416=ORIENTED_EDGE('',*,*,#17894,.F.);
#24417=ORIENTED_EDGE('',*,*,#18044,.F.);
#24418=ORIENTED_EDGE('',*,*,#17868,.F.);
#24419=ORIENTED_EDGE('',*,*,#17876,.F.);
#24420=ORIENTED_EDGE('',*,*,#17878,.F.);
#24421=ORIENTED_EDGE('',*,*,#17880,.F.);
#24422=ORIENTED_EDGE('',*,*,#17869,.T.);
#24423=ORIENTED_EDGE('',*,*,#18044,.T.);
#24424=ORIENTED_EDGE('',*,*,#17893,.F.);
#24425=ORIENTED_EDGE('',*,*,#18045,.F.);
#24426=ORIENTED_EDGE('',*,*,#18046,.F.);
#24427=ORIENTED_EDGE('',*,*,#17900,.F.);
#24428=ORIENTED_EDGE('',*,*,#17902,.F.);
#24429=ORIENTED_EDGE('',*,*,#17903,.F.);
#24430=ORIENTED_EDGE('',*,*,#17912,.F.);
#24431=ORIENTED_EDGE('',*,*,#18047,.F.);
#24432=ORIENTED_EDGE('',*,*,#17896,.F.);
#24433=ORIENTED_EDGE('',*,*,#18048,.T.);
#24434=ORIENTED_EDGE('',*,*,#17897,.T.);
#24435=ORIENTED_EDGE('',*,*,#18047,.T.);
#24436=ORIENTED_EDGE('',*,*,#17911,.F.);
#24437=ORIENTED_EDGE('',*,*,#18049,.F.);
#24438=ORIENTED_EDGE('',*,*,#18050,.T.);
#24439=ORIENTED_EDGE('',*,*,#18051,.F.);
#24440=ORIENTED_EDGE('',*,*,#18052,.T.);
#24441=ORIENTED_EDGE('',*,*,#18053,.F.);
#24442=ORIENTED_EDGE('',*,*,#18054,.T.);
#24443=ORIENTED_EDGE('',*,*,#18055,.F.);
#24444=ORIENTED_EDGE('',*,*,#18056,.F.);
#24445=ORIENTED_EDGE('',*,*,#17885,.T.);
#24446=ORIENTED_EDGE('',*,*,#17886,.T.);
#24447=ORIENTED_EDGE('',*,*,#18056,.T.);
#24448=ORIENTED_EDGE('',*,*,#18057,.T.);
#24449=ORIENTED_EDGE('',*,*,#18058,.F.);
#24450=ORIENTED_EDGE('',*,*,#17887,.F.);
#24451=ORIENTED_EDGE('',*,*,#18058,.T.);
#24452=ORIENTED_EDGE('',*,*,#18059,.T.);
#24453=ORIENTED_EDGE('',*,*,#18060,.F.);
#24454=ORIENTED_EDGE('',*,*,#18061,.T.);
#24455=ORIENTED_EDGE('',*,*,#18062,.F.);
#24456=ORIENTED_EDGE('',*,*,#18063,.T.);
#24457=ORIENTED_EDGE('',*,*,#18064,.F.);
#24458=ORIENTED_EDGE('',*,*,#18065,.T.);
#24459=ORIENTED_EDGE('',*,*,#17909,.F.);
#24460=ORIENTED_EDGE('',*,*,#18066,.F.);
#24461=ORIENTED_EDGE('',*,*,#18067,.T.);
#24462=ORIENTED_EDGE('',*,*,#18049,.T.);
#24463=ORIENTED_EDGE('',*,*,#17910,.T.);
#24464=ORIENTED_EDGE('',*,*,#18065,.F.);
#24465=ORIENTED_EDGE('',*,*,#18068,.T.);
#24466=ORIENTED_EDGE('',*,*,#18041,.F.);
#24467=ORIENTED_EDGE('',*,*,#18069,.F.);
#24468=ORIENTED_EDGE('',*,*,#18066,.T.);
#24469=ORIENTED_EDGE('',*,*,#17908,.T.);
#24470=ORIENTED_EDGE('',*,*,#17938,.T.);
#24471=ORIENTED_EDGE('',*,*,#17922,.F.);
#24472=ORIENTED_EDGE('',*,*,#18070,.F.);
#24473=ORIENTED_EDGE('',*,*,#18071,.T.);
#24474=ORIENTED_EDGE('',*,*,#17924,.T.);
#24475=ORIENTED_EDGE('',*,*,#17930,.T.);
#24476=ORIENTED_EDGE('',*,*,#18072,.F.);
#24477=ORIENTED_EDGE('',*,*,#18073,.T.);
#24478=ORIENTED_EDGE('',*,*,#18074,.T.);
#24479=ORIENTED_EDGE('',*,*,#17933,.T.);
#24480=ORIENTED_EDGE('',*,*,#17939,.T.);
#24481=ORIENTED_EDGE('',*,*,#18071,.F.);
#24482=ORIENTED_EDGE('',*,*,#18070,.T.);
#24483=ORIENTED_EDGE('',*,*,#17921,.F.);
#24484=ORIENTED_EDGE('',*,*,#18075,.F.);
#24485=ORIENTED_EDGE('',*,*,#18076,.F.);
#24486=ORIENTED_EDGE('',*,*,#17925,.T.);
#24487=ORIENTED_EDGE('',*,*,#18076,.T.);
#24488=ORIENTED_EDGE('',*,*,#18075,.T.);
#24489=ORIENTED_EDGE('',*,*,#17920,.F.);
#24490=ORIENTED_EDGE('',*,*,#17934,.T.);
#24491=ORIENTED_EDGE('',*,*,#18074,.F.);
#24492=ORIENTED_EDGE('',*,*,#18073,.F.);
#24493=ORIENTED_EDGE('',*,*,#18072,.T.);
#24494=ORIENTED_EDGE('',*,*,#17929,.T.);
#24495=ORIENTED_EDGE('',*,*,#18077,.T.);
#24496=ORIENTED_EDGE('',*,*,#18078,.F.);
#24497=ORIENTED_EDGE('',*,*,#17927,.T.);
#24498=ORIENTED_EDGE('',*,*,#17932,.F.);
#24499=ORIENTED_EDGE('',*,*,#17936,.T.);
#24500=ORIENTED_EDGE('',*,*,#18079,.T.);
#24501=ORIENTED_EDGE('',*,*,#18080,.T.);
#24502=ORIENTED_EDGE('',*,*,#17928,.T.);
#24503=ORIENTED_EDGE('',*,*,#18078,.T.);
#24504=ORIENTED_EDGE('',*,*,#18077,.F.);
#24505=ORIENTED_EDGE('',*,*,#18080,.F.);
#24506=ORIENTED_EDGE('',*,*,#18079,.F.);
#24507=ORIENTED_EDGE('',*,*,#17935,.T.);
#24508=ORIENTED_EDGE('',*,*,#18081,.F.);
#24509=ORIENTED_EDGE('',*,*,#17955,.T.);
#24510=ORIENTED_EDGE('',*,*,#17957,.T.);
#24511=ORIENTED_EDGE('',*,*,#17942,.F.);
#24512=ORIENTED_EDGE('',*,*,#18082,.T.);
#24513=ORIENTED_EDGE('',*,*,#17946,.T.);
#24514=ORIENTED_EDGE('',*,*,#18083,.F.);
#24515=ORIENTED_EDGE('',*,*,#17950,.F.);
#24516=ORIENTED_EDGE('',*,*,#17953,.T.);
#24517=ORIENTED_EDGE('',*,*,#17956,.T.);
#24518=ORIENTED_EDGE('',*,*,#18081,.T.);
#24519=ORIENTED_EDGE('',*,*,#18082,.F.);
#24520=ORIENTED_EDGE('',*,*,#17941,.F.);
#24521=ORIENTED_EDGE('',*,*,#17945,.T.);
#24522=ORIENTED_EDGE('',*,*,#17948,.F.);
#24523=ORIENTED_EDGE('',*,*,#17951,.F.);
#24524=ORIENTED_EDGE('',*,*,#18083,.T.);
#24525=ORIENTED_EDGE('',*,*,#17981,.F.);
#24526=ORIENTED_EDGE('',*,*,#17964,.F.);
#24527=ORIENTED_EDGE('',*,*,#17967,.F.);
#24528=ORIENTED_EDGE('',*,*,#17970,.F.);
#24529=ORIENTED_EDGE('',*,*,#18084,.T.);
#24530=ORIENTED_EDGE('',*,*,#18085,.F.);
#24531=ORIENTED_EDGE('',*,*,#17982,.F.);
#24532=ORIENTED_EDGE('',*,*,#18085,.T.);
#24533=ORIENTED_EDGE('',*,*,#18084,.F.);
#24534=ORIENTED_EDGE('',*,*,#17969,.F.);
#24535=ORIENTED_EDGE('',*,*,#17973,.F.);
#24536=ORIENTED_EDGE('',*,*,#18086,.T.);
#24537=ORIENTED_EDGE('',*,*,#17983,.F.);
#24538=ORIENTED_EDGE('',*,*,#18086,.F.);
#24539=ORIENTED_EDGE('',*,*,#17972,.F.);
#24540=ORIENTED_EDGE('',*,*,#17975,.F.);
#24541=ORIENTED_EDGE('',*,*,#17976,.F.);
#24542=ORIENTED_EDGE('',*,*,#17980,.F.);
#24543=ORIENTED_EDGE('',*,*,#17978,.F.);
#24544=ORIENTED_EDGE('',*,*,#18087,.T.);
#24545=ORIENTED_EDGE('',*,*,#18088,.T.);
#24546=ORIENTED_EDGE('',*,*,#18087,.F.);
#24547=ORIENTED_EDGE('',*,*,#17998,.F.);
#24548=ORIENTED_EDGE('',*,*,#18000,.F.);
#24549=ORIENTED_EDGE('',*,*,#17985,.F.);
#24550=ORIENTED_EDGE('',*,*,#17763,.T.);
#24551=ORIENTED_EDGE('',*,*,#17987,.T.);
#24552=ORIENTED_EDGE('',*,*,#17988,.F.);
#24553=ORIENTED_EDGE('',*,*,#17990,.T.);
#24554=ORIENTED_EDGE('',*,*,#17992,.F.);
#24555=ORIENTED_EDGE('',*,*,#17994,.F.);
#24556=ORIENTED_EDGE('',*,*,#17997,.F.);
#24557=ORIENTED_EDGE('',*,*,#18089,.F.);
#24558=ORIENTED_EDGE('',*,*,#18090,.F.);
#24559=ORIENTED_EDGE('',*,*,#18091,.F.);
#24560=ORIENTED_EDGE('',*,*,#18092,.T.);
#24561=ORIENTED_EDGE('',*,*,#18093,.F.);
#24562=ORIENTED_EDGE('',*,*,#18094,.F.);
#24563=ORIENTED_EDGE('',*,*,#18095,.F.);
#24564=ORIENTED_EDGE('',*,*,#18096,.T.);
#24565=ORIENTED_EDGE('',*,*,#18097,.T.);
#24566=ORIENTED_EDGE('',*,*,#18098,.T.);
#24567=ORIENTED_EDGE('',*,*,#18099,.F.);
#24568=ORIENTED_EDGE('',*,*,#18016,.T.);
#24569=ORIENTED_EDGE('',*,*,#18019,.T.);
#24570=ORIENTED_EDGE('',*,*,#18002,.T.);
#24571=ORIENTED_EDGE('',*,*,#18004,.T.);
#24572=ORIENTED_EDGE('',*,*,#18008,.T.);
#24573=ORIENTED_EDGE('',*,*,#18100,.F.);
#24574=ORIENTED_EDGE('',*,*,#18017,.T.);
#24575=ORIENTED_EDGE('',*,*,#18100,.T.);
#24576=ORIENTED_EDGE('',*,*,#18007,.T.);
#24577=ORIENTED_EDGE('',*,*,#18011,.F.);
#24578=ORIENTED_EDGE('',*,*,#18101,.T.);
#24579=ORIENTED_EDGE('',*,*,#18102,.T.);
#24580=ORIENTED_EDGE('',*,*,#18018,.T.);
#24581=ORIENTED_EDGE('',*,*,#18102,.F.);
#24582=ORIENTED_EDGE('',*,*,#18101,.F.);
#24583=ORIENTED_EDGE('',*,*,#18010,.F.);
#24584=ORIENTED_EDGE('',*,*,#18013,.T.);
#24585=ORIENTED_EDGE('',*,*,#18014,.T.);
#24586=ORIENTED_EDGE('',*,*,#18022,.T.);
#24587=ORIENTED_EDGE('',*,*,#18103,.T.);
#24588=ORIENTED_EDGE('',*,*,#18104,.F.);
#24589=ORIENTED_EDGE('',*,*,#18103,.F.);
#24590=ORIENTED_EDGE('',*,*,#18021,.T.);
#24591=ORIENTED_EDGE('',*,*,#18024,.F.);
#24592=ORIENTED_EDGE('',*,*,#17872,.T.);
#24593=ORIENTED_EDGE('',*,*,#18105,.T.);
#24594=ORIENTED_EDGE('',*,*,#18106,.T.);
#24595=ORIENTED_EDGE('',*,*,#18025,.F.);
#24596=ORIENTED_EDGE('',*,*,#18106,.F.);
#24597=ORIENTED_EDGE('',*,*,#18107,.F.);
#24598=ORIENTED_EDGE('',*,*,#18108,.F.);
#24599=ORIENTED_EDGE('',*,*,#18045,.T.);
#24600=ORIENTED_EDGE('',*,*,#18109,.T.);
#24601=ORIENTED_EDGE('',*,*,#18110,.F.);
#24602=ORIENTED_EDGE('',*,*,#18111,.T.);
#24603=ORIENTED_EDGE('',*,*,#18031,.T.);
#24604=ORIENTED_EDGE('',*,*,#18112,.T.);
#24605=ORIENTED_EDGE('',*,*,#18113,.T.);
#24606=ORIENTED_EDGE('',*,*,#18114,.F.);
#24607=ORIENTED_EDGE('',*,*,#18115,.T.);
#24608=ORIENTED_EDGE('',*,*,#18116,.T.);
#24609=ORIENTED_EDGE('',*,*,#18117,.T.);
#24610=ORIENTED_EDGE('',*,*,#18118,.T.);
#24611=ORIENTED_EDGE('',*,*,#18119,.F.);
#24612=ORIENTED_EDGE('',*,*,#18120,.T.);
#24613=ORIENTED_EDGE('',*,*,#18121,.F.);
#24614=ORIENTED_EDGE('',*,*,#18122,.T.);
#24615=ORIENTED_EDGE('',*,*,#18123,.T.);
#24616=ORIENTED_EDGE('',*,*,#18124,.T.);
#24617=ORIENTED_EDGE('',*,*,#18125,.T.);
#24618=ORIENTED_EDGE('',*,*,#18126,.F.);
#24619=ORIENTED_EDGE('',*,*,#18127,.F.);
#24620=ORIENTED_EDGE('',*,*,#18128,.T.);
#24621=ORIENTED_EDGE('',*,*,#18129,.T.);
#24622=ORIENTED_EDGE('',*,*,#18130,.T.);
#24623=ORIENTED_EDGE('',*,*,#18063,.F.);
#24624=ORIENTED_EDGE('',*,*,#18131,.T.);
#24625=ORIENTED_EDGE('',*,*,#18040,.F.);
#24626=ORIENTED_EDGE('',*,*,#18132,.F.);
#24627=ORIENTED_EDGE('',*,*,#18026,.T.);
#24628=ORIENTED_EDGE('',*,*,#18133,.T.);
#24629=ORIENTED_EDGE('',*,*,#18134,.T.);
#24630=ORIENTED_EDGE('',*,*,#18027,.F.);
#24631=ORIENTED_EDGE('',*,*,#18132,.T.);
#24632=ORIENTED_EDGE('',*,*,#18039,.T.);
#24633=ORIENTED_EDGE('',*,*,#18033,.T.);
#24634=ORIENTED_EDGE('',*,*,#18028,.T.);
#24635=ORIENTED_EDGE('',*,*,#18134,.F.);
#24636=ORIENTED_EDGE('',*,*,#18038,.F.);
#24637=ORIENTED_EDGE('',*,*,#18135,.T.);
#24638=ORIENTED_EDGE('',*,*,#18136,.F.);
#24639=ORIENTED_EDGE('',*,*,#18137,.F.);
#24640=ORIENTED_EDGE('',*,*,#18138,.T.);
#24641=ORIENTED_EDGE('',*,*,#18139,.F.);
#24642=ORIENTED_EDGE('',*,*,#18140,.F.);
#24643=ORIENTED_EDGE('',*,*,#18141,.T.);
#24644=ORIENTED_EDGE('',*,*,#18142,.T.);
#24645=ORIENTED_EDGE('',*,*,#18143,.F.);
#24646=ORIENTED_EDGE('',*,*,#18144,.F.);
#24647=ORIENTED_EDGE('',*,*,#18145,.T.);
#24648=ORIENTED_EDGE('',*,*,#18146,.F.);
#24649=ORIENTED_EDGE('',*,*,#18147,.F.);
#24650=ORIENTED_EDGE('',*,*,#18035,.F.);
#24651=ORIENTED_EDGE('',*,*,#18133,.F.);
#24652=ORIENTED_EDGE('',*,*,#18032,.T.);
#24653=ORIENTED_EDGE('',*,*,#18111,.F.);
#24654=ORIENTED_EDGE('',*,*,#18148,.F.);
#24655=ORIENTED_EDGE('',*,*,#18149,.F.);
#24656=ORIENTED_EDGE('',*,*,#18150,.T.);
#24657=ORIENTED_EDGE('',*,*,#18151,.F.);
#24658=ORIENTED_EDGE('',*,*,#18152,.T.);
#24659=ORIENTED_EDGE('',*,*,#18153,.T.);
#24660=ORIENTED_EDGE('',*,*,#18113,.F.);
#24661=ORIENTED_EDGE('',*,*,#18154,.T.);
#24662=ORIENTED_EDGE('',*,*,#18155,.F.);
#24663=ORIENTED_EDGE('',*,*,#18156,.F.);
#24664=ORIENTED_EDGE('',*,*,#18157,.T.);
#24665=ORIENTED_EDGE('',*,*,#18158,.F.);
#24666=ORIENTED_EDGE('',*,*,#18159,.T.);
#24667=ORIENTED_EDGE('',*,*,#18120,.F.);
#24668=ORIENTED_EDGE('',*,*,#18160,.T.);
#24669=ORIENTED_EDGE('',*,*,#18161,.T.);
#24670=ORIENTED_EDGE('',*,*,#18162,.T.);
#24671=ORIENTED_EDGE('',*,*,#18163,.F.);
#24672=ORIENTED_EDGE('',*,*,#18164,.T.);
#24673=ORIENTED_EDGE('',*,*,#18165,.F.);
#24674=ORIENTED_EDGE('',*,*,#18166,.T.);
#24675=ORIENTED_EDGE('',*,*,#18167,.T.);
#24676=ORIENTED_EDGE('',*,*,#18036,.F.);
#24677=ORIENTED_EDGE('',*,*,#18147,.T.);
#24678=ORIENTED_EDGE('',*,*,#18140,.T.);
#24679=ORIENTED_EDGE('',*,*,#18168,.F.);
#24680=ORIENTED_EDGE('',*,*,#18169,.T.);
#24681=ORIENTED_EDGE('',*,*,#18170,.T.);
#24682=ORIENTED_EDGE('',*,*,#18171,.F.);
#24683=ORIENTED_EDGE('',*,*,#18139,.T.);
#24684=ORIENTED_EDGE('',*,*,#18172,.T.);
#24685=ORIENTED_EDGE('',*,*,#18173,.T.);
#24686=ORIENTED_EDGE('',*,*,#18174,.T.);
#24687=ORIENTED_EDGE('',*,*,#18175,.T.);
#24688=ORIENTED_EDGE('',*,*,#18176,.F.);
#24689=ORIENTED_EDGE('',*,*,#18177,.T.);
#24690=ORIENTED_EDGE('',*,*,#18178,.T.);
#24691=ORIENTED_EDGE('',*,*,#18179,.F.);
#24692=ORIENTED_EDGE('',*,*,#18180,.F.);
#24693=ORIENTED_EDGE('',*,*,#18181,.T.);
#24694=ORIENTED_EDGE('',*,*,#18182,.F.);
#24695=ORIENTED_EDGE('',*,*,#18183,.T.);
#24696=ORIENTED_EDGE('',*,*,#18051,.T.);
#24697=ORIENTED_EDGE('',*,*,#18184,.T.);
#24698=ORIENTED_EDGE('',*,*,#18185,.T.);
#24699=ORIENTED_EDGE('',*,*,#18048,.F.);
#24700=ORIENTED_EDGE('',*,*,#18068,.F.);
#24701=ORIENTED_EDGE('',*,*,#18067,.F.);
#24702=ORIENTED_EDGE('',*,*,#18069,.T.);
#24703=ORIENTED_EDGE('',*,*,#18043,.T.);
#24704=ORIENTED_EDGE('',*,*,#18107,.T.);
#24705=ORIENTED_EDGE('',*,*,#18105,.F.);
#24706=ORIENTED_EDGE('',*,*,#17871,.F.);
#24707=ORIENTED_EDGE('',*,*,#18186,.T.);
#24708=ORIENTED_EDGE('',*,*,#18186,.F.);
#24709=ORIENTED_EDGE('',*,*,#17870,.T.);
#24710=ORIENTED_EDGE('',*,*,#18046,.T.);
#24711=ORIENTED_EDGE('',*,*,#18108,.T.);
#24712=ORIENTED_EDGE('',*,*,#18055,.T.);
#24713=ORIENTED_EDGE('',*,*,#18187,.T.);
#24714=ORIENTED_EDGE('',*,*,#18059,.F.);
#24715=ORIENTED_EDGE('',*,*,#18057,.F.);
#24716=ORIENTED_EDGE('',*,*,#18054,.F.);
#24717=ORIENTED_EDGE('',*,*,#18188,.F.);
#24718=ORIENTED_EDGE('',*,*,#18060,.T.);
#24719=ORIENTED_EDGE('',*,*,#18187,.F.);
#24720=ORIENTED_EDGE('',*,*,#18189,.F.);
#24721=ORIENTED_EDGE('',*,*,#18061,.F.);
#24722=ORIENTED_EDGE('',*,*,#18188,.T.);
#24723=ORIENTED_EDGE('',*,*,#18053,.T.);
#24724=ORIENTED_EDGE('',*,*,#18177,.F.);
#24725=ORIENTED_EDGE('',*,*,#18190,.F.);
#24726=ORIENTED_EDGE('',*,*,#18191,.F.);
#24727=ORIENTED_EDGE('',*,*,#18192,.T.);
#24728=ORIENTED_EDGE('',*,*,#18193,.F.);
#24729=ORIENTED_EDGE('',*,*,#18194,.F.);
#24730=ORIENTED_EDGE('',*,*,#18195,.T.);
#24731=ORIENTED_EDGE('',*,*,#18178,.F.);
#24732=ORIENTED_EDGE('',*,*,#18196,.T.);
#24733=ORIENTED_EDGE('',*,*,#18197,.T.);
#24734=ORIENTED_EDGE('',*,*,#18198,.T.);
#24735=ORIENTED_EDGE('',*,*,#18125,.F.);
#24736=ORIENTED_EDGE('',*,*,#18199,.T.);
#24737=ORIENTED_EDGE('',*,*,#18200,.F.);
#24738=ORIENTED_EDGE('',*,*,#18201,.F.);
#24739=ORIENTED_EDGE('',*,*,#18202,.F.);
#24740=ORIENTED_EDGE('',*,*,#18203,.F.);
#24741=ORIENTED_EDGE('',*,*,#18204,.T.);
#24742=ORIENTED_EDGE('',*,*,#18131,.F.);
#24743=ORIENTED_EDGE('',*,*,#18062,.T.);
#24744=ORIENTED_EDGE('',*,*,#18189,.T.);
#24745=ORIENTED_EDGE('',*,*,#18052,.F.);
#24746=ORIENTED_EDGE('',*,*,#18183,.F.);
#24747=ORIENTED_EDGE('',*,*,#18205,.T.);
#24748=ORIENTED_EDGE('',*,*,#18206,.T.);
#24749=ORIENTED_EDGE('',*,*,#18207,.F.);
#24750=ORIENTED_EDGE('',*,*,#18208,.T.);
#24751=ORIENTED_EDGE('',*,*,#18209,.F.);
#24752=ORIENTED_EDGE('',*,*,#18210,.F.);
#24753=ORIENTED_EDGE('',*,*,#18211,.F.);
#24754=ORIENTED_EDGE('',*,*,#18122,.F.);
#24755=ORIENTED_EDGE('',*,*,#18212,.F.);
#24756=ORIENTED_EDGE('',*,*,#18213,.F.);
#24757=ORIENTED_EDGE('',*,*,#18214,.F.);
#24758=ORIENTED_EDGE('',*,*,#18215,.F.);
#24759=ORIENTED_EDGE('',*,*,#18216,.T.);
#24760=ORIENTED_EDGE('',*,*,#18217,.T.);
#24761=ORIENTED_EDGE('',*,*,#18088,.F.);
#24762=ORIENTED_EDGE('',*,*,#18218,.T.);
#24763=ORIENTED_EDGE('',*,*,#18089,.T.);
#24764=ORIENTED_EDGE('',*,*,#18219,.F.);
#24765=ORIENTED_EDGE('',*,*,#18220,.T.);
#24766=ORIENTED_EDGE('',*,*,#18221,.T.);
#24767=ORIENTED_EDGE('',*,*,#18221,.F.);
#24768=ORIENTED_EDGE('',*,*,#18222,.T.);
#24769=ORIENTED_EDGE('',*,*,#18223,.T.);
#24770=ORIENTED_EDGE('',*,*,#18090,.T.);
#24771=ORIENTED_EDGE('',*,*,#18091,.T.);
#24772=ORIENTED_EDGE('',*,*,#18223,.F.);
#24773=ORIENTED_EDGE('',*,*,#18224,.T.);
#24774=ORIENTED_EDGE('',*,*,#18225,.T.);
#24775=ORIENTED_EDGE('',*,*,#18226,.T.);
#24776=ORIENTED_EDGE('',*,*,#18092,.F.);
#24777=ORIENTED_EDGE('',*,*,#18225,.F.);
#24778=ORIENTED_EDGE('',*,*,#18227,.F.);
#24779=ORIENTED_EDGE('',*,*,#18093,.T.);
#24780=ORIENTED_EDGE('',*,*,#18226,.F.);
#24781=ORIENTED_EDGE('',*,*,#18228,.T.);
#24782=ORIENTED_EDGE('',*,*,#18229,.T.);
#24783=ORIENTED_EDGE('',*,*,#18229,.F.);
#24784=ORIENTED_EDGE('',*,*,#18230,.F.);
#24785=ORIENTED_EDGE('',*,*,#18231,.T.);
#24786=ORIENTED_EDGE('',*,*,#18094,.T.);
#24787=ORIENTED_EDGE('',*,*,#18231,.F.);
#24788=ORIENTED_EDGE('',*,*,#18232,.F.);
#24789=ORIENTED_EDGE('',*,*,#18233,.T.);
#24790=ORIENTED_EDGE('',*,*,#18095,.T.);
#24791=ORIENTED_EDGE('',*,*,#18233,.F.);
#24792=ORIENTED_EDGE('',*,*,#18234,.T.);
#24793=ORIENTED_EDGE('',*,*,#18235,.T.);
#24794=ORIENTED_EDGE('',*,*,#18096,.F.);
#24795=ORIENTED_EDGE('',*,*,#18097,.F.);
#24796=ORIENTED_EDGE('',*,*,#18235,.F.);
#24797=ORIENTED_EDGE('',*,*,#18236,.T.);
#24798=ORIENTED_EDGE('',*,*,#18219,.T.);
#24799=ORIENTED_EDGE('',*,*,#18098,.F.);
#24800=ORIENTED_EDGE('',*,*,#18237,.T.);
#24801=ORIENTED_EDGE('',*,*,#18238,.T.);
#24802=ORIENTED_EDGE('',*,*,#18237,.F.);
#24803=ORIENTED_EDGE('',*,*,#18239,.F.);
#24804=ORIENTED_EDGE('',*,*,#18240,.T.);
#24805=ORIENTED_EDGE('',*,*,#18099,.T.);
#24806=ORIENTED_EDGE('',*,*,#18240,.F.);
#24807=ORIENTED_EDGE('',*,*,#18104,.T.);
#24808=ORIENTED_EDGE('',*,*,#18241,.F.);
#24809=ORIENTED_EDGE('',*,*,#18242,.T.);
#24810=ORIENTED_EDGE('',*,*,#18243,.F.);
#24811=ORIENTED_EDGE('',*,*,#18161,.F.);
#24812=ORIENTED_EDGE('',*,*,#18244,.T.);
#24813=ORIENTED_EDGE('',*,*,#18162,.F.);
#24814=ORIENTED_EDGE('',*,*,#18243,.T.);
#24815=ORIENTED_EDGE('',*,*,#18245,.F.);
#24816=ORIENTED_EDGE('',*,*,#18246,.F.);
#24817=ORIENTED_EDGE('',*,*,#18247,.F.);
#24818=ORIENTED_EDGE('',*,*,#18163,.T.);
#24819=ORIENTED_EDGE('',*,*,#18246,.T.);
#24820=ORIENTED_EDGE('',*,*,#18248,.F.);
#24821=ORIENTED_EDGE('',*,*,#18164,.F.);
#24822=ORIENTED_EDGE('',*,*,#18247,.T.);
#24823=ORIENTED_EDGE('',*,*,#18249,.T.);
#24824=ORIENTED_EDGE('',*,*,#18250,.F.);
#24825=ORIENTED_EDGE('',*,*,#18165,.T.);
#24826=ORIENTED_EDGE('',*,*,#18250,.T.);
#24827=ORIENTED_EDGE('',*,*,#18251,.F.);
#24828=ORIENTED_EDGE('',*,*,#18252,.F.);
#24829=ORIENTED_EDGE('',*,*,#18143,.T.);
#24830=ORIENTED_EDGE('',*,*,#18253,.T.);
#24831=ORIENTED_EDGE('',*,*,#18254,.F.);
#24832=ORIENTED_EDGE('',*,*,#18255,.F.);
#24833=ORIENTED_EDGE('',*,*,#18256,.F.);
#24834=ORIENTED_EDGE('',*,*,#18257,.F.);
#24835=ORIENTED_EDGE('',*,*,#18136,.T.);
#24836=ORIENTED_EDGE('',*,*,#18258,.T.);
#24837=ORIENTED_EDGE('',*,*,#18137,.T.);
#24838=ORIENTED_EDGE('',*,*,#18257,.T.);
#24839=ORIENTED_EDGE('',*,*,#18259,.T.);
#24840=ORIENTED_EDGE('',*,*,#18260,.F.);
#24841=ORIENTED_EDGE('',*,*,#18261,.T.);
#24842=ORIENTED_EDGE('',*,*,#18262,.F.);
#24843=ORIENTED_EDGE('',*,*,#18191,.T.);
#24844=ORIENTED_EDGE('',*,*,#18263,.T.);
#24845=ORIENTED_EDGE('',*,*,#18264,.F.);
#24846=ORIENTED_EDGE('',*,*,#18192,.F.);
#24847=ORIENTED_EDGE('',*,*,#18262,.T.);
#24848=ORIENTED_EDGE('',*,*,#18265,.T.);
#24849=ORIENTED_EDGE('',*,*,#18266,.F.);
#24850=ORIENTED_EDGE('',*,*,#18198,.F.);
#24851=ORIENTED_EDGE('',*,*,#18267,.T.);
#24852=ORIENTED_EDGE('',*,*,#18268,.T.);
#24853=ORIENTED_EDGE('',*,*,#18269,.T.);
#24854=ORIENTED_EDGE('',*,*,#18270,.T.);
#24855=ORIENTED_EDGE('',*,*,#18271,.F.);
#24856=ORIENTED_EDGE('',*,*,#18206,.F.);
#24857=ORIENTED_EDGE('',*,*,#18272,.F.);
#24858=ORIENTED_EDGE('',*,*,#18207,.T.);
#24859=ORIENTED_EDGE('',*,*,#18271,.T.);
#24860=ORIENTED_EDGE('',*,*,#18273,.F.);
#24861=ORIENTED_EDGE('',*,*,#18208,.F.);
#24862=ORIENTED_EDGE('',*,*,#18272,.T.);
#24863=ORIENTED_EDGE('',*,*,#18274,.T.);
#24864=ORIENTED_EDGE('',*,*,#18275,.T.);
#24865=ORIENTED_EDGE('',*,*,#18276,.F.);
#24866=ORIENTED_EDGE('',*,*,#18277,.T.);
#24867=ORIENTED_EDGE('',*,*,#18209,.T.);
#24868=ORIENTED_EDGE('',*,*,#18275,.F.);
#24869=ORIENTED_EDGE('',*,*,#18210,.T.);
#24870=ORIENTED_EDGE('',*,*,#18277,.F.);
#24871=ORIENTED_EDGE('',*,*,#18278,.F.);
#24872=ORIENTED_EDGE('',*,*,#18279,.F.);
#24873=ORIENTED_EDGE('',*,*,#18280,.F.);
#24874=ORIENTED_EDGE('',*,*,#18281,.T.);
#24875=ORIENTED_EDGE('',*,*,#18218,.F.);
#24876=ORIENTED_EDGE('',*,*,#18281,.F.);
#24877=ORIENTED_EDGE('',*,*,#18236,.F.);
#24878=ORIENTED_EDGE('',*,*,#18234,.F.);
#24879=ORIENTED_EDGE('',*,*,#18232,.T.);
#24880=ORIENTED_EDGE('',*,*,#18230,.T.);
#24881=ORIENTED_EDGE('',*,*,#18228,.F.);
#24882=ORIENTED_EDGE('',*,*,#18227,.T.);
#24883=ORIENTED_EDGE('',*,*,#18224,.F.);
#24884=ORIENTED_EDGE('',*,*,#18222,.F.);
#24885=ORIENTED_EDGE('',*,*,#18220,.F.);
#24886=ORIENTED_EDGE('',*,*,#18282,.T.);
#24887=ORIENTED_EDGE('',*,*,#17758,.F.);
#24888=ORIENTED_EDGE('',*,*,#18283,.F.);
#24889=ORIENTED_EDGE('',*,*,#18284,.F.);
#24890=ORIENTED_EDGE('',*,*,#18285,.T.);
#24891=ORIENTED_EDGE('',*,*,#18286,.T.);
#24892=ORIENTED_EDGE('',*,*,#18238,.F.);
#24893=ORIENTED_EDGE('',*,*,#18287,.T.);
#24894=ORIENTED_EDGE('',*,*,#18239,.T.);
#24895=ORIENTED_EDGE('',*,*,#18288,.F.);
#24896=ORIENTED_EDGE('',*,*,#18241,.T.);
#24897=ORIENTED_EDGE('',*,*,#18289,.T.);
#24898=ORIENTED_EDGE('',*,*,#18290,.T.);
#24899=ORIENTED_EDGE('',*,*,#18289,.F.);
#24900=ORIENTED_EDGE('',*,*,#18280,.T.);
#24901=ORIENTED_EDGE('',*,*,#18291,.T.);
#24902=ORIENTED_EDGE('',*,*,#18292,.T.);
#24903=ORIENTED_EDGE('',*,*,#18293,.T.);
#24904=ORIENTED_EDGE('',*,*,#17759,.F.);
#24905=ORIENTED_EDGE('',*,*,#18282,.F.);
#24906=ORIENTED_EDGE('',*,*,#18283,.T.);
#24907=ORIENTED_EDGE('',*,*,#17762,.T.);
#24908=ORIENTED_EDGE('',*,*,#18294,.F.);
#24909=ORIENTED_EDGE('',*,*,#18295,.F.);
#24910=ORIENTED_EDGE('',*,*,#18296,.F.);
#24911=ORIENTED_EDGE('',*,*,#18297,.F.);
#24912=ORIENTED_EDGE('',*,*,#18284,.T.);
#24913=ORIENTED_EDGE('',*,*,#18297,.T.);
#24914=ORIENTED_EDGE('',*,*,#18298,.F.);
#24915=ORIENTED_EDGE('',*,*,#18299,.F.);
#24916=ORIENTED_EDGE('',*,*,#18300,.F.);
#24917=ORIENTED_EDGE('',*,*,#18300,.T.);
#24918=ORIENTED_EDGE('',*,*,#18301,.T.);
#24919=ORIENTED_EDGE('',*,*,#18302,.T.);
#24920=ORIENTED_EDGE('',*,*,#18303,.F.);
#24921=ORIENTED_EDGE('',*,*,#18285,.F.);
#24922=ORIENTED_EDGE('',*,*,#18303,.T.);
#24923=ORIENTED_EDGE('',*,*,#18304,.T.);
#24924=ORIENTED_EDGE('',*,*,#18305,.T.);
#24925=ORIENTED_EDGE('',*,*,#18306,.T.);
#24926=ORIENTED_EDGE('',*,*,#18291,.F.);
#24927=ORIENTED_EDGE('',*,*,#18286,.F.);
#24928=ORIENTED_EDGE('',*,*,#18287,.F.);
#24929=ORIENTED_EDGE('',*,*,#18307,.T.);
#24930=ORIENTED_EDGE('',*,*,#18308,.F.);
#24931=ORIENTED_EDGE('',*,*,#18309,.F.);
#24932=ORIENTED_EDGE('',*,*,#18310,.F.);
#24933=ORIENTED_EDGE('',*,*,#18311,.F.);
#24934=ORIENTED_EDGE('',*,*,#18312,.F.);
#24935=ORIENTED_EDGE('',*,*,#18313,.F.);
#24936=ORIENTED_EDGE('',*,*,#18314,.F.);
#24937=ORIENTED_EDGE('',*,*,#18307,.F.);
#24938=ORIENTED_EDGE('',*,*,#18315,.T.);
#24939=ORIENTED_EDGE('',*,*,#18316,.T.);
#24940=ORIENTED_EDGE('',*,*,#18288,.T.);
#24941=ORIENTED_EDGE('',*,*,#18316,.F.);
#24942=ORIENTED_EDGE('',*,*,#18317,.T.);
#24943=ORIENTED_EDGE('',*,*,#18318,.T.);
#24944=ORIENTED_EDGE('',*,*,#18319,.T.);
#24945=ORIENTED_EDGE('',*,*,#18320,.T.);
#24946=ORIENTED_EDGE('',*,*,#18321,.T.);
#24947=ORIENTED_EDGE('',*,*,#18322,.T.);
#24948=ORIENTED_EDGE('',*,*,#18290,.F.);
#24949=ORIENTED_EDGE('',*,*,#18323,.F.);
#24950=ORIENTED_EDGE('',*,*,#18324,.F.);
#24951=ORIENTED_EDGE('',*,*,#18325,.T.);
#24952=ORIENTED_EDGE('',*,*,#18326,.F.);
#24953=ORIENTED_EDGE('',*,*,#18327,.F.);
#24954=ORIENTED_EDGE('',*,*,#18328,.T.);
#24955=ORIENTED_EDGE('',*,*,#18326,.T.);
#24956=ORIENTED_EDGE('',*,*,#18329,.F.);
#24957=ORIENTED_EDGE('',*,*,#18330,.F.);
#24958=ORIENTED_EDGE('',*,*,#18331,.T.);
#24959=ORIENTED_EDGE('',*,*,#18332,.T.);
#24960=ORIENTED_EDGE('',*,*,#18327,.T.);
#24961=ORIENTED_EDGE('',*,*,#18333,.T.);
#24962=ORIENTED_EDGE('',*,*,#18334,.F.);
#24963=ORIENTED_EDGE('',*,*,#18331,.F.);
#24964=ORIENTED_EDGE('',*,*,#18335,.T.);
#24965=ORIENTED_EDGE('',*,*,#18336,.T.);
#24966=ORIENTED_EDGE('',*,*,#18333,.F.);
#24967=ORIENTED_EDGE('',*,*,#18337,.F.);
#24968=ORIENTED_EDGE('',*,*,#18338,.F.);
#24969=ORIENTED_EDGE('',*,*,#18339,.F.);
#24970=ORIENTED_EDGE('',*,*,#18338,.T.);
#24971=ORIENTED_EDGE('',*,*,#18340,.T.);
#24972=ORIENTED_EDGE('',*,*,#18341,.F.);
#24973=ORIENTED_EDGE('',*,*,#18342,.T.);
#24974=ORIENTED_EDGE('',*,*,#18343,.F.);
#24975=ORIENTED_EDGE('',*,*,#18341,.T.);
#24976=ORIENTED_EDGE('',*,*,#18344,.T.);
#24977=ORIENTED_EDGE('',*,*,#18345,.T.);
#24978=ORIENTED_EDGE('',*,*,#18342,.F.);
#24979=ORIENTED_EDGE('',*,*,#18346,.F.);
#24980=ORIENTED_EDGE('',*,*,#18347,.T.);
#24981=ORIENTED_EDGE('',*,*,#18348,.T.);
#24982=ORIENTED_EDGE('',*,*,#18349,.F.);
#24983=ORIENTED_EDGE('',*,*,#18347,.F.);
#24984=ORIENTED_EDGE('',*,*,#18350,.T.);
#24985=ORIENTED_EDGE('',*,*,#18351,.T.);
#24986=ORIENTED_EDGE('',*,*,#18352,.T.);
#24987=ORIENTED_EDGE('',*,*,#18348,.F.);
#24988=ORIENTED_EDGE('',*,*,#18353,.T.);
#24989=ORIENTED_EDGE('',*,*,#18354,.T.);
#24990=ORIENTED_EDGE('',*,*,#18351,.F.);
#24991=ORIENTED_EDGE('',*,*,#18355,.F.);
#24992=ORIENTED_EDGE('',*,*,#18324,.T.);
#24993=ORIENTED_EDGE('',*,*,#17760,.T.);
#24994=ORIENTED_EDGE('',*,*,#18293,.F.);
#24995=ORIENTED_EDGE('',*,*,#18356,.F.);
#24996=ORIENTED_EDGE('',*,*,#18357,.T.);
#24997=ORIENTED_EDGE('',*,*,#18292,.F.);
#24998=ORIENTED_EDGE('',*,*,#18306,.F.);
#24999=ORIENTED_EDGE('',*,*,#18358,.F.);
#25000=ORIENTED_EDGE('',*,*,#18359,.F.);
#25001=ORIENTED_EDGE('',*,*,#18360,.T.);
#25002=ORIENTED_EDGE('',*,*,#18361,.T.);
#25003=ORIENTED_EDGE('',*,*,#18294,.T.);
#25004=ORIENTED_EDGE('',*,*,#17761,.T.);
#25005=ORIENTED_EDGE('',*,*,#18357,.F.);
#25006=ORIENTED_EDGE('',*,*,#18356,.T.);
#25007=ORIENTED_EDGE('',*,*,#18298,.T.);
#25008=ORIENTED_EDGE('',*,*,#18296,.T.);
#25009=ORIENTED_EDGE('',*,*,#18362,.T.);
#25010=ORIENTED_EDGE('',*,*,#18363,.T.);
#25011=ORIENTED_EDGE('',*,*,#18364,.T.);
#25012=ORIENTED_EDGE('',*,*,#18365,.F.);
#25013=ORIENTED_EDGE('',*,*,#18362,.F.);
#25014=ORIENTED_EDGE('',*,*,#18295,.T.);
#25015=ORIENTED_EDGE('',*,*,#18361,.F.);
#25016=ORIENTED_EDGE('',*,*,#18366,.F.);
#25017=ORIENTED_EDGE('',*,*,#18301,.F.);
#25018=ORIENTED_EDGE('',*,*,#18299,.T.);
#25019=ORIENTED_EDGE('',*,*,#18365,.T.);
#25020=ORIENTED_EDGE('',*,*,#18367,.F.);
#25021=ORIENTED_EDGE('',*,*,#18368,.F.);
#25022=ORIENTED_EDGE('',*,*,#18369,.T.);
#25023=ORIENTED_EDGE('',*,*,#18370,.F.);
#25024=ORIENTED_EDGE('',*,*,#18304,.F.);
#25025=ORIENTED_EDGE('',*,*,#18302,.F.);
#25026=ORIENTED_EDGE('',*,*,#18371,.F.);
#25027=ORIENTED_EDGE('',*,*,#18372,.T.);
#25028=ORIENTED_EDGE('',*,*,#18358,.T.);
#25029=ORIENTED_EDGE('',*,*,#18305,.F.);
#25030=ORIENTED_EDGE('',*,*,#18371,.T.);
#25031=ORIENTED_EDGE('',*,*,#18370,.T.);
#25032=ORIENTED_EDGE('',*,*,#18373,.F.);
#25033=ORIENTED_EDGE('',*,*,#18374,.F.);
#25034=ORIENTED_EDGE('',*,*,#18375,.F.);
#25035=ORIENTED_EDGE('',*,*,#18376,.T.);
#25036=ORIENTED_EDGE('',*,*,#18377,.F.);
#25037=ORIENTED_EDGE('',*,*,#18312,.T.);
#25038=ORIENTED_EDGE('',*,*,#18378,.T.);
#25039=ORIENTED_EDGE('',*,*,#18379,.F.);
#25040=ORIENTED_EDGE('',*,*,#18380,.T.);
#25041=ORIENTED_EDGE('',*,*,#18310,.T.);
#25042=ORIENTED_EDGE('',*,*,#18378,.F.);
#25043=ORIENTED_EDGE('',*,*,#18311,.T.);
#25044=ORIENTED_EDGE('',*,*,#18380,.F.);
#25045=ORIENTED_EDGE('',*,*,#18379,.T.);
#25046=ORIENTED_EDGE('',*,*,#18313,.T.);
#25047=ORIENTED_EDGE('',*,*,#18381,.F.);
#25048=ORIENTED_EDGE('',*,*,#18382,.F.);
#25049=ORIENTED_EDGE('',*,*,#18383,.F.);
#25050=ORIENTED_EDGE('',*,*,#18384,.T.);
#25051=ORIENTED_EDGE('',*,*,#18385,.F.);
#25052=ORIENTED_EDGE('',*,*,#18308,.T.);
#25053=ORIENTED_EDGE('',*,*,#18314,.T.);
#25054=ORIENTED_EDGE('',*,*,#18386,.F.);
#25055=ORIENTED_EDGE('',*,*,#18309,.T.);
#25056=ORIENTED_EDGE('',*,*,#18387,.F.);
#25057=ORIENTED_EDGE('',*,*,#18388,.T.);
#25058=ORIENTED_EDGE('',*,*,#18389,.F.);
#25059=ORIENTED_EDGE('',*,*,#18390,.T.);
#25060=ORIENTED_EDGE('',*,*,#18391,.F.);
#25061=ORIENTED_EDGE('',*,*,#18315,.F.);
#25062=ORIENTED_EDGE('',*,*,#18392,.T.);
#25063=ORIENTED_EDGE('',*,*,#18317,.F.);
#25064=ORIENTED_EDGE('',*,*,#18322,.F.);
#25065=ORIENTED_EDGE('',*,*,#18393,.T.);
#25066=ORIENTED_EDGE('',*,*,#18394,.F.);
#25067=ORIENTED_EDGE('',*,*,#18395,.T.);
#25068=ORIENTED_EDGE('',*,*,#18396,.F.);
#25069=ORIENTED_EDGE('',*,*,#18397,.T.);
#25070=ORIENTED_EDGE('',*,*,#18398,.T.);
#25071=ORIENTED_EDGE('',*,*,#18399,.F.);
#25072=ORIENTED_EDGE('',*,*,#18400,.T.);
#25073=ORIENTED_EDGE('',*,*,#18321,.F.);
#25074=ORIENTED_EDGE('',*,*,#18401,.F.);
#25075=ORIENTED_EDGE('',*,*,#18402,.T.);
#25076=ORIENTED_EDGE('',*,*,#18403,.F.);
#25077=ORIENTED_EDGE('',*,*,#18319,.F.);
#25078=ORIENTED_EDGE('',*,*,#18401,.T.);
#25079=ORIENTED_EDGE('',*,*,#18320,.F.);
#25080=ORIENTED_EDGE('',*,*,#18403,.T.);
#25081=ORIENTED_EDGE('',*,*,#18402,.F.);
#25082=ORIENTED_EDGE('',*,*,#18318,.F.);
#25083=ORIENTED_EDGE('',*,*,#18404,.T.);
#25084=ORIENTED_EDGE('',*,*,#18405,.F.);
#25085=ORIENTED_EDGE('',*,*,#18406,.T.);
#25086=ORIENTED_EDGE('',*,*,#18407,.T.);
#25087=ORIENTED_EDGE('',*,*,#18408,.T.);
#25088=ORIENTED_EDGE('',*,*,#18350,.F.);
#25089=ORIENTED_EDGE('',*,*,#18346,.T.);
#25090=ORIENTED_EDGE('',*,*,#18344,.F.);
#25091=ORIENTED_EDGE('',*,*,#18340,.F.);
#25092=ORIENTED_EDGE('',*,*,#18337,.T.);
#25093=ORIENTED_EDGE('',*,*,#18335,.F.);
#25094=ORIENTED_EDGE('',*,*,#18330,.T.);
#25095=ORIENTED_EDGE('',*,*,#18329,.T.);
#25096=ORIENTED_EDGE('',*,*,#18325,.F.);
#25097=ORIENTED_EDGE('',*,*,#18355,.T.);
#25098=ORIENTED_EDGE('',*,*,#18353,.F.);
#25099=ORIENTED_EDGE('',*,*,#18409,.T.);
#25100=ORIENTED_EDGE('',*,*,#18410,.T.);
#25101=ORIENTED_EDGE('',*,*,#18411,.T.);
#25102=ORIENTED_EDGE('',*,*,#18412,.T.);
#25103=ORIENTED_EDGE('',*,*,#18413,.T.);
#25104=ORIENTED_EDGE('',*,*,#18414,.F.);
#25105=ORIENTED_EDGE('',*,*,#18415,.F.);
#25106=ORIENTED_EDGE('',*,*,#18416,.T.);
#25107=ORIENTED_EDGE('',*,*,#18417,.F.);
#25108=ORIENTED_EDGE('',*,*,#18418,.T.);
#25109=ORIENTED_EDGE('',*,*,#18419,.F.);
#25110=ORIENTED_EDGE('',*,*,#18420,.F.);
#25111=ORIENTED_EDGE('',*,*,#18421,.T.);
#25112=ORIENTED_EDGE('',*,*,#18422,.F.);
#25113=ORIENTED_EDGE('',*,*,#18423,.F.);
#25114=ORIENTED_EDGE('',*,*,#18424,.T.);
#25115=ORIENTED_EDGE('',*,*,#18425,.T.);
#25116=ORIENTED_EDGE('',*,*,#18426,.T.);
#25117=ORIENTED_EDGE('',*,*,#18427,.F.);
#25118=ORIENTED_EDGE('',*,*,#18428,.F.);
#25119=ORIENTED_EDGE('',*,*,#18429,.F.);
#25120=ORIENTED_EDGE('',*,*,#18430,.F.);
#25121=ORIENTED_EDGE('',*,*,#18431,.F.);
#25122=ORIENTED_EDGE('',*,*,#18432,.T.);
#25123=ORIENTED_EDGE('',*,*,#18433,.F.);
#25124=ORIENTED_EDGE('',*,*,#18434,.T.);
#25125=ORIENTED_EDGE('',*,*,#18366,.T.);
#25126=ORIENTED_EDGE('',*,*,#18360,.F.);
#25127=ORIENTED_EDGE('',*,*,#18435,.F.);
#25128=ORIENTED_EDGE('',*,*,#18436,.F.);
#25129=ORIENTED_EDGE('',*,*,#18435,.T.);
#25130=ORIENTED_EDGE('',*,*,#18359,.T.);
#25131=ORIENTED_EDGE('',*,*,#18372,.F.);
#25132=ORIENTED_EDGE('',*,*,#18364,.F.);
#25133=ORIENTED_EDGE('',*,*,#18437,.F.);
#25134=ORIENTED_EDGE('',*,*,#18438,.T.);
#25135=ORIENTED_EDGE('',*,*,#18367,.T.);
#25136=ORIENTED_EDGE('',*,*,#18439,.T.);
#25137=ORIENTED_EDGE('',*,*,#18440,.F.);
#25138=ORIENTED_EDGE('',*,*,#18441,.F.);
#25139=ORIENTED_EDGE('',*,*,#18442,.T.);
#25140=ORIENTED_EDGE('',*,*,#18443,.T.);
#25141=ORIENTED_EDGE('',*,*,#18444,.F.);
#25142=ORIENTED_EDGE('',*,*,#18445,.F.);
#25143=ORIENTED_EDGE('',*,*,#18446,.T.);
#25144=ORIENTED_EDGE('',*,*,#18437,.T.);
#25145=ORIENTED_EDGE('',*,*,#18363,.F.);
#25146=ORIENTED_EDGE('',*,*,#18434,.F.);
#25147=ORIENTED_EDGE('',*,*,#18436,.T.);
#25148=ORIENTED_EDGE('',*,*,#18374,.T.);
#25149=ORIENTED_EDGE('',*,*,#18447,.F.);
#25150=ORIENTED_EDGE('',*,*,#18446,.F.);
#25151=ORIENTED_EDGE('',*,*,#18448,.T.);
#25152=ORIENTED_EDGE('',*,*,#18368,.T.);
#25153=ORIENTED_EDGE('',*,*,#18438,.F.);
#25154=ORIENTED_EDGE('',*,*,#18369,.F.);
#25155=ORIENTED_EDGE('',*,*,#18448,.F.);
#25156=ORIENTED_EDGE('',*,*,#18447,.T.);
#25157=ORIENTED_EDGE('',*,*,#18373,.T.);
#25158=ORIENTED_EDGE('',*,*,#18449,.F.);
#25159=ORIENTED_EDGE('',*,*,#18450,.F.);
#25160=ORIENTED_EDGE('',*,*,#18451,.T.);
#25161=ORIENTED_EDGE('',*,*,#18381,.T.);
#25162=ORIENTED_EDGE('',*,*,#18377,.T.);
#25163=ORIENTED_EDGE('',*,*,#18452,.T.);
#25164=ORIENTED_EDGE('',*,*,#18449,.T.);
#25165=ORIENTED_EDGE('',*,*,#18376,.F.);
#25166=ORIENTED_EDGE('',*,*,#18453,.F.);
#25167=ORIENTED_EDGE('',*,*,#18454,.F.);
#25168=ORIENTED_EDGE('',*,*,#18455,.F.);
#25169=ORIENTED_EDGE('',*,*,#18453,.T.);
#25170=ORIENTED_EDGE('',*,*,#18375,.T.);
#25171=ORIENTED_EDGE('',*,*,#18391,.T.);
#25172=ORIENTED_EDGE('',*,*,#18456,.T.);
#25173=ORIENTED_EDGE('',*,*,#18382,.T.);
#25174=ORIENTED_EDGE('',*,*,#18451,.F.);
#25175=ORIENTED_EDGE('',*,*,#18457,.F.);
#25176=ORIENTED_EDGE('',*,*,#18458,.T.);
#25177=ORIENTED_EDGE('',*,*,#18383,.T.);
#25178=ORIENTED_EDGE('',*,*,#18456,.F.);
#25179=ORIENTED_EDGE('',*,*,#18459,.F.);
#25180=ORIENTED_EDGE('',*,*,#18460,.T.);
#25181=ORIENTED_EDGE('',*,*,#18461,.T.);
#25182=ORIENTED_EDGE('',*,*,#18384,.F.);
#25183=ORIENTED_EDGE('',*,*,#18458,.F.);
#25184=ORIENTED_EDGE('',*,*,#18461,.F.);
#25185=ORIENTED_EDGE('',*,*,#18462,.F.);
#25186=ORIENTED_EDGE('',*,*,#18463,.T.);
#25187=ORIENTED_EDGE('',*,*,#18387,.T.);
#25188=ORIENTED_EDGE('',*,*,#18386,.T.);
#25189=ORIENTED_EDGE('',*,*,#18385,.T.);
#25190=ORIENTED_EDGE('',*,*,#18464,.T.);
#25191=ORIENTED_EDGE('',*,*,#18465,.T.);
#25192=ORIENTED_EDGE('',*,*,#18388,.F.);
#25193=ORIENTED_EDGE('',*,*,#18463,.F.);
#25194=ORIENTED_EDGE('',*,*,#18465,.F.);
#25195=ORIENTED_EDGE('',*,*,#18466,.F.);
#25196=ORIENTED_EDGE('',*,*,#18467,.T.);
#25197=ORIENTED_EDGE('',*,*,#18389,.T.);
#25198=ORIENTED_EDGE('',*,*,#18468,.T.);
#25199=ORIENTED_EDGE('',*,*,#18454,.T.);
#25200=ORIENTED_EDGE('',*,*,#18390,.F.);
#25201=ORIENTED_EDGE('',*,*,#18467,.F.);
#25202=ORIENTED_EDGE('',*,*,#18469,.T.);
#25203=ORIENTED_EDGE('',*,*,#18470,.T.);
#25204=ORIENTED_EDGE('',*,*,#18404,.F.);
#25205=ORIENTED_EDGE('',*,*,#18392,.F.);
#25206=ORIENTED_EDGE('',*,*,#18397,.F.);
#25207=ORIENTED_EDGE('',*,*,#18471,.F.);
#25208=ORIENTED_EDGE('',*,*,#18472,.T.);
#25209=ORIENTED_EDGE('',*,*,#18473,.T.);
#25210=ORIENTED_EDGE('',*,*,#18393,.F.);
#25211=ORIENTED_EDGE('',*,*,#18400,.F.);
#25212=ORIENTED_EDGE('',*,*,#18474,.F.);
#25213=ORIENTED_EDGE('',*,*,#18475,.F.);
#25214=ORIENTED_EDGE('',*,*,#18476,.T.);
#25215=ORIENTED_EDGE('',*,*,#18394,.T.);
#25216=ORIENTED_EDGE('',*,*,#18473,.F.);
#25217=ORIENTED_EDGE('',*,*,#18477,.T.);
#25218=ORIENTED_EDGE('',*,*,#18478,.T.);
#25219=ORIENTED_EDGE('',*,*,#18395,.F.);
#25220=ORIENTED_EDGE('',*,*,#18476,.F.);
#25221=ORIENTED_EDGE('',*,*,#18479,.F.);
#25222=ORIENTED_EDGE('',*,*,#18471,.T.);
#25223=ORIENTED_EDGE('',*,*,#18396,.T.);
#25224=ORIENTED_EDGE('',*,*,#18478,.F.);
#25225=ORIENTED_EDGE('',*,*,#18480,.F.);
#25226=ORIENTED_EDGE('',*,*,#18474,.T.);
#25227=ORIENTED_EDGE('',*,*,#18399,.T.);
#25228=ORIENTED_EDGE('',*,*,#18481,.F.);
#25229=ORIENTED_EDGE('',*,*,#18482,.T.);
#25230=ORIENTED_EDGE('',*,*,#18481,.T.);
#25231=ORIENTED_EDGE('',*,*,#18398,.F.);
#25232=ORIENTED_EDGE('',*,*,#18408,.F.);
#25233=ORIENTED_EDGE('',*,*,#18483,.F.);
#25234=ORIENTED_EDGE('',*,*,#18470,.F.);
#25235=ORIENTED_EDGE('',*,*,#18484,.F.);
#25236=ORIENTED_EDGE('',*,*,#18485,.T.);
#25237=ORIENTED_EDGE('',*,*,#18405,.T.);
#25238=ORIENTED_EDGE('',*,*,#18406,.F.);
#25239=ORIENTED_EDGE('',*,*,#18485,.F.);
#25240=ORIENTED_EDGE('',*,*,#18486,.T.);
#25241=ORIENTED_EDGE('',*,*,#18487,.T.);
#25242=ORIENTED_EDGE('',*,*,#18407,.F.);
#25243=ORIENTED_EDGE('',*,*,#18487,.F.);
#25244=ORIENTED_EDGE('',*,*,#18488,.T.);
#25245=ORIENTED_EDGE('',*,*,#18483,.T.);
#25246=ORIENTED_EDGE('',*,*,#18409,.F.);
#25247=ORIENTED_EDGE('',*,*,#18489,.T.);
#25248=ORIENTED_EDGE('',*,*,#18490,.T.);
#25249=ORIENTED_EDGE('',*,*,#18491,.F.);
#25250=ORIENTED_EDGE('',*,*,#18410,.F.);
#25251=ORIENTED_EDGE('',*,*,#18491,.T.);
#25252=ORIENTED_EDGE('',*,*,#18492,.T.);
#25253=ORIENTED_EDGE('',*,*,#18493,.F.);
#25254=ORIENTED_EDGE('',*,*,#18411,.F.);
#25255=ORIENTED_EDGE('',*,*,#18493,.T.);
#25256=ORIENTED_EDGE('',*,*,#18494,.T.);
#25257=ORIENTED_EDGE('',*,*,#18495,.T.);
#25258=ORIENTED_EDGE('',*,*,#18496,.T.);
#25259=ORIENTED_EDGE('',*,*,#18412,.F.);
#25260=ORIENTED_EDGE('',*,*,#18495,.F.);
#25261=ORIENTED_EDGE('',*,*,#18497,.T.);
#25262=ORIENTED_EDGE('',*,*,#18413,.F.);
#25263=ORIENTED_EDGE('',*,*,#18496,.F.);
#25264=ORIENTED_EDGE('',*,*,#18498,.T.);
#25265=ORIENTED_EDGE('',*,*,#18499,.F.);
#25266=ORIENTED_EDGE('',*,*,#18500,.T.);
#25267=ORIENTED_EDGE('',*,*,#18414,.T.);
#25268=ORIENTED_EDGE('',*,*,#18499,.T.);
#25269=ORIENTED_EDGE('',*,*,#18501,.F.);
#25270=ORIENTED_EDGE('',*,*,#18415,.T.);
#25271=ORIENTED_EDGE('',*,*,#18500,.F.);
#25272=ORIENTED_EDGE('',*,*,#18502,.F.);
#25273=ORIENTED_EDGE('',*,*,#18503,.T.);
#25274=ORIENTED_EDGE('',*,*,#18416,.F.);
#25275=ORIENTED_EDGE('',*,*,#18503,.F.);
#25276=ORIENTED_EDGE('',*,*,#18504,.T.);
#25277=ORIENTED_EDGE('',*,*,#18505,.F.);
#25278=ORIENTED_EDGE('',*,*,#18505,.T.);
#25279=ORIENTED_EDGE('',*,*,#18506,.F.);
#25280=ORIENTED_EDGE('',*,*,#18489,.F.);
#25281=ORIENTED_EDGE('',*,*,#18417,.T.);
#25282=ORIENTED_EDGE('',*,*,#18440,.T.);
#25283=ORIENTED_EDGE('',*,*,#18507,.F.);
#25284=ORIENTED_EDGE('',*,*,#18418,.F.);
#25285=ORIENTED_EDGE('',*,*,#18508,.T.);
#25286=ORIENTED_EDGE('',*,*,#18507,.T.);
#25287=ORIENTED_EDGE('',*,*,#18439,.F.);
#25288=ORIENTED_EDGE('',*,*,#18509,.F.);
#25289=ORIENTED_EDGE('',*,*,#18419,.T.);
#25290=ORIENTED_EDGE('',*,*,#18509,.T.);
#25291=ORIENTED_EDGE('',*,*,#18445,.T.);
#25292=ORIENTED_EDGE('',*,*,#18510,.F.);
#25293=ORIENTED_EDGE('',*,*,#18420,.T.);
#25294=ORIENTED_EDGE('',*,*,#18421,.F.);
#25295=ORIENTED_EDGE('',*,*,#18510,.T.);
#25296=ORIENTED_EDGE('',*,*,#18444,.T.);
#25297=ORIENTED_EDGE('',*,*,#18511,.F.);
#25298=ORIENTED_EDGE('',*,*,#18512,.F.);
#25299=ORIENTED_EDGE('',*,*,#18422,.T.);
#25300=ORIENTED_EDGE('',*,*,#18511,.T.);
#25301=ORIENTED_EDGE('',*,*,#18443,.F.);
#25302=ORIENTED_EDGE('',*,*,#18513,.F.);
#25303=ORIENTED_EDGE('',*,*,#18423,.T.);
#25304=ORIENTED_EDGE('',*,*,#18512,.T.);
#25305=ORIENTED_EDGE('',*,*,#18442,.F.);
#25306=ORIENTED_EDGE('',*,*,#18508,.F.);
#25307=ORIENTED_EDGE('',*,*,#18424,.F.);
#25308=ORIENTED_EDGE('',*,*,#18513,.T.);
#25309=ORIENTED_EDGE('',*,*,#18441,.T.);
#25310=ORIENTED_EDGE('',*,*,#18514,.F.);
#25311=ORIENTED_EDGE('',*,*,#18515,.F.);
#25312=ORIENTED_EDGE('',*,*,#18425,.F.);
#25313=ORIENTED_EDGE('',*,*,#18516,.T.);
#25314=ORIENTED_EDGE('',*,*,#18515,.T.);
#25315=ORIENTED_EDGE('',*,*,#18517,.T.);
#25316=ORIENTED_EDGE('',*,*,#18518,.F.);
#25317=ORIENTED_EDGE('',*,*,#18426,.F.);
#25318=ORIENTED_EDGE('',*,*,#18518,.T.);
#25319=ORIENTED_EDGE('',*,*,#18519,.F.);
#25320=ORIENTED_EDGE('',*,*,#18520,.F.);
#25321=ORIENTED_EDGE('',*,*,#18427,.T.);
#25322=ORIENTED_EDGE('',*,*,#18520,.T.);
#25323=ORIENTED_EDGE('',*,*,#18521,.T.);
#25324=ORIENTED_EDGE('',*,*,#18522,.F.);
#25325=ORIENTED_EDGE('',*,*,#18428,.T.);
#25326=ORIENTED_EDGE('',*,*,#18523,.F.);
#25327=ORIENTED_EDGE('',*,*,#18524,.F.);
#25328=ORIENTED_EDGE('',*,*,#18429,.T.);
#25329=ORIENTED_EDGE('',*,*,#18522,.T.);
#25330=ORIENTED_EDGE('',*,*,#18524,.T.);
#25331=ORIENTED_EDGE('',*,*,#18525,.F.);
#25332=ORIENTED_EDGE('',*,*,#18526,.F.);
#25333=ORIENTED_EDGE('',*,*,#18430,.T.);
#25334=ORIENTED_EDGE('',*,*,#18526,.T.);
#25335=ORIENTED_EDGE('',*,*,#18527,.F.);
#25336=ORIENTED_EDGE('',*,*,#18528,.F.);
#25337=ORIENTED_EDGE('',*,*,#18431,.T.);
#25338=ORIENTED_EDGE('',*,*,#18432,.F.);
#25339=ORIENTED_EDGE('',*,*,#18528,.T.);
#25340=ORIENTED_EDGE('',*,*,#18529,.T.);
#25341=ORIENTED_EDGE('',*,*,#18530,.F.);
#25342=ORIENTED_EDGE('',*,*,#18530,.T.);
#25343=ORIENTED_EDGE('',*,*,#18531,.F.);
#25344=ORIENTED_EDGE('',*,*,#18516,.F.);
#25345=ORIENTED_EDGE('',*,*,#18433,.T.);
#25346=ORIENTED_EDGE('',*,*,#18494,.F.);
#25347=ORIENTED_EDGE('',*,*,#18492,.F.);
#25348=ORIENTED_EDGE('',*,*,#18490,.F.);
#25349=ORIENTED_EDGE('',*,*,#18506,.T.);
#25350=ORIENTED_EDGE('',*,*,#18504,.F.);
#25351=ORIENTED_EDGE('',*,*,#18502,.T.);
#25352=ORIENTED_EDGE('',*,*,#18501,.T.);
#25353=ORIENTED_EDGE('',*,*,#18498,.F.);
#25354=ORIENTED_EDGE('',*,*,#18497,.F.);
#25355=ORIENTED_EDGE('',*,*,#18457,.T.);
#25356=ORIENTED_EDGE('',*,*,#18450,.T.);
#25357=ORIENTED_EDGE('',*,*,#18452,.F.);
#25358=ORIENTED_EDGE('',*,*,#18455,.T.);
#25359=ORIENTED_EDGE('',*,*,#18468,.F.);
#25360=ORIENTED_EDGE('',*,*,#18466,.T.);
#25361=ORIENTED_EDGE('',*,*,#18464,.F.);
#25362=ORIENTED_EDGE('',*,*,#18462,.T.);
#25363=ORIENTED_EDGE('',*,*,#18460,.F.);
#25364=ORIENTED_EDGE('',*,*,#18459,.T.);
#25365=ORIENTED_EDGE('',*,*,#18519,.T.);
#25366=ORIENTED_EDGE('',*,*,#18517,.F.);
#25367=ORIENTED_EDGE('',*,*,#18514,.T.);
#25368=ORIENTED_EDGE('',*,*,#18531,.T.);
#25369=ORIENTED_EDGE('',*,*,#18529,.F.);
#25370=ORIENTED_EDGE('',*,*,#18527,.T.);
#25371=ORIENTED_EDGE('',*,*,#18525,.T.);
#25372=ORIENTED_EDGE('',*,*,#18523,.T.);
#25373=ORIENTED_EDGE('',*,*,#18521,.F.);
#25374=ORIENTED_EDGE('',*,*,#18486,.F.);
#25375=ORIENTED_EDGE('',*,*,#18484,.T.);
#25376=ORIENTED_EDGE('',*,*,#18469,.F.);
#25377=ORIENTED_EDGE('',*,*,#18479,.T.);
#25378=ORIENTED_EDGE('',*,*,#18477,.F.);
#25379=ORIENTED_EDGE('',*,*,#18475,.T.);
#25380=ORIENTED_EDGE('',*,*,#18472,.F.);
#25381=ORIENTED_EDGE('',*,*,#18480,.T.);
#25382=ORIENTED_EDGE('',*,*,#18482,.F.);
#25383=ORIENTED_EDGE('',*,*,#18488,.F.);
#25384=ORIENTED_EDGE('',*,*,#18211,.T.);
#25385=ORIENTED_EDGE('',*,*,#18279,.T.);
#25386=ORIENTED_EDGE('',*,*,#18532,.T.);
#25387=ORIENTED_EDGE('',*,*,#18123,.F.);
#25388=ORIENTED_EDGE('',*,*,#18119,.T.);
#25389=ORIENTED_EDGE('',*,*,#18533,.F.);
#25390=ORIENTED_EDGE('',*,*,#18244,.F.);
#25391=ORIENTED_EDGE('',*,*,#18160,.F.);
#25392=ORIENTED_EDGE('',*,*,#18190,.T.);
#25393=ORIENTED_EDGE('',*,*,#18176,.T.);
#25394=ORIENTED_EDGE('',*,*,#18534,.T.);
#25395=ORIENTED_EDGE('',*,*,#18263,.F.);
#25396=ORIENTED_EDGE('',*,*,#18260,.T.);
#25397=ORIENTED_EDGE('',*,*,#18535,.F.);
#25398=ORIENTED_EDGE('',*,*,#18172,.F.);
#25399=ORIENTED_EDGE('',*,*,#18138,.F.);
#25400=ORIENTED_EDGE('',*,*,#18253,.F.);
#25401=ORIENTED_EDGE('',*,*,#18142,.F.);
#25402=ORIENTED_EDGE('',*,*,#18536,.F.);
#25403=ORIENTED_EDGE('',*,*,#18537,.T.);
#25404=ORIENTED_EDGE('',*,*,#18538,.F.);
#25405=ORIENTED_EDGE('',*,*,#18539,.T.);
#25406=ORIENTED_EDGE('',*,*,#18540,.F.);
#25407=ORIENTED_EDGE('',*,*,#18541,.T.);
#25408=ORIENTED_EDGE('',*,*,#18542,.T.);
#25409=ORIENTED_EDGE('',*,*,#18543,.F.);
#25410=ORIENTED_EDGE('',*,*,#18544,.F.);
#25411=ORIENTED_EDGE('',*,*,#18166,.F.);
#25412=ORIENTED_EDGE('',*,*,#18146,.T.);
#25413=ORIENTED_EDGE('',*,*,#18252,.T.);
#25414=ORIENTED_EDGE('',*,*,#18258,.F.);
#25415=ORIENTED_EDGE('',*,*,#18135,.F.);
#25416=ORIENTED_EDGE('',*,*,#18171,.T.);
#25417=ORIENTED_EDGE('',*,*,#18545,.T.);
#25418=ORIENTED_EDGE('',*,*,#18546,.T.);
#25419=ORIENTED_EDGE('',*,*,#18547,.T.);
#25420=ORIENTED_EDGE('',*,*,#18548,.F.);
#25421=ORIENTED_EDGE('',*,*,#18549,.T.);
#25422=ORIENTED_EDGE('',*,*,#18550,.F.);
#25423=ORIENTED_EDGE('',*,*,#18551,.T.);
#25424=ORIENTED_EDGE('',*,*,#18552,.T.);
#25425=ORIENTED_EDGE('',*,*,#18553,.T.);
#25426=ORIENTED_EDGE('',*,*,#18144,.T.);
#25427=ORIENTED_EDGE('',*,*,#18255,.T.);
#25428=ORIENTED_EDGE('',*,*,#18267,.F.);
#25429=ORIENTED_EDGE('',*,*,#18197,.F.);
#25430=ORIENTED_EDGE('',*,*,#18554,.F.);
#25431=ORIENTED_EDGE('',*,*,#18555,.F.);
#25432=ORIENTED_EDGE('',*,*,#18556,.F.);
#25433=ORIENTED_EDGE('',*,*,#18557,.T.);
#25434=ORIENTED_EDGE('',*,*,#18558,.F.);
#25435=ORIENTED_EDGE('',*,*,#18559,.T.);
#25436=ORIENTED_EDGE('',*,*,#18560,.F.);
#25437=ORIENTED_EDGE('',*,*,#18561,.F.);
#25438=ORIENTED_EDGE('',*,*,#18562,.F.);
#25439=ORIENTED_EDGE('',*,*,#18174,.F.);
#25440=ORIENTED_EDGE('',*,*,#18193,.T.);
#25441=ORIENTED_EDGE('',*,*,#18264,.T.);
#25442=ORIENTED_EDGE('',*,*,#18269,.F.);
#25443=ORIENTED_EDGE('',*,*,#18205,.F.);
#25444=ORIENTED_EDGE('',*,*,#18182,.T.);
#25445=ORIENTED_EDGE('',*,*,#18563,.T.);
#25446=ORIENTED_EDGE('',*,*,#18564,.T.);
#25447=ORIENTED_EDGE('',*,*,#18565,.F.);
#25448=ORIENTED_EDGE('',*,*,#18566,.F.);
#25449=ORIENTED_EDGE('',*,*,#18567,.T.);
#25450=ORIENTED_EDGE('',*,*,#18568,.F.);
#25451=ORIENTED_EDGE('',*,*,#18569,.T.);
#25452=ORIENTED_EDGE('',*,*,#18570,.F.);
#25453=ORIENTED_EDGE('',*,*,#18571,.T.);
#25454=ORIENTED_EDGE('',*,*,#18194,.T.);
#25455=ORIENTED_EDGE('',*,*,#18266,.T.);
#25456=ORIENTED_EDGE('',*,*,#18184,.F.);
#25457=ORIENTED_EDGE('',*,*,#18050,.F.);
#25458=ORIENTED_EDGE('',*,*,#17884,.F.);
#25459=ORIENTED_EDGE('',*,*,#18572,.F.);
#25460=ORIENTED_EDGE('',*,*,#18563,.F.);
#25461=ORIENTED_EDGE('',*,*,#17888,.F.);
#25462=ORIENTED_EDGE('',*,*,#18064,.T.);
#25463=ORIENTED_EDGE('',*,*,#18130,.F.);
#25464=ORIENTED_EDGE('',*,*,#18573,.T.);
#25465=ORIENTED_EDGE('',*,*,#18574,.F.);
#25466=ORIENTED_EDGE('',*,*,#18568,.T.);
#25467=ORIENTED_EDGE('',*,*,#18268,.F.);
#25468=ORIENTED_EDGE('',*,*,#18557,.F.);
#25469=ORIENTED_EDGE('',*,*,#18575,.F.);
#25470=ORIENTED_EDGE('',*,*,#18576,.T.);
#25471=ORIENTED_EDGE('',*,*,#18577,.F.);
#25472=ORIENTED_EDGE('',*,*,#18558,.T.);
#25473=ORIENTED_EDGE('',*,*,#18265,.F.);
#25474=ORIENTED_EDGE('',*,*,#18261,.F.);
#25475=ORIENTED_EDGE('',*,*,#18534,.F.);
#25476=ORIENTED_EDGE('',*,*,#18175,.F.);
#25477=ORIENTED_EDGE('',*,*,#18562,.T.);
#25478=ORIENTED_EDGE('',*,*,#18578,.F.);
#25479=ORIENTED_EDGE('',*,*,#17898,.F.);
#25480=ORIENTED_EDGE('',*,*,#18185,.F.);
#25481=ORIENTED_EDGE('',*,*,#17853,.F.);
#25482=ORIENTED_EDGE('',*,*,#18579,.F.);
#25483=ORIENTED_EDGE('',*,*,#18545,.F.);
#25484=ORIENTED_EDGE('',*,*,#18173,.F.);
#25485=ORIENTED_EDGE('',*,*,#18535,.T.);
#25486=ORIENTED_EDGE('',*,*,#18259,.F.);
#25487=ORIENTED_EDGE('',*,*,#18256,.T.);
#25488=ORIENTED_EDGE('',*,*,#18549,.F.);
#25489=ORIENTED_EDGE('',*,*,#18580,.F.);
#25490=ORIENTED_EDGE('',*,*,#18581,.F.);
#25491=ORIENTED_EDGE('',*,*,#18582,.F.);
#25492=ORIENTED_EDGE('',*,*,#18550,.T.);
#25493=ORIENTED_EDGE('',*,*,#18254,.T.);
#25494=ORIENTED_EDGE('',*,*,#18539,.F.);
#25495=ORIENTED_EDGE('',*,*,#18583,.F.);
#25496=ORIENTED_EDGE('',*,*,#18584,.F.);
#25497=ORIENTED_EDGE('',*,*,#18585,.F.);
#25498=ORIENTED_EDGE('',*,*,#18540,.T.);
#25499=ORIENTED_EDGE('',*,*,#18251,.T.);
#25500=ORIENTED_EDGE('',*,*,#18249,.F.);
#25501=ORIENTED_EDGE('',*,*,#18248,.T.);
#25502=ORIENTED_EDGE('',*,*,#18245,.T.);
#25503=ORIENTED_EDGE('',*,*,#18242,.F.);
#25504=ORIENTED_EDGE('',*,*,#18533,.T.);
#25505=ORIENTED_EDGE('',*,*,#18118,.F.);
#25506=ORIENTED_EDGE('',*,*,#18586,.T.);
#25507=ORIENTED_EDGE('',*,*,#18587,.F.);
#25508=ORIENTED_EDGE('',*,*,#17860,.F.);
#25509=ORIENTED_EDGE('',*,*,#18109,.F.);
#25510=ORIENTED_EDGE('',*,*,#17892,.F.);
#25511=ORIENTED_EDGE('',*,*,#18588,.F.);
#25512=ORIENTED_EDGE('',*,*,#18589,.F.);
#25513=ORIENTED_EDGE('',*,*,#18124,.F.);
#25514=ORIENTED_EDGE('',*,*,#18532,.F.);
#25515=ORIENTED_EDGE('',*,*,#18278,.T.);
#25516=ORIENTED_EDGE('',*,*,#18276,.T.);
#25517=ORIENTED_EDGE('',*,*,#18274,.F.);
#25518=ORIENTED_EDGE('',*,*,#18273,.T.);
#25519=ORIENTED_EDGE('',*,*,#18270,.F.);
#25520=ORIENTED_EDGE('',*,*,#18567,.F.);
#25521=ORIENTED_EDGE('',*,*,#18590,.F.);
#25522=ORIENTED_EDGE('',*,*,#18591,.T.);
#25523=ORIENTED_EDGE('',*,*,#18592,.F.);
#25524=ORIENTED_EDGE('',*,*,#18328,.F.);
#25525=ORIENTED_EDGE('',*,*,#18332,.F.);
#25526=ORIENTED_EDGE('',*,*,#18334,.T.);
#25527=ORIENTED_EDGE('',*,*,#18336,.F.);
#25528=ORIENTED_EDGE('',*,*,#18339,.T.);
#25529=ORIENTED_EDGE('',*,*,#18343,.T.);
#25530=ORIENTED_EDGE('',*,*,#18345,.F.);
#25531=ORIENTED_EDGE('',*,*,#18349,.T.);
#25532=ORIENTED_EDGE('',*,*,#18352,.F.);
#25533=ORIENTED_EDGE('',*,*,#18354,.F.);
#25534=ORIENTED_EDGE('',*,*,#18323,.T.);
#25535=ORIENTED_EDGE('',*,*,#17849,.F.);
#25536=ORIENTED_EDGE('',*,*,#18037,.F.);
#25537=ORIENTED_EDGE('',*,*,#18167,.F.);
#25538=ORIENTED_EDGE('',*,*,#18544,.T.);
#25539=ORIENTED_EDGE('',*,*,#18593,.F.);
#25540=ORIENTED_EDGE('',*,*,#18112,.F.);
#25541=ORIENTED_EDGE('',*,*,#18030,.T.);
#25542=ORIENTED_EDGE('',*,*,#17845,.F.);
#25543=ORIENTED_EDGE('',*,*,#18594,.F.);
#25544=ORIENTED_EDGE('',*,*,#18595,.F.);
#25545=ORIENTED_EDGE('',*,*,#18596,.T.);
#25546=ORIENTED_EDGE('',*,*,#18565,.T.);
#25547=ORIENTED_EDGE('',*,*,#18597,.F.);
#25548=ORIENTED_EDGE('',*,*,#18598,.F.);
#25549=ORIENTED_EDGE('',*,*,#17883,.T.);
#25550=ORIENTED_EDGE('',*,*,#18599,.F.);
#25551=ORIENTED_EDGE('',*,*,#18564,.F.);
#25552=ORIENTED_EDGE('',*,*,#18572,.T.);
#25553=ORIENTED_EDGE('',*,*,#18597,.T.);
#25554=ORIENTED_EDGE('',*,*,#18599,.T.);
#25555=ORIENTED_EDGE('',*,*,#18600,.F.);
#25556=ORIENTED_EDGE('',*,*,#18566,.T.);
#25557=ORIENTED_EDGE('',*,*,#18601,.F.);
#25558=ORIENTED_EDGE('',*,*,#18602,.F.);
#25559=ORIENTED_EDGE('',*,*,#18590,.T.);
#25560=ORIENTED_EDGE('',*,*,#18603,.T.);
#25561=ORIENTED_EDGE('',*,*,#18601,.T.);
#25562=ORIENTED_EDGE('',*,*,#18596,.F.);
#25563=ORIENTED_EDGE('',*,*,#18600,.T.);
#25564=ORIENTED_EDGE('',*,*,#17882,.T.);
#25565=ORIENTED_EDGE('',*,*,#18604,.F.);
#25566=ORIENTED_EDGE('',*,*,#18605,.F.);
#25567=ORIENTED_EDGE('',*,*,#18561,.T.);
#25568=ORIENTED_EDGE('',*,*,#18606,.F.);
#25569=ORIENTED_EDGE('',*,*,#17881,.F.);
#25570=ORIENTED_EDGE('',*,*,#18578,.T.);
#25571=ORIENTED_EDGE('',*,*,#18604,.T.);
#25572=ORIENTED_EDGE('',*,*,#18606,.T.);
#25573=ORIENTED_EDGE('',*,*,#18607,.F.);
#25574=ORIENTED_EDGE('',*,*,#18605,.T.);
#25575=ORIENTED_EDGE('',*,*,#18608,.T.);
#25576=ORIENTED_EDGE('',*,*,#18609,.T.);
#25577=ORIENTED_EDGE('',*,*,#18610,.T.);
#25578=ORIENTED_EDGE('',*,*,#18611,.T.);
#25579=ORIENTED_EDGE('',*,*,#18612,.T.);
#25580=ORIENTED_EDGE('',*,*,#18613,.T.);
#25581=ORIENTED_EDGE('',*,*,#18614,.T.);
#25582=ORIENTED_EDGE('',*,*,#18615,.T.);
#25583=ORIENTED_EDGE('',*,*,#18598,.T.);
#25584=ORIENTED_EDGE('',*,*,#18616,.T.);
#25585=ORIENTED_EDGE('',*,*,#18617,.T.);
#25586=ORIENTED_EDGE('',*,*,#18603,.F.);
#25587=ORIENTED_EDGE('',*,*,#18615,.F.);
#25588=ORIENTED_EDGE('',*,*,#18618,.T.);
#25589=ORIENTED_EDGE('',*,*,#18619,.T.);
#25590=ORIENTED_EDGE('',*,*,#18616,.F.);
#25591=ORIENTED_EDGE('',*,*,#18607,.T.);
#25592=ORIENTED_EDGE('',*,*,#18560,.T.);
#25593=ORIENTED_EDGE('',*,*,#18620,.F.);
#25594=ORIENTED_EDGE('',*,*,#18608,.F.);
#25595=ORIENTED_EDGE('',*,*,#18620,.T.);
#25596=ORIENTED_EDGE('',*,*,#18621,.T.);
#25597=ORIENTED_EDGE('',*,*,#18622,.F.);
#25598=ORIENTED_EDGE('',*,*,#18622,.T.);
#25599=ORIENTED_EDGE('',*,*,#18623,.T.);
#25600=ORIENTED_EDGE('',*,*,#18624,.F.);
#25601=ORIENTED_EDGE('',*,*,#18609,.F.);
#25602=ORIENTED_EDGE('',*,*,#18624,.T.);
#25603=ORIENTED_EDGE('',*,*,#18625,.T.);
#25604=ORIENTED_EDGE('',*,*,#18626,.F.);
#25605=ORIENTED_EDGE('',*,*,#18626,.T.);
#25606=ORIENTED_EDGE('',*,*,#18555,.T.);
#25607=ORIENTED_EDGE('',*,*,#18627,.F.);
#25608=ORIENTED_EDGE('',*,*,#18610,.F.);
#25609=ORIENTED_EDGE('',*,*,#18627,.T.);
#25610=ORIENTED_EDGE('',*,*,#18628,.T.);
#25611=ORIENTED_EDGE('',*,*,#18629,.F.);
#25612=ORIENTED_EDGE('',*,*,#18611,.F.);
#25613=ORIENTED_EDGE('',*,*,#18629,.T.);
#25614=ORIENTED_EDGE('',*,*,#18180,.T.);
#25615=ORIENTED_EDGE('',*,*,#18630,.F.);
#25616=ORIENTED_EDGE('',*,*,#18612,.F.);
#25617=ORIENTED_EDGE('',*,*,#18630,.T.);
#25618=ORIENTED_EDGE('',*,*,#18631,.T.);
#25619=ORIENTED_EDGE('',*,*,#18632,.F.);
#25620=ORIENTED_EDGE('',*,*,#18613,.F.);
#25621=ORIENTED_EDGE('',*,*,#18632,.T.);
#25622=ORIENTED_EDGE('',*,*,#18570,.T.);
#25623=ORIENTED_EDGE('',*,*,#18618,.F.);
#25624=ORIENTED_EDGE('',*,*,#18614,.F.);
#25625=ORIENTED_EDGE('',*,*,#18591,.F.);
#25626=ORIENTED_EDGE('',*,*,#18602,.T.);
#25627=ORIENTED_EDGE('',*,*,#18617,.F.);
#25628=ORIENTED_EDGE('',*,*,#18633,.F.);
#25629=ORIENTED_EDGE('',*,*,#18633,.T.);
#25630=ORIENTED_EDGE('',*,*,#18619,.F.);
#25631=ORIENTED_EDGE('',*,*,#18569,.F.);
#25632=ORIENTED_EDGE('',*,*,#18592,.T.);
#25633=ORIENTED_EDGE('',*,*,#18634,.T.);
#25634=ORIENTED_EDGE('',*,*,#18621,.F.);
#25635=ORIENTED_EDGE('',*,*,#18559,.F.);
#25636=ORIENTED_EDGE('',*,*,#18577,.T.);
#25637=ORIENTED_EDGE('',*,*,#18576,.F.);
#25638=ORIENTED_EDGE('',*,*,#18635,.T.);
#25639=ORIENTED_EDGE('',*,*,#18623,.F.);
#25640=ORIENTED_EDGE('',*,*,#18634,.F.);
#25641=ORIENTED_EDGE('',*,*,#18556,.T.);
#25642=ORIENTED_EDGE('',*,*,#18625,.F.);
#25643=ORIENTED_EDGE('',*,*,#18635,.F.);
#25644=ORIENTED_EDGE('',*,*,#18575,.T.);
#25645=ORIENTED_EDGE('',*,*,#18628,.F.);
#25646=ORIENTED_EDGE('',*,*,#18554,.T.);
#25647=ORIENTED_EDGE('',*,*,#18196,.F.);
#25648=ORIENTED_EDGE('',*,*,#18181,.F.);
#25649=ORIENTED_EDGE('',*,*,#18631,.F.);
#25650=ORIENTED_EDGE('',*,*,#18179,.T.);
#25651=ORIENTED_EDGE('',*,*,#18195,.F.);
#25652=ORIENTED_EDGE('',*,*,#18571,.F.);
#25653=ORIENTED_EDGE('',*,*,#18636,.T.);
#25654=ORIENTED_EDGE('',*,*,#18637,.F.);
#25655=ORIENTED_EDGE('',*,*,#18638,.F.);
#25656=ORIENTED_EDGE('',*,*,#18212,.T.);
#25657=ORIENTED_EDGE('',*,*,#18121,.T.);
#25658=ORIENTED_EDGE('',*,*,#18589,.T.);
#25659=ORIENTED_EDGE('',*,*,#18639,.T.);
#25660=ORIENTED_EDGE('',*,*,#18637,.T.);
#25661=ORIENTED_EDGE('',*,*,#18640,.F.);
#25662=ORIENTED_EDGE('',*,*,#18641,.F.);
#25663=ORIENTED_EDGE('',*,*,#17891,.T.);
#25664=ORIENTED_EDGE('',*,*,#18642,.F.);
#25665=ORIENTED_EDGE('',*,*,#18636,.F.);
#25666=ORIENTED_EDGE('',*,*,#18588,.T.);
#25667=ORIENTED_EDGE('',*,*,#18640,.T.);
#25668=ORIENTED_EDGE('',*,*,#18642,.T.);
#25669=ORIENTED_EDGE('',*,*,#18643,.F.);
#25670=ORIENTED_EDGE('',*,*,#18644,.F.);
#25671=ORIENTED_EDGE('',*,*,#18213,.T.);
#25672=ORIENTED_EDGE('',*,*,#18638,.T.);
#25673=ORIENTED_EDGE('',*,*,#18645,.F.);
#25674=ORIENTED_EDGE('',*,*,#18646,.T.);
#25675=ORIENTED_EDGE('',*,*,#18645,.T.);
#25676=ORIENTED_EDGE('',*,*,#18639,.F.);
#25677=ORIENTED_EDGE('',*,*,#18643,.T.);
#25678=ORIENTED_EDGE('',*,*,#17890,.T.);
#25679=ORIENTED_EDGE('',*,*,#18647,.F.);
#25680=ORIENTED_EDGE('',*,*,#18648,.F.);
#25681=ORIENTED_EDGE('',*,*,#18649,.T.);
#25682=ORIENTED_EDGE('',*,*,#18650,.F.);
#25683=ORIENTED_EDGE('',*,*,#17889,.F.);
#25684=ORIENTED_EDGE('',*,*,#18574,.T.);
#25685=ORIENTED_EDGE('',*,*,#18647,.T.);
#25686=ORIENTED_EDGE('',*,*,#18650,.T.);
#25687=ORIENTED_EDGE('',*,*,#18651,.F.);
#25688=ORIENTED_EDGE('',*,*,#18648,.T.);
#25689=ORIENTED_EDGE('',*,*,#18652,.T.);
#25690=ORIENTED_EDGE('',*,*,#18653,.T.);
#25691=ORIENTED_EDGE('',*,*,#18654,.T.);
#25692=ORIENTED_EDGE('',*,*,#18655,.T.);
#25693=ORIENTED_EDGE('',*,*,#18656,.T.);
#25694=ORIENTED_EDGE('',*,*,#18657,.T.);
#25695=ORIENTED_EDGE('',*,*,#18658,.T.);
#25696=ORIENTED_EDGE('',*,*,#18659,.T.);
#25697=ORIENTED_EDGE('',*,*,#18641,.T.);
#25698=ORIENTED_EDGE('',*,*,#18660,.T.);
#25699=ORIENTED_EDGE('',*,*,#18661,.T.);
#25700=ORIENTED_EDGE('',*,*,#18646,.F.);
#25701=ORIENTED_EDGE('',*,*,#18659,.F.);
#25702=ORIENTED_EDGE('',*,*,#18662,.T.);
#25703=ORIENTED_EDGE('',*,*,#18663,.T.);
#25704=ORIENTED_EDGE('',*,*,#18660,.F.);
#25705=ORIENTED_EDGE('',*,*,#18651,.T.);
#25706=ORIENTED_EDGE('',*,*,#18664,.T.);
#25707=ORIENTED_EDGE('',*,*,#18665,.F.);
#25708=ORIENTED_EDGE('',*,*,#18652,.F.);
#25709=ORIENTED_EDGE('',*,*,#18665,.T.);
#25710=ORIENTED_EDGE('',*,*,#18666,.T.);
#25711=ORIENTED_EDGE('',*,*,#18667,.F.);
#25712=ORIENTED_EDGE('',*,*,#18667,.T.);
#25713=ORIENTED_EDGE('',*,*,#18668,.T.);
#25714=ORIENTED_EDGE('',*,*,#18669,.F.);
#25715=ORIENTED_EDGE('',*,*,#18653,.F.);
#25716=ORIENTED_EDGE('',*,*,#18669,.T.);
#25717=ORIENTED_EDGE('',*,*,#18670,.T.);
#25718=ORIENTED_EDGE('',*,*,#18671,.F.);
#25719=ORIENTED_EDGE('',*,*,#18671,.T.);
#25720=ORIENTED_EDGE('',*,*,#18672,.T.);
#25721=ORIENTED_EDGE('',*,*,#18673,.F.);
#25722=ORIENTED_EDGE('',*,*,#18654,.F.);
#25723=ORIENTED_EDGE('',*,*,#18673,.T.);
#25724=ORIENTED_EDGE('',*,*,#18674,.T.);
#25725=ORIENTED_EDGE('',*,*,#18675,.F.);
#25726=ORIENTED_EDGE('',*,*,#18655,.F.);
#25727=ORIENTED_EDGE('',*,*,#18675,.T.);
#25728=ORIENTED_EDGE('',*,*,#18127,.T.);
#25729=ORIENTED_EDGE('',*,*,#18676,.F.);
#25730=ORIENTED_EDGE('',*,*,#18656,.F.);
#25731=ORIENTED_EDGE('',*,*,#18676,.T.);
#25732=ORIENTED_EDGE('',*,*,#18677,.T.);
#25733=ORIENTED_EDGE('',*,*,#18678,.F.);
#25734=ORIENTED_EDGE('',*,*,#18657,.F.);
#25735=ORIENTED_EDGE('',*,*,#18678,.T.);
#25736=ORIENTED_EDGE('',*,*,#18679,.T.);
#25737=ORIENTED_EDGE('',*,*,#18662,.F.);
#25738=ORIENTED_EDGE('',*,*,#18658,.F.);
#25739=ORIENTED_EDGE('',*,*,#18680,.F.);
#25740=ORIENTED_EDGE('',*,*,#18214,.T.);
#25741=ORIENTED_EDGE('',*,*,#18644,.T.);
#25742=ORIENTED_EDGE('',*,*,#18661,.F.);
#25743=ORIENTED_EDGE('',*,*,#18681,.F.);
#25744=ORIENTED_EDGE('',*,*,#18215,.T.);
#25745=ORIENTED_EDGE('',*,*,#18680,.T.);
#25746=ORIENTED_EDGE('',*,*,#18663,.F.);
#25747=ORIENTED_EDGE('',*,*,#18573,.F.);
#25748=ORIENTED_EDGE('',*,*,#18129,.F.);
#25749=ORIENTED_EDGE('',*,*,#18204,.F.);
#25750=ORIENTED_EDGE('',*,*,#18682,.T.);
#25751=ORIENTED_EDGE('',*,*,#18664,.F.);
#25752=ORIENTED_EDGE('',*,*,#18649,.F.);
#25753=ORIENTED_EDGE('',*,*,#18682,.F.);
#25754=ORIENTED_EDGE('',*,*,#18203,.T.);
#25755=ORIENTED_EDGE('',*,*,#18683,.T.);
#25756=ORIENTED_EDGE('',*,*,#18666,.F.);
#25757=ORIENTED_EDGE('',*,*,#18683,.F.);
#25758=ORIENTED_EDGE('',*,*,#18202,.T.);
#25759=ORIENTED_EDGE('',*,*,#18684,.T.);
#25760=ORIENTED_EDGE('',*,*,#18668,.F.);
#25761=ORIENTED_EDGE('',*,*,#18684,.F.);
#25762=ORIENTED_EDGE('',*,*,#18201,.T.);
#25763=ORIENTED_EDGE('',*,*,#18685,.T.);
#25764=ORIENTED_EDGE('',*,*,#18670,.F.);
#25765=ORIENTED_EDGE('',*,*,#18685,.F.);
#25766=ORIENTED_EDGE('',*,*,#18200,.T.);
#25767=ORIENTED_EDGE('',*,*,#18686,.F.);
#25768=ORIENTED_EDGE('',*,*,#18672,.F.);
#25769=ORIENTED_EDGE('',*,*,#18674,.F.);
#25770=ORIENTED_EDGE('',*,*,#18686,.T.);
#25771=ORIENTED_EDGE('',*,*,#18199,.F.);
#25772=ORIENTED_EDGE('',*,*,#18128,.F.);
#25773=ORIENTED_EDGE('',*,*,#18677,.F.);
#25774=ORIENTED_EDGE('',*,*,#18126,.T.);
#25775=ORIENTED_EDGE('',*,*,#18217,.F.);
#25776=ORIENTED_EDGE('',*,*,#18687,.F.);
#25777=ORIENTED_EDGE('',*,*,#18679,.F.);
#25778=ORIENTED_EDGE('',*,*,#18687,.T.);
#25779=ORIENTED_EDGE('',*,*,#18216,.F.);
#25780=ORIENTED_EDGE('',*,*,#18681,.T.);
#25781=ORIENTED_EDGE('',*,*,#18688,.T.);
#25782=ORIENTED_EDGE('',*,*,#18689,.T.);
#25783=ORIENTED_EDGE('',*,*,#18690,.F.);
#25784=ORIENTED_EDGE('',*,*,#18542,.F.);
#25785=ORIENTED_EDGE('',*,*,#18543,.T.);
#25786=ORIENTED_EDGE('',*,*,#18691,.T.);
#25787=ORIENTED_EDGE('',*,*,#17850,.F.);
#25788=ORIENTED_EDGE('',*,*,#18593,.T.);
#25789=ORIENTED_EDGE('',*,*,#18690,.T.);
#25790=ORIENTED_EDGE('',*,*,#18692,.F.);
#25791=ORIENTED_EDGE('',*,*,#18691,.F.);
#25792=ORIENTED_EDGE('',*,*,#18693,.T.);
#25793=ORIENTED_EDGE('',*,*,#18694,.T.);
#25794=ORIENTED_EDGE('',*,*,#18541,.F.);
#25795=ORIENTED_EDGE('',*,*,#18585,.T.);
#25796=ORIENTED_EDGE('',*,*,#18695,.T.);
#25797=ORIENTED_EDGE('',*,*,#18688,.F.);
#25798=ORIENTED_EDGE('',*,*,#18694,.F.);
#25799=ORIENTED_EDGE('',*,*,#18692,.T.);
#25800=ORIENTED_EDGE('',*,*,#18696,.T.);
#25801=ORIENTED_EDGE('',*,*,#18697,.F.);
#25802=ORIENTED_EDGE('',*,*,#17851,.F.);
#25803=ORIENTED_EDGE('',*,*,#17852,.T.);
#25804=ORIENTED_EDGE('',*,*,#18698,.T.);
#25805=ORIENTED_EDGE('',*,*,#18546,.F.);
#25806=ORIENTED_EDGE('',*,*,#18579,.T.);
#25807=ORIENTED_EDGE('',*,*,#18697,.T.);
#25808=ORIENTED_EDGE('',*,*,#18699,.F.);
#25809=ORIENTED_EDGE('',*,*,#18698,.F.);
#25810=ORIENTED_EDGE('',*,*,#18689,.F.);
#25811=ORIENTED_EDGE('',*,*,#18700,.F.);
#25812=ORIENTED_EDGE('',*,*,#18701,.F.);
#25813=ORIENTED_EDGE('',*,*,#18702,.F.);
#25814=ORIENTED_EDGE('',*,*,#18703,.F.);
#25815=ORIENTED_EDGE('',*,*,#18704,.F.);
#25816=ORIENTED_EDGE('',*,*,#18705,.F.);
#25817=ORIENTED_EDGE('',*,*,#18706,.F.);
#25818=ORIENTED_EDGE('',*,*,#18707,.F.);
#25819=ORIENTED_EDGE('',*,*,#18696,.F.);
#25820=ORIENTED_EDGE('',*,*,#18708,.T.);
#25821=ORIENTED_EDGE('',*,*,#18700,.T.);
#25822=ORIENTED_EDGE('',*,*,#18695,.F.);
#25823=ORIENTED_EDGE('',*,*,#18709,.F.);
#25824=ORIENTED_EDGE('',*,*,#18710,.T.);
#25825=ORIENTED_EDGE('',*,*,#18708,.F.);
#25826=ORIENTED_EDGE('',*,*,#18711,.F.);
#25827=ORIENTED_EDGE('',*,*,#18699,.T.);
#25828=ORIENTED_EDGE('',*,*,#18707,.T.);
#25829=ORIENTED_EDGE('',*,*,#18712,.F.);
#25830=ORIENTED_EDGE('',*,*,#18547,.F.);
#25831=ORIENTED_EDGE('',*,*,#18712,.T.);
#25832=ORIENTED_EDGE('',*,*,#18713,.F.);
#25833=ORIENTED_EDGE('',*,*,#18714,.F.);
#25834=ORIENTED_EDGE('',*,*,#18713,.T.);
#25835=ORIENTED_EDGE('',*,*,#18706,.T.);
#25836=ORIENTED_EDGE('',*,*,#18715,.F.);
#25837=ORIENTED_EDGE('',*,*,#18716,.F.);
#25838=ORIENTED_EDGE('',*,*,#18715,.T.);
#25839=ORIENTED_EDGE('',*,*,#18717,.F.);
#25840=ORIENTED_EDGE('',*,*,#18718,.F.);
#25841=ORIENTED_EDGE('',*,*,#18717,.T.);
#25842=ORIENTED_EDGE('',*,*,#18705,.T.);
#25843=ORIENTED_EDGE('',*,*,#18719,.F.);
#25844=ORIENTED_EDGE('',*,*,#18552,.F.);
#25845=ORIENTED_EDGE('',*,*,#18719,.T.);
#25846=ORIENTED_EDGE('',*,*,#18704,.T.);
#25847=ORIENTED_EDGE('',*,*,#18720,.F.);
#25848=ORIENTED_EDGE('',*,*,#18721,.F.);
#25849=ORIENTED_EDGE('',*,*,#18720,.T.);
#25850=ORIENTED_EDGE('',*,*,#18703,.T.);
#25851=ORIENTED_EDGE('',*,*,#18722,.F.);
#25852=ORIENTED_EDGE('',*,*,#18169,.F.);
#25853=ORIENTED_EDGE('',*,*,#18722,.T.);
#25854=ORIENTED_EDGE('',*,*,#18702,.T.);
#25855=ORIENTED_EDGE('',*,*,#18723,.F.);
#25856=ORIENTED_EDGE('',*,*,#18724,.F.);
#25857=ORIENTED_EDGE('',*,*,#18723,.T.);
#25858=ORIENTED_EDGE('',*,*,#18701,.T.);
#25859=ORIENTED_EDGE('',*,*,#18710,.F.);
#25860=ORIENTED_EDGE('',*,*,#18537,.F.);
#25861=ORIENTED_EDGE('',*,*,#18725,.T.);
#25862=ORIENTED_EDGE('',*,*,#18709,.T.);
#25863=ORIENTED_EDGE('',*,*,#18693,.F.);
#25864=ORIENTED_EDGE('',*,*,#18584,.T.);
#25865=ORIENTED_EDGE('',*,*,#18538,.T.);
#25866=ORIENTED_EDGE('',*,*,#18711,.T.);
#25867=ORIENTED_EDGE('',*,*,#18725,.F.);
#25868=ORIENTED_EDGE('',*,*,#18583,.T.);
#25869=ORIENTED_EDGE('',*,*,#18548,.T.);
#25870=ORIENTED_EDGE('',*,*,#18714,.T.);
#25871=ORIENTED_EDGE('',*,*,#18726,.F.);
#25872=ORIENTED_EDGE('',*,*,#18580,.T.);
#25873=ORIENTED_EDGE('',*,*,#18726,.T.);
#25874=ORIENTED_EDGE('',*,*,#18716,.T.);
#25875=ORIENTED_EDGE('',*,*,#18727,.F.);
#25876=ORIENTED_EDGE('',*,*,#18581,.T.);
#25877=ORIENTED_EDGE('',*,*,#18727,.T.);
#25878=ORIENTED_EDGE('',*,*,#18718,.T.);
#25879=ORIENTED_EDGE('',*,*,#18551,.F.);
#25880=ORIENTED_EDGE('',*,*,#18582,.T.);
#25881=ORIENTED_EDGE('',*,*,#18721,.T.);
#25882=ORIENTED_EDGE('',*,*,#18168,.T.);
#25883=ORIENTED_EDGE('',*,*,#18145,.F.);
#25884=ORIENTED_EDGE('',*,*,#18553,.F.);
#25885=ORIENTED_EDGE('',*,*,#18724,.T.);
#25886=ORIENTED_EDGE('',*,*,#18536,.T.);
#25887=ORIENTED_EDGE('',*,*,#18141,.F.);
#25888=ORIENTED_EDGE('',*,*,#18170,.F.);
#25889=ORIENTED_EDGE('',*,*,#18586,.F.);
#25890=ORIENTED_EDGE('',*,*,#18117,.F.);
#25891=ORIENTED_EDGE('',*,*,#18159,.F.);
#25892=ORIENTED_EDGE('',*,*,#18728,.T.);
#25893=ORIENTED_EDGE('',*,*,#18729,.T.);
#25894=ORIENTED_EDGE('',*,*,#18730,.F.);
#25895=ORIENTED_EDGE('',*,*,#18731,.T.);
#25896=ORIENTED_EDGE('',*,*,#18732,.T.);
#25897=ORIENTED_EDGE('',*,*,#18733,.F.);
#25898=ORIENTED_EDGE('',*,*,#18729,.F.);
#25899=ORIENTED_EDGE('',*,*,#18728,.F.);
#25900=ORIENTED_EDGE('',*,*,#18158,.T.);
#25901=ORIENTED_EDGE('',*,*,#18734,.T.);
#25902=ORIENTED_EDGE('',*,*,#18735,.T.);
#25903=ORIENTED_EDGE('',*,*,#18736,.T.);
#25904=ORIENTED_EDGE('',*,*,#18731,.F.);
#25905=ORIENTED_EDGE('',*,*,#18735,.F.);
#25906=ORIENTED_EDGE('',*,*,#18730,.T.);
#25907=ORIENTED_EDGE('',*,*,#18737,.T.);
#25908=ORIENTED_EDGE('',*,*,#17842,.F.);
#25909=ORIENTED_EDGE('',*,*,#18587,.T.);
#25910=ORIENTED_EDGE('',*,*,#18733,.T.);
#25911=ORIENTED_EDGE('',*,*,#18738,.F.);
#25912=ORIENTED_EDGE('',*,*,#18737,.F.);
#25913=ORIENTED_EDGE('',*,*,#18732,.F.);
#25914=ORIENTED_EDGE('',*,*,#18739,.F.);
#25915=ORIENTED_EDGE('',*,*,#18740,.F.);
#25916=ORIENTED_EDGE('',*,*,#18741,.F.);
#25917=ORIENTED_EDGE('',*,*,#18742,.F.);
#25918=ORIENTED_EDGE('',*,*,#18743,.F.);
#25919=ORIENTED_EDGE('',*,*,#18744,.F.);
#25920=ORIENTED_EDGE('',*,*,#18745,.F.);
#25921=ORIENTED_EDGE('',*,*,#18746,.F.);
#25922=ORIENTED_EDGE('',*,*,#18747,.F.);
#25923=ORIENTED_EDGE('',*,*,#18748,.T.);
#25924=ORIENTED_EDGE('',*,*,#18739,.T.);
#25925=ORIENTED_EDGE('',*,*,#18736,.F.);
#25926=ORIENTED_EDGE('',*,*,#18749,.F.);
#25927=ORIENTED_EDGE('',*,*,#18750,.T.);
#25928=ORIENTED_EDGE('',*,*,#18748,.F.);
#25929=ORIENTED_EDGE('',*,*,#18751,.F.);
#25930=ORIENTED_EDGE('',*,*,#18738,.T.);
#25931=ORIENTED_EDGE('',*,*,#18747,.T.);
#25932=ORIENTED_EDGE('',*,*,#18752,.F.);
#25933=ORIENTED_EDGE('',*,*,#17843,.F.);
#25934=ORIENTED_EDGE('',*,*,#18752,.T.);
#25935=ORIENTED_EDGE('',*,*,#18753,.F.);
#25936=ORIENTED_EDGE('',*,*,#18754,.F.);
#25937=ORIENTED_EDGE('',*,*,#18755,.T.);
#25938=ORIENTED_EDGE('',*,*,#18745,.T.);
#25939=ORIENTED_EDGE('',*,*,#18756,.F.);
#25940=ORIENTED_EDGE('',*,*,#18757,.F.);
#25941=ORIENTED_EDGE('',*,*,#18758,.T.);
#25942=ORIENTED_EDGE('',*,*,#18755,.F.);
#25943=ORIENTED_EDGE('',*,*,#18759,.F.);
#25944=ORIENTED_EDGE('',*,*,#18756,.T.);
#25945=ORIENTED_EDGE('',*,*,#18760,.F.);
#25946=ORIENTED_EDGE('',*,*,#18761,.F.);
#25947=ORIENTED_EDGE('',*,*,#18753,.T.);
#25948=ORIENTED_EDGE('',*,*,#18746,.T.);
#25949=ORIENTED_EDGE('',*,*,#18758,.F.);
#25950=ORIENTED_EDGE('',*,*,#18762,.F.);
#25951=ORIENTED_EDGE('',*,*,#18760,.T.);
#25952=ORIENTED_EDGE('',*,*,#18744,.T.);
#25953=ORIENTED_EDGE('',*,*,#18763,.F.);
#25954=ORIENTED_EDGE('',*,*,#18764,.F.);
#25955=ORIENTED_EDGE('',*,*,#18763,.T.);
#25956=ORIENTED_EDGE('',*,*,#18743,.T.);
#25957=ORIENTED_EDGE('',*,*,#18765,.F.);
#25958=ORIENTED_EDGE('',*,*,#18766,.F.);
#25959=ORIENTED_EDGE('',*,*,#18765,.T.);
#25960=ORIENTED_EDGE('',*,*,#18742,.T.);
#25961=ORIENTED_EDGE('',*,*,#18767,.F.);
#25962=ORIENTED_EDGE('',*,*,#18115,.F.);
#25963=ORIENTED_EDGE('',*,*,#18767,.T.);
#25964=ORIENTED_EDGE('',*,*,#18741,.T.);
#25965=ORIENTED_EDGE('',*,*,#18768,.F.);
#25966=ORIENTED_EDGE('',*,*,#18769,.F.);
#25967=ORIENTED_EDGE('',*,*,#18768,.T.);
#25968=ORIENTED_EDGE('',*,*,#18740,.T.);
#25969=ORIENTED_EDGE('',*,*,#18750,.F.);
#25970=ORIENTED_EDGE('',*,*,#18770,.F.);
#25971=ORIENTED_EDGE('',*,*,#18749,.T.);
#25972=ORIENTED_EDGE('',*,*,#18734,.F.);
#25973=ORIENTED_EDGE('',*,*,#18157,.F.);
#25974=ORIENTED_EDGE('',*,*,#18771,.T.);
#25975=ORIENTED_EDGE('',*,*,#18771,.F.);
#25976=ORIENTED_EDGE('',*,*,#18156,.T.);
#25977=ORIENTED_EDGE('',*,*,#18772,.T.);
#25978=ORIENTED_EDGE('',*,*,#18751,.T.);
#25979=ORIENTED_EDGE('',*,*,#17844,.T.);
#25980=ORIENTED_EDGE('',*,*,#18754,.T.);
#25981=ORIENTED_EDGE('',*,*,#18773,.F.);
#25982=ORIENTED_EDGE('',*,*,#18594,.T.);
#25983=ORIENTED_EDGE('',*,*,#18757,.T.);
#25984=ORIENTED_EDGE('',*,*,#18774,.F.);
#25985=ORIENTED_EDGE('',*,*,#18150,.F.);
#25986=ORIENTED_EDGE('',*,*,#18775,.T.);
#25987=ORIENTED_EDGE('',*,*,#18775,.F.);
#25988=ORIENTED_EDGE('',*,*,#18149,.T.);
#25989=ORIENTED_EDGE('',*,*,#18776,.T.);
#25990=ORIENTED_EDGE('',*,*,#18759,.T.);
#25991=ORIENTED_EDGE('',*,*,#18777,.F.);
#25992=ORIENTED_EDGE('',*,*,#18151,.T.);
#25993=ORIENTED_EDGE('',*,*,#18774,.T.);
#25994=ORIENTED_EDGE('',*,*,#18761,.T.);
#25995=ORIENTED_EDGE('',*,*,#18773,.T.);
#25996=ORIENTED_EDGE('',*,*,#18762,.T.);
#25997=ORIENTED_EDGE('',*,*,#18776,.F.);
#25998=ORIENTED_EDGE('',*,*,#18148,.T.);
#25999=ORIENTED_EDGE('',*,*,#18110,.T.);
#26000=ORIENTED_EDGE('',*,*,#18595,.T.);
#26001=ORIENTED_EDGE('',*,*,#18764,.T.);
#26002=ORIENTED_EDGE('',*,*,#18778,.T.);
#26003=ORIENTED_EDGE('',*,*,#18152,.F.);
#26004=ORIENTED_EDGE('',*,*,#18777,.T.);
#26005=ORIENTED_EDGE('',*,*,#18766,.T.);
#26006=ORIENTED_EDGE('',*,*,#18114,.T.);
#26007=ORIENTED_EDGE('',*,*,#18153,.F.);
#26008=ORIENTED_EDGE('',*,*,#18778,.F.);
#26009=ORIENTED_EDGE('',*,*,#18769,.T.);
#26010=ORIENTED_EDGE('',*,*,#18779,.T.);
#26011=ORIENTED_EDGE('',*,*,#18154,.F.);
#26012=ORIENTED_EDGE('',*,*,#18116,.F.);
#26013=ORIENTED_EDGE('',*,*,#18772,.F.);
#26014=ORIENTED_EDGE('',*,*,#18155,.T.);
#26015=ORIENTED_EDGE('',*,*,#18779,.F.);
#26016=ORIENTED_EDGE('',*,*,#18770,.T.);
#26017=ORIENTED_EDGE('',*,*,#18780,.F.);
#26018=ORIENTED_EDGE('',*,*,#18781,.F.);
#26019=ORIENTED_EDGE('',*,*,#18782,.T.);
#26020=ORIENTED_EDGE('',*,*,#18783,.T.);
#26021=ORIENTED_EDGE('',*,*,#18784,.T.);
#26022=ORIENTED_EDGE('',*,*,#18785,.F.);
#26023=ORIENTED_EDGE('',*,*,#18786,.F.);
#26024=ORIENTED_EDGE('',*,*,#18787,.F.);
#26025=ORIENTED_EDGE('',*,*,#18788,.T.);
#26026=ORIENTED_EDGE('',*,*,#18789,.T.);
#26027=ORIENTED_EDGE('',*,*,#18790,.T.);
#26028=ORIENTED_EDGE('',*,*,#18791,.F.);
#26029=ORIENTED_EDGE('',*,*,#18792,.T.);
#26030=ORIENTED_EDGE('',*,*,#18793,.T.);
#26031=ORIENTED_EDGE('',*,*,#18794,.F.);
#26032=ORIENTED_EDGE('',*,*,#18795,.F.);
#26033=ORIENTED_EDGE('',*,*,#18796,.F.);
#26034=ORIENTED_EDGE('',*,*,#18797,.T.);
#26035=ORIENTED_EDGE('',*,*,#18798,.T.);
#26036=ORIENTED_EDGE('',*,*,#18799,.T.);
#26037=ORIENTED_EDGE('',*,*,#18800,.F.);
#26038=ORIENTED_EDGE('',*,*,#18801,.F.);
#26039=ORIENTED_EDGE('',*,*,#18802,.F.);
#26040=ORIENTED_EDGE('',*,*,#18803,.T.);
#26041=ORIENTED_EDGE('',*,*,#18804,.T.);
#26042=ORIENTED_EDGE('',*,*,#18805,.T.);
#26043=ORIENTED_EDGE('',*,*,#18806,.F.);
#26044=ORIENTED_EDGE('',*,*,#18807,.F.);
#26045=ORIENTED_EDGE('',*,*,#18808,.F.);
#26046=ORIENTED_EDGE('',*,*,#18809,.T.);
#26047=ORIENTED_EDGE('',*,*,#18810,.T.);
#26048=ORIENTED_EDGE('',*,*,#18811,.F.);
#26049=ORIENTED_EDGE('',*,*,#18812,.F.);
#26050=ORIENTED_EDGE('',*,*,#18813,.F.);
#26051=ORIENTED_EDGE('',*,*,#18814,.F.);
#26052=ORIENTED_EDGE('',*,*,#18815,.T.);
#26053=ORIENTED_EDGE('',*,*,#18816,.T.);
#26054=ORIENTED_EDGE('',*,*,#18817,.F.);
#26055=ORIENTED_EDGE('',*,*,#18818,.F.);
#26056=ORIENTED_EDGE('',*,*,#18819,.T.);
#26057=ORIENTED_EDGE('',*,*,#18820,.F.);
#26058=ORIENTED_EDGE('',*,*,#18816,.F.);
#26059=ORIENTED_EDGE('',*,*,#18821,.F.);
#26060=ORIENTED_EDGE('',*,*,#18822,.F.);
#26061=ORIENTED_EDGE('',*,*,#18819,.F.);
#26062=ORIENTED_EDGE('',*,*,#18823,.F.);
#26063=ORIENTED_EDGE('',*,*,#18821,.T.);
#26064=ORIENTED_EDGE('',*,*,#18824,.F.);
#26065=ORIENTED_EDGE('',*,*,#18825,.F.);
#26066=ORIENTED_EDGE('',*,*,#18826,.F.);
#26067=ORIENTED_EDGE('',*,*,#18810,.F.);
#26068=ORIENTED_EDGE('',*,*,#18825,.T.);
#26069=ORIENTED_EDGE('',*,*,#18827,.T.);
#26070=ORIENTED_EDGE('',*,*,#18818,.T.);
#26071=ORIENTED_EDGE('',*,*,#18828,.F.);
#26072=ORIENTED_EDGE('',*,*,#18829,.T.);
#26073=ORIENTED_EDGE('',*,*,#18823,.T.);
#26074=ORIENTED_EDGE('',*,*,#18827,.F.);
#26075=ORIENTED_EDGE('',*,*,#18830,.F.);
#26076=ORIENTED_EDGE('',*,*,#18811,.T.);
#26077=ORIENTED_EDGE('',*,*,#18824,.T.);
#26078=ORIENTED_EDGE('',*,*,#18829,.F.);
#26079=ORIENTED_EDGE('',*,*,#18831,.F.);
#26080=ORIENTED_EDGE('',*,*,#18832,.T.);
#26081=ORIENTED_EDGE('',*,*,#18833,.T.);
#26082=ORIENTED_EDGE('',*,*,#18834,.T.);
#26083=ORIENTED_EDGE('',*,*,#18814,.T.);
#26084=ORIENTED_EDGE('',*,*,#18835,.T.);
#26085=ORIENTED_EDGE('',*,*,#18835,.F.);
#26086=ORIENTED_EDGE('',*,*,#18813,.T.);
#26087=ORIENTED_EDGE('',*,*,#18812,.T.);
#26088=ORIENTED_EDGE('',*,*,#18831,.T.);
#26089=ORIENTED_EDGE('',*,*,#18830,.T.);
#26090=ORIENTED_EDGE('',*,*,#18836,.T.);
#26091=ORIENTED_EDGE('',*,*,#18837,.F.);
#26092=ORIENTED_EDGE('',*,*,#18838,.F.);
#26093=ORIENTED_EDGE('',*,*,#18839,.F.);
#26094=ORIENTED_EDGE('',*,*,#18840,.F.);
#26095=ORIENTED_EDGE('',*,*,#18809,.F.);
#26096=ORIENTED_EDGE('',*,*,#18841,.F.);
#26097=ORIENTED_EDGE('',*,*,#18842,.F.);
#26098=ORIENTED_EDGE('',*,*,#18843,.F.);
#26099=ORIENTED_EDGE('',*,*,#18844,.F.);
#26100=ORIENTED_EDGE('',*,*,#18803,.F.);
#26101=ORIENTED_EDGE('',*,*,#18845,.F.);
#26102=ORIENTED_EDGE('',*,*,#18846,.F.);
#26103=ORIENTED_EDGE('',*,*,#18847,.F.);
#26104=ORIENTED_EDGE('',*,*,#18797,.F.);
#26105=ORIENTED_EDGE('',*,*,#18848,.F.);
#26106=ORIENTED_EDGE('',*,*,#18849,.F.);
#26107=ORIENTED_EDGE('',*,*,#18850,.F.);
#26108=ORIENTED_EDGE('',*,*,#18788,.F.);
#26109=ORIENTED_EDGE('',*,*,#18851,.F.);
#26110=ORIENTED_EDGE('',*,*,#18852,.F.);
#26111=ORIENTED_EDGE('',*,*,#18853,.F.);
#26112=ORIENTED_EDGE('',*,*,#18854,.F.);
#26113=ORIENTED_EDGE('',*,*,#18782,.F.);
#26114=ORIENTED_EDGE('',*,*,#18855,.F.);
#26115=ORIENTED_EDGE('',*,*,#18856,.F.);
#26116=ORIENTED_EDGE('',*,*,#18857,.F.);
#26117=ORIENTED_EDGE('',*,*,#18858,.T.);
#26118=ORIENTED_EDGE('',*,*,#18820,.T.);
#26119=ORIENTED_EDGE('',*,*,#18859,.F.);
#26120=ORIENTED_EDGE('',*,*,#18859,.T.);
#26121=ORIENTED_EDGE('',*,*,#18822,.T.);
#26122=ORIENTED_EDGE('',*,*,#18860,.F.);
#26123=ORIENTED_EDGE('',*,*,#18833,.F.);
#26124=ORIENTED_EDGE('',*,*,#18860,.T.);
#26125=ORIENTED_EDGE('',*,*,#18826,.T.);
#26126=ORIENTED_EDGE('',*,*,#18815,.F.);
#26127=ORIENTED_EDGE('',*,*,#18834,.F.);
#26128=ORIENTED_EDGE('',*,*,#18828,.T.);
#26129=ORIENTED_EDGE('',*,*,#18817,.T.);
#26130=ORIENTED_EDGE('',*,*,#18858,.F.);
#26131=ORIENTED_EDGE('',*,*,#18832,.F.);
#26132=ORIENTED_EDGE('',*,*,#18836,.F.);
#26133=ORIENTED_EDGE('',*,*,#18861,.F.);
#26134=ORIENTED_EDGE('',*,*,#18861,.T.);
#26135=ORIENTED_EDGE('',*,*,#18862,.T.);
#26136=ORIENTED_EDGE('',*,*,#18863,.T.);
#26137=ORIENTED_EDGE('',*,*,#18862,.F.);
#26138=ORIENTED_EDGE('',*,*,#18864,.T.);
#26139=ORIENTED_EDGE('',*,*,#18865,.F.);
#26140=ORIENTED_EDGE('',*,*,#18866,.F.);
#26141=ORIENTED_EDGE('',*,*,#18867,.F.);
#26142=ORIENTED_EDGE('',*,*,#18868,.F.);
#26143=ORIENTED_EDGE('',*,*,#18869,.F.);
#26144=ORIENTED_EDGE('',*,*,#18870,.F.);
#26145=ORIENTED_EDGE('',*,*,#18871,.F.);
#26146=ORIENTED_EDGE('',*,*,#18863,.F.);
#26147=ORIENTED_EDGE('',*,*,#18871,.T.);
#26148=ORIENTED_EDGE('',*,*,#18872,.T.);
#26149=ORIENTED_EDGE('',*,*,#18873,.F.);
#26150=ORIENTED_EDGE('',*,*,#18874,.F.);
#26151=ORIENTED_EDGE('',*,*,#18870,.T.);
#26152=ORIENTED_EDGE('',*,*,#18875,.T.);
#26153=ORIENTED_EDGE('',*,*,#18876,.F.);
#26154=ORIENTED_EDGE('',*,*,#18872,.F.);
#26155=ORIENTED_EDGE('',*,*,#18869,.T.);
#26156=ORIENTED_EDGE('',*,*,#18877,.T.);
#26157=ORIENTED_EDGE('',*,*,#18878,.F.);
#26158=ORIENTED_EDGE('',*,*,#18875,.F.);
#26159=ORIENTED_EDGE('',*,*,#18868,.T.);
#26160=ORIENTED_EDGE('',*,*,#18879,.T.);
#26161=ORIENTED_EDGE('',*,*,#18880,.F.);
#26162=ORIENTED_EDGE('',*,*,#18877,.F.);
#26163=ORIENTED_EDGE('',*,*,#18867,.T.);
#26164=ORIENTED_EDGE('',*,*,#18881,.T.);
#26165=ORIENTED_EDGE('',*,*,#18882,.F.);
#26166=ORIENTED_EDGE('',*,*,#18879,.F.);
#26167=ORIENTED_EDGE('',*,*,#18866,.T.);
#26168=ORIENTED_EDGE('',*,*,#18883,.T.);
#26169=ORIENTED_EDGE('',*,*,#18884,.F.);
#26170=ORIENTED_EDGE('',*,*,#18881,.F.);
#26171=ORIENTED_EDGE('',*,*,#18865,.T.);
#26172=ORIENTED_EDGE('',*,*,#18885,.T.);
#26173=ORIENTED_EDGE('',*,*,#18886,.F.);
#26174=ORIENTED_EDGE('',*,*,#18883,.F.);
#26175=ORIENTED_EDGE('',*,*,#18887,.F.);
#26176=ORIENTED_EDGE('',*,*,#18864,.F.);
#26177=ORIENTED_EDGE('',*,*,#18888,.F.);
#26178=ORIENTED_EDGE('',*,*,#18889,.F.);
#26179=ORIENTED_EDGE('',*,*,#18890,.F.);
#26180=ORIENTED_EDGE('',*,*,#18891,.T.);
#26181=ORIENTED_EDGE('',*,*,#18892,.T.);
#26182=ORIENTED_EDGE('',*,*,#18893,.F.);
#26183=ORIENTED_EDGE('',*,*,#18894,.T.);
#26184=ORIENTED_EDGE('',*,*,#18895,.T.);
#26185=ORIENTED_EDGE('',*,*,#18896,.T.);
#26186=ORIENTED_EDGE('',*,*,#18873,.T.);
#26187=ORIENTED_EDGE('',*,*,#18897,.T.);
#26188=ORIENTED_EDGE('',*,*,#18888,.T.);
#26189=ORIENTED_EDGE('',*,*,#18874,.T.);
#26190=ORIENTED_EDGE('',*,*,#18896,.F.);
#26191=ORIENTED_EDGE('',*,*,#18898,.F.);
#26192=ORIENTED_EDGE('',*,*,#18897,.F.);
#26193=ORIENTED_EDGE('',*,*,#18876,.T.);
#26194=ORIENTED_EDGE('',*,*,#18899,.T.);
#26195=ORIENTED_EDGE('',*,*,#18900,.T.);
#26196=ORIENTED_EDGE('',*,*,#18901,.T.);
#26197=ORIENTED_EDGE('',*,*,#18899,.F.);
#26198=ORIENTED_EDGE('',*,*,#18878,.T.);
#26199=ORIENTED_EDGE('',*,*,#18902,.F.);
#26200=ORIENTED_EDGE('',*,*,#18903,.T.);
#26201=ORIENTED_EDGE('',*,*,#18902,.T.);
#26202=ORIENTED_EDGE('',*,*,#18880,.T.);
#26203=ORIENTED_EDGE('',*,*,#18904,.F.);
#26204=ORIENTED_EDGE('',*,*,#18905,.T.);
#26205=ORIENTED_EDGE('',*,*,#18904,.T.);
#26206=ORIENTED_EDGE('',*,*,#18882,.T.);
#26207=ORIENTED_EDGE('',*,*,#18906,.F.);
#26208=ORIENTED_EDGE('',*,*,#18907,.T.);
#26209=ORIENTED_EDGE('',*,*,#18906,.T.);
#26210=ORIENTED_EDGE('',*,*,#18884,.T.);
#26211=ORIENTED_EDGE('',*,*,#18908,.F.);
#26212=ORIENTED_EDGE('',*,*,#18887,.T.);
#26213=ORIENTED_EDGE('',*,*,#18909,.T.);
#26214=ORIENTED_EDGE('',*,*,#18910,.F.);
#26215=ORIENTED_EDGE('',*,*,#18885,.F.);
#26216=ORIENTED_EDGE('',*,*,#18908,.T.);
#26217=ORIENTED_EDGE('',*,*,#18886,.T.);
#26218=ORIENTED_EDGE('',*,*,#18910,.T.);
#26219=ORIENTED_EDGE('',*,*,#18911,.T.);
#26220=ORIENTED_EDGE('',*,*,#18912,.T.);
#26221=ORIENTED_EDGE('',*,*,#18913,.T.);
#26222=ORIENTED_EDGE('',*,*,#18914,.F.);
#26223=ORIENTED_EDGE('',*,*,#18915,.T.);
#26224=ORIENTED_EDGE('',*,*,#18890,.T.);
#26225=ORIENTED_EDGE('',*,*,#18916,.T.);
#26226=ORIENTED_EDGE('',*,*,#18917,.F.);
#26227=ORIENTED_EDGE('',*,*,#18918,.F.);
#26228=ORIENTED_EDGE('',*,*,#18889,.T.);
#26229=ORIENTED_EDGE('',*,*,#18898,.T.);
#26230=ORIENTED_EDGE('',*,*,#18919,.F.);
#26231=ORIENTED_EDGE('',*,*,#18916,.F.);
#26232=ORIENTED_EDGE('',*,*,#18920,.T.);
#26233=ORIENTED_EDGE('',*,*,#18891,.F.);
#26234=ORIENTED_EDGE('',*,*,#18921,.F.);
#26235=ORIENTED_EDGE('',*,*,#18922,.T.);
#26236=ORIENTED_EDGE('',*,*,#18923,.T.);
#26237=ORIENTED_EDGE('',*,*,#18892,.F.);
#26238=ORIENTED_EDGE('',*,*,#18924,.F.);
#26239=ORIENTED_EDGE('',*,*,#18893,.T.);
#26240=ORIENTED_EDGE('',*,*,#18925,.T.);
#26241=ORIENTED_EDGE('',*,*,#18926,.F.);
#26242=ORIENTED_EDGE('',*,*,#18927,.T.);
#26243=ORIENTED_EDGE('',*,*,#18928,.T.);
#26244=ORIENTED_EDGE('',*,*,#18929,.F.);
#26245=ORIENTED_EDGE('',*,*,#18894,.F.);
#26246=ORIENTED_EDGE('',*,*,#18930,.T.);
#26247=ORIENTED_EDGE('',*,*,#18931,.T.);
#26248=ORIENTED_EDGE('',*,*,#18919,.T.);
#26249=ORIENTED_EDGE('',*,*,#18895,.F.);
#26250=ORIENTED_EDGE('',*,*,#18932,.T.);
#26251=ORIENTED_EDGE('',*,*,#18933,.T.);
#26252=ORIENTED_EDGE('',*,*,#18927,.F.);
#26253=ORIENTED_EDGE('',*,*,#18900,.F.);
#26254=ORIENTED_EDGE('',*,*,#18934,.T.);
#26255=ORIENTED_EDGE('',*,*,#18935,.T.);
#26256=ORIENTED_EDGE('',*,*,#18932,.F.);
#26257=ORIENTED_EDGE('',*,*,#18901,.F.);
#26258=ORIENTED_EDGE('',*,*,#18936,.T.);
#26259=ORIENTED_EDGE('',*,*,#18937,.T.);
#26260=ORIENTED_EDGE('',*,*,#18934,.F.);
#26261=ORIENTED_EDGE('',*,*,#18903,.F.);
#26262=ORIENTED_EDGE('',*,*,#18938,.T.);
#26263=ORIENTED_EDGE('',*,*,#18939,.T.);
#26264=ORIENTED_EDGE('',*,*,#18936,.F.);
#26265=ORIENTED_EDGE('',*,*,#18905,.F.);
#26266=ORIENTED_EDGE('',*,*,#18940,.T.);
#26267=ORIENTED_EDGE('',*,*,#18941,.T.);
#26268=ORIENTED_EDGE('',*,*,#18938,.F.);
#26269=ORIENTED_EDGE('',*,*,#18907,.F.);
#26270=ORIENTED_EDGE('',*,*,#18926,.T.);
#26271=ORIENTED_EDGE('',*,*,#18942,.T.);
#26272=ORIENTED_EDGE('',*,*,#18911,.F.);
#26273=ORIENTED_EDGE('',*,*,#18909,.F.);
#26274=ORIENTED_EDGE('',*,*,#18943,.T.);
#26275=ORIENTED_EDGE('',*,*,#18912,.F.);
#26276=ORIENTED_EDGE('',*,*,#18942,.F.);
#26277=ORIENTED_EDGE('',*,*,#18944,.T.);
#26278=ORIENTED_EDGE('',*,*,#18945,.T.);
#26279=ORIENTED_EDGE('',*,*,#18946,.T.);
#26280=ORIENTED_EDGE('',*,*,#18913,.F.);
#26281=ORIENTED_EDGE('',*,*,#18947,.F.);
#26282=ORIENTED_EDGE('',*,*,#18948,.T.);
#26283=ORIENTED_EDGE('',*,*,#18914,.T.);
#26284=ORIENTED_EDGE('',*,*,#18949,.T.);
#26285=ORIENTED_EDGE('',*,*,#18950,.F.);
#26286=ORIENTED_EDGE('',*,*,#18951,.T.);
#26287=ORIENTED_EDGE('',*,*,#18952,.T.);
#26288=ORIENTED_EDGE('',*,*,#18940,.F.);
#26289=ORIENTED_EDGE('',*,*,#18915,.F.);
#26290=ORIENTED_EDGE('',*,*,#18953,.T.);
#26291=ORIENTED_EDGE('',*,*,#18954,.T.);
#26292=ORIENTED_EDGE('',*,*,#18955,.T.);
#26293=ORIENTED_EDGE('',*,*,#18956,.T.);
#26294=ORIENTED_EDGE('',*,*,#18957,.T.);
#26295=ORIENTED_EDGE('',*,*,#18917,.T.);
#26296=ORIENTED_EDGE('',*,*,#18931,.F.);
#26297=ORIENTED_EDGE('',*,*,#18921,.T.);
#26298=ORIENTED_EDGE('',*,*,#18918,.T.);
#26299=ORIENTED_EDGE('',*,*,#18957,.F.);
#26300=ORIENTED_EDGE('',*,*,#18958,.F.);
#26301=ORIENTED_EDGE('',*,*,#18924,.T.);
#26302=ORIENTED_EDGE('',*,*,#18920,.F.);
#26303=ORIENTED_EDGE('',*,*,#18959,.F.);
#26304=ORIENTED_EDGE('',*,*,#18960,.T.);
#26305=ORIENTED_EDGE('',*,*,#18961,.T.);
#26306=ORIENTED_EDGE('',*,*,#18962,.T.);
#26307=ORIENTED_EDGE('',*,*,#18922,.F.);
#26308=ORIENTED_EDGE('',*,*,#18963,.F.);
#26309=ORIENTED_EDGE('',*,*,#18944,.F.);
#26310=ORIENTED_EDGE('',*,*,#18925,.F.);
#26311=ORIENTED_EDGE('',*,*,#18923,.F.);
#26312=ORIENTED_EDGE('',*,*,#18964,.T.);
#26313=ORIENTED_EDGE('',*,*,#18929,.T.);
#26314=ORIENTED_EDGE('',*,*,#18965,.T.);
#26315=ORIENTED_EDGE('',*,*,#18966,.F.);
#26316=ORIENTED_EDGE('',*,*,#18930,.F.);
#26317=ORIENTED_EDGE('',*,*,#18967,.F.);
#26318=ORIENTED_EDGE('',*,*,#18968,.F.);
#26319=ORIENTED_EDGE('',*,*,#18969,.F.);
#26320=ORIENTED_EDGE('',*,*,#18970,.F.);
#26321=ORIENTED_EDGE('',*,*,#18971,.F.);
#26322=ORIENTED_EDGE('',*,*,#18972,.F.);
#26323=ORIENTED_EDGE('',*,*,#18973,.F.);
#26324=ORIENTED_EDGE('',*,*,#18974,.F.);
#26325=ORIENTED_EDGE('',*,*,#18975,.F.);
#26326=ORIENTED_EDGE('',*,*,#18976,.F.);
#26327=ORIENTED_EDGE('',*,*,#18977,.F.);
#26328=ORIENTED_EDGE('',*,*,#18978,.F.);
#26329=ORIENTED_EDGE('',*,*,#18979,.F.);
#26330=ORIENTED_EDGE('',*,*,#18980,.F.);
#26331=ORIENTED_EDGE('',*,*,#18981,.F.);
#26332=ORIENTED_EDGE('',*,*,#18982,.F.);
#26333=ORIENTED_EDGE('',*,*,#18983,.F.);
#26334=ORIENTED_EDGE('',*,*,#18984,.F.);
#26335=ORIENTED_EDGE('',*,*,#18985,.F.);
#26336=ORIENTED_EDGE('',*,*,#18986,.F.);
#26337=ORIENTED_EDGE('',*,*,#18987,.F.);
#26338=ORIENTED_EDGE('',*,*,#18988,.F.);
#26339=ORIENTED_EDGE('',*,*,#18989,.F.);
#26340=ORIENTED_EDGE('',*,*,#18990,.F.);
#26341=ORIENTED_EDGE('',*,*,#18965,.F.);
#26342=ORIENTED_EDGE('',*,*,#18928,.F.);
#26343=ORIENTED_EDGE('',*,*,#18933,.F.);
#26344=ORIENTED_EDGE('',*,*,#18935,.F.);
#26345=ORIENTED_EDGE('',*,*,#18937,.F.);
#26346=ORIENTED_EDGE('',*,*,#18939,.F.);
#26347=ORIENTED_EDGE('',*,*,#18941,.F.);
#26348=ORIENTED_EDGE('',*,*,#18952,.F.);
#26349=ORIENTED_EDGE('',*,*,#18991,.F.);
#26350=ORIENTED_EDGE('',*,*,#18992,.F.);
#26351=ORIENTED_EDGE('',*,*,#18993,.F.);
#26352=ORIENTED_EDGE('',*,*,#18994,.F.);
#26353=ORIENTED_EDGE('',*,*,#18995,.F.);
#26354=ORIENTED_EDGE('',*,*,#18996,.F.);
#26355=ORIENTED_EDGE('',*,*,#18997,.F.);
#26356=ORIENTED_EDGE('',*,*,#18998,.F.);
#26357=ORIENTED_EDGE('',*,*,#18999,.F.);
#26358=ORIENTED_EDGE('',*,*,#18947,.T.);
#26359=ORIENTED_EDGE('',*,*,#18943,.F.);
#26360=ORIENTED_EDGE('',*,*,#19000,.F.);
#26361=ORIENTED_EDGE('',*,*,#18842,.T.);
#26362=ORIENTED_EDGE('',*,*,#19001,.T.);
#26363=ORIENTED_EDGE('',*,*,#19002,.F.);
#26364=ORIENTED_EDGE('',*,*,#19003,.F.);
#26365=ORIENTED_EDGE('',*,*,#19004,.F.);
#26366=ORIENTED_EDGE('',*,*,#19005,.F.);
#26367=ORIENTED_EDGE('',*,*,#19006,.F.);
#26368=ORIENTED_EDGE('',*,*,#18945,.F.);
#26369=ORIENTED_EDGE('',*,*,#19007,.F.);
#26370=ORIENTED_EDGE('',*,*,#18961,.F.);
#26371=ORIENTED_EDGE('',*,*,#19008,.F.);
#26372=ORIENTED_EDGE('',*,*,#19009,.F.);
#26373=ORIENTED_EDGE('',*,*,#19010,.F.);
#26374=ORIENTED_EDGE('',*,*,#19011,.F.);
#26375=ORIENTED_EDGE('',*,*,#19002,.T.);
#26376=ORIENTED_EDGE('',*,*,#19012,.T.);
#26377=ORIENTED_EDGE('',*,*,#19006,.T.);
#26378=ORIENTED_EDGE('',*,*,#19013,.T.);
#26379=ORIENTED_EDGE('',*,*,#18949,.F.);
#26380=ORIENTED_EDGE('',*,*,#18946,.F.);
#26381=ORIENTED_EDGE('',*,*,#18950,.T.);
#26382=ORIENTED_EDGE('',*,*,#19014,.T.);
#26383=ORIENTED_EDGE('',*,*,#19015,.F.);
#26384=ORIENTED_EDGE('',*,*,#19016,.T.);
#26385=ORIENTED_EDGE('',*,*,#19017,.T.);
#26386=ORIENTED_EDGE('',*,*,#18991,.T.);
#26387=ORIENTED_EDGE('',*,*,#18951,.F.);
#26388=ORIENTED_EDGE('',*,*,#18948,.F.);
#26389=ORIENTED_EDGE('',*,*,#19009,.T.);
#26390=ORIENTED_EDGE('',*,*,#19018,.T.);
#26391=ORIENTED_EDGE('',*,*,#18955,.F.);
#26392=ORIENTED_EDGE('',*,*,#19019,.F.);
#26393=ORIENTED_EDGE('',*,*,#19020,.T.);
#26394=ORIENTED_EDGE('',*,*,#18959,.T.);
#26395=ORIENTED_EDGE('',*,*,#18958,.T.);
#26396=ORIENTED_EDGE('',*,*,#18956,.F.);
#26397=ORIENTED_EDGE('',*,*,#19021,.T.);
#26398=ORIENTED_EDGE('',*,*,#19022,.T.);
#26399=ORIENTED_EDGE('',*,*,#19023,.T.);
#26400=ORIENTED_EDGE('',*,*,#18954,.F.);
#26401=ORIENTED_EDGE('',*,*,#18966,.T.);
#26402=ORIENTED_EDGE('',*,*,#18990,.T.);
#26403=ORIENTED_EDGE('',*,*,#19024,.F.);
#26404=ORIENTED_EDGE('',*,*,#18953,.F.);
#26405=ORIENTED_EDGE('',*,*,#19008,.T.);
#26406=ORIENTED_EDGE('',*,*,#18963,.T.);
#26407=ORIENTED_EDGE('',*,*,#18960,.F.);
#26408=ORIENTED_EDGE('',*,*,#19025,.F.);
#26409=ORIENTED_EDGE('',*,*,#19007,.T.);
#26410=ORIENTED_EDGE('',*,*,#19000,.T.);
#26411=ORIENTED_EDGE('',*,*,#18964,.F.);
#26412=ORIENTED_EDGE('',*,*,#18962,.F.);
#26413=ORIENTED_EDGE('',*,*,#18999,.T.);
#26414=ORIENTED_EDGE('',*,*,#19026,.F.);
#26415=ORIENTED_EDGE('',*,*,#19027,.F.);
#26416=ORIENTED_EDGE('',*,*,#19028,.F.);
#26417=ORIENTED_EDGE('',*,*,#19026,.T.);
#26418=ORIENTED_EDGE('',*,*,#18998,.T.);
#26419=ORIENTED_EDGE('',*,*,#19029,.F.);
#26420=ORIENTED_EDGE('',*,*,#19030,.F.);
#26421=ORIENTED_EDGE('',*,*,#19029,.T.);
#26422=ORIENTED_EDGE('',*,*,#18997,.T.);
#26423=ORIENTED_EDGE('',*,*,#19031,.F.);
#26424=ORIENTED_EDGE('',*,*,#19032,.F.);
#26425=ORIENTED_EDGE('',*,*,#19031,.T.);
#26426=ORIENTED_EDGE('',*,*,#18996,.T.);
#26427=ORIENTED_EDGE('',*,*,#19033,.F.);
#26428=ORIENTED_EDGE('',*,*,#19034,.F.);
#26429=ORIENTED_EDGE('',*,*,#19033,.T.);
#26430=ORIENTED_EDGE('',*,*,#18995,.T.);
#26431=ORIENTED_EDGE('',*,*,#19035,.F.);
#26432=ORIENTED_EDGE('',*,*,#19036,.F.);
#26433=ORIENTED_EDGE('',*,*,#19037,.T.);
#26434=ORIENTED_EDGE('',*,*,#18994,.T.);
#26435=ORIENTED_EDGE('',*,*,#19038,.F.);
#26436=ORIENTED_EDGE('',*,*,#19039,.F.);
#26437=ORIENTED_EDGE('',*,*,#19038,.T.);
#26438=ORIENTED_EDGE('',*,*,#18993,.T.);
#26439=ORIENTED_EDGE('',*,*,#19040,.F.);
#26440=ORIENTED_EDGE('',*,*,#19041,.F.);
#26441=ORIENTED_EDGE('',*,*,#19040,.T.);
#26442=ORIENTED_EDGE('',*,*,#18992,.T.);
#26443=ORIENTED_EDGE('',*,*,#19017,.F.);
#26444=ORIENTED_EDGE('',*,*,#19016,.F.);
#26445=ORIENTED_EDGE('',*,*,#19024,.T.);
#26446=ORIENTED_EDGE('',*,*,#18989,.T.);
#26447=ORIENTED_EDGE('',*,*,#19042,.F.);
#26448=ORIENTED_EDGE('',*,*,#19021,.F.);
#26449=ORIENTED_EDGE('',*,*,#19042,.T.);
#26450=ORIENTED_EDGE('',*,*,#18988,.T.);
#26451=ORIENTED_EDGE('',*,*,#19043,.F.);
#26452=ORIENTED_EDGE('',*,*,#19044,.F.);
#26453=ORIENTED_EDGE('',*,*,#19043,.T.);
#26454=ORIENTED_EDGE('',*,*,#18987,.T.);
#26455=ORIENTED_EDGE('',*,*,#19045,.F.);
#26456=ORIENTED_EDGE('',*,*,#19046,.F.);
#26457=ORIENTED_EDGE('',*,*,#19045,.T.);
#26458=ORIENTED_EDGE('',*,*,#18986,.T.);
#26459=ORIENTED_EDGE('',*,*,#19047,.F.);
#26460=ORIENTED_EDGE('',*,*,#19048,.F.);
#26461=ORIENTED_EDGE('',*,*,#19049,.T.);
#26462=ORIENTED_EDGE('',*,*,#18985,.T.);
#26463=ORIENTED_EDGE('',*,*,#19050,.F.);
#26464=ORIENTED_EDGE('',*,*,#19051,.F.);
#26465=ORIENTED_EDGE('',*,*,#19050,.T.);
#26466=ORIENTED_EDGE('',*,*,#18984,.T.);
#26467=ORIENTED_EDGE('',*,*,#19052,.F.);
#26468=ORIENTED_EDGE('',*,*,#19053,.F.);
#26469=ORIENTED_EDGE('',*,*,#19052,.T.);
#26470=ORIENTED_EDGE('',*,*,#18983,.T.);
#26471=ORIENTED_EDGE('',*,*,#19054,.F.);
#26472=ORIENTED_EDGE('',*,*,#19055,.F.);
#26473=ORIENTED_EDGE('',*,*,#19054,.T.);
#26474=ORIENTED_EDGE('',*,*,#18982,.T.);
#26475=ORIENTED_EDGE('',*,*,#19056,.F.);
#26476=ORIENTED_EDGE('',*,*,#19057,.F.);
#26477=ORIENTED_EDGE('',*,*,#19056,.T.);
#26478=ORIENTED_EDGE('',*,*,#18981,.T.);
#26479=ORIENTED_EDGE('',*,*,#19058,.F.);
#26480=ORIENTED_EDGE('',*,*,#19059,.F.);
#26481=ORIENTED_EDGE('',*,*,#19058,.T.);
#26482=ORIENTED_EDGE('',*,*,#18980,.T.);
#26483=ORIENTED_EDGE('',*,*,#19060,.F.);
#26484=ORIENTED_EDGE('',*,*,#19061,.F.);
#26485=ORIENTED_EDGE('',*,*,#19060,.T.);
#26486=ORIENTED_EDGE('',*,*,#18979,.T.);
#26487=ORIENTED_EDGE('',*,*,#19062,.F.);
#26488=ORIENTED_EDGE('',*,*,#19063,.F.);
#26489=ORIENTED_EDGE('',*,*,#19062,.T.);
#26490=ORIENTED_EDGE('',*,*,#18978,.T.);
#26491=ORIENTED_EDGE('',*,*,#19064,.F.);
#26492=ORIENTED_EDGE('',*,*,#19065,.F.);
#26493=ORIENTED_EDGE('',*,*,#19064,.T.);
#26494=ORIENTED_EDGE('',*,*,#18977,.T.);
#26495=ORIENTED_EDGE('',*,*,#19066,.F.);
#26496=ORIENTED_EDGE('',*,*,#19067,.F.);
#26497=ORIENTED_EDGE('',*,*,#19066,.T.);
#26498=ORIENTED_EDGE('',*,*,#18976,.T.);
#26499=ORIENTED_EDGE('',*,*,#19068,.F.);
#26500=ORIENTED_EDGE('',*,*,#19069,.F.);
#26501=ORIENTED_EDGE('',*,*,#19068,.T.);
#26502=ORIENTED_EDGE('',*,*,#18975,.T.);
#26503=ORIENTED_EDGE('',*,*,#19070,.F.);
#26504=ORIENTED_EDGE('',*,*,#19071,.F.);
#26505=ORIENTED_EDGE('',*,*,#19072,.T.);
#26506=ORIENTED_EDGE('',*,*,#18974,.T.);
#26507=ORIENTED_EDGE('',*,*,#19073,.F.);
#26508=ORIENTED_EDGE('',*,*,#19074,.F.);
#26509=ORIENTED_EDGE('',*,*,#19075,.T.);
#26510=ORIENTED_EDGE('',*,*,#18973,.T.);
#26511=ORIENTED_EDGE('',*,*,#19076,.F.);
#26512=ORIENTED_EDGE('',*,*,#19077,.F.);
#26513=ORIENTED_EDGE('',*,*,#19076,.T.);
#26514=ORIENTED_EDGE('',*,*,#18972,.T.);
#26515=ORIENTED_EDGE('',*,*,#19078,.F.);
#26516=ORIENTED_EDGE('',*,*,#19079,.F.);
#26517=ORIENTED_EDGE('',*,*,#19078,.T.);
#26518=ORIENTED_EDGE('',*,*,#18971,.T.);
#26519=ORIENTED_EDGE('',*,*,#19080,.F.);
#26520=ORIENTED_EDGE('',*,*,#19081,.F.);
#26521=ORIENTED_EDGE('',*,*,#19082,.T.);
#26522=ORIENTED_EDGE('',*,*,#18970,.T.);
#26523=ORIENTED_EDGE('',*,*,#19083,.F.);
#26524=ORIENTED_EDGE('',*,*,#19084,.F.);
#26525=ORIENTED_EDGE('',*,*,#19085,.T.);
#26526=ORIENTED_EDGE('',*,*,#18969,.T.);
#26527=ORIENTED_EDGE('',*,*,#19086,.F.);
#26528=ORIENTED_EDGE('',*,*,#19087,.F.);
#26529=ORIENTED_EDGE('',*,*,#19086,.T.);
#26530=ORIENTED_EDGE('',*,*,#18968,.T.);
#26531=ORIENTED_EDGE('',*,*,#19088,.F.);
#26532=ORIENTED_EDGE('',*,*,#19089,.F.);
#26533=ORIENTED_EDGE('',*,*,#19090,.F.);
#26534=ORIENTED_EDGE('',*,*,#19088,.T.);
#26535=ORIENTED_EDGE('',*,*,#18967,.T.);
#26536=ORIENTED_EDGE('',*,*,#19028,.T.);
#26537=ORIENTED_EDGE('',*,*,#19091,.T.);
#26538=ORIENTED_EDGE('',*,*,#19092,.T.);
#26539=ORIENTED_EDGE('',*,*,#19093,.T.);
#26540=ORIENTED_EDGE('',*,*,#19012,.F.);
#26541=ORIENTED_EDGE('',*,*,#19093,.F.);
#26542=ORIENTED_EDGE('',*,*,#19010,.T.);
#26543=ORIENTED_EDGE('',*,*,#19019,.T.);
#26544=ORIENTED_EDGE('',*,*,#19023,.F.);
#26545=ORIENTED_EDGE('',*,*,#19094,.F.);
#26546=ORIENTED_EDGE('',*,*,#18846,.T.);
#26547=ORIENTED_EDGE('',*,*,#19095,.T.);
#26548=ORIENTED_EDGE('',*,*,#19096,.F.);
#26549=ORIENTED_EDGE('',*,*,#19097,.F.);
#26550=ORIENTED_EDGE('',*,*,#19096,.T.);
#26551=ORIENTED_EDGE('',*,*,#19098,.F.);
#26552=ORIENTED_EDGE('',*,*,#19051,.T.);
#26553=ORIENTED_EDGE('',*,*,#19099,.T.);
#26554=ORIENTED_EDGE('',*,*,#18849,.T.);
#26555=ORIENTED_EDGE('',*,*,#19100,.T.);
#26556=ORIENTED_EDGE('',*,*,#19101,.F.);
#26557=ORIENTED_EDGE('',*,*,#19102,.F.);
#26558=ORIENTED_EDGE('',*,*,#19101,.T.);
#26559=ORIENTED_EDGE('',*,*,#19103,.T.);
#26560=ORIENTED_EDGE('',*,*,#19104,.F.);
#26561=ORIENTED_EDGE('',*,*,#19105,.T.);
#26562=ORIENTED_EDGE('',*,*,#18839,.T.);
#26563=ORIENTED_EDGE('',*,*,#19106,.T.);
#26564=ORIENTED_EDGE('',*,*,#19107,.F.);
#26565=ORIENTED_EDGE('',*,*,#19108,.F.);
#26566=ORIENTED_EDGE('',*,*,#19107,.T.);
#26567=ORIENTED_EDGE('',*,*,#19109,.F.);
#26568=ORIENTED_EDGE('',*,*,#19036,.T.);
#26569=ORIENTED_EDGE('',*,*,#19110,.T.);
#26570=ORIENTED_EDGE('',*,*,#18856,.T.);
#26571=ORIENTED_EDGE('',*,*,#19111,.T.);
#26572=ORIENTED_EDGE('',*,*,#19112,.F.);
#26573=ORIENTED_EDGE('',*,*,#19113,.F.);
#26574=ORIENTED_EDGE('',*,*,#19112,.T.);
#26575=ORIENTED_EDGE('',*,*,#19114,.F.);
#26576=ORIENTED_EDGE('',*,*,#19115,.F.);
#26577=ORIENTED_EDGE('',*,*,#19116,.F.);
#26578=ORIENTED_EDGE('',*,*,#19003,.T.);
#26579=ORIENTED_EDGE('',*,*,#19117,.F.);
#26580=ORIENTED_EDGE('',*,*,#19118,.F.);
#26581=ORIENTED_EDGE('',*,*,#19117,.T.);
#26582=ORIENTED_EDGE('',*,*,#19011,.T.);
#26583=ORIENTED_EDGE('',*,*,#19094,.T.);
#26584=ORIENTED_EDGE('',*,*,#19119,.F.);
#26585=ORIENTED_EDGE('',*,*,#19120,.T.);
#26586=ORIENTED_EDGE('',*,*,#19121,.F.);
#26587=ORIENTED_EDGE('',*,*,#19001,.F.);
#26588=ORIENTED_EDGE('',*,*,#19121,.T.);
#26589=ORIENTED_EDGE('',*,*,#19122,.F.);
#26590=ORIENTED_EDGE('',*,*,#19123,.F.);
#26591=ORIENTED_EDGE('',*,*,#19004,.T.);
#26592=ORIENTED_EDGE('',*,*,#19005,.T.);
#26593=ORIENTED_EDGE('',*,*,#19123,.T.);
#26594=ORIENTED_EDGE('',*,*,#19014,.F.);
#26595=ORIENTED_EDGE('',*,*,#19013,.F.);
#26596=ORIENTED_EDGE('',*,*,#18841,.T.);
#26597=ORIENTED_EDGE('',*,*,#18808,.T.);
#26598=ORIENTED_EDGE('',*,*,#18807,.T.);
#26599=ORIENTED_EDGE('',*,*,#19124,.F.);
#26600=ORIENTED_EDGE('',*,*,#19120,.F.);
#26601=ORIENTED_EDGE('',*,*,#19125,.F.);
#26602=ORIENTED_EDGE('',*,*,#19041,.T.);
#26603=ORIENTED_EDGE('',*,*,#19015,.T.);
#26604=ORIENTED_EDGE('',*,*,#19122,.T.);
#26605=ORIENTED_EDGE('',*,*,#19124,.T.);
#26606=ORIENTED_EDGE('',*,*,#19025,.T.);
#26607=ORIENTED_EDGE('',*,*,#19020,.F.);
#26608=ORIENTED_EDGE('',*,*,#19018,.F.);
#26609=ORIENTED_EDGE('',*,*,#18843,.T.);
#26610=ORIENTED_EDGE('',*,*,#19118,.T.);
#26611=ORIENTED_EDGE('',*,*,#19126,.F.);
#26612=ORIENTED_EDGE('',*,*,#19127,.F.);
#26613=ORIENTED_EDGE('',*,*,#19126,.T.);
#26614=ORIENTED_EDGE('',*,*,#19119,.T.);
#26615=ORIENTED_EDGE('',*,*,#19022,.F.);
#26616=ORIENTED_EDGE('',*,*,#19044,.T.);
#26617=ORIENTED_EDGE('',*,*,#19128,.T.);
#26618=ORIENTED_EDGE('',*,*,#19027,.T.);
#26619=ORIENTED_EDGE('',*,*,#19129,.T.);
#26620=ORIENTED_EDGE('',*,*,#19130,.F.);
#26621=ORIENTED_EDGE('',*,*,#19131,.F.);
#26622=ORIENTED_EDGE('',*,*,#19132,.T.);
#26623=ORIENTED_EDGE('',*,*,#19133,.F.);
#26624=ORIENTED_EDGE('',*,*,#19129,.F.);
#26625=ORIENTED_EDGE('',*,*,#19030,.T.);
#26626=ORIENTED_EDGE('',*,*,#18837,.T.);
#26627=ORIENTED_EDGE('',*,*,#19134,.T.);
#26628=ORIENTED_EDGE('',*,*,#19135,.F.);
#26629=ORIENTED_EDGE('',*,*,#19136,.F.);
#26630=ORIENTED_EDGE('',*,*,#19135,.T.);
#26631=ORIENTED_EDGE('',*,*,#19137,.T.);
#26632=ORIENTED_EDGE('',*,*,#19138,.F.);
#26633=ORIENTED_EDGE('',*,*,#19132,.F.);
#26634=ORIENTED_EDGE('',*,*,#19032,.T.);
#26635=ORIENTED_EDGE('',*,*,#19139,.T.);
#26636=ORIENTED_EDGE('',*,*,#18857,.T.);
#26637=ORIENTED_EDGE('',*,*,#19113,.T.);
#26638=ORIENTED_EDGE('',*,*,#19140,.F.);
#26639=ORIENTED_EDGE('',*,*,#19134,.F.);
#26640=ORIENTED_EDGE('',*,*,#19116,.T.);
#26641=ORIENTED_EDGE('',*,*,#19141,.F.);
#26642=ORIENTED_EDGE('',*,*,#19137,.F.);
#26643=ORIENTED_EDGE('',*,*,#19140,.T.);
#26644=ORIENTED_EDGE('',*,*,#18838,.T.);
#26645=ORIENTED_EDGE('',*,*,#19136,.T.);
#26646=ORIENTED_EDGE('',*,*,#19142,.F.);
#26647=ORIENTED_EDGE('',*,*,#19106,.F.);
#26648=ORIENTED_EDGE('',*,*,#19139,.F.);
#26649=ORIENTED_EDGE('',*,*,#19034,.T.);
#26650=ORIENTED_EDGE('',*,*,#19109,.T.);
#26651=ORIENTED_EDGE('',*,*,#19142,.T.);
#26652=ORIENTED_EDGE('',*,*,#19035,.T.);
#26653=ORIENTED_EDGE('',*,*,#19037,.F.);
#26654=ORIENTED_EDGE('',*,*,#19143,.F.);
#26655=ORIENTED_EDGE('',*,*,#19144,.F.);
#26656=ORIENTED_EDGE('',*,*,#19039,.T.);
#26657=ORIENTED_EDGE('',*,*,#19125,.T.);
#26658=ORIENTED_EDGE('',*,*,#18806,.T.);
#26659=ORIENTED_EDGE('',*,*,#18844,.T.);
#26660=ORIENTED_EDGE('',*,*,#19127,.T.);
#26661=ORIENTED_EDGE('',*,*,#19145,.F.);
#26662=ORIENTED_EDGE('',*,*,#18799,.F.);
#26663=ORIENTED_EDGE('',*,*,#18798,.F.);
#26664=ORIENTED_EDGE('',*,*,#19128,.F.);
#26665=ORIENTED_EDGE('',*,*,#19046,.T.);
#26666=ORIENTED_EDGE('',*,*,#19146,.T.);
#26667=ORIENTED_EDGE('',*,*,#19145,.T.);
#26668=ORIENTED_EDGE('',*,*,#19146,.F.);
#26669=ORIENTED_EDGE('',*,*,#19048,.T.);
#26670=ORIENTED_EDGE('',*,*,#19147,.T.);
#26671=ORIENTED_EDGE('',*,*,#18800,.T.);
#26672=ORIENTED_EDGE('',*,*,#19047,.T.);
#26673=ORIENTED_EDGE('',*,*,#19049,.F.);
#26674=ORIENTED_EDGE('',*,*,#19148,.F.);
#26675=ORIENTED_EDGE('',*,*,#18847,.T.);
#26676=ORIENTED_EDGE('',*,*,#19097,.T.);
#26677=ORIENTED_EDGE('',*,*,#19149,.F.);
#26678=ORIENTED_EDGE('',*,*,#18793,.F.);
#26679=ORIENTED_EDGE('',*,*,#18792,.F.);
#26680=ORIENTED_EDGE('',*,*,#19099,.F.);
#26681=ORIENTED_EDGE('',*,*,#19053,.T.);
#26682=ORIENTED_EDGE('',*,*,#19150,.T.);
#26683=ORIENTED_EDGE('',*,*,#19149,.T.);
#26684=ORIENTED_EDGE('',*,*,#18848,.T.);
#26685=ORIENTED_EDGE('',*,*,#18796,.T.);
#26686=ORIENTED_EDGE('',*,*,#18795,.T.);
#26687=ORIENTED_EDGE('',*,*,#19151,.F.);
#26688=ORIENTED_EDGE('',*,*,#19100,.F.);
#26689=ORIENTED_EDGE('',*,*,#19152,.T.);
#26690=ORIENTED_EDGE('',*,*,#19153,.F.);
#26691=ORIENTED_EDGE('',*,*,#19103,.F.);
#26692=ORIENTED_EDGE('',*,*,#19151,.T.);
#26693=ORIENTED_EDGE('',*,*,#19150,.F.);
#26694=ORIENTED_EDGE('',*,*,#19055,.T.);
#26695=ORIENTED_EDGE('',*,*,#19154,.T.);
#26696=ORIENTED_EDGE('',*,*,#19155,.F.);
#26697=ORIENTED_EDGE('',*,*,#19152,.F.);
#26698=ORIENTED_EDGE('',*,*,#18794,.T.);
#26699=ORIENTED_EDGE('',*,*,#19156,.T.);
#26700=ORIENTED_EDGE('',*,*,#19157,.F.);
#26701=ORIENTED_EDGE('',*,*,#19154,.F.);
#26702=ORIENTED_EDGE('',*,*,#19057,.T.);
#26703=ORIENTED_EDGE('',*,*,#19158,.T.);
#26704=ORIENTED_EDGE('',*,*,#19159,.F.);
#26705=ORIENTED_EDGE('',*,*,#19156,.F.);
#26706=ORIENTED_EDGE('',*,*,#19059,.T.);
#26707=ORIENTED_EDGE('',*,*,#19160,.T.);
#26708=ORIENTED_EDGE('',*,*,#19161,.F.);
#26709=ORIENTED_EDGE('',*,*,#19158,.F.);
#26710=ORIENTED_EDGE('',*,*,#19061,.T.);
#26711=ORIENTED_EDGE('',*,*,#19162,.F.);
#26712=ORIENTED_EDGE('',*,*,#19163,.F.);
#26713=ORIENTED_EDGE('',*,*,#19160,.F.);
#26714=ORIENTED_EDGE('',*,*,#19063,.T.);
#26715=ORIENTED_EDGE('',*,*,#19065,.T.);
#26716=ORIENTED_EDGE('',*,*,#19164,.F.);
#26717=ORIENTED_EDGE('',*,*,#19165,.F.);
#26718=ORIENTED_EDGE('',*,*,#19162,.T.);
#26719=ORIENTED_EDGE('',*,*,#19166,.F.);
#26720=ORIENTED_EDGE('',*,*,#19167,.F.);
#26721=ORIENTED_EDGE('',*,*,#19164,.T.);
#26722=ORIENTED_EDGE('',*,*,#19067,.T.);
#26723=ORIENTED_EDGE('',*,*,#19069,.T.);
#26724=ORIENTED_EDGE('',*,*,#19168,.F.);
#26725=ORIENTED_EDGE('',*,*,#19169,.F.);
#26726=ORIENTED_EDGE('',*,*,#19166,.T.);
#26727=ORIENTED_EDGE('',*,*,#19170,.T.);
#26728=ORIENTED_EDGE('',*,*,#19171,.F.);
#26729=ORIENTED_EDGE('',*,*,#19168,.T.);
#26730=ORIENTED_EDGE('',*,*,#19071,.T.);
#26731=ORIENTED_EDGE('',*,*,#19070,.T.);
#26732=ORIENTED_EDGE('',*,*,#19072,.F.);
#26733=ORIENTED_EDGE('',*,*,#19172,.F.);
#26734=ORIENTED_EDGE('',*,*,#19173,.T.);
#26735=ORIENTED_EDGE('',*,*,#19174,.F.);
#26736=ORIENTED_EDGE('',*,*,#19175,.F.);
#26737=ORIENTED_EDGE('',*,*,#19074,.T.);
#26738=ORIENTED_EDGE('',*,*,#19073,.T.);
#26739=ORIENTED_EDGE('',*,*,#19075,.F.);
#26740=ORIENTED_EDGE('',*,*,#19176,.F.);
#26741=ORIENTED_EDGE('',*,*,#19177,.F.);
#26742=ORIENTED_EDGE('',*,*,#19178,.F.);
#26743=ORIENTED_EDGE('',*,*,#19179,.F.);
#26744=ORIENTED_EDGE('',*,*,#19077,.T.);
#26745=ORIENTED_EDGE('',*,*,#19079,.T.);
#26746=ORIENTED_EDGE('',*,*,#19180,.F.);
#26747=ORIENTED_EDGE('',*,*,#19181,.F.);
#26748=ORIENTED_EDGE('',*,*,#19177,.T.);
#26749=ORIENTED_EDGE('',*,*,#19182,.T.);
#26750=ORIENTED_EDGE('',*,*,#19183,.F.);
#26751=ORIENTED_EDGE('',*,*,#19180,.T.);
#26752=ORIENTED_EDGE('',*,*,#19081,.T.);
#26753=ORIENTED_EDGE('',*,*,#19080,.T.);
#26754=ORIENTED_EDGE('',*,*,#19082,.F.);
#26755=ORIENTED_EDGE('',*,*,#19184,.F.);
#26756=ORIENTED_EDGE('',*,*,#19185,.T.);
#26757=ORIENTED_EDGE('',*,*,#19186,.F.);
#26758=ORIENTED_EDGE('',*,*,#19187,.F.);
#26759=ORIENTED_EDGE('',*,*,#19084,.T.);
#26760=ORIENTED_EDGE('',*,*,#19083,.T.);
#26761=ORIENTED_EDGE('',*,*,#19085,.F.);
#26762=ORIENTED_EDGE('',*,*,#19188,.F.);
#26763=ORIENTED_EDGE('',*,*,#19087,.T.);
#26764=ORIENTED_EDGE('',*,*,#19189,.F.);
#26765=ORIENTED_EDGE('',*,*,#19190,.F.);
#26766=ORIENTED_EDGE('',*,*,#19191,.F.);
#26767=ORIENTED_EDGE('',*,*,#19089,.T.);
#26768=ORIENTED_EDGE('',*,*,#19192,.F.);
#26769=ORIENTED_EDGE('',*,*,#19193,.F.);
#26770=ORIENTED_EDGE('',*,*,#19189,.T.);
#26771=ORIENTED_EDGE('',*,*,#19131,.T.);
#26772=ORIENTED_EDGE('',*,*,#19194,.F.);
#26773=ORIENTED_EDGE('',*,*,#19192,.T.);
#26774=ORIENTED_EDGE('',*,*,#19090,.T.);
#26775=ORIENTED_EDGE('',*,*,#19195,.T.);
#26776=ORIENTED_EDGE('',*,*,#19196,.T.);
#26777=ORIENTED_EDGE('',*,*,#19091,.F.);
#26778=ORIENTED_EDGE('',*,*,#19092,.F.);
#26779=ORIENTED_EDGE('',*,*,#19196,.F.);
#26780=ORIENTED_EDGE('',*,*,#19104,.T.);
#26781=ORIENTED_EDGE('',*,*,#19197,.T.);
#26782=ORIENTED_EDGE('',*,*,#19198,.F.);
#26783=ORIENTED_EDGE('',*,*,#19199,.F.);
#26784=ORIENTED_EDGE('',*,*,#18850,.T.);
#26785=ORIENTED_EDGE('',*,*,#19102,.T.);
#26786=ORIENTED_EDGE('',*,*,#19200,.F.);
#26787=ORIENTED_EDGE('',*,*,#18790,.F.);
#26788=ORIENTED_EDGE('',*,*,#18789,.F.);
#26789=ORIENTED_EDGE('',*,*,#19105,.F.);
#26790=ORIENTED_EDGE('',*,*,#19201,.F.);
#26791=ORIENTED_EDGE('',*,*,#19202,.T.);
#26792=ORIENTED_EDGE('',*,*,#19200,.T.);
#26793=ORIENTED_EDGE('',*,*,#18853,.T.);
#26794=ORIENTED_EDGE('',*,*,#19203,.T.);
#26795=ORIENTED_EDGE('',*,*,#19204,.F.);
#26796=ORIENTED_EDGE('',*,*,#19205,.F.);
#26797=ORIENTED_EDGE('',*,*,#19204,.T.);
#26798=ORIENTED_EDGE('',*,*,#19206,.T.);
#26799=ORIENTED_EDGE('',*,*,#19207,.T.);
#26800=ORIENTED_EDGE('',*,*,#19208,.T.);
#26801=ORIENTED_EDGE('',*,*,#19209,.T.);
#26802=ORIENTED_EDGE('',*,*,#19210,.T.);
#26803=ORIENTED_EDGE('',*,*,#19211,.T.);
#26804=ORIENTED_EDGE('',*,*,#19212,.T.);
#26805=ORIENTED_EDGE('',*,*,#19213,.T.);
#26806=ORIENTED_EDGE('',*,*,#19214,.T.);
#26807=ORIENTED_EDGE('',*,*,#19215,.T.);
#26808=ORIENTED_EDGE('',*,*,#19216,.F.);
#26809=ORIENTED_EDGE('',*,*,#18855,.T.);
#26810=ORIENTED_EDGE('',*,*,#18781,.T.);
#26811=ORIENTED_EDGE('',*,*,#18780,.T.);
#26812=ORIENTED_EDGE('',*,*,#19217,.F.);
#26813=ORIENTED_EDGE('',*,*,#19111,.F.);
#26814=ORIENTED_EDGE('',*,*,#19218,.F.);
#26815=ORIENTED_EDGE('',*,*,#19219,.F.);
#26816=ORIENTED_EDGE('',*,*,#19114,.T.);
#26817=ORIENTED_EDGE('',*,*,#19217,.T.);
#26818=ORIENTED_EDGE('',*,*,#19220,.T.);
#26819=ORIENTED_EDGE('',*,*,#19221,.T.);
#26820=ORIENTED_EDGE('',*,*,#19222,.F.);
#26821=ORIENTED_EDGE('',*,*,#18845,.T.);
#26822=ORIENTED_EDGE('',*,*,#18802,.T.);
#26823=ORIENTED_EDGE('',*,*,#18801,.T.);
#26824=ORIENTED_EDGE('',*,*,#19223,.F.);
#26825=ORIENTED_EDGE('',*,*,#19095,.F.);
#26826=ORIENTED_EDGE('',*,*,#19147,.F.);
#26827=ORIENTED_EDGE('',*,*,#19148,.T.);
#26828=ORIENTED_EDGE('',*,*,#19098,.T.);
#26829=ORIENTED_EDGE('',*,*,#19223,.T.);
#26830=ORIENTED_EDGE('',*,*,#18840,.T.);
#26831=ORIENTED_EDGE('',*,*,#19108,.T.);
#26832=ORIENTED_EDGE('',*,*,#19224,.F.);
#26833=ORIENTED_EDGE('',*,*,#18805,.F.);
#26834=ORIENTED_EDGE('',*,*,#18804,.F.);
#26835=ORIENTED_EDGE('',*,*,#19110,.F.);
#26836=ORIENTED_EDGE('',*,*,#19143,.T.);
#26837=ORIENTED_EDGE('',*,*,#19144,.T.);
#26838=ORIENTED_EDGE('',*,*,#19224,.T.);
#26839=ORIENTED_EDGE('',*,*,#19225,.T.);
#26840=ORIENTED_EDGE('',*,*,#19130,.T.);
#26841=ORIENTED_EDGE('',*,*,#19226,.T.);
#26842=ORIENTED_EDGE('',*,*,#19227,.F.);
#26843=ORIENTED_EDGE('',*,*,#19133,.T.);
#26844=ORIENTED_EDGE('',*,*,#19228,.T.);
#26845=ORIENTED_EDGE('',*,*,#19229,.F.);
#26846=ORIENTED_EDGE('',*,*,#19226,.F.);
#26847=ORIENTED_EDGE('',*,*,#19138,.T.);
#26848=ORIENTED_EDGE('',*,*,#19230,.T.);
#26849=ORIENTED_EDGE('',*,*,#19231,.F.);
#26850=ORIENTED_EDGE('',*,*,#19228,.F.);
#26851=ORIENTED_EDGE('',*,*,#19141,.T.);
#26852=ORIENTED_EDGE('',*,*,#19232,.T.);
#26853=ORIENTED_EDGE('',*,*,#19233,.F.);
#26854=ORIENTED_EDGE('',*,*,#19230,.F.);
#26855=ORIENTED_EDGE('',*,*,#19153,.T.);
#26856=ORIENTED_EDGE('',*,*,#19234,.T.);
#26857=ORIENTED_EDGE('',*,*,#19235,.F.);
#26858=ORIENTED_EDGE('',*,*,#19197,.F.);
#26859=ORIENTED_EDGE('',*,*,#19155,.T.);
#26860=ORIENTED_EDGE('',*,*,#19236,.T.);
#26861=ORIENTED_EDGE('',*,*,#19237,.F.);
#26862=ORIENTED_EDGE('',*,*,#19234,.F.);
#26863=ORIENTED_EDGE('',*,*,#19157,.T.);
#26864=ORIENTED_EDGE('',*,*,#19238,.T.);
#26865=ORIENTED_EDGE('',*,*,#19239,.F.);
#26866=ORIENTED_EDGE('',*,*,#19236,.F.);
#26867=ORIENTED_EDGE('',*,*,#19159,.T.);
#26868=ORIENTED_EDGE('',*,*,#19240,.T.);
#26869=ORIENTED_EDGE('',*,*,#19241,.F.);
#26870=ORIENTED_EDGE('',*,*,#19238,.F.);
#26871=ORIENTED_EDGE('',*,*,#19161,.T.);
#26872=ORIENTED_EDGE('',*,*,#19242,.T.);
#26873=ORIENTED_EDGE('',*,*,#19243,.F.);
#26874=ORIENTED_EDGE('',*,*,#19240,.F.);
#26875=ORIENTED_EDGE('',*,*,#19163,.T.);
#26876=ORIENTED_EDGE('',*,*,#19244,.T.);
#26877=ORIENTED_EDGE('',*,*,#19245,.F.);
#26878=ORIENTED_EDGE('',*,*,#19242,.F.);
#26879=ORIENTED_EDGE('',*,*,#19165,.T.);
#26880=ORIENTED_EDGE('',*,*,#19246,.T.);
#26881=ORIENTED_EDGE('',*,*,#19247,.F.);
#26882=ORIENTED_EDGE('',*,*,#19244,.F.);
#26883=ORIENTED_EDGE('',*,*,#19167,.T.);
#26884=ORIENTED_EDGE('',*,*,#19248,.T.);
#26885=ORIENTED_EDGE('',*,*,#19249,.F.);
#26886=ORIENTED_EDGE('',*,*,#19246,.F.);
#26887=ORIENTED_EDGE('',*,*,#19169,.T.);
#26888=ORIENTED_EDGE('',*,*,#19250,.T.);
#26889=ORIENTED_EDGE('',*,*,#19251,.F.);
#26890=ORIENTED_EDGE('',*,*,#19248,.F.);
#26891=ORIENTED_EDGE('',*,*,#19171,.T.);
#26892=ORIENTED_EDGE('',*,*,#19252,.T.);
#26893=ORIENTED_EDGE('',*,*,#19253,.F.);
#26894=ORIENTED_EDGE('',*,*,#19250,.F.);
#26895=ORIENTED_EDGE('',*,*,#19175,.T.);
#26896=ORIENTED_EDGE('',*,*,#19254,.F.);
#26897=ORIENTED_EDGE('',*,*,#19170,.F.);
#26898=ORIENTED_EDGE('',*,*,#19172,.T.);
#26899=ORIENTED_EDGE('',*,*,#19174,.T.);
#26900=ORIENTED_EDGE('',*,*,#19255,.T.);
#26901=ORIENTED_EDGE('',*,*,#19256,.F.);
#26902=ORIENTED_EDGE('',*,*,#19257,.F.);
#26903=ORIENTED_EDGE('',*,*,#19179,.T.);
#26904=ORIENTED_EDGE('',*,*,#19258,.F.);
#26905=ORIENTED_EDGE('',*,*,#19173,.F.);
#26906=ORIENTED_EDGE('',*,*,#19176,.T.);
#26907=ORIENTED_EDGE('',*,*,#19178,.T.);
#26908=ORIENTED_EDGE('',*,*,#19259,.T.);
#26909=ORIENTED_EDGE('',*,*,#19260,.F.);
#26910=ORIENTED_EDGE('',*,*,#19261,.F.);
#26911=ORIENTED_EDGE('',*,*,#19181,.T.);
#26912=ORIENTED_EDGE('',*,*,#19262,.T.);
#26913=ORIENTED_EDGE('',*,*,#19263,.F.);
#26914=ORIENTED_EDGE('',*,*,#19259,.F.);
#26915=ORIENTED_EDGE('',*,*,#19183,.T.);
#26916=ORIENTED_EDGE('',*,*,#19264,.T.);
#26917=ORIENTED_EDGE('',*,*,#19265,.F.);
#26918=ORIENTED_EDGE('',*,*,#19262,.F.);
#26919=ORIENTED_EDGE('',*,*,#19187,.T.);
#26920=ORIENTED_EDGE('',*,*,#19266,.F.);
#26921=ORIENTED_EDGE('',*,*,#19182,.F.);
#26922=ORIENTED_EDGE('',*,*,#19184,.T.);
#26923=ORIENTED_EDGE('',*,*,#19186,.T.);
#26924=ORIENTED_EDGE('',*,*,#19267,.T.);
#26925=ORIENTED_EDGE('',*,*,#19268,.F.);
#26926=ORIENTED_EDGE('',*,*,#19269,.F.);
#26927=ORIENTED_EDGE('',*,*,#19191,.T.);
#26928=ORIENTED_EDGE('',*,*,#19270,.F.);
#26929=ORIENTED_EDGE('',*,*,#19185,.F.);
#26930=ORIENTED_EDGE('',*,*,#19188,.T.);
#26931=ORIENTED_EDGE('',*,*,#19190,.T.);
#26932=ORIENTED_EDGE('',*,*,#19271,.T.);
#26933=ORIENTED_EDGE('',*,*,#19272,.F.);
#26934=ORIENTED_EDGE('',*,*,#19273,.F.);
#26935=ORIENTED_EDGE('',*,*,#19193,.T.);
#26936=ORIENTED_EDGE('',*,*,#19274,.T.);
#26937=ORIENTED_EDGE('',*,*,#19275,.F.);
#26938=ORIENTED_EDGE('',*,*,#19271,.F.);
#26939=ORIENTED_EDGE('',*,*,#19225,.F.);
#26940=ORIENTED_EDGE('',*,*,#19276,.F.);
#26941=ORIENTED_EDGE('',*,*,#19274,.F.);
#26942=ORIENTED_EDGE('',*,*,#19194,.T.);
#26943=ORIENTED_EDGE('',*,*,#19195,.F.);
#26944=ORIENTED_EDGE('',*,*,#19277,.F.);
#26945=ORIENTED_EDGE('',*,*,#19201,.T.);
#26946=ORIENTED_EDGE('',*,*,#19199,.T.);
#26947=ORIENTED_EDGE('',*,*,#19278,.F.);
#26948=ORIENTED_EDGE('',*,*,#19279,.T.);
#26949=ORIENTED_EDGE('',*,*,#19280,.T.);
#26950=ORIENTED_EDGE('',*,*,#19281,.F.);
#26951=ORIENTED_EDGE('',*,*,#19282,.F.);
#26952=ORIENTED_EDGE('',*,*,#19280,.F.);
#26953=ORIENTED_EDGE('',*,*,#18791,.T.);
#26954=ORIENTED_EDGE('',*,*,#19202,.F.);
#26955=ORIENTED_EDGE('',*,*,#19283,.F.);
#26956=ORIENTED_EDGE('',*,*,#19284,.T.);
#26957=ORIENTED_EDGE('',*,*,#19285,.F.);
#26958=ORIENTED_EDGE('',*,*,#19286,.T.);
#26959=ORIENTED_EDGE('',*,*,#19216,.T.);
#26960=ORIENTED_EDGE('',*,*,#19286,.F.);
#26961=ORIENTED_EDGE('',*,*,#19287,.T.);
#26962=ORIENTED_EDGE('',*,*,#19288,.T.);
#26963=ORIENTED_EDGE('',*,*,#19289,.F.);
#26964=ORIENTED_EDGE('',*,*,#19208,.F.);
#26965=ORIENTED_EDGE('',*,*,#19290,.T.);
#26966=ORIENTED_EDGE('',*,*,#19291,.T.);
#26967=ORIENTED_EDGE('',*,*,#19287,.F.);
#26968=ORIENTED_EDGE('',*,*,#19207,.F.);
#26969=ORIENTED_EDGE('',*,*,#19292,.T.);
#26970=ORIENTED_EDGE('',*,*,#19293,.T.);
#26971=ORIENTED_EDGE('',*,*,#19294,.F.);
#26972=ORIENTED_EDGE('',*,*,#19213,.F.);
#26973=ORIENTED_EDGE('',*,*,#19222,.T.);
#26974=ORIENTED_EDGE('',*,*,#19295,.T.);
#26975=ORIENTED_EDGE('',*,*,#19292,.F.);
#26976=ORIENTED_EDGE('',*,*,#19212,.F.);
#26977=ORIENTED_EDGE('',*,*,#19296,.T.);
#26978=ORIENTED_EDGE('',*,*,#19297,.T.);
#26979=ORIENTED_EDGE('',*,*,#19220,.F.);
#26980=ORIENTED_EDGE('',*,*,#19211,.F.);
#26981=ORIENTED_EDGE('',*,*,#19298,.T.);
#26982=ORIENTED_EDGE('',*,*,#19299,.F.);
#26983=ORIENTED_EDGE('',*,*,#19203,.F.);
#26984=ORIENTED_EDGE('',*,*,#19299,.T.);
#26985=ORIENTED_EDGE('',*,*,#19300,.T.);
#26986=ORIENTED_EDGE('',*,*,#19290,.F.);
#26987=ORIENTED_EDGE('',*,*,#19206,.F.);
#26988=ORIENTED_EDGE('',*,*,#19205,.T.);
#26989=ORIENTED_EDGE('',*,*,#19301,.F.);
#26990=ORIENTED_EDGE('',*,*,#19302,.F.);
#26991=ORIENTED_EDGE('',*,*,#19215,.F.);
#26992=ORIENTED_EDGE('',*,*,#19303,.T.);
#26993=ORIENTED_EDGE('',*,*,#19304,.T.);
#26994=ORIENTED_EDGE('',*,*,#19301,.T.);
#26995=ORIENTED_EDGE('',*,*,#19294,.T.);
#26996=ORIENTED_EDGE('',*,*,#19305,.T.);
#26997=ORIENTED_EDGE('',*,*,#19303,.F.);
#26998=ORIENTED_EDGE('',*,*,#19214,.F.);
#26999=ORIENTED_EDGE('',*,*,#19306,.T.);
#27000=ORIENTED_EDGE('',*,*,#19307,.T.);
#27001=ORIENTED_EDGE('',*,*,#19308,.F.);
#27002=ORIENTED_EDGE('',*,*,#19209,.F.);
#27003=ORIENTED_EDGE('',*,*,#19308,.T.);
#27004=ORIENTED_EDGE('',*,*,#19309,.T.);
#27005=ORIENTED_EDGE('',*,*,#19296,.F.);
#27006=ORIENTED_EDGE('',*,*,#19210,.F.);
#27007=ORIENTED_EDGE('',*,*,#18785,.T.);
#27008=ORIENTED_EDGE('',*,*,#19310,.F.);
#27009=ORIENTED_EDGE('',*,*,#19311,.F.);
#27010=ORIENTED_EDGE('',*,*,#19218,.T.);
#27011=ORIENTED_EDGE('',*,*,#19282,.T.);
#27012=ORIENTED_EDGE('',*,*,#19312,.T.);
#27013=ORIENTED_EDGE('',*,*,#19313,.F.);
#27014=ORIENTED_EDGE('',*,*,#19314,.F.);
#27015=ORIENTED_EDGE('',*,*,#19315,.F.);
#27016=ORIENTED_EDGE('',*,*,#19312,.F.);
#27017=ORIENTED_EDGE('',*,*,#19281,.T.);
#27018=ORIENTED_EDGE('',*,*,#19254,.T.);
#27019=ORIENTED_EDGE('',*,*,#19257,.T.);
#27020=ORIENTED_EDGE('',*,*,#19252,.F.);
#27021=ORIENTED_EDGE('',*,*,#19258,.T.);
#27022=ORIENTED_EDGE('',*,*,#19261,.T.);
#27023=ORIENTED_EDGE('',*,*,#19255,.F.);
#27024=ORIENTED_EDGE('',*,*,#19266,.T.);
#27025=ORIENTED_EDGE('',*,*,#19269,.T.);
#27026=ORIENTED_EDGE('',*,*,#19264,.F.);
#27027=ORIENTED_EDGE('',*,*,#19270,.T.);
#27028=ORIENTED_EDGE('',*,*,#19273,.T.);
#27029=ORIENTED_EDGE('',*,*,#19267,.F.);
#27030=ORIENTED_EDGE('',*,*,#19316,.T.);
#27031=ORIENTED_EDGE('',*,*,#19317,.T.);
#27032=ORIENTED_EDGE('',*,*,#19277,.T.);
#27033=ORIENTED_EDGE('',*,*,#19317,.F.);
#27034=ORIENTED_EDGE('',*,*,#19283,.T.);
#27035=ORIENTED_EDGE('',*,*,#19278,.T.);
#27036=ORIENTED_EDGE('',*,*,#19318,.F.);
#27037=ORIENTED_EDGE('',*,*,#19319,.F.);
#27038=ORIENTED_EDGE('',*,*,#19320,.T.);
#27039=ORIENTED_EDGE('',*,*,#19319,.T.);
#27040=ORIENTED_EDGE('',*,*,#19321,.F.);
#27041=ORIENTED_EDGE('',*,*,#19322,.F.);
#27042=ORIENTED_EDGE('',*,*,#19323,.T.);
#27043=ORIENTED_EDGE('',*,*,#19322,.T.);
#27044=ORIENTED_EDGE('',*,*,#19324,.F.);
#27045=ORIENTED_EDGE('',*,*,#19325,.F.);
#27046=ORIENTED_EDGE('',*,*,#19326,.T.);
#27047=ORIENTED_EDGE('',*,*,#19325,.T.);
#27048=ORIENTED_EDGE('',*,*,#19327,.F.);
#27049=ORIENTED_EDGE('',*,*,#19328,.F.);
#27050=ORIENTED_EDGE('',*,*,#19329,.T.);
#27051=ORIENTED_EDGE('',*,*,#19328,.T.);
#27052=ORIENTED_EDGE('',*,*,#19330,.F.);
#27053=ORIENTED_EDGE('',*,*,#19331,.F.);
#27054=ORIENTED_EDGE('',*,*,#19289,.T.);
#27055=ORIENTED_EDGE('',*,*,#19332,.T.);
#27056=ORIENTED_EDGE('',*,*,#19306,.F.);
#27057=ORIENTED_EDGE('',*,*,#19333,.T.);
#27058=ORIENTED_EDGE('',*,*,#19291,.F.);
#27059=ORIENTED_EDGE('',*,*,#19334,.F.);
#27060=ORIENTED_EDGE('',*,*,#19326,.F.);
#27061=ORIENTED_EDGE('',*,*,#18852,.T.);
#27062=ORIENTED_EDGE('',*,*,#19335,.T.);
#27063=ORIENTED_EDGE('',*,*,#19336,.F.);
#27064=ORIENTED_EDGE('',*,*,#19298,.F.);
#27065=ORIENTED_EDGE('',*,*,#19336,.T.);
#27066=ORIENTED_EDGE('',*,*,#19337,.F.);
#27067=ORIENTED_EDGE('',*,*,#19323,.F.);
#27068=ORIENTED_EDGE('',*,*,#19334,.T.);
#27069=ORIENTED_EDGE('',*,*,#19300,.F.);
#27070=ORIENTED_EDGE('',*,*,#19279,.F.);
#27071=ORIENTED_EDGE('',*,*,#19338,.T.);
#27072=ORIENTED_EDGE('',*,*,#19339,.T.);
#27073=ORIENTED_EDGE('',*,*,#19338,.F.);
#27074=ORIENTED_EDGE('',*,*,#19313,.T.);
#27075=ORIENTED_EDGE('',*,*,#19315,.T.);
#27076=ORIENTED_EDGE('',*,*,#19314,.T.);
#27077=ORIENTED_EDGE('',*,*,#19316,.F.);
#27078=ORIENTED_EDGE('',*,*,#19340,.T.);
#27079=ORIENTED_EDGE('',*,*,#19341,.T.);
#27080=ORIENTED_EDGE('',*,*,#19342,.F.);
#27081=ORIENTED_EDGE('',*,*,#19343,.F.);
#27082=ORIENTED_EDGE('',*,*,#19344,.F.);
#27083=ORIENTED_EDGE('',*,*,#19345,.T.);
#27084=ORIENTED_EDGE('',*,*,#19346,.T.);
#27085=ORIENTED_EDGE('',*,*,#19221,.F.);
#27086=ORIENTED_EDGE('',*,*,#19347,.T.);
#27087=ORIENTED_EDGE('',*,*,#19348,.T.);
#27088=ORIENTED_EDGE('',*,*,#19349,.F.);
#27089=ORIENTED_EDGE('',*,*,#19350,.F.);
#27090=ORIENTED_EDGE('',*,*,#19342,.T.);
#27091=ORIENTED_EDGE('',*,*,#19351,.T.);
#27092=ORIENTED_EDGE('',*,*,#19347,.F.);
#27093=ORIENTED_EDGE('',*,*,#19352,.F.);
#27094=ORIENTED_EDGE('',*,*,#18851,.T.);
#27095=ORIENTED_EDGE('',*,*,#18787,.T.);
#27096=ORIENTED_EDGE('',*,*,#18786,.T.);
#27097=ORIENTED_EDGE('',*,*,#19353,.F.);
#27098=ORIENTED_EDGE('',*,*,#19335,.F.);
#27099=ORIENTED_EDGE('',*,*,#19284,.F.);
#27100=ORIENTED_EDGE('',*,*,#19320,.F.);
#27101=ORIENTED_EDGE('',*,*,#19337,.T.);
#27102=ORIENTED_EDGE('',*,*,#19353,.T.);
#27103=ORIENTED_EDGE('',*,*,#19285,.T.);
#27104=ORIENTED_EDGE('',*,*,#19354,.T.);
#27105=ORIENTED_EDGE('',*,*,#19339,.F.);
#27106=ORIENTED_EDGE('',*,*,#19354,.F.);
#27107=ORIENTED_EDGE('',*,*,#19349,.T.);
#27108=ORIENTED_EDGE('',*,*,#19355,.T.);
#27109=ORIENTED_EDGE('',*,*,#19356,.F.);
#27110=ORIENTED_EDGE('',*,*,#19357,.F.);
#27111=ORIENTED_EDGE('',*,*,#19358,.T.);
#27112=ORIENTED_EDGE('',*,*,#19359,.T.);
#27113=ORIENTED_EDGE('',*,*,#19360,.F.);
#27114=ORIENTED_EDGE('',*,*,#19361,.F.);
#27115=ORIENTED_EDGE('',*,*,#19362,.T.);
#27116=ORIENTED_EDGE('',*,*,#19361,.T.);
#27117=ORIENTED_EDGE('',*,*,#19363,.F.);
#27118=ORIENTED_EDGE('',*,*,#19364,.F.);
#27119=ORIENTED_EDGE('',*,*,#19227,.T.);
#27120=ORIENTED_EDGE('',*,*,#19229,.T.);
#27121=ORIENTED_EDGE('',*,*,#19231,.T.);
#27122=ORIENTED_EDGE('',*,*,#19233,.T.);
#27123=ORIENTED_EDGE('',*,*,#19365,.T.);
#27124=ORIENTED_EDGE('',*,*,#19366,.T.);
#27125=ORIENTED_EDGE('',*,*,#19367,.T.);
#27126=ORIENTED_EDGE('',*,*,#19363,.T.);
#27127=ORIENTED_EDGE('',*,*,#19360,.T.);
#27128=ORIENTED_EDGE('',*,*,#19368,.T.);
#27129=ORIENTED_EDGE('',*,*,#19369,.T.);
#27130=ORIENTED_EDGE('',*,*,#19370,.T.);
#27131=ORIENTED_EDGE('',*,*,#19371,.T.);
#27132=ORIENTED_EDGE('',*,*,#19372,.T.);
#27133=ORIENTED_EDGE('',*,*,#19373,.T.);
#27134=ORIENTED_EDGE('',*,*,#19374,.T.);
#27135=ORIENTED_EDGE('',*,*,#19375,.T.);
#27136=ORIENTED_EDGE('',*,*,#19330,.T.);
#27137=ORIENTED_EDGE('',*,*,#19327,.T.);
#27138=ORIENTED_EDGE('',*,*,#19324,.T.);
#27139=ORIENTED_EDGE('',*,*,#19321,.T.);
#27140=ORIENTED_EDGE('',*,*,#19318,.T.);
#27141=ORIENTED_EDGE('',*,*,#19198,.T.);
#27142=ORIENTED_EDGE('',*,*,#19235,.T.);
#27143=ORIENTED_EDGE('',*,*,#19237,.T.);
#27144=ORIENTED_EDGE('',*,*,#19239,.T.);
#27145=ORIENTED_EDGE('',*,*,#19241,.T.);
#27146=ORIENTED_EDGE('',*,*,#19243,.T.);
#27147=ORIENTED_EDGE('',*,*,#19245,.T.);
#27148=ORIENTED_EDGE('',*,*,#19247,.T.);
#27149=ORIENTED_EDGE('',*,*,#19249,.T.);
#27150=ORIENTED_EDGE('',*,*,#19251,.T.);
#27151=ORIENTED_EDGE('',*,*,#19253,.T.);
#27152=ORIENTED_EDGE('',*,*,#19256,.T.);
#27153=ORIENTED_EDGE('',*,*,#19260,.T.);
#27154=ORIENTED_EDGE('',*,*,#19263,.T.);
#27155=ORIENTED_EDGE('',*,*,#19265,.T.);
#27156=ORIENTED_EDGE('',*,*,#19268,.T.);
#27157=ORIENTED_EDGE('',*,*,#19272,.T.);
#27158=ORIENTED_EDGE('',*,*,#19275,.T.);
#27159=ORIENTED_EDGE('',*,*,#19276,.T.);
#27160=ORIENTED_EDGE('',*,*,#19115,.T.);
#27161=ORIENTED_EDGE('',*,*,#19376,.T.);
#27162=ORIENTED_EDGE('',*,*,#19365,.F.);
#27163=ORIENTED_EDGE('',*,*,#19232,.F.);
#27164=ORIENTED_EDGE('',*,*,#19219,.T.);
#27165=ORIENTED_EDGE('',*,*,#19377,.T.);
#27166=ORIENTED_EDGE('',*,*,#19376,.F.);
#27167=ORIENTED_EDGE('',*,*,#19311,.T.);
#27168=ORIENTED_EDGE('',*,*,#19378,.T.);
#27169=ORIENTED_EDGE('',*,*,#19366,.F.);
#27170=ORIENTED_EDGE('',*,*,#19377,.F.);
#27171=ORIENTED_EDGE('',*,*,#19379,.T.);
#27172=ORIENTED_EDGE('',*,*,#19364,.T.);
#27173=ORIENTED_EDGE('',*,*,#19367,.F.);
#27174=ORIENTED_EDGE('',*,*,#19378,.F.);
#27175=ORIENTED_EDGE('',*,*,#18854,.T.);
#27176=ORIENTED_EDGE('',*,*,#19302,.T.);
#27177=ORIENTED_EDGE('',*,*,#19380,.F.);
#27178=ORIENTED_EDGE('',*,*,#18784,.F.);
#27179=ORIENTED_EDGE('',*,*,#18783,.F.);
#27180=ORIENTED_EDGE('',*,*,#19304,.F.);
#27181=ORIENTED_EDGE('',*,*,#19381,.F.);
#27182=ORIENTED_EDGE('',*,*,#19379,.F.);
#27183=ORIENTED_EDGE('',*,*,#19310,.T.);
#27184=ORIENTED_EDGE('',*,*,#19380,.T.);
#27185=ORIENTED_EDGE('',*,*,#19362,.F.);
#27186=ORIENTED_EDGE('',*,*,#19381,.T.);
#27187=ORIENTED_EDGE('',*,*,#19305,.F.);
#27188=ORIENTED_EDGE('',*,*,#19382,.F.);
#27189=ORIENTED_EDGE('',*,*,#19382,.T.);
#27190=ORIENTED_EDGE('',*,*,#19293,.F.);
#27191=ORIENTED_EDGE('',*,*,#19383,.F.);
#27192=ORIENTED_EDGE('',*,*,#19358,.F.);
#27193=ORIENTED_EDGE('',*,*,#19384,.F.);
#27194=ORIENTED_EDGE('',*,*,#19383,.T.);
#27195=ORIENTED_EDGE('',*,*,#19295,.F.);
#27196=ORIENTED_EDGE('',*,*,#19346,.F.);
#27197=ORIENTED_EDGE('',*,*,#19385,.F.);
#27198=ORIENTED_EDGE('',*,*,#19386,.F.);
#27199=ORIENTED_EDGE('',*,*,#19387,.F.);
#27200=ORIENTED_EDGE('',*,*,#19388,.F.);
#27201=ORIENTED_EDGE('',*,*,#19384,.T.);
#27202=ORIENTED_EDGE('',*,*,#19389,.T.);
#27203=ORIENTED_EDGE('',*,*,#19368,.F.);
#27204=ORIENTED_EDGE('',*,*,#19359,.F.);
#27205=ORIENTED_EDGE('',*,*,#19390,.T.);
#27206=ORIENTED_EDGE('',*,*,#19391,.T.);
#27207=ORIENTED_EDGE('',*,*,#19369,.F.);
#27208=ORIENTED_EDGE('',*,*,#19389,.F.);
#27209=ORIENTED_EDGE('',*,*,#19392,.T.);
#27210=ORIENTED_EDGE('',*,*,#19393,.T.);
#27211=ORIENTED_EDGE('',*,*,#19370,.F.);
#27212=ORIENTED_EDGE('',*,*,#19391,.F.);
#27213=ORIENTED_EDGE('',*,*,#19394,.T.);
#27214=ORIENTED_EDGE('',*,*,#19395,.T.);
#27215=ORIENTED_EDGE('',*,*,#19371,.F.);
#27216=ORIENTED_EDGE('',*,*,#19393,.F.);
#27217=ORIENTED_EDGE('',*,*,#19396,.T.);
#27218=ORIENTED_EDGE('',*,*,#19397,.T.);
#27219=ORIENTED_EDGE('',*,*,#19372,.F.);
#27220=ORIENTED_EDGE('',*,*,#19395,.F.);
#27221=ORIENTED_EDGE('',*,*,#19398,.T.);
#27222=ORIENTED_EDGE('',*,*,#19399,.T.);
#27223=ORIENTED_EDGE('',*,*,#19373,.F.);
#27224=ORIENTED_EDGE('',*,*,#19397,.F.);
#27225=ORIENTED_EDGE('',*,*,#19400,.T.);
#27226=ORIENTED_EDGE('',*,*,#19401,.T.);
#27227=ORIENTED_EDGE('',*,*,#19374,.F.);
#27228=ORIENTED_EDGE('',*,*,#19399,.F.);
#27229=ORIENTED_EDGE('',*,*,#19402,.T.);
#27230=ORIENTED_EDGE('',*,*,#19331,.T.);
#27231=ORIENTED_EDGE('',*,*,#19375,.F.);
#27232=ORIENTED_EDGE('',*,*,#19401,.F.);
#27233=ORIENTED_EDGE('',*,*,#19403,.T.);
#27234=ORIENTED_EDGE('',*,*,#19404,.F.);
#27235=ORIENTED_EDGE('',*,*,#19405,.F.);
#27236=ORIENTED_EDGE('',*,*,#19402,.F.);
#27237=ORIENTED_EDGE('',*,*,#19406,.F.);
#27238=ORIENTED_EDGE('',*,*,#19407,.F.);
#27239=ORIENTED_EDGE('',*,*,#19408,.F.);
#27240=ORIENTED_EDGE('',*,*,#19403,.F.);
#27241=ORIENTED_EDGE('',*,*,#19400,.F.);
#27242=ORIENTED_EDGE('',*,*,#19398,.F.);
#27243=ORIENTED_EDGE('',*,*,#19409,.F.);
#27244=ORIENTED_EDGE('',*,*,#19341,.F.);
#27245=ORIENTED_EDGE('',*,*,#19406,.T.);
#27246=ORIENTED_EDGE('',*,*,#19410,.T.);
#27247=ORIENTED_EDGE('',*,*,#19351,.F.);
#27248=ORIENTED_EDGE('',*,*,#19409,.T.);
#27249=ORIENTED_EDGE('',*,*,#19396,.F.);
#27250=ORIENTED_EDGE('',*,*,#19411,.T.);
#27251=ORIENTED_EDGE('',*,*,#19348,.F.);
#27252=ORIENTED_EDGE('',*,*,#19410,.F.);
#27253=ORIENTED_EDGE('',*,*,#19394,.F.);
#27254=ORIENTED_EDGE('',*,*,#19412,.T.);
#27255=ORIENTED_EDGE('',*,*,#19355,.F.);
#27256=ORIENTED_EDGE('',*,*,#19411,.F.);
#27257=ORIENTED_EDGE('',*,*,#19392,.F.);
#27258=ORIENTED_EDGE('',*,*,#19388,.T.);
#27259=ORIENTED_EDGE('',*,*,#19413,.F.);
#27260=ORIENTED_EDGE('',*,*,#19412,.F.);
#27261=ORIENTED_EDGE('',*,*,#19390,.F.);
#27262=ORIENTED_EDGE('',*,*,#19356,.T.);
#27263=ORIENTED_EDGE('',*,*,#19413,.T.);
#27264=ORIENTED_EDGE('',*,*,#19414,.F.);
#27265=ORIENTED_EDGE('',*,*,#19415,.F.);
#27266=ORIENTED_EDGE('',*,*,#19414,.T.);
#27267=ORIENTED_EDGE('',*,*,#19387,.T.);
#27268=ORIENTED_EDGE('',*,*,#19416,.F.);
#27269=ORIENTED_EDGE('',*,*,#19417,.F.);
#27270=ORIENTED_EDGE('',*,*,#19416,.T.);
#27271=ORIENTED_EDGE('',*,*,#19386,.T.);
#27272=ORIENTED_EDGE('',*,*,#19418,.F.);
#27273=ORIENTED_EDGE('',*,*,#19419,.F.);
#27274=ORIENTED_EDGE('',*,*,#19418,.T.);
#27275=ORIENTED_EDGE('',*,*,#19385,.T.);
#27276=ORIENTED_EDGE('',*,*,#19345,.F.);
#27277=ORIENTED_EDGE('',*,*,#19420,.F.);
#27278=ORIENTED_EDGE('',*,*,#19420,.T.);
#27279=ORIENTED_EDGE('',*,*,#19421,.F.);
#27280=ORIENTED_EDGE('',*,*,#19422,.F.);
#27281=ORIENTED_EDGE('',*,*,#19297,.F.);
#27282=ORIENTED_EDGE('',*,*,#19423,.T.);
#27283=ORIENTED_EDGE('',*,*,#19421,.T.);
#27284=ORIENTED_EDGE('',*,*,#19344,.T.);
#27285=ORIENTED_EDGE('',*,*,#19424,.T.);
#27286=ORIENTED_EDGE('',*,*,#19425,.T.);
#27287=ORIENTED_EDGE('',*,*,#19423,.F.);
#27288=ORIENTED_EDGE('',*,*,#19309,.F.);
#27289=ORIENTED_EDGE('',*,*,#19307,.F.);
#27290=ORIENTED_EDGE('',*,*,#19426,.T.);
#27291=ORIENTED_EDGE('',*,*,#19427,.T.);
#27292=ORIENTED_EDGE('',*,*,#19424,.F.);
#27293=ORIENTED_EDGE('',*,*,#19428,.T.);
#27294=ORIENTED_EDGE('',*,*,#19429,.F.);
#27295=ORIENTED_EDGE('',*,*,#19426,.F.);
#27296=ORIENTED_EDGE('',*,*,#19332,.F.);
#27297=ORIENTED_EDGE('',*,*,#19405,.T.);
#27298=ORIENTED_EDGE('',*,*,#19430,.F.);
#27299=ORIENTED_EDGE('',*,*,#19431,.F.);
#27300=ORIENTED_EDGE('',*,*,#19428,.F.);
#27301=ORIENTED_EDGE('',*,*,#19288,.F.);
#27302=ORIENTED_EDGE('',*,*,#19333,.F.);
#27303=ORIENTED_EDGE('',*,*,#19329,.F.);
#27304=ORIENTED_EDGE('',*,*,#19432,.T.);
#27305=ORIENTED_EDGE('',*,*,#19430,.T.);
#27306=ORIENTED_EDGE('',*,*,#19433,.F.);
#27307=ORIENTED_EDGE('',*,*,#19434,.F.);
#27308=ORIENTED_EDGE('',*,*,#19429,.T.);
#27309=ORIENTED_EDGE('',*,*,#19431,.T.);
#27310=ORIENTED_EDGE('',*,*,#19432,.F.);
#27311=ORIENTED_EDGE('',*,*,#19435,.F.);
#27312=ORIENTED_EDGE('',*,*,#19435,.T.);
#27313=ORIENTED_EDGE('',*,*,#19436,.T.);
#27314=ORIENTED_EDGE('',*,*,#19427,.F.);
#27315=ORIENTED_EDGE('',*,*,#19422,.T.);
#27316=ORIENTED_EDGE('',*,*,#19425,.F.);
#27317=ORIENTED_EDGE('',*,*,#19436,.F.);
#27318=ORIENTED_EDGE('',*,*,#19434,.T.);
#27319=ORIENTED_EDGE('',*,*,#19437,.T.);
#27320=ORIENTED_EDGE('',*,*,#19438,.T.);
#27321=ORIENTED_EDGE('',*,*,#19439,.T.);
#27322=ORIENTED_EDGE('',*,*,#19419,.T.);
#27323=ORIENTED_EDGE('',*,*,#19433,.T.);
#27324=ORIENTED_EDGE('',*,*,#19404,.T.);
#27325=ORIENTED_EDGE('',*,*,#19440,.F.);
#27326=ORIENTED_EDGE('',*,*,#19437,.F.);
#27327=ORIENTED_EDGE('',*,*,#19440,.T.);
#27328=ORIENTED_EDGE('',*,*,#19408,.T.);
#27329=ORIENTED_EDGE('',*,*,#19441,.F.);
#27330=ORIENTED_EDGE('',*,*,#19438,.F.);
#27331=ORIENTED_EDGE('',*,*,#19441,.T.);
#27332=ORIENTED_EDGE('',*,*,#19407,.T.);
#27333=ORIENTED_EDGE('',*,*,#19340,.F.);
#27334=ORIENTED_EDGE('',*,*,#19442,.F.);
#27335=ORIENTED_EDGE('',*,*,#19442,.T.);
#27336=ORIENTED_EDGE('',*,*,#19343,.T.);
#27337=ORIENTED_EDGE('',*,*,#19352,.T.);
#27338=ORIENTED_EDGE('',*,*,#19350,.T.);
#27339=ORIENTED_EDGE('',*,*,#19357,.T.);
#27340=ORIENTED_EDGE('',*,*,#19415,.T.);
#27341=ORIENTED_EDGE('',*,*,#19417,.T.);
#27342=ORIENTED_EDGE('',*,*,#19439,.F.);
#27343=ORIENTED_EDGE('',*,*,#19443,.T.);
#27344=ORIENTED_EDGE('',*,*,#19444,.T.);
#27345=ORIENTED_EDGE('',*,*,#19445,.F.);
#27346=ORIENTED_EDGE('',*,*,#19446,.F.);
#27347=ORIENTED_EDGE('',*,*,#19447,.T.);
#27348=ORIENTED_EDGE('',*,*,#19448,.F.);
#27349=ORIENTED_EDGE('',*,*,#19449,.F.);
#27350=ORIENTED_EDGE('',*,*,#19450,.F.);
#27351=ORIENTED_EDGE('',*,*,#19451,.T.);
#27352=ORIENTED_EDGE('',*,*,#19452,.F.);
#27353=ORIENTED_EDGE('',*,*,#19453,.F.);
#27354=ORIENTED_EDGE('',*,*,#19454,.F.);
#27355=ORIENTED_EDGE('',*,*,#19455,.T.);
#27356=ORIENTED_EDGE('',*,*,#19456,.F.);
#27357=ORIENTED_EDGE('',*,*,#19455,.F.);
#27358=ORIENTED_EDGE('',*,*,#19457,.T.);
#27359=ORIENTED_EDGE('',*,*,#19458,.T.);
#27360=ORIENTED_EDGE('',*,*,#19459,.T.);
#27361=ORIENTED_EDGE('',*,*,#19460,.T.);
#27362=ORIENTED_EDGE('',*,*,#19461,.T.);
#27363=ORIENTED_EDGE('',*,*,#19462,.F.);
#27364=ORIENTED_EDGE('',*,*,#19463,.F.);
#27365=ORIENTED_EDGE('',*,*,#19464,.F.);
#27366=ORIENTED_EDGE('',*,*,#19445,.T.);
#27367=ORIENTED_EDGE('',*,*,#19465,.T.);
#27368=ORIENTED_EDGE('',*,*,#19466,.T.);
#27369=ORIENTED_EDGE('',*,*,#19467,.T.);
#27370=ORIENTED_EDGE('',*,*,#19468,.F.);
#27371=ORIENTED_EDGE('',*,*,#19469,.F.);
#27372=ORIENTED_EDGE('',*,*,#19470,.T.);
#27373=ORIENTED_EDGE('',*,*,#19471,.T.);
#27374=ORIENTED_EDGE('',*,*,#19469,.T.);
#27375=ORIENTED_EDGE('',*,*,#19472,.F.);
#27376=ORIENTED_EDGE('',*,*,#19473,.F.);
#27377=ORIENTED_EDGE('',*,*,#19474,.T.);
#27378=ORIENTED_EDGE('',*,*,#19475,.T.);
#27379=ORIENTED_EDGE('',*,*,#19467,.F.);
#27380=ORIENTED_EDGE('',*,*,#19476,.F.);
#27381=ORIENTED_EDGE('',*,*,#19473,.T.);
#27382=ORIENTED_EDGE('',*,*,#19477,.F.);
#27383=ORIENTED_EDGE('',*,*,#19474,.F.);
#27384=ORIENTED_EDGE('',*,*,#19478,.T.);
#27385=ORIENTED_EDGE('',*,*,#19479,.F.);
#27386=ORIENTED_EDGE('',*,*,#19480,.F.);
#27387=ORIENTED_EDGE('',*,*,#19481,.T.);
#27388=ORIENTED_EDGE('',*,*,#19482,.T.);
#27389=ORIENTED_EDGE('',*,*,#19481,.F.);
#27390=ORIENTED_EDGE('',*,*,#19483,.F.);
#27391=ORIENTED_EDGE('',*,*,#19484,.T.);
#27392=ORIENTED_EDGE('',*,*,#19485,.T.);
#27393=ORIENTED_EDGE('',*,*,#19486,.F.);
#27394=ORIENTED_EDGE('',*,*,#19487,.F.);
#27395=ORIENTED_EDGE('',*,*,#19488,.T.);
#27396=ORIENTED_EDGE('',*,*,#19479,.T.);
#27397=ORIENTED_EDGE('',*,*,#19484,.F.);
#27398=ORIENTED_EDGE('',*,*,#19489,.F.);
#27399=ORIENTED_EDGE('',*,*,#19487,.T.);
#27400=ORIENTED_EDGE('',*,*,#19490,.T.);
#27401=ORIENTED_EDGE('',*,*,#19491,.T.);
#27402=ORIENTED_EDGE('',*,*,#19492,.T.);
#27403=ORIENTED_EDGE('',*,*,#19493,.T.);
#27404=ORIENTED_EDGE('',*,*,#19494,.T.);
#27405=ORIENTED_EDGE('',*,*,#19495,.F.);
#27406=ORIENTED_EDGE('',*,*,#19496,.F.);
#27407=ORIENTED_EDGE('',*,*,#19497,.T.);
#27408=ORIENTED_EDGE('',*,*,#19498,.T.);
#27409=ORIENTED_EDGE('',*,*,#19499,.F.);
#27410=ORIENTED_EDGE('',*,*,#19500,.F.);
#27411=ORIENTED_EDGE('',*,*,#19501,.T.);
#27412=ORIENTED_EDGE('',*,*,#19502,.T.);
#27413=ORIENTED_EDGE('',*,*,#19503,.F.);
#27414=ORIENTED_EDGE('',*,*,#19504,.F.);
#27415=ORIENTED_EDGE('',*,*,#19505,.F.);
#27416=ORIENTED_EDGE('',*,*,#19506,.F.);
#27417=ORIENTED_EDGE('',*,*,#19507,.T.);
#27418=ORIENTED_EDGE('',*,*,#19508,.T.);
#27419=ORIENTED_EDGE('',*,*,#19509,.F.);
#27420=ORIENTED_EDGE('',*,*,#19510,.T.);
#27421=ORIENTED_EDGE('',*,*,#19511,.T.);
#27422=ORIENTED_EDGE('',*,*,#19512,.F.);
#27423=ORIENTED_EDGE('',*,*,#19513,.T.);
#27424=ORIENTED_EDGE('',*,*,#19514,.T.);
#27425=ORIENTED_EDGE('',*,*,#19515,.T.);
#27426=ORIENTED_EDGE('',*,*,#19516,.T.);
#27427=ORIENTED_EDGE('',*,*,#19517,.T.);
#27428=ORIENTED_EDGE('',*,*,#19518,.F.);
#27429=ORIENTED_EDGE('',*,*,#19519,.T.);
#27430=ORIENTED_EDGE('',*,*,#19520,.T.);
#27431=ORIENTED_EDGE('',*,*,#19521,.F.);
#27432=ORIENTED_EDGE('',*,*,#19522,.F.);
#27433=ORIENTED_EDGE('',*,*,#19523,.T.);
#27434=ORIENTED_EDGE('',*,*,#19524,.T.);
#27435=ORIENTED_EDGE('',*,*,#19525,.F.);
#27436=ORIENTED_EDGE('',*,*,#19526,.F.);
#27437=ORIENTED_EDGE('',*,*,#19527,.T.);
#27438=ORIENTED_EDGE('',*,*,#19492,.F.);
#27439=ORIENTED_EDGE('',*,*,#19528,.T.);
#27440=ORIENTED_EDGE('',*,*,#19529,.F.);
#27441=ORIENTED_EDGE('',*,*,#19530,.T.);
#27442=ORIENTED_EDGE('',*,*,#19531,.T.);
#27443=ORIENTED_EDGE('',*,*,#19532,.T.);
#27444=ORIENTED_EDGE('',*,*,#19533,.T.);
#27445=ORIENTED_EDGE('',*,*,#19534,.F.);
#27446=ORIENTED_EDGE('',*,*,#19535,.F.);
#27447=ORIENTED_EDGE('',*,*,#19536,.T.);
#27448=ORIENTED_EDGE('',*,*,#19537,.F.);
#27449=ORIENTED_EDGE('',*,*,#19538,.T.);
#27450=ORIENTED_EDGE('',*,*,#19539,.T.);
#27451=ORIENTED_EDGE('',*,*,#19540,.F.);
#27452=ORIENTED_EDGE('',*,*,#19541,.T.);
#27453=ORIENTED_EDGE('',*,*,#19542,.F.);
#27454=ORIENTED_EDGE('',*,*,#19543,.F.);
#27455=ORIENTED_EDGE('',*,*,#19490,.F.);
#27456=ORIENTED_EDGE('',*,*,#19486,.T.);
#27457=ORIENTED_EDGE('',*,*,#19482,.F.);
#27458=ORIENTED_EDGE('',*,*,#19485,.F.);
#27459=ORIENTED_EDGE('',*,*,#19476,.T.);
#27460=ORIENTED_EDGE('',*,*,#19470,.F.);
#27461=ORIENTED_EDGE('',*,*,#19471,.F.);
#27462=ORIENTED_EDGE('',*,*,#19478,.F.);
#27463=ORIENTED_EDGE('',*,*,#19453,.T.);
#27464=ORIENTED_EDGE('',*,*,#19454,.T.);
#27465=ORIENTED_EDGE('',*,*,#19544,.T.);
#27466=ORIENTED_EDGE('',*,*,#19545,.F.);
#27467=ORIENTED_EDGE('',*,*,#19546,.F.);
#27468=ORIENTED_EDGE('',*,*,#19547,.T.);
#27469=ORIENTED_EDGE('',*,*,#19548,.T.);
#27470=ORIENTED_EDGE('',*,*,#19549,.T.);
#27471=ORIENTED_EDGE('',*,*,#19550,.T.);
#27472=ORIENTED_EDGE('',*,*,#19551,.F.);
#27473=ORIENTED_EDGE('',*,*,#19552,.F.);
#27474=ORIENTED_EDGE('',*,*,#19553,.T.);
#27475=ORIENTED_EDGE('',*,*,#19554,.F.);
#27476=ORIENTED_EDGE('',*,*,#19555,.T.);
#27477=ORIENTED_EDGE('',*,*,#19556,.T.);
#27478=ORIENTED_EDGE('',*,*,#19557,.F.);
#27479=ORIENTED_EDGE('',*,*,#19558,.T.);
#27480=ORIENTED_EDGE('',*,*,#19559,.F.);
#27481=ORIENTED_EDGE('',*,*,#19560,.F.);
#27482=ORIENTED_EDGE('',*,*,#19561,.F.);
#27483=ORIENTED_EDGE('',*,*,#19544,.F.);
#27484=ORIENTED_EDGE('',*,*,#19477,.T.);
#27485=ORIENTED_EDGE('',*,*,#19472,.T.);
#27486=ORIENTED_EDGE('',*,*,#19468,.T.);
#27487=ORIENTED_EDGE('',*,*,#19475,.F.);
#27488=ORIENTED_EDGE('',*,*,#19483,.T.);
#27489=ORIENTED_EDGE('',*,*,#19480,.T.);
#27490=ORIENTED_EDGE('',*,*,#19488,.F.);
#27491=ORIENTED_EDGE('',*,*,#19489,.T.);
#27492=ORIENTED_EDGE('',*,*,#19524,.F.);
#27493=ORIENTED_EDGE('',*,*,#19562,.F.);
#27494=ORIENTED_EDGE('',*,*,#19563,.T.);
#27495=ORIENTED_EDGE('',*,*,#19564,.T.);
#27496=ORIENTED_EDGE('',*,*,#19565,.F.);
#27497=ORIENTED_EDGE('',*,*,#19566,.T.);
#27498=ORIENTED_EDGE('',*,*,#19567,.T.);
#27499=ORIENTED_EDGE('',*,*,#19522,.T.);
#27500=ORIENTED_EDGE('',*,*,#19568,.F.);
#27501=ORIENTED_EDGE('',*,*,#19563,.F.);
#27502=ORIENTED_EDGE('',*,*,#19569,.T.);
#27503=ORIENTED_EDGE('',*,*,#19570,.F.);
#27504=ORIENTED_EDGE('',*,*,#19570,.T.);
#27505=ORIENTED_EDGE('',*,*,#19571,.T.);
#27506=ORIENTED_EDGE('',*,*,#19566,.F.);
#27507=ORIENTED_EDGE('',*,*,#19572,.F.);
#27508=ORIENTED_EDGE('',*,*,#19573,.T.);
#27509=ORIENTED_EDGE('',*,*,#19574,.T.);
#27510=ORIENTED_EDGE('',*,*,#19575,.T.);
#27511=ORIENTED_EDGE('',*,*,#19576,.F.);
#27512=ORIENTED_EDGE('',*,*,#19577,.F.);
#27513=ORIENTED_EDGE('',*,*,#19578,.F.);
#27514=ORIENTED_EDGE('',*,*,#19573,.F.);
#27515=ORIENTED_EDGE('',*,*,#19579,.F.);
#27516=ORIENTED_EDGE('',*,*,#19580,.T.);
#27517=ORIENTED_EDGE('',*,*,#19581,.F.);
#27518=ORIENTED_EDGE('',*,*,#19582,.T.);
#27519=ORIENTED_EDGE('',*,*,#19577,.T.);
#27520=ORIENTED_EDGE('',*,*,#19581,.T.);
#27521=ORIENTED_EDGE('',*,*,#19583,.F.);
#27522=ORIENTED_EDGE('',*,*,#19520,.F.);
#27523=ORIENTED_EDGE('',*,*,#19584,.T.);
#27524=ORIENTED_EDGE('',*,*,#19585,.T.);
#27525=ORIENTED_EDGE('',*,*,#19575,.F.);
#27526=ORIENTED_EDGE('',*,*,#19586,.T.);
#27527=ORIENTED_EDGE('',*,*,#19587,.T.);
#27528=ORIENTED_EDGE('',*,*,#19521,.T.);
#27529=ORIENTED_EDGE('',*,*,#19583,.T.);
#27530=ORIENTED_EDGE('',*,*,#19580,.F.);
#27531=ORIENTED_EDGE('',*,*,#19579,.T.);
#27532=ORIENTED_EDGE('',*,*,#19576,.T.);
#27533=ORIENTED_EDGE('',*,*,#19585,.F.);
#27534=ORIENTED_EDGE('',*,*,#19588,.T.);
#27535=ORIENTED_EDGE('',*,*,#19525,.T.);
#27536=ORIENTED_EDGE('',*,*,#19564,.F.);
#27537=ORIENTED_EDGE('',*,*,#19568,.T.);
#27538=ORIENTED_EDGE('',*,*,#19572,.T.);
#27539=ORIENTED_EDGE('',*,*,#19565,.T.);
#27540=ORIENTED_EDGE('',*,*,#19589,.T.);
#27541=ORIENTED_EDGE('',*,*,#19526,.T.);
#27542=ORIENTED_EDGE('',*,*,#19588,.F.);
#27543=ORIENTED_EDGE('',*,*,#19587,.F.);
#27544=ORIENTED_EDGE('',*,*,#19590,.T.);
#27545=ORIENTED_EDGE('',*,*,#19591,.F.);
#27546=ORIENTED_EDGE('',*,*,#19592,.T.);
#27547=ORIENTED_EDGE('',*,*,#19593,.T.);
#27548=ORIENTED_EDGE('',*,*,#19591,.T.);
#27549=ORIENTED_EDGE('',*,*,#19594,.T.);
#27550=ORIENTED_EDGE('',*,*,#19595,.F.);
#27551=ORIENTED_EDGE('',*,*,#19596,.T.);
#27552=ORIENTED_EDGE('',*,*,#19597,.T.);
#27553=ORIENTED_EDGE('',*,*,#19460,.F.);
#27554=ORIENTED_EDGE('',*,*,#19598,.F.);
#27555=ORIENTED_EDGE('',*,*,#19599,.T.);
#27556=ORIENTED_EDGE('',*,*,#19600,.T.);
#27557=ORIENTED_EDGE('',*,*,#19601,.T.);
#27558=ORIENTED_EDGE('',*,*,#19597,.F.);
#27559=ORIENTED_EDGE('',*,*,#19602,.F.);
#27560=ORIENTED_EDGE('',*,*,#19511,.F.);
#27561=ORIENTED_EDGE('',*,*,#19603,.T.);
#27562=ORIENTED_EDGE('',*,*,#19602,.T.);
#27563=ORIENTED_EDGE('',*,*,#19604,.F.);
#27564=ORIENTED_EDGE('',*,*,#19599,.F.);
#27565=ORIENTED_EDGE('',*,*,#19605,.F.);
#27566=ORIENTED_EDGE('',*,*,#19606,.F.);
#27567=ORIENTED_EDGE('',*,*,#19607,.F.);
#27568=ORIENTED_EDGE('',*,*,#19608,.F.);
#27569=ORIENTED_EDGE('',*,*,#19512,.T.);
#27570=ORIENTED_EDGE('',*,*,#19604,.T.);
#27571=ORIENTED_EDGE('',*,*,#19607,.T.);
#27572=ORIENTED_EDGE('',*,*,#19609,.F.);
#27573=ORIENTED_EDGE('',*,*,#19610,.F.);
#27574=ORIENTED_EDGE('',*,*,#19611,.T.);
#27575=ORIENTED_EDGE('',*,*,#19610,.T.);
#27576=ORIENTED_EDGE('',*,*,#19612,.T.);
#27577=ORIENTED_EDGE('',*,*,#19514,.F.);
#27578=ORIENTED_EDGE('',*,*,#19613,.F.);
#27579=ORIENTED_EDGE('',*,*,#19614,.T.);
#27580=ORIENTED_EDGE('',*,*,#19615,.F.);
#27581=ORIENTED_EDGE('',*,*,#19616,.T.);
#27582=ORIENTED_EDGE('',*,*,#19595,.T.);
#27583=ORIENTED_EDGE('',*,*,#19609,.T.);
#27584=ORIENTED_EDGE('',*,*,#19606,.T.);
#27585=ORIENTED_EDGE('',*,*,#19617,.F.);
#27586=ORIENTED_EDGE('',*,*,#19618,.F.);
#27587=ORIENTED_EDGE('',*,*,#19618,.T.);
#27588=ORIENTED_EDGE('',*,*,#19619,.T.);
#27589=ORIENTED_EDGE('',*,*,#19515,.F.);
#27590=ORIENTED_EDGE('',*,*,#19612,.F.);
#27591=ORIENTED_EDGE('',*,*,#19620,.T.);
#27592=ORIENTED_EDGE('',*,*,#19459,.F.);
#27593=ORIENTED_EDGE('',*,*,#19621,.F.);
#27594=ORIENTED_EDGE('',*,*,#19622,.T.);
#27595=ORIENTED_EDGE('',*,*,#19598,.T.);
#27596=ORIENTED_EDGE('',*,*,#19620,.F.);
#27597=ORIENTED_EDGE('',*,*,#19623,.F.);
#27598=ORIENTED_EDGE('',*,*,#19624,.F.);
#27599=ORIENTED_EDGE('',*,*,#19625,.F.);
#27600=ORIENTED_EDGE('',*,*,#19617,.T.);
#27601=ORIENTED_EDGE('',*,*,#19605,.T.);
#27602=ORIENTED_EDGE('',*,*,#19622,.F.);
#27603=ORIENTED_EDGE('',*,*,#19626,.F.);
#27604=ORIENTED_EDGE('',*,*,#19627,.F.);
#27605=ORIENTED_EDGE('',*,*,#19516,.F.);
#27606=ORIENTED_EDGE('',*,*,#19619,.F.);
#27607=ORIENTED_EDGE('',*,*,#19625,.T.);
#27608=ORIENTED_EDGE('',*,*,#19623,.T.);
#27609=ORIENTED_EDGE('',*,*,#19621,.T.);
#27610=ORIENTED_EDGE('',*,*,#19628,.F.);
#27611=ORIENTED_EDGE('',*,*,#19629,.F.);
#27612=ORIENTED_EDGE('',*,*,#19628,.T.);
#27613=ORIENTED_EDGE('',*,*,#19458,.F.);
#27614=ORIENTED_EDGE('',*,*,#19630,.F.);
#27615=ORIENTED_EDGE('',*,*,#19631,.F.);
#27616=ORIENTED_EDGE('',*,*,#19624,.T.);
#27617=ORIENTED_EDGE('',*,*,#19629,.T.);
#27618=ORIENTED_EDGE('',*,*,#19632,.F.);
#27619=ORIENTED_EDGE('',*,*,#19633,.F.);
#27620=ORIENTED_EDGE('',*,*,#19626,.T.);
#27621=ORIENTED_EDGE('',*,*,#19633,.T.);
#27622=ORIENTED_EDGE('',*,*,#19634,.F.);
#27623=ORIENTED_EDGE('',*,*,#19635,.F.);
#27624=ORIENTED_EDGE('',*,*,#19517,.F.);
#27625=ORIENTED_EDGE('',*,*,#19627,.T.);
#27626=ORIENTED_EDGE('',*,*,#19635,.T.);
#27627=ORIENTED_EDGE('',*,*,#19636,.F.);
#27628=ORIENTED_EDGE('',*,*,#19631,.T.);
#27629=ORIENTED_EDGE('',*,*,#19637,.F.);
#27630=ORIENTED_EDGE('',*,*,#19518,.T.);
#27631=ORIENTED_EDGE('',*,*,#19636,.T.);
#27632=ORIENTED_EDGE('',*,*,#19634,.T.);
#27633=ORIENTED_EDGE('',*,*,#19632,.T.);
#27634=ORIENTED_EDGE('',*,*,#19638,.T.);
#27635=ORIENTED_EDGE('',*,*,#19639,.F.);
#27636=ORIENTED_EDGE('',*,*,#19593,.F.);
#27637=ORIENTED_EDGE('',*,*,#19640,.T.);
#27638=ORIENTED_EDGE('',*,*,#19638,.F.);
#27639=ORIENTED_EDGE('',*,*,#19641,.F.);
#27640=ORIENTED_EDGE('',*,*,#19642,.T.);
#27641=ORIENTED_EDGE('',*,*,#19643,.F.);
#27642=ORIENTED_EDGE('',*,*,#19644,.F.);
#27643=ORIENTED_EDGE('',*,*,#19645,.T.);
#27644=ORIENTED_EDGE('',*,*,#19646,.F.);
#27645=ORIENTED_EDGE('',*,*,#19642,.F.);
#27646=ORIENTED_EDGE('',*,*,#19647,.F.);
#27647=ORIENTED_EDGE('',*,*,#19648,.T.);
#27648=ORIENTED_EDGE('',*,*,#19462,.T.);
#27649=ORIENTED_EDGE('',*,*,#19649,.F.);
#27650=ORIENTED_EDGE('',*,*,#19650,.T.);
#27651=ORIENTED_EDGE('',*,*,#19649,.T.);
#27652=ORIENTED_EDGE('',*,*,#19651,.F.);
#27653=ORIENTED_EDGE('',*,*,#19652,.F.);
#27654=ORIENTED_EDGE('',*,*,#19603,.F.);
#27655=ORIENTED_EDGE('',*,*,#19510,.F.);
#27656=ORIENTED_EDGE('',*,*,#19653,.T.);
#27657=ORIENTED_EDGE('',*,*,#19652,.T.);
#27658=ORIENTED_EDGE('',*,*,#19654,.T.);
#27659=ORIENTED_EDGE('',*,*,#19600,.F.);
#27660=ORIENTED_EDGE('',*,*,#19641,.T.);
#27661=ORIENTED_EDGE('',*,*,#19640,.F.);
#27662=ORIENTED_EDGE('',*,*,#19592,.F.);
#27663=ORIENTED_EDGE('',*,*,#19596,.F.);
#27664=ORIENTED_EDGE('',*,*,#19616,.F.);
#27665=ORIENTED_EDGE('',*,*,#19655,.T.);
#27666=ORIENTED_EDGE('',*,*,#19656,.T.);
#27667=ORIENTED_EDGE('',*,*,#19644,.T.);
#27668=ORIENTED_EDGE('',*,*,#19657,.T.);
#27669=ORIENTED_EDGE('',*,*,#19650,.F.);
#27670=ORIENTED_EDGE('',*,*,#19653,.F.);
#27671=ORIENTED_EDGE('',*,*,#19509,.T.);
#27672=ORIENTED_EDGE('',*,*,#19657,.F.);
#27673=ORIENTED_EDGE('',*,*,#19508,.F.);
#27674=ORIENTED_EDGE('',*,*,#19658,.T.);
#27675=ORIENTED_EDGE('',*,*,#19659,.T.);
#27676=ORIENTED_EDGE('',*,*,#19660,.T.);
#27677=ORIENTED_EDGE('',*,*,#19661,.T.);
#27678=ORIENTED_EDGE('',*,*,#19647,.T.);
#27679=ORIENTED_EDGE('',*,*,#19662,.F.);
#27680=ORIENTED_EDGE('',*,*,#19663,.T.);
#27681=ORIENTED_EDGE('',*,*,#19664,.T.);
#27682=ORIENTED_EDGE('',*,*,#19659,.F.);
#27683=ORIENTED_EDGE('',*,*,#19665,.T.);
#27684=ORIENTED_EDGE('',*,*,#19506,.T.);
#27685=ORIENTED_EDGE('',*,*,#19666,.F.);
#27686=ORIENTED_EDGE('',*,*,#19663,.F.);
#27687=ORIENTED_EDGE('',*,*,#19645,.F.);
#27688=ORIENTED_EDGE('',*,*,#19656,.F.);
#27689=ORIENTED_EDGE('',*,*,#19667,.T.);
#27690=ORIENTED_EDGE('',*,*,#19668,.F.);
#27691=ORIENTED_EDGE('',*,*,#19655,.F.);
#27692=ORIENTED_EDGE('',*,*,#19615,.T.);
#27693=ORIENTED_EDGE('',*,*,#19669,.F.);
#27694=ORIENTED_EDGE('',*,*,#19667,.F.);
#27695=ORIENTED_EDGE('',*,*,#19654,.F.);
#27696=ORIENTED_EDGE('',*,*,#19651,.T.);
#27697=ORIENTED_EDGE('',*,*,#19461,.F.);
#27698=ORIENTED_EDGE('',*,*,#19601,.F.);
#27699=ORIENTED_EDGE('',*,*,#19670,.T.);
#27700=ORIENTED_EDGE('',*,*,#19671,.T.);
#27701=ORIENTED_EDGE('',*,*,#19660,.F.);
#27702=ORIENTED_EDGE('',*,*,#19664,.F.);
#27703=ORIENTED_EDGE('',*,*,#19666,.T.);
#27704=ORIENTED_EDGE('',*,*,#19505,.T.);
#27705=ORIENTED_EDGE('',*,*,#19672,.F.);
#27706=ORIENTED_EDGE('',*,*,#19670,.F.);
#27707=ORIENTED_EDGE('',*,*,#19673,.T.);
#27708=ORIENTED_EDGE('',*,*,#19463,.T.);
#27709=ORIENTED_EDGE('',*,*,#19674,.F.);
#27710=ORIENTED_EDGE('',*,*,#19675,.T.);
#27711=ORIENTED_EDGE('',*,*,#19676,.T.);
#27712=ORIENTED_EDGE('',*,*,#19674,.T.);
#27713=ORIENTED_EDGE('',*,*,#19648,.F.);
#27714=ORIENTED_EDGE('',*,*,#19677,.F.);
#27715=ORIENTED_EDGE('',*,*,#19678,.T.);
#27716=ORIENTED_EDGE('',*,*,#19677,.T.);
#27717=ORIENTED_EDGE('',*,*,#19661,.F.);
#27718=ORIENTED_EDGE('',*,*,#19671,.F.);
#27719=ORIENTED_EDGE('',*,*,#19679,.T.);
#27720=ORIENTED_EDGE('',*,*,#19679,.F.);
#27721=ORIENTED_EDGE('',*,*,#19672,.T.);
#27722=ORIENTED_EDGE('',*,*,#19504,.T.);
#27723=ORIENTED_EDGE('',*,*,#19680,.T.);
#27724=ORIENTED_EDGE('',*,*,#19681,.T.);
#27725=ORIENTED_EDGE('',*,*,#19682,.T.);
#27726=ORIENTED_EDGE('',*,*,#19673,.F.);
#27727=ORIENTED_EDGE('',*,*,#19676,.F.);
#27728=ORIENTED_EDGE('',*,*,#19683,.T.);
#27729=ORIENTED_EDGE('',*,*,#19684,.T.);
#27730=ORIENTED_EDGE('',*,*,#19464,.T.);
#27731=ORIENTED_EDGE('',*,*,#19682,.F.);
#27732=ORIENTED_EDGE('',*,*,#19685,.T.);
#27733=ORIENTED_EDGE('',*,*,#19686,.T.);
#27734=ORIENTED_EDGE('',*,*,#19681,.F.);
#27735=ORIENTED_EDGE('',*,*,#19675,.F.);
#27736=ORIENTED_EDGE('',*,*,#19687,.T.);
#27737=ORIENTED_EDGE('',*,*,#19688,.T.);
#27738=ORIENTED_EDGE('',*,*,#19685,.F.);
#27739=ORIENTED_EDGE('',*,*,#19678,.F.);
#27740=ORIENTED_EDGE('',*,*,#19689,.T.);
#27741=ORIENTED_EDGE('',*,*,#19687,.F.);
#27742=ORIENTED_EDGE('',*,*,#19680,.F.);
#27743=ORIENTED_EDGE('',*,*,#19503,.T.);
#27744=ORIENTED_EDGE('',*,*,#19686,.F.);
#27745=ORIENTED_EDGE('',*,*,#19688,.F.);
#27746=ORIENTED_EDGE('',*,*,#19689,.F.);
#27747=ORIENTED_EDGE('',*,*,#19502,.F.);
#27748=ORIENTED_EDGE('',*,*,#19690,.T.);
#27749=ORIENTED_EDGE('',*,*,#19683,.F.);
#27750=ORIENTED_EDGE('',*,*,#19498,.F.);
#27751=ORIENTED_EDGE('',*,*,#19691,.F.);
#27752=ORIENTED_EDGE('',*,*,#19692,.T.);
#27753=ORIENTED_EDGE('',*,*,#19693,.T.);
#27754=ORIENTED_EDGE('',*,*,#19694,.F.);
#27755=ORIENTED_EDGE('',*,*,#19695,.T.);
#27756=ORIENTED_EDGE('',*,*,#19696,.T.);
#27757=ORIENTED_EDGE('',*,*,#19496,.T.);
#27758=ORIENTED_EDGE('',*,*,#19697,.F.);
#27759=ORIENTED_EDGE('',*,*,#19692,.F.);
#27760=ORIENTED_EDGE('',*,*,#19698,.T.);
#27761=ORIENTED_EDGE('',*,*,#19699,.F.);
#27762=ORIENTED_EDGE('',*,*,#19699,.T.);
#27763=ORIENTED_EDGE('',*,*,#19700,.T.);
#27764=ORIENTED_EDGE('',*,*,#19695,.F.);
#27765=ORIENTED_EDGE('',*,*,#19701,.F.);
#27766=ORIENTED_EDGE('',*,*,#19702,.T.);
#27767=ORIENTED_EDGE('',*,*,#19703,.T.);
#27768=ORIENTED_EDGE('',*,*,#19704,.T.);
#27769=ORIENTED_EDGE('',*,*,#19705,.F.);
#27770=ORIENTED_EDGE('',*,*,#19706,.F.);
#27771=ORIENTED_EDGE('',*,*,#19707,.F.);
#27772=ORIENTED_EDGE('',*,*,#19702,.F.);
#27773=ORIENTED_EDGE('',*,*,#19708,.F.);
#27774=ORIENTED_EDGE('',*,*,#19709,.T.);
#27775=ORIENTED_EDGE('',*,*,#19710,.F.);
#27776=ORIENTED_EDGE('',*,*,#19711,.T.);
#27777=ORIENTED_EDGE('',*,*,#19706,.T.);
#27778=ORIENTED_EDGE('',*,*,#19710,.T.);
#27779=ORIENTED_EDGE('',*,*,#19712,.F.);
#27780=ORIENTED_EDGE('',*,*,#19494,.F.);
#27781=ORIENTED_EDGE('',*,*,#19713,.T.);
#27782=ORIENTED_EDGE('',*,*,#19714,.T.);
#27783=ORIENTED_EDGE('',*,*,#19704,.F.);
#27784=ORIENTED_EDGE('',*,*,#19715,.T.);
#27785=ORIENTED_EDGE('',*,*,#19716,.T.);
#27786=ORIENTED_EDGE('',*,*,#19495,.T.);
#27787=ORIENTED_EDGE('',*,*,#19712,.T.);
#27788=ORIENTED_EDGE('',*,*,#19709,.F.);
#27789=ORIENTED_EDGE('',*,*,#19708,.T.);
#27790=ORIENTED_EDGE('',*,*,#19705,.T.);
#27791=ORIENTED_EDGE('',*,*,#19714,.F.);
#27792=ORIENTED_EDGE('',*,*,#19717,.T.);
#27793=ORIENTED_EDGE('',*,*,#19499,.T.);
#27794=ORIENTED_EDGE('',*,*,#19693,.F.);
#27795=ORIENTED_EDGE('',*,*,#19697,.T.);
#27796=ORIENTED_EDGE('',*,*,#19701,.T.);
#27797=ORIENTED_EDGE('',*,*,#19694,.T.);
#27798=ORIENTED_EDGE('',*,*,#19718,.T.);
#27799=ORIENTED_EDGE('',*,*,#19500,.T.);
#27800=ORIENTED_EDGE('',*,*,#19717,.F.);
#27801=ORIENTED_EDGE('',*,*,#19716,.F.);
#27802=ORIENTED_EDGE('',*,*,#19534,.T.);
#27803=ORIENTED_EDGE('',*,*,#19719,.F.);
#27804=ORIENTED_EDGE('',*,*,#19555,.F.);
#27805=ORIENTED_EDGE('',*,*,#19720,.F.);
#27806=ORIENTED_EDGE('',*,*,#19721,.F.);
#27807=ORIENTED_EDGE('',*,*,#19556,.F.);
#27808=ORIENTED_EDGE('',*,*,#19719,.T.);
#27809=ORIENTED_EDGE('',*,*,#19533,.F.);
#27810=ORIENTED_EDGE('',*,*,#19532,.F.);
#27811=ORIENTED_EDGE('',*,*,#19722,.F.);
#27812=ORIENTED_EDGE('',*,*,#19557,.T.);
#27813=ORIENTED_EDGE('',*,*,#19721,.T.);
#27814=ORIENTED_EDGE('',*,*,#19723,.F.);
#27815=ORIENTED_EDGE('',*,*,#19558,.F.);
#27816=ORIENTED_EDGE('',*,*,#19722,.T.);
#27817=ORIENTED_EDGE('',*,*,#19531,.F.);
#27818=ORIENTED_EDGE('',*,*,#19724,.T.);
#27819=ORIENTED_EDGE('',*,*,#19559,.T.);
#27820=ORIENTED_EDGE('',*,*,#19723,.T.);
#27821=ORIENTED_EDGE('',*,*,#19530,.F.);
#27822=ORIENTED_EDGE('',*,*,#19551,.T.);
#27823=ORIENTED_EDGE('',*,*,#19725,.F.);
#27824=ORIENTED_EDGE('',*,*,#19538,.F.);
#27825=ORIENTED_EDGE('',*,*,#19726,.F.);
#27826=ORIENTED_EDGE('',*,*,#19727,.F.);
#27827=ORIENTED_EDGE('',*,*,#19539,.F.);
#27828=ORIENTED_EDGE('',*,*,#19725,.T.);
#27829=ORIENTED_EDGE('',*,*,#19550,.F.);
#27830=ORIENTED_EDGE('',*,*,#19540,.T.);
#27831=ORIENTED_EDGE('',*,*,#19727,.T.);
#27832=ORIENTED_EDGE('',*,*,#19549,.F.);
#27833=ORIENTED_EDGE('',*,*,#19728,.F.);
#27834=ORIENTED_EDGE('',*,*,#19729,.F.);
#27835=ORIENTED_EDGE('',*,*,#19541,.F.);
#27836=ORIENTED_EDGE('',*,*,#19728,.T.);
#27837=ORIENTED_EDGE('',*,*,#19548,.F.);
#27838=ORIENTED_EDGE('',*,*,#19730,.T.);
#27839=ORIENTED_EDGE('',*,*,#19542,.T.);
#27840=ORIENTED_EDGE('',*,*,#19729,.T.);
#27841=ORIENTED_EDGE('',*,*,#19547,.F.);
#27842=ORIENTED_EDGE('',*,*,#19560,.T.);
#27843=ORIENTED_EDGE('',*,*,#19724,.F.);
#27844=ORIENTED_EDGE('',*,*,#19529,.T.);
#27845=ORIENTED_EDGE('',*,*,#19731,.T.);
#27846=ORIENTED_EDGE('',*,*,#19543,.T.);
#27847=ORIENTED_EDGE('',*,*,#19730,.F.);
#27848=ORIENTED_EDGE('',*,*,#19546,.T.);
#27849=ORIENTED_EDGE('',*,*,#19732,.T.);
#27850=ORIENTED_EDGE('',*,*,#19732,.F.);
#27851=ORIENTED_EDGE('',*,*,#19545,.T.);
#27852=ORIENTED_EDGE('',*,*,#19561,.T.);
#27853=ORIENTED_EDGE('',*,*,#19731,.F.);
#27854=ORIENTED_EDGE('',*,*,#19528,.F.);
#27855=ORIENTED_EDGE('',*,*,#19491,.F.);
#27856=ORIENTED_EDGE('',*,*,#19554,.T.);
#27857=ORIENTED_EDGE('',*,*,#19733,.F.);
#27858=ORIENTED_EDGE('',*,*,#19535,.T.);
#27859=ORIENTED_EDGE('',*,*,#19720,.T.);
#27860=ORIENTED_EDGE('',*,*,#19537,.T.);
#27861=ORIENTED_EDGE('',*,*,#19734,.F.);
#27862=ORIENTED_EDGE('',*,*,#19552,.T.);
#27863=ORIENTED_EDGE('',*,*,#19726,.T.);
#27864=ORIENTED_EDGE('',*,*,#19734,.T.);
#27865=ORIENTED_EDGE('',*,*,#19536,.F.);
#27866=ORIENTED_EDGE('',*,*,#19733,.T.);
#27867=ORIENTED_EDGE('',*,*,#19553,.F.);
#27868=ORIENTED_EDGE('',*,*,#19735,.F.);
#27869=ORIENTED_EDGE('',*,*,#19736,.T.);
#27870=ORIENTED_EDGE('',*,*,#19466,.F.);
#27871=ORIENTED_EDGE('',*,*,#19736,.F.);
#27872=ORIENTED_EDGE('',*,*,#19608,.T.);
#27873=ORIENTED_EDGE('',*,*,#19611,.F.);
#27874=ORIENTED_EDGE('',*,*,#19613,.T.);
#27875=ORIENTED_EDGE('',*,*,#19513,.F.);
#27876=ORIENTED_EDGE('',*,*,#19669,.T.);
#27877=ORIENTED_EDGE('',*,*,#19614,.F.);
#27878=ORIENTED_EDGE('',*,*,#19594,.F.);
#27879=ORIENTED_EDGE('',*,*,#19590,.F.);
#27880=ORIENTED_EDGE('',*,*,#19639,.T.);
#27881=ORIENTED_EDGE('',*,*,#19643,.T.);
#27882=ORIENTED_EDGE('',*,*,#19646,.T.);
#27883=ORIENTED_EDGE('',*,*,#19668,.T.);
#27884=ORIENTED_EDGE('',*,*,#19665,.F.);
#27885=ORIENTED_EDGE('',*,*,#19662,.T.);
#27886=ORIENTED_EDGE('',*,*,#19658,.F.);
#27887=ORIENTED_EDGE('',*,*,#19507,.F.);
#27888=ORIENTED_EDGE('',*,*,#19567,.F.);
#27889=ORIENTED_EDGE('',*,*,#19571,.F.);
#27890=ORIENTED_EDGE('',*,*,#19569,.F.);
#27891=ORIENTED_EDGE('',*,*,#19562,.T.);
#27892=ORIENTED_EDGE('',*,*,#19523,.F.);
#27893=ORIENTED_EDGE('',*,*,#19589,.F.);
#27894=ORIENTED_EDGE('',*,*,#19586,.F.);
#27895=ORIENTED_EDGE('',*,*,#19574,.F.);
#27896=ORIENTED_EDGE('',*,*,#19578,.T.);
#27897=ORIENTED_EDGE('',*,*,#19582,.F.);
#27898=ORIENTED_EDGE('',*,*,#19584,.F.);
#27899=ORIENTED_EDGE('',*,*,#19519,.F.);
#27900=ORIENTED_EDGE('',*,*,#19637,.T.);
#27901=ORIENTED_EDGE('',*,*,#19630,.T.);
#27902=ORIENTED_EDGE('',*,*,#19457,.F.);
#27903=ORIENTED_EDGE('',*,*,#19684,.F.);
#27904=ORIENTED_EDGE('',*,*,#19690,.F.);
#27905=ORIENTED_EDGE('',*,*,#19501,.F.);
#27906=ORIENTED_EDGE('',*,*,#19718,.F.);
#27907=ORIENTED_EDGE('',*,*,#19715,.F.);
#27908=ORIENTED_EDGE('',*,*,#19703,.F.);
#27909=ORIENTED_EDGE('',*,*,#19707,.T.);
#27910=ORIENTED_EDGE('',*,*,#19711,.F.);
#27911=ORIENTED_EDGE('',*,*,#19713,.F.);
#27912=ORIENTED_EDGE('',*,*,#19493,.F.);
#27913=ORIENTED_EDGE('',*,*,#19527,.F.);
#27914=ORIENTED_EDGE('',*,*,#19735,.T.);
#27915=ORIENTED_EDGE('',*,*,#19696,.F.);
#27916=ORIENTED_EDGE('',*,*,#19700,.F.);
#27917=ORIENTED_EDGE('',*,*,#19698,.F.);
#27918=ORIENTED_EDGE('',*,*,#19691,.T.);
#27919=ORIENTED_EDGE('',*,*,#19497,.F.);
#27920=ORIENTED_EDGE('',*,*,#19456,.T.);
#27921=ORIENTED_EDGE('',*,*,#19737,.F.);
#27922=ORIENTED_EDGE('',*,*,#19738,.F.);
#27923=ORIENTED_EDGE('',*,*,#19739,.F.);
#27924=ORIENTED_EDGE('',*,*,#19740,.F.);
#27925=ORIENTED_EDGE('',*,*,#19741,.F.);
#27926=ORIENTED_EDGE('',*,*,#19742,.F.);
#27927=ORIENTED_EDGE('',*,*,#19743,.F.);
#27928=ORIENTED_EDGE('',*,*,#19744,.F.);
#27929=ORIENTED_EDGE('',*,*,#19745,.F.);
#27930=ORIENTED_EDGE('',*,*,#19746,.F.);
#27931=ORIENTED_EDGE('',*,*,#19747,.F.);
#27932=ORIENTED_EDGE('',*,*,#19748,.F.);
#27933=ORIENTED_EDGE('',*,*,#19749,.F.);
#27934=ORIENTED_EDGE('',*,*,#19450,.T.);
#27935=ORIENTED_EDGE('',*,*,#19750,.T.);
#27936=ORIENTED_EDGE('',*,*,#19738,.T.);
#27937=ORIENTED_EDGE('',*,*,#19751,.F.);
#27938=ORIENTED_EDGE('',*,*,#19451,.F.);
#27939=ORIENTED_EDGE('',*,*,#19749,.T.);
#27940=ORIENTED_EDGE('',*,*,#19737,.T.);
#27941=ORIENTED_EDGE('',*,*,#19752,.F.);
#27942=ORIENTED_EDGE('',*,*,#19452,.T.);
#27943=ORIENTED_EDGE('',*,*,#19751,.T.);
#27944=ORIENTED_EDGE('',*,*,#19748,.T.);
#27945=ORIENTED_EDGE('',*,*,#19753,.F.);
#27946=ORIENTED_EDGE('',*,*,#19754,.F.);
#27947=ORIENTED_EDGE('',*,*,#19443,.F.);
#27948=ORIENTED_EDGE('',*,*,#19752,.T.);
#27949=ORIENTED_EDGE('',*,*,#19747,.T.);
#27950=ORIENTED_EDGE('',*,*,#19755,.F.);
#27951=ORIENTED_EDGE('',*,*,#19756,.T.);
#27952=ORIENTED_EDGE('',*,*,#19753,.T.);
#27953=ORIENTED_EDGE('',*,*,#19746,.T.);
#27954=ORIENTED_EDGE('',*,*,#19757,.F.);
#27955=ORIENTED_EDGE('',*,*,#19758,.F.);
#27956=ORIENTED_EDGE('',*,*,#19755,.T.);
#27957=ORIENTED_EDGE('',*,*,#19745,.T.);
#27958=ORIENTED_EDGE('',*,*,#19759,.F.);
#27959=ORIENTED_EDGE('',*,*,#19760,.T.);
#27960=ORIENTED_EDGE('',*,*,#19757,.T.);
#27961=ORIENTED_EDGE('',*,*,#19744,.T.);
#27962=ORIENTED_EDGE('',*,*,#19761,.F.);
#27963=ORIENTED_EDGE('',*,*,#19762,.F.);
#27964=ORIENTED_EDGE('',*,*,#19759,.T.);
#27965=ORIENTED_EDGE('',*,*,#19743,.T.);
#27966=ORIENTED_EDGE('',*,*,#19763,.F.);
#27967=ORIENTED_EDGE('',*,*,#19764,.T.);
#27968=ORIENTED_EDGE('',*,*,#19761,.T.);
#27969=ORIENTED_EDGE('',*,*,#19742,.T.);
#27970=ORIENTED_EDGE('',*,*,#19765,.F.);
#27971=ORIENTED_EDGE('',*,*,#19447,.F.);
#27972=ORIENTED_EDGE('',*,*,#19766,.F.);
#27973=ORIENTED_EDGE('',*,*,#19763,.T.);
#27974=ORIENTED_EDGE('',*,*,#19741,.T.);
#27975=ORIENTED_EDGE('',*,*,#19767,.F.);
#27976=ORIENTED_EDGE('',*,*,#19448,.T.);
#27977=ORIENTED_EDGE('',*,*,#19765,.T.);
#27978=ORIENTED_EDGE('',*,*,#19740,.T.);
#27979=ORIENTED_EDGE('',*,*,#19750,.F.);
#27980=ORIENTED_EDGE('',*,*,#19449,.T.);
#27981=ORIENTED_EDGE('',*,*,#19767,.T.);
#27982=ORIENTED_EDGE('',*,*,#19739,.T.);
#27983=ORIENTED_EDGE('',*,*,#19444,.F.);
#27984=ORIENTED_EDGE('',*,*,#19754,.T.);
#27985=ORIENTED_EDGE('',*,*,#19756,.F.);
#27986=ORIENTED_EDGE('',*,*,#19758,.T.);
#27987=ORIENTED_EDGE('',*,*,#19760,.F.);
#27988=ORIENTED_EDGE('',*,*,#19762,.T.);
#27989=ORIENTED_EDGE('',*,*,#19764,.F.);
#27990=ORIENTED_EDGE('',*,*,#19766,.T.);
#27991=ORIENTED_EDGE('',*,*,#19446,.T.);
#27992=ORIENTED_EDGE('',*,*,#19465,.F.);
#27993=ORIENTED_EDGE('',*,*,#19768,.F.);
#27994=ORIENTED_EDGE('',*,*,#19769,.F.);
#27995=ORIENTED_EDGE('',*,*,#19770,.T.);
#27996=ORIENTED_EDGE('',*,*,#19771,.T.);
#27997=ORIENTED_EDGE('',*,*,#19772,.F.);
#27998=ORIENTED_EDGE('',*,*,#19773,.T.);
#27999=ORIENTED_EDGE('',*,*,#19774,.T.);
#28000=ORIENTED_EDGE('',*,*,#19770,.F.);
#28001=ORIENTED_EDGE('',*,*,#19775,.F.);
#28002=ORIENTED_EDGE('',*,*,#19776,.F.);
#28003=ORIENTED_EDGE('',*,*,#19777,.F.);
#28004=ORIENTED_EDGE('',*,*,#19778,.T.);
#28005=ORIENTED_EDGE('',*,*,#19779,.T.);
#28006=ORIENTED_EDGE('',*,*,#19773,.F.);
#28007=ORIENTED_EDGE('',*,*,#19780,.F.);
#28008=ORIENTED_EDGE('',*,*,#19781,.T.);
#28009=ORIENTED_EDGE('',*,*,#19782,.T.);
#28010=ORIENTED_EDGE('',*,*,#19783,.T.);
#28011=ORIENTED_EDGE('',*,*,#19784,.F.);
#28012=ORIENTED_EDGE('',*,*,#19785,.T.);
#28013=ORIENTED_EDGE('',*,*,#19786,.T.);
#28014=ORIENTED_EDGE('',*,*,#19787,.T.);
#28015=ORIENTED_EDGE('',*,*,#19788,.T.);
#28016=ORIENTED_EDGE('',*,*,#19789,.T.);
#28017=ORIENTED_EDGE('',*,*,#19784,.T.);
#28018=ORIENTED_EDGE('',*,*,#19790,.T.);
#28019=ORIENTED_EDGE('',*,*,#19791,.T.);
#28020=ORIENTED_EDGE('',*,*,#19792,.T.);
#28021=ORIENTED_EDGE('',*,*,#19793,.T.);
#28022=ORIENTED_EDGE('',*,*,#19788,.F.);
#28023=ORIENTED_EDGE('',*,*,#19794,.T.);
#28024=ORIENTED_EDGE('',*,*,#19795,.T.);
#28025=ORIENTED_EDGE('',*,*,#19792,.F.);
#28026=ORIENTED_EDGE('',*,*,#19796,.T.);
#28027=ORIENTED_EDGE('',*,*,#19797,.T.);
#28028=ORIENTED_EDGE('',*,*,#19798,.T.);
#28029=ORIENTED_EDGE('',*,*,#19799,.T.);
#28030=ORIENTED_EDGE('',*,*,#19800,.T.);
#28031=ORIENTED_EDGE('',*,*,#19801,.T.);
#28032=ORIENTED_EDGE('',*,*,#19794,.F.);
#28033=ORIENTED_EDGE('',*,*,#19802,.F.);
#28034=ORIENTED_EDGE('',*,*,#19803,.T.);
#28035=ORIENTED_EDGE('',*,*,#19800,.F.);
#28036=ORIENTED_EDGE('',*,*,#19804,.T.);
#28037=ORIENTED_EDGE('',*,*,#19805,.T.);
#28038=ORIENTED_EDGE('',*,*,#19806,.F.);
#28039=ORIENTED_EDGE('',*,*,#19807,.F.);
#28040=ORIENTED_EDGE('',*,*,#19808,.F.);
#28041=ORIENTED_EDGE('',*,*,#19809,.T.);
#28042=ORIENTED_EDGE('',*,*,#19808,.T.);
#28043=ORIENTED_EDGE('',*,*,#19771,.F.);
#28044=ORIENTED_EDGE('',*,*,#19810,.F.);
#28045=ORIENTED_EDGE('',*,*,#19811,.T.);
#28046=ORIENTED_EDGE('',*,*,#19810,.T.);
#28047=ORIENTED_EDGE('',*,*,#19774,.F.);
#28048=ORIENTED_EDGE('',*,*,#19812,.F.);
#28049=ORIENTED_EDGE('',*,*,#19812,.T.);
#28050=ORIENTED_EDGE('',*,*,#19779,.F.);
#28051=ORIENTED_EDGE('',*,*,#19813,.F.);
#28052=ORIENTED_EDGE('',*,*,#19814,.T.);
#28053=ORIENTED_EDGE('',*,*,#19813,.T.);
#28054=ORIENTED_EDGE('',*,*,#19815,.F.);
#28055=ORIENTED_EDGE('',*,*,#19816,.F.);
#28056=ORIENTED_EDGE('',*,*,#19817,.T.);
#28057=ORIENTED_EDGE('',*,*,#19816,.T.);
#28058=ORIENTED_EDGE('',*,*,#19818,.F.);
#28059=ORIENTED_EDGE('',*,*,#19819,.F.);
#28060=ORIENTED_EDGE('',*,*,#19820,.T.);
#28061=ORIENTED_EDGE('',*,*,#19819,.T.);
#28062=ORIENTED_EDGE('',*,*,#19821,.F.);
#28063=ORIENTED_EDGE('',*,*,#19822,.F.);
#28064=ORIENTED_EDGE('',*,*,#19823,.T.);
#28065=ORIENTED_EDGE('',*,*,#19822,.T.);
#28066=ORIENTED_EDGE('',*,*,#19781,.F.);
#28067=ORIENTED_EDGE('',*,*,#19824,.F.);
#28068=ORIENTED_EDGE('',*,*,#19825,.T.);
#28069=ORIENTED_EDGE('',*,*,#19824,.T.);
#28070=ORIENTED_EDGE('',*,*,#19826,.F.);
#28071=ORIENTED_EDGE('',*,*,#19827,.F.);
#28072=ORIENTED_EDGE('',*,*,#19828,.T.);
#28073=ORIENTED_EDGE('',*,*,#19827,.T.);
#28074=ORIENTED_EDGE('',*,*,#19785,.F.);
#28075=ORIENTED_EDGE('',*,*,#19829,.F.);
#28076=ORIENTED_EDGE('',*,*,#19830,.T.);
#28077=ORIENTED_EDGE('',*,*,#19829,.T.);
#28078=ORIENTED_EDGE('',*,*,#19789,.F.);
#28079=ORIENTED_EDGE('',*,*,#19831,.F.);
#28080=ORIENTED_EDGE('',*,*,#19831,.T.);
#28081=ORIENTED_EDGE('',*,*,#19793,.F.);
#28082=ORIENTED_EDGE('',*,*,#19832,.F.);
#28083=ORIENTED_EDGE('',*,*,#19833,.T.);
#28084=ORIENTED_EDGE('',*,*,#19832,.T.);
#28085=ORIENTED_EDGE('',*,*,#19795,.F.);
#28086=ORIENTED_EDGE('',*,*,#19834,.F.);
#28087=ORIENTED_EDGE('',*,*,#19834,.T.);
#28088=ORIENTED_EDGE('',*,*,#19801,.F.);
#28089=ORIENTED_EDGE('',*,*,#19835,.F.);
#28090=ORIENTED_EDGE('',*,*,#19836,.F.);
#28091=ORIENTED_EDGE('',*,*,#19837,.T.);
#28092=ORIENTED_EDGE('',*,*,#19835,.T.);
#28093=ORIENTED_EDGE('',*,*,#19803,.F.);
#28094=ORIENTED_EDGE('',*,*,#19838,.F.);
#28095=ORIENTED_EDGE('',*,*,#19839,.F.);
#28096=ORIENTED_EDGE('',*,*,#19809,.F.);
#28097=ORIENTED_EDGE('',*,*,#19811,.F.);
#28098=ORIENTED_EDGE('',*,*,#19814,.F.);
#28099=ORIENTED_EDGE('',*,*,#19817,.F.);
#28100=ORIENTED_EDGE('',*,*,#19820,.F.);
#28101=ORIENTED_EDGE('',*,*,#19823,.F.);
#28102=ORIENTED_EDGE('',*,*,#19825,.F.);
#28103=ORIENTED_EDGE('',*,*,#19828,.F.);
#28104=ORIENTED_EDGE('',*,*,#19830,.F.);
#28105=ORIENTED_EDGE('',*,*,#19833,.F.);
#28106=ORIENTED_EDGE('',*,*,#19837,.F.);
#28107=ORIENTED_EDGE('',*,*,#19840,.T.);
#28108=ORIENTED_EDGE('',*,*,#19841,.T.);
#28109=ORIENTED_EDGE('',*,*,#19842,.F.);
#28110=ORIENTED_EDGE('',*,*,#19843,.F.);
#28111=ORIENTED_EDGE('',*,*,#19844,.F.);
#28112=ORIENTED_EDGE('',*,*,#19845,.F.);
#28113=ORIENTED_EDGE('',*,*,#19846,.F.);
#28114=ORIENTED_EDGE('',*,*,#19847,.F.);
#28115=ORIENTED_EDGE('',*,*,#19848,.T.);
#28116=ORIENTED_EDGE('',*,*,#19849,.T.);
#28117=ORIENTED_EDGE('',*,*,#19840,.F.);
#28118=ORIENTED_EDGE('',*,*,#19850,.T.);
#28119=ORIENTED_EDGE('',*,*,#19851,.T.);
#28120=ORIENTED_EDGE('',*,*,#19848,.F.);
#28121=ORIENTED_EDGE('',*,*,#19852,.F.);
#28122=ORIENTED_EDGE('',*,*,#19853,.F.);
#28123=ORIENTED_EDGE('',*,*,#19854,.T.);
#28124=ORIENTED_EDGE('',*,*,#19855,.T.);
#28125=ORIENTED_EDGE('',*,*,#19850,.F.);
#28126=ORIENTED_EDGE('',*,*,#19856,.F.);
#28127=ORIENTED_EDGE('',*,*,#19857,.F.);
#28128=ORIENTED_EDGE('',*,*,#19858,.T.);
#28129=ORIENTED_EDGE('',*,*,#19854,.F.);
#28130=ORIENTED_EDGE('',*,*,#19859,.F.);
#28131=ORIENTED_EDGE('',*,*,#19860,.T.);
#28132=ORIENTED_EDGE('',*,*,#19857,.T.);
#28133=ORIENTED_EDGE('',*,*,#19861,.F.);
#28134=ORIENTED_EDGE('',*,*,#19862,.T.);
#28135=ORIENTED_EDGE('',*,*,#19842,.T.);
#28136=ORIENTED_EDGE('',*,*,#19863,.T.);
#28137=ORIENTED_EDGE('',*,*,#19864,.F.);
#28138=ORIENTED_EDGE('',*,*,#19865,.T.);
#28139=ORIENTED_EDGE('',*,*,#19866,.T.);
#28140=ORIENTED_EDGE('',*,*,#19841,.F.);
#28141=ORIENTED_EDGE('',*,*,#19867,.F.);
#28142=ORIENTED_EDGE('',*,*,#19867,.T.);
#28143=ORIENTED_EDGE('',*,*,#19849,.F.);
#28144=ORIENTED_EDGE('',*,*,#19868,.F.);
#28145=ORIENTED_EDGE('',*,*,#19869,.T.);
#28146=ORIENTED_EDGE('',*,*,#19868,.T.);
#28147=ORIENTED_EDGE('',*,*,#19851,.F.);
#28148=ORIENTED_EDGE('',*,*,#19870,.F.);
#28149=ORIENTED_EDGE('',*,*,#19870,.T.);
#28150=ORIENTED_EDGE('',*,*,#19855,.F.);
#28151=ORIENTED_EDGE('',*,*,#19871,.F.);
#28152=ORIENTED_EDGE('',*,*,#19872,.T.);
#28153=ORIENTED_EDGE('',*,*,#19871,.T.);
#28154=ORIENTED_EDGE('',*,*,#19858,.F.);
#28155=ORIENTED_EDGE('',*,*,#19873,.F.);
#28156=ORIENTED_EDGE('',*,*,#19874,.T.);
#28157=ORIENTED_EDGE('',*,*,#19873,.T.);
#28158=ORIENTED_EDGE('',*,*,#19860,.F.);
#28159=ORIENTED_EDGE('',*,*,#19875,.F.);
#28160=ORIENTED_EDGE('',*,*,#19876,.F.);
#28161=ORIENTED_EDGE('',*,*,#19877,.T.);
#28162=ORIENTED_EDGE('',*,*,#19875,.T.);
#28163=ORIENTED_EDGE('',*,*,#19878,.F.);
#28164=ORIENTED_EDGE('',*,*,#19879,.T.);
#28165=ORIENTED_EDGE('',*,*,#19863,.F.);
#28166=ORIENTED_EDGE('',*,*,#19866,.F.);
#28167=ORIENTED_EDGE('',*,*,#19880,.T.);
#28168=ORIENTED_EDGE('',*,*,#19881,.F.);
#28169=ORIENTED_EDGE('',*,*,#19879,.F.);
#28170=ORIENTED_EDGE('',*,*,#19882,.T.);
#28171=ORIENTED_EDGE('',*,*,#19883,.F.);
#28172=ORIENTED_EDGE('',*,*,#19884,.F.);
#28173=ORIENTED_EDGE('',*,*,#19885,.T.);
#28174=ORIENTED_EDGE('',*,*,#19886,.F.);
#28175=ORIENTED_EDGE('',*,*,#19887,.T.);
#28176=ORIENTED_EDGE('',*,*,#19888,.F.);
#28177=ORIENTED_EDGE('',*,*,#19889,.F.);
#28178=ORIENTED_EDGE('',*,*,#19890,.T.);
#28179=ORIENTED_EDGE('',*,*,#19891,.T.);
#28180=ORIENTED_EDGE('',*,*,#19892,.T.);
#28181=ORIENTED_EDGE('',*,*,#19893,.F.);
#28182=ORIENTED_EDGE('',*,*,#19894,.T.);
#28183=ORIENTED_EDGE('',*,*,#19895,.F.);
#28184=ORIENTED_EDGE('',*,*,#19896,.F.);
#28185=ORIENTED_EDGE('',*,*,#19897,.T.);
#28186=ORIENTED_EDGE('',*,*,#19898,.T.);
#28187=ORIENTED_EDGE('',*,*,#19884,.T.);
#28188=ORIENTED_EDGE('',*,*,#19899,.F.);
#28189=ORIENTED_EDGE('',*,*,#19898,.F.);
#28190=ORIENTED_EDGE('',*,*,#19900,.F.);
#28191=ORIENTED_EDGE('',*,*,#19901,.F.);
#28192=ORIENTED_EDGE('',*,*,#19883,.T.);
#28193=ORIENTED_EDGE('',*,*,#19902,.F.);
#28194=ORIENTED_EDGE('',*,*,#19903,.T.);
#28195=ORIENTED_EDGE('',*,*,#19886,.T.);
#28196=ORIENTED_EDGE('',*,*,#19890,.F.);
#28197=ORIENTED_EDGE('',*,*,#19904,.F.);
#28198=ORIENTED_EDGE('',*,*,#19905,.T.);
#28199=ORIENTED_EDGE('',*,*,#19889,.T.);
#28200=ORIENTED_EDGE('',*,*,#19906,.F.);
#28201=ORIENTED_EDGE('',*,*,#19907,.T.);
#28202=ORIENTED_EDGE('',*,*,#19888,.T.);
#28203=ORIENTED_EDGE('',*,*,#19894,.F.);
#28204=ORIENTED_EDGE('',*,*,#19908,.T.);
#28205=ORIENTED_EDGE('',*,*,#19893,.T.);
#28206=ORIENTED_EDGE('',*,*,#19909,.T.);
#28207=ORIENTED_EDGE('',*,*,#19910,.F.);
#28208=ORIENTED_EDGE('',*,*,#19896,.T.);
#28209=ORIENTED_EDGE('',*,*,#19911,.F.);
#28210=ORIENTED_EDGE('',*,*,#19892,.F.);
#28211=ORIENTED_EDGE('',*,*,#19912,.F.);
#28212=ORIENTED_EDGE('',*,*,#19895,.T.);
#28213=ORIENTED_EDGE('',*,*,#19913,.T.);
#28214=ORIENTED_EDGE('',*,*,#19914,.F.);
#28215=ORIENTED_EDGE('',*,*,#19913,.F.);
#28216=ORIENTED_EDGE('',*,*,#19899,.T.);
#28217=ORIENTED_EDGE('',*,*,#19901,.T.);
#28218=ORIENTED_EDGE('',*,*,#19915,.F.);
#28219=ORIENTED_EDGE('',*,*,#19900,.T.);
#28220=ORIENTED_EDGE('',*,*,#19916,.T.);
#28221=ORIENTED_EDGE('',*,*,#19917,.F.);
#28222=ORIENTED_EDGE('',*,*,#19918,.F.);
#28223=ORIENTED_EDGE('',*,*,#19902,.T.);
#28224=ORIENTED_EDGE('',*,*,#19903,.F.);
#28225=ORIENTED_EDGE('',*,*,#19905,.F.);
#28226=ORIENTED_EDGE('',*,*,#19919,.F.);
#28227=ORIENTED_EDGE('',*,*,#19904,.T.);
#28228=ORIENTED_EDGE('',*,*,#19920,.T.);
#28229=ORIENTED_EDGE('',*,*,#19921,.F.);
#28230=ORIENTED_EDGE('',*,*,#19922,.F.);
#28231=ORIENTED_EDGE('',*,*,#19906,.T.);
#28232=ORIENTED_EDGE('',*,*,#19907,.F.);
#28233=ORIENTED_EDGE('',*,*,#19908,.F.);
#28234=ORIENTED_EDGE('',*,*,#19923,.F.);
#28235=ORIENTED_EDGE('',*,*,#19910,.T.);
#28236=ORIENTED_EDGE('',*,*,#19924,.T.);
#28237=ORIENTED_EDGE('',*,*,#19925,.F.);
#28238=ORIENTED_EDGE('',*,*,#19926,.F.);
#28239=ORIENTED_EDGE('',*,*,#19909,.F.);
#28240=ORIENTED_EDGE('',*,*,#19911,.T.);
#28241=ORIENTED_EDGE('',*,*,#19912,.T.);
#28242=ORIENTED_EDGE('',*,*,#19927,.F.);
#28243=ORIENTED_EDGE('',*,*,#19914,.T.);
#28244=ORIENTED_EDGE('',*,*,#19928,.T.);
#28245=ORIENTED_EDGE('',*,*,#19929,.F.);
#28246=ORIENTED_EDGE('',*,*,#19930,.F.);
#28247=ORIENTED_EDGE('',*,*,#19915,.T.);
#28248=ORIENTED_EDGE('',*,*,#19918,.T.);
#28249=ORIENTED_EDGE('',*,*,#19931,.F.);
#28250=ORIENTED_EDGE('',*,*,#19928,.F.);
#28251=ORIENTED_EDGE('',*,*,#19932,.T.);
#28252=ORIENTED_EDGE('',*,*,#19933,.T.);
#28253=ORIENTED_EDGE('',*,*,#19934,.F.);
#28254=ORIENTED_EDGE('',*,*,#19919,.T.);
#28255=ORIENTED_EDGE('',*,*,#19922,.T.);
#28256=ORIENTED_EDGE('',*,*,#19935,.F.);
#28257=ORIENTED_EDGE('',*,*,#19916,.F.);
#28258=ORIENTED_EDGE('',*,*,#19923,.T.);
#28259=ORIENTED_EDGE('',*,*,#19926,.T.);
#28260=ORIENTED_EDGE('',*,*,#19936,.F.);
#28261=ORIENTED_EDGE('',*,*,#19920,.F.);
#28262=ORIENTED_EDGE('',*,*,#19927,.T.);
#28263=ORIENTED_EDGE('',*,*,#19930,.T.);
#28264=ORIENTED_EDGE('',*,*,#19937,.F.);
#28265=ORIENTED_EDGE('',*,*,#19924,.F.);
#28266=ORIENTED_EDGE('',*,*,#19938,.F.);
#28267=ORIENTED_EDGE('',*,*,#19939,.F.);
#28268=ORIENTED_EDGE('',*,*,#19940,.T.);
#28269=ORIENTED_EDGE('',*,*,#19941,.T.);
#28270=ORIENTED_EDGE('',*,*,#19897,.F.);
#28271=ORIENTED_EDGE('',*,*,#19891,.F.);
#28272=ORIENTED_EDGE('',*,*,#19887,.F.);
#28273=ORIENTED_EDGE('',*,*,#19885,.F.);
#28274=ORIENTED_EDGE('',*,*,#19942,.T.);
#28275=ORIENTED_EDGE('',*,*,#19844,.T.);
#28276=ORIENTED_EDGE('',*,*,#19943,.F.);
#28277=ORIENTED_EDGE('',*,*,#19944,.F.);
#28278=ORIENTED_EDGE('',*,*,#19944,.T.);
#28279=ORIENTED_EDGE('',*,*,#19945,.F.);
#28280=ORIENTED_EDGE('',*,*,#19946,.F.);
#28281=ORIENTED_EDGE('',*,*,#19947,.T.);
#28282=ORIENTED_EDGE('',*,*,#19948,.T.);
#28283=ORIENTED_EDGE('',*,*,#19949,.T.);
#28284=ORIENTED_EDGE('',*,*,#19950,.T.);
#28285=ORIENTED_EDGE('',*,*,#19951,.F.);
#28286=ORIENTED_EDGE('',*,*,#19952,.T.);
#28287=ORIENTED_EDGE('',*,*,#19953,.T.);
#28288=ORIENTED_EDGE('',*,*,#19954,.T.);
#28289=ORIENTED_EDGE('',*,*,#19955,.T.);
#28290=ORIENTED_EDGE('',*,*,#19956,.T.);
#28291=ORIENTED_EDGE('',*,*,#19957,.T.);
#28292=ORIENTED_EDGE('',*,*,#19958,.T.);
#28293=ORIENTED_EDGE('',*,*,#19959,.T.);
#28294=ORIENTED_EDGE('',*,*,#19960,.T.);
#28295=ORIENTED_EDGE('',*,*,#19961,.T.);
#28296=ORIENTED_EDGE('',*,*,#19962,.T.);
#28297=ORIENTED_EDGE('',*,*,#19864,.T.);
#28298=ORIENTED_EDGE('',*,*,#19881,.T.);
#28299=ORIENTED_EDGE('',*,*,#19963,.T.);
#28300=ORIENTED_EDGE('',*,*,#19964,.T.);
#28301=ORIENTED_EDGE('',*,*,#19965,.T.);
#28302=ORIENTED_EDGE('',*,*,#19966,.T.);
#28303=ORIENTED_EDGE('',*,*,#19967,.T.);
#28304=ORIENTED_EDGE('',*,*,#19968,.F.);
#28305=ORIENTED_EDGE('',*,*,#19969,.T.);
#28306=ORIENTED_EDGE('',*,*,#19970,.T.);
#28307=ORIENTED_EDGE('',*,*,#19971,.T.);
#28308=ORIENTED_EDGE('',*,*,#19965,.F.);
#28309=ORIENTED_EDGE('',*,*,#19972,.T.);
#28310=ORIENTED_EDGE('',*,*,#19973,.T.);
#28311=ORIENTED_EDGE('',*,*,#19974,.T.);
#28312=ORIENTED_EDGE('',*,*,#19975,.T.);
#28313=ORIENTED_EDGE('',*,*,#19976,.T.);
#28314=ORIENTED_EDGE('',*,*,#19970,.F.);
#28315=ORIENTED_EDGE('',*,*,#19977,.T.);
#28316=ORIENTED_EDGE('',*,*,#19978,.T.);
#28317=ORIENTED_EDGE('',*,*,#19979,.T.);
#28318=ORIENTED_EDGE('',*,*,#19973,.F.);
#28319=ORIENTED_EDGE('',*,*,#19980,.T.);
#28320=ORIENTED_EDGE('',*,*,#19981,.T.);
#28321=ORIENTED_EDGE('',*,*,#19982,.T.);
#28322=ORIENTED_EDGE('',*,*,#19983,.T.);
#28323=ORIENTED_EDGE('',*,*,#19984,.T.);
#28324=ORIENTED_EDGE('',*,*,#19978,.F.);
#28325=ORIENTED_EDGE('',*,*,#19985,.T.);
#28326=ORIENTED_EDGE('',*,*,#19951,.T.);
#28327=ORIENTED_EDGE('',*,*,#19986,.T.);
#28328=ORIENTED_EDGE('',*,*,#19981,.F.);
#28329=ORIENTED_EDGE('',*,*,#19806,.T.);
#28330=ORIENTED_EDGE('',*,*,#19987,.T.);
#28331=ORIENTED_EDGE('',*,*,#19988,.F.);
#28332=ORIENTED_EDGE('',*,*,#19839,.T.);
#28333=ORIENTED_EDGE('',*,*,#19989,.T.);
#28334=ORIENTED_EDGE('',*,*,#19990,.F.);
#28335=ORIENTED_EDGE('',*,*,#19987,.F.);
#28336=ORIENTED_EDGE('',*,*,#19991,.T.);
#28337=ORIENTED_EDGE('',*,*,#19988,.T.);
#28338=ORIENTED_EDGE('',*,*,#19992,.F.);
#28339=ORIENTED_EDGE('',*,*,#19993,.F.);
#28340=ORIENTED_EDGE('',*,*,#19991,.F.);
#28341=ORIENTED_EDGE('',*,*,#19994,.F.);
#28342=ORIENTED_EDGE('',*,*,#19995,.F.);
#28343=ORIENTED_EDGE('',*,*,#19996,.F.);
#28344=ORIENTED_EDGE('',*,*,#19997,.F.);
#28345=ORIENTED_EDGE('',*,*,#19998,.T.);
#28346=ORIENTED_EDGE('',*,*,#19999,.F.);
#28347=ORIENTED_EDGE('',*,*,#19772,.T.);
#28348=ORIENTED_EDGE('',*,*,#19807,.T.);
#28349=ORIENTED_EDGE('',*,*,#19998,.F.);
#28350=ORIENTED_EDGE('',*,*,#20000,.F.);
#28351=ORIENTED_EDGE('',*,*,#20001,.T.);
#28352=ORIENTED_EDGE('',*,*,#20002,.F.);
#28353=ORIENTED_EDGE('',*,*,#20003,.F.);
#28354=ORIENTED_EDGE('',*,*,#20001,.F.);
#28355=ORIENTED_EDGE('',*,*,#20004,.F.);
#28356=ORIENTED_EDGE('',*,*,#20005,.T.);
#28357=ORIENTED_EDGE('',*,*,#20005,.F.);
#28358=ORIENTED_EDGE('',*,*,#20006,.F.);
#28359=ORIENTED_EDGE('',*,*,#20007,.T.);
#28360=ORIENTED_EDGE('',*,*,#20008,.F.);
#28361=ORIENTED_EDGE('',*,*,#20009,.F.);
#28362=ORIENTED_EDGE('',*,*,#20007,.F.);
#28363=ORIENTED_EDGE('',*,*,#20010,.F.);
#28364=ORIENTED_EDGE('',*,*,#20011,.T.);
#28365=ORIENTED_EDGE('',*,*,#20012,.F.);
#28366=ORIENTED_EDGE('',*,*,#20013,.F.);
#28367=ORIENTED_EDGE('',*,*,#19996,.T.);
#28368=ORIENTED_EDGE('',*,*,#20014,.F.);
#28369=ORIENTED_EDGE('',*,*,#20011,.F.);
#28370=ORIENTED_EDGE('',*,*,#20015,.F.);
#28371=ORIENTED_EDGE('',*,*,#20016,.T.);
#28372=ORIENTED_EDGE('',*,*,#20017,.F.);
#28373=ORIENTED_EDGE('',*,*,#20016,.F.);
#28374=ORIENTED_EDGE('',*,*,#20018,.F.);
#28375=ORIENTED_EDGE('',*,*,#20012,.T.);
#28376=ORIENTED_EDGE('',*,*,#20019,.F.);
#28377=ORIENTED_EDGE('',*,*,#20020,.T.);
#28378=ORIENTED_EDGE('',*,*,#20021,.T.);
#28379=ORIENTED_EDGE('',*,*,#20022,.F.);
#28380=ORIENTED_EDGE('',*,*,#20023,.F.);
#28381=ORIENTED_EDGE('',*,*,#20024,.T.);
#28382=ORIENTED_EDGE('',*,*,#20025,.T.);
#28383=ORIENTED_EDGE('',*,*,#20026,.F.);
#28384=ORIENTED_EDGE('',*,*,#20027,.F.);
#28385=ORIENTED_EDGE('',*,*,#20028,.T.);
#28386=ORIENTED_EDGE('',*,*,#20027,.T.);
#28387=ORIENTED_EDGE('',*,*,#20029,.F.);
#28388=ORIENTED_EDGE('',*,*,#20030,.F.);
#28389=ORIENTED_EDGE('',*,*,#20031,.T.);
#28390=ORIENTED_EDGE('',*,*,#20030,.T.);
#28391=ORIENTED_EDGE('',*,*,#20032,.F.);
#28392=ORIENTED_EDGE('',*,*,#20033,.F.);
#28393=ORIENTED_EDGE('',*,*,#20034,.T.);
#28394=ORIENTED_EDGE('',*,*,#20033,.T.);
#28395=ORIENTED_EDGE('',*,*,#20035,.F.);
#28396=ORIENTED_EDGE('',*,*,#20036,.F.);
#28397=ORIENTED_EDGE('',*,*,#20037,.T.);
#28398=ORIENTED_EDGE('',*,*,#20036,.T.);
#28399=ORIENTED_EDGE('',*,*,#20038,.F.);
#28400=ORIENTED_EDGE('',*,*,#20039,.F.);
#28401=ORIENTED_EDGE('',*,*,#20040,.T.);
#28402=ORIENTED_EDGE('',*,*,#20041,.T.);
#28403=ORIENTED_EDGE('',*,*,#20042,.F.);
#28404=ORIENTED_EDGE('',*,*,#20025,.F.);
#28405=ORIENTED_EDGE('',*,*,#20043,.T.);
#28406=ORIENTED_EDGE('',*,*,#20039,.T.);
#28407=ORIENTED_EDGE('',*,*,#20044,.F.);
#28408=ORIENTED_EDGE('',*,*,#20045,.F.);
#28409=ORIENTED_EDGE('',*,*,#20046,.T.);
#28410=ORIENTED_EDGE('',*,*,#20045,.T.);
#28411=ORIENTED_EDGE('',*,*,#20047,.F.);
#28412=ORIENTED_EDGE('',*,*,#20041,.F.);
#28413=ORIENTED_EDGE('',*,*,#20048,.T.);
#28414=ORIENTED_EDGE('',*,*,#20049,.T.);
#28415=ORIENTED_EDGE('',*,*,#20050,.F.);
#28416=ORIENTED_EDGE('',*,*,#20051,.F.);
#28417=ORIENTED_EDGE('',*,*,#20052,.T.);
#28418=ORIENTED_EDGE('',*,*,#20053,.T.);
#28419=ORIENTED_EDGE('',*,*,#20054,.F.);
#28420=ORIENTED_EDGE('',*,*,#19983,.F.);
#28421=ORIENTED_EDGE('',*,*,#20053,.F.);
#28422=ORIENTED_EDGE('',*,*,#20055,.F.);
#28423=ORIENTED_EDGE('',*,*,#20049,.F.);
#28424=ORIENTED_EDGE('',*,*,#20056,.T.);
#28425=ORIENTED_EDGE('',*,*,#20057,.T.);
#28426=ORIENTED_EDGE('',*,*,#20058,.T.);
#28427=ORIENTED_EDGE('',*,*,#20059,.T.);
#28428=ORIENTED_EDGE('',*,*,#20060,.F.);
#28429=ORIENTED_EDGE('',*,*,#19974,.F.);
#28430=ORIENTED_EDGE('',*,*,#20061,.T.);
#28431=ORIENTED_EDGE('',*,*,#20062,.T.);
#28432=ORIENTED_EDGE('',*,*,#20058,.F.);
#28433=ORIENTED_EDGE('',*,*,#19979,.F.);
#28434=ORIENTED_EDGE('',*,*,#20054,.T.);
#28435=ORIENTED_EDGE('',*,*,#20063,.T.);
#28436=ORIENTED_EDGE('',*,*,#20061,.F.);
#28437=ORIENTED_EDGE('',*,*,#19984,.F.);
#28438=ORIENTED_EDGE('',*,*,#20059,.F.);
#28439=ORIENTED_EDGE('',*,*,#20062,.F.);
#28440=ORIENTED_EDGE('',*,*,#20063,.F.);
#28441=ORIENTED_EDGE('',*,*,#20057,.F.);
#28442=ORIENTED_EDGE('',*,*,#20064,.T.);
#28443=ORIENTED_EDGE('',*,*,#20065,.T.);
#28444=ORIENTED_EDGE('',*,*,#20066,.F.);
#28445=ORIENTED_EDGE('',*,*,#20067,.T.);
#28446=ORIENTED_EDGE('',*,*,#20051,.T.);
#28447=ORIENTED_EDGE('',*,*,#20068,.F.);
#28448=ORIENTED_EDGE('',*,*,#20069,.F.);
#28449=ORIENTED_EDGE('',*,*,#20070,.T.);
#28450=ORIENTED_EDGE('',*,*,#20071,.T.);
#28451=ORIENTED_EDGE('',*,*,#20072,.F.);
#28452=ORIENTED_EDGE('',*,*,#20065,.F.);
#28453=ORIENTED_EDGE('',*,*,#20073,.T.);
#28454=ORIENTED_EDGE('',*,*,#20069,.T.);
#28455=ORIENTED_EDGE('',*,*,#20074,.F.);
#28456=ORIENTED_EDGE('',*,*,#20071,.F.);
#28457=ORIENTED_EDGE('',*,*,#20075,.T.);
#28458=ORIENTED_EDGE('',*,*,#20076,.T.);
#28459=ORIENTED_EDGE('',*,*,#20077,.F.);
#28460=ORIENTED_EDGE('',*,*,#19966,.F.);
#28461=ORIENTED_EDGE('',*,*,#20078,.T.);
#28462=ORIENTED_EDGE('',*,*,#20079,.T.);
#28463=ORIENTED_EDGE('',*,*,#20075,.F.);
#28464=ORIENTED_EDGE('',*,*,#19971,.F.);
#28465=ORIENTED_EDGE('',*,*,#20080,.T.);
#28466=ORIENTED_EDGE('',*,*,#20081,.T.);
#28467=ORIENTED_EDGE('',*,*,#20078,.F.);
#28468=ORIENTED_EDGE('',*,*,#19976,.F.);
#28469=ORIENTED_EDGE('',*,*,#20076,.F.);
#28470=ORIENTED_EDGE('',*,*,#20079,.F.);
#28471=ORIENTED_EDGE('',*,*,#20081,.F.);
#28472=ORIENTED_EDGE('',*,*,#20082,.T.);
#28473=ORIENTED_EDGE('',*,*,#20083,.T.);
#28474=ORIENTED_EDGE('',*,*,#20084,.F.);
#28475=ORIENTED_EDGE('',*,*,#20085,.F.);
#28476=ORIENTED_EDGE('',*,*,#20086,.T.);
#28477=ORIENTED_EDGE('',*,*,#20087,.T.);
#28478=ORIENTED_EDGE('',*,*,#20085,.T.);
#28479=ORIENTED_EDGE('',*,*,#20088,.F.);
#28480=ORIENTED_EDGE('',*,*,#20089,.F.);
#28481=ORIENTED_EDGE('',*,*,#20090,.T.);
#28482=ORIENTED_EDGE('',*,*,#20089,.T.);
#28483=ORIENTED_EDGE('',*,*,#20091,.F.);
#28484=ORIENTED_EDGE('',*,*,#20092,.F.);
#28485=ORIENTED_EDGE('',*,*,#20093,.T.);
#28486=ORIENTED_EDGE('',*,*,#20092,.T.);
#28487=ORIENTED_EDGE('',*,*,#20094,.F.);
#28488=ORIENTED_EDGE('',*,*,#20095,.F.);
#28489=ORIENTED_EDGE('',*,*,#20096,.T.);
#28490=ORIENTED_EDGE('',*,*,#20095,.T.);
#28491=ORIENTED_EDGE('',*,*,#20097,.F.);
#28492=ORIENTED_EDGE('',*,*,#20098,.F.);
#28493=ORIENTED_EDGE('',*,*,#20099,.T.);
#28494=ORIENTED_EDGE('',*,*,#20100,.T.);
#28495=ORIENTED_EDGE('',*,*,#20101,.F.);
#28496=ORIENTED_EDGE('',*,*,#20083,.F.);
#28497=ORIENTED_EDGE('',*,*,#20102,.T.);
#28498=ORIENTED_EDGE('',*,*,#20098,.T.);
#28499=ORIENTED_EDGE('',*,*,#20103,.F.);
#28500=ORIENTED_EDGE('',*,*,#20104,.F.);
#28501=ORIENTED_EDGE('',*,*,#20105,.T.);
#28502=ORIENTED_EDGE('',*,*,#20104,.T.);
#28503=ORIENTED_EDGE('',*,*,#20106,.F.);
#28504=ORIENTED_EDGE('',*,*,#20100,.F.);
#28505=ORIENTED_EDGE('',*,*,#20107,.T.);
#28506=ORIENTED_EDGE('',*,*,#20108,.T.);
#28507=ORIENTED_EDGE('',*,*,#20109,.F.);
#28508=ORIENTED_EDGE('',*,*,#20110,.F.);
#28509=ORIENTED_EDGE('',*,*,#20111,.T.);
#28510=ORIENTED_EDGE('',*,*,#20112,.F.);
#28511=ORIENTED_EDGE('',*,*,#20113,.F.);
#28512=ORIENTED_EDGE('',*,*,#19934,.T.);
#28513=ORIENTED_EDGE('',*,*,#20114,.F.);
#28514=ORIENTED_EDGE('',*,*,#20115,.F.);
#28515=ORIENTED_EDGE('',*,*,#20116,.T.);
#28516=ORIENTED_EDGE('',*,*,#20117,.T.);
#28517=ORIENTED_EDGE('',*,*,#20118,.T.);
#28518=ORIENTED_EDGE('',*,*,#20115,.T.);
#28519=ORIENTED_EDGE('',*,*,#20119,.F.);
#28520=ORIENTED_EDGE('',*,*,#20120,.T.);
#28521=ORIENTED_EDGE('',*,*,#20119,.T.);
#28522=ORIENTED_EDGE('',*,*,#20121,.F.);
#28523=ORIENTED_EDGE('',*,*,#20122,.F.);
#28524=ORIENTED_EDGE('',*,*,#20123,.T.);
#28525=ORIENTED_EDGE('',*,*,#20124,.T.);
#28526=ORIENTED_EDGE('',*,*,#20117,.F.);
#28527=ORIENTED_EDGE('',*,*,#20125,.T.);
#28528=ORIENTED_EDGE('',*,*,#20122,.T.);
#28529=ORIENTED_EDGE('',*,*,#20126,.F.);
#28530=ORIENTED_EDGE('',*,*,#20110,.T.);
#28531=ORIENTED_EDGE('',*,*,#20127,.F.);
#28532=ORIENTED_EDGE('',*,*,#20128,.F.);
#28533=ORIENTED_EDGE('',*,*,#20129,.T.);
#28534=ORIENTED_EDGE('',*,*,#20126,.T.);
#28535=ORIENTED_EDGE('',*,*,#20130,.F.);
#28536=ORIENTED_EDGE('',*,*,#20124,.F.);
#28537=ORIENTED_EDGE('',*,*,#20131,.T.);
#28538=ORIENTED_EDGE('',*,*,#20128,.T.);
#28539=ORIENTED_EDGE('',*,*,#20132,.F.);
#28540=ORIENTED_EDGE('',*,*,#20133,.T.);
#28541=ORIENTED_EDGE('',*,*,#20134,.T.);
#28542=ORIENTED_EDGE('',*,*,#20135,.T.);
#28543=ORIENTED_EDGE('',*,*,#20136,.F.);
#28544=ORIENTED_EDGE('',*,*,#20021,.F.);
#28545=ORIENTED_EDGE('',*,*,#20137,.T.);
#28546=ORIENTED_EDGE('',*,*,#20138,.T.);
#28547=ORIENTED_EDGE('',*,*,#20139,.F.);
#28548=ORIENTED_EDGE('',*,*,#20135,.F.);
#28549=ORIENTED_EDGE('',*,*,#20140,.T.);
#28550=ORIENTED_EDGE('',*,*,#19946,.T.);
#28551=ORIENTED_EDGE('',*,*,#20141,.F.);
#28552=ORIENTED_EDGE('',*,*,#20142,.F.);
#28553=ORIENTED_EDGE('',*,*,#20143,.T.);
#28554=ORIENTED_EDGE('',*,*,#20144,.T.);
#28555=ORIENTED_EDGE('',*,*,#20145,.F.);
#28556=ORIENTED_EDGE('',*,*,#20138,.F.);
#28557=ORIENTED_EDGE('',*,*,#20146,.T.);
#28558=ORIENTED_EDGE('',*,*,#20112,.T.);
#28559=ORIENTED_EDGE('',*,*,#20147,.F.);
#28560=ORIENTED_EDGE('',*,*,#20148,.T.);
#28561=ORIENTED_EDGE('',*,*,#20149,.T.);
#28562=ORIENTED_EDGE('',*,*,#19939,.T.);
#28563=ORIENTED_EDGE('',*,*,#20150,.F.);
#28564=ORIENTED_EDGE('',*,*,#20151,.T.);
#28565=ORIENTED_EDGE('',*,*,#20023,.T.);
#28566=ORIENTED_EDGE('',*,*,#19940,.F.);
#28567=ORIENTED_EDGE('',*,*,#20152,.T.);
#28568=ORIENTED_EDGE('',*,*,#20153,.T.);
#28569=ORIENTED_EDGE('',*,*,#20148,.F.);
#28570=ORIENTED_EDGE('',*,*,#20154,.F.);
#28571=ORIENTED_EDGE('',*,*,#20155,.F.);
#28572=ORIENTED_EDGE('',*,*,#20156,.F.);
#28573=ORIENTED_EDGE('',*,*,#20157,.T.);
#28574=ORIENTED_EDGE('',*,*,#20158,.F.);
#28575=ORIENTED_EDGE('',*,*,#20159,.T.);
#28576=ORIENTED_EDGE('',*,*,#20160,.F.);
#28577=ORIENTED_EDGE('',*,*,#20161,.F.);
#28578=ORIENTED_EDGE('',*,*,#20147,.T.);
#28579=ORIENTED_EDGE('',*,*,#20162,.F.);
#28580=ORIENTED_EDGE('',*,*,#20163,.T.);
#28581=ORIENTED_EDGE('',*,*,#20164,.T.);
#28582=ORIENTED_EDGE('',*,*,#20165,.T.);
#28583=ORIENTED_EDGE('',*,*,#19958,.F.);
#28584=ORIENTED_EDGE('',*,*,#20166,.F.);
#28585=ORIENTED_EDGE('',*,*,#20167,.T.);
#28586=ORIENTED_EDGE('',*,*,#20168,.T.);
#28587=ORIENTED_EDGE('',*,*,#20169,.F.);
#28588=ORIENTED_EDGE('',*,*,#20170,.F.);
#28589=ORIENTED_EDGE('',*,*,#20171,.T.);
#28590=ORIENTED_EDGE('',*,*,#20172,.T.);
#28591=ORIENTED_EDGE('',*,*,#20173,.T.);
#28592=ORIENTED_EDGE('',*,*,#19952,.F.);
#28593=ORIENTED_EDGE('',*,*,#20174,.F.);
#28594=ORIENTED_EDGE('',*,*,#20175,.T.);
#28595=ORIENTED_EDGE('',*,*,#20176,.T.);
#28596=ORIENTED_EDGE('',*,*,#20177,.F.);
#28597=ORIENTED_EDGE('',*,*,#19802,.T.);
#28598=ORIENTED_EDGE('',*,*,#20178,.T.);
#28599=ORIENTED_EDGE('',*,*,#20179,.F.);
#28600=ORIENTED_EDGE('',*,*,#20180,.F.);
#28601=ORIENTED_EDGE('',*,*,#19836,.T.);
#28602=ORIENTED_EDGE('',*,*,#20180,.T.);
#28603=ORIENTED_EDGE('',*,*,#20181,.F.);
#28604=ORIENTED_EDGE('',*,*,#19838,.T.);
#28605=ORIENTED_EDGE('',*,*,#20181,.T.);
#28606=ORIENTED_EDGE('',*,*,#20182,.F.);
#28607=ORIENTED_EDGE('',*,*,#19989,.F.);
#28608=ORIENTED_EDGE('',*,*,#20183,.T.);
#28609=ORIENTED_EDGE('',*,*,#20170,.T.);
#28610=ORIENTED_EDGE('',*,*,#20184,.F.);
#28611=ORIENTED_EDGE('',*,*,#20165,.F.);
#28612=ORIENTED_EDGE('',*,*,#20184,.T.);
#28613=ORIENTED_EDGE('',*,*,#20185,.T.);
#28614=ORIENTED_EDGE('',*,*,#20182,.T.);
#28615=ORIENTED_EDGE('',*,*,#20179,.T.);
#28616=ORIENTED_EDGE('',*,*,#20186,.T.);
#28617=ORIENTED_EDGE('',*,*,#19959,.F.);
#28618=ORIENTED_EDGE('',*,*,#20187,.T.);
#28619=ORIENTED_EDGE('',*,*,#20188,.T.);
#28620=ORIENTED_EDGE('',*,*,#19954,.F.);
#28621=ORIENTED_EDGE('',*,*,#20189,.F.);
#28622=ORIENTED_EDGE('',*,*,#20162,.T.);
#28623=ORIENTED_EDGE('',*,*,#20190,.T.);
#28624=ORIENTED_EDGE('',*,*,#19955,.F.);
#28625=ORIENTED_EDGE('',*,*,#20188,.F.);
#28626=ORIENTED_EDGE('',*,*,#20191,.T.);
#28627=ORIENTED_EDGE('',*,*,#20192,.T.);
#28628=ORIENTED_EDGE('',*,*,#19956,.F.);
#28629=ORIENTED_EDGE('',*,*,#20190,.F.);
#28630=ORIENTED_EDGE('',*,*,#20174,.T.);
#28631=ORIENTED_EDGE('',*,*,#20166,.T.);
#28632=ORIENTED_EDGE('',*,*,#20193,.F.);
#28633=ORIENTED_EDGE('',*,*,#20193,.T.);
#28634=ORIENTED_EDGE('',*,*,#19957,.F.);
#28635=ORIENTED_EDGE('',*,*,#20192,.F.);
#28636=ORIENTED_EDGE('',*,*,#20194,.T.);
#28637=ORIENTED_EDGE('',*,*,#20195,.T.);
#28638=ORIENTED_EDGE('',*,*,#20189,.T.);
#28639=ORIENTED_EDGE('',*,*,#19953,.F.);
#28640=ORIENTED_EDGE('',*,*,#20196,.F.);
#28641=ORIENTED_EDGE('',*,*,#20197,.T.);
#28642=ORIENTED_EDGE('',*,*,#20198,.T.);
#28643=ORIENTED_EDGE('',*,*,#20168,.F.);
#28644=ORIENTED_EDGE('',*,*,#20199,.F.);
#28645=ORIENTED_EDGE('',*,*,#20199,.T.);
#28646=ORIENTED_EDGE('',*,*,#20197,.F.);
#28647=ORIENTED_EDGE('',*,*,#20200,.F.);
#28648=ORIENTED_EDGE('',*,*,#20201,.F.);
#28649=ORIENTED_EDGE('',*,*,#20202,.T.);
#28650=ORIENTED_EDGE('',*,*,#20203,.T.);
#28651=ORIENTED_EDGE('',*,*,#20204,.T.);
#28652=ORIENTED_EDGE('',*,*,#20205,.F.);
#28653=ORIENTED_EDGE('',*,*,#20198,.F.);
#28654=ORIENTED_EDGE('',*,*,#20203,.F.);
#28655=ORIENTED_EDGE('',*,*,#20202,.F.);
#28656=ORIENTED_EDGE('',*,*,#20157,.F.);
#28657=ORIENTED_EDGE('',*,*,#20206,.F.);
#28658=ORIENTED_EDGE('',*,*,#20207,.T.);
#28659=ORIENTED_EDGE('',*,*,#20208,.T.);
#28660=ORIENTED_EDGE('',*,*,#20209,.F.);
#28661=ORIENTED_EDGE('',*,*,#20204,.F.);
#28662=ORIENTED_EDGE('',*,*,#20206,.T.);
#28663=ORIENTED_EDGE('',*,*,#20210,.F.);
#28664=ORIENTED_EDGE('',*,*,#20211,.F.);
#28665=ORIENTED_EDGE('',*,*,#20212,.T.);
#28666=ORIENTED_EDGE('',*,*,#20213,.F.);
#28667=ORIENTED_EDGE('',*,*,#20214,.T.);
#28668=ORIENTED_EDGE('',*,*,#20207,.F.);
#28669=ORIENTED_EDGE('',*,*,#20215,.T.);
#28670=ORIENTED_EDGE('',*,*,#19997,.T.);
#28671=ORIENTED_EDGE('',*,*,#20216,.F.);
#28672=ORIENTED_EDGE('',*,*,#20217,.F.);
#28673=ORIENTED_EDGE('',*,*,#20218,.T.);
#28674=ORIENTED_EDGE('',*,*,#20000,.T.);
#28675=ORIENTED_EDGE('',*,*,#20215,.F.);
#28676=ORIENTED_EDGE('',*,*,#20219,.T.);
#28677=ORIENTED_EDGE('',*,*,#20004,.T.);
#28678=ORIENTED_EDGE('',*,*,#20218,.F.);
#28679=ORIENTED_EDGE('',*,*,#20220,.F.);
#28680=ORIENTED_EDGE('',*,*,#20211,.T.);
#28681=ORIENTED_EDGE('',*,*,#20221,.T.);
#28682=ORIENTED_EDGE('',*,*,#20222,.T.);
#28683=ORIENTED_EDGE('',*,*,#20223,.T.);
#28684=ORIENTED_EDGE('',*,*,#20224,.T.);
#28685=ORIENTED_EDGE('',*,*,#20225,.T.);
#28686=ORIENTED_EDGE('',*,*,#20006,.T.);
#28687=ORIENTED_EDGE('',*,*,#20219,.F.);
#28688=ORIENTED_EDGE('',*,*,#20226,.T.);
#28689=ORIENTED_EDGE('',*,*,#20227,.T.);
#28690=ORIENTED_EDGE('',*,*,#20010,.T.);
#28691=ORIENTED_EDGE('',*,*,#20225,.F.);
#28692=ORIENTED_EDGE('',*,*,#20216,.T.);
#28693=ORIENTED_EDGE('',*,*,#20013,.T.);
#28694=ORIENTED_EDGE('',*,*,#20228,.F.);
#28695=ORIENTED_EDGE('',*,*,#20229,.T.);
#28696=ORIENTED_EDGE('',*,*,#20230,.T.);
#28697=ORIENTED_EDGE('',*,*,#20015,.T.);
#28698=ORIENTED_EDGE('',*,*,#20227,.F.);
#28699=ORIENTED_EDGE('',*,*,#20231,.F.);
#28700=ORIENTED_EDGE('',*,*,#20228,.T.);
#28701=ORIENTED_EDGE('',*,*,#20018,.T.);
#28702=ORIENTED_EDGE('',*,*,#20230,.F.);
#28703=ORIENTED_EDGE('',*,*,#20232,.T.);
#28704=ORIENTED_EDGE('',*,*,#20213,.T.);
#28705=ORIENTED_EDGE('',*,*,#20212,.F.);
#28706=ORIENTED_EDGE('',*,*,#20220,.T.);
#28707=ORIENTED_EDGE('',*,*,#20217,.T.);
#28708=ORIENTED_EDGE('',*,*,#20231,.T.);
#28709=ORIENTED_EDGE('',*,*,#20210,.T.);
#28710=ORIENTED_EDGE('',*,*,#20156,.T.);
#28711=ORIENTED_EDGE('',*,*,#20233,.T.);
#28712=ORIENTED_EDGE('',*,*,#20221,.F.);
#28713=ORIENTED_EDGE('',*,*,#20020,.F.);
#28714=ORIENTED_EDGE('',*,*,#20234,.F.);
#28715=ORIENTED_EDGE('',*,*,#20235,.T.);
#28716=ORIENTED_EDGE('',*,*,#20236,.F.);
#28717=ORIENTED_EDGE('',*,*,#20026,.T.);
#28718=ORIENTED_EDGE('',*,*,#20237,.T.);
#28719=ORIENTED_EDGE('',*,*,#20161,.T.);
#28720=ORIENTED_EDGE('',*,*,#20238,.F.);
#28721=ORIENTED_EDGE('',*,*,#20238,.T.);
#28722=ORIENTED_EDGE('',*,*,#20239,.F.);
#28723=ORIENTED_EDGE('',*,*,#20240,.F.);
#28724=ORIENTED_EDGE('',*,*,#20029,.T.);
#28725=ORIENTED_EDGE('',*,*,#20032,.T.);
#28726=ORIENTED_EDGE('',*,*,#20240,.T.);
#28727=ORIENTED_EDGE('',*,*,#20241,.T.);
#28728=ORIENTED_EDGE('',*,*,#20242,.T.);
#28729=ORIENTED_EDGE('',*,*,#20242,.F.);
#28730=ORIENTED_EDGE('',*,*,#20243,.T.);
#28731=ORIENTED_EDGE('',*,*,#20244,.T.);
#28732=ORIENTED_EDGE('',*,*,#20035,.T.);
#28733=ORIENTED_EDGE('',*,*,#20244,.F.);
#28734=ORIENTED_EDGE('',*,*,#20245,.T.);
#28735=ORIENTED_EDGE('',*,*,#20246,.F.);
#28736=ORIENTED_EDGE('',*,*,#20038,.T.);
#28737=ORIENTED_EDGE('',*,*,#20247,.T.);
#28738=ORIENTED_EDGE('',*,*,#20146,.F.);
#28739=ORIENTED_EDGE('',*,*,#20237,.F.);
#28740=ORIENTED_EDGE('',*,*,#20042,.T.);
#28741=ORIENTED_EDGE('',*,*,#20246,.T.);
#28742=ORIENTED_EDGE('',*,*,#19932,.F.);
#28743=ORIENTED_EDGE('',*,*,#20248,.F.);
#28744=ORIENTED_EDGE('',*,*,#20044,.T.);
#28745=ORIENTED_EDGE('',*,*,#20047,.T.);
#28746=ORIENTED_EDGE('',*,*,#20248,.T.);
#28747=ORIENTED_EDGE('',*,*,#20113,.T.);
#28748=ORIENTED_EDGE('',*,*,#20247,.F.);
#28749=ORIENTED_EDGE('',*,*,#20249,.T.);
#28750=ORIENTED_EDGE('',*,*,#20116,.F.);
#28751=ORIENTED_EDGE('',*,*,#20250,.F.);
#28752=ORIENTED_EDGE('',*,*,#20048,.F.);
#28753=ORIENTED_EDGE('',*,*,#20250,.T.);
#28754=ORIENTED_EDGE('',*,*,#20118,.F.);
#28755=ORIENTED_EDGE('',*,*,#20251,.F.);
#28756=ORIENTED_EDGE('',*,*,#20056,.F.);
#28757=ORIENTED_EDGE('',*,*,#20064,.F.);
#28758=ORIENTED_EDGE('',*,*,#20251,.T.);
#28759=ORIENTED_EDGE('',*,*,#20120,.F.);
#28760=ORIENTED_EDGE('',*,*,#20252,.F.);
#28761=ORIENTED_EDGE('',*,*,#20253,.T.);
#28762=ORIENTED_EDGE('',*,*,#20123,.F.);
#28763=ORIENTED_EDGE('',*,*,#20249,.F.);
#28764=ORIENTED_EDGE('',*,*,#20067,.F.);
#28765=ORIENTED_EDGE('',*,*,#20252,.T.);
#28766=ORIENTED_EDGE('',*,*,#20125,.F.);
#28767=ORIENTED_EDGE('',*,*,#20254,.F.);
#28768=ORIENTED_EDGE('',*,*,#20070,.F.);
#28769=ORIENTED_EDGE('',*,*,#20254,.T.);
#28770=ORIENTED_EDGE('',*,*,#20129,.F.);
#28771=ORIENTED_EDGE('',*,*,#20253,.F.);
#28772=ORIENTED_EDGE('',*,*,#20073,.F.);
#28773=ORIENTED_EDGE('',*,*,#20084,.T.);
#28774=ORIENTED_EDGE('',*,*,#20255,.T.);
#28775=ORIENTED_EDGE('',*,*,#20132,.T.);
#28776=ORIENTED_EDGE('',*,*,#20256,.T.);
#28777=ORIENTED_EDGE('',*,*,#20256,.F.);
#28778=ORIENTED_EDGE('',*,*,#20127,.T.);
#28779=ORIENTED_EDGE('',*,*,#20257,.T.);
#28780=ORIENTED_EDGE('',*,*,#20088,.T.);
#28781=ORIENTED_EDGE('',*,*,#20257,.F.);
#28782=ORIENTED_EDGE('',*,*,#20109,.T.);
#28783=ORIENTED_EDGE('',*,*,#20258,.T.);
#28784=ORIENTED_EDGE('',*,*,#20091,.T.);
#28785=ORIENTED_EDGE('',*,*,#20258,.F.);
#28786=ORIENTED_EDGE('',*,*,#20259,.T.);
#28787=ORIENTED_EDGE('',*,*,#20260,.T.);
#28788=ORIENTED_EDGE('',*,*,#20094,.T.);
#28789=ORIENTED_EDGE('',*,*,#20260,.F.);
#28790=ORIENTED_EDGE('',*,*,#20261,.T.);
#28791=ORIENTED_EDGE('',*,*,#20262,.T.);
#28792=ORIENTED_EDGE('',*,*,#20097,.T.);
#28793=ORIENTED_EDGE('',*,*,#20263,.T.);
#28794=ORIENTED_EDGE('',*,*,#20264,.F.);
#28795=ORIENTED_EDGE('',*,*,#20255,.F.);
#28796=ORIENTED_EDGE('',*,*,#20101,.T.);
#28797=ORIENTED_EDGE('',*,*,#20262,.F.);
#28798=ORIENTED_EDGE('',*,*,#20265,.T.);
#28799=ORIENTED_EDGE('',*,*,#20266,.T.);
#28800=ORIENTED_EDGE('',*,*,#20103,.T.);
#28801=ORIENTED_EDGE('',*,*,#20106,.T.);
#28802=ORIENTED_EDGE('',*,*,#20266,.F.);
#28803=ORIENTED_EDGE('',*,*,#20267,.T.);
#28804=ORIENTED_EDGE('',*,*,#20263,.F.);
#28805=ORIENTED_EDGE('',*,*,#20268,.T.);
#28806=ORIENTED_EDGE('',*,*,#20259,.F.);
#28807=ORIENTED_EDGE('',*,*,#20108,.F.);
#28808=ORIENTED_EDGE('',*,*,#20261,.F.);
#28809=ORIENTED_EDGE('',*,*,#20268,.F.);
#28810=ORIENTED_EDGE('',*,*,#20269,.T.);
#28811=ORIENTED_EDGE('',*,*,#20270,.T.);
#28812=ORIENTED_EDGE('',*,*,#20264,.T.);
#28813=ORIENTED_EDGE('',*,*,#20271,.T.);
#28814=ORIENTED_EDGE('',*,*,#20133,.F.);
#28815=ORIENTED_EDGE('',*,*,#20272,.T.);
#28816=ORIENTED_EDGE('',*,*,#20265,.F.);
#28817=ORIENTED_EDGE('',*,*,#20270,.F.);
#28818=ORIENTED_EDGE('',*,*,#20267,.F.);
#28819=ORIENTED_EDGE('',*,*,#20272,.F.);
#28820=ORIENTED_EDGE('',*,*,#20273,.T.);
#28821=ORIENTED_EDGE('',*,*,#20271,.F.);
#28822=ORIENTED_EDGE('',*,*,#20274,.F.);
#28823=ORIENTED_EDGE('',*,*,#20159,.F.);
#28824=ORIENTED_EDGE('',*,*,#20111,.F.);
#28825=ORIENTED_EDGE('',*,*,#20275,.F.);
#28826=ORIENTED_EDGE('',*,*,#20196,.T.);
#28827=ORIENTED_EDGE('',*,*,#20173,.F.);
#28828=ORIENTED_EDGE('',*,*,#20176,.F.);
#28829=ORIENTED_EDGE('',*,*,#20276,.T.);
#28830=ORIENTED_EDGE('',*,*,#20277,.T.);
#28831=ORIENTED_EDGE('',*,*,#20278,.F.);
#28832=ORIENTED_EDGE('',*,*,#20121,.T.);
#28833=ORIENTED_EDGE('',*,*,#20114,.T.);
#28834=ORIENTED_EDGE('',*,*,#20130,.T.);
#28835=ORIENTED_EDGE('',*,*,#20269,.F.);
#28836=ORIENTED_EDGE('',*,*,#20107,.F.);
#28837=ORIENTED_EDGE('',*,*,#20131,.F.);
#28838=ORIENTED_EDGE('',*,*,#20273,.F.);
#28839=ORIENTED_EDGE('',*,*,#20236,.T.);
#28840=ORIENTED_EDGE('',*,*,#20276,.F.);
#28841=ORIENTED_EDGE('',*,*,#20279,.F.);
#28842=ORIENTED_EDGE('',*,*,#20134,.F.);
#28843=ORIENTED_EDGE('',*,*,#20280,.F.);
#28844=ORIENTED_EDGE('',*,*,#20195,.F.);
#28845=ORIENTED_EDGE('',*,*,#20175,.F.);
#28846=ORIENTED_EDGE('',*,*,#20194,.F.);
#28847=ORIENTED_EDGE('',*,*,#20239,.T.);
#28848=ORIENTED_EDGE('',*,*,#20160,.T.);
#28849=ORIENTED_EDGE('',*,*,#20281,.F.);
#28850=ORIENTED_EDGE('',*,*,#20245,.F.);
#28851=ORIENTED_EDGE('',*,*,#20282,.F.);
#28852=ORIENTED_EDGE('',*,*,#20275,.T.);
#28853=ORIENTED_EDGE('',*,*,#19933,.F.);
#28854=ORIENTED_EDGE('',*,*,#20151,.F.);
#28855=ORIENTED_EDGE('',*,*,#20149,.F.);
#28856=ORIENTED_EDGE('',*,*,#20283,.F.);
#28857=ORIENTED_EDGE('',*,*,#20234,.T.);
#28858=ORIENTED_EDGE('',*,*,#20284,.T.);
#28859=ORIENTED_EDGE('',*,*,#20283,.T.);
#28860=ORIENTED_EDGE('',*,*,#20153,.F.);
#28861=ORIENTED_EDGE('',*,*,#20241,.F.);
#28862=ORIENTED_EDGE('',*,*,#20281,.T.);
#28863=ORIENTED_EDGE('',*,*,#20274,.T.);
#28864=ORIENTED_EDGE('',*,*,#20285,.T.);
#28865=ORIENTED_EDGE('',*,*,#20235,.F.);
#28866=ORIENTED_EDGE('',*,*,#20284,.F.);
#28867=ORIENTED_EDGE('',*,*,#20286,.T.);
#28868=ORIENTED_EDGE('',*,*,#20277,.F.);
#28869=ORIENTED_EDGE('',*,*,#20282,.T.);
#28870=ORIENTED_EDGE('',*,*,#20243,.F.);
#28871=ORIENTED_EDGE('',*,*,#20285,.F.);
#28872=ORIENTED_EDGE('',*,*,#20187,.F.);
#28873=ORIENTED_EDGE('',*,*,#20280,.T.);
#28874=ORIENTED_EDGE('',*,*,#20191,.F.);
#28875=ORIENTED_EDGE('',*,*,#20163,.F.);
#28876=ORIENTED_EDGE('',*,*,#20158,.T.);
#28877=ORIENTED_EDGE('',*,*,#20201,.T.);
#28878=ORIENTED_EDGE('',*,*,#20287,.F.);
#28879=ORIENTED_EDGE('',*,*,#20288,.F.);
#28880=ORIENTED_EDGE('',*,*,#20289,.T.);
#28881=ORIENTED_EDGE('',*,*,#20290,.T.);
#28882=ORIENTED_EDGE('',*,*,#20291,.F.);
#28883=ORIENTED_EDGE('',*,*,#20292,.T.);
#28884=ORIENTED_EDGE('',*,*,#20289,.F.);
#28885=ORIENTED_EDGE('',*,*,#20293,.F.);
#28886=ORIENTED_EDGE('',*,*,#20143,.F.);
#28887=ORIENTED_EDGE('',*,*,#20137,.F.);
#28888=ORIENTED_EDGE('',*,*,#20279,.T.);
#28889=ORIENTED_EDGE('',*,*,#20294,.T.);
#28890=ORIENTED_EDGE('',*,*,#20292,.F.);
#28891=ORIENTED_EDGE('',*,*,#20294,.F.);
#28892=ORIENTED_EDGE('',*,*,#20278,.T.);
#28893=ORIENTED_EDGE('',*,*,#20295,.T.);
#28894=ORIENTED_EDGE('',*,*,#20290,.F.);
#28895=ORIENTED_EDGE('',*,*,#20296,.T.);
#28896=ORIENTED_EDGE('',*,*,#19846,.T.);
#28897=ORIENTED_EDGE('',*,*,#20297,.F.);
#28898=ORIENTED_EDGE('',*,*,#20298,.F.);
#28899=ORIENTED_EDGE('',*,*,#20299,.T.);
#28900=ORIENTED_EDGE('',*,*,#19847,.T.);
#28901=ORIENTED_EDGE('',*,*,#20296,.F.);
#28902=ORIENTED_EDGE('',*,*,#20300,.F.);
#28903=ORIENTED_EDGE('',*,*,#20301,.T.);
#28904=ORIENTED_EDGE('',*,*,#19852,.T.);
#28905=ORIENTED_EDGE('',*,*,#20299,.F.);
#28906=ORIENTED_EDGE('',*,*,#20302,.F.);
#28907=ORIENTED_EDGE('',*,*,#20303,.T.);
#28908=ORIENTED_EDGE('',*,*,#19853,.T.);
#28909=ORIENTED_EDGE('',*,*,#20301,.F.);
#28910=ORIENTED_EDGE('',*,*,#20304,.F.);
#28911=ORIENTED_EDGE('',*,*,#20305,.T.);
#28912=ORIENTED_EDGE('',*,*,#19856,.T.);
#28913=ORIENTED_EDGE('',*,*,#20303,.F.);
#28914=ORIENTED_EDGE('',*,*,#20306,.F.);
#28915=ORIENTED_EDGE('',*,*,#20297,.T.);
#28916=ORIENTED_EDGE('',*,*,#20307,.F.);
#28917=ORIENTED_EDGE('',*,*,#20308,.F.);
#28918=ORIENTED_EDGE('',*,*,#20309,.T.);
#28919=ORIENTED_EDGE('',*,*,#20309,.F.);
#28920=ORIENTED_EDGE('',*,*,#20310,.T.);
#28921=ORIENTED_EDGE('',*,*,#20311,.F.);
#28922=ORIENTED_EDGE('',*,*,#20312,.F.);
#28923=ORIENTED_EDGE('',*,*,#20308,.T.);
#28924=ORIENTED_EDGE('',*,*,#19861,.T.);
#28925=ORIENTED_EDGE('',*,*,#20305,.F.);
#28926=ORIENTED_EDGE('',*,*,#20313,.F.);
#28927=ORIENTED_EDGE('',*,*,#20314,.T.);
#28928=ORIENTED_EDGE('',*,*,#20313,.T.);
#28929=ORIENTED_EDGE('',*,*,#20315,.F.);
#28930=ORIENTED_EDGE('',*,*,#20316,.F.);
#28931=ORIENTED_EDGE('',*,*,#20307,.T.);
#28932=ORIENTED_EDGE('',*,*,#19845,.T.);
#28933=ORIENTED_EDGE('',*,*,#19942,.F.);
#28934=ORIENTED_EDGE('',*,*,#20317,.F.);
#28935=ORIENTED_EDGE('',*,*,#19947,.F.);
#28936=ORIENTED_EDGE('',*,*,#20318,.F.);
#28937=ORIENTED_EDGE('',*,*,#20310,.F.);
#28938=ORIENTED_EDGE('',*,*,#20317,.T.);
#28939=ORIENTED_EDGE('',*,*,#20319,.F.);
#28940=ORIENTED_EDGE('',*,*,#19878,.T.);
#28941=ORIENTED_EDGE('',*,*,#19859,.T.);
#28942=ORIENTED_EDGE('',*,*,#20314,.F.);
#28943=ORIENTED_EDGE('',*,*,#20320,.F.);
#28944=ORIENTED_EDGE('',*,*,#20321,.T.);
#28945=ORIENTED_EDGE('',*,*,#20318,.T.);
#28946=ORIENTED_EDGE('',*,*,#20140,.F.);
#28947=ORIENTED_EDGE('',*,*,#20311,.T.);
#28948=ORIENTED_EDGE('',*,*,#20321,.F.);
#28949=ORIENTED_EDGE('',*,*,#20322,.F.);
#28950=ORIENTED_EDGE('',*,*,#20323,.F.);
#28951=ORIENTED_EDGE('',*,*,#20291,.T.);
#28952=ORIENTED_EDGE('',*,*,#20324,.T.);
#28953=ORIENTED_EDGE('',*,*,#20322,.T.);
#28954=ORIENTED_EDGE('',*,*,#20293,.T.);
#28955=ORIENTED_EDGE('',*,*,#20323,.T.);
#28956=ORIENTED_EDGE('',*,*,#20320,.T.);
#28957=ORIENTED_EDGE('',*,*,#20325,.F.);
#28958=ORIENTED_EDGE('',*,*,#20325,.T.);
#28959=ORIENTED_EDGE('',*,*,#20142,.T.);
#28960=ORIENTED_EDGE('',*,*,#20326,.F.);
#28961=ORIENTED_EDGE('',*,*,#20144,.F.);
#28962=ORIENTED_EDGE('',*,*,#20327,.T.);
#28963=ORIENTED_EDGE('',*,*,#19768,.T.);
#28964=ORIENTED_EDGE('',*,*,#20328,.F.);
#28965=ORIENTED_EDGE('',*,*,#20328,.T.);
#28966=ORIENTED_EDGE('',*,*,#19999,.T.);
#28967=ORIENTED_EDGE('',*,*,#20329,.T.);
#28968=ORIENTED_EDGE('',*,*,#20330,.F.);
#28969=ORIENTED_EDGE('',*,*,#20002,.T.);
#28970=ORIENTED_EDGE('',*,*,#20331,.T.);
#28971=ORIENTED_EDGE('',*,*,#20332,.F.);
#28972=ORIENTED_EDGE('',*,*,#20329,.F.);
#28973=ORIENTED_EDGE('',*,*,#20003,.T.);
#28974=ORIENTED_EDGE('',*,*,#20333,.T.);
#28975=ORIENTED_EDGE('',*,*,#20334,.F.);
#28976=ORIENTED_EDGE('',*,*,#20331,.F.);
#28977=ORIENTED_EDGE('',*,*,#20008,.T.);
#28978=ORIENTED_EDGE('',*,*,#20335,.T.);
#28979=ORIENTED_EDGE('',*,*,#20336,.F.);
#28980=ORIENTED_EDGE('',*,*,#20333,.F.);
#28981=ORIENTED_EDGE('',*,*,#20009,.T.);
#28982=ORIENTED_EDGE('',*,*,#20337,.T.);
#28983=ORIENTED_EDGE('',*,*,#20338,.F.);
#28984=ORIENTED_EDGE('',*,*,#20335,.F.);
#28985=ORIENTED_EDGE('',*,*,#20339,.F.);
#28986=ORIENTED_EDGE('',*,*,#20340,.F.);
#28987=ORIENTED_EDGE('',*,*,#20014,.T.);
#28988=ORIENTED_EDGE('',*,*,#19995,.T.);
#28989=ORIENTED_EDGE('',*,*,#20340,.T.);
#28990=ORIENTED_EDGE('',*,*,#20341,.F.);
#28991=ORIENTED_EDGE('',*,*,#20342,.F.);
#28992=ORIENTED_EDGE('',*,*,#20017,.T.);
#28993=ORIENTED_EDGE('',*,*,#20343,.T.);
#28994=ORIENTED_EDGE('',*,*,#20344,.F.);
#28995=ORIENTED_EDGE('',*,*,#20337,.F.);
#28996=ORIENTED_EDGE('',*,*,#20019,.T.);
#28997=ORIENTED_EDGE('',*,*,#20342,.T.);
#28998=ORIENTED_EDGE('',*,*,#20345,.F.);
#28999=ORIENTED_EDGE('',*,*,#20343,.F.);
#29000=ORIENTED_EDGE('',*,*,#20346,.T.);
#29001=ORIENTED_EDGE('',*,*,#19769,.T.);
#29002=ORIENTED_EDGE('',*,*,#20327,.F.);
#29003=ORIENTED_EDGE('',*,*,#20347,.F.);
#29004=ORIENTED_EDGE('',*,*,#20348,.T.);
#29005=ORIENTED_EDGE('',*,*,#19775,.T.);
#29006=ORIENTED_EDGE('',*,*,#20346,.F.);
#29007=ORIENTED_EDGE('',*,*,#20349,.F.);
#29008=ORIENTED_EDGE('',*,*,#20350,.T.);
#29009=ORIENTED_EDGE('',*,*,#20351,.T.);
#29010=ORIENTED_EDGE('',*,*,#19960,.F.);
#29011=ORIENTED_EDGE('',*,*,#20352,.F.);
#29012=ORIENTED_EDGE('',*,*,#20353,.T.);
#29013=ORIENTED_EDGE('',*,*,#20352,.T.);
#29014=ORIENTED_EDGE('',*,*,#20186,.F.);
#29015=ORIENTED_EDGE('',*,*,#20178,.F.);
#29016=ORIENTED_EDGE('',*,*,#19805,.F.);
#29017=ORIENTED_EDGE('',*,*,#20354,.T.);
#29018=ORIENTED_EDGE('',*,*,#20355,.T.);
#29019=ORIENTED_EDGE('',*,*,#20350,.F.);
#29020=ORIENTED_EDGE('',*,*,#20353,.F.);
#29021=ORIENTED_EDGE('',*,*,#20356,.T.);
#29022=ORIENTED_EDGE('',*,*,#19862,.F.);
#29023=ORIENTED_EDGE('',*,*,#19962,.F.);
#29024=ORIENTED_EDGE('',*,*,#20357,.F.);
#29025=ORIENTED_EDGE('',*,*,#20358,.F.);
#29026=ORIENTED_EDGE('',*,*,#19943,.T.);
#29027=ORIENTED_EDGE('',*,*,#19843,.T.);
#29028=ORIENTED_EDGE('',*,*,#20356,.F.);
#29029=ORIENTED_EDGE('',*,*,#20359,.T.);
#29030=ORIENTED_EDGE('',*,*,#19993,.T.);
#29031=ORIENTED_EDGE('',*,*,#20360,.F.);
#29032=ORIENTED_EDGE('',*,*,#20361,.F.);
#29033=ORIENTED_EDGE('',*,*,#20362,.F.);
#29034=ORIENTED_EDGE('',*,*,#20339,.T.);
#29035=ORIENTED_EDGE('',*,*,#19994,.T.);
#29036=ORIENTED_EDGE('',*,*,#20359,.F.);
#29037=ORIENTED_EDGE('',*,*,#20363,.T.);
#29038=ORIENTED_EDGE('',*,*,#20357,.T.);
#29039=ORIENTED_EDGE('',*,*,#19961,.F.);
#29040=ORIENTED_EDGE('',*,*,#20351,.F.);
#29041=ORIENTED_EDGE('',*,*,#20364,.T.);
#29042=ORIENTED_EDGE('',*,*,#19783,.F.);
#29043=ORIENTED_EDGE('',*,*,#20365,.F.);
#29044=ORIENTED_EDGE('',*,*,#20366,.T.);
#29045=ORIENTED_EDGE('',*,*,#20367,.T.);
#29046=ORIENTED_EDGE('',*,*,#20368,.T.);
#29047=ORIENTED_EDGE('',*,*,#20369,.F.);
#29048=ORIENTED_EDGE('',*,*,#19799,.F.);
#29049=ORIENTED_EDGE('',*,*,#20369,.T.);
#29050=ORIENTED_EDGE('',*,*,#20370,.T.);
#29051=ORIENTED_EDGE('',*,*,#20354,.F.);
#29052=ORIENTED_EDGE('',*,*,#19804,.F.);
#29053=ORIENTED_EDGE('',*,*,#20370,.F.);
#29054=ORIENTED_EDGE('',*,*,#20368,.F.);
#29055=ORIENTED_EDGE('',*,*,#20371,.T.);
#29056=ORIENTED_EDGE('',*,*,#20372,.T.);
#29057=ORIENTED_EDGE('',*,*,#20373,.F.);
#29058=ORIENTED_EDGE('',*,*,#20374,.T.);
#29059=ORIENTED_EDGE('',*,*,#20375,.T.);
#29060=ORIENTED_EDGE('',*,*,#20376,.F.);
#29061=ORIENTED_EDGE('',*,*,#20372,.F.);
#29062=ORIENTED_EDGE('',*,*,#20377,.T.);
#29063=ORIENTED_EDGE('',*,*,#20378,.T.);
#29064=ORIENTED_EDGE('',*,*,#20379,.F.);
#29065=ORIENTED_EDGE('',*,*,#20375,.F.);
#29066=ORIENTED_EDGE('',*,*,#20380,.T.);
#29067=ORIENTED_EDGE('',*,*,#20381,.T.);
#29068=ORIENTED_EDGE('',*,*,#20382,.F.);
#29069=ORIENTED_EDGE('',*,*,#20378,.F.);
#29070=ORIENTED_EDGE('',*,*,#20383,.T.);
#29071=ORIENTED_EDGE('',*,*,#20384,.T.);
#29072=ORIENTED_EDGE('',*,*,#20385,.F.);
#29073=ORIENTED_EDGE('',*,*,#20381,.F.);
#29074=ORIENTED_EDGE('',*,*,#20386,.T.);
#29075=ORIENTED_EDGE('',*,*,#20387,.T.);
#29076=ORIENTED_EDGE('',*,*,#20388,.F.);
#29077=ORIENTED_EDGE('',*,*,#20384,.F.);
#29078=ORIENTED_EDGE('',*,*,#20389,.T.);
#29079=ORIENTED_EDGE('',*,*,#19776,.T.);
#29080=ORIENTED_EDGE('',*,*,#20348,.F.);
#29081=ORIENTED_EDGE('',*,*,#20390,.F.);
#29082=ORIENTED_EDGE('',*,*,#19777,.T.);
#29083=ORIENTED_EDGE('',*,*,#20389,.F.);
#29084=ORIENTED_EDGE('',*,*,#20391,.F.);
#29085=ORIENTED_EDGE('',*,*,#20391,.T.);
#29086=ORIENTED_EDGE('',*,*,#20390,.T.);
#29087=ORIENTED_EDGE('',*,*,#20392,.F.);
#29088=ORIENTED_EDGE('',*,*,#20387,.F.);
#29089=ORIENTED_EDGE('',*,*,#20393,.T.);
#29090=ORIENTED_EDGE('',*,*,#19782,.F.);
#29091=ORIENTED_EDGE('',*,*,#19821,.T.);
#29092=ORIENTED_EDGE('',*,*,#20394,.T.);
#29093=ORIENTED_EDGE('',*,*,#20395,.T.);
#29094=ORIENTED_EDGE('',*,*,#20396,.T.);
#29095=ORIENTED_EDGE('',*,*,#20365,.T.);
#29096=ORIENTED_EDGE('',*,*,#20396,.F.);
#29097=ORIENTED_EDGE('',*,*,#20397,.T.);
#29098=ORIENTED_EDGE('',*,*,#20398,.T.);
#29099=ORIENTED_EDGE('',*,*,#20366,.F.);
#29100=ORIENTED_EDGE('',*,*,#20398,.F.);
#29101=ORIENTED_EDGE('',*,*,#20399,.T.);
#29102=ORIENTED_EDGE('',*,*,#19786,.F.);
#29103=ORIENTED_EDGE('',*,*,#19826,.T.);
#29104=ORIENTED_EDGE('',*,*,#19780,.T.);
#29105=ORIENTED_EDGE('',*,*,#20364,.F.);
#29106=ORIENTED_EDGE('',*,*,#20400,.T.);
#29107=ORIENTED_EDGE('',*,*,#20401,.T.);
#29108=ORIENTED_EDGE('',*,*,#20367,.F.);
#29109=ORIENTED_EDGE('',*,*,#19798,.F.);
#29110=ORIENTED_EDGE('',*,*,#20402,.T.);
#29111=ORIENTED_EDGE('',*,*,#20403,.F.);
#29112=ORIENTED_EDGE('',*,*,#20371,.F.);
#29113=ORIENTED_EDGE('',*,*,#20401,.F.);
#29114=ORIENTED_EDGE('',*,*,#20403,.T.);
#29115=ORIENTED_EDGE('',*,*,#20404,.F.);
#29116=ORIENTED_EDGE('',*,*,#20405,.F.);
#29117=ORIENTED_EDGE('',*,*,#20374,.F.);
#29118=ORIENTED_EDGE('',*,*,#20377,.F.);
#29119=ORIENTED_EDGE('',*,*,#20405,.T.);
#29120=ORIENTED_EDGE('',*,*,#20406,.T.);
#29121=ORIENTED_EDGE('',*,*,#20407,.F.);
#29122=ORIENTED_EDGE('',*,*,#20407,.T.);
#29123=ORIENTED_EDGE('',*,*,#20408,.F.);
#29124=ORIENTED_EDGE('',*,*,#20409,.F.);
#29125=ORIENTED_EDGE('',*,*,#20380,.F.);
#29126=ORIENTED_EDGE('',*,*,#20383,.F.);
#29127=ORIENTED_EDGE('',*,*,#20409,.T.);
#29128=ORIENTED_EDGE('',*,*,#20410,.T.);
#29129=ORIENTED_EDGE('',*,*,#20411,.F.);
#29130=ORIENTED_EDGE('',*,*,#20411,.T.);
#29131=ORIENTED_EDGE('',*,*,#20412,.F.);
#29132=ORIENTED_EDGE('',*,*,#20413,.F.);
#29133=ORIENTED_EDGE('',*,*,#20386,.F.);
#29134=ORIENTED_EDGE('',*,*,#20414,.T.);
#29135=ORIENTED_EDGE('',*,*,#20415,.F.);
#29136=ORIENTED_EDGE('',*,*,#19815,.T.);
#29137=ORIENTED_EDGE('',*,*,#19778,.F.);
#29138=ORIENTED_EDGE('',*,*,#20393,.F.);
#29139=ORIENTED_EDGE('',*,*,#20413,.T.);
#29140=ORIENTED_EDGE('',*,*,#20394,.F.);
#29141=ORIENTED_EDGE('',*,*,#19818,.T.);
#29142=ORIENTED_EDGE('',*,*,#20415,.T.);
#29143=ORIENTED_EDGE('',*,*,#20416,.T.);
#29144=ORIENTED_EDGE('',*,*,#20417,.T.);
#29145=ORIENTED_EDGE('',*,*,#20416,.F.);
#29146=ORIENTED_EDGE('',*,*,#20418,.F.);
#29147=ORIENTED_EDGE('',*,*,#20419,.T.);
#29148=ORIENTED_EDGE('',*,*,#20420,.F.);
#29149=ORIENTED_EDGE('',*,*,#20395,.F.);
#29150=ORIENTED_EDGE('',*,*,#20417,.F.);
#29151=ORIENTED_EDGE('',*,*,#20420,.T.);
#29152=ORIENTED_EDGE('',*,*,#20421,.T.);
#29153=ORIENTED_EDGE('',*,*,#20422,.F.);
#29154=ORIENTED_EDGE('',*,*,#20397,.F.);
#29155=ORIENTED_EDGE('',*,*,#20423,.T.);
#29156=ORIENTED_EDGE('',*,*,#20424,.F.);
#29157=ORIENTED_EDGE('',*,*,#19787,.F.);
#29158=ORIENTED_EDGE('',*,*,#20399,.F.);
#29159=ORIENTED_EDGE('',*,*,#20422,.T.);
#29160=ORIENTED_EDGE('',*,*,#20425,.T.);
#29161=ORIENTED_EDGE('',*,*,#20423,.F.);
#29162=ORIENTED_EDGE('',*,*,#20426,.T.);
#29163=ORIENTED_EDGE('',*,*,#20427,.T.);
#29164=ORIENTED_EDGE('',*,*,#20400,.F.);
#29165=ORIENTED_EDGE('',*,*,#20428,.T.);
#29166=ORIENTED_EDGE('',*,*,#20429,.F.);
#29167=ORIENTED_EDGE('',*,*,#20402,.F.);
#29168=ORIENTED_EDGE('',*,*,#20427,.F.);
#29169=ORIENTED_EDGE('',*,*,#20404,.T.);
#29170=ORIENTED_EDGE('',*,*,#20429,.T.);
#29171=ORIENTED_EDGE('',*,*,#20430,.F.);
#29172=ORIENTED_EDGE('',*,*,#20406,.F.);
#29173=ORIENTED_EDGE('',*,*,#20430,.T.);
#29174=ORIENTED_EDGE('',*,*,#20431,.T.);
#29175=ORIENTED_EDGE('',*,*,#20432,.F.);
#29176=ORIENTED_EDGE('',*,*,#20408,.T.);
#29177=ORIENTED_EDGE('',*,*,#20432,.T.);
#29178=ORIENTED_EDGE('',*,*,#20433,.F.);
#29179=ORIENTED_EDGE('',*,*,#20434,.T.);
#29180=ORIENTED_EDGE('',*,*,#20435,.F.);
#29181=ORIENTED_EDGE('',*,*,#20410,.F.);
#29182=ORIENTED_EDGE('',*,*,#20433,.T.);
#29183=ORIENTED_EDGE('',*,*,#20412,.T.);
#29184=ORIENTED_EDGE('',*,*,#20435,.T.);
#29185=ORIENTED_EDGE('',*,*,#20436,.F.);
#29186=ORIENTED_EDGE('',*,*,#20437,.T.);
#29187=ORIENTED_EDGE('',*,*,#20418,.T.);
#29188=ORIENTED_EDGE('',*,*,#20414,.F.);
#29189=ORIENTED_EDGE('',*,*,#20436,.T.);
#29190=ORIENTED_EDGE('',*,*,#20424,.T.);
#29191=ORIENTED_EDGE('',*,*,#20438,.T.);
#29192=ORIENTED_EDGE('',*,*,#20439,.F.);
#29193=ORIENTED_EDGE('',*,*,#19790,.F.);
#29194=ORIENTED_EDGE('',*,*,#20439,.T.);
#29195=ORIENTED_EDGE('',*,*,#20440,.T.);
#29196=ORIENTED_EDGE('',*,*,#20441,.F.);
#29197=ORIENTED_EDGE('',*,*,#19791,.F.);
#29198=ORIENTED_EDGE('',*,*,#20441,.T.);
#29199=ORIENTED_EDGE('',*,*,#20442,.T.);
#29200=ORIENTED_EDGE('',*,*,#20443,.F.);
#29201=ORIENTED_EDGE('',*,*,#19796,.F.);
#29202=ORIENTED_EDGE('',*,*,#20443,.T.);
#29203=ORIENTED_EDGE('',*,*,#20444,.T.);
#29204=ORIENTED_EDGE('',*,*,#20426,.F.);
#29205=ORIENTED_EDGE('',*,*,#19797,.F.);
#29206=ORIENTED_EDGE('',*,*,#20425,.F.);
#29207=ORIENTED_EDGE('',*,*,#20421,.F.);
#29208=ORIENTED_EDGE('',*,*,#20419,.F.);
#29209=ORIENTED_EDGE('',*,*,#20437,.F.);
#29210=ORIENTED_EDGE('',*,*,#20434,.F.);
#29211=ORIENTED_EDGE('',*,*,#20431,.F.);
#29212=ORIENTED_EDGE('',*,*,#20428,.F.);
#29213=ORIENTED_EDGE('',*,*,#20444,.F.);
#29214=ORIENTED_EDGE('',*,*,#20442,.F.);
#29215=ORIENTED_EDGE('',*,*,#20440,.F.);
#29216=ORIENTED_EDGE('',*,*,#20438,.F.);
#29217=ORIENTED_EDGE('',*,*,#20445,.T.);
#29218=ORIENTED_EDGE('',*,*,#20446,.F.);
#29219=ORIENTED_EDGE('',*,*,#20447,.F.);
#29220=ORIENTED_EDGE('',*,*,#20448,.T.);
#29221=ORIENTED_EDGE('',*,*,#20449,.T.);
#29222=ORIENTED_EDGE('',*,*,#20450,.T.);
#29223=ORIENTED_EDGE('',*,*,#20451,.T.);
#29224=ORIENTED_EDGE('',*,*,#20447,.T.);
#29225=ORIENTED_EDGE('',*,*,#20452,.F.);
#29226=ORIENTED_EDGE('',*,*,#20453,.F.);
#29227=ORIENTED_EDGE('',*,*,#20453,.T.);
#29228=ORIENTED_EDGE('',*,*,#20454,.F.);
#29229=ORIENTED_EDGE('',*,*,#20455,.F.);
#29230=ORIENTED_EDGE('',*,*,#20456,.T.);
#29231=ORIENTED_EDGE('',*,*,#20457,.F.);
#29232=ORIENTED_EDGE('',*,*,#20458,.F.);
#29233=ORIENTED_EDGE('',*,*,#20459,.F.);
#29234=ORIENTED_EDGE('',*,*,#20460,.T.);
#29235=ORIENTED_EDGE('',*,*,#20461,.F.);
#29236=ORIENTED_EDGE('',*,*,#20462,.F.);
#29237=ORIENTED_EDGE('',*,*,#20463,.F.);
#29238=ORIENTED_EDGE('',*,*,#20464,.T.);
#29239=ORIENTED_EDGE('',*,*,#20465,.F.);
#29240=ORIENTED_EDGE('',*,*,#20464,.F.);
#29241=ORIENTED_EDGE('',*,*,#20466,.F.);
#29242=ORIENTED_EDGE('',*,*,#20467,.F.);
#29243=ORIENTED_EDGE('',*,*,#20467,.T.);
#29244=ORIENTED_EDGE('',*,*,#20468,.F.);
#29245=ORIENTED_EDGE('',*,*,#20469,.F.);
#29246=ORIENTED_EDGE('',*,*,#20470,.F.);
#29247=ORIENTED_EDGE('',*,*,#20471,.F.);
#29248=ORIENTED_EDGE('',*,*,#20469,.T.);
#29249=ORIENTED_EDGE('',*,*,#20472,.F.);
#29250=ORIENTED_EDGE('',*,*,#20473,.F.);
#29251=ORIENTED_EDGE('',*,*,#20473,.T.);
#29252=ORIENTED_EDGE('',*,*,#20474,.F.);
#29253=ORIENTED_EDGE('',*,*,#20475,.F.);
#29254=ORIENTED_EDGE('',*,*,#20476,.F.);
#29255=ORIENTED_EDGE('',*,*,#20477,.F.);
#29256=ORIENTED_EDGE('',*,*,#20478,.F.);
#29257=ORIENTED_EDGE('',*,*,#20479,.F.);
#29258=ORIENTED_EDGE('',*,*,#20480,.F.);
#29259=ORIENTED_EDGE('',*,*,#20475,.T.);
#29260=ORIENTED_EDGE('',*,*,#20481,.F.);
#29261=ORIENTED_EDGE('',*,*,#20482,.T.);
#29262=ORIENTED_EDGE('',*,*,#20483,.F.);
#29263=ORIENTED_EDGE('',*,*,#20484,.T.);
#29264=ORIENTED_EDGE('',*,*,#20485,.T.);
#29265=ORIENTED_EDGE('',*,*,#20486,.T.);
#29266=ORIENTED_EDGE('',*,*,#20487,.T.);
#29267=ORIENTED_EDGE('',*,*,#20446,.T.);
#29268=ORIENTED_EDGE('',*,*,#20484,.F.);
#29269=ORIENTED_EDGE('',*,*,#20488,.T.);
#29270=ORIENTED_EDGE('',*,*,#20452,.T.);
#29271=ORIENTED_EDGE('',*,*,#20487,.F.);
#29272=ORIENTED_EDGE('',*,*,#20489,.F.);
#29273=ORIENTED_EDGE('',*,*,#20490,.T.);
#29274=ORIENTED_EDGE('',*,*,#20454,.T.);
#29275=ORIENTED_EDGE('',*,*,#20488,.F.);
#29276=ORIENTED_EDGE('',*,*,#20491,.T.);
#29277=ORIENTED_EDGE('',*,*,#20492,.T.);
#29278=ORIENTED_EDGE('',*,*,#20490,.F.);
#29279=ORIENTED_EDGE('',*,*,#20493,.F.);
#29280=ORIENTED_EDGE('',*,*,#20494,.T.);
#29281=ORIENTED_EDGE('',*,*,#20495,.T.);
#29282=ORIENTED_EDGE('',*,*,#20491,.F.);
#29283=ORIENTED_EDGE('',*,*,#20496,.F.);
#29284=ORIENTED_EDGE('',*,*,#20497,.T.);
#29285=ORIENTED_EDGE('',*,*,#20498,.T.);
#29286=ORIENTED_EDGE('',*,*,#20494,.F.);
#29287=ORIENTED_EDGE('',*,*,#20499,.F.);
#29288=ORIENTED_EDGE('',*,*,#20500,.T.);
#29289=ORIENTED_EDGE('',*,*,#20459,.T.);
#29290=ORIENTED_EDGE('',*,*,#20497,.F.);
#29291=ORIENTED_EDGE('',*,*,#20501,.F.);
#29292=ORIENTED_EDGE('',*,*,#20502,.T.);
#29293=ORIENTED_EDGE('',*,*,#20503,.T.);
#29294=ORIENTED_EDGE('',*,*,#20500,.F.);
#29295=ORIENTED_EDGE('',*,*,#20504,.F.);
#29296=ORIENTED_EDGE('',*,*,#20505,.T.);
#29297=ORIENTED_EDGE('',*,*,#20463,.T.);
#29298=ORIENTED_EDGE('',*,*,#20502,.F.);
#29299=ORIENTED_EDGE('',*,*,#20506,.F.);
#29300=ORIENTED_EDGE('',*,*,#20507,.T.);
#29301=ORIENTED_EDGE('',*,*,#20466,.T.);
#29302=ORIENTED_EDGE('',*,*,#20505,.F.);
#29303=ORIENTED_EDGE('',*,*,#20508,.F.);
#29304=ORIENTED_EDGE('',*,*,#20509,.T.);
#29305=ORIENTED_EDGE('',*,*,#20468,.T.);
#29306=ORIENTED_EDGE('',*,*,#20507,.F.);
#29307=ORIENTED_EDGE('',*,*,#20510,.T.);
#29308=ORIENTED_EDGE('',*,*,#20472,.T.);
#29309=ORIENTED_EDGE('',*,*,#20509,.F.);
#29310=ORIENTED_EDGE('',*,*,#20511,.F.);
#29311=ORIENTED_EDGE('',*,*,#20512,.T.);
#29312=ORIENTED_EDGE('',*,*,#20474,.T.);
#29313=ORIENTED_EDGE('',*,*,#20510,.F.);
#29314=ORIENTED_EDGE('',*,*,#20481,.T.);
#29315=ORIENTED_EDGE('',*,*,#20512,.F.);
#29316=ORIENTED_EDGE('',*,*,#20513,.F.);
#29317=ORIENTED_EDGE('',*,*,#20514,.T.);
#29318=ORIENTED_EDGE('',*,*,#20513,.T.);
#29319=ORIENTED_EDGE('',*,*,#20511,.T.);
#29320=ORIENTED_EDGE('',*,*,#20508,.T.);
#29321=ORIENTED_EDGE('',*,*,#20506,.T.);
#29322=ORIENTED_EDGE('',*,*,#20504,.T.);
#29323=ORIENTED_EDGE('',*,*,#20501,.T.);
#29324=ORIENTED_EDGE('',*,*,#20499,.T.);
#29325=ORIENTED_EDGE('',*,*,#20496,.T.);
#29326=ORIENTED_EDGE('',*,*,#20493,.T.);
#29327=ORIENTED_EDGE('',*,*,#20489,.T.);
#29328=ORIENTED_EDGE('',*,*,#20483,.T.);
#29329=ORIENTED_EDGE('',*,*,#20515,.T.);
#29330=ORIENTED_EDGE('',*,*,#20516,.T.);
#29331=ORIENTED_EDGE('',*,*,#20517,.T.);
#29332=ORIENTED_EDGE('',*,*,#20518,.T.);
#29333=ORIENTED_EDGE('',*,*,#20519,.T.);
#29334=ORIENTED_EDGE('',*,*,#20520,.T.);
#29335=ORIENTED_EDGE('',*,*,#20521,.T.);
#29336=ORIENTED_EDGE('',*,*,#20522,.F.);
#29337=ORIENTED_EDGE('',*,*,#20523,.F.);
#29338=ORIENTED_EDGE('',*,*,#20523,.T.);
#29339=ORIENTED_EDGE('',*,*,#20524,.F.);
#29340=ORIENTED_EDGE('',*,*,#20525,.F.);
#29341=ORIENTED_EDGE('',*,*,#20526,.T.);
#29342=ORIENTED_EDGE('',*,*,#20527,.T.);
#29343=ORIENTED_EDGE('',*,*,#20525,.T.);
#29344=ORIENTED_EDGE('',*,*,#20528,.F.);
#29345=ORIENTED_EDGE('',*,*,#20529,.F.);
#29346=ORIENTED_EDGE('',*,*,#20529,.T.);
#29347=ORIENTED_EDGE('',*,*,#20530,.F.);
#29348=ORIENTED_EDGE('',*,*,#20531,.F.);
#29349=ORIENTED_EDGE('',*,*,#20532,.T.);
#29350=ORIENTED_EDGE('',*,*,#20531,.T.);
#29351=ORIENTED_EDGE('',*,*,#20533,.F.);
#29352=ORIENTED_EDGE('',*,*,#20534,.T.);
#29353=ORIENTED_EDGE('',*,*,#20535,.T.);
#29354=ORIENTED_EDGE('',*,*,#20536,.T.);
#29355=ORIENTED_EDGE('',*,*,#20534,.F.);
#29356=ORIENTED_EDGE('',*,*,#20537,.F.);
#29357=ORIENTED_EDGE('',*,*,#20538,.T.);
#29358=ORIENTED_EDGE('',*,*,#20539,.T.);
#29359=ORIENTED_EDGE('',*,*,#20540,.F.);
#29360=ORIENTED_EDGE('',*,*,#20521,.F.);
#29361=ORIENTED_EDGE('',*,*,#20541,.F.);
#29362=ORIENTED_EDGE('',*,*,#20542,.T.);
#29363=ORIENTED_EDGE('',*,*,#20522,.T.);
#29364=ORIENTED_EDGE('',*,*,#20543,.F.);
#29365=ORIENTED_EDGE('',*,*,#20544,.F.);
#29366=ORIENTED_EDGE('',*,*,#20545,.T.);
#29367=ORIENTED_EDGE('',*,*,#20524,.T.);
#29368=ORIENTED_EDGE('',*,*,#20542,.F.);
#29369=ORIENTED_EDGE('',*,*,#20546,.T.);
#29370=ORIENTED_EDGE('',*,*,#20528,.T.);
#29371=ORIENTED_EDGE('',*,*,#20545,.F.);
#29372=ORIENTED_EDGE('',*,*,#20547,.F.);
#29373=ORIENTED_EDGE('',*,*,#20548,.T.);
#29374=ORIENTED_EDGE('',*,*,#20530,.T.);
#29375=ORIENTED_EDGE('',*,*,#20546,.F.);
#29376=ORIENTED_EDGE('',*,*,#20549,.T.);
#29377=ORIENTED_EDGE('',*,*,#20533,.T.);
#29378=ORIENTED_EDGE('',*,*,#20548,.F.);
#29379=ORIENTED_EDGE('',*,*,#20550,.F.);
#29380=ORIENTED_EDGE('',*,*,#20551,.T.);
#29381=ORIENTED_EDGE('',*,*,#20537,.T.);
#29382=ORIENTED_EDGE('',*,*,#20549,.F.);
#29383=ORIENTED_EDGE('',*,*,#20552,.F.);
#29384=ORIENTED_EDGE('',*,*,#19876,.T.);
#29385=ORIENTED_EDGE('',*,*,#20553,.T.);
#29386=ORIENTED_EDGE('',*,*,#20554,.F.);
#29387=ORIENTED_EDGE('',*,*,#20555,.T.);
#29388=ORIENTED_EDGE('',*,*,#20551,.F.);
#29389=ORIENTED_EDGE('',*,*,#20556,.F.);
#29390=ORIENTED_EDGE('',*,*,#20554,.T.);
#29391=ORIENTED_EDGE('',*,*,#20543,.T.);
#29392=ORIENTED_EDGE('',*,*,#20540,.T.);
#29393=ORIENTED_EDGE('',*,*,#20557,.F.);
#29394=ORIENTED_EDGE('',*,*,#20558,.T.);
#29395=ORIENTED_EDGE('',*,*,#20559,.F.);
#29396=ORIENTED_EDGE('',*,*,#19880,.F.);
#29397=ORIENTED_EDGE('',*,*,#20560,.F.);
#29398=ORIENTED_EDGE('',*,*,#20557,.T.);
#29399=ORIENTED_EDGE('',*,*,#20561,.T.);
#29400=ORIENTED_EDGE('',*,*,#20558,.F.);
#29401=ORIENTED_EDGE('',*,*,#20556,.T.);
#29402=ORIENTED_EDGE('',*,*,#20552,.T.);
#29403=ORIENTED_EDGE('',*,*,#20550,.T.);
#29404=ORIENTED_EDGE('',*,*,#20547,.T.);
#29405=ORIENTED_EDGE('',*,*,#20544,.T.);
#29406=ORIENTED_EDGE('',*,*,#20560,.T.);
#29407=ORIENTED_EDGE('',*,*,#19882,.F.);
#29408=ORIENTED_EDGE('',*,*,#19865,.F.);
#29409=ORIENTED_EDGE('',*,*,#19869,.F.);
#29410=ORIENTED_EDGE('',*,*,#19872,.F.);
#29411=ORIENTED_EDGE('',*,*,#19874,.F.);
#29412=ORIENTED_EDGE('',*,*,#19877,.F.);
#29413=ORIENTED_EDGE('',*,*,#20562,.T.);
#29414=ORIENTED_EDGE('',*,*,#20563,.F.);
#29415=ORIENTED_EDGE('',*,*,#20564,.T.);
#29416=ORIENTED_EDGE('',*,*,#20565,.T.);
#29417=ORIENTED_EDGE('',*,*,#20566,.F.);
#29418=ORIENTED_EDGE('',*,*,#20567,.T.);
#29419=ORIENTED_EDGE('',*,*,#20568,.T.);
#29420=ORIENTED_EDGE('',*,*,#20569,.F.);
#29421=ORIENTED_EDGE('',*,*,#20570,.F.);
#29422=ORIENTED_EDGE('',*,*,#20571,.T.);
#29423=ORIENTED_EDGE('',*,*,#20572,.F.);
#29424=ORIENTED_EDGE('',*,*,#20573,.F.);
#29425=ORIENTED_EDGE('',*,*,#20574,.F.);
#29426=ORIENTED_EDGE('',*,*,#20575,.F.);
#29427=ORIENTED_EDGE('',*,*,#20576,.T.);
#29428=ORIENTED_EDGE('',*,*,#20577,.T.);
#29429=ORIENTED_EDGE('',*,*,#20574,.T.);
#29430=ORIENTED_EDGE('',*,*,#20578,.T.);
#29431=ORIENTED_EDGE('',*,*,#20564,.F.);
#29432=ORIENTED_EDGE('',*,*,#20579,.T.);
#29433=ORIENTED_EDGE('',*,*,#20565,.F.);
#29434=ORIENTED_EDGE('',*,*,#20580,.T.);
#29435=ORIENTED_EDGE('',*,*,#20581,.T.);
#29436=ORIENTED_EDGE('',*,*,#20566,.T.);
#29437=ORIENTED_EDGE('',*,*,#20562,.F.);
#29438=ORIENTED_EDGE('',*,*,#20582,.F.);
#29439=ORIENTED_EDGE('',*,*,#20583,.T.);
#29440=ORIENTED_EDGE('',*,*,#20567,.F.);
#29441=ORIENTED_EDGE('',*,*,#20584,.F.);
#29442=ORIENTED_EDGE('',*,*,#20585,.T.);
#29443=ORIENTED_EDGE('',*,*,#20570,.T.);
#29444=ORIENTED_EDGE('',*,*,#20568,.F.);
#29445=ORIENTED_EDGE('',*,*,#20586,.F.);
#29446=ORIENTED_EDGE('',*,*,#20587,.T.);
#29447=ORIENTED_EDGE('',*,*,#20588,.F.);
#29448=ORIENTED_EDGE('',*,*,#20571,.F.);
#29449=ORIENTED_EDGE('',*,*,#20589,.F.);
#29450=ORIENTED_EDGE('',*,*,#20572,.T.);
#29451=ORIENTED_EDGE('',*,*,#20590,.T.);
#29452=ORIENTED_EDGE('',*,*,#20576,.F.);
#29453=ORIENTED_EDGE('',*,*,#20591,.T.);
#29454=ORIENTED_EDGE('',*,*,#20592,.F.);
#29455=ORIENTED_EDGE('',*,*,#20577,.F.);
#29456=ORIENTED_EDGE('',*,*,#20593,.T.);
#29457=ORIENTED_EDGE('',*,*,#20594,.T.);
#29458=ORIENTED_EDGE('',*,*,#20580,.F.);
#29459=ORIENTED_EDGE('',*,*,#20578,.F.);
#29460=ORIENTED_EDGE('',*,*,#20592,.T.);
#29461=ORIENTED_EDGE('',*,*,#20595,.T.);
#29462=ORIENTED_EDGE('',*,*,#20596,.T.);
#29463=ORIENTED_EDGE('',*,*,#20597,.F.);
#29464=ORIENTED_EDGE('',*,*,#20581,.F.);
#29465=ORIENTED_EDGE('',*,*,#20598,.T.);
#29466=ORIENTED_EDGE('',*,*,#20584,.T.);
#29467=ORIENTED_EDGE('',*,*,#20582,.T.);
#29468=ORIENTED_EDGE('',*,*,#20579,.F.);
#29469=ORIENTED_EDGE('',*,*,#20599,.T.);
#29470=ORIENTED_EDGE('',*,*,#20600,.T.);
#29471=ORIENTED_EDGE('',*,*,#20601,.F.);
#29472=ORIENTED_EDGE('',*,*,#20585,.F.);
#29473=ORIENTED_EDGE('',*,*,#20602,.T.);
#29474=ORIENTED_EDGE('',*,*,#20589,.T.);
#29475=ORIENTED_EDGE('',*,*,#20586,.T.);
#29476=ORIENTED_EDGE('',*,*,#20583,.F.);
#29477=ORIENTED_EDGE('',*,*,#20603,.T.);
#29478=ORIENTED_EDGE('',*,*,#20604,.T.);
#29479=ORIENTED_EDGE('',*,*,#20605,.F.);
#29480=ORIENTED_EDGE('',*,*,#20587,.F.);
#29481=ORIENTED_EDGE('',*,*,#20606,.T.);
#29482=ORIENTED_EDGE('',*,*,#20593,.F.);
#29483=ORIENTED_EDGE('',*,*,#20590,.F.);
#29484=ORIENTED_EDGE('',*,*,#20588,.T.);
#29485=ORIENTED_EDGE('',*,*,#20607,.T.);
#29486=ORIENTED_EDGE('',*,*,#20608,.T.);
#29487=ORIENTED_EDGE('',*,*,#20609,.F.);
#29488=ORIENTED_EDGE('',*,*,#20591,.F.);
#29489=ORIENTED_EDGE('',*,*,#20609,.T.);
#29490=ORIENTED_EDGE('',*,*,#20610,.T.);
#29491=ORIENTED_EDGE('',*,*,#20595,.F.);
#29492=ORIENTED_EDGE('',*,*,#20594,.F.);
#29493=ORIENTED_EDGE('',*,*,#20611,.T.);
#29494=ORIENTED_EDGE('',*,*,#20612,.F.);
#29495=ORIENTED_EDGE('',*,*,#20613,.F.);
#29496=ORIENTED_EDGE('',*,*,#20597,.T.);
#29497=ORIENTED_EDGE('',*,*,#20614,.T.);
#29498=ORIENTED_EDGE('',*,*,#20599,.F.);
#29499=ORIENTED_EDGE('',*,*,#20598,.F.);
#29500=ORIENTED_EDGE('',*,*,#20601,.T.);
#29501=ORIENTED_EDGE('',*,*,#20615,.T.);
#29502=ORIENTED_EDGE('',*,*,#20603,.F.);
#29503=ORIENTED_EDGE('',*,*,#20602,.F.);
#29504=ORIENTED_EDGE('',*,*,#20605,.T.);
#29505=ORIENTED_EDGE('',*,*,#20616,.T.);
#29506=ORIENTED_EDGE('',*,*,#20607,.F.);
#29507=ORIENTED_EDGE('',*,*,#20606,.F.);
#29508=ORIENTED_EDGE('',*,*,#20617,.T.);
#29509=ORIENTED_EDGE('',*,*,#19938,.T.);
#29510=ORIENTED_EDGE('',*,*,#20618,.F.);
#29511=ORIENTED_EDGE('',*,*,#20619,.F.);
#29512=ORIENTED_EDGE('',*,*,#20620,.F.);
#29513=ORIENTED_EDGE('',*,*,#20621,.T.);
#29514=ORIENTED_EDGE('',*,*,#20618,.T.);
#29515=ORIENTED_EDGE('',*,*,#20563,.T.);
#29516=ORIENTED_EDGE('',*,*,#20569,.T.);
#29517=ORIENTED_EDGE('',*,*,#20573,.T.);
#29518=ORIENTED_EDGE('',*,*,#20575,.T.);
#29519=ORIENTED_EDGE('',*,*,#20622,.T.);
#29520=ORIENTED_EDGE('',*,*,#20623,.T.);
#29521=ORIENTED_EDGE('',*,*,#20519,.F.);
#29522=ORIENTED_EDGE('',*,*,#20624,.F.);
#29523=ORIENTED_EDGE('',*,*,#20625,.F.);
#29524=ORIENTED_EDGE('',*,*,#20626,.T.);
#29525=ORIENTED_EDGE('',*,*,#20627,.T.);
#29526=ORIENTED_EDGE('',*,*,#20622,.F.);
#29527=ORIENTED_EDGE('',*,*,#20628,.T.);
#29528=ORIENTED_EDGE('',*,*,#20629,.T.);
#29529=ORIENTED_EDGE('',*,*,#20630,.T.);
#29530=ORIENTED_EDGE('',*,*,#19949,.F.);
#29531=ORIENTED_EDGE('',*,*,#20631,.T.);
#29532=ORIENTED_EDGE('',*,*,#20632,.T.);
#29533=ORIENTED_EDGE('',*,*,#20629,.F.);
#29534=ORIENTED_EDGE('',*,*,#20633,.T.);
#29535=ORIENTED_EDGE('',*,*,#20559,.T.);
#29536=ORIENTED_EDGE('',*,*,#20634,.T.);
#29537=ORIENTED_EDGE('',*,*,#20635,.F.);
#29538=ORIENTED_EDGE('',*,*,#19963,.F.);
#29539=ORIENTED_EDGE('',*,*,#20561,.F.);
#29540=ORIENTED_EDGE('',*,*,#20539,.F.);
#29541=ORIENTED_EDGE('',*,*,#20636,.F.);
#29542=ORIENTED_EDGE('',*,*,#20637,.F.);
#29543=ORIENTED_EDGE('',*,*,#20638,.F.);
#29544=ORIENTED_EDGE('',*,*,#20639,.F.);
#29545=ORIENTED_EDGE('',*,*,#20640,.F.);
#29546=ORIENTED_EDGE('',*,*,#20641,.F.);
#29547=ORIENTED_EDGE('',*,*,#20642,.F.);
#29548=ORIENTED_EDGE('',*,*,#20643,.F.);
#29549=ORIENTED_EDGE('',*,*,#20644,.F.);
#29550=ORIENTED_EDGE('',*,*,#20645,.F.);
#29551=ORIENTED_EDGE('',*,*,#20646,.F.);
#29552=ORIENTED_EDGE('',*,*,#20634,.F.);
#29553=ORIENTED_EDGE('',*,*,#20647,.T.);
#29554=ORIENTED_EDGE('',*,*,#19968,.T.);
#29555=ORIENTED_EDGE('',*,*,#20648,.T.);
#29556=ORIENTED_EDGE('',*,*,#20649,.F.);
#29557=ORIENTED_EDGE('',*,*,#20649,.T.);
#29558=ORIENTED_EDGE('',*,*,#20650,.T.);
#29559=ORIENTED_EDGE('',*,*,#20651,.T.);
#29560=ORIENTED_EDGE('',*,*,#20652,.F.);
#29561=ORIENTED_EDGE('',*,*,#20653,.T.);
#29562=ORIENTED_EDGE('',*,*,#20654,.T.);
#29563=ORIENTED_EDGE('',*,*,#20652,.T.);
#29564=ORIENTED_EDGE('',*,*,#20655,.T.);
#29565=ORIENTED_EDGE('',*,*,#20656,.F.);
#29566=ORIENTED_EDGE('',*,*,#20656,.T.);
#29567=ORIENTED_EDGE('',*,*,#20657,.T.);
#29568=ORIENTED_EDGE('',*,*,#20658,.T.);
#29569=ORIENTED_EDGE('',*,*,#20659,.T.);
#29570=ORIENTED_EDGE('',*,*,#20660,.F.);
#29571=ORIENTED_EDGE('',*,*,#20661,.T.);
#29572=ORIENTED_EDGE('',*,*,#20662,.T.);
#29573=ORIENTED_EDGE('',*,*,#20660,.T.);
#29574=ORIENTED_EDGE('',*,*,#20663,.T.);
#29575=ORIENTED_EDGE('',*,*,#20664,.F.);
#29576=ORIENTED_EDGE('',*,*,#20664,.T.);
#29577=ORIENTED_EDGE('',*,*,#20665,.T.);
#29578=ORIENTED_EDGE('',*,*,#20666,.T.);
#29579=ORIENTED_EDGE('',*,*,#20667,.T.);
#29580=ORIENTED_EDGE('',*,*,#20668,.F.);
#29581=ORIENTED_EDGE('',*,*,#20669,.T.);
#29582=ORIENTED_EDGE('',*,*,#20670,.T.);
#29583=ORIENTED_EDGE('',*,*,#20668,.T.);
#29584=ORIENTED_EDGE('',*,*,#20671,.T.);
#29585=ORIENTED_EDGE('',*,*,#20631,.F.);
#29586=ORIENTED_EDGE('',*,*,#20672,.T.);
#29587=ORIENTED_EDGE('',*,*,#20673,.F.);
#29588=ORIENTED_EDGE('',*,*,#20486,.F.);
#29589=ORIENTED_EDGE('',*,*,#20673,.T.);
#29590=ORIENTED_EDGE('',*,*,#20674,.T.);
#29591=ORIENTED_EDGE('',*,*,#20675,.F.);
#29592=ORIENTED_EDGE('',*,*,#20515,.F.);
#29593=ORIENTED_EDGE('',*,*,#20676,.F.);
#29594=ORIENTED_EDGE('',*,*,#20677,.T.);
#29595=ORIENTED_EDGE('',*,*,#20674,.F.);
#29596=ORIENTED_EDGE('',*,*,#20678,.F.);
#29597=ORIENTED_EDGE('',*,*,#20679,.F.);
#29598=ORIENTED_EDGE('',*,*,#20680,.T.);
#29599=ORIENTED_EDGE('',*,*,#20360,.T.);
#29600=ORIENTED_EDGE('',*,*,#19992,.T.);
#29601=ORIENTED_EDGE('',*,*,#19990,.T.);
#29602=ORIENTED_EDGE('',*,*,#20185,.F.);
#29603=ORIENTED_EDGE('',*,*,#20169,.T.);
#29604=ORIENTED_EDGE('',*,*,#20205,.T.);
#29605=ORIENTED_EDGE('',*,*,#20209,.T.);
#29606=ORIENTED_EDGE('',*,*,#20681,.T.);
#29607=ORIENTED_EDGE('',*,*,#20682,.F.);
#29608=ORIENTED_EDGE('',*,*,#20683,.F.);
#29609=ORIENTED_EDGE('',*,*,#20684,.T.);
#29610=ORIENTED_EDGE('',*,*,#20678,.T.);
#29611=ORIENTED_EDGE('',*,*,#20672,.F.);
#29612=ORIENTED_EDGE('',*,*,#20685,.F.);
#29613=ORIENTED_EDGE('',*,*,#20485,.F.);
#29614=ORIENTED_EDGE('',*,*,#20445,.F.);
#29615=ORIENTED_EDGE('',*,*,#20686,.T.);
#29616=ORIENTED_EDGE('',*,*,#20687,.F.);
#29617=ORIENTED_EDGE('',*,*,#20688,.T.);
#29618=ORIENTED_EDGE('',*,*,#20689,.T.);
#29619=ORIENTED_EDGE('',*,*,#20690,.T.);
#29620=ORIENTED_EDGE('',*,*,#20691,.T.);
#29621=ORIENTED_EDGE('',*,*,#20685,.T.);
#29622=ORIENTED_EDGE('',*,*,#20692,.T.);
#29623=ORIENTED_EDGE('',*,*,#20693,.F.);
#29624=ORIENTED_EDGE('',*,*,#20694,.T.);
#29625=ORIENTED_EDGE('',*,*,#20687,.T.);
#29626=ORIENTED_EDGE('',*,*,#20695,.F.);
#29627=ORIENTED_EDGE('',*,*,#20696,.T.);
#29628=ORIENTED_EDGE('',*,*,#20693,.T.);
#29629=ORIENTED_EDGE('',*,*,#20697,.T.);
#29630=ORIENTED_EDGE('',*,*,#20698,.T.);
#29631=ORIENTED_EDGE('',*,*,#20699,.F.);
#29632=ORIENTED_EDGE('',*,*,#20700,.T.);
#29633=ORIENTED_EDGE('',*,*,#20695,.T.);
#29634=ORIENTED_EDGE('',*,*,#20701,.F.);
#29635=ORIENTED_EDGE('',*,*,#20702,.T.);
#29636=ORIENTED_EDGE('',*,*,#20699,.T.);
#29637=ORIENTED_EDGE('',*,*,#20703,.T.);
#29638=ORIENTED_EDGE('',*,*,#20704,.T.);
#29639=ORIENTED_EDGE('',*,*,#20689,.F.);
#29640=ORIENTED_EDGE('',*,*,#20705,.T.);
#29641=ORIENTED_EDGE('',*,*,#20706,.T.);
#29642=ORIENTED_EDGE('',*,*,#20707,.T.);
#29643=ORIENTED_EDGE('',*,*,#20708,.F.);
#29644=ORIENTED_EDGE('',*,*,#20709,.T.);
#29645=ORIENTED_EDGE('',*,*,#20701,.T.);
#29646=ORIENTED_EDGE('',*,*,#20710,.T.);
#29647=ORIENTED_EDGE('',*,*,#20706,.F.);
#29648=ORIENTED_EDGE('',*,*,#20711,.T.);
#29649=ORIENTED_EDGE('',*,*,#20708,.T.);
#29650=ORIENTED_EDGE('',*,*,#20712,.T.);
#29651=ORIENTED_EDGE('',*,*,#20713,.T.);
#29652=ORIENTED_EDGE('',*,*,#20714,.F.);
#29653=ORIENTED_EDGE('',*,*,#20715,.F.);
#29654=ORIENTED_EDGE('',*,*,#20716,.T.);
#29655=ORIENTED_EDGE('',*,*,#20717,.T.);
#29656=ORIENTED_EDGE('',*,*,#20718,.F.);
#29657=ORIENTED_EDGE('',*,*,#20719,.F.);
#29658=ORIENTED_EDGE('',*,*,#20720,.T.);
#29659=ORIENTED_EDGE('',*,*,#20721,.T.);
#29660=ORIENTED_EDGE('',*,*,#20716,.F.);
#29661=ORIENTED_EDGE('',*,*,#20722,.F.);
#29662=ORIENTED_EDGE('',*,*,#20723,.T.);
#29663=ORIENTED_EDGE('',*,*,#20724,.T.);
#29664=ORIENTED_EDGE('',*,*,#20720,.F.);
#29665=ORIENTED_EDGE('',*,*,#20725,.F.);
#29666=ORIENTED_EDGE('',*,*,#20726,.T.);
#29667=ORIENTED_EDGE('',*,*,#20727,.T.);
#29668=ORIENTED_EDGE('',*,*,#20723,.F.);
#29669=ORIENTED_EDGE('',*,*,#20728,.F.);
#29670=ORIENTED_EDGE('',*,*,#20729,.T.);
#29671=ORIENTED_EDGE('',*,*,#20730,.T.);
#29672=ORIENTED_EDGE('',*,*,#20726,.F.);
#29673=ORIENTED_EDGE('',*,*,#20731,.F.);
#29674=ORIENTED_EDGE('',*,*,#20718,.T.);
#29675=ORIENTED_EDGE('',*,*,#20732,.T.);
#29676=ORIENTED_EDGE('',*,*,#20733,.F.);
#29677=ORIENTED_EDGE('',*,*,#20734,.F.);
#29678=ORIENTED_EDGE('',*,*,#20735,.T.);
#29679=ORIENTED_EDGE('',*,*,#20736,.T.);
#29680=ORIENTED_EDGE('',*,*,#20729,.F.);
#29681=ORIENTED_EDGE('',*,*,#20737,.F.);
#29682=ORIENTED_EDGE('',*,*,#20733,.T.);
#29683=ORIENTED_EDGE('',*,*,#20738,.T.);
#29684=ORIENTED_EDGE('',*,*,#20735,.F.);
#29685=ORIENTED_EDGE('',*,*,#20739,.F.);
#29686=ORIENTED_EDGE('',*,*,#20740,.T.);
#29687=ORIENTED_EDGE('',*,*,#20741,.T.);
#29688=ORIENTED_EDGE('',*,*,#20742,.F.);
#29689=ORIENTED_EDGE('',*,*,#20743,.F.);
#29690=ORIENTED_EDGE('',*,*,#20744,.T.);
#29691=ORIENTED_EDGE('',*,*,#20745,.T.);
#29692=ORIENTED_EDGE('',*,*,#20746,.F.);
#29693=ORIENTED_EDGE('',*,*,#20666,.F.);
#29694=ORIENTED_EDGE('',*,*,#20747,.F.);
#29695=ORIENTED_EDGE('',*,*,#20748,.F.);
#29696=ORIENTED_EDGE('',*,*,#20742,.T.);
#29697=ORIENTED_EDGE('',*,*,#20749,.T.);
#29698=ORIENTED_EDGE('',*,*,#20745,.F.);
#29699=ORIENTED_EDGE('',*,*,#20750,.T.);
#29700=ORIENTED_EDGE('',*,*,#20751,.T.);
#29701=ORIENTED_EDGE('',*,*,#20752,.F.);
#29702=ORIENTED_EDGE('',*,*,#20659,.F.);
#29703=ORIENTED_EDGE('',*,*,#20752,.T.);
#29704=ORIENTED_EDGE('',*,*,#20753,.T.);
#29705=ORIENTED_EDGE('',*,*,#20754,.F.);
#29706=ORIENTED_EDGE('',*,*,#20663,.F.);
#29707=ORIENTED_EDGE('',*,*,#20754,.T.);
#29708=ORIENTED_EDGE('',*,*,#20755,.T.);
#29709=ORIENTED_EDGE('',*,*,#20744,.F.);
#29710=ORIENTED_EDGE('',*,*,#20665,.F.);
#29711=ORIENTED_EDGE('',*,*,#20756,.T.);
#29712=ORIENTED_EDGE('',*,*,#20757,.F.);
#29713=ORIENTED_EDGE('',*,*,#20758,.F.);
#29714=ORIENTED_EDGE('',*,*,#20747,.T.);
#29715=ORIENTED_EDGE('',*,*,#20755,.F.);
#29716=ORIENTED_EDGE('',*,*,#20753,.F.);
#29717=ORIENTED_EDGE('',*,*,#20751,.F.);
#29718=ORIENTED_EDGE('',*,*,#20759,.T.);
#29719=ORIENTED_EDGE('',*,*,#20760,.T.);
#29720=ORIENTED_EDGE('',*,*,#20740,.F.);
#29721=ORIENTED_EDGE('',*,*,#20761,.F.);
#29722=ORIENTED_EDGE('',*,*,#20757,.T.);
#29723=ORIENTED_EDGE('',*,*,#20762,.T.);
#29724=ORIENTED_EDGE('',*,*,#20763,.F.);
#29725=ORIENTED_EDGE('',*,*,#20764,.F.);
#29726=ORIENTED_EDGE('',*,*,#20763,.T.);
#29727=ORIENTED_EDGE('',*,*,#20765,.T.);
#29728=ORIENTED_EDGE('',*,*,#20759,.F.);
#29729=ORIENTED_EDGE('',*,*,#20766,.F.);
#29730=ORIENTED_EDGE('',*,*,#20767,.T.);
#29731=ORIENTED_EDGE('',*,*,#20768,.T.);
#29732=ORIENTED_EDGE('',*,*,#20769,.F.);
#29733=ORIENTED_EDGE('',*,*,#20651,.F.);
#29734=ORIENTED_EDGE('',*,*,#20769,.T.);
#29735=ORIENTED_EDGE('',*,*,#20770,.T.);
#29736=ORIENTED_EDGE('',*,*,#20771,.F.);
#29737=ORIENTED_EDGE('',*,*,#20655,.F.);
#29738=ORIENTED_EDGE('',*,*,#20771,.T.);
#29739=ORIENTED_EDGE('',*,*,#20772,.T.);
#29740=ORIENTED_EDGE('',*,*,#20773,.F.);
#29741=ORIENTED_EDGE('',*,*,#20657,.F.);
#29742=ORIENTED_EDGE('',*,*,#20774,.F.);
#29743=ORIENTED_EDGE('',*,*,#20775,.T.);
#29744=ORIENTED_EDGE('',*,*,#20776,.T.);
#29745=ORIENTED_EDGE('',*,*,#20777,.F.);
#29746=ORIENTED_EDGE('',*,*,#20778,.F.);
#29747=ORIENTED_EDGE('',*,*,#20772,.F.);
#29748=ORIENTED_EDGE('',*,*,#20770,.F.);
#29749=ORIENTED_EDGE('',*,*,#20768,.F.);
#29750=ORIENTED_EDGE('',*,*,#20779,.T.);
#29751=ORIENTED_EDGE('',*,*,#20780,.T.);
#29752=ORIENTED_EDGE('',*,*,#20775,.F.);
#29753=ORIENTED_EDGE('',*,*,#20781,.F.);
#29754=ORIENTED_EDGE('',*,*,#20782,.T.);
#29755=ORIENTED_EDGE('',*,*,#20783,.T.);
#29756=ORIENTED_EDGE('',*,*,#20779,.F.);
#29757=ORIENTED_EDGE('',*,*,#20784,.F.);
#29758=ORIENTED_EDGE('',*,*,#20785,.T.);
#29759=ORIENTED_EDGE('',*,*,#20786,.T.);
#29760=ORIENTED_EDGE('',*,*,#20782,.F.);
#29761=ORIENTED_EDGE('',*,*,#20787,.F.);
#29762=ORIENTED_EDGE('',*,*,#20788,.T.);
#29763=ORIENTED_EDGE('',*,*,#20789,.T.);
#29764=ORIENTED_EDGE('',*,*,#20785,.F.);
#29765=ORIENTED_EDGE('',*,*,#20790,.F.);
#29766=ORIENTED_EDGE('',*,*,#20777,.T.);
#29767=ORIENTED_EDGE('',*,*,#20791,.T.);
#29768=ORIENTED_EDGE('',*,*,#20792,.F.);
#29769=ORIENTED_EDGE('',*,*,#20793,.F.);
#29770=ORIENTED_EDGE('',*,*,#20794,.T.);
#29771=ORIENTED_EDGE('',*,*,#20795,.T.);
#29772=ORIENTED_EDGE('',*,*,#20788,.F.);
#29773=ORIENTED_EDGE('',*,*,#20796,.F.);
#29774=ORIENTED_EDGE('',*,*,#20792,.T.);
#29775=ORIENTED_EDGE('',*,*,#20797,.T.);
#29776=ORIENTED_EDGE('',*,*,#20794,.F.);
#29777=ORIENTED_EDGE('',*,*,#20798,.F.);
#29778=ORIENTED_EDGE('',*,*,#20799,.T.);
#29779=ORIENTED_EDGE('',*,*,#20800,.T.);
#29780=ORIENTED_EDGE('',*,*,#20801,.F.);
#29781=ORIENTED_EDGE('',*,*,#20802,.F.);
#29782=ORIENTED_EDGE('',*,*,#20611,.F.);
#29783=ORIENTED_EDGE('',*,*,#20803,.T.);
#29784=ORIENTED_EDGE('',*,*,#20804,.T.);
#29785=ORIENTED_EDGE('',*,*,#20805,.F.);
#29786=ORIENTED_EDGE('',*,*,#20806,.F.);
#29787=ORIENTED_EDGE('',*,*,#20807,.F.);
#29788=ORIENTED_EDGE('',*,*,#20808,.T.);
#29789=ORIENTED_EDGE('',*,*,#20809,.T.);
#29790=ORIENTED_EDGE('',*,*,#20810,.T.);
#29791=ORIENTED_EDGE('',*,*,#20808,.F.);
#29792=ORIENTED_EDGE('',*,*,#20811,.F.);
#29793=ORIENTED_EDGE('',*,*,#20812,.T.);
#29794=ORIENTED_EDGE('',*,*,#20813,.T.);
#29795=ORIENTED_EDGE('',*,*,#20810,.F.);
#29796=ORIENTED_EDGE('',*,*,#20814,.F.);
#29797=ORIENTED_EDGE('',*,*,#20806,.T.);
#29798=ORIENTED_EDGE('',*,*,#20815,.F.);
#29799=ORIENTED_EDGE('',*,*,#20816,.F.);
#29800=ORIENTED_EDGE('',*,*,#20817,.T.);
#29801=ORIENTED_EDGE('',*,*,#20812,.F.);
#29802=ORIENTED_EDGE('',*,*,#20818,.F.);
#29803=ORIENTED_EDGE('',*,*,#20819,.T.);
#29804=ORIENTED_EDGE('',*,*,#20820,.T.);
#29805=ORIENTED_EDGE('',*,*,#20799,.F.);
#29806=ORIENTED_EDGE('',*,*,#20815,.T.);
#29807=ORIENTED_EDGE('',*,*,#20821,.T.);
#29808=ORIENTED_EDGE('',*,*,#20817,.F.);
#29809=ORIENTED_EDGE('',*,*,#20822,.F.);
#29810=ORIENTED_EDGE('',*,*,#20823,.F.);
#29811=ORIENTED_EDGE('',*,*,#20824,.T.);
#29812=ORIENTED_EDGE('',*,*,#20819,.F.);
#29813=ORIENTED_EDGE('',*,*,#20825,.F.);
#29814=ORIENTED_EDGE('',*,*,#20714,.T.);
#29815=ORIENTED_EDGE('',*,*,#20826,.T.);
#29816=ORIENTED_EDGE('',*,*,#20827,.F.);
#29817=ORIENTED_EDGE('',*,*,#20828,.F.);
#29818=ORIENTED_EDGE('',*,*,#20827,.T.);
#29819=ORIENTED_EDGE('',*,*,#20829,.T.);
#29820=ORIENTED_EDGE('',*,*,#20830,.F.);
#29821=ORIENTED_EDGE('',*,*,#20831,.F.);
#29822=ORIENTED_EDGE('',*,*,#20832,.T.);
#29823=ORIENTED_EDGE('',*,*,#20833,.T.);
#29824=ORIENTED_EDGE('',*,*,#20626,.F.);
#29825=ORIENTED_EDGE('',*,*,#20834,.F.);
#29826=ORIENTED_EDGE('',*,*,#20830,.T.);
#29827=ORIENTED_EDGE('',*,*,#20835,.T.);
#29828=ORIENTED_EDGE('',*,*,#20836,.F.);
#29829=ORIENTED_EDGE('',*,*,#20837,.F.);
#29830=ORIENTED_EDGE('',*,*,#20838,.T.);
#29831=ORIENTED_EDGE('',*,*,#20804,.F.);
#29832=ORIENTED_EDGE('',*,*,#20839,.F.);
#29833=ORIENTED_EDGE('',*,*,#20840,.T.);
#29834=ORIENTED_EDGE('',*,*,#20150,.T.);
#29835=ORIENTED_EDGE('',*,*,#20617,.F.);
#29836=ORIENTED_EDGE('',*,*,#20841,.F.);
#29837=ORIENTED_EDGE('',*,*,#20621,.F.);
#29838=ORIENTED_EDGE('',*,*,#20842,.F.);
#29839=ORIENTED_EDGE('',*,*,#20843,.F.);
#29840=ORIENTED_EDGE('',*,*,#20841,.T.);
#29841=ORIENTED_EDGE('',*,*,#20620,.T.);
#29842=ORIENTED_EDGE('',*,*,#20712,.F.);
#29843=ORIENTED_EDGE('',*,*,#20844,.F.);
#29844=ORIENTED_EDGE('',*,*,#20154,.T.);
#29845=ORIENTED_EDGE('',*,*,#20840,.F.);
#29846=ORIENTED_EDGE('',*,*,#20845,.F.);
#29847=ORIENTED_EDGE('',*,*,#20845,.T.);
#29848=ORIENTED_EDGE('',*,*,#20843,.T.);
#29849=ORIENTED_EDGE('',*,*,#20846,.F.);
#29850=ORIENTED_EDGE('',*,*,#20847,.F.);
#29851=ORIENTED_EDGE('',*,*,#20848,.T.);
#29852=ORIENTED_EDGE('',*,*,#20849,.F.);
#29853=ORIENTED_EDGE('',*,*,#20850,.T.);
#29854=ORIENTED_EDGE('',*,*,#20851,.T.);
#29855=ORIENTED_EDGE('',*,*,#20838,.F.);
#29856=ORIENTED_EDGE('',*,*,#20852,.T.);
#29857=ORIENTED_EDGE('',*,*,#20853,.T.);
#29858=ORIENTED_EDGE('',*,*,#20854,.F.);
#29859=ORIENTED_EDGE('',*,*,#20855,.F.);
#29860=ORIENTED_EDGE('',*,*,#20856,.T.);
#29861=ORIENTED_EDGE('',*,*,#20857,.T.);
#29862=ORIENTED_EDGE('',*,*,#20640,.T.);
#29863=ORIENTED_EDGE('',*,*,#20858,.F.);
#29864=ORIENTED_EDGE('',*,*,#20859,.F.);
#29865=ORIENTED_EDGE('',*,*,#20860,.T.);
#29866=ORIENTED_EDGE('',*,*,#20676,.T.);
#29867=ORIENTED_EDGE('',*,*,#20861,.F.);
#29868=ORIENTED_EDGE('',*,*,#20862,.F.);
#29869=ORIENTED_EDGE('',*,*,#20863,.T.);
#29870=ORIENTED_EDGE('',*,*,#20864,.T.);
#29871=ORIENTED_EDGE('',*,*,#20865,.F.);
#29872=ORIENTED_EDGE('',*,*,#19948,.F.);
#29873=ORIENTED_EDGE('',*,*,#20866,.T.);
#29874=ORIENTED_EDGE('',*,*,#20867,.T.);
#29875=ORIENTED_EDGE('',*,*,#20868,.F.);
#29876=ORIENTED_EDGE('',*,*,#19964,.F.);
#29877=ORIENTED_EDGE('',*,*,#20868,.T.);
#29878=ORIENTED_EDGE('',*,*,#20869,.T.);
#29879=ORIENTED_EDGE('',*,*,#20870,.F.);
#29880=ORIENTED_EDGE('',*,*,#19969,.F.);
#29881=ORIENTED_EDGE('',*,*,#20870,.T.);
#29882=ORIENTED_EDGE('',*,*,#20871,.T.);
#29883=ORIENTED_EDGE('',*,*,#20872,.F.);
#29884=ORIENTED_EDGE('',*,*,#19972,.F.);
#29885=ORIENTED_EDGE('',*,*,#20872,.T.);
#29886=ORIENTED_EDGE('',*,*,#20873,.T.);
#29887=ORIENTED_EDGE('',*,*,#20874,.F.);
#29888=ORIENTED_EDGE('',*,*,#19977,.F.);
#29889=ORIENTED_EDGE('',*,*,#20874,.T.);
#29890=ORIENTED_EDGE('',*,*,#20875,.T.);
#29891=ORIENTED_EDGE('',*,*,#20876,.F.);
#29892=ORIENTED_EDGE('',*,*,#19980,.F.);
#29893=ORIENTED_EDGE('',*,*,#20876,.T.);
#29894=ORIENTED_EDGE('',*,*,#20877,.T.);
#29895=ORIENTED_EDGE('',*,*,#20863,.F.);
#29896=ORIENTED_EDGE('',*,*,#19985,.F.);
#29897=ORIENTED_EDGE('',*,*,#20865,.T.);
#29898=ORIENTED_EDGE('',*,*,#20878,.T.);
#29899=ORIENTED_EDGE('',*,*,#20879,.F.);
#29900=ORIENTED_EDGE('',*,*,#20628,.F.);
#29901=ORIENTED_EDGE('',*,*,#20879,.T.);
#29902=ORIENTED_EDGE('',*,*,#20880,.T.);
#29903=ORIENTED_EDGE('',*,*,#20881,.F.);
#29904=ORIENTED_EDGE('',*,*,#20633,.F.);
#29905=ORIENTED_EDGE('',*,*,#20882,.T.);
#29906=ORIENTED_EDGE('',*,*,#20883,.T.);
#29907=ORIENTED_EDGE('',*,*,#20866,.F.);
#29908=ORIENTED_EDGE('',*,*,#20647,.F.);
#29909=ORIENTED_EDGE('',*,*,#20884,.T.);
#29910=ORIENTED_EDGE('',*,*,#20885,.T.);
#29911=ORIENTED_EDGE('',*,*,#20882,.F.);
#29912=ORIENTED_EDGE('',*,*,#20653,.F.);
#29913=ORIENTED_EDGE('',*,*,#20886,.T.);
#29914=ORIENTED_EDGE('',*,*,#20887,.T.);
#29915=ORIENTED_EDGE('',*,*,#20884,.F.);
#29916=ORIENTED_EDGE('',*,*,#20654,.F.);
#29917=ORIENTED_EDGE('',*,*,#20888,.T.);
#29918=ORIENTED_EDGE('',*,*,#20889,.T.);
#29919=ORIENTED_EDGE('',*,*,#20886,.F.);
#29920=ORIENTED_EDGE('',*,*,#20661,.F.);
#29921=ORIENTED_EDGE('',*,*,#20890,.T.);
#29922=ORIENTED_EDGE('',*,*,#20891,.T.);
#29923=ORIENTED_EDGE('',*,*,#20888,.F.);
#29924=ORIENTED_EDGE('',*,*,#20662,.F.);
#29925=ORIENTED_EDGE('',*,*,#20892,.T.);
#29926=ORIENTED_EDGE('',*,*,#20893,.T.);
#29927=ORIENTED_EDGE('',*,*,#20890,.F.);
#29928=ORIENTED_EDGE('',*,*,#20669,.F.);
#29929=ORIENTED_EDGE('',*,*,#20881,.T.);
#29930=ORIENTED_EDGE('',*,*,#20894,.T.);
#29931=ORIENTED_EDGE('',*,*,#20892,.F.);
#29932=ORIENTED_EDGE('',*,*,#20670,.F.);
#29933=ORIENTED_EDGE('',*,*,#20859,.T.);
#29934=ORIENTED_EDGE('',*,*,#20895,.T.);
#29935=ORIENTED_EDGE('',*,*,#20862,.T.);
#29936=ORIENTED_EDGE('',*,*,#20896,.F.);
#29937=ORIENTED_EDGE('',*,*,#20897,.F.);
#29938=ORIENTED_EDGE('',*,*,#20898,.T.);
#29939=ORIENTED_EDGE('',*,*,#20287,.T.);
#29940=ORIENTED_EDGE('',*,*,#20200,.T.);
#29941=ORIENTED_EDGE('',*,*,#20167,.F.);
#29942=ORIENTED_EDGE('',*,*,#20183,.F.);
#29943=ORIENTED_EDGE('',*,*,#20164,.F.);
#29944=ORIENTED_EDGE('',*,*,#20177,.T.);
#29945=ORIENTED_EDGE('',*,*,#20172,.F.);
#29946=ORIENTED_EDGE('',*,*,#20899,.T.);
#29947=ORIENTED_EDGE('',*,*,#20900,.F.);
#29948=ORIENTED_EDGE('',*,*,#20869,.F.);
#29949=ORIENTED_EDGE('',*,*,#20867,.F.);
#29950=ORIENTED_EDGE('',*,*,#20883,.F.);
#29951=ORIENTED_EDGE('',*,*,#20885,.F.);
#29952=ORIENTED_EDGE('',*,*,#20887,.F.);
#29953=ORIENTED_EDGE('',*,*,#20889,.F.);
#29954=ORIENTED_EDGE('',*,*,#20891,.F.);
#29955=ORIENTED_EDGE('',*,*,#20893,.F.);
#29956=ORIENTED_EDGE('',*,*,#20894,.F.);
#29957=ORIENTED_EDGE('',*,*,#20880,.F.);
#29958=ORIENTED_EDGE('',*,*,#20878,.F.);
#29959=ORIENTED_EDGE('',*,*,#20864,.F.);
#29960=ORIENTED_EDGE('',*,*,#20877,.F.);
#29961=ORIENTED_EDGE('',*,*,#20875,.F.);
#29962=ORIENTED_EDGE('',*,*,#20873,.F.);
#29963=ORIENTED_EDGE('',*,*,#20871,.F.);
#29964=ORIENTED_EDGE('',*,*,#20635,.T.);
#29965=ORIENTED_EDGE('',*,*,#20901,.T.);
#29966=ORIENTED_EDGE('',*,*,#20171,.F.);
#29967=ORIENTED_EDGE('',*,*,#20646,.T.);
#29968=ORIENTED_EDGE('',*,*,#20902,.F.);
#29969=ORIENTED_EDGE('',*,*,#20899,.F.);
#29970=ORIENTED_EDGE('',*,*,#20901,.F.);
#29971=ORIENTED_EDGE('',*,*,#20900,.T.);
#29972=ORIENTED_EDGE('',*,*,#20903,.F.);
#29973=ORIENTED_EDGE('',*,*,#20904,.F.);
#29974=ORIENTED_EDGE('',*,*,#20905,.T.);
#29975=ORIENTED_EDGE('',*,*,#20906,.T.);
#29976=ORIENTED_EDGE('',*,*,#20907,.T.);
#29977=ORIENTED_EDGE('',*,*,#20908,.F.);
#29978=ORIENTED_EDGE('',*,*,#20482,.F.);
#29979=ORIENTED_EDGE('',*,*,#20909,.T.);
#29980=ORIENTED_EDGE('',*,*,#20906,.F.);
#29981=ORIENTED_EDGE('',*,*,#20514,.F.);
#29982=ORIENTED_EDGE('',*,*,#20675,.T.);
#29983=ORIENTED_EDGE('',*,*,#20910,.T.);
#29984=ORIENTED_EDGE('',*,*,#20909,.F.);
#29985=ORIENTED_EDGE('',*,*,#20516,.F.);
#29986=ORIENTED_EDGE('',*,*,#20858,.T.);
#29987=ORIENTED_EDGE('',*,*,#20911,.T.);
#29988=ORIENTED_EDGE('',*,*,#20860,.F.);
#29989=ORIENTED_EDGE('',*,*,#20895,.F.);
#29990=ORIENTED_EDGE('',*,*,#20639,.T.);
#29991=ORIENTED_EDGE('',*,*,#20912,.F.);
#29992=ORIENTED_EDGE('',*,*,#20907,.F.);
#29993=ORIENTED_EDGE('',*,*,#20910,.F.);
#29994=ORIENTED_EDGE('',*,*,#20677,.F.);
#29995=ORIENTED_EDGE('',*,*,#20911,.F.);
#29996=ORIENTED_EDGE('',*,*,#20913,.T.);
#29997=ORIENTED_EDGE('',*,*,#20644,.T.);
#29998=ORIENTED_EDGE('',*,*,#20914,.F.);
#29999=ORIENTED_EDGE('',*,*,#20915,.F.);
#30000=ORIENTED_EDGE('',*,*,#20914,.T.);
#30001=ORIENTED_EDGE('',*,*,#20643,.T.);
#30002=ORIENTED_EDGE('',*,*,#20916,.F.);
#30003=ORIENTED_EDGE('',*,*,#20856,.F.);
#30004=ORIENTED_EDGE('',*,*,#20916,.T.);
#30005=ORIENTED_EDGE('',*,*,#20642,.T.);
#30006=ORIENTED_EDGE('',*,*,#20917,.F.);
#30007=ORIENTED_EDGE('',*,*,#20918,.F.);
#30008=ORIENTED_EDGE('',*,*,#20919,.T.);
#30009=ORIENTED_EDGE('',*,*,#20857,.F.);
#30010=ORIENTED_EDGE('',*,*,#20905,.F.);
#30011=ORIENTED_EDGE('',*,*,#20920,.F.);
#30012=ORIENTED_EDGE('',*,*,#20917,.T.);
#30013=ORIENTED_EDGE('',*,*,#20641,.T.);
#30014=ORIENTED_EDGE('',*,*,#20919,.F.);
#30015=ORIENTED_EDGE('',*,*,#20921,.T.);
#30016=ORIENTED_EDGE('',*,*,#20645,.T.);
#30017=ORIENTED_EDGE('',*,*,#20913,.F.);
#30018=ORIENTED_EDGE('',*,*,#20922,.F.);
#30019=ORIENTED_EDGE('',*,*,#20898,.F.);
#30020=ORIENTED_EDGE('',*,*,#20923,.F.);
#30021=ORIENTED_EDGE('',*,*,#20924,.T.);
#30022=ORIENTED_EDGE('',*,*,#20288,.T.);
#30023=ORIENTED_EDGE('',*,*,#20924,.F.);
#30024=ORIENTED_EDGE('',*,*,#20851,.F.);
#30025=ORIENTED_EDGE('',*,*,#20925,.F.);
#30026=ORIENTED_EDGE('',*,*,#20155,.T.);
#30027=ORIENTED_EDGE('',*,*,#20222,.F.);
#30028=ORIENTED_EDGE('',*,*,#20233,.F.);
#30029=ORIENTED_EDGE('',*,*,#20925,.T.);
#30030=ORIENTED_EDGE('',*,*,#20926,.T.);
#30031=ORIENTED_EDGE('',*,*,#20927,.T.);
#30032=ORIENTED_EDGE('',*,*,#20928,.T.);
#30033=ORIENTED_EDGE('',*,*,#20929,.F.);
#30034=ORIENTED_EDGE('',*,*,#20930,.T.);
#30035=ORIENTED_EDGE('',*,*,#20681,.F.);
#30036=ORIENTED_EDGE('',*,*,#20208,.F.);
#30037=ORIENTED_EDGE('',*,*,#20928,.F.);
#30038=ORIENTED_EDGE('',*,*,#20931,.T.);
#30039=ORIENTED_EDGE('',*,*,#20932,.T.);
#30040=ORIENTED_EDGE('',*,*,#20933,.T.);
#30041=ORIENTED_EDGE('',*,*,#20934,.T.);
#30042=ORIENTED_EDGE('',*,*,#20935,.T.);
#30043=ORIENTED_EDGE('',*,*,#20936,.T.);
#30044=ORIENTED_EDGE('',*,*,#20929,.T.);
#30045=ORIENTED_EDGE('',*,*,#20214,.F.);
#30046=ORIENTED_EDGE('',*,*,#20232,.F.);
#30047=ORIENTED_EDGE('',*,*,#20229,.F.);
#30048=ORIENTED_EDGE('',*,*,#20226,.F.);
#30049=ORIENTED_EDGE('',*,*,#20224,.F.);
#30050=ORIENTED_EDGE('',*,*,#20223,.F.);
#30051=ORIENTED_EDGE('',*,*,#20861,.T.);
#30052=ORIENTED_EDGE('',*,*,#20937,.F.);
#30053=ORIENTED_EDGE('',*,*,#20938,.F.);
#30054=ORIENTED_EDGE('',*,*,#20939,.F.);
#30055=ORIENTED_EDGE('',*,*,#20939,.T.);
#30056=ORIENTED_EDGE('',*,*,#20940,.F.);
#30057=ORIENTED_EDGE('',*,*,#20941,.T.);
#30058=ORIENTED_EDGE('',*,*,#20896,.T.);
#30059=ORIENTED_EDGE('',*,*,#20938,.T.);
#30060=ORIENTED_EDGE('',*,*,#20937,.T.);
#30061=ORIENTED_EDGE('',*,*,#20683,.T.);
#30062=ORIENTED_EDGE('',*,*,#20942,.F.);
#30063=ORIENTED_EDGE('',*,*,#20943,.F.);
#30064=ORIENTED_EDGE('',*,*,#20944,.T.);
#30065=ORIENTED_EDGE('',*,*,#20849,.T.);
#30066=ORIENTED_EDGE('',*,*,#20940,.T.);
#30067=ORIENTED_EDGE('',*,*,#20943,.T.);
#30068=ORIENTED_EDGE('',*,*,#20942,.T.);
#30069=ORIENTED_EDGE('',*,*,#20682,.T.);
#30070=ORIENTED_EDGE('',*,*,#20930,.F.);
#30071=ORIENTED_EDGE('',*,*,#20945,.F.);
#30072=ORIENTED_EDGE('',*,*,#20945,.T.);
#30073=ORIENTED_EDGE('',*,*,#20936,.F.);
#30074=ORIENTED_EDGE('',*,*,#20946,.T.);
#30075=ORIENTED_EDGE('',*,*,#20947,.F.);
#30076=ORIENTED_EDGE('',*,*,#20948,.T.);
#30077=ORIENTED_EDGE('',*,*,#20949,.T.);
#30078=ORIENTED_EDGE('',*,*,#20944,.F.);
#30079=ORIENTED_EDGE('',*,*,#20950,.T.);
#30080=ORIENTED_EDGE('',*,*,#20951,.T.);
#30081=ORIENTED_EDGE('',*,*,#20688,.F.);
#30082=ORIENTED_EDGE('',*,*,#20952,.F.);
#30083=ORIENTED_EDGE('',*,*,#20952,.T.);
#30084=ORIENTED_EDGE('',*,*,#20694,.F.);
#30085=ORIENTED_EDGE('',*,*,#20953,.F.);
#30086=ORIENTED_EDGE('',*,*,#20931,.F.);
#30087=ORIENTED_EDGE('',*,*,#20927,.F.);
#30088=ORIENTED_EDGE('',*,*,#20954,.F.);
#30089=ORIENTED_EDGE('',*,*,#20948,.F.);
#30090=ORIENTED_EDGE('',*,*,#20955,.T.);
#30091=ORIENTED_EDGE('',*,*,#20953,.T.);
#30092=ORIENTED_EDGE('',*,*,#20696,.F.);
#30093=ORIENTED_EDGE('',*,*,#20956,.F.);
#30094=ORIENTED_EDGE('',*,*,#20956,.T.);
#30095=ORIENTED_EDGE('',*,*,#20700,.F.);
#30096=ORIENTED_EDGE('',*,*,#20957,.F.);
#30097=ORIENTED_EDGE('',*,*,#20932,.F.);
#30098=ORIENTED_EDGE('',*,*,#20957,.T.);
#30099=ORIENTED_EDGE('',*,*,#20702,.F.);
#30100=ORIENTED_EDGE('',*,*,#20958,.F.);
#30101=ORIENTED_EDGE('',*,*,#20933,.F.);
#30102=ORIENTED_EDGE('',*,*,#20959,.T.);
#30103=ORIENTED_EDGE('',*,*,#20705,.F.);
#30104=ORIENTED_EDGE('',*,*,#20951,.F.);
#30105=ORIENTED_EDGE('',*,*,#20958,.T.);
#30106=ORIENTED_EDGE('',*,*,#20709,.F.);
#30107=ORIENTED_EDGE('',*,*,#20960,.F.);
#30108=ORIENTED_EDGE('',*,*,#20934,.F.);
#30109=ORIENTED_EDGE('',*,*,#20946,.F.);
#30110=ORIENTED_EDGE('',*,*,#20935,.F.);
#30111=ORIENTED_EDGE('',*,*,#20960,.T.);
#30112=ORIENTED_EDGE('',*,*,#20711,.F.);
#30113=ORIENTED_EDGE('',*,*,#20959,.F.);
#30114=ORIENTED_EDGE('',*,*,#20961,.T.);
#30115=ORIENTED_EDGE('',*,*,#20961,.F.);
#30116=ORIENTED_EDGE('',*,*,#20950,.F.);
#30117=ORIENTED_EDGE('',*,*,#20955,.F.);
#30118=ORIENTED_EDGE('',*,*,#20947,.T.);
#30119=ORIENTED_EDGE('',*,*,#20954,.T.);
#30120=ORIENTED_EDGE('',*,*,#20926,.F.);
#30121=ORIENTED_EDGE('',*,*,#20850,.F.);
#30122=ORIENTED_EDGE('',*,*,#20949,.F.);
#30123=ORIENTED_EDGE('',*,*,#20962,.T.);
#30124=ORIENTED_EDGE('',*,*,#20963,.F.);
#30125=ORIENTED_EDGE('',*,*,#20964,.T.);
#30126=ORIENTED_EDGE('',*,*,#20715,.T.);
#30127=ORIENTED_EDGE('',*,*,#20965,.T.);
#30128=ORIENTED_EDGE('',*,*,#20852,.F.);
#30129=ORIENTED_EDGE('',*,*,#20966,.F.);
#30130=ORIENTED_EDGE('',*,*,#20717,.F.);
#30131=ORIENTED_EDGE('',*,*,#20721,.F.);
#30132=ORIENTED_EDGE('',*,*,#20967,.T.);
#30133=ORIENTED_EDGE('',*,*,#20968,.T.);
#30134=ORIENTED_EDGE('',*,*,#20965,.F.);
#30135=ORIENTED_EDGE('',*,*,#20969,.F.);
#30136=ORIENTED_EDGE('',*,*,#20970,.F.);
#30137=ORIENTED_EDGE('',*,*,#20967,.F.);
#30138=ORIENTED_EDGE('',*,*,#20724,.F.);
#30139=ORIENTED_EDGE('',*,*,#20727,.F.);
#30140=ORIENTED_EDGE('',*,*,#20971,.F.);
#30141=ORIENTED_EDGE('',*,*,#20972,.F.);
#30142=ORIENTED_EDGE('',*,*,#20969,.T.);
#30143=ORIENTED_EDGE('',*,*,#20730,.F.);
#30144=ORIENTED_EDGE('',*,*,#20973,.T.);
#30145=ORIENTED_EDGE('',*,*,#20974,.F.);
#30146=ORIENTED_EDGE('',*,*,#20971,.T.);
#30147=ORIENTED_EDGE('',*,*,#20732,.F.);
#30148=ORIENTED_EDGE('',*,*,#20966,.T.);
#30149=ORIENTED_EDGE('',*,*,#20839,.T.);
#30150=ORIENTED_EDGE('',*,*,#20975,.F.);
#30151=ORIENTED_EDGE('',*,*,#20736,.F.);
#30152=ORIENTED_EDGE('',*,*,#20976,.T.);
#30153=ORIENTED_EDGE('',*,*,#20613,.T.);
#30154=ORIENTED_EDGE('',*,*,#20973,.F.);
#30155=ORIENTED_EDGE('',*,*,#20975,.T.);
#30156=ORIENTED_EDGE('',*,*,#20803,.F.);
#30157=ORIENTED_EDGE('',*,*,#20976,.F.);
#30158=ORIENTED_EDGE('',*,*,#20738,.F.);
#30159=ORIENTED_EDGE('',*,*,#20743,.T.);
#30160=ORIENTED_EDGE('',*,*,#20977,.T.);
#30161=ORIENTED_EDGE('',*,*,#20807,.T.);
#30162=ORIENTED_EDGE('',*,*,#20978,.F.);
#30163=ORIENTED_EDGE('',*,*,#20748,.T.);
#30164=ORIENTED_EDGE('',*,*,#20979,.T.);
#30165=ORIENTED_EDGE('',*,*,#20811,.T.);
#30166=ORIENTED_EDGE('',*,*,#20977,.F.);
#30167=ORIENTED_EDGE('',*,*,#20980,.T.);
#30168=ORIENTED_EDGE('',*,*,#20814,.T.);
#30169=ORIENTED_EDGE('',*,*,#20979,.F.);
#30170=ORIENTED_EDGE('',*,*,#20758,.T.);
#30171=ORIENTED_EDGE('',*,*,#20761,.T.);
#30172=ORIENTED_EDGE('',*,*,#20978,.T.);
#30173=ORIENTED_EDGE('',*,*,#20816,.T.);
#30174=ORIENTED_EDGE('',*,*,#20981,.F.);
#30175=ORIENTED_EDGE('',*,*,#20764,.T.);
#30176=ORIENTED_EDGE('',*,*,#20982,.T.);
#30177=ORIENTED_EDGE('',*,*,#20818,.T.);
#30178=ORIENTED_EDGE('',*,*,#20980,.F.);
#30179=ORIENTED_EDGE('',*,*,#20766,.T.);
#30180=ORIENTED_EDGE('',*,*,#20981,.T.);
#30181=ORIENTED_EDGE('',*,*,#20822,.T.);
#30182=ORIENTED_EDGE('',*,*,#20982,.F.);
#30183=ORIENTED_EDGE('',*,*,#20983,.F.);
#30184=ORIENTED_EDGE('',*,*,#20824,.F.);
#30185=ORIENTED_EDGE('',*,*,#20984,.F.);
#30186=ORIENTED_EDGE('',*,*,#20776,.F.);
#30187=ORIENTED_EDGE('',*,*,#20780,.F.);
#30188=ORIENTED_EDGE('',*,*,#20985,.F.);
#30189=ORIENTED_EDGE('',*,*,#20820,.F.);
#30190=ORIENTED_EDGE('',*,*,#20983,.T.);
#30191=ORIENTED_EDGE('',*,*,#20783,.F.);
#30192=ORIENTED_EDGE('',*,*,#20986,.F.);
#30193=ORIENTED_EDGE('',*,*,#20800,.F.);
#30194=ORIENTED_EDGE('',*,*,#20985,.T.);
#30195=ORIENTED_EDGE('',*,*,#20786,.F.);
#30196=ORIENTED_EDGE('',*,*,#20987,.F.);
#30197=ORIENTED_EDGE('',*,*,#20988,.F.);
#30198=ORIENTED_EDGE('',*,*,#20986,.T.);
#30199=ORIENTED_EDGE('',*,*,#20789,.F.);
#30200=ORIENTED_EDGE('',*,*,#20989,.F.);
#30201=ORIENTED_EDGE('',*,*,#20990,.F.);
#30202=ORIENTED_EDGE('',*,*,#20987,.T.);
#30203=ORIENTED_EDGE('',*,*,#20791,.F.);
#30204=ORIENTED_EDGE('',*,*,#20984,.T.);
#30205=ORIENTED_EDGE('',*,*,#20991,.T.);
#30206=ORIENTED_EDGE('',*,*,#20992,.F.);
#30207=ORIENTED_EDGE('',*,*,#20795,.F.);
#30208=ORIENTED_EDGE('',*,*,#20993,.F.);
#30209=ORIENTED_EDGE('',*,*,#20994,.F.);
#30210=ORIENTED_EDGE('',*,*,#20989,.T.);
#30211=ORIENTED_EDGE('',*,*,#20992,.T.);
#30212=ORIENTED_EDGE('',*,*,#20995,.F.);
#30213=ORIENTED_EDGE('',*,*,#20993,.T.);
#30214=ORIENTED_EDGE('',*,*,#20797,.F.);
#30215=ORIENTED_EDGE('',*,*,#20801,.T.);
#30216=ORIENTED_EDGE('',*,*,#20988,.T.);
#30217=ORIENTED_EDGE('',*,*,#20996,.F.);
#30218=ORIENTED_EDGE('',*,*,#20997,.F.);
#30219=ORIENTED_EDGE('',*,*,#20998,.F.);
#30220=ORIENTED_EDGE('',*,*,#20996,.T.);
#30221=ORIENTED_EDGE('',*,*,#20990,.T.);
#30222=ORIENTED_EDGE('',*,*,#20823,.T.);
#30223=ORIENTED_EDGE('',*,*,#20999,.F.);
#30224=ORIENTED_EDGE('',*,*,#20991,.F.);
#30225=ORIENTED_EDGE('',*,*,#20997,.T.);
#30226=ORIENTED_EDGE('',*,*,#20994,.T.);
#30227=ORIENTED_EDGE('',*,*,#21000,.F.);
#30228=ORIENTED_EDGE('',*,*,#20999,.T.);
#30229=ORIENTED_EDGE('',*,*,#21001,.F.);
#30230=ORIENTED_EDGE('',*,*,#21000,.T.);
#30231=ORIENTED_EDGE('',*,*,#20995,.T.);
#30232=ORIENTED_EDGE('',*,*,#21002,.T.);
#30233=ORIENTED_EDGE('',*,*,#20805,.T.);
#30234=ORIENTED_EDGE('',*,*,#20854,.T.);
#30235=ORIENTED_EDGE('',*,*,#21003,.T.);
#30236=ORIENTED_EDGE('',*,*,#20903,.T.);
#30237=ORIENTED_EDGE('',*,*,#20902,.T.);
#30238=ORIENTED_EDGE('',*,*,#20921,.F.);
#30239=ORIENTED_EDGE('',*,*,#21004,.T.);
#30240=ORIENTED_EDGE('',*,*,#21005,.F.);
#30241=ORIENTED_EDGE('',*,*,#21006,.F.);
#30242=ORIENTED_EDGE('',*,*,#20821,.F.);
#30243=ORIENTED_EDGE('',*,*,#20809,.F.);
#30244=ORIENTED_EDGE('',*,*,#20813,.F.);
#30245=ORIENTED_EDGE('',*,*,#21001,.T.);
#30246=ORIENTED_EDGE('',*,*,#20825,.T.);
#30247=ORIENTED_EDGE('',*,*,#20802,.T.);
#30248=ORIENTED_EDGE('',*,*,#20998,.T.);
#30249=ORIENTED_EDGE('',*,*,#20828,.T.);
#30250=ORIENTED_EDGE('',*,*,#21007,.T.);
#30251=ORIENTED_EDGE('',*,*,#21006,.T.);
#30252=ORIENTED_EDGE('',*,*,#20962,.F.);
#30253=ORIENTED_EDGE('',*,*,#20904,.T.);
#30254=ORIENTED_EDGE('',*,*,#20922,.T.);
#30255=ORIENTED_EDGE('',*,*,#21008,.T.);
#30256=ORIENTED_EDGE('',*,*,#20920,.T.);
#30257=ORIENTED_EDGE('',*,*,#21009,.T.);
#30258=ORIENTED_EDGE('',*,*,#20853,.F.);
#30259=ORIENTED_EDGE('',*,*,#20968,.F.);
#30260=ORIENTED_EDGE('',*,*,#20612,.T.);
#30261=ORIENTED_EDGE('',*,*,#21002,.F.);
#30262=ORIENTED_EDGE('',*,*,#21010,.T.);
#30263=ORIENTED_EDGE('',*,*,#20974,.T.);
#30264=ORIENTED_EDGE('',*,*,#20964,.F.);
#30265=ORIENTED_EDGE('',*,*,#21011,.T.);
#30266=ORIENTED_EDGE('',*,*,#20842,.T.);
#30267=ORIENTED_EDGE('',*,*,#20844,.T.);
#30268=ORIENTED_EDGE('',*,*,#20846,.T.);
#30269=ORIENTED_EDGE('',*,*,#21011,.F.);
#30270=ORIENTED_EDGE('',*,*,#21012,.F.);
#30271=ORIENTED_EDGE('',*,*,#21013,.F.);
#30272=ORIENTED_EDGE('',*,*,#21003,.F.);
#30273=ORIENTED_EDGE('',*,*,#21009,.F.);
#30274=ORIENTED_EDGE('',*,*,#20970,.T.);
#30275=ORIENTED_EDGE('',*,*,#21005,.T.);
#30276=ORIENTED_EDGE('',*,*,#21014,.F.);
#30277=ORIENTED_EDGE('',*,*,#21012,.T.);
#30278=ORIENTED_EDGE('',*,*,#20963,.T.);
#30279=ORIENTED_EDGE('',*,*,#21013,.T.);
#30280=ORIENTED_EDGE('',*,*,#20972,.T.);
#30281=ORIENTED_EDGE('',*,*,#21010,.F.);
#30282=ORIENTED_EDGE('',*,*,#20855,.T.);
#30283=ORIENTED_EDGE('',*,*,#20918,.T.);
#30284=ORIENTED_EDGE('',*,*,#21008,.F.);
#30285=ORIENTED_EDGE('',*,*,#20915,.T.);
#30286=ORIENTED_EDGE('',*,*,#20923,.T.);
#30287=ORIENTED_EDGE('',*,*,#20897,.T.);
#30288=ORIENTED_EDGE('',*,*,#20941,.F.);
#30289=ORIENTED_EDGE('',*,*,#20848,.F.);
#30290=ORIENTED_EDGE('',*,*,#21015,.T.);
#30291=ORIENTED_EDGE('',*,*,#21016,.F.);
#30292=ORIENTED_EDGE('',*,*,#21017,.F.);
#30293=ORIENTED_EDGE('',*,*,#20837,.T.);
#30294=ORIENTED_EDGE('',*,*,#21018,.T.);
#30295=ORIENTED_EDGE('',*,*,#21017,.T.);
#30296=ORIENTED_EDGE('',*,*,#21019,.F.);
#30297=ORIENTED_EDGE('',*,*,#21019,.T.);
#30298=ORIENTED_EDGE('',*,*,#21020,.F.);
#30299=ORIENTED_EDGE('',*,*,#21007,.F.);
#30300=ORIENTED_EDGE('',*,*,#20831,.T.);
#30301=ORIENTED_EDGE('',*,*,#21016,.T.);
#30302=ORIENTED_EDGE('',*,*,#21021,.F.);
#30303=ORIENTED_EDGE('',*,*,#21004,.F.);
#30304=ORIENTED_EDGE('',*,*,#21020,.T.);
#30305=ORIENTED_EDGE('',*,*,#21022,.T.);
#30306=ORIENTED_EDGE('',*,*,#21023,.T.);
#30307=ORIENTED_EDGE('',*,*,#20517,.F.);
#30308=ORIENTED_EDGE('',*,*,#21024,.F.);
#30309=ORIENTED_EDGE('',*,*,#21025,.T.);
#30310=ORIENTED_EDGE('',*,*,#21024,.T.);
#30311=ORIENTED_EDGE('',*,*,#20526,.F.);
#30312=ORIENTED_EDGE('',*,*,#21026,.F.);
#30313=ORIENTED_EDGE('',*,*,#21027,.T.);
#30314=ORIENTED_EDGE('',*,*,#21026,.T.);
#30315=ORIENTED_EDGE('',*,*,#20527,.F.);
#30316=ORIENTED_EDGE('',*,*,#21028,.F.);
#30317=ORIENTED_EDGE('',*,*,#21029,.T.);
#30318=ORIENTED_EDGE('',*,*,#21028,.T.);
#30319=ORIENTED_EDGE('',*,*,#20532,.F.);
#30320=ORIENTED_EDGE('',*,*,#21030,.F.);
#30321=ORIENTED_EDGE('',*,*,#21031,.T.);
#30322=ORIENTED_EDGE('',*,*,#21030,.T.);
#30323=ORIENTED_EDGE('',*,*,#20535,.F.);
#30324=ORIENTED_EDGE('',*,*,#21032,.F.);
#30325=ORIENTED_EDGE('',*,*,#21022,.F.);
#30326=ORIENTED_EDGE('',*,*,#21025,.F.);
#30327=ORIENTED_EDGE('',*,*,#21027,.F.);
#30328=ORIENTED_EDGE('',*,*,#21029,.F.);
#30329=ORIENTED_EDGE('',*,*,#21031,.F.);
#30330=ORIENTED_EDGE('',*,*,#21033,.F.);
#30331=ORIENTED_EDGE('',*,*,#20315,.T.);
#30332=ORIENTED_EDGE('',*,*,#20306,.T.);
#30333=ORIENTED_EDGE('',*,*,#20304,.T.);
#30334=ORIENTED_EDGE('',*,*,#20302,.T.);
#30335=ORIENTED_EDGE('',*,*,#20300,.T.);
#30336=ORIENTED_EDGE('',*,*,#20298,.T.);
#30337=ORIENTED_EDGE('',*,*,#20312,.T.);
#30338=ORIENTED_EDGE('',*,*,#20324,.F.);
#30339=ORIENTED_EDGE('',*,*,#20295,.F.);
#30340=ORIENTED_EDGE('',*,*,#20286,.F.);
#30341=ORIENTED_EDGE('',*,*,#20152,.F.);
#30342=ORIENTED_EDGE('',*,*,#20847,.T.);
#30343=ORIENTED_EDGE('',*,*,#21014,.T.);
#30344=ORIENTED_EDGE('',*,*,#21021,.T.);
#30345=ORIENTED_EDGE('',*,*,#21034,.T.);
#30346=ORIENTED_EDGE('',*,*,#21035,.F.);
#30347=ORIENTED_EDGE('',*,*,#21036,.T.);
#30348=ORIENTED_EDGE('',*,*,#21037,.T.);
#30349=ORIENTED_EDGE('',*,*,#21023,.F.);
#30350=ORIENTED_EDGE('',*,*,#21038,.T.);
#30351=ORIENTED_EDGE('',*,*,#21038,.F.);
#30352=ORIENTED_EDGE('',*,*,#21036,.F.);
#30353=ORIENTED_EDGE('',*,*,#21035,.T.);
#30354=ORIENTED_EDGE('',*,*,#21039,.T.);
#30355=ORIENTED_EDGE('',*,*,#21040,.F.);
#30356=ORIENTED_EDGE('',*,*,#21041,.T.);
#30357=ORIENTED_EDGE('',*,*,#21032,.T.);
#30358=ORIENTED_EDGE('',*,*,#20536,.F.);
#30359=ORIENTED_EDGE('',*,*,#20316,.T.);
#30360=ORIENTED_EDGE('',*,*,#21042,.F.);
#30361=ORIENTED_EDGE('',*,*,#21043,.F.);
#30362=ORIENTED_EDGE('',*,*,#21042,.T.);
#30363=ORIENTED_EDGE('',*,*,#21033,.T.);
#30364=ORIENTED_EDGE('',*,*,#21041,.F.);
#30365=ORIENTED_EDGE('',*,*,#21044,.F.);
#30366=ORIENTED_EDGE('',*,*,#21045,.T.);
#30367=ORIENTED_EDGE('',*,*,#20624,.T.);
#30368=ORIENTED_EDGE('',*,*,#20518,.F.);
#30369=ORIENTED_EDGE('',*,*,#21037,.F.);
#30370=ORIENTED_EDGE('',*,*,#21045,.F.);
#30371=ORIENTED_EDGE('',*,*,#21040,.T.);
#30372=ORIENTED_EDGE('',*,*,#21046,.T.);
#30373=ORIENTED_EDGE('',*,*,#20625,.T.);
#30374=ORIENTED_EDGE('',*,*,#20319,.T.);
#30375=ORIENTED_EDGE('',*,*,#21043,.T.);
#30376=ORIENTED_EDGE('',*,*,#21047,.F.);
#30377=ORIENTED_EDGE('',*,*,#20553,.F.);
#30378=ORIENTED_EDGE('',*,*,#21047,.T.);
#30379=ORIENTED_EDGE('',*,*,#21044,.T.);
#30380=ORIENTED_EDGE('',*,*,#20538,.F.);
#30381=ORIENTED_EDGE('',*,*,#20555,.F.);
#30382=ORIENTED_EDGE('',*,*,#20834,.T.);
#30383=ORIENTED_EDGE('',*,*,#21046,.F.);
#30384=ORIENTED_EDGE('',*,*,#21048,.F.);
#30385=ORIENTED_EDGE('',*,*,#21049,.T.);
#30386=ORIENTED_EDGE('',*,*,#21050,.T.);
#30387=ORIENTED_EDGE('',*,*,#21048,.T.);
#30388=ORIENTED_EDGE('',*,*,#21039,.F.);
#30389=ORIENTED_EDGE('',*,*,#21050,.F.);
#30390=ORIENTED_EDGE('',*,*,#21034,.F.);
#30391=ORIENTED_EDGE('',*,*,#21015,.F.);
#30392=ORIENTED_EDGE('',*,*,#21051,.T.);
#30393=ORIENTED_EDGE('',*,*,#21052,.T.);
#30394=ORIENTED_EDGE('',*,*,#21049,.F.);
#30395=ORIENTED_EDGE('',*,*,#21051,.F.);
#30396=ORIENTED_EDGE('',*,*,#21018,.F.);
#30397=ORIENTED_EDGE('',*,*,#20836,.T.);
#30398=ORIENTED_EDGE('',*,*,#21053,.T.);
#30399=ORIENTED_EDGE('',*,*,#20832,.F.);
#30400=ORIENTED_EDGE('',*,*,#21052,.F.);
#30401=ORIENTED_EDGE('',*,*,#21054,.T.);
#30402=ORIENTED_EDGE('',*,*,#20449,.F.);
#30403=ORIENTED_EDGE('',*,*,#21055,.F.);
#30404=ORIENTED_EDGE('',*,*,#21056,.T.);
#30405=ORIENTED_EDGE('',*,*,#21057,.F.);
#30406=ORIENTED_EDGE('',*,*,#20686,.F.);
#30407=ORIENTED_EDGE('',*,*,#21054,.F.);
#30408=ORIENTED_EDGE('',*,*,#21057,.T.);
#30409=ORIENTED_EDGE('',*,*,#21058,.T.);
#30410=ORIENTED_EDGE('',*,*,#21059,.F.);
#30411=ORIENTED_EDGE('',*,*,#20692,.F.);
#30412=ORIENTED_EDGE('',*,*,#21059,.T.);
#30413=ORIENTED_EDGE('',*,*,#21060,.T.);
#30414=ORIENTED_EDGE('',*,*,#21061,.F.);
#30415=ORIENTED_EDGE('',*,*,#20697,.F.);
#30416=ORIENTED_EDGE('',*,*,#21061,.T.);
#30417=ORIENTED_EDGE('',*,*,#21062,.T.);
#30418=ORIENTED_EDGE('',*,*,#21063,.F.);
#30419=ORIENTED_EDGE('',*,*,#20698,.F.);
#30420=ORIENTED_EDGE('',*,*,#21063,.T.);
#30421=ORIENTED_EDGE('',*,*,#21064,.T.);
#30422=ORIENTED_EDGE('',*,*,#21065,.F.);
#30423=ORIENTED_EDGE('',*,*,#20703,.F.);
#30424=ORIENTED_EDGE('',*,*,#20690,.F.);
#30425=ORIENTED_EDGE('',*,*,#20704,.F.);
#30426=ORIENTED_EDGE('',*,*,#21066,.T.);
#30427=ORIENTED_EDGE('',*,*,#21067,.T.);
#30428=ORIENTED_EDGE('',*,*,#21068,.T.);
#30429=ORIENTED_EDGE('',*,*,#21069,.T.);
#30430=ORIENTED_EDGE('',*,*,#21066,.F.);
#30431=ORIENTED_EDGE('',*,*,#21065,.T.);
#30432=ORIENTED_EDGE('',*,*,#21070,.T.);
#30433=ORIENTED_EDGE('',*,*,#21071,.F.);
#30434=ORIENTED_EDGE('',*,*,#20707,.F.);
#30435=ORIENTED_EDGE('',*,*,#21071,.T.);
#30436=ORIENTED_EDGE('',*,*,#21072,.T.);
#30437=ORIENTED_EDGE('',*,*,#21068,.F.);
#30438=ORIENTED_EDGE('',*,*,#20710,.F.);
#30439=ORIENTED_EDGE('',*,*,#21073,.T.);
#30440=ORIENTED_EDGE('',*,*,#21055,.T.);
#30441=ORIENTED_EDGE('',*,*,#20448,.F.);
#30442=ORIENTED_EDGE('',*,*,#21074,.F.);
#30443=ORIENTED_EDGE('',*,*,#21075,.T.);
#30444=ORIENTED_EDGE('',*,*,#21074,.T.);
#30445=ORIENTED_EDGE('',*,*,#20451,.F.);
#30446=ORIENTED_EDGE('',*,*,#21076,.F.);
#30447=ORIENTED_EDGE('',*,*,#21077,.T.);
#30448=ORIENTED_EDGE('',*,*,#20638,.T.);
#30449=ORIENTED_EDGE('',*,*,#21078,.F.);
#30450=ORIENTED_EDGE('',*,*,#21079,.F.);
#30451=ORIENTED_EDGE('',*,*,#20908,.T.);
#30452=ORIENTED_EDGE('',*,*,#20912,.T.);
#30453=ORIENTED_EDGE('',*,*,#21077,.F.);
#30454=ORIENTED_EDGE('',*,*,#21080,.F.);
#30455=ORIENTED_EDGE('',*,*,#21080,.T.);
#30456=ORIENTED_EDGE('',*,*,#21079,.T.);
#30457=ORIENTED_EDGE('',*,*,#21081,.F.);
#30458=ORIENTED_EDGE('',*,*,#21082,.F.);
#30459=ORIENTED_EDGE('',*,*,#20479,.T.);
#30460=ORIENTED_EDGE('',*,*,#21083,.T.);
#30461=ORIENTED_EDGE('',*,*,#20636,.T.);
#30462=ORIENTED_EDGE('',*,*,#20541,.T.);
#30463=ORIENTED_EDGE('',*,*,#21084,.F.);
#30464=ORIENTED_EDGE('',*,*,#21084,.T.);
#30465=ORIENTED_EDGE('',*,*,#20520,.F.);
#30466=ORIENTED_EDGE('',*,*,#20623,.F.);
#30467=ORIENTED_EDGE('',*,*,#21085,.T.);
#30468=ORIENTED_EDGE('',*,*,#21086,.T.);
#30469=ORIENTED_EDGE('',*,*,#20679,.T.);
#30470=ORIENTED_EDGE('',*,*,#20684,.F.);
#30471=ORIENTED_EDGE('',*,*,#21087,.F.);
#30472=ORIENTED_EDGE('',*,*,#21087,.T.);
#30473=ORIENTED_EDGE('',*,*,#20691,.F.);
#30474=ORIENTED_EDGE('',*,*,#21067,.F.);
#30475=ORIENTED_EDGE('',*,*,#21088,.T.);
#30476=ORIENTED_EDGE('',*,*,#21078,.T.);
#30477=ORIENTED_EDGE('',*,*,#20637,.T.);
#30478=ORIENTED_EDGE('',*,*,#21083,.F.);
#30479=ORIENTED_EDGE('',*,*,#21089,.F.);
#30480=ORIENTED_EDGE('',*,*,#20680,.F.);
#30481=ORIENTED_EDGE('',*,*,#21086,.F.);
#30482=ORIENTED_EDGE('',*,*,#21090,.T.);
#30483=ORIENTED_EDGE('',*,*,#20361,.T.);
#30484=ORIENTED_EDGE('',*,*,#21091,.T.);
#30485=ORIENTED_EDGE('',*,*,#21092,.T.);
#30486=ORIENTED_EDGE('',*,*,#21093,.F.);
#30487=ORIENTED_EDGE('',*,*,#19950,.F.);
#30488=ORIENTED_EDGE('',*,*,#20077,.T.);
#30489=ORIENTED_EDGE('',*,*,#21094,.T.);
#30490=ORIENTED_EDGE('',*,*,#21095,.F.);
#30491=ORIENTED_EDGE('',*,*,#19967,.F.);
#30492=ORIENTED_EDGE('',*,*,#20060,.T.);
#30493=ORIENTED_EDGE('',*,*,#21096,.T.);
#30494=ORIENTED_EDGE('',*,*,#20080,.F.);
#30495=ORIENTED_EDGE('',*,*,#19975,.F.);
#30496=ORIENTED_EDGE('',*,*,#21097,.T.);
#30497=ORIENTED_EDGE('',*,*,#21098,.T.);
#30498=ORIENTED_EDGE('',*,*,#20052,.F.);
#30499=ORIENTED_EDGE('',*,*,#19982,.F.);
#30500=ORIENTED_EDGE('',*,*,#21093,.T.);
#30501=ORIENTED_EDGE('',*,*,#21099,.T.);
#30502=ORIENTED_EDGE('',*,*,#21097,.F.);
#30503=ORIENTED_EDGE('',*,*,#19986,.F.);
#30504=ORIENTED_EDGE('',*,*,#21100,.T.);
#30505=ORIENTED_EDGE('',*,*,#21101,.T.);
#30506=ORIENTED_EDGE('',*,*,#21091,.F.);
#30507=ORIENTED_EDGE('',*,*,#20630,.F.);
#30508=ORIENTED_EDGE('',*,*,#21102,.T.);
#30509=ORIENTED_EDGE('',*,*,#21103,.T.);
#30510=ORIENTED_EDGE('',*,*,#21100,.F.);
#30511=ORIENTED_EDGE('',*,*,#20632,.F.);
#30512=ORIENTED_EDGE('',*,*,#21095,.T.);
#30513=ORIENTED_EDGE('',*,*,#21104,.T.);
#30514=ORIENTED_EDGE('',*,*,#21105,.F.);
#30515=ORIENTED_EDGE('',*,*,#20648,.F.);
#30516=ORIENTED_EDGE('',*,*,#21105,.T.);
#30517=ORIENTED_EDGE('',*,*,#21106,.T.);
#30518=ORIENTED_EDGE('',*,*,#20767,.F.);
#30519=ORIENTED_EDGE('',*,*,#20650,.F.);
#30520=ORIENTED_EDGE('',*,*,#20773,.T.);
#30521=ORIENTED_EDGE('',*,*,#21107,.T.);
#30522=ORIENTED_EDGE('',*,*,#20750,.F.);
#30523=ORIENTED_EDGE('',*,*,#20658,.F.);
#30524=ORIENTED_EDGE('',*,*,#20746,.T.);
#30525=ORIENTED_EDGE('',*,*,#21108,.T.);
#30526=ORIENTED_EDGE('',*,*,#21109,.F.);
#30527=ORIENTED_EDGE('',*,*,#20667,.F.);
#30528=ORIENTED_EDGE('',*,*,#21109,.T.);
#30529=ORIENTED_EDGE('',*,*,#21110,.T.);
#30530=ORIENTED_EDGE('',*,*,#21102,.F.);
#30531=ORIENTED_EDGE('',*,*,#20671,.F.);
#30532=ORIENTED_EDGE('',*,*,#21085,.F.);
#30533=ORIENTED_EDGE('',*,*,#20627,.F.);
#30534=ORIENTED_EDGE('',*,*,#20833,.F.);
#30535=ORIENTED_EDGE('',*,*,#21053,.F.);
#30536=ORIENTED_EDGE('',*,*,#20835,.F.);
#30537=ORIENTED_EDGE('',*,*,#20829,.F.);
#30538=ORIENTED_EDGE('',*,*,#20826,.F.);
#30539=ORIENTED_EDGE('',*,*,#20713,.F.);
#30540=ORIENTED_EDGE('',*,*,#20619,.T.);
#30541=ORIENTED_EDGE('',*,*,#19941,.F.);
#30542=ORIENTED_EDGE('',*,*,#20022,.T.);
#30543=ORIENTED_EDGE('',*,*,#20136,.T.);
#30544=ORIENTED_EDGE('',*,*,#20139,.T.);
#30545=ORIENTED_EDGE('',*,*,#20145,.T.);
#30546=ORIENTED_EDGE('',*,*,#20326,.T.);
#30547=ORIENTED_EDGE('',*,*,#20141,.T.);
#30548=ORIENTED_EDGE('',*,*,#19945,.T.);
#30549=ORIENTED_EDGE('',*,*,#20358,.T.);
#30550=ORIENTED_EDGE('',*,*,#20363,.F.);
#30551=ORIENTED_EDGE('',*,*,#20355,.F.);
#30552=ORIENTED_EDGE('',*,*,#20373,.T.);
#30553=ORIENTED_EDGE('',*,*,#20376,.T.);
#30554=ORIENTED_EDGE('',*,*,#20379,.T.);
#30555=ORIENTED_EDGE('',*,*,#20382,.T.);
#30556=ORIENTED_EDGE('',*,*,#20385,.T.);
#30557=ORIENTED_EDGE('',*,*,#20388,.T.);
#30558=ORIENTED_EDGE('',*,*,#20392,.T.);
#30559=ORIENTED_EDGE('',*,*,#20349,.T.);
#30560=ORIENTED_EDGE('',*,*,#20347,.T.);
#30561=ORIENTED_EDGE('',*,*,#20330,.T.);
#30562=ORIENTED_EDGE('',*,*,#20332,.T.);
#30563=ORIENTED_EDGE('',*,*,#20334,.T.);
#30564=ORIENTED_EDGE('',*,*,#20336,.T.);
#30565=ORIENTED_EDGE('',*,*,#20338,.T.);
#30566=ORIENTED_EDGE('',*,*,#20344,.T.);
#30567=ORIENTED_EDGE('',*,*,#20345,.T.);
#30568=ORIENTED_EDGE('',*,*,#20341,.T.);
#30569=ORIENTED_EDGE('',*,*,#20362,.T.);
#30570=ORIENTED_EDGE('',*,*,#21090,.F.);
#30571=ORIENTED_EDGE('',*,*,#21088,.F.);
#30572=ORIENTED_EDGE('',*,*,#21069,.F.);
#30573=ORIENTED_EDGE('',*,*,#21072,.F.);
#30574=ORIENTED_EDGE('',*,*,#21070,.F.);
#30575=ORIENTED_EDGE('',*,*,#21064,.F.);
#30576=ORIENTED_EDGE('',*,*,#21062,.F.);
#30577=ORIENTED_EDGE('',*,*,#21060,.F.);
#30578=ORIENTED_EDGE('',*,*,#21058,.F.);
#30579=ORIENTED_EDGE('',*,*,#21056,.F.);
#30580=ORIENTED_EDGE('',*,*,#21073,.F.);
#30581=ORIENTED_EDGE('',*,*,#21075,.F.);
#30582=ORIENTED_EDGE('',*,*,#21111,.F.);
#30583=ORIENTED_EDGE('',*,*,#21112,.F.);
#30584=ORIENTED_EDGE('',*,*,#21113,.F.);
#30585=ORIENTED_EDGE('',*,*,#21114,.F.);
#30586=ORIENTED_EDGE('',*,*,#21115,.F.);
#30587=ORIENTED_EDGE('',*,*,#21116,.F.);
#30588=ORIENTED_EDGE('',*,*,#21117,.F.);
#30589=ORIENTED_EDGE('',*,*,#21081,.T.);
#30590=ORIENTED_EDGE('',*,*,#21089,.T.);
#30591=ORIENTED_EDGE('',*,*,#20034,.F.);
#30592=ORIENTED_EDGE('',*,*,#20037,.F.);
#30593=ORIENTED_EDGE('',*,*,#20043,.F.);
#30594=ORIENTED_EDGE('',*,*,#20046,.F.);
#30595=ORIENTED_EDGE('',*,*,#20040,.F.);
#30596=ORIENTED_EDGE('',*,*,#20024,.F.);
#30597=ORIENTED_EDGE('',*,*,#20028,.F.);
#30598=ORIENTED_EDGE('',*,*,#20031,.F.);
#30599=ORIENTED_EDGE('',*,*,#20739,.T.);
#30600=ORIENTED_EDGE('',*,*,#20737,.T.);
#30601=ORIENTED_EDGE('',*,*,#20731,.T.);
#30602=ORIENTED_EDGE('',*,*,#20728,.T.);
#30603=ORIENTED_EDGE('',*,*,#20725,.T.);
#30604=ORIENTED_EDGE('',*,*,#20722,.T.);
#30605=ORIENTED_EDGE('',*,*,#20719,.T.);
#30606=ORIENTED_EDGE('',*,*,#20734,.T.);
#30607=ORIENTED_EDGE('',*,*,#20614,.F.);
#30608=ORIENTED_EDGE('',*,*,#20596,.F.);
#30609=ORIENTED_EDGE('',*,*,#20610,.F.);
#30610=ORIENTED_EDGE('',*,*,#20608,.F.);
#30611=ORIENTED_EDGE('',*,*,#20616,.F.);
#30612=ORIENTED_EDGE('',*,*,#20604,.F.);
#30613=ORIENTED_EDGE('',*,*,#20615,.F.);
#30614=ORIENTED_EDGE('',*,*,#20600,.F.);
#30615=ORIENTED_EDGE('',*,*,#21107,.F.);
#30616=ORIENTED_EDGE('',*,*,#20778,.T.);
#30617=ORIENTED_EDGE('',*,*,#20793,.T.);
#30618=ORIENTED_EDGE('',*,*,#20798,.T.);
#30619=ORIENTED_EDGE('',*,*,#20796,.T.);
#30620=ORIENTED_EDGE('',*,*,#20790,.T.);
#30621=ORIENTED_EDGE('',*,*,#20787,.T.);
#30622=ORIENTED_EDGE('',*,*,#20784,.T.);
#30623=ORIENTED_EDGE('',*,*,#20781,.T.);
#30624=ORIENTED_EDGE('',*,*,#20774,.T.);
#30625=ORIENTED_EDGE('',*,*,#21106,.F.);
#30626=ORIENTED_EDGE('',*,*,#21104,.F.);
#30627=ORIENTED_EDGE('',*,*,#21094,.F.);
#30628=ORIENTED_EDGE('',*,*,#20086,.F.);
#30629=ORIENTED_EDGE('',*,*,#20087,.F.);
#30630=ORIENTED_EDGE('',*,*,#20090,.F.);
#30631=ORIENTED_EDGE('',*,*,#20093,.F.);
#30632=ORIENTED_EDGE('',*,*,#20096,.F.);
#30633=ORIENTED_EDGE('',*,*,#20102,.F.);
#30634=ORIENTED_EDGE('',*,*,#20105,.F.);
#30635=ORIENTED_EDGE('',*,*,#20099,.F.);
#30636=ORIENTED_EDGE('',*,*,#20082,.F.);
#30637=ORIENTED_EDGE('',*,*,#21096,.F.);
#30638=ORIENTED_EDGE('',*,*,#20066,.T.);
#30639=ORIENTED_EDGE('',*,*,#20072,.T.);
#30640=ORIENTED_EDGE('',*,*,#20074,.T.);
#30641=ORIENTED_EDGE('',*,*,#20068,.T.);
#30642=ORIENTED_EDGE('',*,*,#20050,.T.);
#30643=ORIENTED_EDGE('',*,*,#20055,.T.);
#30644=ORIENTED_EDGE('',*,*,#21098,.F.);
#30645=ORIENTED_EDGE('',*,*,#21099,.F.);
#30646=ORIENTED_EDGE('',*,*,#21092,.F.);
#30647=ORIENTED_EDGE('',*,*,#21101,.F.);
#30648=ORIENTED_EDGE('',*,*,#21103,.F.);
#30649=ORIENTED_EDGE('',*,*,#21110,.F.);
#30650=ORIENTED_EDGE('',*,*,#21108,.F.);
#30651=ORIENTED_EDGE('',*,*,#20749,.F.);
#30652=ORIENTED_EDGE('',*,*,#20741,.F.);
#30653=ORIENTED_EDGE('',*,*,#20760,.F.);
#30654=ORIENTED_EDGE('',*,*,#20765,.F.);
#30655=ORIENTED_EDGE('',*,*,#20762,.F.);
#30656=ORIENTED_EDGE('',*,*,#20756,.F.);
#30657=ORIENTED_EDGE('',*,*,#19931,.T.);
#30658=ORIENTED_EDGE('',*,*,#19917,.T.);
#30659=ORIENTED_EDGE('',*,*,#19935,.T.);
#30660=ORIENTED_EDGE('',*,*,#19921,.T.);
#30661=ORIENTED_EDGE('',*,*,#19936,.T.);
#30662=ORIENTED_EDGE('',*,*,#19925,.T.);
#30663=ORIENTED_EDGE('',*,*,#19937,.T.);
#30664=ORIENTED_EDGE('',*,*,#19929,.T.);
#30665=ORIENTED_EDGE('',*,*,#21118,.F.);
#30666=ORIENTED_EDGE('',*,*,#21119,.T.);
#30667=ORIENTED_EDGE('',*,*,#20457,.T.);
#30668=ORIENTED_EDGE('',*,*,#21120,.F.);
#30669=ORIENTED_EDGE('',*,*,#20476,.T.);
#30670=ORIENTED_EDGE('',*,*,#21121,.T.);
#30671=ORIENTED_EDGE('',*,*,#21122,.F.);
#30672=ORIENTED_EDGE('',*,*,#21123,.F.);
#30673=ORIENTED_EDGE('',*,*,#20480,.T.);
#30674=ORIENTED_EDGE('',*,*,#21082,.T.);
#30675=ORIENTED_EDGE('',*,*,#21124,.F.);
#30676=ORIENTED_EDGE('',*,*,#21121,.F.);
#30677=ORIENTED_EDGE('',*,*,#21117,.T.);
#30678=ORIENTED_EDGE('',*,*,#21125,.F.);
#30679=ORIENTED_EDGE('',*,*,#21126,.F.);
#30680=ORIENTED_EDGE('',*,*,#21122,.T.);
#30681=ORIENTED_EDGE('',*,*,#21124,.T.);
#30682=ORIENTED_EDGE('',*,*,#21125,.T.);
#30683=ORIENTED_EDGE('',*,*,#21116,.T.);
#30684=ORIENTED_EDGE('',*,*,#21127,.F.);
#30685=ORIENTED_EDGE('',*,*,#21128,.F.);
#30686=ORIENTED_EDGE('',*,*,#21127,.T.);
#30687=ORIENTED_EDGE('',*,*,#21115,.T.);
#30688=ORIENTED_EDGE('',*,*,#21129,.F.);
#30689=ORIENTED_EDGE('',*,*,#21130,.F.);
#30690=ORIENTED_EDGE('',*,*,#21129,.T.);
#30691=ORIENTED_EDGE('',*,*,#21114,.T.);
#30692=ORIENTED_EDGE('',*,*,#21131,.F.);
#30693=ORIENTED_EDGE('',*,*,#21132,.F.);
#30694=ORIENTED_EDGE('',*,*,#21131,.T.);
#30695=ORIENTED_EDGE('',*,*,#21113,.T.);
#30696=ORIENTED_EDGE('',*,*,#21133,.F.);
#30697=ORIENTED_EDGE('',*,*,#21134,.F.);
#30698=ORIENTED_EDGE('',*,*,#21133,.T.);
#30699=ORIENTED_EDGE('',*,*,#21112,.T.);
#30700=ORIENTED_EDGE('',*,*,#21135,.F.);
#30701=ORIENTED_EDGE('',*,*,#21136,.F.);
#30702=ORIENTED_EDGE('',*,*,#21137,.T.);
#30703=ORIENTED_EDGE('',*,*,#21076,.T.);
#30704=ORIENTED_EDGE('',*,*,#20450,.F.);
#30705=ORIENTED_EDGE('',*,*,#21138,.F.);
#30706=ORIENTED_EDGE('',*,*,#21139,.T.);
#30707=ORIENTED_EDGE('',*,*,#21138,.T.);
#30708=ORIENTED_EDGE('',*,*,#20456,.F.);
#30709=ORIENTED_EDGE('',*,*,#21140,.F.);
#30710=ORIENTED_EDGE('',*,*,#21135,.T.);
#30711=ORIENTED_EDGE('',*,*,#21111,.T.);
#30712=ORIENTED_EDGE('',*,*,#21137,.F.);
#30713=ORIENTED_EDGE('',*,*,#21139,.F.);
#30714=ORIENTED_EDGE('',*,*,#21119,.F.);
#30715=ORIENTED_EDGE('',*,*,#21141,.F.);
#30716=ORIENTED_EDGE('',*,*,#21142,.F.);
#30717=ORIENTED_EDGE('',*,*,#21143,.F.);
#30718=ORIENTED_EDGE('',*,*,#20498,.F.);
#30719=ORIENTED_EDGE('',*,*,#20458,.T.);
#30720=ORIENTED_EDGE('',*,*,#21118,.T.);
#30721=ORIENTED_EDGE('',*,*,#21144,.F.);
#30722=ORIENTED_EDGE('',*,*,#21145,.F.);
#30723=ORIENTED_EDGE('',*,*,#21141,.T.);
#30724=ORIENTED_EDGE('',*,*,#21120,.T.);
#30725=ORIENTED_EDGE('',*,*,#20460,.F.);
#30726=ORIENTED_EDGE('',*,*,#20503,.F.);
#30727=ORIENTED_EDGE('',*,*,#20462,.T.);
#30728=ORIENTED_EDGE('',*,*,#21146,.F.);
#30729=ORIENTED_EDGE('',*,*,#21144,.T.);
#30730=ORIENTED_EDGE('',*,*,#20477,.T.);
#30731=ORIENTED_EDGE('',*,*,#21123,.T.);
#30732=ORIENTED_EDGE('',*,*,#21147,.F.);
#30733=ORIENTED_EDGE('',*,*,#21148,.F.);
#30734=ORIENTED_EDGE('',*,*,#21147,.T.);
#30735=ORIENTED_EDGE('',*,*,#21126,.T.);
#30736=ORIENTED_EDGE('',*,*,#21149,.T.);
#30737=ORIENTED_EDGE('',*,*,#21150,.F.);
#30738=ORIENTED_EDGE('',*,*,#21128,.T.);
#30739=ORIENTED_EDGE('',*,*,#21151,.T.);
#30740=ORIENTED_EDGE('',*,*,#21152,.T.);
#30741=ORIENTED_EDGE('',*,*,#21149,.F.);
#30742=ORIENTED_EDGE('',*,*,#21153,.T.);
#30743=ORIENTED_EDGE('',*,*,#21154,.F.);
#30744=ORIENTED_EDGE('',*,*,#21151,.F.);
#30745=ORIENTED_EDGE('',*,*,#21130,.T.);
#30746=ORIENTED_EDGE('',*,*,#21132,.T.);
#30747=ORIENTED_EDGE('',*,*,#21155,.T.);
#30748=ORIENTED_EDGE('',*,*,#21156,.T.);
#30749=ORIENTED_EDGE('',*,*,#21153,.F.);
#30750=ORIENTED_EDGE('',*,*,#21157,.T.);
#30751=ORIENTED_EDGE('',*,*,#21158,.F.);
#30752=ORIENTED_EDGE('',*,*,#21155,.F.);
#30753=ORIENTED_EDGE('',*,*,#21134,.T.);
#30754=ORIENTED_EDGE('',*,*,#21136,.T.);
#30755=ORIENTED_EDGE('',*,*,#21159,.T.);
#30756=ORIENTED_EDGE('',*,*,#21160,.T.);
#30757=ORIENTED_EDGE('',*,*,#21157,.F.);
#30758=ORIENTED_EDGE('',*,*,#21159,.F.);
#30759=ORIENTED_EDGE('',*,*,#21140,.T.);
#30760=ORIENTED_EDGE('',*,*,#20455,.T.);
#30761=ORIENTED_EDGE('',*,*,#20492,.F.);
#30762=ORIENTED_EDGE('',*,*,#21161,.T.);
#30763=ORIENTED_EDGE('',*,*,#21162,.F.);
#30764=ORIENTED_EDGE('',*,*,#21163,.F.);
#30765=ORIENTED_EDGE('',*,*,#21161,.F.);
#30766=ORIENTED_EDGE('',*,*,#20495,.F.);
#30767=ORIENTED_EDGE('',*,*,#21143,.T.);
#30768=ORIENTED_EDGE('',*,*,#21164,.T.);
#30769=ORIENTED_EDGE('',*,*,#21163,.T.);
#30770=ORIENTED_EDGE('',*,*,#21165,.F.);
#30771=ORIENTED_EDGE('',*,*,#21165,.T.);
#30772=ORIENTED_EDGE('',*,*,#21142,.T.);
#30773=ORIENTED_EDGE('',*,*,#21166,.T.);
#30774=ORIENTED_EDGE('',*,*,#21167,.F.);
#30775=ORIENTED_EDGE('',*,*,#21145,.T.);
#30776=ORIENTED_EDGE('',*,*,#21168,.T.);
#30777=ORIENTED_EDGE('',*,*,#21169,.F.);
#30778=ORIENTED_EDGE('',*,*,#21166,.F.);
#30779=ORIENTED_EDGE('',*,*,#20461,.T.);
#30780=ORIENTED_EDGE('',*,*,#21170,.T.);
#30781=ORIENTED_EDGE('',*,*,#21171,.F.);
#30782=ORIENTED_EDGE('',*,*,#21171,.T.);
#30783=ORIENTED_EDGE('',*,*,#21172,.F.);
#30784=ORIENTED_EDGE('',*,*,#21168,.F.);
#30785=ORIENTED_EDGE('',*,*,#21146,.T.);
#30786=ORIENTED_EDGE('',*,*,#21148,.T.);
#30787=ORIENTED_EDGE('',*,*,#21173,.F.);
#30788=ORIENTED_EDGE('',*,*,#21174,.F.);
#30789=ORIENTED_EDGE('',*,*,#21173,.T.);
#30790=ORIENTED_EDGE('',*,*,#21150,.T.);
#30791=ORIENTED_EDGE('',*,*,#21175,.T.);
#30792=ORIENTED_EDGE('',*,*,#21176,.F.);
#30793=ORIENTED_EDGE('',*,*,#21177,.T.);
#30794=ORIENTED_EDGE('',*,*,#21175,.F.);
#30795=ORIENTED_EDGE('',*,*,#21152,.F.);
#30796=ORIENTED_EDGE('',*,*,#21178,.T.);
#30797=ORIENTED_EDGE('',*,*,#21179,.F.);
#30798=ORIENTED_EDGE('',*,*,#21177,.F.);
#30799=ORIENTED_EDGE('',*,*,#21154,.T.);
#30800=ORIENTED_EDGE('',*,*,#21180,.T.);
#30801=ORIENTED_EDGE('',*,*,#21178,.F.);
#30802=ORIENTED_EDGE('',*,*,#21156,.F.);
#30803=ORIENTED_EDGE('',*,*,#21180,.F.);
#30804=ORIENTED_EDGE('',*,*,#21158,.T.);
#30805=ORIENTED_EDGE('',*,*,#21181,.T.);
#30806=ORIENTED_EDGE('',*,*,#21182,.F.);
#30807=ORIENTED_EDGE('',*,*,#21183,.T.);
#30808=ORIENTED_EDGE('',*,*,#21181,.F.);
#30809=ORIENTED_EDGE('',*,*,#21160,.F.);
#30810=ORIENTED_EDGE('',*,*,#21183,.F.);
#30811=ORIENTED_EDGE('',*,*,#21162,.T.);
#30812=ORIENTED_EDGE('',*,*,#21164,.F.);
#30813=ORIENTED_EDGE('',*,*,#21184,.F.);
#30814=ORIENTED_EDGE('',*,*,#20465,.T.);
#30815=ORIENTED_EDGE('',*,*,#21185,.T.);
#30816=ORIENTED_EDGE('',*,*,#21186,.F.);
#30817=ORIENTED_EDGE('',*,*,#21170,.F.);
#30818=ORIENTED_EDGE('',*,*,#20470,.T.);
#30819=ORIENTED_EDGE('',*,*,#21187,.T.);
#30820=ORIENTED_EDGE('',*,*,#21188,.F.);
#30821=ORIENTED_EDGE('',*,*,#21185,.F.);
#30822=ORIENTED_EDGE('',*,*,#20471,.T.);
#30823=ORIENTED_EDGE('',*,*,#21189,.T.);
#30824=ORIENTED_EDGE('',*,*,#21190,.F.);
#30825=ORIENTED_EDGE('',*,*,#21187,.F.);
#30826=ORIENTED_EDGE('',*,*,#20478,.T.);
#30827=ORIENTED_EDGE('',*,*,#21174,.T.);
#30828=ORIENTED_EDGE('',*,*,#21191,.F.);
#30829=ORIENTED_EDGE('',*,*,#21189,.F.);
#30830=ORIENTED_EDGE('',*,*,#21186,.T.);
#30831=ORIENTED_EDGE('',*,*,#21188,.T.);
#30832=ORIENTED_EDGE('',*,*,#21190,.T.);
#30833=ORIENTED_EDGE('',*,*,#21191,.T.);
#30834=ORIENTED_EDGE('',*,*,#21176,.T.);
#30835=ORIENTED_EDGE('',*,*,#21179,.T.);
#30836=ORIENTED_EDGE('',*,*,#21182,.T.);
#30837=ORIENTED_EDGE('',*,*,#21184,.T.);
#30838=ORIENTED_EDGE('',*,*,#21167,.T.);
#30839=ORIENTED_EDGE('',*,*,#21169,.T.);
#30840=ORIENTED_EDGE('',*,*,#21172,.T.);
#30841=ORIENTED_EDGE('',*,*,#21192,.F.);
#30842=ORIENTED_EDGE('',*,*,#21193,.T.);
#30843=ORIENTED_EDGE('',*,*,#21194,.T.);
#30844=ORIENTED_EDGE('',*,*,#21195,.F.);
#30845=ORIENTED_EDGE('',*,*,#21196,.F.);
#30846=ORIENTED_EDGE('',*,*,#21197,.F.);
#30847=ORIENTED_EDGE('',*,*,#21198,.F.);
#30848=ORIENTED_EDGE('',*,*,#21199,.T.);
#30849=ORIENTED_EDGE('',*,*,#21200,.T.);
#30850=ORIENTED_EDGE('',*,*,#21199,.F.);
#30851=ORIENTED_EDGE('',*,*,#21201,.F.);
#30852=ORIENTED_EDGE('',*,*,#21202,.T.);
#30853=ORIENTED_EDGE('',*,*,#21203,.F.);
#30854=ORIENTED_EDGE('',*,*,#21202,.F.);
#30855=ORIENTED_EDGE('',*,*,#21204,.F.);
#30856=ORIENTED_EDGE('',*,*,#21205,.T.);
#30857=ORIENTED_EDGE('',*,*,#21206,.T.);
#30858=ORIENTED_EDGE('',*,*,#21207,.F.);
#30859=ORIENTED_EDGE('',*,*,#21208,.F.);
#30860=ORIENTED_EDGE('',*,*,#21196,.T.);
#30861=ORIENTED_EDGE('',*,*,#21209,.T.);
#30862=ORIENTED_EDGE('',*,*,#21206,.F.);
#30863=ORIENTED_EDGE('',*,*,#21200,.F.);
#30864=ORIENTED_EDGE('',*,*,#21209,.F.);
#30865=ORIENTED_EDGE('',*,*,#21203,.T.);
#30866=ORIENTED_EDGE('',*,*,#21210,.T.);
#30867=ORIENTED_EDGE('',*,*,#21211,.F.);
#30868=ORIENTED_EDGE('',*,*,#21212,.T.);
#30869=ORIENTED_EDGE('',*,*,#21213,.T.);
#30870=ORIENTED_EDGE('',*,*,#21207,.T.);
#30871=ORIENTED_EDGE('',*,*,#21211,.T.);
#30872=ORIENTED_EDGE('',*,*,#21214,.T.);
#30873=ORIENTED_EDGE('',*,*,#21215,.T.);
#30874=ORIENTED_EDGE('',*,*,#21216,.T.);
#30875=ORIENTED_EDGE('',*,*,#21208,.T.);
#30876=ORIENTED_EDGE('',*,*,#21213,.F.);
#30877=ORIENTED_EDGE('',*,*,#21217,.F.);
#30878=ORIENTED_EDGE('',*,*,#21216,.F.);
#30879=ORIENTED_EDGE('',*,*,#21218,.F.);
#30880=ORIENTED_EDGE('',*,*,#21219,.F.);
#30881=ORIENTED_EDGE('',*,*,#21197,.T.);
#30882=ORIENTED_EDGE('',*,*,#21220,.F.);
#30883=ORIENTED_EDGE('',*,*,#21221,.T.);
#30884=ORIENTED_EDGE('',*,*,#21217,.T.);
#30885=ORIENTED_EDGE('',*,*,#21212,.F.);
#30886=ORIENTED_EDGE('',*,*,#21221,.F.);
#30887=ORIENTED_EDGE('',*,*,#21222,.F.);
#30888=ORIENTED_EDGE('',*,*,#21223,.T.);
#30889=ORIENTED_EDGE('',*,*,#21218,.T.);
#30890=ORIENTED_EDGE('',*,*,#21224,.T.);
#30891=ORIENTED_EDGE('',*,*,#21225,.T.);
#30892=ORIENTED_EDGE('',*,*,#21214,.F.);
#30893=ORIENTED_EDGE('',*,*,#21210,.F.);
#30894=ORIENTED_EDGE('',*,*,#21224,.F.);
#30895=ORIENTED_EDGE('',*,*,#21205,.F.);
#30896=ORIENTED_EDGE('',*,*,#21226,.F.);
#30897=ORIENTED_EDGE('',*,*,#21227,.T.);
#30898=ORIENTED_EDGE('',*,*,#21228,.T.);
#30899=ORIENTED_EDGE('',*,*,#21229,.F.);
#30900=ORIENTED_EDGE('',*,*,#21230,.F.);
#30901=ORIENTED_EDGE('',*,*,#21222,.T.);
#30902=ORIENTED_EDGE('',*,*,#21231,.T.);
#30903=ORIENTED_EDGE('',*,*,#21215,.F.);
#30904=ORIENTED_EDGE('',*,*,#21225,.F.);
#30905=ORIENTED_EDGE('',*,*,#21232,.T.);
#30906=ORIENTED_EDGE('',*,*,#21220,.T.);
#30907=ORIENTED_EDGE('',*,*,#21231,.F.);
#30908=ORIENTED_EDGE('',*,*,#21228,.F.);
#30909=ORIENTED_EDGE('',*,*,#21232,.F.);
#30910=ORIENTED_EDGE('',*,*,#21227,.F.);
#30911=ORIENTED_EDGE('',*,*,#21233,.T.);
#30912=ORIENTED_EDGE('',*,*,#21229,.T.);
#30913=ORIENTED_EDGE('',*,*,#21234,.F.);
#30914=ORIENTED_EDGE('',*,*,#21235,.F.);
#30915=ORIENTED_EDGE('',*,*,#21236,.F.);
#30916=ORIENTED_EDGE('',*,*,#21237,.F.);
#30917=ORIENTED_EDGE('',*,*,#21238,.F.);
#30918=ORIENTED_EDGE('',*,*,#21239,.F.);
#30919=ORIENTED_EDGE('',*,*,#21240,.F.);
#30920=ORIENTED_EDGE('',*,*,#21236,.T.);
#30921=ORIENTED_EDGE('',*,*,#21241,.T.);
#30922=ORIENTED_EDGE('',*,*,#21242,.F.);
#30923=ORIENTED_EDGE('',*,*,#21243,.F.);
#30924=ORIENTED_EDGE('',*,*,#21244,.F.);
#30925=ORIENTED_EDGE('',*,*,#21242,.T.);
#30926=ORIENTED_EDGE('',*,*,#21245,.F.);
#30927=ORIENTED_EDGE('',*,*,#21235,.T.);
#30928=ORIENTED_EDGE('',*,*,#21246,.T.);
#30929=ORIENTED_EDGE('',*,*,#21247,.F.);
#30930=ORIENTED_EDGE('',*,*,#21248,.F.);
#30931=ORIENTED_EDGE('',*,*,#21248,.T.);
#30932=ORIENTED_EDGE('',*,*,#21249,.F.);
#30933=ORIENTED_EDGE('',*,*,#21241,.F.);
#30934=ORIENTED_EDGE('',*,*,#21250,.F.);
#30935=ORIENTED_EDGE('',*,*,#21245,.T.);
#30936=ORIENTED_EDGE('',*,*,#21249,.T.);
#30937=ORIENTED_EDGE('',*,*,#21251,.F.);
#30938=ORIENTED_EDGE('',*,*,#21251,.T.);
#30939=ORIENTED_EDGE('',*,*,#21247,.T.);
#30940=ORIENTED_EDGE('',*,*,#21252,.F.);
#30941=ORIENTED_EDGE('',*,*,#21253,.F.);
#30942=ORIENTED_EDGE('',*,*,#21254,.F.);
#30943=ORIENTED_EDGE('',*,*,#21255,.F.);
#30944=ORIENTED_EDGE('',*,*,#21256,.F.);
#30945=ORIENTED_EDGE('',*,*,#21234,.T.);
#30946=ORIENTED_EDGE('',*,*,#21256,.T.);
#30947=ORIENTED_EDGE('',*,*,#21257,.F.);
#30948=ORIENTED_EDGE('',*,*,#21246,.F.);
#30949=ORIENTED_EDGE('',*,*,#21258,.F.);
#30950=ORIENTED_EDGE('',*,*,#21252,.T.);
#30951=ORIENTED_EDGE('',*,*,#21257,.T.);
#30952=ORIENTED_EDGE('',*,*,#21259,.F.);
#30953=ORIENTED_EDGE('',*,*,#21259,.T.);
#30954=ORIENTED_EDGE('',*,*,#21255,.T.);
#30955=ORIENTED_EDGE('',*,*,#21260,.F.);
#30956=ORIENTED_EDGE('',*,*,#21261,.F.);
#30957=ORIENTED_EDGE('',*,*,#21262,.F.);
#30958=ORIENTED_EDGE('',*,*,#21263,.F.);
#30959=ORIENTED_EDGE('',*,*,#21264,.F.);
#30960=ORIENTED_EDGE('',*,*,#21265,.F.);
#30961=ORIENTED_EDGE('',*,*,#21266,.F.);
#30962=ORIENTED_EDGE('',*,*,#21267,.F.);
#30963=ORIENTED_EDGE('',*,*,#21264,.T.);
#30964=ORIENTED_EDGE('',*,*,#21268,.T.);
#30965=ORIENTED_EDGE('',*,*,#21269,.F.);
#30966=ORIENTED_EDGE('',*,*,#21270,.F.);
#30967=ORIENTED_EDGE('',*,*,#21271,.F.);
#30968=ORIENTED_EDGE('',*,*,#21269,.T.);
#30969=ORIENTED_EDGE('',*,*,#21272,.T.);
#30970=ORIENTED_EDGE('',*,*,#21273,.T.);
#30971=ORIENTED_EDGE('',*,*,#21274,.F.);
#30972=ORIENTED_EDGE('',*,*,#21268,.F.);
#30973=ORIENTED_EDGE('',*,*,#21275,.F.);
#30974=ORIENTED_EDGE('',*,*,#21272,.F.);
#30975=ORIENTED_EDGE('',*,*,#21274,.T.);
#30976=ORIENTED_EDGE('',*,*,#21276,.T.);
#30977=ORIENTED_EDGE('',*,*,#21276,.F.);
#30978=ORIENTED_EDGE('',*,*,#21277,.T.);
#30979=ORIENTED_EDGE('',*,*,#21278,.F.);
#30980=ORIENTED_EDGE('',*,*,#21194,.F.);
#30981=ORIENTED_EDGE('',*,*,#21263,.T.);
#30982=ORIENTED_EDGE('',*,*,#21279,.T.);
#30983=ORIENTED_EDGE('',*,*,#21277,.F.);
#30984=ORIENTED_EDGE('',*,*,#21273,.F.);
#30985=ORIENTED_EDGE('',*,*,#21280,.F.);
#30986=ORIENTED_EDGE('',*,*,#21281,.F.);
#30987=ORIENTED_EDGE('',*,*,#21282,.F.);
#30988=ORIENTED_EDGE('',*,*,#21283,.F.);
#30989=ORIENTED_EDGE('',*,*,#21262,.T.);
#30990=ORIENTED_EDGE('',*,*,#21283,.T.);
#30991=ORIENTED_EDGE('',*,*,#21284,.F.);
#30992=ORIENTED_EDGE('',*,*,#21279,.F.);
#30993=ORIENTED_EDGE('',*,*,#21285,.F.);
#30994=ORIENTED_EDGE('',*,*,#21278,.T.);
#30995=ORIENTED_EDGE('',*,*,#21284,.T.);
#30996=ORIENTED_EDGE('',*,*,#21286,.F.);
#30997=ORIENTED_EDGE('',*,*,#21286,.T.);
#30998=ORIENTED_EDGE('',*,*,#21282,.T.);
#30999=ORIENTED_EDGE('',*,*,#21287,.F.);
#31000=ORIENTED_EDGE('',*,*,#21288,.F.);
#31001=ORIENTED_EDGE('',*,*,#21289,.T.);
#31002=ORIENTED_EDGE('',*,*,#21290,.T.);
#31003=ORIENTED_EDGE('',*,*,#21291,.F.);
#31004=ORIENTED_EDGE('',*,*,#21292,.T.);
#31005=ORIENTED_EDGE('',*,*,#21293,.T.);
#31006=ORIENTED_EDGE('',*,*,#21294,.F.);
#31007=ORIENTED_EDGE('',*,*,#21295,.F.);
#31008=ORIENTED_EDGE('',*,*,#21291,.T.);
#31009=ORIENTED_EDGE('',*,*,#21296,.T.);
#31010=ORIENTED_EDGE('',*,*,#21297,.T.);
#31011=ORIENTED_EDGE('',*,*,#21298,.T.);
#31012=ORIENTED_EDGE('',*,*,#21299,.T.);
#31013=ORIENTED_EDGE('',*,*,#21294,.T.);
#31014=ORIENTED_EDGE('',*,*,#21300,.T.);
#31015=ORIENTED_EDGE('',*,*,#21301,.T.);
#31016=ORIENTED_EDGE('',*,*,#21302,.T.);
#31017=ORIENTED_EDGE('',*,*,#21303,.T.);
#31018=ORIENTED_EDGE('',*,*,#21292,.F.);
#31019=ORIENTED_EDGE('',*,*,#21304,.F.);
#31020=ORIENTED_EDGE('',*,*,#21305,.T.);
#31021=ORIENTED_EDGE('',*,*,#21304,.T.);
#31022=ORIENTED_EDGE('',*,*,#21295,.T.);
#31023=ORIENTED_EDGE('',*,*,#21306,.F.);
#31024=ORIENTED_EDGE('',*,*,#21307,.T.);
#31025=ORIENTED_EDGE('',*,*,#21306,.T.);
#31026=ORIENTED_EDGE('',*,*,#21299,.F.);
#31027=ORIENTED_EDGE('',*,*,#21308,.F.);
#31028=ORIENTED_EDGE('',*,*,#21305,.F.);
#31029=ORIENTED_EDGE('',*,*,#21307,.F.);
#31030=ORIENTED_EDGE('',*,*,#21309,.T.);
#31031=ORIENTED_EDGE('',*,*,#21310,.T.);
#31032=ORIENTED_EDGE('',*,*,#21311,.T.);
#31033=ORIENTED_EDGE('',*,*,#21308,.T.);
#31034=ORIENTED_EDGE('',*,*,#21298,.F.);
#31035=ORIENTED_EDGE('',*,*,#21312,.F.);
#31036=ORIENTED_EDGE('',*,*,#21309,.F.);
#31037=ORIENTED_EDGE('',*,*,#21311,.F.);
#31038=ORIENTED_EDGE('',*,*,#21313,.T.);
#31039=ORIENTED_EDGE('',*,*,#21314,.T.);
#31040=ORIENTED_EDGE('',*,*,#21315,.T.);
#31041=ORIENTED_EDGE('',*,*,#21312,.T.);
#31042=ORIENTED_EDGE('',*,*,#21297,.F.);
#31043=ORIENTED_EDGE('',*,*,#21316,.F.);
#31044=ORIENTED_EDGE('',*,*,#21313,.F.);
#31045=ORIENTED_EDGE('',*,*,#21315,.F.);
#31046=ORIENTED_EDGE('',*,*,#21317,.F.);
#31047=ORIENTED_EDGE('',*,*,#21318,.T.);
#31048=ORIENTED_EDGE('',*,*,#21319,.T.);
#31049=ORIENTED_EDGE('',*,*,#21320,.T.);
#31050=ORIENTED_EDGE('',*,*,#21321,.T.);
#31051=ORIENTED_EDGE('',*,*,#21296,.F.);
#31052=ORIENTED_EDGE('',*,*,#21322,.T.);
#31053=ORIENTED_EDGE('',*,*,#21316,.T.);
#31054=ORIENTED_EDGE('',*,*,#21321,.F.);
#31055=ORIENTED_EDGE('',*,*,#21323,.T.);
#31056=ORIENTED_EDGE('',*,*,#21317,.T.);
#31057=ORIENTED_EDGE('',*,*,#21322,.F.);
#31058=ORIENTED_EDGE('',*,*,#21324,.F.);
#31059=ORIENTED_EDGE('',*,*,#21324,.T.);
#31060=ORIENTED_EDGE('',*,*,#21320,.F.);
#31061=ORIENTED_EDGE('',*,*,#21325,.T.);
#31062=ORIENTED_EDGE('',*,*,#21326,.T.);
#31063=ORIENTED_EDGE('',*,*,#21327,.T.);
#31064=ORIENTED_EDGE('',*,*,#21328,.F.);
#31065=ORIENTED_EDGE('',*,*,#21329,.T.);
#31066=ORIENTED_EDGE('',*,*,#21330,.F.);
#31067=ORIENTED_EDGE('',*,*,#21331,.T.);
#31068=ORIENTED_EDGE('',*,*,#21332,.F.);
#31069=ORIENTED_EDGE('',*,*,#21230,.T.);
#31070=ORIENTED_EDGE('',*,*,#21233,.F.);
#31071=ORIENTED_EDGE('',*,*,#21226,.T.);
#31072=ORIENTED_EDGE('',*,*,#21204,.T.);
#31073=ORIENTED_EDGE('',*,*,#21201,.T.);
#31074=ORIENTED_EDGE('',*,*,#21198,.T.);
#31075=ORIENTED_EDGE('',*,*,#21219,.T.);
#31076=ORIENTED_EDGE('',*,*,#21223,.F.);
#31077=ORIENTED_EDGE('',*,*,#21333,.T.);
#31078=ORIENTED_EDGE('',*,*,#21243,.T.);
#31079=ORIENTED_EDGE('',*,*,#21334,.F.);
#31080=ORIENTED_EDGE('',*,*,#21335,.F.);
#31081=ORIENTED_EDGE('',*,*,#21334,.T.);
#31082=ORIENTED_EDGE('',*,*,#21250,.T.);
#31083=ORIENTED_EDGE('',*,*,#21336,.F.);
#31084=ORIENTED_EDGE('',*,*,#21337,.F.);
#31085=ORIENTED_EDGE('',*,*,#21336,.T.);
#31086=ORIENTED_EDGE('',*,*,#21253,.T.);
#31087=ORIENTED_EDGE('',*,*,#21338,.F.);
#31088=ORIENTED_EDGE('',*,*,#21339,.F.);
#31089=ORIENTED_EDGE('',*,*,#21338,.T.);
#31090=ORIENTED_EDGE('',*,*,#21258,.T.);
#31091=ORIENTED_EDGE('',*,*,#21340,.F.);
#31092=ORIENTED_EDGE('',*,*,#21341,.F.);
#31093=ORIENTED_EDGE('',*,*,#21340,.T.);
#31094=ORIENTED_EDGE('',*,*,#21261,.T.);
#31095=ORIENTED_EDGE('',*,*,#21342,.F.);
#31096=ORIENTED_EDGE('',*,*,#21343,.F.);
#31097=ORIENTED_EDGE('',*,*,#21344,.T.);
#31098=ORIENTED_EDGE('',*,*,#21270,.T.);
#31099=ORIENTED_EDGE('',*,*,#21345,.F.);
#31100=ORIENTED_EDGE('',*,*,#21346,.F.);
#31101=ORIENTED_EDGE('',*,*,#21345,.T.);
#31102=ORIENTED_EDGE('',*,*,#21275,.T.);
#31103=ORIENTED_EDGE('',*,*,#21193,.F.);
#31104=ORIENTED_EDGE('',*,*,#21347,.F.);
#31105=ORIENTED_EDGE('',*,*,#21195,.T.);
#31106=ORIENTED_EDGE('',*,*,#21285,.T.);
#31107=ORIENTED_EDGE('',*,*,#21348,.F.);
#31108=ORIENTED_EDGE('',*,*,#21349,.F.);
#31109=ORIENTED_EDGE('',*,*,#21348,.T.);
#31110=ORIENTED_EDGE('',*,*,#21288,.T.);
#31111=ORIENTED_EDGE('',*,*,#21350,.F.);
#31112=ORIENTED_EDGE('',*,*,#21351,.F.);
#31113=ORIENTED_EDGE('',*,*,#21352,.T.);
#31114=ORIENTED_EDGE('',*,*,#21353,.T.);
#31115=ORIENTED_EDGE('',*,*,#21354,.F.);
#31116=ORIENTED_EDGE('',*,*,#21289,.F.);
#31117=ORIENTED_EDGE('',*,*,#21355,.T.);
#31118=ORIENTED_EDGE('',*,*,#21356,.T.);
#31119=ORIENTED_EDGE('',*,*,#21352,.F.);
#31120=ORIENTED_EDGE('',*,*,#21303,.F.);
#31121=ORIENTED_EDGE('',*,*,#21357,.T.);
#31122=ORIENTED_EDGE('',*,*,#21358,.T.);
#31123=ORIENTED_EDGE('',*,*,#21355,.F.);
#31124=ORIENTED_EDGE('',*,*,#21310,.F.);
#31125=ORIENTED_EDGE('',*,*,#21359,.T.);
#31126=ORIENTED_EDGE('',*,*,#21360,.T.);
#31127=ORIENTED_EDGE('',*,*,#21357,.F.);
#31128=ORIENTED_EDGE('',*,*,#21314,.F.);
#31129=ORIENTED_EDGE('',*,*,#21361,.T.);
#31130=ORIENTED_EDGE('',*,*,#21362,.T.);
#31131=ORIENTED_EDGE('',*,*,#21359,.F.);
#31132=ORIENTED_EDGE('',*,*,#21318,.F.);
#31133=ORIENTED_EDGE('',*,*,#21363,.T.);
#31134=ORIENTED_EDGE('',*,*,#21364,.T.);
#31135=ORIENTED_EDGE('',*,*,#21361,.F.);
#31136=ORIENTED_EDGE('',*,*,#21323,.F.);
#31137=ORIENTED_EDGE('',*,*,#21365,.T.);
#31138=ORIENTED_EDGE('',*,*,#21366,.T.);
#31139=ORIENTED_EDGE('',*,*,#21363,.F.);
#31140=ORIENTED_EDGE('',*,*,#21326,.F.);
#31141=ORIENTED_EDGE('',*,*,#21346,.T.);
#31142=ORIENTED_EDGE('',*,*,#21347,.T.);
#31143=ORIENTED_EDGE('',*,*,#21192,.T.);
#31144=ORIENTED_EDGE('',*,*,#21349,.T.);
#31145=ORIENTED_EDGE('',*,*,#21351,.T.);
#31146=ORIENTED_EDGE('',*,*,#21367,.F.);
#31147=ORIENTED_EDGE('',*,*,#21353,.F.);
#31148=ORIENTED_EDGE('',*,*,#21356,.F.);
#31149=ORIENTED_EDGE('',*,*,#21358,.F.);
#31150=ORIENTED_EDGE('',*,*,#21360,.F.);
#31151=ORIENTED_EDGE('',*,*,#21362,.F.);
#31152=ORIENTED_EDGE('',*,*,#21364,.F.);
#31153=ORIENTED_EDGE('',*,*,#21366,.F.);
#31154=ORIENTED_EDGE('',*,*,#21368,.F.);
#31155=ORIENTED_EDGE('',*,*,#21335,.T.);
#31156=ORIENTED_EDGE('',*,*,#21337,.T.);
#31157=ORIENTED_EDGE('',*,*,#21339,.T.);
#31158=ORIENTED_EDGE('',*,*,#21341,.T.);
#31159=ORIENTED_EDGE('',*,*,#21343,.T.);
#31160=ORIENTED_EDGE('',*,*,#21369,.F.);
#31161=ORIENTED_EDGE('',*,*,#21350,.T.);
#31162=ORIENTED_EDGE('',*,*,#21370,.F.);
#31163=ORIENTED_EDGE('',*,*,#21371,.F.);
#31164=ORIENTED_EDGE('',*,*,#21372,.F.);
#31165=ORIENTED_EDGE('',*,*,#21372,.T.);
#31166=ORIENTED_EDGE('',*,*,#21354,.T.);
#31167=ORIENTED_EDGE('',*,*,#21373,.T.);
#31168=ORIENTED_EDGE('',*,*,#21374,.F.);
#31169=ORIENTED_EDGE('',*,*,#21375,.F.);
#31170=ORIENTED_EDGE('',*,*,#21375,.T.);
#31171=ORIENTED_EDGE('',*,*,#21376,.F.);
#31172=ORIENTED_EDGE('',*,*,#21377,.F.);
#31173=ORIENTED_EDGE('',*,*,#21373,.F.);
#31174=ORIENTED_EDGE('',*,*,#21367,.T.);
#31175=ORIENTED_EDGE('',*,*,#21371,.T.);
#31176=ORIENTED_EDGE('',*,*,#21378,.T.);
#31177=ORIENTED_EDGE('',*,*,#21281,.T.);
#31178=ORIENTED_EDGE('',*,*,#21379,.F.);
#31179=ORIENTED_EDGE('',*,*,#21380,.F.);
#31180=ORIENTED_EDGE('',*,*,#21370,.T.);
#31181=ORIENTED_EDGE('',*,*,#21287,.T.);
#31182=ORIENTED_EDGE('',*,*,#21378,.F.);
#31183=ORIENTED_EDGE('',*,*,#21381,.F.);
#31184=ORIENTED_EDGE('',*,*,#21376,.T.);
#31185=ORIENTED_EDGE('',*,*,#21374,.T.);
#31186=ORIENTED_EDGE('',*,*,#21382,.T.);
#31187=ORIENTED_EDGE('',*,*,#21383,.F.);
#31188=ORIENTED_EDGE('',*,*,#21290,.F.);
#31189=ORIENTED_EDGE('',*,*,#21383,.T.);
#31190=ORIENTED_EDGE('',*,*,#21384,.T.);
#31191=ORIENTED_EDGE('',*,*,#21385,.F.);
#31192=ORIENTED_EDGE('',*,*,#21293,.F.);
#31193=ORIENTED_EDGE('',*,*,#21385,.T.);
#31194=ORIENTED_EDGE('',*,*,#21386,.T.);
#31195=ORIENTED_EDGE('',*,*,#21387,.F.);
#31196=ORIENTED_EDGE('',*,*,#21300,.F.);
#31197=ORIENTED_EDGE('',*,*,#21388,.T.);
#31198=ORIENTED_EDGE('',*,*,#21331,.F.);
#31199=ORIENTED_EDGE('',*,*,#21389,.F.);
#31200=ORIENTED_EDGE('',*,*,#21386,.F.);
#31201=ORIENTED_EDGE('',*,*,#21384,.F.);
#31202=ORIENTED_EDGE('',*,*,#21382,.F.);
#31203=ORIENTED_EDGE('',*,*,#21377,.T.);
#31204=ORIENTED_EDGE('',*,*,#21381,.T.);
#31205=ORIENTED_EDGE('',*,*,#21380,.T.);
#31206=ORIENTED_EDGE('',*,*,#21387,.T.);
#31207=ORIENTED_EDGE('',*,*,#21390,.T.);
#31208=ORIENTED_EDGE('',*,*,#21391,.F.);
#31209=ORIENTED_EDGE('',*,*,#21301,.F.);
#31210=ORIENTED_EDGE('',*,*,#21389,.T.);
#31211=ORIENTED_EDGE('',*,*,#21330,.T.);
#31212=ORIENTED_EDGE('',*,*,#21392,.F.);
#31213=ORIENTED_EDGE('',*,*,#21390,.F.);
#31214=ORIENTED_EDGE('',*,*,#21393,.T.);
#31215=ORIENTED_EDGE('',*,*,#21394,.F.);
#31216=ORIENTED_EDGE('',*,*,#21394,.T.);
#31217=ORIENTED_EDGE('',*,*,#21395,.T.);
#31218=ORIENTED_EDGE('',*,*,#21333,.F.);
#31219=ORIENTED_EDGE('',*,*,#21396,.F.);
#31220=ORIENTED_EDGE('',*,*,#21397,.T.);
#31221=ORIENTED_EDGE('',*,*,#21398,.T.);
#31222=ORIENTED_EDGE('',*,*,#21399,.F.);
#31223=ORIENTED_EDGE('',*,*,#21399,.T.);
#31224=ORIENTED_EDGE('',*,*,#21365,.F.);
#31225=ORIENTED_EDGE('',*,*,#21400,.F.);
#31226=ORIENTED_EDGE('',*,*,#21396,.T.);
#31227=ORIENTED_EDGE('',*,*,#21368,.T.);
#31228=ORIENTED_EDGE('',*,*,#21398,.F.);
#31229=ORIENTED_EDGE('',*,*,#21401,.T.);
#31230=ORIENTED_EDGE('',*,*,#21239,.T.);
#31231=ORIENTED_EDGE('',*,*,#21402,.F.);
#31232=ORIENTED_EDGE('',*,*,#21403,.F.);
#31233=ORIENTED_EDGE('',*,*,#21402,.T.);
#31234=ORIENTED_EDGE('',*,*,#21244,.T.);
#31235=ORIENTED_EDGE('',*,*,#21395,.F.);
#31236=ORIENTED_EDGE('',*,*,#21393,.F.);
#31237=ORIENTED_EDGE('',*,*,#21404,.F.);
#31238=ORIENTED_EDGE('',*,*,#21391,.T.);
#31239=ORIENTED_EDGE('',*,*,#21405,.T.);
#31240=ORIENTED_EDGE('',*,*,#21406,.F.);
#31241=ORIENTED_EDGE('',*,*,#21302,.F.);
#31242=ORIENTED_EDGE('',*,*,#21406,.T.);
#31243=ORIENTED_EDGE('',*,*,#21407,.T.);
#31244=ORIENTED_EDGE('',*,*,#21408,.F.);
#31245=ORIENTED_EDGE('',*,*,#21319,.F.);
#31246=ORIENTED_EDGE('',*,*,#21408,.T.);
#31247=ORIENTED_EDGE('',*,*,#21409,.T.);
#31248=ORIENTED_EDGE('',*,*,#21397,.F.);
#31249=ORIENTED_EDGE('',*,*,#21325,.F.);
#31250=ORIENTED_EDGE('',*,*,#21392,.T.);
#31251=ORIENTED_EDGE('',*,*,#21329,.F.);
#31252=ORIENTED_EDGE('',*,*,#21410,.F.);
#31253=ORIENTED_EDGE('',*,*,#21403,.T.);
#31254=ORIENTED_EDGE('',*,*,#21404,.T.);
#31255=ORIENTED_EDGE('',*,*,#21400,.T.);
#31256=ORIENTED_EDGE('',*,*,#21409,.F.);
#31257=ORIENTED_EDGE('',*,*,#21407,.F.);
#31258=ORIENTED_EDGE('',*,*,#21405,.F.);
#31259=ORIENTED_EDGE('',*,*,#21411,.T.);
#31260=ORIENTED_EDGE('',*,*,#21266,.T.);
#31261=ORIENTED_EDGE('',*,*,#21412,.F.);
#31262=ORIENTED_EDGE('',*,*,#21413,.F.);
#31263=ORIENTED_EDGE('',*,*,#21379,.T.);
#31264=ORIENTED_EDGE('',*,*,#21280,.T.);
#31265=ORIENTED_EDGE('',*,*,#21411,.F.);
#31266=ORIENTED_EDGE('',*,*,#21414,.F.);
#31267=ORIENTED_EDGE('',*,*,#21415,.T.);
#31268=ORIENTED_EDGE('',*,*,#21332,.T.);
#31269=ORIENTED_EDGE('',*,*,#21388,.F.);
#31270=ORIENTED_EDGE('',*,*,#21414,.T.);
#31271=ORIENTED_EDGE('',*,*,#21413,.T.);
#31272=ORIENTED_EDGE('',*,*,#21416,.T.);
#31273=ORIENTED_EDGE('',*,*,#21237,.T.);
#31274=ORIENTED_EDGE('',*,*,#21417,.F.);
#31275=ORIENTED_EDGE('',*,*,#21418,.F.);
#31276=ORIENTED_EDGE('',*,*,#21417,.T.);
#31277=ORIENTED_EDGE('',*,*,#21240,.T.);
#31278=ORIENTED_EDGE('',*,*,#21401,.F.);
#31279=ORIENTED_EDGE('',*,*,#21419,.F.);
#31280=ORIENTED_EDGE('',*,*,#21410,.T.);
#31281=ORIENTED_EDGE('',*,*,#21328,.T.);
#31282=ORIENTED_EDGE('',*,*,#21420,.F.);
#31283=ORIENTED_EDGE('',*,*,#21418,.T.);
#31284=ORIENTED_EDGE('',*,*,#21419,.T.);
#31285=ORIENTED_EDGE('',*,*,#21342,.T.);
#31286=ORIENTED_EDGE('',*,*,#21421,.F.);
#31287=ORIENTED_EDGE('',*,*,#21422,.F.);
#31288=ORIENTED_EDGE('',*,*,#21423,.F.);
#31289=ORIENTED_EDGE('',*,*,#21423,.T.);
#31290=ORIENTED_EDGE('',*,*,#21424,.T.);
#31291=ORIENTED_EDGE('',*,*,#21425,.F.);
#31292=ORIENTED_EDGE('',*,*,#21425,.T.);
#31293=ORIENTED_EDGE('',*,*,#21426,.T.);
#31294=ORIENTED_EDGE('',*,*,#21344,.F.);
#31295=ORIENTED_EDGE('',*,*,#21427,.F.);
#31296=ORIENTED_EDGE('',*,*,#21369,.T.);
#31297=ORIENTED_EDGE('',*,*,#21422,.T.);
#31298=ORIENTED_EDGE('',*,*,#21428,.F.);
#31299=ORIENTED_EDGE('',*,*,#21427,.T.);
#31300=ORIENTED_EDGE('',*,*,#21429,.T.);
#31301=ORIENTED_EDGE('',*,*,#21238,.T.);
#31302=ORIENTED_EDGE('',*,*,#21416,.F.);
#31303=ORIENTED_EDGE('',*,*,#21430,.F.);
#31304=ORIENTED_EDGE('',*,*,#21431,.T.);
#31305=ORIENTED_EDGE('',*,*,#21254,.T.);
#31306=ORIENTED_EDGE('',*,*,#21429,.F.);
#31307=ORIENTED_EDGE('',*,*,#21432,.F.);
#31308=ORIENTED_EDGE('',*,*,#21421,.T.);
#31309=ORIENTED_EDGE('',*,*,#21260,.T.);
#31310=ORIENTED_EDGE('',*,*,#21431,.F.);
#31311=ORIENTED_EDGE('',*,*,#21433,.F.);
#31312=ORIENTED_EDGE('',*,*,#21412,.T.);
#31313=ORIENTED_EDGE('',*,*,#21265,.T.);
#31314=ORIENTED_EDGE('',*,*,#21434,.F.);
#31315=ORIENTED_EDGE('',*,*,#21435,.F.);
#31316=ORIENTED_EDGE('',*,*,#21434,.T.);
#31317=ORIENTED_EDGE('',*,*,#21267,.T.);
#31318=ORIENTED_EDGE('',*,*,#21436,.F.);
#31319=ORIENTED_EDGE('',*,*,#21437,.F.);
#31320=ORIENTED_EDGE('',*,*,#21436,.T.);
#31321=ORIENTED_EDGE('',*,*,#21271,.T.);
#31322=ORIENTED_EDGE('',*,*,#21426,.F.);
#31323=ORIENTED_EDGE('',*,*,#21424,.F.);
#31324=ORIENTED_EDGE('',*,*,#21438,.F.);
#31325=ORIENTED_EDGE('',*,*,#21428,.T.);
#31326=ORIENTED_EDGE('',*,*,#21433,.T.);
#31327=ORIENTED_EDGE('',*,*,#21432,.T.);
#31328=ORIENTED_EDGE('',*,*,#21430,.T.);
#31329=ORIENTED_EDGE('',*,*,#21420,.T.);
#31330=ORIENTED_EDGE('',*,*,#21327,.F.);
#31331=ORIENTED_EDGE('',*,*,#21415,.F.);
#31332=ORIENTED_EDGE('',*,*,#21435,.T.);
#31333=ORIENTED_EDGE('',*,*,#21437,.T.);
#31334=ORIENTED_EDGE('',*,*,#21438,.T.);
#31335=ORIENTED_EDGE('',*,*,#21439,.T.);
#31336=ORIENTED_EDGE('',*,*,#21440,.T.);
#31337=ORIENTED_EDGE('',*,*,#21441,.T.);
#31338=ORIENTED_EDGE('',*,*,#21442,.F.);
#31339=ORIENTED_EDGE('',*,*,#21443,.F.);
#31340=ORIENTED_EDGE('',*,*,#21444,.T.);
#31341=ORIENTED_EDGE('',*,*,#21445,.T.);
#31342=ORIENTED_EDGE('',*,*,#21446,.T.);
#31343=ORIENTED_EDGE('',*,*,#21447,.T.);
#31344=ORIENTED_EDGE('',*,*,#21448,.T.);
#31345=ORIENTED_EDGE('',*,*,#21449,.T.);
#31346=ORIENTED_EDGE('',*,*,#21450,.F.);
#31347=ORIENTED_EDGE('',*,*,#21451,.T.);
#31348=ORIENTED_EDGE('',*,*,#21452,.T.);
#31349=ORIENTED_EDGE('',*,*,#21449,.F.);
#31350=ORIENTED_EDGE('',*,*,#21453,.F.);
#31351=ORIENTED_EDGE('',*,*,#21454,.T.);
#31352=ORIENTED_EDGE('',*,*,#21450,.T.);
#31353=ORIENTED_EDGE('',*,*,#21448,.F.);
#31354=ORIENTED_EDGE('',*,*,#21455,.F.);
#31355=ORIENTED_EDGE('',*,*,#21456,.T.);
#31356=ORIENTED_EDGE('',*,*,#21453,.T.);
#31357=ORIENTED_EDGE('',*,*,#21447,.F.);
#31358=ORIENTED_EDGE('',*,*,#21457,.F.);
#31359=ORIENTED_EDGE('',*,*,#21458,.T.);
#31360=ORIENTED_EDGE('',*,*,#21455,.T.);
#31361=ORIENTED_EDGE('',*,*,#21446,.F.);
#31362=ORIENTED_EDGE('',*,*,#21459,.F.);
#31363=ORIENTED_EDGE('',*,*,#21460,.F.);
#31364=ORIENTED_EDGE('',*,*,#21461,.T.);
#31365=ORIENTED_EDGE('',*,*,#21462,.F.);
#31366=ORIENTED_EDGE('',*,*,#21463,.T.);
#31367=ORIENTED_EDGE('',*,*,#21464,.T.);
#31368=ORIENTED_EDGE('',*,*,#21460,.T.);
#31369=ORIENTED_EDGE('',*,*,#21465,.F.);
#31370=ORIENTED_EDGE('',*,*,#21459,.T.);
#31371=ORIENTED_EDGE('',*,*,#21466,.F.);
#31372=ORIENTED_EDGE('',*,*,#21467,.T.);
#31373=ORIENTED_EDGE('',*,*,#21465,.T.);
#31374=ORIENTED_EDGE('',*,*,#21462,.T.);
#31375=ORIENTED_EDGE('',*,*,#21468,.F.);
#31376=ORIENTED_EDGE('',*,*,#21469,.T.);
#31377=ORIENTED_EDGE('',*,*,#21466,.T.);
#31378=ORIENTED_EDGE('',*,*,#21470,.T.);
#31379=ORIENTED_EDGE('',*,*,#21470,.F.);
#31380=ORIENTED_EDGE('',*,*,#21471,.T.);
#31381=ORIENTED_EDGE('',*,*,#21472,.T.);
#31382=ORIENTED_EDGE('',*,*,#21471,.F.);
#31383=ORIENTED_EDGE('',*,*,#21473,.T.);
#31384=ORIENTED_EDGE('',*,*,#21474,.F.);
#31385=ORIENTED_EDGE('',*,*,#21475,.F.);
#31386=ORIENTED_EDGE('',*,*,#21476,.T.);
#31387=ORIENTED_EDGE('',*,*,#21477,.F.);
#31388=ORIENTED_EDGE('',*,*,#21478,.F.);
#31389=ORIENTED_EDGE('',*,*,#21479,.F.);
#31390=ORIENTED_EDGE('',*,*,#21480,.T.);
#31391=ORIENTED_EDGE('',*,*,#21481,.T.);
#31392=ORIENTED_EDGE('',*,*,#21482,.F.);
#31393=ORIENTED_EDGE('',*,*,#21483,.T.);
#31394=ORIENTED_EDGE('',*,*,#21484,.T.);
#31395=ORIENTED_EDGE('',*,*,#21485,.F.);
#31396=ORIENTED_EDGE('',*,*,#21486,.F.);
#31397=ORIENTED_EDGE('',*,*,#21487,.T.);
#31398=ORIENTED_EDGE('',*,*,#21488,.T.);
#31399=ORIENTED_EDGE('',*,*,#21489,.F.);
#31400=ORIENTED_EDGE('',*,*,#21490,.T.);
#31401=ORIENTED_EDGE('',*,*,#21491,.F.);
#31402=ORIENTED_EDGE('',*,*,#21492,.T.);
#31403=ORIENTED_EDGE('',*,*,#21493,.T.);
#31404=ORIENTED_EDGE('',*,*,#21494,.T.);
#31405=ORIENTED_EDGE('',*,*,#21495,.F.);
#31406=ORIENTED_EDGE('',*,*,#21496,.F.);
#31407=ORIENTED_EDGE('',*,*,#21497,.T.);
#31408=ORIENTED_EDGE('',*,*,#21498,.T.);
#31409=ORIENTED_EDGE('',*,*,#21499,.T.);
#31410=ORIENTED_EDGE('',*,*,#21500,.F.);
#31411=ORIENTED_EDGE('',*,*,#21501,.T.);
#31412=ORIENTED_EDGE('',*,*,#21440,.F.);
#31413=ORIENTED_EDGE('',*,*,#21472,.F.);
#31414=ORIENTED_EDGE('',*,*,#21502,.T.);
#31415=ORIENTED_EDGE('',*,*,#21503,.T.);
#31416=ORIENTED_EDGE('',*,*,#21443,.T.);
#31417=ORIENTED_EDGE('',*,*,#21504,.T.);
#31418=ORIENTED_EDGE('',*,*,#21505,.F.);
#31419=ORIENTED_EDGE('',*,*,#21506,.T.);
#31420=ORIENTED_EDGE('',*,*,#21507,.F.);
#31421=ORIENTED_EDGE('',*,*,#21508,.T.);
#31422=ORIENTED_EDGE('',*,*,#21509,.T.);
#31423=ORIENTED_EDGE('',*,*,#21510,.T.);
#31424=ORIENTED_EDGE('',*,*,#21511,.F.);
#31425=ORIENTED_EDGE('',*,*,#21512,.T.);
#31426=ORIENTED_EDGE('',*,*,#21513,.F.);
#31427=ORIENTED_EDGE('',*,*,#21514,.F.);
#31428=ORIENTED_EDGE('',*,*,#21515,.F.);
#31429=ORIENTED_EDGE('',*,*,#21516,.F.);
#31430=ORIENTED_EDGE('',*,*,#21456,.F.);
#31431=ORIENTED_EDGE('',*,*,#21458,.F.);
#31432=ORIENTED_EDGE('',*,*,#21517,.T.);
#31433=ORIENTED_EDGE('',*,*,#21463,.F.);
#31434=ORIENTED_EDGE('',*,*,#21467,.F.);
#31435=ORIENTED_EDGE('',*,*,#21469,.F.);
#31436=ORIENTED_EDGE('',*,*,#21518,.T.);
#31437=ORIENTED_EDGE('',*,*,#21519,.T.);
#31438=ORIENTED_EDGE('',*,*,#21451,.F.);
#31439=ORIENTED_EDGE('',*,*,#21454,.F.);
#31440=ORIENTED_EDGE('',*,*,#21520,.F.);
#31441=ORIENTED_EDGE('',*,*,#21521,.F.);
#31442=ORIENTED_EDGE('',*,*,#21512,.F.);
#31443=ORIENTED_EDGE('',*,*,#21522,.T.);
#31444=ORIENTED_EDGE('',*,*,#21523,.F.);
#31445=ORIENTED_EDGE('',*,*,#21524,.F.);
#31446=ORIENTED_EDGE('',*,*,#21508,.F.);
#31447=ORIENTED_EDGE('',*,*,#21525,.T.);
#31448=ORIENTED_EDGE('',*,*,#21526,.F.);
#31449=ORIENTED_EDGE('',*,*,#21527,.F.);
#31450=ORIENTED_EDGE('',*,*,#21528,.T.);
#31451=ORIENTED_EDGE('',*,*,#21529,.T.);
#31452=ORIENTED_EDGE('',*,*,#21528,.F.);
#31453=ORIENTED_EDGE('',*,*,#21530,.F.);
#31454=ORIENTED_EDGE('',*,*,#21531,.T.);
#31455=ORIENTED_EDGE('',*,*,#21532,.T.);
#31456=ORIENTED_EDGE('',*,*,#21533,.T.);
#31457=ORIENTED_EDGE('',*,*,#21534,.F.);
#31458=ORIENTED_EDGE('',*,*,#21535,.T.);
#31459=ORIENTED_EDGE('',*,*,#21535,.F.);
#31460=ORIENTED_EDGE('',*,*,#21536,.T.);
#31461=ORIENTED_EDGE('',*,*,#21537,.F.);
#31462=ORIENTED_EDGE('',*,*,#21538,.F.);
#31463=ORIENTED_EDGE('',*,*,#21536,.F.);
#31464=ORIENTED_EDGE('',*,*,#21534,.T.);
#31465=ORIENTED_EDGE('',*,*,#21539,.F.);
#31466=ORIENTED_EDGE('',*,*,#21540,.T.);
#31467=ORIENTED_EDGE('',*,*,#21539,.T.);
#31468=ORIENTED_EDGE('',*,*,#21533,.F.);
#31469=ORIENTED_EDGE('',*,*,#21541,.T.);
#31470=ORIENTED_EDGE('',*,*,#21542,.F.);
#31471=ORIENTED_EDGE('',*,*,#21541,.F.);
#31472=ORIENTED_EDGE('',*,*,#21532,.F.);
#31473=ORIENTED_EDGE('',*,*,#21543,.T.);
#31474=ORIENTED_EDGE('',*,*,#21544,.T.);
#31475=ORIENTED_EDGE('',*,*,#21543,.F.);
#31476=ORIENTED_EDGE('',*,*,#21531,.F.);
#31477=ORIENTED_EDGE('',*,*,#21545,.T.);
#31478=ORIENTED_EDGE('',*,*,#21546,.T.);
#31479=ORIENTED_EDGE('',*,*,#21547,.T.);
#31480=ORIENTED_EDGE('',*,*,#21548,.F.);
#31481=ORIENTED_EDGE('',*,*,#21549,.F.);
#31482=ORIENTED_EDGE('',*,*,#21550,.T.);
#31483=ORIENTED_EDGE('',*,*,#21551,.T.);
#31484=ORIENTED_EDGE('',*,*,#21546,.F.);
#31485=ORIENTED_EDGE('',*,*,#21552,.F.);
#31486=ORIENTED_EDGE('',*,*,#21547,.F.);
#31487=ORIENTED_EDGE('',*,*,#21551,.F.);
#31488=ORIENTED_EDGE('',*,*,#21553,.F.);
#31489=ORIENTED_EDGE('',*,*,#21553,.T.);
#31490=ORIENTED_EDGE('',*,*,#21550,.F.);
#31491=ORIENTED_EDGE('',*,*,#21554,.T.);
#31492=ORIENTED_EDGE('',*,*,#21555,.T.);
#31493=ORIENTED_EDGE('',*,*,#21556,.T.);
#31494=ORIENTED_EDGE('',*,*,#21554,.F.);
#31495=ORIENTED_EDGE('',*,*,#21549,.T.);
#31496=ORIENTED_EDGE('',*,*,#21557,.T.);
#31497=ORIENTED_EDGE('',*,*,#21558,.F.);
#31498=ORIENTED_EDGE('',*,*,#21559,.F.);
#31499=ORIENTED_EDGE('',*,*,#21560,.T.);
#31500=ORIENTED_EDGE('',*,*,#21561,.F.);
#31501=ORIENTED_EDGE('',*,*,#21562,.T.);
#31502=ORIENTED_EDGE('',*,*,#21561,.T.);
#31503=ORIENTED_EDGE('',*,*,#21563,.T.);
#31504=ORIENTED_EDGE('',*,*,#21563,.F.);
#31505=ORIENTED_EDGE('',*,*,#21560,.F.);
#31506=ORIENTED_EDGE('',*,*,#21564,.F.);
#31507=ORIENTED_EDGE('',*,*,#21565,.F.);
#31508=ORIENTED_EDGE('',*,*,#21564,.T.);
#31509=ORIENTED_EDGE('',*,*,#21559,.T.);
#31510=ORIENTED_EDGE('',*,*,#21566,.T.);
#31511=ORIENTED_EDGE('',*,*,#21567,.T.);
#31512=ORIENTED_EDGE('',*,*,#21568,.T.);
#31513=ORIENTED_EDGE('',*,*,#21566,.F.);
#31514=ORIENTED_EDGE('',*,*,#21558,.T.);
#31515=ORIENTED_EDGE('',*,*,#21569,.T.);
#31516=ORIENTED_EDGE('',*,*,#21570,.F.);
#31517=ORIENTED_EDGE('',*,*,#21571,.T.);
#31518=ORIENTED_EDGE('',*,*,#21572,.T.);
#31519=ORIENTED_EDGE('',*,*,#21573,.T.);
#31520=ORIENTED_EDGE('',*,*,#21574,.T.);
#31521=ORIENTED_EDGE('',*,*,#21575,.T.);
#31522=ORIENTED_EDGE('',*,*,#21576,.F.);
#31523=ORIENTED_EDGE('',*,*,#21570,.T.);
#31524=ORIENTED_EDGE('',*,*,#21571,.F.);
#31525=ORIENTED_EDGE('',*,*,#21576,.T.);
#31526=ORIENTED_EDGE('',*,*,#21577,.T.);
#31527=ORIENTED_EDGE('',*,*,#21578,.T.);
#31528=ORIENTED_EDGE('',*,*,#21579,.T.);
#31529=ORIENTED_EDGE('',*,*,#21577,.F.);
#31530=ORIENTED_EDGE('',*,*,#21575,.F.);
#31531=ORIENTED_EDGE('',*,*,#21580,.F.);
#31532=ORIENTED_EDGE('',*,*,#21581,.T.);
#31533=ORIENTED_EDGE('',*,*,#21580,.T.);
#31534=ORIENTED_EDGE('',*,*,#21574,.F.);
#31535=ORIENTED_EDGE('',*,*,#21582,.T.);
#31536=ORIENTED_EDGE('',*,*,#21582,.F.);
#31537=ORIENTED_EDGE('',*,*,#21573,.F.);
#31538=ORIENTED_EDGE('',*,*,#21583,.F.);
#31539=ORIENTED_EDGE('',*,*,#21584,.T.);
#31540=ORIENTED_EDGE('',*,*,#21585,.F.);
#31541=ORIENTED_EDGE('',*,*,#21586,.T.);
#31542=ORIENTED_EDGE('',*,*,#21587,.T.);
#31543=ORIENTED_EDGE('',*,*,#21498,.F.);
#31544=ORIENTED_EDGE('',*,*,#21588,.F.);
#31545=ORIENTED_EDGE('',*,*,#21586,.F.);
#31546=ORIENTED_EDGE('',*,*,#21589,.F.);
#31547=ORIENTED_EDGE('',*,*,#21584,.F.);
#31548=ORIENTED_EDGE('',*,*,#21590,.T.);
#31549=ORIENTED_EDGE('',*,*,#21476,.F.);
#31550=ORIENTED_EDGE('',*,*,#21591,.T.);
#31551=ORIENTED_EDGE('',*,*,#21592,.F.);
#31552=ORIENTED_EDGE('',*,*,#21593,.F.);
#31553=ORIENTED_EDGE('',*,*,#21594,.F.);
#31554=ORIENTED_EDGE('',*,*,#21595,.F.);
#31555=ORIENTED_EDGE('',*,*,#21585,.T.);
#31556=ORIENTED_EDGE('',*,*,#21591,.F.);
#31557=ORIENTED_EDGE('',*,*,#21596,.F.);
#31558=ORIENTED_EDGE('',*,*,#21590,.F.);
#31559=ORIENTED_EDGE('',*,*,#21588,.T.);
#31560=ORIENTED_EDGE('',*,*,#21597,.T.);
#31561=ORIENTED_EDGE('',*,*,#21589,.T.);
#31562=ORIENTED_EDGE('',*,*,#21587,.F.);
#31563=ORIENTED_EDGE('',*,*,#21598,.F.);
#31564=ORIENTED_EDGE('',*,*,#21599,.T.);
#31565=ORIENTED_EDGE('',*,*,#21592,.T.);
#31566=ORIENTED_EDGE('',*,*,#21600,.T.);
#31567=ORIENTED_EDGE('',*,*,#21601,.F.);
#31568=ORIENTED_EDGE('',*,*,#21600,.F.);
#31569=ORIENTED_EDGE('',*,*,#21595,.T.);
#31570=ORIENTED_EDGE('',*,*,#21602,.T.);
#31571=ORIENTED_EDGE('',*,*,#21603,.T.);
#31572=ORIENTED_EDGE('',*,*,#21604,.F.);
#31573=ORIENTED_EDGE('',*,*,#21602,.F.);
#31574=ORIENTED_EDGE('',*,*,#21594,.T.);
#31575=ORIENTED_EDGE('',*,*,#21603,.F.);
#31576=ORIENTED_EDGE('',*,*,#21593,.T.);
#31577=ORIENTED_EDGE('',*,*,#21599,.F.);
#31578=ORIENTED_EDGE('',*,*,#21605,.F.);
#31579=ORIENTED_EDGE('',*,*,#21606,.T.);
#31580=ORIENTED_EDGE('',*,*,#21607,.T.);
#31581=ORIENTED_EDGE('',*,*,#21608,.T.);
#31582=ORIENTED_EDGE('',*,*,#21609,.T.);
#31583=ORIENTED_EDGE('',*,*,#21607,.F.);
#31584=ORIENTED_EDGE('',*,*,#21610,.T.);
#31585=ORIENTED_EDGE('',*,*,#21611,.F.);
#31586=ORIENTED_EDGE('',*,*,#21612,.T.);
#31587=ORIENTED_EDGE('',*,*,#21611,.T.);
#31588=ORIENTED_EDGE('',*,*,#21613,.T.);
#31589=ORIENTED_EDGE('',*,*,#21614,.T.);
#31590=ORIENTED_EDGE('',*,*,#21615,.F.);
#31591=ORIENTED_EDGE('',*,*,#21614,.F.);
#31592=ORIENTED_EDGE('',*,*,#21616,.F.);
#31593=ORIENTED_EDGE('',*,*,#21617,.F.);
#31594=ORIENTED_EDGE('',*,*,#21618,.T.);
#31595=ORIENTED_EDGE('',*,*,#21619,.T.);
#31596=ORIENTED_EDGE('',*,*,#21620,.T.);
#31597=ORIENTED_EDGE('',*,*,#21617,.T.);
#31598=ORIENTED_EDGE('',*,*,#21621,.T.);
#31599=ORIENTED_EDGE('',*,*,#21622,.F.);
#31600=ORIENTED_EDGE('',*,*,#21623,.F.);
#31601=ORIENTED_EDGE('',*,*,#21624,.F.);
#31602=ORIENTED_EDGE('',*,*,#21625,.F.);
#31603=ORIENTED_EDGE('',*,*,#21623,.T.);
#31604=ORIENTED_EDGE('',*,*,#21626,.F.);
#31605=ORIENTED_EDGE('',*,*,#21627,.T.);
#31606=ORIENTED_EDGE('',*,*,#21628,.T.);
#31607=ORIENTED_EDGE('',*,*,#21629,.T.);
#31608=ORIENTED_EDGE('',*,*,#21627,.F.);
#31609=ORIENTED_EDGE('',*,*,#21630,.F.);
#31610=ORIENTED_EDGE('',*,*,#21631,.F.);
#31611=ORIENTED_EDGE('',*,*,#21631,.T.);
#31612=ORIENTED_EDGE('',*,*,#21632,.T.);
#31613=ORIENTED_EDGE('',*,*,#21633,.T.);
#31614=ORIENTED_EDGE('',*,*,#21634,.F.);
#31615=ORIENTED_EDGE('',*,*,#21635,.F.);
#31616=ORIENTED_EDGE('',*,*,#21636,.F.);
#31617=ORIENTED_EDGE('',*,*,#21636,.T.);
#31618=ORIENTED_EDGE('',*,*,#21637,.T.);
#31619=ORIENTED_EDGE('',*,*,#21638,.T.);
#31620=ORIENTED_EDGE('',*,*,#21639,.T.);
#31621=ORIENTED_EDGE('',*,*,#21638,.F.);
#31622=ORIENTED_EDGE('',*,*,#21640,.F.);
#31623=ORIENTED_EDGE('',*,*,#21641,.T.);
#31624=ORIENTED_EDGE('',*,*,#21642,.F.);
#31625=ORIENTED_EDGE('',*,*,#21643,.F.);
#31626=ORIENTED_EDGE('',*,*,#21644,.T.);
#31627=ORIENTED_EDGE('',*,*,#21645,.F.);
#31628=ORIENTED_EDGE('',*,*,#21646,.F.);
#31629=ORIENTED_EDGE('',*,*,#21647,.F.);
#31630=ORIENTED_EDGE('',*,*,#21644,.F.);
#31631=ORIENTED_EDGE('',*,*,#21648,.T.);
#31632=ORIENTED_EDGE('',*,*,#21649,.T.);
#31633=ORIENTED_EDGE('',*,*,#21650,.F.);
#31634=ORIENTED_EDGE('',*,*,#21651,.T.);
#31635=ORIENTED_EDGE('',*,*,#21646,.T.);
#31636=ORIENTED_EDGE('',*,*,#21652,.T.);
#31637=ORIENTED_EDGE('',*,*,#21520,.T.);
#31638=ORIENTED_EDGE('',*,*,#21653,.F.);
#31639=ORIENTED_EDGE('',*,*,#21654,.F.);
#31640=ORIENTED_EDGE('',*,*,#21655,.T.);
#31641=ORIENTED_EDGE('',*,*,#21656,.T.);
#31642=ORIENTED_EDGE('',*,*,#21657,.T.);
#31643=ORIENTED_EDGE('',*,*,#21658,.T.);
#31644=ORIENTED_EDGE('',*,*,#21659,.F.);
#31645=ORIENTED_EDGE('',*,*,#21660,.T.);
#31646=ORIENTED_EDGE('',*,*,#21661,.F.);
#31647=ORIENTED_EDGE('',*,*,#21662,.T.);
#31648=ORIENTED_EDGE('',*,*,#21663,.T.);
#31649=ORIENTED_EDGE('',*,*,#21664,.T.);
#31650=ORIENTED_EDGE('',*,*,#21665,.T.);
#31651=ORIENTED_EDGE('',*,*,#21666,.F.);
#31652=ORIENTED_EDGE('',*,*,#21667,.T.);
#31653=ORIENTED_EDGE('',*,*,#21668,.F.);
#31654=ORIENTED_EDGE('',*,*,#21669,.T.);
#31655=ORIENTED_EDGE('',*,*,#21670,.T.);
#31656=ORIENTED_EDGE('',*,*,#21671,.T.);
#31657=ORIENTED_EDGE('',*,*,#21672,.T.);
#31658=ORIENTED_EDGE('',*,*,#21673,.F.);
#31659=ORIENTED_EDGE('',*,*,#21674,.T.);
#31660=ORIENTED_EDGE('',*,*,#21675,.F.);
#31661=ORIENTED_EDGE('',*,*,#21676,.F.);
#31662=ORIENTED_EDGE('',*,*,#21677,.T.);
#31663=ORIENTED_EDGE('',*,*,#21678,.T.);
#31664=ORIENTED_EDGE('',*,*,#21679,.T.);
#31665=ORIENTED_EDGE('',*,*,#21680,.T.);
#31666=ORIENTED_EDGE('',*,*,#21598,.T.);
#31667=ORIENTED_EDGE('',*,*,#21601,.T.);
#31668=ORIENTED_EDGE('',*,*,#21604,.T.);
#31669=ORIENTED_EDGE('',*,*,#21605,.T.);
#31670=ORIENTED_EDGE('',*,*,#21439,.F.);
#31671=ORIENTED_EDGE('',*,*,#21681,.T.);
#31672=ORIENTED_EDGE('',*,*,#21654,.T.);
#31673=ORIENTED_EDGE('',*,*,#21682,.T.);
#31674=ORIENTED_EDGE('',*,*,#21683,.T.);
#31675=ORIENTED_EDGE('',*,*,#21684,.T.);
#31676=ORIENTED_EDGE('',*,*,#21685,.T.);
#31677=ORIENTED_EDGE('',*,*,#21686,.T.);
#31678=ORIENTED_EDGE('',*,*,#21441,.F.);
#31679=ORIENTED_EDGE('',*,*,#21501,.F.);
#31680=ORIENTED_EDGE('',*,*,#21500,.T.);
#31681=ORIENTED_EDGE('',*,*,#21499,.F.);
#31682=ORIENTED_EDGE('',*,*,#21597,.F.);
#31683=ORIENTED_EDGE('',*,*,#21497,.F.);
#31684=ORIENTED_EDGE('',*,*,#21496,.T.);
#31685=ORIENTED_EDGE('',*,*,#21495,.T.);
#31686=ORIENTED_EDGE('',*,*,#21494,.F.);
#31687=ORIENTED_EDGE('',*,*,#21493,.F.);
#31688=ORIENTED_EDGE('',*,*,#21492,.F.);
#31689=ORIENTED_EDGE('',*,*,#21491,.T.);
#31690=ORIENTED_EDGE('',*,*,#21490,.F.);
#31691=ORIENTED_EDGE('',*,*,#21489,.T.);
#31692=ORIENTED_EDGE('',*,*,#21488,.F.);
#31693=ORIENTED_EDGE('',*,*,#21487,.F.);
#31694=ORIENTED_EDGE('',*,*,#21486,.T.);
#31695=ORIENTED_EDGE('',*,*,#21485,.T.);
#31696=ORIENTED_EDGE('',*,*,#21484,.F.);
#31697=ORIENTED_EDGE('',*,*,#21483,.F.);
#31698=ORIENTED_EDGE('',*,*,#21482,.T.);
#31699=ORIENTED_EDGE('',*,*,#21481,.F.);
#31700=ORIENTED_EDGE('',*,*,#21480,.F.);
#31701=ORIENTED_EDGE('',*,*,#21479,.T.);
#31702=ORIENTED_EDGE('',*,*,#21478,.T.);
#31703=ORIENTED_EDGE('',*,*,#21477,.T.);
#31704=ORIENTED_EDGE('',*,*,#21596,.T.);
#31705=ORIENTED_EDGE('',*,*,#21475,.T.);
#31706=ORIENTED_EDGE('',*,*,#21474,.T.);
#31707=ORIENTED_EDGE('',*,*,#21473,.F.);
#31708=ORIENTED_EDGE('',*,*,#21687,.T.);
#31709=ORIENTED_EDGE('',*,*,#21656,.F.);
#31710=ORIENTED_EDGE('',*,*,#21688,.T.);
#31711=ORIENTED_EDGE('',*,*,#21689,.T.);
#31712=ORIENTED_EDGE('',*,*,#21690,.F.);
#31713=ORIENTED_EDGE('',*,*,#21691,.T.);
#31714=ORIENTED_EDGE('',*,*,#21688,.F.);
#31715=ORIENTED_EDGE('',*,*,#21655,.F.);
#31716=ORIENTED_EDGE('',*,*,#21692,.T.);
#31717=ORIENTED_EDGE('',*,*,#21690,.T.);
#31718=ORIENTED_EDGE('',*,*,#21680,.F.);
#31719=ORIENTED_EDGE('',*,*,#21693,.F.);
#31720=ORIENTED_EDGE('',*,*,#21679,.F.);
#31721=ORIENTED_EDGE('',*,*,#21694,.T.);
#31722=ORIENTED_EDGE('',*,*,#21695,.T.);
#31723=ORIENTED_EDGE('',*,*,#21693,.T.);
#31724=ORIENTED_EDGE('',*,*,#21696,.F.);
#31725=ORIENTED_EDGE('',*,*,#21697,.T.);
#31726=ORIENTED_EDGE('',*,*,#21694,.F.);
#31727=ORIENTED_EDGE('',*,*,#21678,.F.);
#31728=ORIENTED_EDGE('',*,*,#21698,.F.);
#31729=ORIENTED_EDGE('',*,*,#21699,.F.);
#31730=ORIENTED_EDGE('',*,*,#21696,.T.);
#31731=ORIENTED_EDGE('',*,*,#21677,.F.);
#31732=ORIENTED_EDGE('',*,*,#21698,.T.);
#31733=ORIENTED_EDGE('',*,*,#21676,.T.);
#31734=ORIENTED_EDGE('',*,*,#21700,.T.);
#31735=ORIENTED_EDGE('',*,*,#21701,.T.);
#31736=ORIENTED_EDGE('',*,*,#21702,.T.);
#31737=ORIENTED_EDGE('',*,*,#21700,.F.);
#31738=ORIENTED_EDGE('',*,*,#21675,.T.);
#31739=ORIENTED_EDGE('',*,*,#21703,.T.);
#31740=ORIENTED_EDGE('',*,*,#21704,.T.);
#31741=ORIENTED_EDGE('',*,*,#21703,.F.);
#31742=ORIENTED_EDGE('',*,*,#21674,.F.);
#31743=ORIENTED_EDGE('',*,*,#21705,.T.);
#31744=ORIENTED_EDGE('',*,*,#21706,.T.);
#31745=ORIENTED_EDGE('',*,*,#21705,.F.);
#31746=ORIENTED_EDGE('',*,*,#21673,.T.);
#31747=ORIENTED_EDGE('',*,*,#21707,.F.);
#31748=ORIENTED_EDGE('',*,*,#21708,.F.);
#31749=ORIENTED_EDGE('',*,*,#21709,.F.);
#31750=ORIENTED_EDGE('',*,*,#21707,.T.);
#31751=ORIENTED_EDGE('',*,*,#21672,.F.);
#31752=ORIENTED_EDGE('',*,*,#21671,.F.);
#31753=ORIENTED_EDGE('',*,*,#21710,.F.);
#31754=ORIENTED_EDGE('',*,*,#21711,.T.);
#31755=ORIENTED_EDGE('',*,*,#21708,.T.);
#31756=ORIENTED_EDGE('',*,*,#21712,.F.);
#31757=ORIENTED_EDGE('',*,*,#21713,.F.);
#31758=ORIENTED_EDGE('',*,*,#21710,.T.);
#31759=ORIENTED_EDGE('',*,*,#21670,.F.);
#31760=ORIENTED_EDGE('',*,*,#21714,.T.);
#31761=ORIENTED_EDGE('',*,*,#21712,.T.);
#31762=ORIENTED_EDGE('',*,*,#21669,.F.);
#31763=ORIENTED_EDGE('',*,*,#21715,.T.);
#31764=ORIENTED_EDGE('',*,*,#21716,.T.);
#31765=ORIENTED_EDGE('',*,*,#21715,.F.);
#31766=ORIENTED_EDGE('',*,*,#21668,.T.);
#31767=ORIENTED_EDGE('',*,*,#21717,.T.);
#31768=ORIENTED_EDGE('',*,*,#21667,.F.);
#31769=ORIENTED_EDGE('',*,*,#21718,.T.);
#31770=ORIENTED_EDGE('',*,*,#21719,.T.);
#31771=ORIENTED_EDGE('',*,*,#21717,.F.);
#31772=ORIENTED_EDGE('',*,*,#21720,.T.);
#31773=ORIENTED_EDGE('',*,*,#21718,.F.);
#31774=ORIENTED_EDGE('',*,*,#21666,.T.);
#31775=ORIENTED_EDGE('',*,*,#21721,.T.);
#31776=ORIENTED_EDGE('',*,*,#21722,.F.);
#31777=ORIENTED_EDGE('',*,*,#21723,.T.);
#31778=ORIENTED_EDGE('',*,*,#21721,.F.);
#31779=ORIENTED_EDGE('',*,*,#21665,.F.);
#31780=ORIENTED_EDGE('',*,*,#21724,.F.);
#31781=ORIENTED_EDGE('',*,*,#21725,.F.);
#31782=ORIENTED_EDGE('',*,*,#21722,.T.);
#31783=ORIENTED_EDGE('',*,*,#21664,.F.);
#31784=ORIENTED_EDGE('',*,*,#21663,.F.);
#31785=ORIENTED_EDGE('',*,*,#21726,.F.);
#31786=ORIENTED_EDGE('',*,*,#21727,.T.);
#31787=ORIENTED_EDGE('',*,*,#21724,.T.);
#31788=ORIENTED_EDGE('',*,*,#21728,.T.);
#31789=ORIENTED_EDGE('',*,*,#21729,.F.);
#31790=ORIENTED_EDGE('',*,*,#21726,.T.);
#31791=ORIENTED_EDGE('',*,*,#21662,.F.);
#31792=ORIENTED_EDGE('',*,*,#21730,.T.);
#31793=ORIENTED_EDGE('',*,*,#21728,.F.);
#31794=ORIENTED_EDGE('',*,*,#21661,.T.);
#31795=ORIENTED_EDGE('',*,*,#21731,.T.);
#31796=ORIENTED_EDGE('',*,*,#21660,.F.);
#31797=ORIENTED_EDGE('',*,*,#21732,.T.);
#31798=ORIENTED_EDGE('',*,*,#21733,.T.);
#31799=ORIENTED_EDGE('',*,*,#21731,.F.);
#31800=ORIENTED_EDGE('',*,*,#21734,.T.);
#31801=ORIENTED_EDGE('',*,*,#21732,.F.);
#31802=ORIENTED_EDGE('',*,*,#21659,.T.);
#31803=ORIENTED_EDGE('',*,*,#21735,.T.);
#31804=ORIENTED_EDGE('',*,*,#21736,.F.);
#31805=ORIENTED_EDGE('',*,*,#21737,.T.);
#31806=ORIENTED_EDGE('',*,*,#21735,.F.);
#31807=ORIENTED_EDGE('',*,*,#21658,.F.);
#31808=ORIENTED_EDGE('',*,*,#21687,.F.);
#31809=ORIENTED_EDGE('',*,*,#21738,.F.);
#31810=ORIENTED_EDGE('',*,*,#21736,.T.);
#31811=ORIENTED_EDGE('',*,*,#21657,.F.);
#31812=ORIENTED_EDGE('',*,*,#21739,.T.);
#31813=ORIENTED_EDGE('',*,*,#21740,.F.);
#31814=ORIENTED_EDGE('',*,*,#21641,.F.);
#31815=ORIENTED_EDGE('',*,*,#21740,.T.);
#31816=ORIENTED_EDGE('',*,*,#21741,.F.);
#31817=ORIENTED_EDGE('',*,*,#21634,.T.);
#31818=ORIENTED_EDGE('',*,*,#21639,.F.);
#31819=ORIENTED_EDGE('',*,*,#21642,.T.);
#31820=ORIENTED_EDGE('',*,*,#21742,.F.);
#31821=ORIENTED_EDGE('',*,*,#21743,.F.);
#31822=ORIENTED_EDGE('',*,*,#21624,.T.);
#31823=ORIENTED_EDGE('',*,*,#21628,.F.);
#31824=ORIENTED_EDGE('',*,*,#21629,.F.);
#31825=ORIENTED_EDGE('',*,*,#21633,.F.);
#31826=ORIENTED_EDGE('',*,*,#21743,.T.);
#31827=ORIENTED_EDGE('',*,*,#21744,.T.);
#31828=ORIENTED_EDGE('',*,*,#21625,.T.);
#31829=ORIENTED_EDGE('',*,*,#21745,.T.);
#31830=ORIENTED_EDGE('',*,*,#21746,.T.);
#31831=ORIENTED_EDGE('',*,*,#21619,.F.);
#31832=ORIENTED_EDGE('',*,*,#21746,.F.);
#31833=ORIENTED_EDGE('',*,*,#21747,.T.);
#31834=ORIENTED_EDGE('',*,*,#21612,.F.);
#31835=ORIENTED_EDGE('',*,*,#21615,.T.);
#31836=ORIENTED_EDGE('',*,*,#21618,.F.);
#31837=ORIENTED_EDGE('',*,*,#21620,.F.);
#31838=ORIENTED_EDGE('',*,*,#21517,.F.);
#31839=ORIENTED_EDGE('',*,*,#21457,.T.);
#31840=ORIENTED_EDGE('',*,*,#21445,.F.);
#31841=ORIENTED_EDGE('',*,*,#21452,.F.);
#31842=ORIENTED_EDGE('',*,*,#21519,.F.);
#31843=ORIENTED_EDGE('',*,*,#21748,.T.);
#31844=ORIENTED_EDGE('',*,*,#21749,.F.);
#31845=ORIENTED_EDGE('',*,*,#21748,.F.);
#31846=ORIENTED_EDGE('',*,*,#21518,.F.);
#31847=ORIENTED_EDGE('',*,*,#21468,.T.);
#31848=ORIENTED_EDGE('',*,*,#21461,.F.);
#31849=ORIENTED_EDGE('',*,*,#21464,.F.);
#31850=ORIENTED_EDGE('',*,*,#21568,.F.);
#31851=ORIENTED_EDGE('',*,*,#21557,.F.);
#31852=ORIENTED_EDGE('',*,*,#21562,.F.);
#31853=ORIENTED_EDGE('',*,*,#21565,.T.);
#31854=ORIENTED_EDGE('',*,*,#21567,.F.);
#31855=ORIENTED_EDGE('',*,*,#21552,.T.);
#31856=ORIENTED_EDGE('',*,*,#21555,.F.);
#31857=ORIENTED_EDGE('',*,*,#21556,.F.);
#31858=ORIENTED_EDGE('',*,*,#21548,.T.);
#31859=ORIENTED_EDGE('',*,*,#21545,.F.);
#31860=ORIENTED_EDGE('',*,*,#21537,.T.);
#31861=ORIENTED_EDGE('',*,*,#21538,.T.);
#31862=ORIENTED_EDGE('',*,*,#21540,.F.);
#31863=ORIENTED_EDGE('',*,*,#21542,.T.);
#31864=ORIENTED_EDGE('',*,*,#21544,.F.);
#31865=ORIENTED_EDGE('',*,*,#21530,.T.);
#31866=ORIENTED_EDGE('',*,*,#21526,.T.);
#31867=ORIENTED_EDGE('',*,*,#21527,.T.);
#31868=ORIENTED_EDGE('',*,*,#21578,.F.);
#31869=ORIENTED_EDGE('',*,*,#21579,.F.);
#31870=ORIENTED_EDGE('',*,*,#21581,.F.);
#31871=ORIENTED_EDGE('',*,*,#21583,.T.);
#31872=ORIENTED_EDGE('',*,*,#21572,.F.);
#31873=ORIENTED_EDGE('',*,*,#21569,.F.);
#31874=ORIENTED_EDGE('',*,*,#21640,.T.);
#31875=ORIENTED_EDGE('',*,*,#21637,.F.);
#31876=ORIENTED_EDGE('',*,*,#21635,.T.);
#31877=ORIENTED_EDGE('',*,*,#21741,.T.);
#31878=ORIENTED_EDGE('',*,*,#21739,.F.);
#31879=ORIENTED_EDGE('',*,*,#21750,.F.);
#31880=ORIENTED_EDGE('',*,*,#21751,.F.);
#31881=ORIENTED_EDGE('',*,*,#21645,.T.);
#31882=ORIENTED_EDGE('',*,*,#21647,.T.);
#31883=ORIENTED_EDGE('',*,*,#21651,.F.);
#31884=ORIENTED_EDGE('',*,*,#21747,.F.);
#31885=ORIENTED_EDGE('',*,*,#21745,.F.);
#31886=ORIENTED_EDGE('',*,*,#21621,.F.);
#31887=ORIENTED_EDGE('',*,*,#21616,.T.);
#31888=ORIENTED_EDGE('',*,*,#21613,.F.);
#31889=ORIENTED_EDGE('',*,*,#21610,.F.);
#31890=ORIENTED_EDGE('',*,*,#21744,.F.);
#31891=ORIENTED_EDGE('',*,*,#21742,.T.);
#31892=ORIENTED_EDGE('',*,*,#21632,.F.);
#31893=ORIENTED_EDGE('',*,*,#21630,.T.);
#31894=ORIENTED_EDGE('',*,*,#21626,.T.);
#31895=ORIENTED_EDGE('',*,*,#21622,.T.);
#31896=ORIENTED_EDGE('',*,*,#21609,.F.);
#31897=ORIENTED_EDGE('',*,*,#21608,.F.);
#31898=ORIENTED_EDGE('',*,*,#21751,.T.);
#31899=ORIENTED_EDGE('',*,*,#21752,.T.);
#31900=ORIENTED_EDGE('',*,*,#21649,.F.);
#31901=ORIENTED_EDGE('',*,*,#21648,.F.);
#31902=ORIENTED_EDGE('',*,*,#21643,.T.);
#31903=ORIENTED_EDGE('',*,*,#21752,.F.);
#31904=ORIENTED_EDGE('',*,*,#21750,.T.);
#31905=ORIENTED_EDGE('',*,*,#21650,.T.);
#31906=ORIENTED_EDGE('',*,*,#21653,.T.);
#31907=ORIENTED_EDGE('',*,*,#21753,.T.);
#31908=ORIENTED_EDGE('',*,*,#21754,.F.);
#31909=ORIENTED_EDGE('',*,*,#21682,.F.);
#31910=ORIENTED_EDGE('',*,*,#21753,.F.);
#31911=ORIENTED_EDGE('',*,*,#21525,.F.);
#31912=ORIENTED_EDGE('',*,*,#21507,.T.);
#31913=ORIENTED_EDGE('',*,*,#21755,.T.);
#31914=ORIENTED_EDGE('',*,*,#21754,.T.);
#31915=ORIENTED_EDGE('',*,*,#21756,.T.);
#31916=ORIENTED_EDGE('',*,*,#21757,.F.);
#31917=ORIENTED_EDGE('',*,*,#21683,.F.);
#31918=ORIENTED_EDGE('',*,*,#21756,.F.);
#31919=ORIENTED_EDGE('',*,*,#21755,.F.);
#31920=ORIENTED_EDGE('',*,*,#21506,.F.);
#31921=ORIENTED_EDGE('',*,*,#21758,.T.);
#31922=ORIENTED_EDGE('',*,*,#21757,.T.);
#31923=ORIENTED_EDGE('',*,*,#21759,.T.);
#31924=ORIENTED_EDGE('',*,*,#21760,.F.);
#31925=ORIENTED_EDGE('',*,*,#21684,.F.);
#31926=ORIENTED_EDGE('',*,*,#21759,.F.);
#31927=ORIENTED_EDGE('',*,*,#21758,.F.);
#31928=ORIENTED_EDGE('',*,*,#21505,.T.);
#31929=ORIENTED_EDGE('',*,*,#21761,.T.);
#31930=ORIENTED_EDGE('',*,*,#21760,.T.);
#31931=ORIENTED_EDGE('',*,*,#21762,.T.);
#31932=ORIENTED_EDGE('',*,*,#21763,.F.);
#31933=ORIENTED_EDGE('',*,*,#21685,.F.);
#31934=ORIENTED_EDGE('',*,*,#21761,.F.);
#31935=ORIENTED_EDGE('',*,*,#21516,.T.);
#31936=ORIENTED_EDGE('',*,*,#21764,.T.);
#31937=ORIENTED_EDGE('',*,*,#21762,.F.);
#31938=ORIENTED_EDGE('',*,*,#21606,.F.);
#31939=ORIENTED_EDGE('',*,*,#21765,.T.);
#31940=ORIENTED_EDGE('',*,*,#21766,.T.);
#31941=ORIENTED_EDGE('',*,*,#21767,.F.);
#31942=ORIENTED_EDGE('',*,*,#21504,.F.);
#31943=ORIENTED_EDGE('',*,*,#21442,.T.);
#31944=ORIENTED_EDGE('',*,*,#21768,.T.);
#31945=ORIENTED_EDGE('',*,*,#21765,.F.);
#31946=ORIENTED_EDGE('',*,*,#21686,.F.);
#31947=ORIENTED_EDGE('',*,*,#21763,.T.);
#31948=ORIENTED_EDGE('',*,*,#21769,.T.);
#31949=ORIENTED_EDGE('',*,*,#21768,.F.);
#31950=ORIENTED_EDGE('',*,*,#21766,.F.);
#31951=ORIENTED_EDGE('',*,*,#21769,.F.);
#31952=ORIENTED_EDGE('',*,*,#21764,.F.);
#31953=ORIENTED_EDGE('',*,*,#21515,.T.);
#31954=ORIENTED_EDGE('',*,*,#21770,.T.);
#31955=ORIENTED_EDGE('',*,*,#21767,.T.);
#31956=ORIENTED_EDGE('',*,*,#21771,.T.);
#31957=ORIENTED_EDGE('',*,*,#21772,.F.);
#31958=ORIENTED_EDGE('',*,*,#21502,.F.);
#31959=ORIENTED_EDGE('',*,*,#21770,.F.);
#31960=ORIENTED_EDGE('',*,*,#21514,.T.);
#31961=ORIENTED_EDGE('',*,*,#21773,.T.);
#31962=ORIENTED_EDGE('',*,*,#21771,.F.);
#31963=ORIENTED_EDGE('',*,*,#21772,.T.);
#31964=ORIENTED_EDGE('',*,*,#21774,.T.);
#31965=ORIENTED_EDGE('',*,*,#21775,.F.);
#31966=ORIENTED_EDGE('',*,*,#21503,.F.);
#31967=ORIENTED_EDGE('',*,*,#21775,.T.);
#31968=ORIENTED_EDGE('',*,*,#21776,.T.);
#31969=ORIENTED_EDGE('',*,*,#21444,.F.);
#31970=ORIENTED_EDGE('',*,*,#21777,.T.);
#31971=ORIENTED_EDGE('',*,*,#21652,.F.);
#31972=ORIENTED_EDGE('',*,*,#21681,.F.);
#31973=ORIENTED_EDGE('',*,*,#21776,.F.);
#31974=ORIENTED_EDGE('',*,*,#21774,.F.);
#31975=ORIENTED_EDGE('',*,*,#21773,.F.);
#31976=ORIENTED_EDGE('',*,*,#21513,.T.);
#31977=ORIENTED_EDGE('',*,*,#21521,.T.);
#31978=ORIENTED_EDGE('',*,*,#21777,.F.);
#31979=ORIENTED_EDGE('',*,*,#21689,.F.);
#31980=ORIENTED_EDGE('',*,*,#21691,.F.);
#31981=ORIENTED_EDGE('',*,*,#21692,.F.);
#31982=ORIENTED_EDGE('',*,*,#21695,.F.);
#31983=ORIENTED_EDGE('',*,*,#21697,.F.);
#31984=ORIENTED_EDGE('',*,*,#21699,.T.);
#31985=ORIENTED_EDGE('',*,*,#21701,.F.);
#31986=ORIENTED_EDGE('',*,*,#21702,.F.);
#31987=ORIENTED_EDGE('',*,*,#21704,.F.);
#31988=ORIENTED_EDGE('',*,*,#21706,.F.);
#31989=ORIENTED_EDGE('',*,*,#21709,.T.);
#31990=ORIENTED_EDGE('',*,*,#21711,.F.);
#31991=ORIENTED_EDGE('',*,*,#21713,.T.);
#31992=ORIENTED_EDGE('',*,*,#21714,.F.);
#31993=ORIENTED_EDGE('',*,*,#21716,.F.);
#31994=ORIENTED_EDGE('',*,*,#21719,.F.);
#31995=ORIENTED_EDGE('',*,*,#21720,.F.);
#31996=ORIENTED_EDGE('',*,*,#21723,.F.);
#31997=ORIENTED_EDGE('',*,*,#21725,.T.);
#31998=ORIENTED_EDGE('',*,*,#21727,.F.);
#31999=ORIENTED_EDGE('',*,*,#21729,.T.);
#32000=ORIENTED_EDGE('',*,*,#21730,.F.);
#32001=ORIENTED_EDGE('',*,*,#21733,.F.);
#32002=ORIENTED_EDGE('',*,*,#21734,.F.);
#32003=ORIENTED_EDGE('',*,*,#21737,.F.);
#32004=ORIENTED_EDGE('',*,*,#21738,.T.);
#32005=ORIENTED_EDGE('',*,*,#21749,.T.);
#32006=ORIENTED_EDGE('',*,*,#21778,.F.);
#32007=ORIENTED_EDGE('',*,*,#21779,.F.);
#32008=ORIENTED_EDGE('',*,*,#21509,.F.);
#32009=ORIENTED_EDGE('',*,*,#21524,.T.);
#32010=ORIENTED_EDGE('',*,*,#21780,.T.);
#32011=ORIENTED_EDGE('',*,*,#21781,.F.);
#32012=ORIENTED_EDGE('',*,*,#21510,.F.);
#32013=ORIENTED_EDGE('',*,*,#21779,.T.);
#32014=ORIENTED_EDGE('',*,*,#21529,.F.);
#32015=ORIENTED_EDGE('',*,*,#21782,.F.);
#32016=ORIENTED_EDGE('',*,*,#21780,.F.);
#32017=ORIENTED_EDGE('',*,*,#21778,.T.);
#32018=ORIENTED_EDGE('',*,*,#21523,.T.);
#32019=ORIENTED_EDGE('',*,*,#21522,.F.);
#32020=ORIENTED_EDGE('',*,*,#21511,.T.);
#32021=ORIENTED_EDGE('',*,*,#21781,.T.);
#32022=ORIENTED_EDGE('',*,*,#21782,.T.);
#32023=CONICAL_SURFACE('',#34292,0.999999999999103,0.785398163397);
#32024=CONICAL_SURFACE('',#34300,0.999999999999103,0.785398163397);
#32025=CONICAL_SURFACE('',#36201,0.781285626506967,0.663225115758);
#32026=CONICAL_SURFACE('',#36375,16.4,0.785398163397448);
#32027=ADVANCED_FACE('',(#3279),#32023,.T.);
#32028=ADVANCED_FACE('',(#3280),#2521,.T.);
#32029=ADVANCED_FACE('',(#3281),#2082,.F.);
#32030=ADVANCED_FACE('',(#3282),#32024,.T.);
#32031=ADVANCED_FACE('',(#3283),#2083,.T.);
#32032=ADVANCED_FACE('',(#3284),#2522,.T.);
#32033=ADVANCED_FACE('',(#3285,#1254,#1255,#1256),#2084,.T.);
#32034=ADVANCED_FACE('',(#3286),#862,.T.);
#32035=ADVANCED_FACE('',(#3287),#710,.T.);
#32036=ADVANCED_FACE('',(#3288),#2085,.T.);
#32037=ADVANCED_FACE('',(#3289),#863,.T.);
#32038=ADVANCED_FACE('',(#3290),#2523,.F.);
#32039=ADVANCED_FACE('',(#3291),#2086,.T.);
#32040=ADVANCED_FACE('',(#3292),#2524,.F.);
#32041=ADVANCED_FACE('',(#3293),#864,.T.);
#32042=ADVANCED_FACE('',(#3294),#865,.F.);
#32043=ADVANCED_FACE('',(#3295),#866,.T.);
#32044=ADVANCED_FACE('',(#3296),#867,.T.);
#32045=ADVANCED_FACE('',(#3297),#868,.T.);
#32046=ADVANCED_FACE('',(#3298),#2525,.F.);
#32047=ADVANCED_FACE('',(#3299),#2526,.F.);
#32048=ADVANCED_FACE('',(#3300),#869,.F.);
#32049=ADVANCED_FACE('',(#3301),#2527,.F.);
#32050=ADVANCED_FACE('',(#3302),#870,.F.);
#32051=ADVANCED_FACE('',(#3303),#871,.F.);
#32052=ADVANCED_FACE('',(#3304),#872,.F.);
#32053=ADVANCED_FACE('',(#3305),#873,.T.);
#32054=ADVANCED_FACE('',(#3306),#874,.F.);
#32055=ADVANCED_FACE('',(#3307),#2528,.F.);
#32056=ADVANCED_FACE('',(#3308),#2087,.F.);
#32057=ADVANCED_FACE('',(#3309),#2529,.T.);
#32058=ADVANCED_FACE('',(#3310),#66,.T.);
#32059=ADVANCED_FACE('',(#3311),#67,.T.);
#32060=ADVANCED_FACE('',(#3312),#2530,.T.);
#32061=ADVANCED_FACE('',(#3313),#2531,.T.);
#32062=ADVANCED_FACE('',(#3314),#2088,.T.);
#32063=ADVANCED_FACE('',(#3315),#68,.T.);
#32064=ADVANCED_FACE('',(#3316),#2532,.F.);
#32065=ADVANCED_FACE('',(#3317),#2533,.T.);
#32066=ADVANCED_FACE('',(#3318),#2089,.T.);
#32067=ADVANCED_FACE('',(#3319),#69,.T.);
#32068=ADVANCED_FACE('',(#3320),#2534,.F.);
#32069=ADVANCED_FACE('',(#3321),#2535,.T.);
#32070=ADVANCED_FACE('',(#3322),#2090,.F.);
#32071=ADVANCED_FACE('',(#3323),#70,.T.);
#32072=ADVANCED_FACE('',(#3324),#2536,.T.);
#32073=ADVANCED_FACE('',(#3325),#71,.T.);
#32074=ADVANCED_FACE('',(#3326),#2537,.T.);
#32075=ADVANCED_FACE('',(#3327),#72,.T.);
#32076=ADVANCED_FACE('',(#3328),#2538,.T.);
#32077=ADVANCED_FACE('',(#3329),#2539,.T.);
#32078=ADVANCED_FACE('',(#3330),#2091,.F.);
#32079=ADVANCED_FACE('',(#3331),#73,.T.);
#32080=ADVANCED_FACE('',(#3332),#2540,.T.);
#32081=ADVANCED_FACE('',(#3333),#74,.T.);
#32082=ADVANCED_FACE('',(#3334),#2541,.T.);
#32083=ADVANCED_FACE('',(#3335),#75,.T.);
#32084=ADVANCED_FACE('',(#3336),#2542,.T.);
#32085=ADVANCED_FACE('',(#3337),#2543,.T.);
#32086=ADVANCED_FACE('',(#3338),#2092,.T.);
#32087=ADVANCED_FACE('',(#3339),#76,.T.);
#32088=ADVANCED_FACE('',(#3340),#2544,.F.);
#32089=ADVANCED_FACE('',(#3341),#2545,.T.);
#32090=ADVANCED_FACE('',(#3342),#2093,.F.);
#32091=ADVANCED_FACE('',(#3343),#77,.T.);
#32092=ADVANCED_FACE('',(#3344),#2546,.F.);
#32093=ADVANCED_FACE('',(#3345),#2547,.T.);
#32094=ADVANCED_FACE('',(#3346),#2094,.F.);
#32095=ADVANCED_FACE('',(#3347),#78,.T.);
#32096=ADVANCED_FACE('',(#3348),#2548,.T.);
#32097=ADVANCED_FACE('',(#3349),#2549,.T.);
#32098=ADVANCED_FACE('',(#3350),#79,.T.);
#32099=ADVANCED_FACE('',(#3351),#80,.T.);
#32100=ADVANCED_FACE('',(#3352),#2550,.T.);
#32101=ADVANCED_FACE('',(#3353),#2551,.T.);
#32102=ADVANCED_FACE('',(#3354),#2095,.T.);
#32103=ADVANCED_FACE('',(#3355),#81,.T.);
#32104=ADVANCED_FACE('',(#3356),#2552,.F.);
#32105=ADVANCED_FACE('',(#3357),#2553,.T.);
#32106=ADVANCED_FACE('',(#3358),#2096,.T.);
#32107=ADVANCED_FACE('',(#3359),#82,.T.);
#32108=ADVANCED_FACE('',(#3360),#2554,.F.);
#32109=ADVANCED_FACE('',(#3361),#2555,.T.);
#32110=ADVANCED_FACE('',(#3362),#2097,.F.);
#32111=ADVANCED_FACE('',(#3363),#83,.T.);
#32112=ADVANCED_FACE('',(#3364),#2556,.T.);
#32113=ADVANCED_FACE('',(#3365),#84,.T.);
#32114=ADVANCED_FACE('',(#3366),#2557,.T.);
#32115=ADVANCED_FACE('',(#3367),#85,.T.);
#32116=ADVANCED_FACE('',(#3368),#2558,.T.);
#32117=ADVANCED_FACE('',(#3369),#2559,.T.);
#32118=ADVANCED_FACE('',(#3370),#2098,.T.);
#32119=ADVANCED_FACE('',(#3371),#86,.T.);
#32120=ADVANCED_FACE('',(#3372),#2560,.T.);
#32121=ADVANCED_FACE('',(#3373),#87,.T.);
#32122=ADVANCED_FACE('',(#3374),#2561,.T.);
#32123=ADVANCED_FACE('',(#3375),#88,.T.);
#32124=ADVANCED_FACE('',(#3376),#2562,.T.);
#32125=ADVANCED_FACE('',(#3377),#2563,.T.);
#32126=ADVANCED_FACE('',(#3378),#2099,.T.);
#32127=ADVANCED_FACE('',(#3379),#89,.T.);
#32128=ADVANCED_FACE('',(#3380),#2564,.F.);
#32129=ADVANCED_FACE('',(#3381),#2565,.T.);
#32130=ADVANCED_FACE('',(#3382),#2100,.F.);
#32131=ADVANCED_FACE('',(#3383),#90,.T.);
#32132=ADVANCED_FACE('',(#3384),#2566,.T.);
#32133=ADVANCED_FACE('',(#3385),#91,.T.);
#32134=ADVANCED_FACE('',(#3386),#2567,.F.);
#32135=ADVANCED_FACE('',(#3387),#2568,.T.);
#32136=ADVANCED_FACE('',(#3388),#2101,.F.);
#32137=ADVANCED_FACE('',(#3389),#2102,.F.);
#32138=ADVANCED_FACE('',(#3390),#875,.T.);
#32139=ADVANCED_FACE('',(#3391),#2103,.T.);
#32140=ADVANCED_FACE('',(#3392),#876,.T.);
#32141=ADVANCED_FACE('',(#3393),#877,.T.);
#32142=ADVANCED_FACE('',(#3394),#878,.T.);
#32143=ADVANCED_FACE('',(#3395),#879,.T.);
#32144=ADVANCED_FACE('',(#3396),#880,.T.);
#32145=ADVANCED_FACE('',(#3397),#881,.T.);
#32146=ADVANCED_FACE('',(#3398),#882,.T.);
#32147=ADVANCED_FACE('',(#3399),#2104,.F.);
#32148=ADVANCED_FACE('',(#3400),#2105,.T.);
#32149=ADVANCED_FACE('',(#3401),#883,.F.);
#32150=ADVANCED_FACE('',(#3402),#884,.F.);
#32151=ADVANCED_FACE('',(#3403),#885,.F.);
#32152=ADVANCED_FACE('',(#3404),#2569,.T.);
#32153=ADVANCED_FACE('',(#3405),#886,.F.);
#32154=ADVANCED_FACE('',(#3406),#887,.F.);
#32155=ADVANCED_FACE('',(#3407),#888,.F.);
#32156=ADVANCED_FACE('',(#3408),#889,.F.);
#32157=ADVANCED_FACE('',(#3409),#890,.F.);
#32158=ADVANCED_FACE('',(#3410),#891,.F.);
#32159=ADVANCED_FACE('',(#3411),#892,.F.);
#32160=ADVANCED_FACE('',(#3412),#893,.T.);
#32161=ADVANCED_FACE('',(#3413),#894,.T.);
#32162=ADVANCED_FACE('',(#3414),#895,.F.);
#32163=ADVANCED_FACE('',(#3415),#896,.F.);
#32164=ADVANCED_FACE('',(#3416),#897,.F.);
#32165=ADVANCED_FACE('',(#3417),#898,.F.);
#32166=ADVANCED_FACE('',(#3418),#899,.F.);
#32167=ADVANCED_FACE('',(#3419),#900,.F.);
#32168=ADVANCED_FACE('',(#3420),#901,.F.);
#32169=ADVANCED_FACE('',(#3421),#902,.F.);
#32170=ADVANCED_FACE('',(#3422),#903,.F.);
#32171=ADVANCED_FACE('',(#3423),#904,.F.);
#32172=ADVANCED_FACE('',(#3424),#905,.F.);
#32173=ADVANCED_FACE('',(#3425),#906,.T.);
#32174=ADVANCED_FACE('',(#3426),#907,.T.);
#32175=ADVANCED_FACE('',(#3427),#908,.T.);
#32176=ADVANCED_FACE('',(#3428),#909,.T.);
#32177=ADVANCED_FACE('',(#3429),#910,.T.);
#32178=ADVANCED_FACE('',(#3430),#911,.T.);
#32179=ADVANCED_FACE('',(#3431),#912,.T.);
#32180=ADVANCED_FACE('',(#3432),#913,.T.);
#32181=ADVANCED_FACE('',(#3433),#914,.T.);
#32182=ADVANCED_FACE('',(#3434),#915,.T.);
#32183=ADVANCED_FACE('',(#3435),#916,.T.);
#32184=ADVANCED_FACE('',(#3436),#917,.T.);
#32185=ADVANCED_FACE('',(#3437),#918,.T.);
#32186=ADVANCED_FACE('',(#3438),#919,.T.);
#32187=ADVANCED_FACE('',(#3439),#920,.F.);
#32188=ADVANCED_FACE('',(#3440),#921,.F.);
#32189=ADVANCED_FACE('',(#3441),#922,.T.);
#32190=ADVANCED_FACE('',(#3442),#923,.T.);
#32191=ADVANCED_FACE('',(#3443),#924,.T.);
#32192=ADVANCED_FACE('',(#3444),#925,.T.);
#32193=ADVANCED_FACE('',(#3445),#926,.T.);
#32194=ADVANCED_FACE('',(#3446),#927,.T.);
#32195=ADVANCED_FACE('',(#3447),#928,.T.);
#32196=ADVANCED_FACE('',(#3448),#2570,.T.);
#32197=ADVANCED_FACE('',(#3449),#92,.T.);
#32198=ADVANCED_FACE('',(#3450),#93,.T.);
#32199=ADVANCED_FACE('',(#3451),#2571,.T.);
#32200=ADVANCED_FACE('',(#3452),#94,.T.);
#32201=ADVANCED_FACE('',(#3453),#2572,.T.);
#32202=ADVANCED_FACE('',(#3454),#95,.T.);
#32203=ADVANCED_FACE('',(#3455),#2573,.T.);
#32204=ADVANCED_FACE('',(#3456),#96,.T.);
#32205=ADVANCED_FACE('',(#3457),#97,.T.);
#32206=ADVANCED_FACE('',(#3458),#98,.T.);
#32207=ADVANCED_FACE('',(#3459),#2574,.T.);
#32208=ADVANCED_FACE('',(#3460),#99,.T.);
#32209=ADVANCED_FACE('',(#3461),#100,.T.);
#32210=ADVANCED_FACE('',(#3462),#101,.T.);
#32211=ADVANCED_FACE('',(#3463),#2575,.T.);
#32212=ADVANCED_FACE('',(#3464),#102,.T.);
#32213=ADVANCED_FACE('',(#3465),#2576,.T.);
#32214=ADVANCED_FACE('',(#3466),#103,.T.);
#32215=ADVANCED_FACE('',(#3467),#2577,.T.);
#32216=ADVANCED_FACE('',(#3468),#104,.T.);
#32217=ADVANCED_FACE('',(#3469),#105,.T.);
#32218=ADVANCED_FACE('',(#3470),#106,.T.);
#32219=ADVANCED_FACE('',(#3471),#2578,.T.);
#32220=ADVANCED_FACE('',(#3472),#107,.T.);
#32221=ADVANCED_FACE('',(#3473),#2579,.T.);
#32222=ADVANCED_FACE('',(#3474),#108,.T.);
#32223=ADVANCED_FACE('',(#3475),#2580,.T.);
#32224=ADVANCED_FACE('',(#3476),#109,.T.);
#32225=ADVANCED_FACE('',(#3477),#110,.T.);
#32226=ADVANCED_FACE('',(#3478),#111,.T.);
#32227=ADVANCED_FACE('',(#3479),#2581,.T.);
#32228=ADVANCED_FACE('',(#3480),#112,.T.);
#32229=ADVANCED_FACE('',(#3481),#113,.T.);
#32230=ADVANCED_FACE('',(#3482),#114,.T.);
#32231=ADVANCED_FACE('',(#3483),#2582,.T.);
#32232=ADVANCED_FACE('',(#3484),#115,.T.);
#32233=ADVANCED_FACE('',(#3485),#2583,.T.);
#32234=ADVANCED_FACE('',(#3486),#116,.T.);
#32235=ADVANCED_FACE('',(#3487),#117,.T.);
#32236=ADVANCED_FACE('',(#3488),#2584,.T.);
#32237=ADVANCED_FACE('',(#3489,#1257),#2106,.F.);
#32238=ADVANCED_FACE('',(#3490),#2585,.F.);
#32239=ADVANCED_FACE('',(#3491),#2107,.T.);
#32240=ADVANCED_FACE('',(#3492),#2108,.T.);
#32241=ADVANCED_FACE('',(#3493),#2586,.T.);
#32242=ADVANCED_FACE('',(#3494),#2109,.T.);
#32243=ADVANCED_FACE('',(#3495),#2587,.T.);
#32244=ADVANCED_FACE('',(#3496),#2110,.F.);
#32245=ADVANCED_FACE('',(#3497),#2588,.T.);
#32246=ADVANCED_FACE('',(#3498),#2589,.T.);
#32247=ADVANCED_FACE('',(#3499),#2111,.F.);
#32248=ADVANCED_FACE('',(#3500),#2590,.F.);
#32249=ADVANCED_FACE('',(#3501),#2112,.F.);
#32250=ADVANCED_FACE('',(#3502),#2591,.T.);
#32251=ADVANCED_FACE('',(#3503),#2113,.F.);
#32252=ADVANCED_FACE('',(#3504),#2592,.T.);
#32253=ADVANCED_FACE('',(#3505),#2114,.T.);
#32254=ADVANCED_FACE('',(#3506),#2593,.T.);
#32255=ADVANCED_FACE('',(#3507),#2115,.T.);
#32256=ADVANCED_FACE('',(#3508),#929,.F.);
#32257=ADVANCED_FACE('',(#3509),#930,.F.);
#32258=ADVANCED_FACE('',(#3510),#2116,.F.);
#32259=ADVANCED_FACE('',(#3511),#931,.F.);
#32260=ADVANCED_FACE('',(#3512),#932,.F.);
#32261=ADVANCED_FACE('',(#3513),#933,.F.);
#32262=ADVANCED_FACE('',(#3514),#934,.F.);
#32263=ADVANCED_FACE('',(#3515),#935,.F.);
#32264=ADVANCED_FACE('',(#3516),#936,.F.);
#32265=ADVANCED_FACE('',(#3517),#937,.F.);
#32266=ADVANCED_FACE('',(#3518),#938,.F.);
#32267=ADVANCED_FACE('',(#3519),#2594,.T.);
#32268=ADVANCED_FACE('',(#3520),#939,.F.);
#32269=ADVANCED_FACE('',(#3521),#940,.T.);
#32270=ADVANCED_FACE('',(#3522),#941,.T.);
#32271=ADVANCED_FACE('',(#3523),#942,.T.);
#32272=ADVANCED_FACE('',(#3524),#943,.T.);
#32273=ADVANCED_FACE('',(#3525),#944,.T.);
#32274=ADVANCED_FACE('',(#3526),#945,.T.);
#32275=ADVANCED_FACE('',(#3527),#2595,.F.);
#32276=ADVANCED_FACE('',(#3528),#2596,.F.);
#32277=ADVANCED_FACE('',(#3529),#2597,.T.);
#32278=ADVANCED_FACE('',(#3530),#2117,.T.);
#32279=ADVANCED_FACE('',(#3531),#2598,.F.);
#32280=ADVANCED_FACE('',(#3532),#2599,.F.);
#32281=ADVANCED_FACE('',(#3533),#2600,.F.);
#32282=ADVANCED_FACE('',(#3534),#2118,.F.);
#32283=ADVANCED_FACE('',(#3535),#946,.T.);
#32284=ADVANCED_FACE('',(#3536),#947,.T.);
#32285=ADVANCED_FACE('',(#3537),#948,.T.);
#32286=ADVANCED_FACE('',(#3538),#949,.T.);
#32287=ADVANCED_FACE('',(#3539),#950,.T.);
#32288=ADVANCED_FACE('',(#3540),#951,.T.);
#32289=ADVANCED_FACE('',(#3541),#952,.F.);
#32290=ADVANCED_FACE('',(#3542),#953,.F.);
#32291=ADVANCED_FACE('',(#3543),#954,.F.);
#32292=ADVANCED_FACE('',(#3544),#955,.F.);
#32293=ADVANCED_FACE('',(#3545),#956,.F.);
#32294=ADVANCED_FACE('',(#3546),#957,.F.);
#32295=ADVANCED_FACE('',(#3547),#711,.T.);
#32296=ADVANCED_FACE('',(#3548),#958,.F.);
#32297=ADVANCED_FACE('',(#3549),#959,.F.);
#32298=ADVANCED_FACE('',(#3550),#960,.F.);
#32299=ADVANCED_FACE('',(#3551),#961,.F.);
#32300=ADVANCED_FACE('',(#3552),#962,.F.);
#32301=ADVANCED_FACE('',(#3553),#963,.T.);
#32302=ADVANCED_FACE('',(#3554),#964,.T.);
#32303=ADVANCED_FACE('',(#3555),#965,.T.);
#32304=ADVANCED_FACE('',(#3556),#966,.T.);
#32305=ADVANCED_FACE('',(#3557),#967,.T.);
#32306=ADVANCED_FACE('',(#3558),#968,.T.);
#32307=ADVANCED_FACE('',(#3559),#969,.T.);
#32308=ADVANCED_FACE('',(#3560),#970,.F.);
#32309=ADVANCED_FACE('',(#3561),#971,.F.);
#32310=ADVANCED_FACE('',(#3562),#972,.F.);
#32311=ADVANCED_FACE('',(#3563),#973,.F.);
#32312=ADVANCED_FACE('',(#3564),#974,.F.);
#32313=ADVANCED_FACE('',(#3565),#975,.F.);
#32314=ADVANCED_FACE('',(#3566,#1258,#1259,#1260),#2119,.F.);
#32315=ADVANCED_FACE('',(#3567),#2601,.T.);
#32316=ADVANCED_FACE('',(#3568),#2602,.T.);
#32317=ADVANCED_FACE('',(#3569),#2603,.T.);
#32318=ADVANCED_FACE('',(#3570),#2604,.T.);
#32319=ADVANCED_FACE('',(#3571),#2605,.T.);
#32320=ADVANCED_FACE('',(#3572),#2606,.T.);
#32321=ADVANCED_FACE('',(#3573),#2607,.T.);
#32322=ADVANCED_FACE('',(#3574,#1261),#2120,.F.);
#32323=ADVANCED_FACE('',(#3575,#1262,#1263,#1264),#2121,.T.);
#32324=ADVANCED_FACE('',(#3576,#1265,#1266,#1267),#2122,.F.);
#32325=ADVANCED_FACE('',(#3577),#976,.T.);
#32326=ADVANCED_FACE('',(#3578),#977,.F.);
#32327=ADVANCED_FACE('',(#3579),#2608,.T.);
#32328=ADVANCED_FACE('',(#3580),#978,.T.);
#32329=ADVANCED_FACE('',(#3581),#979,.F.);
#32330=ADVANCED_FACE('',(#3582),#980,.F.);
#32331=ADVANCED_FACE('',(#3583),#981,.T.);
#32332=ADVANCED_FACE('',(#3584),#982,.F.);
#32333=ADVANCED_FACE('',(#3585),#983,.F.);
#32334=ADVANCED_FACE('',(#3586),#984,.T.);
#32335=ADVANCED_FACE('',(#3587),#985,.F.);
#32336=ADVANCED_FACE('',(#3588),#986,.F.);
#32337=ADVANCED_FACE('',(#3589),#987,.T.);
#32338=ADVANCED_FACE('',(#3590),#988,.F.);
#32339=ADVANCED_FACE('',(#3591),#989,.F.);
#32340=ADVANCED_FACE('',(#3592),#990,.T.);
#32341=ADVANCED_FACE('',(#3593),#991,.F.);
#32342=ADVANCED_FACE('',(#3594),#992,.F.);
#32343=ADVANCED_FACE('',(#3595),#993,.T.);
#32344=ADVANCED_FACE('',(#3596),#994,.F.);
#32345=ADVANCED_FACE('',(#3597),#995,.F.);
#32346=ADVANCED_FACE('',(#3598),#2609,.T.);
#32347=ADVANCED_FACE('',(#3599),#2610,.T.);
#32348=ADVANCED_FACE('',(#3600),#2123,.F.);
#32349=ADVANCED_FACE('',(#3601),#996,.T.);
#32350=ADVANCED_FACE('',(#3602),#997,.F.);
#32351=ADVANCED_FACE('',(#3603),#998,.F.);
#32352=ADVANCED_FACE('',(#3604),#999,.T.);
#32353=ADVANCED_FACE('',(#3605),#1000,.F.);
#32354=ADVANCED_FACE('',(#3606),#1001,.F.);
#32355=ADVANCED_FACE('',(#3607),#1002,.T.);
#32356=ADVANCED_FACE('',(#3608),#1003,.F.);
#32357=ADVANCED_FACE('',(#3609),#1004,.F.);
#32358=ADVANCED_FACE('',(#3610),#1005,.T.);
#32359=ADVANCED_FACE('',(#3611),#1006,.F.);
#32360=ADVANCED_FACE('',(#3612),#1007,.F.);
#32361=ADVANCED_FACE('',(#3613),#1008,.T.);
#32362=ADVANCED_FACE('',(#3614),#1009,.F.);
#32363=ADVANCED_FACE('',(#3615),#1010,.F.);
#32364=ADVANCED_FACE('',(#3616),#1011,.T.);
#32365=ADVANCED_FACE('',(#3617),#1012,.F.);
#32366=ADVANCED_FACE('',(#3618),#1013,.F.);
#32367=ADVANCED_FACE('',(#3619),#1014,.T.);
#32368=ADVANCED_FACE('',(#3620),#1015,.F.);
#32369=ADVANCED_FACE('',(#3621),#1016,.F.);
#32370=ADVANCED_FACE('',(#3622),#1017,.T.);
#32371=ADVANCED_FACE('',(#3623),#1018,.F.);
#32372=ADVANCED_FACE('',(#3624),#1019,.F.);
#32373=ADVANCED_FACE('',(#3625),#1020,.T.);
#32374=ADVANCED_FACE('',(#3626),#1021,.F.);
#32375=ADVANCED_FACE('',(#3627),#1022,.F.);
#32376=ADVANCED_FACE('',(#3628),#1023,.T.);
#32377=ADVANCED_FACE('',(#3629),#1024,.F.);
#32378=ADVANCED_FACE('',(#3630),#1025,.F.);
#32379=ADVANCED_FACE('',(#3631),#1026,.T.);
#32380=ADVANCED_FACE('',(#3632),#1027,.F.);
#32381=ADVANCED_FACE('',(#3633),#1028,.F.);
#32382=ADVANCED_FACE('',(#3634),#1029,.T.);
#32383=ADVANCED_FACE('',(#3635),#1030,.F.);
#32384=ADVANCED_FACE('',(#3636),#2611,.T.);
#32385=ADVANCED_FACE('',(#3637),#1031,.T.);
#32386=ADVANCED_FACE('',(#3638),#1032,.F.);
#32387=ADVANCED_FACE('',(#3639),#1033,.F.);
#32388=ADVANCED_FACE('',(#3640),#2612,.T.);
#32389=ADVANCED_FACE('',(#3641),#2613,.T.);
#32390=ADVANCED_FACE('',(#3642),#2124,.F.);
#32391=ADVANCED_FACE('',(#3643),#1034,.T.);
#32392=ADVANCED_FACE('',(#3644),#1035,.F.);
#32393=ADVANCED_FACE('',(#3645),#1036,.F.);
#32394=ADVANCED_FACE('',(#3646),#1037,.T.);
#32395=ADVANCED_FACE('',(#3647),#1038,.F.);
#32396=ADVANCED_FACE('',(#3648),#1039,.F.);
#32397=ADVANCED_FACE('',(#3649),#1040,.T.);
#32398=ADVANCED_FACE('',(#3650),#1041,.F.);
#32399=ADVANCED_FACE('',(#3651),#1042,.F.);
#32400=ADVANCED_FACE('',(#3652),#1043,.T.);
#32401=ADVANCED_FACE('',(#3653),#1044,.F.);
#32402=ADVANCED_FACE('',(#3654),#1045,.F.);
#32403=ADVANCED_FACE('',(#3655),#1046,.T.);
#32404=ADVANCED_FACE('',(#3656),#1047,.F.);
#32405=ADVANCED_FACE('',(#3657),#1048,.F.);
#32406=ADVANCED_FACE('',(#3658),#1049,.T.);
#32407=ADVANCED_FACE('',(#3659),#1050,.F.);
#32408=ADVANCED_FACE('',(#3660),#1051,.F.);
#32409=ADVANCED_FACE('',(#3661),#1052,.T.);
#32410=ADVANCED_FACE('',(#3662),#1053,.F.);
#32411=ADVANCED_FACE('',(#3663),#1054,.F.);
#32412=ADVANCED_FACE('',(#3664),#1055,.T.);
#32413=ADVANCED_FACE('',(#3665),#1056,.F.);
#32414=ADVANCED_FACE('',(#3666),#1057,.F.);
#32415=ADVANCED_FACE('',(#3667),#1058,.T.);
#32416=ADVANCED_FACE('',(#3668),#1059,.F.);
#32417=ADVANCED_FACE('',(#3669),#1060,.F.);
#32418=ADVANCED_FACE('',(#3670),#1061,.T.);
#32419=ADVANCED_FACE('',(#3671),#1062,.F.);
#32420=ADVANCED_FACE('',(#3672),#1063,.F.);
#32421=ADVANCED_FACE('',(#3673),#1064,.T.);
#32422=ADVANCED_FACE('',(#3674),#1065,.F.);
#32423=ADVANCED_FACE('',(#3675),#1066,.F.);
#32424=ADVANCED_FACE('',(#3676),#1067,.T.);
#32425=ADVANCED_FACE('',(#3677),#1068,.F.);
#32426=ADVANCED_FACE('',(#3678),#1069,.F.);
#32427=ADVANCED_FACE('',(#3679),#1070,.T.);
#32428=ADVANCED_FACE('',(#3680),#1071,.F.);
#32429=ADVANCED_FACE('',(#3681),#1072,.F.);
#32430=ADVANCED_FACE('',(#3682),#1073,.T.);
#32431=ADVANCED_FACE('',(#3683),#1074,.F.);
#32432=ADVANCED_FACE('',(#3684),#1075,.F.);
#32433=ADVANCED_FACE('',(#3685,#1268,#1269,#1270),#2125,.T.);
#32434=ADVANCED_FACE('',(#3686,#1271,#1272,#1273),#2126,.F.);
#32435=ADVANCED_FACE('',(#3687),#118,.T.);
#32436=ADVANCED_FACE('',(#3688),#2614,.F.);
#32437=ADVANCED_FACE('',(#3689),#119,.T.);
#32438=ADVANCED_FACE('',(#3690),#2615,.F.);
#32439=ADVANCED_FACE('',(#3691),#1076,.T.);
#32440=ADVANCED_FACE('',(#3692),#1077,.F.);
#32441=ADVANCED_FACE('',(#3693),#2616,.T.);
#32442=ADVANCED_FACE('',(#3694),#2127,.F.);
#32443=ADVANCED_FACE('',(#3695),#1078,.T.);
#32444=ADVANCED_FACE('',(#3696),#1079,.F.);
#32445=ADVANCED_FACE('',(#3697),#1080,.T.);
#32446=ADVANCED_FACE('',(#3698),#1081,.F.);
#32447=ADVANCED_FACE('',(#3699),#2617,.T.);
#32448=ADVANCED_FACE('',(#3700),#2128,.F.);
#32449=ADVANCED_FACE('',(#3701),#1082,.T.);
#32450=ADVANCED_FACE('',(#3702),#1083,.F.);
#32451=ADVANCED_FACE('',(#3703),#1084,.T.);
#32452=ADVANCED_FACE('',(#3704),#1085,.F.);
#32453=ADVANCED_FACE('',(#3705),#1086,.T.);
#32454=ADVANCED_FACE('',(#3706),#1087,.F.);
#32455=ADVANCED_FACE('',(#3707),#1088,.T.);
#32456=ADVANCED_FACE('',(#3708),#1089,.F.);
#32457=ADVANCED_FACE('',(#3709),#1090,.T.);
#32458=ADVANCED_FACE('',(#3710),#1091,.F.);
#32459=ADVANCED_FACE('',(#3711),#1092,.T.);
#32460=ADVANCED_FACE('',(#3712),#1093,.F.);
#32461=ADVANCED_FACE('',(#3713),#1094,.T.);
#32462=ADVANCED_FACE('',(#3714),#1095,.F.);
#32463=ADVANCED_FACE('',(#3715),#1096,.T.);
#32464=ADVANCED_FACE('',(#3716),#1097,.F.);
#32465=ADVANCED_FACE('',(#3717),#1098,.T.);
#32466=ADVANCED_FACE('',(#3718),#1099,.F.);
#32467=ADVANCED_FACE('',(#3719),#1100,.T.);
#32468=ADVANCED_FACE('',(#3720),#1101,.F.);
#32469=ADVANCED_FACE('',(#3721),#2618,.T.);
#32470=ADVANCED_FACE('',(#3722),#2129,.F.);
#32471=ADVANCED_FACE('',(#3723),#1102,.T.);
#32472=ADVANCED_FACE('',(#3724),#1103,.F.);
#32473=ADVANCED_FACE('',(#3725),#1104,.T.);
#32474=ADVANCED_FACE('',(#3726),#1105,.F.);
#32475=ADVANCED_FACE('',(#3727),#2619,.T.);
#32476=ADVANCED_FACE('',(#3728),#2130,.F.);
#32477=ADVANCED_FACE('',(#3729),#2131,.F.);
#32478=ADVANCED_FACE('',(#3730),#2620,.T.);
#32479=ADVANCED_FACE('',(#3731),#2132,.F.);
#32480=ADVANCED_FACE('',(#3732),#1106,.T.);
#32481=ADVANCED_FACE('',(#3733),#2133,.T.);
#32482=ADVANCED_FACE('',(#3734),#2134,.F.);
#32483=ADVANCED_FACE('',(#3735),#2135,.T.);
#32484=ADVANCED_FACE('',(#3736),#2621,.T.);
#32485=ADVANCED_FACE('',(#3737),#1107,.F.);
#32486=ADVANCED_FACE('',(#3738),#2136,.T.);
#32487=ADVANCED_FACE('',(#3739),#2622,.F.);
#32488=ADVANCED_FACE('',(#3740),#2623,.F.);
#32489=ADVANCED_FACE('',(#3741),#2137,.F.);
#32490=ADVANCED_FACE('',(#3742,#1274,#1275,#1276,#1277,#1278,#1279),#2138,
 .F.);
#32491=ADVANCED_FACE('',(#3743),#2624,.F.);
#32492=ADVANCED_FACE('',(#3744),#2139,.F.);
#32493=ADVANCED_FACE('',(#3745),#2140,.F.);
#32494=ADVANCED_FACE('',(#3746),#2141,.T.);
#32495=ADVANCED_FACE('',(#3747),#2625,.T.);
#32496=ADVANCED_FACE('',(#3748),#2142,.F.);
#32497=ADVANCED_FACE('',(#3749),#1108,.T.);
#32498=ADVANCED_FACE('',(#3750),#2143,.T.);
#32499=ADVANCED_FACE('',(#3751),#2626,.T.);
#32500=ADVANCED_FACE('',(#3752),#2144,.T.);
#32501=ADVANCED_FACE('',(#3753),#1109,.F.);
#32502=ADVANCED_FACE('',(#3754),#2145,.F.);
#32503=ADVANCED_FACE('',(#3755),#2627,.T.);
#32504=ADVANCED_FACE('',(#3756),#2146,.F.);
#32505=ADVANCED_FACE('',(#3757),#1110,.F.);
#32506=ADVANCED_FACE('',(#3758),#2147,.T.);
#32507=ADVANCED_FACE('',(#3759),#2628,.T.);
#32508=ADVANCED_FACE('',(#3760),#2148,.T.);
#32509=ADVANCED_FACE('',(#3761),#1111,.T.);
#32510=ADVANCED_FACE('',(#3762),#2149,.F.);
#32511=ADVANCED_FACE('',(#3763),#2629,.F.);
#32512=ADVANCED_FACE('',(#3764),#2150,.T.);
#32513=ADVANCED_FACE('',(#3765),#2630,.T.);
#32514=ADVANCED_FACE('',(#3766),#2631,.F.);
#32515=ADVANCED_FACE('',(#3767),#2632,.T.);
#32516=ADVANCED_FACE('',(#3768),#2151,.T.);
#32517=ADVANCED_FACE('',(#3769),#2152,.F.);
#32518=ADVANCED_FACE('',(#3770),#2153,.T.);
#32519=ADVANCED_FACE('',(#3771),#2633,.F.);
#32520=ADVANCED_FACE('',(#3772),#2154,.T.);
#32521=ADVANCED_FACE('',(#3773),#2155,.T.);
#32522=ADVANCED_FACE('',(#3774),#2634,.T.);
#32523=ADVANCED_FACE('',(#3775),#2635,.F.);
#32524=ADVANCED_FACE('',(#3776),#2636,.F.);
#32525=ADVANCED_FACE('',(#3777),#2637,.T.);
#32526=ADVANCED_FACE('',(#3778),#2156,.F.);
#32527=ADVANCED_FACE('',(#3779),#2157,.T.);
#32528=ADVANCED_FACE('',(#3780),#2638,.T.);
#32529=ADVANCED_FACE('',(#3781),#2158,.T.);
#32530=ADVANCED_FACE('',(#3782),#2639,.F.);
#32531=ADVANCED_FACE('',(#3783),#2159,.F.);
#32532=ADVANCED_FACE('',(#3784),#2160,.F.);
#32533=ADVANCED_FACE('',(#3785),#2640,.T.);
#32534=ADVANCED_FACE('',(#3786),#2641,.T.);
#32535=ADVANCED_FACE('',(#3787),#2642,.F.);
#32536=ADVANCED_FACE('',(#3788),#2161,.T.);
#32537=ADVANCED_FACE('',(#3789),#2643,.T.);
#32538=ADVANCED_FACE('',(#3790),#2644,.F.);
#32539=ADVANCED_FACE('',(#3791),#2645,.T.);
#32540=ADVANCED_FACE('',(#3792),#2646,.T.);
#32541=ADVANCED_FACE('',(#3793),#2647,.F.);
#32542=ADVANCED_FACE('',(#3794),#2648,.T.);
#32543=ADVANCED_FACE('',(#3795),#2162,.F.);
#32544=ADVANCED_FACE('',(#3796),#2649,.T.);
#32545=ADVANCED_FACE('',(#3797),#2163,.T.);
#32546=ADVANCED_FACE('',(#3798),#2164,.T.);
#32547=ADVANCED_FACE('',(#3799),#2650,.F.);
#32548=ADVANCED_FACE('',(#3800),#2165,.F.);
#32549=ADVANCED_FACE('',(#3801),#2651,.T.);
#32550=ADVANCED_FACE('',(#3802),#2652,.T.);
#32551=ADVANCED_FACE('',(#3803),#2166,.F.);
#32552=ADVANCED_FACE('',(#3804),#2167,.T.);
#32553=ADVANCED_FACE('',(#3805),#2168,.T.);
#32554=ADVANCED_FACE('',(#3806),#2169,.T.);
#32555=ADVANCED_FACE('',(#3807),#2170,.F.);
#32556=ADVANCED_FACE('',(#3808),#2171,.F.);
#32557=ADVANCED_FACE('',(#3809),#2172,.T.);
#32558=ADVANCED_FACE('',(#3810),#2173,.T.);
#32559=ADVANCED_FACE('',(#3811),#2174,.T.);
#32560=ADVANCED_FACE('',(#3812),#2175,.F.);
#32561=ADVANCED_FACE('',(#3813),#2176,.T.);
#32562=ADVANCED_FACE('',(#3814),#2177,.F.);
#32563=ADVANCED_FACE('',(#3815),#2178,.F.);
#32564=ADVANCED_FACE('',(#3816),#2179,.F.);
#32565=ADVANCED_FACE('',(#3817),#2180,.T.);
#32566=ADVANCED_FACE('',(#3818),#2181,.T.);
#32567=ADVANCED_FACE('',(#3819),#2653,.T.);
#32568=ADVANCED_FACE('',(#3820),#2654,.T.);
#32569=ADVANCED_FACE('',(#3821),#2182,.F.);
#32570=ADVANCED_FACE('',(#3822),#2183,.F.);
#32571=ADVANCED_FACE('',(#3823),#2184,.F.);
#32572=ADVANCED_FACE('',(#3824),#2185,.F.);
#32573=ADVANCED_FACE('',(#3825),#2186,.F.);
#32574=ADVANCED_FACE('',(#3826),#2187,.F.);
#32575=ADVANCED_FACE('',(#3827),#2188,.F.);
#32576=ADVANCED_FACE('',(#3828),#2189,.F.);
#32577=ADVANCED_FACE('',(#3829),#2190,.F.);
#32578=ADVANCED_FACE('',(#3830),#2191,.F.);
#32579=ADVANCED_FACE('',(#3831),#2192,.F.);
#32580=ADVANCED_FACE('',(#3832),#2193,.F.);
#32581=ADVANCED_FACE('',(#3833),#120,.T.);
#32582=ADVANCED_FACE('',(#3834,#1280,#1281,#1282),#2194,.T.);
#32583=ADVANCED_FACE('',(#3835),#2195,.F.);
#32584=ADVANCED_FACE('',(#3836),#2196,.F.);
#32585=ADVANCED_FACE('',(#3837),#2197,.F.);
#32586=ADVANCED_FACE('',(#3838),#121,.T.);
#32587=ADVANCED_FACE('',(#3839),#2655,.T.);
#32588=ADVANCED_FACE('',(#3840),#2656,.F.);
#32589=ADVANCED_FACE('',(#3841),#2657,.F.);
#32590=ADVANCED_FACE('',(#3842),#2658,.F.);
#32591=ADVANCED_FACE('',(#3843),#2659,.F.);
#32592=ADVANCED_FACE('',(#3844),#2660,.F.);
#32593=ADVANCED_FACE('',(#3845),#2661,.F.);
#32594=ADVANCED_FACE('',(#3846),#2662,.F.);
#32595=ADVANCED_FACE('',(#3847),#2198,.T.);
#32596=ADVANCED_FACE('',(#3848),#2199,.T.);
#32597=ADVANCED_FACE('',(#3849),#2663,.T.);
#32598=ADVANCED_FACE('',(#3850),#2200,.T.);
#32599=ADVANCED_FACE('',(#3851),#2201,.T.);
#32600=ADVANCED_FACE('',(#3852),#2202,.T.);
#32601=ADVANCED_FACE('',(#3853),#2664,.F.);
#32602=ADVANCED_FACE('',(#3854),#2665,.F.);
#32603=ADVANCED_FACE('',(#3855),#2666,.F.);
#32604=ADVANCED_FACE('',(#3856),#2667,.F.);
#32605=ADVANCED_FACE('',(#3857),#2668,.F.);
#32606=ADVANCED_FACE('',(#3858),#2669,.F.);
#32607=ADVANCED_FACE('',(#3859),#2670,.F.);
#32608=ADVANCED_FACE('',(#3860),#2203,.T.);
#32609=ADVANCED_FACE('',(#3861),#2671,.T.);
#32610=ADVANCED_FACE('',(#3862),#2672,.T.);
#32611=ADVANCED_FACE('',(#3863),#2204,.T.);
#32612=ADVANCED_FACE('',(#3864),#2205,.F.);
#32613=ADVANCED_FACE('',(#3865),#2206,.T.);
#32614=ADVANCED_FACE('',(#3866),#2207,.T.);
#32615=ADVANCED_FACE('',(#3867),#2208,.T.);
#32616=ADVANCED_FACE('',(#3868,#1283),#2209,.F.);
#32617=ADVANCED_FACE('',(#3869),#2673,.T.);
#32618=ADVANCED_FACE('',(#3870),#2674,.F.);
#32619=ADVANCED_FACE('',(#3871),#2675,.T.);
#32620=ADVANCED_FACE('',(#3872),#2676,.F.);
#32621=ADVANCED_FACE('',(#3873),#2677,.T.);
#32622=ADVANCED_FACE('',(#3874),#2210,.F.);
#32623=ADVANCED_FACE('',(#3875),#2678,.T.);
#32624=ADVANCED_FACE('',(#3876),#2679,.T.);
#32625=ADVANCED_FACE('',(#3877),#2211,.T.);
#32626=ADVANCED_FACE('',(#3878),#2680,.T.);
#32627=ADVANCED_FACE('',(#3879),#2681,.T.);
#32628=ADVANCED_FACE('',(#3880,#1284),#2212,.F.);
#32629=ADVANCED_FACE('',(#3881),#2682,.T.);
#32630=ADVANCED_FACE('',(#3882),#2683,.F.);
#32631=ADVANCED_FACE('',(#3883),#1112,.T.);
#32632=ADVANCED_FACE('',(#3884),#1113,.F.);
#32633=ADVANCED_FACE('',(#3885),#1114,.T.);
#32634=ADVANCED_FACE('',(#3886),#1115,.T.);
#32635=ADVANCED_FACE('',(#3887),#1116,.T.);
#32636=ADVANCED_FACE('',(#3888),#2684,.T.);
#32637=ADVANCED_FACE('',(#3889),#2685,.T.);
#32638=ADVANCED_FACE('',(#3890),#1117,.F.);
#32639=ADVANCED_FACE('',(#3891),#1118,.F.);
#32640=ADVANCED_FACE('',(#3892),#1119,.F.);
#32641=ADVANCED_FACE('',(#3893),#1120,.T.);
#32642=ADVANCED_FACE('',(#3894),#1121,.F.);
#32643=ADVANCED_FACE('',(#3895),#2686,.F.);
#32644=ADVANCED_FACE('',(#3896),#2687,.T.);
#32645=ADVANCED_FACE('',(#3897),#2688,.F.);
#32646=ADVANCED_FACE('',(#3898,#1285),#2213,.F.);
#32647=ADVANCED_FACE('',(#3899,#1286),#2214,.F.);
#32648=ADVANCED_FACE('',(#3900,#1287),#2215,.F.);
#32649=ADVANCED_FACE('',(#3901),#2689,.F.);
#32650=ADVANCED_FACE('',(#3902),#2216,.T.);
#32651=ADVANCED_FACE('',(#3903),#2690,.F.);
#32652=ADVANCED_FACE('',(#3904),#2217,.F.);
#32653=ADVANCED_FACE('',(#3905),#2691,.T.);
#32654=ADVANCED_FACE('',(#3906),#2692,.T.);
#32655=ADVANCED_FACE('',(#3907),#2218,.T.);
#32656=ADVANCED_FACE('',(#3908),#2693,.F.);
#32657=ADVANCED_FACE('',(#3909),#2694,.F.);
#32658=ADVANCED_FACE('',(#3910),#2219,.T.);
#32659=ADVANCED_FACE('',(#3911),#2695,.F.);
#32660=ADVANCED_FACE('',(#3912),#2696,.T.);
#32661=ADVANCED_FACE('',(#3913),#1122,.F.);
#32662=ADVANCED_FACE('',(#3914),#1123,.T.);
#32663=ADVANCED_FACE('',(#3915),#1124,.F.);
#32664=ADVANCED_FACE('',(#3916),#2697,.F.);
#32665=ADVANCED_FACE('',(#3917),#1125,.T.);
#32666=ADVANCED_FACE('',(#3918),#1126,.F.);
#32667=ADVANCED_FACE('',(#3919),#1127,.T.);
#32668=ADVANCED_FACE('',(#3920),#2698,.T.);
#32669=ADVANCED_FACE('',(#3921),#2699,.F.);
#32670=ADVANCED_FACE('',(#3922),#2220,.F.);
#32671=ADVANCED_FACE('',(#3923),#2221,.F.);
#32672=ADVANCED_FACE('',(#3924),#2222,.F.);
#32673=ADVANCED_FACE('',(#3925),#1128,.F.);
#32674=ADVANCED_FACE('',(#3926),#2223,.T.);
#32675=ADVANCED_FACE('',(#3927),#2224,.F.);
#32676=ADVANCED_FACE('',(#3928),#1129,.T.);
#32677=ADVANCED_FACE('',(#3929),#2225,.F.);
#32678=ADVANCED_FACE('',(#3930),#2226,.F.);
#32679=ADVANCED_FACE('',(#3931),#2227,.T.);
#32680=ADVANCED_FACE('',(#3932),#2228,.F.);
#32681=ADVANCED_FACE('',(#3933),#2229,.T.);
#32682=ADVANCED_FACE('',(#3934),#2230,.F.);
#32683=ADVANCED_FACE('',(#3935),#2231,.T.);
#32684=ADVANCED_FACE('',(#3936),#2232,.F.);
#32685=ADVANCED_FACE('',(#3937),#2233,.F.);
#32686=ADVANCED_FACE('',(#3938),#2234,.T.);
#32687=ADVANCED_FACE('',(#3939,#1288,#1289,#1290),#2235,.T.);
#32688=ADVANCED_FACE('',(#3940),#2700,.F.);
#32689=ADVANCED_FACE('',(#3941),#2701,.F.);
#32690=ADVANCED_FACE('',(#3942),#1130,.T.);
#32691=ADVANCED_FACE('',(#3943,#1291),#2236,.T.);
#32692=ADVANCED_FACE('',(#3944),#2702,.F.);
#32693=ADVANCED_FACE('',(#3945),#1131,.F.);
#32694=ADVANCED_FACE('',(#3946),#1132,.T.);
#32695=ADVANCED_FACE('',(#3947),#2703,.F.);
#32696=ADVANCED_FACE('',(#3948),#1133,.T.);
#32697=ADVANCED_FACE('',(#3949),#1134,.T.);
#32698=ADVANCED_FACE('',(#3950),#1135,.T.);
#32699=ADVANCED_FACE('',(#3951),#1136,.F.);
#32700=ADVANCED_FACE('',(#3952),#1137,.T.);
#32701=ADVANCED_FACE('',(#3953),#2704,.F.);
#32702=ADVANCED_FACE('',(#3954),#2237,.T.);
#32703=ADVANCED_FACE('',(#3955),#2705,.F.);
#32704=ADVANCED_FACE('',(#3956),#1138,.F.);
#32705=ADVANCED_FACE('',(#3957),#1139,.F.);
#32706=ADVANCED_FACE('',(#3958),#2706,.F.);
#32707=ADVANCED_FACE('',(#3959),#2238,.F.);
#32708=ADVANCED_FACE('',(#3960),#2707,.F.);
#32709=ADVANCED_FACE('',(#3961),#2708,.F.);
#32710=ADVANCED_FACE('',(#3962),#1140,.F.);
#32711=ADVANCED_FACE('',(#3963),#1141,.T.);
#32712=ADVANCED_FACE('',(#3964),#1142,.F.);
#32713=ADVANCED_FACE('',(#3965),#1143,.F.);
#32714=ADVANCED_FACE('',(#3966),#1144,.F.);
#32715=ADVANCED_FACE('',(#3967),#1145,.F.);
#32716=ADVANCED_FACE('',(#3968),#2709,.F.);
#32717=ADVANCED_FACE('',(#3969),#2710,.T.);
#32718=ADVANCED_FACE('',(#3970),#2239,.F.);
#32719=ADVANCED_FACE('',(#3971),#2711,.T.);
#32720=ADVANCED_FACE('',(#3972),#2712,.F.);
#32721=ADVANCED_FACE('',(#3973),#1146,.F.);
#32722=ADVANCED_FACE('',(#3974),#1147,.T.);
#32723=ADVANCED_FACE('',(#3975),#1148,.F.);
#32724=ADVANCED_FACE('',(#3976),#1149,.T.);
#32725=ADVANCED_FACE('',(#3977),#2713,.T.);
#32726=ADVANCED_FACE('',(#3978),#1150,.F.);
#32727=ADVANCED_FACE('',(#3979),#1151,.T.);
#32728=ADVANCED_FACE('',(#3980),#2714,.T.);
#32729=ADVANCED_FACE('',(#3981),#2715,.T.);
#32730=ADVANCED_FACE('',(#3982),#2716,.F.);
#32731=ADVANCED_FACE('',(#3983),#2717,.T.);
#32732=ADVANCED_FACE('',(#3984),#2240,.T.);
#32733=ADVANCED_FACE('',(#3985),#2718,.T.);
#32734=ADVANCED_FACE('',(#3986),#2719,.F.);
#32735=ADVANCED_FACE('',(#3987),#1152,.T.);
#32736=ADVANCED_FACE('',(#3988),#1153,.T.);
#32737=ADVANCED_FACE('',(#3989),#1154,.F.);
#32738=ADVANCED_FACE('',(#3990),#1155,.T.);
#32739=ADVANCED_FACE('',(#3991,#1292),#2241,.T.);
#32740=ADVANCED_FACE('',(#3992,#1293),#2242,.T.);
#32741=ADVANCED_FACE('',(#3993),#2243,.F.);
#32742=ADVANCED_FACE('',(#3994),#2244,.T.);
#32743=ADVANCED_FACE('',(#3995),#2245,.F.);
#32744=ADVANCED_FACE('',(#3996),#2246,.T.);
#32745=ADVANCED_FACE('',(#3997),#2247,.F.);
#32746=ADVANCED_FACE('',(#3998),#2248,.T.);
#32747=ADVANCED_FACE('',(#3999),#2249,.F.);
#32748=ADVANCED_FACE('',(#4000),#2250,.T.);
#32749=ADVANCED_FACE('',(#4001),#2251,.F.);
#32750=ADVANCED_FACE('',(#4002),#2252,.T.);
#32751=ADVANCED_FACE('',(#4003),#2253,.F.);
#32752=ADVANCED_FACE('',(#4004),#2254,.T.);
#32753=ADVANCED_FACE('',(#4005),#2255,.T.);
#32754=ADVANCED_FACE('',(#4006),#2256,.T.);
#32755=ADVANCED_FACE('',(#4007,#1294),#2257,.T.);
#32756=ADVANCED_FACE('',(#4008),#2258,.T.);
#32757=ADVANCED_FACE('',(#4009),#2259,.T.);
#32758=ADVANCED_FACE('',(#4010),#2720,.T.);
#32759=ADVANCED_FACE('',(#4011),#2721,.T.);
#32760=ADVANCED_FACE('',(#4012),#712,.T.);
#32761=ADVANCED_FACE('',(#4013),#2722,.T.);
#32762=ADVANCED_FACE('',(#4014),#713,.T.);
#32763=ADVANCED_FACE('',(#4015),#122,.T.);
#32764=ADVANCED_FACE('',(#4016),#2723,.T.);
#32765=ADVANCED_FACE('',(#4017),#714,.T.);
#32766=ADVANCED_FACE('',(#4018),#2260,.T.);
#32767=ADVANCED_FACE('',(#4019),#2724,.T.);
#32768=ADVANCED_FACE('',(#4020),#715,.T.);
#32769=ADVANCED_FACE('',(#4021),#2725,.T.);
#32770=ADVANCED_FACE('',(#4022),#716,.T.);
#32771=ADVANCED_FACE('',(#4023),#2726,.T.);
#32772=ADVANCED_FACE('',(#4024),#717,.T.);
#32773=ADVANCED_FACE('',(#4025),#2727,.T.);
#32774=ADVANCED_FACE('',(#4026),#123,.T.);
#32775=ADVANCED_FACE('',(#4027),#124,.T.);
#32776=ADVANCED_FACE('',(#4028),#125,.T.);
#32777=ADVANCED_FACE('',(#4029),#2728,.T.);
#32778=ADVANCED_FACE('',(#4030),#2261,.F.);
#32779=ADVANCED_FACE('',(#4031),#2729,.T.);
#32780=ADVANCED_FACE('',(#4032),#2730,.T.);
#32781=ADVANCED_FACE('',(#4033),#2262,.F.);
#32782=ADVANCED_FACE('',(#4034),#2731,.T.);
#32783=ADVANCED_FACE('',(#4035),#2732,.F.);
#32784=ADVANCED_FACE('',(#4036),#2733,.F.);
#32785=ADVANCED_FACE('',(#4037),#2263,.T.);
#32786=ADVANCED_FACE('',(#4038),#2734,.T.);
#32787=ADVANCED_FACE('',(#4039),#2735,.T.);
#32788=ADVANCED_FACE('',(#4040),#718,.T.);
#32789=ADVANCED_FACE('',(#4041),#2736,.T.);
#32790=ADVANCED_FACE('',(#4042),#719,.T.);
#32791=ADVANCED_FACE('',(#4043),#126,.T.);
#32792=ADVANCED_FACE('',(#4044),#2737,.T.);
#32793=ADVANCED_FACE('',(#4045),#720,.T.);
#32794=ADVANCED_FACE('',(#4046),#2264,.T.);
#32795=ADVANCED_FACE('',(#4047),#2738,.T.);
#32796=ADVANCED_FACE('',(#4048),#721,.T.);
#32797=ADVANCED_FACE('',(#4049),#2739,.T.);
#32798=ADVANCED_FACE('',(#4050),#722,.T.);
#32799=ADVANCED_FACE('',(#4051),#2740,.T.);
#32800=ADVANCED_FACE('',(#4052),#723,.T.);
#32801=ADVANCED_FACE('',(#4053),#2741,.T.);
#32802=ADVANCED_FACE('',(#4054),#127,.T.);
#32803=ADVANCED_FACE('',(#4055),#128,.T.);
#32804=ADVANCED_FACE('',(#4056),#129,.T.);
#32805=ADVANCED_FACE('',(#4057),#2742,.T.);
#32806=ADVANCED_FACE('',(#4058),#2265,.T.);
#32807=ADVANCED_FACE('',(#4059),#2743,.T.);
#32808=ADVANCED_FACE('',(#4060),#2266,.F.);
#32809=ADVANCED_FACE('',(#4061),#2744,.T.);
#32810=ADVANCED_FACE('',(#4062),#2267,.T.);
#32811=ADVANCED_FACE('',(#4063),#2745,.T.);
#32812=ADVANCED_FACE('',(#4064),#2268,.T.);
#32813=ADVANCED_FACE('',(#4065),#2746,.F.);
#32814=ADVANCED_FACE('',(#4066),#2747,.F.);
#32815=ADVANCED_FACE('',(#4067),#2269,.F.);
#32816=ADVANCED_FACE('',(#4068),#2748,.T.);
#32817=ADVANCED_FACE('',(#4069),#2749,.T.);
#32818=ADVANCED_FACE('',(#4070),#724,.T.);
#32819=ADVANCED_FACE('',(#4071),#2750,.T.);
#32820=ADVANCED_FACE('',(#4072),#725,.T.);
#32821=ADVANCED_FACE('',(#4073),#130,.T.);
#32822=ADVANCED_FACE('',(#4074),#2751,.T.);
#32823=ADVANCED_FACE('',(#4075),#726,.T.);
#32824=ADVANCED_FACE('',(#4076),#2270,.T.);
#32825=ADVANCED_FACE('',(#4077),#2752,.T.);
#32826=ADVANCED_FACE('',(#4078),#727,.T.);
#32827=ADVANCED_FACE('',(#4079),#2753,.T.);
#32828=ADVANCED_FACE('',(#4080),#728,.T.);
#32829=ADVANCED_FACE('',(#4081),#2754,.T.);
#32830=ADVANCED_FACE('',(#4082),#729,.T.);
#32831=ADVANCED_FACE('',(#4083),#2755,.T.);
#32832=ADVANCED_FACE('',(#4084),#131,.T.);
#32833=ADVANCED_FACE('',(#4085),#132,.T.);
#32834=ADVANCED_FACE('',(#4086),#133,.T.);
#32835=ADVANCED_FACE('',(#4087),#2756,.T.);
#32836=ADVANCED_FACE('',(#4088),#2271,.T.);
#32837=ADVANCED_FACE('',(#4089),#2757,.T.);
#32838=ADVANCED_FACE('',(#4090),#2758,.T.);
#32839=ADVANCED_FACE('',(#4091),#2272,.T.);
#32840=ADVANCED_FACE('',(#4092),#2759,.T.);
#32841=ADVANCED_FACE('',(#4093),#2760,.F.);
#32842=ADVANCED_FACE('',(#4094),#2761,.F.);
#32843=ADVANCED_FACE('',(#4095),#2273,.F.);
#32844=ADVANCED_FACE('',(#4096),#2762,.T.);
#32845=ADVANCED_FACE('',(#4097),#2763,.T.);
#32846=ADVANCED_FACE('',(#4098),#730,.T.);
#32847=ADVANCED_FACE('',(#4099),#2764,.T.);
#32848=ADVANCED_FACE('',(#4100),#731,.T.);
#32849=ADVANCED_FACE('',(#4101),#2274,.T.);
#32850=ADVANCED_FACE('',(#4102),#2765,.T.);
#32851=ADVANCED_FACE('',(#4103),#732,.T.);
#32852=ADVANCED_FACE('',(#4104),#134,.T.);
#32853=ADVANCED_FACE('',(#4105),#733,.T.);
#32854=ADVANCED_FACE('',(#4106),#2766,.T.);
#32855=ADVANCED_FACE('',(#4107),#734,.T.);
#32856=ADVANCED_FACE('',(#4108),#735,.T.);
#32857=ADVANCED_FACE('',(#4109),#2767,.T.);
#32858=ADVANCED_FACE('',(#4110),#2768,.T.);
#32859=ADVANCED_FACE('',(#4111),#135,.T.);
#32860=ADVANCED_FACE('',(#4112),#136,.T.);
#32861=ADVANCED_FACE('',(#4113),#137,.T.);
#32862=ADVANCED_FACE('',(#4114),#2769,.T.);
#32863=ADVANCED_FACE('',(#4115),#2275,.F.);
#32864=ADVANCED_FACE('',(#4116),#2770,.T.);
#32865=ADVANCED_FACE('',(#4117),#2771,.T.);
#32866=ADVANCED_FACE('',(#4118),#2276,.F.);
#32867=ADVANCED_FACE('',(#4119),#2772,.T.);
#32868=ADVANCED_FACE('',(#4120),#2773,.T.);
#32869=ADVANCED_FACE('',(#4121),#2277,.T.);
#32870=ADVANCED_FACE('',(#4122),#2278,.F.);
#32871=ADVANCED_FACE('',(#4123),#2774,.F.);
#32872=ADVANCED_FACE('',(#4124),#2775,.F.);
#32873=ADVANCED_FACE('',(#4125),#2279,.T.);
#32874=ADVANCED_FACE('',(#4126),#138,.F.);
#32875=ADVANCED_FACE('',(#4127),#139,.F.);
#32876=ADVANCED_FACE('',(#4128),#140,.F.);
#32877=ADVANCED_FACE('',(#4129),#141,.F.);
#32878=ADVANCED_FACE('',(#4130),#142,.F.);
#32879=ADVANCED_FACE('',(#4131),#143,.T.);
#32880=ADVANCED_FACE('',(#4132),#2280,.F.);
#32881=ADVANCED_FACE('',(#4133),#2776,.T.);
#32882=ADVANCED_FACE('',(#4134),#2281,.F.);
#32883=ADVANCED_FACE('',(#4135),#2777,.F.);
#32884=ADVANCED_FACE('',(#4136),#2282,.F.);
#32885=ADVANCED_FACE('',(#4137),#736,.T.);
#32886=ADVANCED_FACE('',(#4138),#144,.T.);
#32887=ADVANCED_FACE('',(#4139),#1156,.T.);
#32888=ADVANCED_FACE('',(#4140,#1295),#737,.T.);
#32889=ADVANCED_FACE('',(#4141),#738,.T.);
#32890=ADVANCED_FACE('',(#4142),#145,.T.);
#32891=ADVANCED_FACE('',(#4143),#1157,.T.);
#32892=ADVANCED_FACE('',(#4144),#146,.T.);
#32893=ADVANCED_FACE('',(#4145),#2283,.T.);
#32894=ADVANCED_FACE('',(#4146),#2778,.F.);
#32895=ADVANCED_FACE('',(#4147,#1296),#2284,.T.);
#32896=ADVANCED_FACE('',(#4148),#2779,.F.);
#32897=ADVANCED_FACE('',(#4149),#147,.F.);
#32898=ADVANCED_FACE('',(#4150),#2780,.F.);
#32899=ADVANCED_FACE('',(#4151),#51,.T.);
#32900=ADVANCED_FACE('',(#4152),#2781,.F.);
#32901=ADVANCED_FACE('',(#4153),#52,.T.);
#32902=ADVANCED_FACE('',(#4154),#2782,.F.);
#32903=ADVANCED_FACE('',(#4155),#148,.T.);
#32904=ADVANCED_FACE('',(#4156),#2285,.F.);
#32905=ADVANCED_FACE('',(#4157),#1158,.F.);
#32906=ADVANCED_FACE('',(#4158),#2783,.T.);
#32907=ADVANCED_FACE('',(#4159),#2286,.F.);
#32908=ADVANCED_FACE('',(#4160),#2784,.F.);
#32909=ADVANCED_FACE('',(#4161),#2287,.F.);
#32910=ADVANCED_FACE('',(#4162),#2785,.F.);
#32911=ADVANCED_FACE('',(#4163),#1159,.T.);
#32912=ADVANCED_FACE('',(#4164),#2288,.T.);
#32913=ADVANCED_FACE('',(#4165),#1160,.F.);
#32914=ADVANCED_FACE('',(#4166),#1161,.F.);
#32915=ADVANCED_FACE('',(#4167),#53,.F.);
#32916=ADVANCED_FACE('',(#4168),#2786,.F.);
#32917=ADVANCED_FACE('',(#4169),#54,.F.);
#32918=ADVANCED_FACE('',(#4170),#2787,.T.);
#32919=ADVANCED_FACE('',(#4171),#2788,.F.);
#32920=ADVANCED_FACE('',(#4172),#149,.T.);
#32921=ADVANCED_FACE('',(#4173),#2789,.T.);
#32922=ADVANCED_FACE('',(#4174),#150,.T.);
#32923=ADVANCED_FACE('',(#4175),#2790,.T.);
#32924=ADVANCED_FACE('',(#4176),#151,.T.);
#32925=ADVANCED_FACE('',(#4177),#1162,.T.);
#32926=ADVANCED_FACE('',(#4178),#2791,.F.);
#32927=ADVANCED_FACE('',(#4179),#2792,.F.);
#32928=ADVANCED_FACE('',(#4180),#2793,.F.);
#32929=ADVANCED_FACE('',(#4181),#2794,.T.);
#32930=ADVANCED_FACE('',(#4182),#2289,.F.);
#32931=ADVANCED_FACE('',(#4183),#1163,.F.);
#32932=ADVANCED_FACE('',(#4184),#2795,.T.);
#32933=ADVANCED_FACE('',(#4185),#152,.F.);
#32934=ADVANCED_FACE('',(#4186),#2796,.T.);
#32935=ADVANCED_FACE('',(#4187),#153,.T.);
#32936=ADVANCED_FACE('',(#4188),#2290,.T.);
#32937=ADVANCED_FACE('',(#4189),#739,.F.);
#32938=ADVANCED_FACE('',(#4190),#154,.F.);
#32939=ADVANCED_FACE('',(#4191,#1297),#2291,.T.);
#32940=ADVANCED_FACE('',(#4192),#155,.F.);
#32941=ADVANCED_FACE('',(#4193),#2292,.T.);
#32942=ADVANCED_FACE('',(#4194),#156,.T.);
#32943=ADVANCED_FACE('',(#4195),#2797,.F.);
#32944=ADVANCED_FACE('',(#4196),#2798,.F.);
#32945=ADVANCED_FACE('',(#4197),#2799,.F.);
#32946=ADVANCED_FACE('',(#4198),#2800,.T.);
#32947=ADVANCED_FACE('',(#4199),#157,.F.);
#32948=ADVANCED_FACE('',(#4200),#158,.F.);
#32949=ADVANCED_FACE('',(#4201),#2801,.T.);
#32950=ADVANCED_FACE('',(#4202),#159,.T.);
#32951=ADVANCED_FACE('',(#4203),#2802,.T.);
#32952=ADVANCED_FACE('',(#4204),#160,.T.);
#32953=ADVANCED_FACE('',(#4205),#161,.T.);
#32954=ADVANCED_FACE('',(#4206),#2803,.T.);
#32955=ADVANCED_FACE('',(#4207),#162,.T.);
#32956=ADVANCED_FACE('',(#4208),#2804,.T.);
#32957=ADVANCED_FACE('',(#4209),#163,.T.);
#32958=ADVANCED_FACE('',(#4210),#2805,.T.);
#32959=ADVANCED_FACE('',(#4211),#164,.T.);
#32960=ADVANCED_FACE('',(#4212),#2806,.T.);
#32961=ADVANCED_FACE('',(#4213),#165,.T.);
#32962=ADVANCED_FACE('',(#4214),#166,.T.);
#32963=ADVANCED_FACE('',(#4215),#2807,.T.);
#32964=ADVANCED_FACE('',(#4216),#167,.T.);
#32965=ADVANCED_FACE('',(#4217),#2808,.T.);
#32966=ADVANCED_FACE('',(#4218),#168,.T.);
#32967=ADVANCED_FACE('',(#4219),#2809,.T.);
#32968=ADVANCED_FACE('',(#4220),#169,.T.);
#32969=ADVANCED_FACE('',(#4221),#2810,.T.);
#32970=ADVANCED_FACE('',(#4222),#170,.T.);
#32971=ADVANCED_FACE('',(#4223),#2811,.T.);
#32972=ADVANCED_FACE('',(#4224),#2812,.T.);
#32973=ADVANCED_FACE('',(#4225),#2813,.T.);
#32974=ADVANCED_FACE('',(#4226),#171,.T.);
#32975=ADVANCED_FACE('',(#4227),#2814,.T.);
#32976=ADVANCED_FACE('',(#4228),#2815,.T.);
#32977=ADVANCED_FACE('',(#4229),#2816,.T.);
#32978=ADVANCED_FACE('',(#4230),#172,.T.);
#32979=ADVANCED_FACE('',(#4231),#2817,.T.);
#32980=ADVANCED_FACE('',(#4232),#173,.F.);
#32981=ADVANCED_FACE('',(#4233),#174,.F.);
#32982=ADVANCED_FACE('',(#4234),#175,.F.);
#32983=ADVANCED_FACE('',(#4235),#2818,.F.);
#32984=ADVANCED_FACE('',(#4236),#176,.F.);
#32985=ADVANCED_FACE('',(#4237),#2819,.F.);
#32986=ADVANCED_FACE('',(#4238),#177,.F.);
#32987=ADVANCED_FACE('',(#4239),#2820,.F.);
#32988=ADVANCED_FACE('',(#4240),#178,.F.);
#32989=ADVANCED_FACE('',(#4241),#2821,.F.);
#32990=ADVANCED_FACE('',(#4242),#740,.F.);
#32991=ADVANCED_FACE('',(#4243),#2822,.F.);
#32992=ADVANCED_FACE('',(#4244),#741,.F.);
#32993=ADVANCED_FACE('',(#4245),#179,.F.);
#32994=ADVANCED_FACE('',(#4246),#2823,.F.);
#32995=ADVANCED_FACE('',(#4247),#1164,.T.);
#32996=ADVANCED_FACE('',(#4248),#2824,.T.);
#32997=ADVANCED_FACE('',(#4249),#742,.F.);
#32998=ADVANCED_FACE('',(#4250),#180,.F.);
#32999=ADVANCED_FACE('',(#4251),#2293,.F.);
#33000=ADVANCED_FACE('',(#4252),#2294,.F.);
#33001=ADVANCED_FACE('',(#4253),#2825,.T.);
#33002=ADVANCED_FACE('',(#4254),#181,.F.);
#33003=ADVANCED_FACE('',(#4255),#2295,.F.);
#33004=ADVANCED_FACE('',(#4256),#1165,.T.);
#33005=ADVANCED_FACE('',(#4257),#2826,.T.);
#33006=ADVANCED_FACE('',(#4258),#1166,.T.);
#33007=ADVANCED_FACE('',(#4259),#2827,.T.);
#33008=ADVANCED_FACE('',(#4260),#743,.T.);
#33009=ADVANCED_FACE('',(#4261),#2296,.T.);
#33010=ADVANCED_FACE('',(#4262),#1167,.T.);
#33011=ADVANCED_FACE('',(#4263),#2828,.T.);
#33012=ADVANCED_FACE('',(#4264),#2297,.T.);
#33013=ADVANCED_FACE('',(#4265),#744,.T.);
#33014=ADVANCED_FACE('',(#4266),#1168,.T.);
#33015=ADVANCED_FACE('',(#4267),#2829,.T.);
#33016=ADVANCED_FACE('',(#4268),#1169,.T.);
#33017=ADVANCED_FACE('',(#4269),#2830,.T.);
#33018=ADVANCED_FACE('',(#4270),#2298,.T.);
#33019=ADVANCED_FACE('',(#4271),#2831,.T.);
#33020=ADVANCED_FACE('',(#4272),#2299,.T.);
#33021=ADVANCED_FACE('',(#4273),#2832,.T.);
#33022=ADVANCED_FACE('',(#4274),#2300,.T.);
#33023=ADVANCED_FACE('',(#4275),#2833,.F.);
#33024=ADVANCED_FACE('',(#4276),#2301,.T.);
#33025=ADVANCED_FACE('',(#4277),#2834,.F.);
#33026=ADVANCED_FACE('',(#4278),#2302,.T.);
#33027=ADVANCED_FACE('',(#4279),#745,.T.);
#33028=ADVANCED_FACE('',(#4280),#2303,.T.);
#33029=ADVANCED_FACE('',(#4281),#746,.T.);
#33030=ADVANCED_FACE('',(#4282),#2304,.T.);
#33031=ADVANCED_FACE('',(#4283),#2835,.F.);
#33032=ADVANCED_FACE('',(#4284),#2305,.T.);
#33033=ADVANCED_FACE('',(#4285),#747,.T.);
#33034=ADVANCED_FACE('',(#4286),#2306,.T.);
#33035=ADVANCED_FACE('',(#4287),#748,.T.);
#33036=ADVANCED_FACE('',(#4288),#2307,.F.);
#33037=ADVANCED_FACE('',(#4289),#2836,.F.);
#33038=ADVANCED_FACE('',(#4290),#2308,.T.);
#33039=ADVANCED_FACE('',(#4291),#2837,.T.);
#33040=ADVANCED_FACE('',(#4292),#182,.T.);
#33041=ADVANCED_FACE('',(#4293),#1170,.T.);
#33042=ADVANCED_FACE('',(#4294),#2838,.T.);
#33043=ADVANCED_FACE('',(#4295),#183,.F.);
#33044=ADVANCED_FACE('',(#4296,#1298),#2309,.F.);
#33045=ADVANCED_FACE('',(#4297),#1171,.T.);
#33046=ADVANCED_FACE('',(#4298),#2839,.T.);
#33047=ADVANCED_FACE('',(#4299),#749,.F.);
#33048=ADVANCED_FACE('',(#4300),#1172,.T.);
#33049=ADVANCED_FACE('',(#4301),#2840,.T.);
#33050=ADVANCED_FACE('',(#4302),#1173,.T.);
#33051=ADVANCED_FACE('',(#4303),#2841,.T.);
#33052=ADVANCED_FACE('',(#4304),#2842,.T.);
#33053=ADVANCED_FACE('',(#4305),#184,.T.);
#33054=ADVANCED_FACE('',(#4306),#2843,.T.);
#33055=ADVANCED_FACE('',(#4307),#185,.T.);
#33056=ADVANCED_FACE('',(#4308),#186,.T.);
#33057=ADVANCED_FACE('',(#4309),#2844,.T.);
#33058=ADVANCED_FACE('',(#4310),#187,.T.);
#33059=ADVANCED_FACE('',(#4311),#2845,.T.);
#33060=ADVANCED_FACE('',(#4312),#188,.T.);
#33061=ADVANCED_FACE('',(#4313),#2846,.T.);
#33062=ADVANCED_FACE('',(#4314),#189,.T.);
#33063=ADVANCED_FACE('',(#4315),#2847,.T.);
#33064=ADVANCED_FACE('',(#4316),#190,.T.);
#33065=ADVANCED_FACE('',(#4317),#2848,.T.);
#33066=ADVANCED_FACE('',(#4318),#2849,.T.);
#33067=ADVANCED_FACE('',(#4319),#2850,.T.);
#33068=ADVANCED_FACE('',(#4320),#2851,.T.);
#33069=ADVANCED_FACE('',(#4321),#2852,.T.);
#33070=ADVANCED_FACE('',(#4322),#191,.T.);
#33071=ADVANCED_FACE('',(#4323),#2853,.T.);
#33072=ADVANCED_FACE('',(#4324),#2854,.T.);
#33073=ADVANCED_FACE('',(#4325),#2855,.T.);
#33074=ADVANCED_FACE('',(#4326),#2856,.T.);
#33075=ADVANCED_FACE('',(#4327),#2857,.T.);
#33076=ADVANCED_FACE('',(#4328),#192,.T.);
#33077=ADVANCED_FACE('',(#4329),#2858,.T.);
#33078=ADVANCED_FACE('',(#4330,#1299),#2310,.T.);
#33079=ADVANCED_FACE('',(#4331),#750,.T.);
#33080=ADVANCED_FACE('',(#4332),#32025,.T.);
#33081=ADVANCED_FACE('',(#4333),#2311,.F.);
#33082=ADVANCED_FACE('',(#4334),#193,.F.);
#33083=ADVANCED_FACE('',(#4335),#2859,.F.);
#33084=ADVANCED_FACE('',(#4336),#194,.F.);
#33085=ADVANCED_FACE('',(#4337),#195,.F.);
#33086=ADVANCED_FACE('',(#4338),#2860,.F.);
#33087=ADVANCED_FACE('',(#4339),#196,.F.);
#33088=ADVANCED_FACE('',(#4340),#751,.F.);
#33089=ADVANCED_FACE('',(#4341),#2861,.F.);
#33090=ADVANCED_FACE('',(#4342),#752,.F.);
#33091=ADVANCED_FACE('',(#4343),#197,.F.);
#33092=ADVANCED_FACE('',(#4344),#2862,.F.);
#33093=ADVANCED_FACE('',(#4345),#198,.F.);
#33094=ADVANCED_FACE('',(#4346),#199,.F.);
#33095=ADVANCED_FACE('',(#4347),#2312,.F.);
#33096=ADVANCED_FACE('',(#4348),#200,.T.);
#33097=ADVANCED_FACE('',(#4349),#753,.T.);
#33098=ADVANCED_FACE('',(#4350),#754,.T.);
#33099=ADVANCED_FACE('',(#4351),#755,.T.);
#33100=ADVANCED_FACE('',(#4352),#756,.T.);
#33101=ADVANCED_FACE('',(#4353),#2863,.F.);
#33102=ADVANCED_FACE('',(#4354),#2864,.T.);
#33103=ADVANCED_FACE('',(#4355),#201,.T.);
#33104=ADVANCED_FACE('',(#4356),#2865,.T.);
#33105=ADVANCED_FACE('',(#4357),#202,.T.);
#33106=ADVANCED_FACE('',(#4358),#2866,.T.);
#33107=ADVANCED_FACE('',(#4359),#757,.F.);
#33108=ADVANCED_FACE('',(#4360),#2867,.F.);
#33109=ADVANCED_FACE('',(#4361),#203,.F.);
#33110=ADVANCED_FACE('',(#4362),#2313,.F.);
#33111=ADVANCED_FACE('',(#4363),#204,.T.);
#33112=ADVANCED_FACE('',(#4364,#1300),#2314,.F.);
#33113=ADVANCED_FACE('',(#4365),#205,.F.);
#33114=ADVANCED_FACE('',(#4366),#2868,.F.);
#33115=ADVANCED_FACE('',(#4367),#55,.T.);
#33116=ADVANCED_FACE('',(#4368),#2869,.F.);
#33117=ADVANCED_FACE('',(#4369),#1174,.T.);
#33118=ADVANCED_FACE('',(#4370),#2870,.T.);
#33119=ADVANCED_FACE('',(#4371),#2871,.T.);
#33120=ADVANCED_FACE('',(#4372),#2872,.F.);
#33121=ADVANCED_FACE('',(#4373),#206,.T.);
#33122=ADVANCED_FACE('',(#4374),#2873,.T.);
#33123=ADVANCED_FACE('',(#4375),#2315,.F.);
#33124=ADVANCED_FACE('',(#4376),#207,.T.);
#33125=ADVANCED_FACE('',(#4377),#758,.T.);
#33126=ADVANCED_FACE('',(#4378),#2874,.T.);
#33127=ADVANCED_FACE('',(#4379),#208,.T.);
#33128=ADVANCED_FACE('',(#4380),#1175,.T.);
#33129=ADVANCED_FACE('',(#4381),#2875,.T.);
#33130=ADVANCED_FACE('',(#4382),#2316,.T.);
#33131=ADVANCED_FACE('',(#4383),#2876,.F.);
#33132=ADVANCED_FACE('',(#4384),#2317,.T.);
#33133=ADVANCED_FACE('',(#4385),#2877,.T.);
#33134=ADVANCED_FACE('',(#4386),#209,.T.);
#33135=ADVANCED_FACE('',(#4387),#2878,.T.);
#33136=ADVANCED_FACE('',(#4388),#210,.T.);
#33137=ADVANCED_FACE('',(#4389),#2879,.T.);
#33138=ADVANCED_FACE('',(#4390),#211,.T.);
#33139=ADVANCED_FACE('',(#4391),#2880,.T.);
#33140=ADVANCED_FACE('',(#4392),#212,.T.);
#33141=ADVANCED_FACE('',(#4393),#2881,.F.);
#33142=ADVANCED_FACE('',(#4394),#2318,.F.);
#33143=ADVANCED_FACE('',(#4395),#2882,.T.);
#33144=ADVANCED_FACE('',(#4396),#2319,.F.);
#33145=ADVANCED_FACE('',(#4397),#2883,.F.);
#33146=ADVANCED_FACE('',(#4398),#2320,.F.);
#33147=ADVANCED_FACE('',(#4399),#2884,.F.);
#33148=ADVANCED_FACE('',(#4400),#56,.T.);
#33149=ADVANCED_FACE('',(#4401),#2885,.F.);
#33150=ADVANCED_FACE('',(#4402),#1176,.F.);
#33151=ADVANCED_FACE('',(#4403),#1177,.F.);
#33152=ADVANCED_FACE('',(#4404),#57,.F.);
#33153=ADVANCED_FACE('',(#4405),#2886,.T.);
#33154=ADVANCED_FACE('',(#4406),#2887,.F.);
#33155=ADVANCED_FACE('',(#4407),#2888,.T.);
#33156=ADVANCED_FACE('',(#4408),#2889,.F.);
#33157=ADVANCED_FACE('',(#4409),#2321,.F.);
#33158=ADVANCED_FACE('',(#4410),#1178,.T.);
#33159=ADVANCED_FACE('',(#4411),#1179,.T.);
#33160=ADVANCED_FACE('',(#4412),#58,.F.);
#33161=ADVANCED_FACE('',(#4413),#213,.T.);
#33162=ADVANCED_FACE('',(#4414),#1180,.T.);
#33163=ADVANCED_FACE('',(#4415),#1181,.T.);
#33164=ADVANCED_FACE('',(#4416),#2890,.F.);
#33165=ADVANCED_FACE('',(#4417),#2322,.F.);
#33166=ADVANCED_FACE('',(#4418),#59,.F.);
#33167=ADVANCED_FACE('',(#4419),#32026,.T.);
#33168=ADVANCED_FACE('',(#4420),#2891,.F.);
#33169=ADVANCED_FACE('',(#4421,#1301),#2323,.T.);
#33170=ADVANCED_FACE('',(#4422),#2324,.F.);
#33171=ADVANCED_FACE('',(#4423),#2325,.T.);
#33172=ADVANCED_FACE('',(#4424),#2326,.F.);
#33173=ADVANCED_FACE('',(#4425),#2327,.F.);
#33174=ADVANCED_FACE('',(#4426),#2328,.F.);
#33175=ADVANCED_FACE('',(#4427),#2329,.F.);
#33176=ADVANCED_FACE('',(#4428),#2330,.T.);
#33177=ADVANCED_FACE('',(#4429),#2331,.F.);
#33178=ADVANCED_FACE('',(#4430,#1302,#1303),#2892,.F.);
#33179=ADVANCED_FACE('',(#4431,#1304,#1305),#2893,.T.);
#33180=ADVANCED_FACE('',(#4432),#2332,.F.);
#33181=ADVANCED_FACE('',(#4433),#2333,.T.);
#33182=ADVANCED_FACE('',(#4434),#2894,.T.);
#33183=ADVANCED_FACE('',(#4435),#2895,.T.);
#33184=ADVANCED_FACE('',(#4436),#2896,.F.);
#33185=ADVANCED_FACE('',(#4437),#2897,.F.);
#33186=ADVANCED_FACE('',(#4438),#2898,.T.);
#33187=ADVANCED_FACE('',(#4439),#2334,.F.);
#33188=ADVANCED_FACE('',(#4440),#2899,.T.);
#33189=ADVANCED_FACE('',(#4441),#2335,.T.);
#33190=ADVANCED_FACE('',(#4442),#2336,.T.);
#33191=ADVANCED_FACE('',(#4443),#2900,.F.);
#33192=ADVANCED_FACE('',(#4444),#2337,.F.);
#33193=ADVANCED_FACE('',(#4445),#2901,.T.);
#33194=ADVANCED_FACE('',(#4446),#60,.F.);
#33195=ADVANCED_FACE('',(#4447),#2902,.T.);
#33196=ADVANCED_FACE('',(#4448),#2338,.T.);
#33197=ADVANCED_FACE('',(#4449),#2903,.F.);
#33198=ADVANCED_FACE('',(#4450),#2339,.F.);
#33199=ADVANCED_FACE('',(#4451),#2904,.F.);
#33200=ADVANCED_FACE('',(#4452),#1182,.T.);
#33201=ADVANCED_FACE('',(#4453),#2905,.T.);
#33202=ADVANCED_FACE('',(#4454),#1183,.T.);
#33203=ADVANCED_FACE('',(#4455),#214,.F.);
#33204=ADVANCED_FACE('',(#4456),#2906,.F.);
#33205=ADVANCED_FACE('',(#4457),#2340,.T.);
#33206=ADVANCED_FACE('',(#4458),#1184,.F.);
#33207=ADVANCED_FACE('',(#4459),#2907,.T.);
#33208=ADVANCED_FACE('',(#4460),#1185,.T.);
#33209=ADVANCED_FACE('',(#4461),#1186,.T.);
#33210=ADVANCED_FACE('',(#4462),#2908,.T.);
#33211=ADVANCED_FACE('',(#4463),#2341,.T.);
#33212=ADVANCED_FACE('',(#4464),#2909,.F.);
#33213=ADVANCED_FACE('',(#4465),#2910,.F.);
#33214=ADVANCED_FACE('',(#4466),#2342,.T.);
#33215=ADVANCED_FACE('',(#4467),#2911,.T.);
#33216=ADVANCED_FACE('',(#4468),#61,.F.);
#33217=ADVANCED_FACE('',(#4469,#1306),#2343,.T.);
#33218=ADVANCED_FACE('',(#4470),#2912,.T.);
#33219=ADVANCED_FACE('',(#4471),#2344,.F.);
#33220=ADVANCED_FACE('',(#4472),#2913,.F.);
#33221=ADVANCED_FACE('',(#4473),#2345,.T.);
#33222=ADVANCED_FACE('',(#4474),#2914,.F.);
#33223=ADVANCED_FACE('',(#4475),#2915,.T.);
#33224=ADVANCED_FACE('',(#4476),#215,.T.);
#33225=ADVANCED_FACE('',(#4477),#1187,.F.);
#33226=ADVANCED_FACE('',(#4478),#2916,.T.);
#33227=ADVANCED_FACE('',(#4479),#1188,.F.);
#33228=ADVANCED_FACE('',(#4480),#216,.F.);
#33229=ADVANCED_FACE('',(#4481),#2917,.F.);
#33230=ADVANCED_FACE('',(#4482),#2346,.T.);
#33231=ADVANCED_FACE('',(#4483),#1189,.T.);
#33232=ADVANCED_FACE('',(#4484),#2918,.T.);
#33233=ADVANCED_FACE('',(#4485),#1190,.F.);
#33234=ADVANCED_FACE('',(#4486),#1191,.F.);
#33235=ADVANCED_FACE('',(#4487),#2919,.T.);
#33236=ADVANCED_FACE('',(#4488),#2347,.F.);
#33237=ADVANCED_FACE('',(#4489),#2348,.F.);
#33238=ADVANCED_FACE('',(#4490),#2349,.T.);
#33239=ADVANCED_FACE('',(#4491),#2920,.T.);
#33240=ADVANCED_FACE('',(#4492),#2921,.T.);
#33241=ADVANCED_FACE('',(#4493),#2922,.F.);
#33242=ADVANCED_FACE('',(#4494),#2923,.F.);
#33243=ADVANCED_FACE('',(#4495),#2924,.T.);
#33244=ADVANCED_FACE('',(#4496),#2350,.F.);
#33245=ADVANCED_FACE('',(#4497),#2925,.T.);
#33246=ADVANCED_FACE('',(#4498),#2351,.T.);
#33247=ADVANCED_FACE('',(#4499),#2352,.T.);
#33248=ADVANCED_FACE('',(#4500),#2353,.T.);
#33249=ADVANCED_FACE('',(#4501),#2926,.F.);
#33250=ADVANCED_FACE('',(#4502),#2354,.T.);
#33251=ADVANCED_FACE('',(#4503),#2927,.F.);
#33252=ADVANCED_FACE('',(#4504),#2355,.F.);
#33253=ADVANCED_FACE('',(#4505),#2356,.T.);
#33254=ADVANCED_FACE('',(#4506),#2928,.F.);
#33255=ADVANCED_FACE('',(#4507),#2357,.T.);
#33256=ADVANCED_FACE('',(#4508),#2929,.F.);
#33257=ADVANCED_FACE('',(#4509),#2358,.F.);
#33258=ADVANCED_FACE('',(#4510),#2930,.T.);
#33259=ADVANCED_FACE('',(#4511),#2931,.T.);
#33260=ADVANCED_FACE('',(#4512),#2359,.F.);
#33261=ADVANCED_FACE('',(#4513),#2932,.T.);
#33262=ADVANCED_FACE('',(#4514),#2933,.T.);
#33263=ADVANCED_FACE('',(#4515),#2360,.F.);
#33264=ADVANCED_FACE('',(#4516),#2934,.F.);
#33265=ADVANCED_FACE('',(#4517),#2361,.F.);
#33266=ADVANCED_FACE('',(#4518),#2362,.F.);
#33267=ADVANCED_FACE('',(#4519),#2363,.F.);
#33268=ADVANCED_FACE('',(#4520),#2364,.F.);
#33269=ADVANCED_FACE('',(#4521,#1307),#2365,.F.);
#33270=ADVANCED_FACE('',(#4522),#2366,.F.);
#33271=ADVANCED_FACE('',(#4523,#1308),#2367,.T.);
#33272=ADVANCED_FACE('',(#4524),#2368,.F.);
#33273=ADVANCED_FACE('',(#4525),#2935,.T.);
#33274=ADVANCED_FACE('',(#4526),#2369,.F.);
#33275=ADVANCED_FACE('',(#4527),#2936,.T.);
#33276=ADVANCED_FACE('',(#4528),#2370,.F.);
#33277=ADVANCED_FACE('',(#4529),#2937,.T.);
#33278=ADVANCED_FACE('',(#4530),#2371,.F.);
#33279=ADVANCED_FACE('',(#4531),#2938,.T.);
#33280=ADVANCED_FACE('',(#4532),#2372,.F.);
#33281=ADVANCED_FACE('',(#4533),#2939,.T.);
#33282=ADVANCED_FACE('',(#4534),#2373,.F.);
#33283=ADVANCED_FACE('',(#4535),#2940,.T.);
#33284=ADVANCED_FACE('',(#4536),#62,.F.);
#33285=ADVANCED_FACE('',(#4537),#2941,.T.);
#33286=ADVANCED_FACE('',(#4538),#2942,.F.);
#33287=ADVANCED_FACE('',(#4539),#2943,.T.);
#33288=ADVANCED_FACE('',(#4540),#2944,.F.);
#33289=ADVANCED_FACE('',(#4541),#2945,.F.);
#33290=ADVANCED_FACE('',(#4542),#2374,.T.);
#33291=ADVANCED_FACE('',(#4543),#2946,.T.);
#33292=ADVANCED_FACE('',(#4544),#2947,.F.);
#33293=ADVANCED_FACE('',(#4545),#2948,.T.);
#33294=ADVANCED_FACE('',(#4546),#2375,.F.);
#33295=ADVANCED_FACE('',(#4547),#2949,.T.);
#33296=ADVANCED_FACE('',(#4548),#759,.T.);
#33297=ADVANCED_FACE('',(#4549),#217,.T.);
#33298=ADVANCED_FACE('',(#4550),#760,.T.);
#33299=ADVANCED_FACE('',(#4551),#2950,.T.);
#33300=ADVANCED_FACE('',(#4552),#218,.T.);
#33301=ADVANCED_FACE('',(#4553),#219,.T.);
#33302=ADVANCED_FACE('',(#4554),#220,.T.);
#33303=ADVANCED_FACE('',(#4555),#221,.T.);
#33304=ADVANCED_FACE('',(#4556),#222,.T.);
#33305=ADVANCED_FACE('',(#4557),#2951,.T.);
#33306=ADVANCED_FACE('',(#4558),#761,.T.);
#33307=ADVANCED_FACE('',(#4559),#223,.T.);
#33308=ADVANCED_FACE('',(#4560),#762,.T.);
#33309=ADVANCED_FACE('',(#4561),#2952,.T.);
#33310=ADVANCED_FACE('',(#4562),#2376,.T.);
#33311=ADVANCED_FACE('',(#4563),#2377,.T.);
#33312=ADVANCED_FACE('',(#4564),#2953,.T.);
#33313=ADVANCED_FACE('',(#4565),#2954,.F.);
#33314=ADVANCED_FACE('',(#4566),#2955,.T.);
#33315=ADVANCED_FACE('',(#4567),#2378,.F.);
#33316=ADVANCED_FACE('',(#4568),#2956,.F.);
#33317=ADVANCED_FACE('',(#4569),#2957,.T.);
#33318=ADVANCED_FACE('',(#4570),#2958,.T.);
#33319=ADVANCED_FACE('',(#4571),#763,.T.);
#33320=ADVANCED_FACE('',(#4572),#224,.T.);
#33321=ADVANCED_FACE('',(#4573),#764,.T.);
#33322=ADVANCED_FACE('',(#4574),#2959,.T.);
#33323=ADVANCED_FACE('',(#4575),#225,.T.);
#33324=ADVANCED_FACE('',(#4576),#226,.T.);
#33325=ADVANCED_FACE('',(#4577),#765,.T.);
#33326=ADVANCED_FACE('',(#4578),#227,.T.);
#33327=ADVANCED_FACE('',(#4579),#2960,.F.);
#33328=ADVANCED_FACE('',(#4580),#228,.F.);
#33329=ADVANCED_FACE('',(#4581),#2961,.F.);
#33330=ADVANCED_FACE('',(#4582),#229,.F.);
#33331=ADVANCED_FACE('',(#4583),#766,.F.);
#33332=ADVANCED_FACE('',(#4584),#2379,.F.);
#33333=ADVANCED_FACE('',(#4585),#767,.F.);
#33334=ADVANCED_FACE('',(#4586),#2962,.T.);
#33335=ADVANCED_FACE('',(#4587),#768,.F.);
#33336=ADVANCED_FACE('',(#4588),#2380,.F.);
#33337=ADVANCED_FACE('',(#4589),#769,.F.);
#33338=ADVANCED_FACE('',(#4590),#2963,.F.);
#33339=ADVANCED_FACE('',(#4591),#2964,.F.);
#33340=ADVANCED_FACE('',(#4592),#2965,.T.);
#33341=ADVANCED_FACE('',(#4593),#2966,.F.);
#33342=ADVANCED_FACE('',(#4594),#230,.T.);
#33343=ADVANCED_FACE('',(#4595),#2967,.F.);
#33344=ADVANCED_FACE('',(#4596),#2968,.T.);
#33345=ADVANCED_FACE('',(#4597),#2969,.F.);
#33346=ADVANCED_FACE('',(#4598),#231,.T.);
#33347=ADVANCED_FACE('',(#4599),#232,.T.);
#33348=ADVANCED_FACE('',(#4600),#770,.F.);
#33349=ADVANCED_FACE('',(#4601),#233,.T.);
#33350=ADVANCED_FACE('',(#4602),#234,.T.);
#33351=ADVANCED_FACE('',(#4603),#235,.T.);
#33352=ADVANCED_FACE('',(#4604),#236,.T.);
#33353=ADVANCED_FACE('',(#4605),#2381,.F.);
#33354=ADVANCED_FACE('',(#4606),#1192,.T.);
#33355=ADVANCED_FACE('',(#4607),#237,.T.);
#33356=ADVANCED_FACE('',(#4608),#2382,.F.);
#33357=ADVANCED_FACE('',(#4609),#2970,.T.);
#33358=ADVANCED_FACE('',(#4610),#2383,.F.);
#33359=ADVANCED_FACE('',(#4611),#2971,.F.);
#33360=ADVANCED_FACE('',(#4612),#2384,.F.);
#33361=ADVANCED_FACE('',(#4613),#2972,.F.);
#33362=ADVANCED_FACE('',(#4614),#2385,.F.);
#33363=ADVANCED_FACE('',(#4615),#2973,.F.);
#33364=ADVANCED_FACE('',(#4616),#771,.T.);
#33365=ADVANCED_FACE('',(#4617),#238,.T.);
#33366=ADVANCED_FACE('',(#4618),#2974,.T.);
#33367=ADVANCED_FACE('',(#4619),#2386,.F.);
#33368=ADVANCED_FACE('',(#4620),#2975,.F.);
#33369=ADVANCED_FACE('',(#4621),#2976,.T.);
#33370=ADVANCED_FACE('',(#4622),#2977,.F.);
#33371=ADVANCED_FACE('',(#4623),#2387,.F.);
#33372=ADVANCED_FACE('',(#4624),#2978,.F.);
#33373=ADVANCED_FACE('',(#4625),#2979,.F.);
#33374=ADVANCED_FACE('',(#4626),#2980,.F.);
#33375=ADVANCED_FACE('',(#4627),#2981,.T.);
#33376=ADVANCED_FACE('',(#4628),#239,.T.);
#33377=ADVANCED_FACE('',(#4629),#240,.T.);
#33378=ADVANCED_FACE('',(#4630),#2982,.T.);
#33379=ADVANCED_FACE('',(#4631),#241,.T.);
#33380=ADVANCED_FACE('',(#4632),#242,.T.);
#33381=ADVANCED_FACE('',(#4633),#243,.T.);
#33382=ADVANCED_FACE('',(#4634),#244,.T.);
#33383=ADVANCED_FACE('',(#4635),#2983,.T.);
#33384=ADVANCED_FACE('',(#4636),#245,.T.);
#33385=ADVANCED_FACE('',(#4637),#1193,.F.);
#33386=ADVANCED_FACE('',(#4638),#246,.T.);
#33387=ADVANCED_FACE('',(#4639),#1194,.F.);
#33388=ADVANCED_FACE('',(#4640),#1195,.F.);
#33389=ADVANCED_FACE('',(#4641),#1196,.F.);
#33390=ADVANCED_FACE('',(#4642),#247,.T.);
#33391=ADVANCED_FACE('',(#4643),#248,.T.);
#33392=ADVANCED_FACE('',(#4644),#249,.T.);
#33393=ADVANCED_FACE('',(#4645),#2984,.T.);
#33394=ADVANCED_FACE('',(#4646),#1197,.F.);
#33395=ADVANCED_FACE('',(#4647),#1198,.F.);
#33396=ADVANCED_FACE('',(#4648),#1199,.F.);
#33397=ADVANCED_FACE('',(#4649),#250,.T.);
#33398=ADVANCED_FACE('',(#4650),#251,.T.);
#33399=ADVANCED_FACE('',(#4651),#2985,.T.);
#33400=ADVANCED_FACE('',(#4652),#252,.T.);
#33401=ADVANCED_FACE('',(#4653),#253,.T.);
#33402=ADVANCED_FACE('',(#4654),#254,.T.);
#33403=ADVANCED_FACE('',(#4655),#255,.T.);
#33404=ADVANCED_FACE('',(#4656),#2986,.T.);
#33405=ADVANCED_FACE('',(#4657),#2987,.F.);
#33406=ADVANCED_FACE('',(#4658),#2988,.F.);
#33407=ADVANCED_FACE('',(#4659),#256,.F.);
#33408=ADVANCED_FACE('',(#4660),#772,.F.);
#33409=ADVANCED_FACE('',(#4661),#257,.F.);
#33410=ADVANCED_FACE('',(#4662),#773,.F.);
#33411=ADVANCED_FACE('',(#4663),#774,.F.);
#33412=ADVANCED_FACE('',(#4664),#775,.F.);
#33413=ADVANCED_FACE('',(#4665),#2989,.F.);
#33414=ADVANCED_FACE('',(#4666),#258,.F.);
#33415=ADVANCED_FACE('',(#4667),#259,.T.);
#33416=ADVANCED_FACE('',(#4668),#260,.T.);
#33417=ADVANCED_FACE('',(#4669),#261,.T.);
#33418=ADVANCED_FACE('',(#4670),#262,.T.);
#33419=ADVANCED_FACE('',(#4671),#776,.F.);
#33420=ADVANCED_FACE('',(#4672),#2990,.T.);
#33421=ADVANCED_FACE('',(#4673),#777,.T.);
#33422=ADVANCED_FACE('',(#4674),#263,.F.);
#33423=ADVANCED_FACE('',(#4675),#2991,.F.);
#33424=ADVANCED_FACE('',(#4676),#264,.F.);
#33425=ADVANCED_FACE('',(#4677),#2388,.T.);
#33426=ADVANCED_FACE('',(#4678),#265,.T.);
#33427=ADVANCED_FACE('',(#4679),#266,.T.);
#33428=ADVANCED_FACE('',(#4680),#267,.T.);
#33429=ADVANCED_FACE('',(#4681),#268,.T.);
#33430=ADVANCED_FACE('',(#4682),#2992,.T.);
#33431=ADVANCED_FACE('',(#4683),#778,.T.);
#33432=ADVANCED_FACE('',(#4684),#269,.T.);
#33433=ADVANCED_FACE('',(#4685),#270,.T.);
#33434=ADVANCED_FACE('',(#4686),#2993,.T.);
#33435=ADVANCED_FACE('',(#4687),#1200,.F.);
#33436=ADVANCED_FACE('',(#4688),#271,.T.);
#33437=ADVANCED_FACE('',(#4689),#1201,.F.);
#33438=ADVANCED_FACE('',(#4690),#779,.T.);
#33439=ADVANCED_FACE('',(#4691),#2994,.T.);
#33440=ADVANCED_FACE('',(#4692),#2995,.T.);
#33441=ADVANCED_FACE('',(#4693),#780,.T.);
#33442=ADVANCED_FACE('',(#4694),#2996,.T.);
#33443=ADVANCED_FACE('',(#4695),#2997,.T.);
#33444=ADVANCED_FACE('',(#4696),#2389,.F.);
#33445=ADVANCED_FACE('',(#4697),#1202,.F.);
#33446=ADVANCED_FACE('',(#4698),#2998,.F.);
#33447=ADVANCED_FACE('',(#4699),#2999,.F.);
#33448=ADVANCED_FACE('',(#4700),#781,.F.);
#33449=ADVANCED_FACE('',(#4701),#272,.F.);
#33450=ADVANCED_FACE('',(#4702),#782,.F.);
#33451=ADVANCED_FACE('',(#4703),#3000,.F.);
#33452=ADVANCED_FACE('',(#4704),#783,.F.);
#33453=ADVANCED_FACE('',(#4705),#784,.F.);
#33454=ADVANCED_FACE('',(#4706),#273,.F.);
#33455=ADVANCED_FACE('',(#4707),#2390,.F.);
#33456=ADVANCED_FACE('',(#4708),#785,.F.);
#33457=ADVANCED_FACE('',(#4709),#2391,.F.);
#33458=ADVANCED_FACE('',(#4710),#3001,.T.);
#33459=ADVANCED_FACE('',(#4711),#3002,.F.);
#33460=ADVANCED_FACE('',(#4712),#2392,.F.);
#33461=ADVANCED_FACE('',(#4713),#3003,.F.);
#33462=ADVANCED_FACE('',(#4714),#3004,.F.);
#33463=ADVANCED_FACE('',(#4715),#3005,.F.);
#33464=ADVANCED_FACE('',(#4716),#3006,.F.);
#33465=ADVANCED_FACE('',(#4717),#2393,.F.);
#33466=ADVANCED_FACE('',(#4718),#3007,.F.);
#33467=ADVANCED_FACE('',(#4719),#3008,.F.);
#33468=ADVANCED_FACE('',(#4720),#3009,.T.);
#33469=ADVANCED_FACE('',(#4721),#3010,.F.);
#33470=ADVANCED_FACE('',(#4722),#3011,.F.);
#33471=ADVANCED_FACE('',(#4723),#2394,.F.);
#33472=ADVANCED_FACE('',(#4724),#3012,.T.);
#33473=ADVANCED_FACE('',(#4725),#3013,.F.);
#33474=ADVANCED_FACE('',(#4726),#2395,.T.);
#33475=ADVANCED_FACE('',(#4727),#3014,.F.);
#33476=ADVANCED_FACE('',(#4728),#3015,.F.);
#33477=ADVANCED_FACE('',(#4729),#3016,.F.);
#33478=ADVANCED_FACE('',(#4730),#3017,.F.);
#33479=ADVANCED_FACE('',(#4731),#2396,.T.);
#33480=ADVANCED_FACE('',(#4732),#786,.F.);
#33481=ADVANCED_FACE('',(#4733),#274,.F.);
#33482=ADVANCED_FACE('',(#4734),#787,.F.);
#33483=ADVANCED_FACE('',(#4735),#788,.F.);
#33484=ADVANCED_FACE('',(#4736),#3018,.F.);
#33485=ADVANCED_FACE('',(#4737),#2397,.F.);
#33486=ADVANCED_FACE('',(#4738),#789,.T.);
#33487=ADVANCED_FACE('',(#4739),#790,.F.);
#33488=ADVANCED_FACE('',(#4740),#2398,.F.);
#33489=ADVANCED_FACE('',(#4741),#2399,.F.);
#33490=ADVANCED_FACE('',(#4742),#3019,.F.);
#33491=ADVANCED_FACE('',(#4743),#3020,.F.);
#33492=ADVANCED_FACE('',(#4744),#791,.F.);
#33493=ADVANCED_FACE('',(#4745),#275,.F.);
#33494=ADVANCED_FACE('',(#4746),#3021,.T.);
#33495=ADVANCED_FACE('',(#4747),#1203,.T.);
#33496=ADVANCED_FACE('',(#4748),#3022,.F.);
#33497=ADVANCED_FACE('',(#4749),#3023,.F.);
#33498=ADVANCED_FACE('',(#4750),#792,.F.);
#33499=ADVANCED_FACE('',(#4751),#276,.F.);
#33500=ADVANCED_FACE('',(#4752),#277,.T.);
#33501=ADVANCED_FACE('',(#4753),#793,.F.);
#33502=ADVANCED_FACE('',(#4754),#3024,.F.);
#33503=ADVANCED_FACE('',(#4755),#3025,.T.);
#33504=ADVANCED_FACE('',(#4756),#278,.F.);
#33505=ADVANCED_FACE('',(#4757),#3026,.F.);
#33506=ADVANCED_FACE('',(#4758),#279,.F.);
#33507=ADVANCED_FACE('',(#4759),#280,.F.);
#33508=ADVANCED_FACE('',(#4760),#281,.F.);
#33509=ADVANCED_FACE('',(#4761),#3027,.F.);
#33510=ADVANCED_FACE('',(#4762),#794,.F.);
#33511=ADVANCED_FACE('',(#4763),#282,.F.);
#33512=ADVANCED_FACE('',(#4764),#795,.F.);
#33513=ADVANCED_FACE('',(#4765),#283,.F.);
#33514=ADVANCED_FACE('',(#4766),#3028,.F.);
#33515=ADVANCED_FACE('',(#4767),#3029,.F.);
#33516=ADVANCED_FACE('',(#4768),#3030,.F.);
#33517=ADVANCED_FACE('',(#4769),#3031,.F.);
#33518=ADVANCED_FACE('',(#4770),#796,.F.);
#33519=ADVANCED_FACE('',(#4771),#3032,.F.);
#33520=ADVANCED_FACE('',(#4772),#2400,.T.);
#33521=ADVANCED_FACE('',(#4773),#3033,.T.);
#33522=ADVANCED_FACE('',(#4774),#1204,.F.);
#33523=ADVANCED_FACE('',(#4775),#3034,.T.);
#33524=ADVANCED_FACE('',(#4776),#284,.T.);
#33525=ADVANCED_FACE('',(#4777),#285,.T.);
#33526=ADVANCED_FACE('',(#4778),#286,.T.);
#33527=ADVANCED_FACE('',(#4779),#3035,.T.);
#33528=ADVANCED_FACE('',(#4780),#1205,.F.);
#33529=ADVANCED_FACE('',(#4781),#287,.T.);
#33530=ADVANCED_FACE('',(#4782),#288,.T.);
#33531=ADVANCED_FACE('',(#4783),#289,.T.);
#33532=ADVANCED_FACE('',(#4784),#290,.F.);
#33533=ADVANCED_FACE('',(#4785),#291,.F.);
#33534=ADVANCED_FACE('',(#4786),#1206,.F.);
#33535=ADVANCED_FACE('',(#4787),#1207,.F.);
#33536=ADVANCED_FACE('',(#4788),#3036,.F.);
#33537=ADVANCED_FACE('',(#4789),#1208,.F.);
#33538=ADVANCED_FACE('',(#4790),#3037,.F.);
#33539=ADVANCED_FACE('',(#4791),#1209,.F.);
#33540=ADVANCED_FACE('',(#4792),#3038,.F.);
#33541=ADVANCED_FACE('',(#4793),#292,.T.);
#33542=ADVANCED_FACE('',(#4794),#293,.T.);
#33543=ADVANCED_FACE('',(#4795),#1210,.F.);
#33544=ADVANCED_FACE('',(#4796),#1211,.F.);
#33545=ADVANCED_FACE('',(#4797),#294,.T.);
#33546=ADVANCED_FACE('',(#4798),#295,.T.);
#33547=ADVANCED_FACE('',(#4799),#3039,.T.);
#33548=ADVANCED_FACE('',(#4800),#296,.T.);
#33549=ADVANCED_FACE('',(#4801),#297,.T.);
#33550=ADVANCED_FACE('',(#4802),#298,.T.);
#33551=ADVANCED_FACE('',(#4803),#1212,.T.);
#33552=ADVANCED_FACE('',(#4804),#1213,.F.);
#33553=ADVANCED_FACE('',(#4805),#3040,.T.);
#33554=ADVANCED_FACE('',(#4806),#3041,.F.);
#33555=ADVANCED_FACE('',(#4807),#3042,.F.);
#33556=ADVANCED_FACE('',(#4808),#3043,.F.);
#33557=ADVANCED_FACE('',(#4809),#3044,.F.);
#33558=ADVANCED_FACE('',(#4810),#3045,.F.);
#33559=ADVANCED_FACE('',(#4811),#3046,.F.);
#33560=ADVANCED_FACE('',(#4812),#2401,.T.);
#33561=ADVANCED_FACE('',(#4813),#3047,.F.);
#33562=ADVANCED_FACE('',(#4814),#3048,.T.);
#33563=ADVANCED_FACE('',(#4815),#3049,.F.);
#33564=ADVANCED_FACE('',(#4816),#2402,.T.);
#33565=ADVANCED_FACE('',(#4817),#3050,.F.);
#33566=ADVANCED_FACE('',(#4818),#797,.F.);
#33567=ADVANCED_FACE('',(#4819),#299,.F.);
#33568=ADVANCED_FACE('',(#4820),#300,.F.);
#33569=ADVANCED_FACE('',(#4821),#798,.F.);
#33570=ADVANCED_FACE('',(#4822),#301,.F.);
#33571=ADVANCED_FACE('',(#4823),#799,.F.);
#33572=ADVANCED_FACE('',(#4824),#302,.F.);
#33573=ADVANCED_FACE('',(#4825),#800,.F.);
#33574=ADVANCED_FACE('',(#4826),#3051,.F.);
#33575=ADVANCED_FACE('',(#4827),#801,.F.);
#33576=ADVANCED_FACE('',(#4828),#303,.F.);
#33577=ADVANCED_FACE('',(#4829),#802,.F.);
#33578=ADVANCED_FACE('',(#4830),#3052,.F.);
#33579=ADVANCED_FACE('',(#4831),#3053,.F.);
#33580=ADVANCED_FACE('',(#4832),#304,.F.);
#33581=ADVANCED_FACE('',(#4833),#305,.F.);
#33582=ADVANCED_FACE('',(#4834),#306,.F.);
#33583=ADVANCED_FACE('',(#4835),#2403,.F.);
#33584=ADVANCED_FACE('',(#4836),#3054,.T.);
#33585=ADVANCED_FACE('',(#4837),#3055,.F.);
#33586=ADVANCED_FACE('',(#4838),#3056,.T.);
#33587=ADVANCED_FACE('',(#4839),#3057,.F.);
#33588=ADVANCED_FACE('',(#4840),#3058,.F.);
#33589=ADVANCED_FACE('',(#4841),#2404,.F.);
#33590=ADVANCED_FACE('',(#4842),#3059,.T.);
#33591=ADVANCED_FACE('',(#4843),#3060,.F.);
#33592=ADVANCED_FACE('',(#4844),#3061,.T.);
#33593=ADVANCED_FACE('',(#4845),#2405,.T.);
#33594=ADVANCED_FACE('',(#4846),#3062,.T.);
#33595=ADVANCED_FACE('',(#4847),#803,.T.);
#33596=ADVANCED_FACE('',(#4848),#307,.T.);
#33597=ADVANCED_FACE('',(#4849),#804,.T.);
#33598=ADVANCED_FACE('',(#4850),#3063,.T.);
#33599=ADVANCED_FACE('',(#4851),#308,.T.);
#33600=ADVANCED_FACE('',(#4852),#309,.T.);
#33601=ADVANCED_FACE('',(#4853),#310,.T.);
#33602=ADVANCED_FACE('',(#4854),#311,.T.);
#33603=ADVANCED_FACE('',(#4855),#312,.T.);
#33604=ADVANCED_FACE('',(#4856),#3064,.T.);
#33605=ADVANCED_FACE('',(#4857),#805,.T.);
#33606=ADVANCED_FACE('',(#4858),#313,.T.);
#33607=ADVANCED_FACE('',(#4859),#806,.T.);
#33608=ADVANCED_FACE('',(#4860),#3065,.T.);
#33609=ADVANCED_FACE('',(#4861),#2406,.T.);
#33610=ADVANCED_FACE('',(#4862),#2407,.F.);
#33611=ADVANCED_FACE('',(#4863),#3066,.T.);
#33612=ADVANCED_FACE('',(#4864),#3067,.F.);
#33613=ADVANCED_FACE('',(#4865),#3068,.T.);
#33614=ADVANCED_FACE('',(#4866),#2408,.T.);
#33615=ADVANCED_FACE('',(#4867),#3069,.F.);
#33616=ADVANCED_FACE('',(#4868),#3070,.T.);
#33617=ADVANCED_FACE('',(#4869),#3071,.T.);
#33618=ADVANCED_FACE('',(#4870),#807,.T.);
#33619=ADVANCED_FACE('',(#4871),#314,.T.);
#33620=ADVANCED_FACE('',(#4872),#808,.T.);
#33621=ADVANCED_FACE('',(#4873),#3072,.T.);
#33622=ADVANCED_FACE('',(#4874),#315,.T.);
#33623=ADVANCED_FACE('',(#4875),#1214,.F.);
#33624=ADVANCED_FACE('',(#4876),#316,.T.);
#33625=ADVANCED_FACE('',(#4877),#809,.T.);
#33626=ADVANCED_FACE('',(#4878),#1215,.F.);
#33627=ADVANCED_FACE('',(#4879),#317,.T.);
#33628=ADVANCED_FACE('',(#4880),#2409,.T.);
#33629=ADVANCED_FACE('',(#4881),#3073,.F.);
#33630=ADVANCED_FACE('',(#4882),#318,.F.);
#33631=ADVANCED_FACE('',(#4883),#3074,.F.);
#33632=ADVANCED_FACE('',(#4884),#319,.F.);
#33633=ADVANCED_FACE('',(#4885),#810,.F.);
#33634=ADVANCED_FACE('',(#4886),#2410,.T.);
#33635=ADVANCED_FACE('',(#4887),#811,.F.);
#33636=ADVANCED_FACE('',(#4888),#3075,.T.);
#33637=ADVANCED_FACE('',(#4889),#812,.F.);
#33638=ADVANCED_FACE('',(#4890),#2411,.F.);
#33639=ADVANCED_FACE('',(#4891),#813,.F.);
#33640=ADVANCED_FACE('',(#4892),#3076,.F.);
#33641=ADVANCED_FACE('',(#4893),#3077,.F.);
#33642=ADVANCED_FACE('',(#4894),#3078,.T.);
#33643=ADVANCED_FACE('',(#4895),#3079,.F.);
#33644=ADVANCED_FACE('',(#4896),#320,.T.);
#33645=ADVANCED_FACE('',(#4897),#3080,.F.);
#33646=ADVANCED_FACE('',(#4898),#3081,.T.);
#33647=ADVANCED_FACE('',(#4899),#3082,.F.);
#33648=ADVANCED_FACE('',(#4900),#321,.T.);
#33649=ADVANCED_FACE('',(#4901),#322,.T.);
#33650=ADVANCED_FACE('',(#4902),#814,.F.);
#33651=ADVANCED_FACE('',(#4903),#323,.T.);
#33652=ADVANCED_FACE('',(#4904),#324,.T.);
#33653=ADVANCED_FACE('',(#4905),#325,.T.);
#33654=ADVANCED_FACE('',(#4906),#1216,.F.);
#33655=ADVANCED_FACE('',(#4907),#326,.T.);
#33656=ADVANCED_FACE('',(#4908),#2412,.F.);
#33657=ADVANCED_FACE('',(#4909),#1217,.F.);
#33658=ADVANCED_FACE('',(#4910),#327,.T.);
#33659=ADVANCED_FACE('',(#4911),#3083,.F.);
#33660=ADVANCED_FACE('',(#4912),#2413,.T.);
#33661=ADVANCED_FACE('',(#4913),#3084,.T.);
#33662=ADVANCED_FACE('',(#4914),#3085,.T.);
#33663=ADVANCED_FACE('',(#4915),#3086,.F.);
#33664=ADVANCED_FACE('',(#4916),#2414,.T.);
#33665=ADVANCED_FACE('',(#4917),#3087,.F.);
#33666=ADVANCED_FACE('',(#4918),#2415,.T.);
#33667=ADVANCED_FACE('',(#4919),#3088,.F.);
#33668=ADVANCED_FACE('',(#4920),#2416,.T.);
#33669=ADVANCED_FACE('',(#4921),#3089,.F.);
#33670=ADVANCED_FACE('',(#4922),#815,.T.);
#33671=ADVANCED_FACE('',(#4923),#328,.T.);
#33672=ADVANCED_FACE('',(#4924),#3090,.T.);
#33673=ADVANCED_FACE('',(#4925),#3091,.T.);
#33674=ADVANCED_FACE('',(#4926),#2417,.T.);
#33675=ADVANCED_FACE('',(#4927),#3092,.F.);
#33676=ADVANCED_FACE('',(#4928),#3093,.T.);
#33677=ADVANCED_FACE('',(#4929),#3094,.F.);
#33678=ADVANCED_FACE('',(#4930),#2418,.T.);
#33679=ADVANCED_FACE('',(#4931),#3095,.F.);
#33680=ADVANCED_FACE('',(#4932),#3096,.F.);
#33681=ADVANCED_FACE('',(#4933),#3097,.F.);
#33682=ADVANCED_FACE('',(#4934),#3098,.T.);
#33683=ADVANCED_FACE('',(#4935),#329,.T.);
#33684=ADVANCED_FACE('',(#4936),#330,.T.);
#33685=ADVANCED_FACE('',(#4937),#3099,.T.);
#33686=ADVANCED_FACE('',(#4938),#331,.T.);
#33687=ADVANCED_FACE('',(#4939),#332,.T.);
#33688=ADVANCED_FACE('',(#4940),#333,.T.);
#33689=ADVANCED_FACE('',(#4941),#334,.T.);
#33690=ADVANCED_FACE('',(#4942),#3100,.T.);
#33691=ADVANCED_FACE('',(#4943),#335,.T.);
#33692=ADVANCED_FACE('',(#4944),#1218,.F.);
#33693=ADVANCED_FACE('',(#4945),#336,.T.);
#33694=ADVANCED_FACE('',(#4946),#1219,.F.);
#33695=ADVANCED_FACE('',(#4947),#1220,.T.);
#33696=ADVANCED_FACE('',(#4948),#1221,.F.);
#33697=ADVANCED_FACE('',(#4949),#337,.T.);
#33698=ADVANCED_FACE('',(#4950),#338,.T.);
#33699=ADVANCED_FACE('',(#4951),#339,.T.);
#33700=ADVANCED_FACE('',(#4952),#3101,.T.);
#33701=ADVANCED_FACE('',(#4953),#1222,.F.);
#33702=ADVANCED_FACE('',(#4954),#1223,.T.);
#33703=ADVANCED_FACE('',(#4955),#1224,.F.);
#33704=ADVANCED_FACE('',(#4956),#340,.T.);
#33705=ADVANCED_FACE('',(#4957),#341,.T.);
#33706=ADVANCED_FACE('',(#4958),#3102,.T.);
#33707=ADVANCED_FACE('',(#4959),#342,.T.);
#33708=ADVANCED_FACE('',(#4960),#343,.T.);
#33709=ADVANCED_FACE('',(#4961),#344,.T.);
#33710=ADVANCED_FACE('',(#4962),#345,.T.);
#33711=ADVANCED_FACE('',(#4963),#3103,.T.);
#33712=ADVANCED_FACE('',(#4964),#3104,.F.);
#33713=ADVANCED_FACE('',(#4965),#3105,.F.);
#33714=ADVANCED_FACE('',(#4966),#346,.F.);
#33715=ADVANCED_FACE('',(#4967),#816,.F.);
#33716=ADVANCED_FACE('',(#4968),#347,.F.);
#33717=ADVANCED_FACE('',(#4969),#817,.F.);
#33718=ADVANCED_FACE('',(#4970),#818,.F.);
#33719=ADVANCED_FACE('',(#4971),#819,.F.);
#33720=ADVANCED_FACE('',(#4972),#3106,.F.);
#33721=ADVANCED_FACE('',(#4973),#348,.F.);
#33722=ADVANCED_FACE('',(#4974),#349,.T.);
#33723=ADVANCED_FACE('',(#4975),#350,.T.);
#33724=ADVANCED_FACE('',(#4976),#351,.T.);
#33725=ADVANCED_FACE('',(#4977),#352,.T.);
#33726=ADVANCED_FACE('',(#4978),#820,.F.);
#33727=ADVANCED_FACE('',(#4979),#3107,.T.);
#33728=ADVANCED_FACE('',(#4980),#3108,.T.);
#33729=ADVANCED_FACE('',(#4981),#821,.T.);
#33730=ADVANCED_FACE('',(#4982),#1225,.T.);
#33731=ADVANCED_FACE('',(#4983),#353,.F.);
#33732=ADVANCED_FACE('',(#4984),#3109,.F.);
#33733=ADVANCED_FACE('',(#4985),#354,.F.);
#33734=ADVANCED_FACE('',(#4986),#2419,.T.);
#33735=ADVANCED_FACE('',(#4987),#355,.T.);
#33736=ADVANCED_FACE('',(#4988),#356,.T.);
#33737=ADVANCED_FACE('',(#4989),#3110,.T.);
#33738=ADVANCED_FACE('',(#4990),#3111,.T.);
#33739=ADVANCED_FACE('',(#4991),#357,.T.);
#33740=ADVANCED_FACE('',(#4992),#3112,.T.);
#33741=ADVANCED_FACE('',(#4993),#358,.T.);
#33742=ADVANCED_FACE('',(#4994),#3113,.T.);
#33743=ADVANCED_FACE('',(#4995),#359,.T.);
#33744=ADVANCED_FACE('',(#4996),#360,.T.);
#33745=ADVANCED_FACE('',(#4997),#3114,.T.);
#33746=ADVANCED_FACE('',(#4998),#361,.T.);
#33747=ADVANCED_FACE('',(#4999),#3115,.T.);
#33748=ADVANCED_FACE('',(#5000),#362,.T.);
#33749=ADVANCED_FACE('',(#5001),#3116,.T.);
#33750=ADVANCED_FACE('',(#5002),#363,.T.);
#33751=ADVANCED_FACE('',(#5003),#3117,.T.);
#33752=ADVANCED_FACE('',(#5004),#364,.T.);
#33753=ADVANCED_FACE('',(#5005,#1309),#2420,.F.);
#33754=ADVANCED_FACE('',(#5006),#1226,.F.);
#33755=ADVANCED_FACE('',(#5007),#365,.T.);
#33756=ADVANCED_FACE('',(#5008),#366,.T.);
#33757=ADVANCED_FACE('',(#5009),#3118,.T.);
#33758=ADVANCED_FACE('',(#5010),#822,.T.);
#33759=ADVANCED_FACE('',(#5011),#367,.T.);
#33760=ADVANCED_FACE('',(#5012),#368,.T.);
#33761=ADVANCED_FACE('',(#5013),#3119,.T.);
#33762=ADVANCED_FACE('',(#5014),#1227,.T.);
#33763=ADVANCED_FACE('',(#5015),#369,.T.);
#33764=ADVANCED_FACE('',(#5016),#1228,.T.);
#33765=ADVANCED_FACE('',(#5017),#823,.T.);
#33766=ADVANCED_FACE('',(#5018),#3120,.T.);
#33767=ADVANCED_FACE('',(#5019),#3121,.T.);
#33768=ADVANCED_FACE('',(#5020),#3122,.T.);
#33769=ADVANCED_FACE('',(#5021),#2421,.F.);
#33770=ADVANCED_FACE('',(#5022),#3123,.F.);
#33771=ADVANCED_FACE('',(#5023),#370,.T.);
#33772=ADVANCED_FACE('',(#5024),#2422,.T.);
#33773=ADVANCED_FACE('',(#5025),#824,.T.);
#33774=ADVANCED_FACE('',(#5026),#3124,.T.);
#33775=ADVANCED_FACE('',(#5027),#3125,.T.);
#33776=ADVANCED_FACE('',(#5028),#2423,.T.);
#33777=ADVANCED_FACE('',(#5029),#1229,.T.);
#33778=ADVANCED_FACE('',(#5030),#3126,.F.);
#33779=ADVANCED_FACE('',(#5031),#3127,.F.);
#33780=ADVANCED_FACE('',(#5032),#825,.F.);
#33781=ADVANCED_FACE('',(#5033),#371,.F.);
#33782=ADVANCED_FACE('',(#5034),#826,.F.);
#33783=ADVANCED_FACE('',(#5035),#3128,.F.);
#33784=ADVANCED_FACE('',(#5036),#827,.F.);
#33785=ADVANCED_FACE('',(#5037),#828,.F.);
#33786=ADVANCED_FACE('',(#5038),#372,.F.);
#33787=ADVANCED_FACE('',(#5039),#2424,.F.);
#33788=ADVANCED_FACE('',(#5040),#829,.F.);
#33789=ADVANCED_FACE('',(#5041),#2425,.T.);
#33790=ADVANCED_FACE('',(#5042),#3129,.T.);
#33791=ADVANCED_FACE('',(#5043),#3130,.F.);
#33792=ADVANCED_FACE('',(#5044),#2426,.T.);
#33793=ADVANCED_FACE('',(#5045),#3131,.F.);
#33794=ADVANCED_FACE('',(#5046),#3132,.F.);
#33795=ADVANCED_FACE('',(#5047),#3133,.F.);
#33796=ADVANCED_FACE('',(#5048),#3134,.F.);
#33797=ADVANCED_FACE('',(#5049),#2427,.T.);
#33798=ADVANCED_FACE('',(#5050),#3135,.F.);
#33799=ADVANCED_FACE('',(#5051),#3136,.F.);
#33800=ADVANCED_FACE('',(#5052),#3137,.T.);
#33801=ADVANCED_FACE('',(#5053),#3138,.F.);
#33802=ADVANCED_FACE('',(#5054),#3139,.F.);
#33803=ADVANCED_FACE('',(#5055),#2428,.F.);
#33804=ADVANCED_FACE('',(#5056),#3140,.T.);
#33805=ADVANCED_FACE('',(#5057),#3141,.F.);
#33806=ADVANCED_FACE('',(#5058),#2429,.F.);
#33807=ADVANCED_FACE('',(#5059),#3142,.F.);
#33808=ADVANCED_FACE('',(#5060),#3143,.F.);
#33809=ADVANCED_FACE('',(#5061),#3144,.F.);
#33810=ADVANCED_FACE('',(#5062),#3145,.F.);
#33811=ADVANCED_FACE('',(#5063),#2430,.T.);
#33812=ADVANCED_FACE('',(#5064),#830,.F.);
#33813=ADVANCED_FACE('',(#5065),#373,.F.);
#33814=ADVANCED_FACE('',(#5066),#831,.F.);
#33815=ADVANCED_FACE('',(#5067),#832,.F.);
#33816=ADVANCED_FACE('',(#5068),#3146,.F.);
#33817=ADVANCED_FACE('',(#5069),#2431,.F.);
#33818=ADVANCED_FACE('',(#5070),#833,.T.);
#33819=ADVANCED_FACE('',(#5071),#834,.F.);
#33820=ADVANCED_FACE('',(#5072),#2432,.F.);
#33821=ADVANCED_FACE('',(#5073),#2433,.F.);
#33822=ADVANCED_FACE('',(#5074),#3147,.F.);
#33823=ADVANCED_FACE('',(#5075),#3148,.F.);
#33824=ADVANCED_FACE('',(#5076),#835,.F.);
#33825=ADVANCED_FACE('',(#5077),#374,.F.);
#33826=ADVANCED_FACE('',(#5078),#3149,.T.);
#33827=ADVANCED_FACE('',(#5079),#1230,.F.);
#33828=ADVANCED_FACE('',(#5080),#3150,.F.);
#33829=ADVANCED_FACE('',(#5081),#3151,.F.);
#33830=ADVANCED_FACE('',(#5082),#836,.F.);
#33831=ADVANCED_FACE('',(#5083),#375,.F.);
#33832=ADVANCED_FACE('',(#5084),#376,.T.);
#33833=ADVANCED_FACE('',(#5085),#837,.F.);
#33834=ADVANCED_FACE('',(#5086),#3152,.F.);
#33835=ADVANCED_FACE('',(#5087),#3153,.T.);
#33836=ADVANCED_FACE('',(#5088),#377,.F.);
#33837=ADVANCED_FACE('',(#5089),#3154,.F.);
#33838=ADVANCED_FACE('',(#5090),#378,.F.);
#33839=ADVANCED_FACE('',(#5091),#379,.F.);
#33840=ADVANCED_FACE('',(#5092),#380,.F.);
#33841=ADVANCED_FACE('',(#5093),#3155,.F.);
#33842=ADVANCED_FACE('',(#5094),#2434,.F.);
#33843=ADVANCED_FACE('',(#5095),#838,.F.);
#33844=ADVANCED_FACE('',(#5096),#381,.F.);
#33845=ADVANCED_FACE('',(#5097),#839,.F.);
#33846=ADVANCED_FACE('',(#5098),#1231,.T.);
#33847=ADVANCED_FACE('',(#5099),#382,.F.);
#33848=ADVANCED_FACE('',(#5100),#3156,.F.);
#33849=ADVANCED_FACE('',(#5101),#3157,.F.);
#33850=ADVANCED_FACE('',(#5102),#3158,.F.);
#33851=ADVANCED_FACE('',(#5103),#3159,.F.);
#33852=ADVANCED_FACE('',(#5104),#3160,.F.);
#33853=ADVANCED_FACE('',(#5105),#840,.F.);
#33854=ADVANCED_FACE('',(#5106),#3161,.F.);
#33855=ADVANCED_FACE('',(#5107),#2435,.F.);
#33856=ADVANCED_FACE('',(#5108),#3162,.T.);
#33857=ADVANCED_FACE('',(#5109),#1232,.T.);
#33858=ADVANCED_FACE('',(#5110),#3163,.T.);
#33859=ADVANCED_FACE('',(#5111),#383,.T.);
#33860=ADVANCED_FACE('',(#5112),#384,.T.);
#33861=ADVANCED_FACE('',(#5113),#385,.T.);
#33862=ADVANCED_FACE('',(#5114),#3164,.T.);
#33863=ADVANCED_FACE('',(#5115),#1233,.T.);
#33864=ADVANCED_FACE('',(#5116),#386,.T.);
#33865=ADVANCED_FACE('',(#5117),#387,.T.);
#33866=ADVANCED_FACE('',(#5118),#388,.T.);
#33867=ADVANCED_FACE('',(#5119),#389,.F.);
#33868=ADVANCED_FACE('',(#5120),#390,.F.);
#33869=ADVANCED_FACE('',(#5121),#1234,.T.);
#33870=ADVANCED_FACE('',(#5122),#1235,.T.);
#33871=ADVANCED_FACE('',(#5123),#3165,.F.);
#33872=ADVANCED_FACE('',(#5124),#1236,.T.);
#33873=ADVANCED_FACE('',(#5125),#3166,.F.);
#33874=ADVANCED_FACE('',(#5126),#1237,.T.);
#33875=ADVANCED_FACE('',(#5127),#3167,.F.);
#33876=ADVANCED_FACE('',(#5128),#391,.T.);
#33877=ADVANCED_FACE('',(#5129),#392,.T.);
#33878=ADVANCED_FACE('',(#5130),#3168,.T.);
#33879=ADVANCED_FACE('',(#5131),#3169,.T.);
#33880=ADVANCED_FACE('',(#5132),#3170,.T.);
#33881=ADVANCED_FACE('',(#5133),#3171,.T.);
#33882=ADVANCED_FACE('',(#5134),#393,.T.);
#33883=ADVANCED_FACE('',(#5135),#394,.T.);
#33884=ADVANCED_FACE('',(#5136),#3172,.T.);
#33885=ADVANCED_FACE('',(#5137),#395,.T.);
#33886=ADVANCED_FACE('',(#5138),#3173,.T.);
#33887=ADVANCED_FACE('',(#5139),#3174,.T.);
#33888=ADVANCED_FACE('',(#5140),#3175,.T.);
#33889=ADVANCED_FACE('',(#5141),#396,.T.);
#33890=ADVANCED_FACE('',(#5142,#1310,#1311,#1312,#1313,#1314),#2436,.T.);
#33891=ADVANCED_FACE('',(#5143),#397,.T.);
#33892=ADVANCED_FACE('',(#5144),#1238,.T.);
#33893=ADVANCED_FACE('',(#5145),#1239,.T.);
#33894=ADVANCED_FACE('',(#5146),#398,.T.);
#33895=ADVANCED_FACE('',(#5147),#399,.T.);
#33896=ADVANCED_FACE('',(#5148),#3176,.T.);
#33897=ADVANCED_FACE('',(#5149),#400,.T.);
#33898=ADVANCED_FACE('',(#5150),#401,.T.);
#33899=ADVANCED_FACE('',(#5151),#402,.T.);
#33900=ADVANCED_FACE('',(#5152),#1240,.F.);
#33901=ADVANCED_FACE('',(#5153),#1241,.T.);
#33902=ADVANCED_FACE('',(#5154),#3177,.T.);
#33903=ADVANCED_FACE('',(#5155),#3178,.F.);
#33904=ADVANCED_FACE('',(#5156),#3179,.F.);
#33905=ADVANCED_FACE('',(#5157),#3180,.F.);
#33906=ADVANCED_FACE('',(#5158),#3181,.F.);
#33907=ADVANCED_FACE('',(#5159),#3182,.F.);
#33908=ADVANCED_FACE('',(#5160),#3183,.F.);
#33909=ADVANCED_FACE('',(#5161),#2437,.T.);
#33910=ADVANCED_FACE('',(#5162),#3184,.F.);
#33911=ADVANCED_FACE('',(#5163),#3185,.T.);
#33912=ADVANCED_FACE('',(#5164),#3186,.F.);
#33913=ADVANCED_FACE('',(#5165),#2438,.F.);
#33914=ADVANCED_FACE('',(#5166),#3187,.F.);
#33915=ADVANCED_FACE('',(#5167),#841,.F.);
#33916=ADVANCED_FACE('',(#5168),#403,.F.);
#33917=ADVANCED_FACE('',(#5169),#404,.F.);
#33918=ADVANCED_FACE('',(#5170),#842,.F.);
#33919=ADVANCED_FACE('',(#5171),#405,.F.);
#33920=ADVANCED_FACE('',(#5172),#843,.F.);
#33921=ADVANCED_FACE('',(#5173),#406,.F.);
#33922=ADVANCED_FACE('',(#5174),#844,.F.);
#33923=ADVANCED_FACE('',(#5175),#3188,.F.);
#33924=ADVANCED_FACE('',(#5176),#845,.F.);
#33925=ADVANCED_FACE('',(#5177),#407,.F.);
#33926=ADVANCED_FACE('',(#5178),#846,.F.);
#33927=ADVANCED_FACE('',(#5179),#3189,.F.);
#33928=ADVANCED_FACE('',(#5180),#3190,.F.);
#33929=ADVANCED_FACE('',(#5181),#408,.F.);
#33930=ADVANCED_FACE('',(#5182),#409,.F.);
#33931=ADVANCED_FACE('',(#5183),#410,.F.);
#33932=ADVANCED_FACE('',(#5184),#2439,.F.);
#33933=ADVANCED_FACE('',(#5185),#411,.T.);
#33934=ADVANCED_FACE('',(#5186),#3191,.F.);
#33935=ADVANCED_FACE('',(#5187),#3192,.F.);
#33936=ADVANCED_FACE('',(#5188),#3193,.F.);
#33937=ADVANCED_FACE('',(#5189),#412,.F.);
#33938=ADVANCED_FACE('',(#5190),#1242,.T.);
#33939=ADVANCED_FACE('',(#5191),#413,.F.);
#33940=ADVANCED_FACE('',(#5192),#2440,.T.);
#33941=ADVANCED_FACE('',(#5193),#414,.F.);
#33942=ADVANCED_FACE('',(#5194),#3194,.F.);
#33943=ADVANCED_FACE('',(#5195),#415,.F.);
#33944=ADVANCED_FACE('',(#5196),#3195,.F.);
#33945=ADVANCED_FACE('',(#5197),#416,.F.);
#33946=ADVANCED_FACE('',(#5198),#3196,.F.);
#33947=ADVANCED_FACE('',(#5199),#3197,.F.);
#33948=ADVANCED_FACE('',(#5200),#417,.F.);
#33949=ADVANCED_FACE('',(#5201),#1243,.T.);
#33950=ADVANCED_FACE('',(#5202),#3198,.F.);
#33951=ADVANCED_FACE('',(#5203),#2441,.T.);
#33952=ADVANCED_FACE('',(#5204),#3199,.F.);
#33953=ADVANCED_FACE('',(#5205),#2442,.F.);
#33954=ADVANCED_FACE('',(#5206),#418,.F.);
#33955=ADVANCED_FACE('',(#5207),#847,.F.);
#33956=ADVANCED_FACE('',(#5208),#3200,.F.);
#33957=ADVANCED_FACE('',(#5209),#3201,.T.);
#33958=ADVANCED_FACE('',(#5210),#3202,.F.);
#33959=ADVANCED_FACE('',(#5211),#848,.F.);
#33960=ADVANCED_FACE('',(#5212),#3203,.F.);
#33961=ADVANCED_FACE('',(#5213),#2443,.T.);
#33962=ADVANCED_FACE('',(#5214),#2444,.T.);
#33963=ADVANCED_FACE('',(#5215),#3204,.F.);
#33964=ADVANCED_FACE('',(#5216),#2445,.F.);
#33965=ADVANCED_FACE('',(#5217),#849,.F.);
#33966=ADVANCED_FACE('',(#5218),#3205,.F.);
#33967=ADVANCED_FACE('',(#5219),#3206,.T.);
#33968=ADVANCED_FACE('',(#5220),#419,.F.);
#33969=ADVANCED_FACE('',(#5221),#3207,.F.);
#33970=ADVANCED_FACE('',(#5222),#850,.F.);
#33971=ADVANCED_FACE('',(#5223),#3208,.F.);
#33972=ADVANCED_FACE('',(#5224),#2446,.T.);
#33973=ADVANCED_FACE('',(#5225),#2447,.F.);
#33974=ADVANCED_FACE('',(#5226),#3209,.F.);
#33975=ADVANCED_FACE('',(#5227),#2448,.T.);
#33976=ADVANCED_FACE('',(#5228),#3210,.F.);
#33977=ADVANCED_FACE('',(#5229),#851,.F.);
#33978=ADVANCED_FACE('',(#5230),#420,.F.);
#33979=ADVANCED_FACE('',(#5231),#3211,.T.);
#33980=ADVANCED_FACE('',(#5232),#421,.F.);
#33981=ADVANCED_FACE('',(#5233),#3212,.T.);
#33982=ADVANCED_FACE('',(#5234),#422,.F.);
#33983=ADVANCED_FACE('',(#5235),#3213,.T.);
#33984=ADVANCED_FACE('',(#5236),#3214,.F.);
#33985=ADVANCED_FACE('',(#5237),#852,.F.);
#33986=ADVANCED_FACE('',(#5238),#3215,.F.);
#33987=ADVANCED_FACE('',(#5239),#2449,.T.);
#33988=ADVANCED_FACE('',(#5240,#1315),#2450,.T.);
#33989=ADVANCED_FACE('',(#5241),#3216,.T.);
#33990=ADVANCED_FACE('',(#5242),#423,.T.);
#33991=ADVANCED_FACE('',(#5243),#424,.T.);
#33992=ADVANCED_FACE('',(#5244),#425,.T.);
#33993=ADVANCED_FACE('',(#5245),#3217,.T.);
#33994=ADVANCED_FACE('',(#5246),#3218,.T.);
#33995=ADVANCED_FACE('',(#5247),#426,.T.);
#33996=ADVANCED_FACE('',(#5248),#427,.T.);
#33997=ADVANCED_FACE('',(#5249),#3219,.T.);
#33998=ADVANCED_FACE('',(#5250),#3220,.T.);
#33999=ADVANCED_FACE('',(#5251),#428,.T.);
#34000=ADVANCED_FACE('',(#5252),#429,.T.);
#34001=ADVANCED_FACE('',(#5253),#430,.T.);
#34002=ADVANCED_FACE('',(#5254),#431,.T.);
#34003=ADVANCED_FACE('',(#5255),#432,.T.);
#34004=ADVANCED_FACE('',(#5256),#3221,.T.);
#34005=ADVANCED_FACE('',(#5257),#2451,.F.);
#34006=ADVANCED_FACE('',(#5258),#853,.T.);
#34007=ADVANCED_FACE('',(#5259),#854,.T.);
#34008=ADVANCED_FACE('',(#5260),#433,.T.);
#34009=ADVANCED_FACE('',(#5261),#1244,.T.);
#34010=ADVANCED_FACE('',(#5262),#3222,.T.);
#34011=ADVANCED_FACE('',(#5263),#3223,.T.);
#34012=ADVANCED_FACE('',(#5264),#1245,.T.);
#34013=ADVANCED_FACE('',(#5265),#434,.T.);
#34014=ADVANCED_FACE('',(#5266),#3224,.T.);
#34015=ADVANCED_FACE('',(#5267),#435,.T.);
#34016=ADVANCED_FACE('',(#5268),#3225,.T.);
#34017=ADVANCED_FACE('',(#5269),#855,.T.);
#34018=ADVANCED_FACE('',(#5270),#856,.T.);
#34019=ADVANCED_FACE('',(#5271),#436,.T.);
#34020=ADVANCED_FACE('',(#5272),#1246,.T.);
#34021=ADVANCED_FACE('',(#5273),#3226,.T.);
#34022=ADVANCED_FACE('',(#5274),#437,.T.);
#34023=ADVANCED_FACE('',(#5275),#1247,.T.);
#34024=ADVANCED_FACE('',(#5276),#3227,.T.);
#34025=ADVANCED_FACE('',(#5277),#3228,.T.);
#34026=ADVANCED_FACE('',(#5278),#438,.T.);
#34027=ADVANCED_FACE('',(#5279),#1248,.T.);
#34028=ADVANCED_FACE('',(#5280),#3229,.T.);
#34029=ADVANCED_FACE('',(#5281),#439,.T.);
#34030=ADVANCED_FACE('',(#5282),#1249,.T.);
#34031=ADVANCED_FACE('',(#5283),#3230,.T.);
#34032=ADVANCED_FACE('',(#5284),#857,.T.);
#34033=ADVANCED_FACE('',(#5285),#858,.T.);
#34034=ADVANCED_FACE('',(#5286),#440,.T.);
#34035=ADVANCED_FACE('',(#5287),#441,.T.);
#34036=ADVANCED_FACE('',(#5288),#1250,.T.);
#34037=ADVANCED_FACE('',(#5289),#3231,.T.);
#34038=ADVANCED_FACE('',(#5290),#442,.T.);
#34039=ADVANCED_FACE('',(#5291),#1251,.T.);
#34040=ADVANCED_FACE('',(#5292),#3232,.T.);
#34041=ADVANCED_FACE('',(#5293),#3233,.T.);
#34042=ADVANCED_FACE('',(#5294),#443,.T.);
#34043=ADVANCED_FACE('',(#5295),#2452,.T.);
#34044=ADVANCED_FACE('',(#5296),#2453,.F.);
#34045=ADVANCED_FACE('',(#5297),#2454,.F.);
#34046=ADVANCED_FACE('',(#5298),#3234,.F.);
#34047=ADVANCED_FACE('',(#5299),#2455,.F.);
#34048=ADVANCED_FACE('',(#5300),#2456,.T.);
#34049=ADVANCED_FACE('',(#5301),#2457,.F.);
#34050=ADVANCED_FACE('',(#5302),#2458,.F.);
#34051=ADVANCED_FACE('',(#5303),#2459,.F.);
#34052=ADVANCED_FACE('',(#5304),#2460,.T.);
#34053=ADVANCED_FACE('',(#5305),#3235,.F.);
#34054=ADVANCED_FACE('',(#5306,#1316),#2461,.T.);
#34055=ADVANCED_FACE('',(#5307),#859,.F.);
#34056=ADVANCED_FACE('',(#5308),#2462,.T.);
#34057=ADVANCED_FACE('',(#5309),#2463,.F.);
#34058=ADVANCED_FACE('',(#5310),#3236,.F.);
#34059=ADVANCED_FACE('',(#5311),#2464,.F.);
#34060=ADVANCED_FACE('',(#5312),#2465,.T.);
#34061=ADVANCED_FACE('',(#5313),#2466,.T.);
#34062=ADVANCED_FACE('',(#5314),#3237,.T.);
#34063=ADVANCED_FACE('',(#5315),#2467,.F.);
#34064=ADVANCED_FACE('',(#5316),#2468,.T.);
#34065=ADVANCED_FACE('',(#5317),#2469,.T.);
#34066=ADVANCED_FACE('',(#5318),#2470,.F.);
#34067=ADVANCED_FACE('',(#5319),#2471,.F.);
#34068=ADVANCED_FACE('',(#5320),#3238,.T.);
#34069=ADVANCED_FACE('',(#5321),#2472,.F.);
#34070=ADVANCED_FACE('',(#5322),#2473,.F.);
#34071=ADVANCED_FACE('',(#5323),#2474,.F.);
#34072=ADVANCED_FACE('',(#5324),#3239,.T.);
#34073=ADVANCED_FACE('',(#5325),#2475,.T.);
#34074=ADVANCED_FACE('',(#5326),#2476,.T.);
#34075=ADVANCED_FACE('',(#5327),#2477,.T.);
#34076=ADVANCED_FACE('',(#5328),#2478,.F.);
#34077=ADVANCED_FACE('',(#5329),#2479,.T.);
#34078=ADVANCED_FACE('',(#5330),#3240,.T.);
#34079=ADVANCED_FACE('',(#5331),#2480,.F.);
#34080=ADVANCED_FACE('',(#5332),#2481,.T.);
#34081=ADVANCED_FACE('',(#5333),#2482,.F.);
#34082=ADVANCED_FACE('',(#5334),#2483,.F.);
#34083=ADVANCED_FACE('',(#5335),#3241,.F.);
#34084=ADVANCED_FACE('',(#5336),#3242,.F.);
#34085=ADVANCED_FACE('',(#5337),#2484,.T.);
#34086=ADVANCED_FACE('',(#5338),#2485,.T.);
#34087=ADVANCED_FACE('',(#5339),#2486,.F.);
#34088=ADVANCED_FACE('',(#5340),#3243,.F.);
#34089=ADVANCED_FACE('',(#5341),#3244,.T.);
#34090=ADVANCED_FACE('',(#5342),#2487,.T.);
#34091=ADVANCED_FACE('',(#5343),#3245,.T.);
#34092=ADVANCED_FACE('',(#5344),#3246,.F.);
#34093=ADVANCED_FACE('',(#5345),#2488,.T.);
#34094=ADVANCED_FACE('',(#5346),#2489,.T.);
#34095=ADVANCED_FACE('',(#5347),#3247,.T.);
#34096=ADVANCED_FACE('',(#5348),#2490,.F.);
#34097=ADVANCED_FACE('',(#5349),#2491,.T.);
#34098=ADVANCED_FACE('',(#5350),#3248,.T.);
#34099=ADVANCED_FACE('',(#5351),#2492,.F.);
#34100=ADVANCED_FACE('',(#5352),#2493,.T.);
#34101=ADVANCED_FACE('',(#5353),#2494,.F.);
#34102=ADVANCED_FACE('',(#5354),#3249,.T.);
#34103=ADVANCED_FACE('',(#5355),#2495,.T.);
#34104=ADVANCED_FACE('',(#5356),#2496,.F.);
#34105=ADVANCED_FACE('',(#5357),#3250,.T.);
#34106=ADVANCED_FACE('',(#5358),#2497,.F.);
#34107=ADVANCED_FACE('',(#5359),#3251,.T.);
#34108=ADVANCED_FACE('',(#5360,#1317,#1318),#2498,.F.);
#34109=ADVANCED_FACE('',(#5361),#3252,.T.);
#34110=ADVANCED_FACE('',(#5362),#2499,.F.);
#34111=ADVANCED_FACE('',(#5363),#3253,.T.);
#34112=ADVANCED_FACE('',(#5364),#2500,.F.);
#34113=ADVANCED_FACE('',(#5365),#3254,.T.);
#34114=ADVANCED_FACE('',(#5366),#3255,.F.);
#34115=ADVANCED_FACE('',(#5367),#2501,.T.);
#34116=ADVANCED_FACE('',(#5368),#3256,.T.);
#34117=ADVANCED_FACE('',(#5369),#3257,.T.);
#34118=ADVANCED_FACE('',(#5370),#3258,.T.);
#34119=ADVANCED_FACE('',(#5371),#3259,.F.);
#34120=ADVANCED_FACE('',(#5372),#3260,.T.);
#34121=ADVANCED_FACE('',(#5373),#3261,.F.);
#34122=ADVANCED_FACE('',(#5374),#2502,.T.);
#34123=ADVANCED_FACE('',(#5375),#3262,.T.);
#34124=ADVANCED_FACE('',(#5376),#3263,.T.);
#34125=ADVANCED_FACE('',(#5377),#3264,.T.);
#34126=ADVANCED_FACE('',(#5378),#2503,.F.);
#34127=ADVANCED_FACE('',(#5379),#3265,.F.);
#34128=ADVANCED_FACE('',(#5380),#3266,.T.);
#34129=ADVANCED_FACE('',(#5381),#3267,.F.);
#34130=ADVANCED_FACE('',(#5382),#3268,.T.);
#34131=ADVANCED_FACE('',(#5383),#3269,.T.);
#34132=ADVANCED_FACE('',(#5384),#3270,.T.);
#34133=ADVANCED_FACE('',(#5385),#2504,.F.);
#34134=ADVANCED_FACE('',(#5386),#3271,.F.);
#34135=ADVANCED_FACE('',(#5387),#2505,.T.);
#34136=ADVANCED_FACE('',(#5388),#2506,.T.);
#34137=ADVANCED_FACE('',(#5389),#2507,.T.);
#34138=ADVANCED_FACE('',(#5390),#2508,.T.);
#34139=ADVANCED_FACE('',(#5391),#2509,.T.);
#34140=ADVANCED_FACE('',(#5392),#2510,.T.);
#34141=ADVANCED_FACE('',(#5393,#1319,#1320,#1321,#1322,#1323,#1324,#1325,
#1326,#1327,#1328),#3272,.T.);
#34142=ADVANCED_FACE('',(#5394),#2511,.T.);
#34143=ADVANCED_FACE('',(#5395),#2512,.T.);
#34144=ADVANCED_FACE('',(#5396),#444,.T.);
#34145=ADVANCED_FACE('',(#5397),#3273,.F.);
#34146=ADVANCED_FACE('',(#5398),#3274,.T.);
#34147=ADVANCED_FACE('',(#5399),#2513,.F.);
#34148=ADVANCED_FACE('',(#5400),#445,.T.);
#34149=ADVANCED_FACE('',(#5401),#3275,.F.);
#34150=ADVANCED_FACE('',(#5402),#3276,.T.);
#34151=ADVANCED_FACE('',(#5403,#1329),#2514,.T.);
#34152=ADVANCED_FACE('',(#5404),#1252,.F.);
#34153=ADVANCED_FACE('',(#5405),#860,.T.);
#34154=ADVANCED_FACE('',(#5406),#446,.T.);
#34155=ADVANCED_FACE('',(#5407),#3277,.F.);
#34156=ADVANCED_FACE('',(#5408),#447,.T.);
#34157=ADVANCED_FACE('',(#5409),#2515,.T.);
#34158=ADVANCED_FACE('',(#5410),#1253,.F.);
#34159=ADVANCED_FACE('',(#5411),#861,.T.);
#34160=ADVANCED_FACE('',(#5412),#448,.T.);
#34161=ADVANCED_FACE('',(#5413),#3278,.F.);
#34162=ADVANCED_FACE('',(#5414,#1330),#2516,.F.);
#34163=ADVANCED_FACE('',(#5415),#2517,.T.);
#34164=ADVANCED_FACE('',(#5416,#1331),#2518,.T.);
#34165=ADVANCED_FACE('',(#5417),#2519,.T.);
#34166=ADVANCED_FACE('',(#5418),#2520,.F.);
#34167=CLOSED_SHELL('',(#32027,#32028,#32029,#32030,#32031));
#34168=CLOSED_SHELL('',(#32032,#32033,#32034,#32035,#32036,#32037,#32038,
#32039,#32040,#32041,#32042,#32043,#32044,#32045,#32046,#32047,#32048,#32049,
#32050,#32051,#32052,#32053,#32054,#32055,#32056,#32057,#32058,#32059,#32060,
#32061,#32062,#32063,#32064,#32065,#32066,#32067,#32068,#32069,#32070,#32071,
#32072,#32073,#32074,#32075,#32076,#32077,#32078,#32079,#32080,#32081,#32082,
#32083,#32084,#32085,#32086,#32087,#32088,#32089,#32090,#32091,#32092,#32093,
#32094,#32095,#32096,#32097,#32098,#32099,#32100,#32101,#32102,#32103,#32104,
#32105,#32106,#32107,#32108,#32109,#32110,#32111,#32112,#32113,#32114,#32115,
#32116,#32117,#32118,#32119,#32120,#32121,#32122,#32123,#32124,#32125,#32126,
#32127,#32128,#32129,#32130,#32131,#32132,#32133,#32134,#32135,#32136,#32137,
#32138,#32139,#32140,#32141,#32142,#32143,#32144,#32145,#32146,#32147,#32148,
#32149,#32150,#32151,#32152,#32153,#32154,#32155,#32156,#32157,#32158,#32159,
#32160,#32161,#32162,#32163,#32164,#32165,#32166,#32167,#32168,#32169,#32170,
#32171,#32172,#32173,#32174,#32175,#32176,#32177,#32178,#32179,#32180,#32181,
#32182,#32183,#32184,#32185,#32186,#32187,#32188,#32189,#32190,#32191,#32192,
#32193,#32194,#32195,#32196,#32197,#32198,#32199,#32200,#32201,#32202,#32203,
#32204,#32205,#32206,#32207,#32208,#32209,#32210,#32211,#32212,#32213,#32214,
#32215,#32216,#32217,#32218,#32219,#32220,#32221,#32222,#32223,#32224,#32225,
#32226,#32227,#32228,#32229,#32230,#32231,#32232,#32233,#32234,#32235,#32236,
#32237,#32238,#32239,#32240,#32241,#32242,#32243,#32244,#32245,#32246,#32247,
#32248,#32249,#32250,#32251,#32252,#32253,#32254,#32255,#32256,#32257,#32258,
#32259,#32260,#32261,#32262,#32263,#32264,#32265,#32266,#32267,#32268,#32269,
#32270,#32271,#32272,#32273,#32274,#32275,#32276,#32277,#32278,#32279,#32280,
#32281,#32282,#32283,#32284,#32285,#32286,#32287,#32288,#32289,#32290,#32291,
#32292,#32293,#32294,#32295,#32296,#32297,#32298,#32299,#32300,#32301,#32302,
#32303,#32304,#32305,#32306,#32307,#32308,#32309,#32310,#32311,#32312,#32313,
#32314,#32315,#32316,#32317,#32318,#32319,#32320,#32321,#32322));
#34169=CLOSED_SHELL('',(#32323,#32324,#32325,#32326,#32327,#32328,#32329,
#32330,#32331,#32332,#32333,#32334,#32335,#32336,#32337,#32338,#32339,#32340,
#32341,#32342,#32343,#32344,#32345,#32346,#32347,#32348,#32349,#32350,#32351,
#32352,#32353,#32354,#32355,#32356,#32357,#32358,#32359,#32360,#32361,#32362,
#32363,#32364,#32365,#32366,#32367,#32368,#32369,#32370,#32371,#32372,#32373,
#32374,#32375,#32376,#32377,#32378,#32379,#32380,#32381,#32382,#32383,#32384,
#32385,#32386,#32387,#32388,#32389,#32390,#32391,#32392,#32393,#32394,#32395,
#32396,#32397,#32398,#32399,#32400,#32401,#32402,#32403,#32404,#32405,#32406,
#32407,#32408,#32409,#32410,#32411,#32412,#32413,#32414,#32415,#32416,#32417,
#32418,#32419,#32420,#32421,#32422,#32423,#32424,#32425,#32426,#32427,#32428,
#32429,#32430,#32431,#32432));
#34170=CLOSED_SHELL('',(#32433,#32434,#32435,#32436,#32437,#32438,#32439,
#32440,#32441,#32442,#32443,#32444,#32445,#32446,#32447,#32448,#32449,#32450,
#32451,#32452,#32453,#32454,#32455,#32456,#32457,#32458,#32459,#32460,#32461,
#32462,#32463,#32464,#32465,#32466,#32467,#32468,#32469,#32470,#32471,#32472,
#32473,#32474,#32475,#32476));
#34171=CLOSED_SHELL('',(#32477,#32478,#32479,#32480,#32481));
#34172=CLOSED_SHELL('',(#32482,#32483,#32484,#32485,#32486));
#34173=CLOSED_SHELL('',(#32487,#32488,#32489,#32490,#32491,#32492,#32493,
#32494,#32495,#32496,#32497,#32498,#32499,#32500,#32501,#32502,#32503,#32504,
#32505,#32506,#32507,#32508,#32509,#32510,#32511,#32512,#32513,#32514,#32515,
#32516,#32517,#32518,#32519,#32520,#32521,#32522,#32523,#32524,#32525,#32526,
#32527,#32528,#32529,#32530,#32531,#32532,#32533,#32534,#32535,#32536,#32537,
#32538,#32539,#32540,#32541,#32542,#32543,#32544,#32545,#32546,#32547,#32548,
#32549,#32550,#32551,#32552,#32553,#32554,#32555,#32556,#32557,#32558,#32559,
#32560,#32561,#32562,#32563,#32564,#32565,#32566,#32567,#32568,#32569,#32570,
#32571,#32572,#32573,#32574,#32575,#32576,#32577,#32578,#32579,#32580,#32581,
#32582,#32583,#32584,#32585,#32586,#32587,#32588,#32589,#32590,#32591,#32592,
#32593,#32594,#32595,#32596,#32597,#32598,#32599,#32600,#32601,#32602,#32603,
#32604,#32605,#32606,#32607,#32608,#32609,#32610,#32611,#32612,#32613,#32614,
#32615,#32616,#32617,#32618,#32619,#32620,#32621,#32622,#32623,#32624,#32625,
#32626,#32627,#32628,#32629,#32630,#32631,#32632,#32633,#32634,#32635,#32636,
#32637,#32638,#32639,#32640,#32641,#32642,#32643,#32644,#32645,#32646,#32647,
#32648,#32649,#32650,#32651,#32652,#32653,#32654,#32655,#32656,#32657,#32658,
#32659,#32660,#32661,#32662,#32663,#32664,#32665,#32666,#32667,#32668,#32669,
#32670,#32671,#32672,#32673,#32674,#32675,#32676,#32677,#32678,#32679,#32680,
#32681,#32682,#32683,#32684,#32685,#32686,#32687,#32688,#32689,#32690,#32691,
#32692,#32693,#32694,#32695,#32696,#32697,#32698,#32699,#32700,#32701,#32702,
#32703,#32704,#32705,#32706,#32707,#32708,#32709,#32710,#32711,#32712,#32713,
#32714,#32715,#32716,#32717,#32718,#32719,#32720,#32721,#32722,#32723,#32724,
#32725,#32726,#32727,#32728,#32729,#32730,#32731,#32732,#32733,#32734,#32735,
#32736,#32737,#32738,#32739,#32740,#32741,#32742,#32743,#32744,#32745,#32746,
#32747,#32748,#32749,#32750,#32751,#32752,#32753,#32754,#32755,#32756,#32757,
#32758,#32759,#32760,#32761,#32762,#32763,#32764,#32765,#32766,#32767,#32768,
#32769,#32770,#32771,#32772,#32773,#32774,#32775,#32776,#32777,#32778,#32779,
#32780,#32781,#32782,#32783,#32784,#32785,#32786,#32787,#32788,#32789,#32790,
#32791,#32792,#32793,#32794,#32795,#32796,#32797,#32798,#32799,#32800,#32801,
#32802,#32803,#32804,#32805,#32806,#32807,#32808,#32809,#32810,#32811,#32812,
#32813,#32814,#32815,#32816,#32817,#32818,#32819,#32820,#32821,#32822,#32823,
#32824,#32825,#32826,#32827,#32828,#32829,#32830,#32831,#32832,#32833,#32834,
#32835,#32836,#32837,#32838,#32839,#32840,#32841,#32842,#32843,#32844,#32845,
#32846,#32847,#32848,#32849,#32850,#32851,#32852,#32853,#32854,#32855,#32856,
#32857,#32858,#32859,#32860,#32861,#32862,#32863,#32864,#32865,#32866,#32867,
#32868,#32869,#32870,#32871,#32872,#32873));
#34174=CLOSED_SHELL('',(#32874,#32875,#32876,#32877,#32878,#32879,#32880,
#32881,#32882,#32883,#32884,#32885,#32886,#32887,#32888,#32889,#32890,#32891,
#32892,#32893,#32894,#32895,#32896,#32897,#32898,#32899,#32900,#32901,#32902,
#32903,#32904,#32905,#32906,#32907,#32908,#32909,#32910,#32911,#32912,#32913,
#32914,#32915,#32916,#32917,#32918,#32919,#32920,#32921,#32922,#32923,#32924,
#32925,#32926,#32927,#32928,#32929,#32930,#32931,#32932,#32933,#32934,#32935,
#32936,#32937,#32938,#32939,#32940,#32941,#32942,#32943,#32944,#32945,#32946,
#32947,#32948,#32949,#32950,#32951,#32952,#32953,#32954,#32955,#32956,#32957,
#32958,#32959,#32960,#32961,#32962,#32963,#32964,#32965,#32966,#32967,#32968,
#32969,#32970,#32971,#32972,#32973,#32974,#32975,#32976,#32977,#32978,#32979,
#32980,#32981,#32982,#32983,#32984,#32985,#32986,#32987,#32988,#32989,#32990,
#32991,#32992,#32993,#32994,#32995,#32996,#32997,#32998,#32999,#33000,#33001,
#33002,#33003,#33004,#33005,#33006,#33007,#33008,#33009,#33010,#33011,#33012,
#33013,#33014,#33015,#33016,#33017,#33018,#33019,#33020,#33021,#33022,#33023,
#33024,#33025,#33026,#33027,#33028,#33029,#33030,#33031,#33032,#33033,#33034,
#33035,#33036,#33037,#33038,#33039,#33040,#33041,#33042,#33043,#33044,#33045,
#33046,#33047,#33048,#33049,#33050,#33051,#33052,#33053,#33054,#33055,#33056,
#33057,#33058,#33059,#33060,#33061,#33062,#33063,#33064,#33065,#33066,#33067,
#33068,#33069,#33070,#33071,#33072,#33073,#33074,#33075,#33076,#33077,#33078,
#33079,#33080,#33081,#33082,#33083,#33084,#33085,#33086,#33087,#33088,#33089,
#33090,#33091,#33092,#33093,#33094,#33095,#33096,#33097,#33098,#33099,#33100,
#33101,#33102,#33103,#33104,#33105,#33106,#33107,#33108,#33109,#33110,#33111,
#33112,#33113,#33114,#33115,#33116,#33117,#33118,#33119,#33120,#33121,#33122,
#33123,#33124,#33125,#33126,#33127,#33128,#33129,#33130,#33131,#33132,#33133,
#33134,#33135,#33136,#33137,#33138,#33139,#33140,#33141,#33142,#33143,#33144,
#33145,#33146,#33147,#33148,#33149,#33150,#33151,#33152,#33153,#33154,#33155,
#33156,#33157,#33158,#33159,#33160,#33161,#33162,#33163,#33164,#33165));
#34175=CLOSED_SHELL('',(#33166,#33167,#33168,#33169,#33170,#33171,#33172,
#33173,#33174,#33175,#33176,#33177,#33178,#33179,#33180,#33181,#33182,#33183,
#33184,#33185,#33186,#33187,#33188,#33189,#33190,#33191,#33192,#33193,#33194,
#33195,#33196,#33197,#33198,#33199,#33200,#33201,#33202,#33203,#33204,#33205,
#33206,#33207,#33208,#33209,#33210,#33211,#33212,#33213,#33214,#33215,#33216,
#33217,#33218,#33219,#33220,#33221,#33222,#33223,#33224,#33225,#33226,#33227,
#33228,#33229,#33230,#33231,#33232,#33233,#33234,#33235,#33236,#33237,#33238,
#33239,#33240,#33241,#33242,#33243,#33244,#33245,#33246,#33247,#33248,#33249,
#33250,#33251,#33252,#33253,#33254,#33255,#33256,#33257,#33258,#33259,#33260,
#33261,#33262,#33263,#33264,#33265,#33266,#33267,#33268,#33269,#33270,#33271,
#33272,#33273,#33274,#33275,#33276,#33277,#33278,#33279,#33280,#33281,#33282,
#33283,#33284));
#34176=CLOSED_SHELL('',(#33285,#33286,#33287,#33288,#33289,#33290,#33291,
#33292,#33293,#33294,#33295,#33296,#33297,#33298,#33299,#33300,#33301,#33302,
#33303,#33304,#33305,#33306,#33307,#33308,#33309,#33310,#33311,#33312,#33313,
#33314,#33315,#33316,#33317,#33318,#33319,#33320,#33321,#33322,#33323,#33324,
#33325,#33326,#33327,#33328,#33329,#33330,#33331,#33332,#33333,#33334,#33335,
#33336,#33337,#33338,#33339,#33340,#33341,#33342,#33343,#33344,#33345,#33346,
#33347,#33348,#33349,#33350,#33351,#33352,#33353,#33354,#33355,#33356,#33357,
#33358,#33359,#33360,#33361,#33362,#33363,#33364,#33365,#33366,#33367,#33368,
#33369,#33370,#33371,#33372,#33373,#33374,#33375,#33376,#33377,#33378,#33379,
#33380,#33381,#33382,#33383,#33384,#33385,#33386,#33387,#33388,#33389,#33390,
#33391,#33392,#33393,#33394,#33395,#33396,#33397,#33398,#33399,#33400,#33401,
#33402,#33403,#33404,#33405,#33406,#33407,#33408,#33409,#33410,#33411,#33412,
#33413,#33414,#33415,#33416,#33417,#33418,#33419,#33420,#33421,#33422,#33423,
#33424,#33425,#33426,#33427,#33428,#33429,#33430,#33431,#33432,#33433,#33434,
#33435,#33436,#33437,#33438,#33439,#33440,#33441,#33442,#33443,#33444,#33445,
#33446,#33447,#33448,#33449,#33450,#33451,#33452,#33453,#33454,#33455,#33456,
#33457,#33458,#33459,#33460,#33461,#33462,#33463,#33464,#33465,#33466,#33467,
#33468,#33469,#33470,#33471,#33472,#33473,#33474,#33475,#33476,#33477,#33478,
#33479,#33480,#33481,#33482,#33483,#33484,#33485,#33486,#33487,#33488,#33489,
#33490,#33491,#33492,#33493,#33494,#33495,#33496,#33497,#33498,#33499,#33500,
#33501,#33502,#33503,#33504,#33505,#33506,#33507,#33508,#33509,#33510,#33511,
#33512,#33513,#33514,#33515,#33516,#33517,#33518,#33519,#33520,#33521,#33522,
#33523,#33524,#33525,#33526,#33527,#33528,#33529,#33530,#33531,#33532,#33533,
#33534,#33535,#33536,#33537,#33538,#33539,#33540,#33541,#33542,#33543,#33544,
#33545,#33546,#33547,#33548,#33549,#33550,#33551,#33552,#33553,#33554,#33555,
#33556,#33557,#33558,#33559,#33560,#33561,#33562,#33563,#33564,#33565,#33566,
#33567,#33568,#33569,#33570,#33571,#33572,#33573,#33574,#33575,#33576,#33577,
#33578,#33579,#33580,#33581,#33582,#33583,#33584,#33585,#33586,#33587,#33588,
#33589,#33590,#33591,#33592,#33593,#33594,#33595,#33596,#33597,#33598,#33599,
#33600,#33601,#33602,#33603,#33604,#33605,#33606,#33607,#33608,#33609,#33610,
#33611,#33612,#33613,#33614,#33615,#33616,#33617,#33618,#33619,#33620,#33621,
#33622,#33623,#33624,#33625,#33626,#33627,#33628,#33629,#33630,#33631,#33632,
#33633,#33634,#33635,#33636,#33637,#33638,#33639,#33640,#33641,#33642,#33643,
#33644,#33645,#33646,#33647,#33648,#33649,#33650,#33651,#33652,#33653,#33654,
#33655,#33656,#33657,#33658,#33659,#33660,#33661,#33662,#33663,#33664,#33665,
#33666,#33667,#33668,#33669,#33670,#33671,#33672,#33673,#33674,#33675,#33676,
#33677,#33678,#33679,#33680,#33681,#33682,#33683,#33684,#33685,#33686,#33687,
#33688,#33689,#33690,#33691,#33692,#33693,#33694,#33695,#33696,#33697,#33698,
#33699,#33700,#33701,#33702,#33703,#33704,#33705,#33706,#33707,#33708,#33709,
#33710,#33711,#33712,#33713,#33714,#33715,#33716,#33717,#33718,#33719,#33720,
#33721,#33722,#33723,#33724,#33725,#33726,#33727,#33728,#33729,#33730,#33731,
#33732,#33733,#33734,#33735,#33736,#33737,#33738,#33739,#33740,#33741,#33742,
#33743,#33744,#33745,#33746,#33747,#33748,#33749,#33750,#33751,#33752,#33753,
#33754,#33755,#33756,#33757,#33758,#33759,#33760,#33761,#33762,#33763,#33764,
#33765,#33766,#33767,#33768,#33769,#33770,#33771,#33772,#33773,#33774,#33775,
#33776,#33777,#33778,#33779,#33780,#33781,#33782,#33783,#33784,#33785,#33786,
#33787,#33788,#33789,#33790,#33791,#33792,#33793,#33794,#33795,#33796,#33797,
#33798,#33799,#33800,#33801,#33802,#33803,#33804,#33805,#33806,#33807,#33808,
#33809,#33810,#33811,#33812,#33813,#33814,#33815,#33816,#33817,#33818,#33819,
#33820,#33821,#33822,#33823,#33824,#33825,#33826,#33827,#33828,#33829,#33830,
#33831,#33832,#33833,#33834,#33835,#33836,#33837,#33838,#33839,#33840,#33841,
#33842,#33843,#33844,#33845,#33846,#33847,#33848,#33849,#33850,#33851,#33852,
#33853,#33854,#33855,#33856,#33857,#33858,#33859,#33860,#33861,#33862,#33863,
#33864,#33865,#33866,#33867,#33868,#33869,#33870,#33871,#33872,#33873,#33874,
#33875,#33876,#33877,#33878,#33879,#33880,#33881,#33882,#33883,#33884,#33885,
#33886,#33887,#33888,#33889,#33890,#33891,#33892,#33893,#33894,#33895,#33896,
#33897,#33898,#33899,#33900,#33901,#33902,#33903,#33904,#33905,#33906,#33907,
#33908,#33909,#33910,#33911,#33912,#33913,#33914,#33915,#33916,#33917,#33918,
#33919,#33920,#33921,#33922,#33923,#33924,#33925,#33926,#33927,#33928,#33929,
#33930,#33931,#33932));
#34177=CLOSED_SHELL('',(#33933,#33934,#33935,#33936,#33937,#33938,#33939,
#33940,#33941,#33942,#33943,#33944,#33945,#33946,#33947,#33948,#33949,#33950,
#33951,#33952,#33953,#33954,#33955,#33956,#33957,#33958,#33959,#33960,#33961,
#33962,#33963,#33964,#33965,#33966,#33967,#33968,#33969,#33970,#33971,#33972,
#33973,#33974,#33975,#33976,#33977,#33978,#33979,#33980,#33981,#33982,#33983,
#33984,#33985,#33986,#33987,#33988,#33989,#33990,#33991,#33992,#33993,#33994,
#33995,#33996,#33997,#33998,#33999,#34000,#34001,#34002,#34003,#34004,#34005,
#34006,#34007,#34008,#34009,#34010,#34011,#34012,#34013,#34014,#34015,#34016,
#34017,#34018,#34019,#34020,#34021,#34022,#34023,#34024,#34025,#34026,#34027,
#34028,#34029,#34030,#34031,#34032,#34033,#34034,#34035,#34036,#34037,#34038,
#34039,#34040,#34041));
#34178=CLOSED_SHELL('',(#34042,#34043,#34044,#34045,#34046,#34047,#34048,
#34049,#34050,#34051,#34052,#34053,#34054,#34055,#34056,#34057,#34058,#34059,
#34060,#34061,#34062,#34063,#34064,#34065,#34066,#34067,#34068,#34069,#34070,
#34071,#34072,#34073,#34074,#34075,#34076,#34077,#34078,#34079,#34080,#34081,
#34082,#34083,#34084,#34085,#34086,#34087,#34088,#34089,#34090,#34091,#34092,
#34093,#34094,#34095,#34096,#34097,#34098,#34099,#34100,#34101,#34102,#34103,
#34104,#34105,#34106,#34107,#34108,#34109,#34110,#34111,#34112,#34113,#34114,
#34115,#34116,#34117,#34118,#34119,#34120,#34121,#34122,#34123,#34124,#34125,
#34126,#34127,#34128,#34129,#34130,#34131,#34132,#34133,#34134,#34135,#34136,
#34137,#34138,#34139,#34140,#34141,#34142,#34143,#34144,#34145,#34146,#34147,
#34148,#34149,#34150,#34151,#34152,#34153,#34154,#34155,#34156,#34157,#34158,
#34159,#34160,#34161,#34162,#34163,#34164,#34165,#34166));
#34179=DERIVED_UNIT_ELEMENT(#34199,1.);
#34180=DERIVED_UNIT_ELEMENT(#98304,-3.);
#34181=DERIVED_UNIT_ELEMENT(#34199,1.);
#34182=DERIVED_UNIT_ELEMENT(#98304,-3.);
#34183=DERIVED_UNIT_ELEMENT(#34199,1.);
#34184=DERIVED_UNIT_ELEMENT(#98304,-3.);
#34185=DERIVED_UNIT_ELEMENT(#34199,1.);
#34186=DERIVED_UNIT_ELEMENT(#98304,-3.);
#34187=DERIVED_UNIT_ELEMENT(#34199,1.);
#34188=DERIVED_UNIT_ELEMENT(#98304,-3.);
#34189=DERIVED_UNIT_ELEMENT(#34199,1.);
#34190=DERIVED_UNIT_ELEMENT(#98304,-3.);
#34191=DERIVED_UNIT_ELEMENT(#34199,1.);
#34192=DERIVED_UNIT_ELEMENT(#98304,-3.);
#34193=DERIVED_UNIT_ELEMENT(#34199,1.);
#34194=DERIVED_UNIT_ELEMENT(#98304,-3.);
#34195=DERIVED_UNIT_ELEMENT(#34199,1.);
#34196=DERIVED_UNIT_ELEMENT(#98304,-3.);
#34197=DERIVED_UNIT_ELEMENT(#34199,1.);
#34198=DERIVED_UNIT_ELEMENT(#98304,-3.);
#34199=(
MASS_UNIT()
NAMED_UNIT(*)
SI_UNIT(.KILO.,.GRAM.)
);
#34200=DERIVED_UNIT((#34179,#34180));
#34201=DERIVED_UNIT((#34181,#34182));
#34202=DERIVED_UNIT((#34183,#34184));
#34203=DERIVED_UNIT((#34185,#34186));
#34204=DERIVED_UNIT((#34187,#34188));
#34205=DERIVED_UNIT((#34189,#34190));
#34206=DERIVED_UNIT((#34191,#34192));
#34207=DERIVED_UNIT((#34193,#34194));
#34208=DERIVED_UNIT((#34195,#34196));
#34209=DERIVED_UNIT((#34197,#34198));
#34210=MEASURE_REPRESENTATION_ITEM('density measure',
POSITIVE_RATIO_MEASURE(7850.),#34200);
#34211=MEASURE_REPRESENTATION_ITEM('density measure',
POSITIVE_RATIO_MEASURE(7850.),#34201);
#34212=MEASURE_REPRESENTATION_ITEM('density measure',
POSITIVE_RATIO_MEASURE(7850.),#34202);
#34213=MEASURE_REPRESENTATION_ITEM('density measure',
POSITIVE_RATIO_MEASURE(7850.),#34203);
#34214=MEASURE_REPRESENTATION_ITEM('density measure',
POSITIVE_RATIO_MEASURE(7850.),#34204);
#34215=MEASURE_REPRESENTATION_ITEM('density measure',
POSITIVE_RATIO_MEASURE(7850.),#34205);
#34216=MEASURE_REPRESENTATION_ITEM('density measure',
POSITIVE_RATIO_MEASURE(7850.),#34206);
#34217=MEASURE_REPRESENTATION_ITEM('density measure',
POSITIVE_RATIO_MEASURE(7850.),#34207);
#34218=MEASURE_REPRESENTATION_ITEM('density measure',
POSITIVE_RATIO_MEASURE(7850.),#34208);
#34219=MEASURE_REPRESENTATION_ITEM('density measure',
POSITIVE_RATIO_MEASURE(7850.),#34209);
#34220=PROPERTY_DEFINITION_REPRESENTATION(#34270,#34240);
#34221=PROPERTY_DEFINITION_REPRESENTATION(#34271,#34241);
#34222=PROPERTY_DEFINITION_REPRESENTATION(#34272,#34242);
#34223=PROPERTY_DEFINITION_REPRESENTATION(#34273,#34243);
#34224=PROPERTY_DEFINITION_REPRESENTATION(#34274,#34244);
#34225=PROPERTY_DEFINITION_REPRESENTATION(#34275,#34245);
#34226=PROPERTY_DEFINITION_REPRESENTATION(#34276,#34246);
#34227=PROPERTY_DEFINITION_REPRESENTATION(#34277,#34247);
#34228=PROPERTY_DEFINITION_REPRESENTATION(#34278,#34248);
#34229=PROPERTY_DEFINITION_REPRESENTATION(#34279,#34249);
#34230=PROPERTY_DEFINITION_REPRESENTATION(#34280,#34250);
#34231=PROPERTY_DEFINITION_REPRESENTATION(#34281,#34251);
#34232=PROPERTY_DEFINITION_REPRESENTATION(#34282,#34252);
#34233=PROPERTY_DEFINITION_REPRESENTATION(#34283,#34253);
#34234=PROPERTY_DEFINITION_REPRESENTATION(#34284,#34254);
#34235=PROPERTY_DEFINITION_REPRESENTATION(#34285,#34255);
#34236=PROPERTY_DEFINITION_REPRESENTATION(#34286,#34256);
#34237=PROPERTY_DEFINITION_REPRESENTATION(#34287,#34257);
#34238=PROPERTY_DEFINITION_REPRESENTATION(#34288,#34258);
#34239=PROPERTY_DEFINITION_REPRESENTATION(#34289,#34259);
#34240=REPRESENTATION('material name',(#34260),#98292);
#34241=REPRESENTATION('density',(#34210),#98292);
#34242=REPRESENTATION('material name',(#34261),#98293);
#34243=REPRESENTATION('density',(#34211),#98293);
#34244=REPRESENTATION('material name',(#34262),#98294);
#34245=REPRESENTATION('density',(#34212),#98294);
#34246=REPRESENTATION('material name',(#34263),#98295);
#34247=REPRESENTATION('density',(#34213),#98295);
#34248=REPRESENTATION('material name',(#34264),#98296);
#34249=REPRESENTATION('density',(#34214),#98296);
#34250=REPRESENTATION('material name',(#34265),#98297);
#34251=REPRESENTATION('density',(#34215),#98297);
#34252=REPRESENTATION('material name',(#34266),#98298);
#34253=REPRESENTATION('density',(#34216),#98298);
#34254=REPRESENTATION('material name',(#34267),#98299);
#34255=REPRESENTATION('density',(#34217),#98299);
#34256=REPRESENTATION('material name',(#34268),#98300);
#34257=REPRESENTATION('density',(#34218),#98300);
#34258=REPRESENTATION('material name',(#34269),#98301);
#34259=REPRESENTATION('density',(#34219),#98301);
#34260=DESCRIPTIVE_REPRESENTATION_ITEM('Steel','Steel');
#34261=DESCRIPTIVE_REPRESENTATION_ITEM('Steel','Steel');
#34262=DESCRIPTIVE_REPRESENTATION_ITEM('Steel','Steel');
#34263=DESCRIPTIVE_REPRESENTATION_ITEM('Steel','Steel');
#34264=DESCRIPTIVE_REPRESENTATION_ITEM('Steel','Steel');
#34265=DESCRIPTIVE_REPRESENTATION_ITEM('Steel','Steel');
#34266=DESCRIPTIVE_REPRESENTATION_ITEM('Steel','Steel');
#34267=DESCRIPTIVE_REPRESENTATION_ITEM('Steel','Steel');
#34268=DESCRIPTIVE_REPRESENTATION_ITEM('Steel','Steel');
#34269=DESCRIPTIVE_REPRESENTATION_ITEM('Steel','Steel');
#34270=PROPERTY_DEFINITION('material property','material name',#98352);
#34271=PROPERTY_DEFINITION('material property','density of part',#98352);
#34272=PROPERTY_DEFINITION('material property','material name',#98353);
#34273=PROPERTY_DEFINITION('material property','density of part',#98353);
#34274=PROPERTY_DEFINITION('material property','material name',#98354);
#34275=PROPERTY_DEFINITION('material property','density of part',#98354);
#34276=PROPERTY_DEFINITION('material property','material name',#98355);
#34277=PROPERTY_DEFINITION('material property','density of part',#98355);
#34278=PROPERTY_DEFINITION('material property','material name',#98356);
#34279=PROPERTY_DEFINITION('material property','density of part',#98356);
#34280=PROPERTY_DEFINITION('material property','material name',#98357);
#34281=PROPERTY_DEFINITION('material property','density of part',#98357);
#34282=PROPERTY_DEFINITION('material property','material name',#98358);
#34283=PROPERTY_DEFINITION('material property','density of part',#98358);
#34284=PROPERTY_DEFINITION('material property','material name',#98359);
#34285=PROPERTY_DEFINITION('material property','density of part',#98359);
#34286=PROPERTY_DEFINITION('material property','material name',#98360);
#34287=PROPERTY_DEFINITION('material property','density of part',#98360);
#34288=PROPERTY_DEFINITION('material property','material name',#98361);
#34289=PROPERTY_DEFINITION('material property','density of part',#98361);
#34290=AXIS2_PLACEMENT_3D('',#49108,#38616,#38617);
#34291=AXIS2_PLACEMENT_3D('',#49109,#38618,#38619);
#34292=AXIS2_PLACEMENT_3D('',#49110,#38620,#38621);
#34293=AXIS2_PLACEMENT_3D('',#49113,#38622,#38623);
#34294=AXIS2_PLACEMENT_3D('',#49116,#38625,#38626);
#34295=AXIS2_PLACEMENT_3D('',#49117,#38627,#38628);
#34296=AXIS2_PLACEMENT_3D('',#49118,#38629,#38630);
#34297=AXIS2_PLACEMENT_3D('',#49121,#38631,#38632);
#34298=AXIS2_PLACEMENT_3D('',#49123,#38634,#38635);
#34299=AXIS2_PLACEMENT_3D('',#49124,#38636,#38637);
#34300=AXIS2_PLACEMENT_3D('',#49125,#38638,#38639);
#34301=AXIS2_PLACEMENT_3D('',#49128,#38641,#38642);
#34302=AXIS2_PLACEMENT_3D('',#49129,#38643,#38644);
#34303=AXIS2_PLACEMENT_3D('',#49130,#38645,#38646);
#34304=AXIS2_PLACEMENT_3D('',#49131,#38647,#38648);
#34305=AXIS2_PLACEMENT_3D('',#49136,#38650,#38651);
#34306=AXIS2_PLACEMENT_3D('',#49139,#38653,#38654);
#34307=AXIS2_PLACEMENT_3D('',#49140,#38655,#38656);
#34308=AXIS2_PLACEMENT_3D('',#49145,#38658,#38659);
#34309=AXIS2_PLACEMENT_3D('',#49147,#38660,#38661);
#34310=AXIS2_PLACEMENT_3D('',#49149,#38662,#38663);
#34311=AXIS2_PLACEMENT_3D('',#49153,#38665,#38666);
#34312=AXIS2_PLACEMENT_3D('',#49157,#38668,#38669);
#34313=AXIS2_PLACEMENT_3D('',#49161,#38671,#38672);
#34314=AXIS2_PLACEMENT_3D('',#49163,#38673,#38674);
#34315=AXIS2_PLACEMENT_3D('',#49165,#38675,#38676);
#34316=AXIS2_PLACEMENT_3D('',#49169,#38678,#38679);
#34317=AXIS2_PLACEMENT_3D('',#49173,#38681,#38682);
#34318=AXIS2_PLACEMENT_3D('',#49177,#38684,#38685);
#34319=AXIS2_PLACEMENT_3D('',#49179,#38686,#38687);
#34320=AXIS2_PLACEMENT_3D('',#49181,#38688,#38689);
#34321=AXIS2_PLACEMENT_3D('',#49185,#38691,#38692);
#34322=AXIS2_PLACEMENT_3D('',#49187,#38693,#38694);
#34323=AXIS2_PLACEMENT_3D('',#49189,#38695,#38696);
#34324=AXIS2_PLACEMENT_3D('',#49193,#38698,#38699);
#34325=AXIS2_PLACEMENT_3D('',#49197,#38701,#38702);
#34326=AXIS2_PLACEMENT_3D('',#49201,#38704,#38705);
#34327=AXIS2_PLACEMENT_3D('',#49203,#38706,#38707);
#34328=AXIS2_PLACEMENT_3D('',#49205,#38708,#38709);
#34329=AXIS2_PLACEMENT_3D('',#49209,#38711,#38712);
#34330=AXIS2_PLACEMENT_3D('',#49213,#38714,#38715);
#34331=AXIS2_PLACEMENT_3D('',#49217,#38717,#38718);
#34332=AXIS2_PLACEMENT_3D('',#49219,#38719,#38720);
#34333=AXIS2_PLACEMENT_3D('',#49220,#38721,#38722);
#34334=AXIS2_PLACEMENT_3D('',#49223,#38723,#38724);
#34335=AXIS2_PLACEMENT_3D('',#49271,#38725,#38726);
#34336=AXIS2_PLACEMENT_3D('',#49275,#38728,#38729);
#34337=AXIS2_PLACEMENT_3D('',#49286,#38730,#38731);
#34338=AXIS2_PLACEMENT_3D('',#49288,#38732,#38733);
#34339=AXIS2_PLACEMENT_3D('',#49290,#38734,#38735);
#34340=AXIS2_PLACEMENT_3D('',#49293,#38737,#38738);
#34341=AXIS2_PLACEMENT_3D('',#49295,#38739,#38740);
#34342=AXIS2_PLACEMENT_3D('',#49297,#38741,#38742);
#34343=AXIS2_PLACEMENT_3D('',#49303,#38745,#38746);
#34344=AXIS2_PLACEMENT_3D('',#49359,#38747,#38748);
#34345=AXIS2_PLACEMENT_3D('',#49365,#38749,#38750);
#34346=AXIS2_PLACEMENT_3D('',#49453,#38753,#38754);
#34347=AXIS2_PLACEMENT_3D('',#49455,#38755,#38756);
#34348=AXIS2_PLACEMENT_3D('',#49456,#38757,#38758);
#34349=AXIS2_PLACEMENT_3D('',#49457,#38759,#38760);
#34350=AXIS2_PLACEMENT_3D('',#49522,#38767,#38768);
#34351=AXIS2_PLACEMENT_3D('',#49535,#38770,#38771);
#34352=AXIS2_PLACEMENT_3D('',#49536,#38772,#38773);
#34353=AXIS2_PLACEMENT_3D('',#49540,#38776,#38777);
#34354=AXIS2_PLACEMENT_3D('',#49544,#38779,#38780);
#34355=AXIS2_PLACEMENT_3D('',#49586,#38781,#38782);
#34356=AXIS2_PLACEMENT_3D('',#49670,#38784,#38785);
#34357=AXIS2_PLACEMENT_3D('',#49745,#38786,#38787);
#34358=AXIS2_PLACEMENT_3D('',#49872,#38790,#38791);
#34359=AXIS2_PLACEMENT_3D('',#49975,#38794,#38795);
#34360=AXIS2_PLACEMENT_3D('',#49977,#38796,#38797);
#34361=AXIS2_PLACEMENT_3D('',#50020,#38798,#38799);
#34362=AXIS2_PLACEMENT_3D('',#50024,#38801,#38802);
#34363=AXIS2_PLACEMENT_3D('',#50118,#38805,#38806);
#34364=AXIS2_PLACEMENT_3D('',#50164,#38808,#38809);
#34365=AXIS2_PLACEMENT_3D('',#50373,#38813,#38814);
#34366=AXIS2_PLACEMENT_3D('',#50639,#38817,#38818);
#34367=AXIS2_PLACEMENT_3D('',#50784,#38819,#38820);
#34368=AXIS2_PLACEMENT_3D('',#50873,#38821,#38822);
#34369=AXIS2_PLACEMENT_3D('',#50877,#38824,#38825);
#34370=AXIS2_PLACEMENT_3D('',#50919,#38826,#38827);
#34371=AXIS2_PLACEMENT_3D('',#50920,#38828,#38829);
#34372=AXIS2_PLACEMENT_3D('',#50922,#38831,#38832);
#34373=AXIS2_PLACEMENT_3D('',#50925,#38833,#38834);
#34374=AXIS2_PLACEMENT_3D('',#50929,#38836,#38837);
#34375=AXIS2_PLACEMENT_3D('',#50931,#38839,#38840);
#34376=AXIS2_PLACEMENT_3D('',#50932,#38841,#38842);
#34377=AXIS2_PLACEMENT_3D('',#50933,#38843,#38844);
#34378=AXIS2_PLACEMENT_3D('',#50934,#38845,#38846);
#34379=AXIS2_PLACEMENT_3D('',#50936,#38847,#38848);
#34380=AXIS2_PLACEMENT_3D('',#50937,#38849,#38850);
#34381=AXIS2_PLACEMENT_3D('',#50938,#38851,#38852);
#34382=AXIS2_PLACEMENT_3D('',#50941,#38854,#38855);
#34383=AXIS2_PLACEMENT_3D('',#50942,#38856,#38857);
#34384=AXIS2_PLACEMENT_3D('',#50944,#38858,#38859);
#34385=AXIS2_PLACEMENT_3D('',#50946,#38861,#38862);
#34386=AXIS2_PLACEMENT_3D('',#50950,#38865,#38866);
#34387=AXIS2_PLACEMENT_3D('',#50952,#38867,#38868);
#34388=AXIS2_PLACEMENT_3D('',#50953,#38869,#38870);
#34389=AXIS2_PLACEMENT_3D('',#50954,#38871,#38872);
#34390=AXIS2_PLACEMENT_3D('',#50957,#38874,#38875);
#34391=AXIS2_PLACEMENT_3D('',#50958,#38876,#38877);
#34392=AXIS2_PLACEMENT_3D('',#50960,#38878,#38879);
#34393=AXIS2_PLACEMENT_3D('',#50962,#38881,#38882);
#34394=AXIS2_PLACEMENT_3D('',#50966,#38885,#38886);
#34395=AXIS2_PLACEMENT_3D('',#50968,#38887,#38888);
#34396=AXIS2_PLACEMENT_3D('',#50969,#38889,#38890);
#34397=AXIS2_PLACEMENT_3D('',#50970,#38891,#38892);
#34398=AXIS2_PLACEMENT_3D('',#50973,#38894,#38895);
#34399=AXIS2_PLACEMENT_3D('',#50974,#38896,#38897);
#34400=AXIS2_PLACEMENT_3D('',#50976,#38898,#38899);
#34401=AXIS2_PLACEMENT_3D('',#50978,#38901,#38902);
#34402=AXIS2_PLACEMENT_3D('',#50982,#38905,#38906);
#34403=AXIS2_PLACEMENT_3D('',#50984,#38907,#38908);
#34404=AXIS2_PLACEMENT_3D('',#50985,#38909,#38910);
#34405=AXIS2_PLACEMENT_3D('',#50986,#38911,#38912);
#34406=AXIS2_PLACEMENT_3D('',#50989,#38914,#38915);
#34407=AXIS2_PLACEMENT_3D('',#50990,#38916,#38917);
#34408=AXIS2_PLACEMENT_3D('',#50992,#38918,#38919);
#34409=AXIS2_PLACEMENT_3D('',#50993,#38920,#38921);
#34410=AXIS2_PLACEMENT_3D('',#50994,#38922,#38923);
#34411=AXIS2_PLACEMENT_3D('',#50997,#38925,#38926);
#34412=AXIS2_PLACEMENT_3D('',#50998,#38927,#38928);
#34413=AXIS2_PLACEMENT_3D('',#51000,#38929,#38930);
#34414=AXIS2_PLACEMENT_3D('',#51001,#38931,#38932);
#34415=AXIS2_PLACEMENT_3D('',#51002,#38933,#38934);
#34416=AXIS2_PLACEMENT_3D('',#51005,#38936,#38937);
#34417=AXIS2_PLACEMENT_3D('',#51006,#38938,#38939);
#34418=AXIS2_PLACEMENT_3D('',#51008,#38940,#38941);
#34419=AXIS2_PLACEMENT_3D('',#51010,#38943,#38944);
#34420=AXIS2_PLACEMENT_3D('',#51014,#38947,#38948);
#34421=AXIS2_PLACEMENT_3D('',#51016,#38949,#38950);
#34422=AXIS2_PLACEMENT_3D('',#51017,#38951,#38952);
#34423=AXIS2_PLACEMENT_3D('',#51018,#38953,#38954);
#34424=AXIS2_PLACEMENT_3D('',#51021,#38956,#38957);
#34425=AXIS2_PLACEMENT_3D('',#51022,#38958,#38959);
#34426=AXIS2_PLACEMENT_3D('',#51024,#38960,#38961);
#34427=AXIS2_PLACEMENT_3D('',#51025,#38962,#38963);
#34428=AXIS2_PLACEMENT_3D('',#51026,#38964,#38965);
#34429=AXIS2_PLACEMENT_3D('',#51029,#38967,#38968);
#34430=AXIS2_PLACEMENT_3D('',#51030,#38969,#38970);
#34431=AXIS2_PLACEMENT_3D('',#51032,#38971,#38972);
#34432=AXIS2_PLACEMENT_3D('',#51033,#38973,#38974);
#34433=AXIS2_PLACEMENT_3D('',#51034,#38975,#38976);
#34434=AXIS2_PLACEMENT_3D('',#51037,#38978,#38979);
#34435=AXIS2_PLACEMENT_3D('',#51038,#38980,#38981);
#34436=AXIS2_PLACEMENT_3D('',#51040,#38982,#38983);
#34437=AXIS2_PLACEMENT_3D('',#51042,#38985,#38986);
#34438=AXIS2_PLACEMENT_3D('',#51046,#38989,#38990);
#34439=AXIS2_PLACEMENT_3D('',#51048,#38991,#38992);
#34440=AXIS2_PLACEMENT_3D('',#51049,#38993,#38994);
#34441=AXIS2_PLACEMENT_3D('',#51050,#38995,#38996);
#34442=AXIS2_PLACEMENT_3D('',#51053,#38998,#38999);
#34443=AXIS2_PLACEMENT_3D('',#51054,#39000,#39001);
#34444=AXIS2_PLACEMENT_3D('',#51056,#39002,#39003);
#34445=AXIS2_PLACEMENT_3D('',#51058,#39005,#39006);
#34446=AXIS2_PLACEMENT_3D('',#51062,#39009,#39010);
#34447=AXIS2_PLACEMENT_3D('',#51064,#39011,#39012);
#34448=AXIS2_PLACEMENT_3D('',#51065,#39013,#39014);
#34449=AXIS2_PLACEMENT_3D('',#51066,#39015,#39016);
#34450=AXIS2_PLACEMENT_3D('',#51069,#39018,#39019);
#34451=AXIS2_PLACEMENT_3D('',#51070,#39020,#39021);
#34452=AXIS2_PLACEMENT_3D('',#51072,#39022,#39023);
#34453=AXIS2_PLACEMENT_3D('',#51074,#39025,#39026);
#34454=AXIS2_PLACEMENT_3D('',#51078,#39029,#39030);
#34455=AXIS2_PLACEMENT_3D('',#51080,#39031,#39032);
#34456=AXIS2_PLACEMENT_3D('',#51081,#39033,#39034);
#34457=AXIS2_PLACEMENT_3D('',#51082,#39035,#39036);
#34458=AXIS2_PLACEMENT_3D('',#51085,#39038,#39039);
#34459=AXIS2_PLACEMENT_3D('',#51086,#39040,#39041);
#34460=AXIS2_PLACEMENT_3D('',#51088,#39042,#39043);
#34461=AXIS2_PLACEMENT_3D('',#51090,#39044,#39045);
#34462=AXIS2_PLACEMENT_3D('',#51092,#39047,#39048);
#34463=AXIS2_PLACEMENT_3D('',#51093,#39049,#39050);
#34464=AXIS2_PLACEMENT_3D('',#51094,#39051,#39052);
#34465=AXIS2_PLACEMENT_3D('',#51096,#39053,#39054);
#34466=AXIS2_PLACEMENT_3D('',#51097,#39055,#39056);
#34467=AXIS2_PLACEMENT_3D('',#51098,#39057,#39058);
#34468=AXIS2_PLACEMENT_3D('',#51101,#39060,#39061);
#34469=AXIS2_PLACEMENT_3D('',#51102,#39062,#39063);
#34470=AXIS2_PLACEMENT_3D('',#51104,#39064,#39065);
#34471=AXIS2_PLACEMENT_3D('',#51106,#39067,#39068);
#34472=AXIS2_PLACEMENT_3D('',#51110,#39071,#39072);
#34473=AXIS2_PLACEMENT_3D('',#51112,#39073,#39074);
#34474=AXIS2_PLACEMENT_3D('',#51113,#39075,#39076);
#34475=AXIS2_PLACEMENT_3D('',#51114,#39077,#39078);
#34476=AXIS2_PLACEMENT_3D('',#51117,#39080,#39081);
#34477=AXIS2_PLACEMENT_3D('',#51118,#39082,#39083);
#34478=AXIS2_PLACEMENT_3D('',#51120,#39084,#39085);
#34479=AXIS2_PLACEMENT_3D('',#51122,#39087,#39088);
#34480=AXIS2_PLACEMENT_3D('',#51126,#39091,#39092);
#34481=AXIS2_PLACEMENT_3D('',#51128,#39093,#39094);
#34482=AXIS2_PLACEMENT_3D('',#51129,#39095,#39096);
#34483=AXIS2_PLACEMENT_3D('',#51130,#39097,#39098);
#34484=AXIS2_PLACEMENT_3D('',#51133,#39100,#39101);
#34485=AXIS2_PLACEMENT_3D('',#51134,#39102,#39103);
#34486=AXIS2_PLACEMENT_3D('',#51136,#39104,#39105);
#34487=AXIS2_PLACEMENT_3D('',#51138,#39107,#39108);
#34488=AXIS2_PLACEMENT_3D('',#51142,#39111,#39112);
#34489=AXIS2_PLACEMENT_3D('',#51144,#39113,#39114);
#34490=AXIS2_PLACEMENT_3D('',#51145,#39115,#39116);
#34491=AXIS2_PLACEMENT_3D('',#51146,#39117,#39118);
#34492=AXIS2_PLACEMENT_3D('',#51149,#39120,#39121);
#34493=AXIS2_PLACEMENT_3D('',#51150,#39122,#39123);
#34494=AXIS2_PLACEMENT_3D('',#51152,#39124,#39125);
#34495=AXIS2_PLACEMENT_3D('',#51153,#39126,#39127);
#34496=AXIS2_PLACEMENT_3D('',#51154,#39128,#39129);
#34497=AXIS2_PLACEMENT_3D('',#51157,#39131,#39132);
#34498=AXIS2_PLACEMENT_3D('',#51158,#39133,#39134);
#34499=AXIS2_PLACEMENT_3D('',#51160,#39135,#39136);
#34500=AXIS2_PLACEMENT_3D('',#51161,#39137,#39138);
#34501=AXIS2_PLACEMENT_3D('',#51162,#39139,#39140);
#34502=AXIS2_PLACEMENT_3D('',#51165,#39142,#39143);
#34503=AXIS2_PLACEMENT_3D('',#51166,#39144,#39145);
#34504=AXIS2_PLACEMENT_3D('',#51168,#39146,#39147);
#34505=AXIS2_PLACEMENT_3D('',#51170,#39149,#39150);
#34506=AXIS2_PLACEMENT_3D('',#51174,#39153,#39154);
#34507=AXIS2_PLACEMENT_3D('',#51176,#39155,#39156);
#34508=AXIS2_PLACEMENT_3D('',#51177,#39157,#39158);
#34509=AXIS2_PLACEMENT_3D('',#51178,#39159,#39160);
#34510=AXIS2_PLACEMENT_3D('',#51181,#39162,#39163);
#34511=AXIS2_PLACEMENT_3D('',#51182,#39164,#39165);
#34512=AXIS2_PLACEMENT_3D('',#51184,#39166,#39167);
#34513=AXIS2_PLACEMENT_3D('',#51185,#39168,#39169);
#34514=AXIS2_PLACEMENT_3D('',#51186,#39170,#39171);
#34515=AXIS2_PLACEMENT_3D('',#51189,#39173,#39174);
#34516=AXIS2_PLACEMENT_3D('',#51190,#39175,#39176);
#34517=AXIS2_PLACEMENT_3D('',#51192,#39177,#39178);
#34518=AXIS2_PLACEMENT_3D('',#51193,#39179,#39180);
#34519=AXIS2_PLACEMENT_3D('',#51194,#39181,#39182);
#34520=AXIS2_PLACEMENT_3D('',#51197,#39184,#39185);
#34521=AXIS2_PLACEMENT_3D('',#51198,#39186,#39187);
#34522=AXIS2_PLACEMENT_3D('',#51200,#39188,#39189);
#34523=AXIS2_PLACEMENT_3D('',#51202,#39191,#39192);
#34524=AXIS2_PLACEMENT_3D('',#51206,#39195,#39196);
#34525=AXIS2_PLACEMENT_3D('',#51208,#39197,#39198);
#34526=AXIS2_PLACEMENT_3D('',#51209,#39199,#39200);
#34527=AXIS2_PLACEMENT_3D('',#51210,#39201,#39202);
#34528=AXIS2_PLACEMENT_3D('',#51213,#39204,#39205);
#34529=AXIS2_PLACEMENT_3D('',#51214,#39206,#39207);
#34530=AXIS2_PLACEMENT_3D('',#51216,#39208,#39209);
#34531=AXIS2_PLACEMENT_3D('',#51218,#39211,#39212);
#34532=AXIS2_PLACEMENT_3D('',#51222,#39215,#39216);
#34533=AXIS2_PLACEMENT_3D('',#51224,#39217,#39218);
#34534=AXIS2_PLACEMENT_3D('',#51225,#39219,#39220);
#34535=AXIS2_PLACEMENT_3D('',#51226,#39221,#39222);
#34536=AXIS2_PLACEMENT_3D('',#51228,#39223,#39224);
#34537=AXIS2_PLACEMENT_3D('',#51230,#39226,#39227);
#34538=AXIS2_PLACEMENT_3D('',#51232,#39228,#39229);
#34539=AXIS2_PLACEMENT_3D('',#51233,#39230,#39231);
#34540=AXIS2_PLACEMENT_3D('',#51234,#39232,#39233);
#34541=AXIS2_PLACEMENT_3D('',#51237,#39235,#39236);
#34542=AXIS2_PLACEMENT_3D('',#51238,#39237,#39238);
#34543=AXIS2_PLACEMENT_3D('',#51240,#39240,#39241);
#34544=AXIS2_PLACEMENT_3D('',#51242,#39243,#39244);
#34545=AXIS2_PLACEMENT_3D('',#51328,#39251,#39252);
#34546=AXIS2_PLACEMENT_3D('',#51334,#39255,#39256);
#34547=AXIS2_PLACEMENT_3D('',#51367,#39259,#39260);
#34548=AXIS2_PLACEMENT_3D('',#51530,#39263,#39264);
#34549=AXIS2_PLACEMENT_3D('',#51694,#39269,#39270);
#34550=AXIS2_PLACEMENT_3D('',#51817,#39271,#39272);
#34551=AXIS2_PLACEMENT_3D('',#51823,#39276,#39277);
#34552=AXIS2_PLACEMENT_3D('',#51866,#39281,#39282);
#34553=AXIS2_PLACEMENT_3D('',#51899,#39283,#39284);
#34554=AXIS2_PLACEMENT_3D('',#51955,#39285,#39286);
#34555=AXIS2_PLACEMENT_3D('',#51994,#39287,#39288);
#34556=AXIS2_PLACEMENT_3D('',#52041,#39289,#39290);
#34557=AXIS2_PLACEMENT_3D('',#52043,#39291,#39292);
#34558=AXIS2_PLACEMENT_3D('',#52082,#39294,#39295);
#34559=AXIS2_PLACEMENT_3D('',#52084,#39296,#39297);
#34560=AXIS2_PLACEMENT_3D('',#52085,#39298,#39299);
#34561=AXIS2_PLACEMENT_3D('',#52178,#39300,#39301);
#34562=AXIS2_PLACEMENT_3D('',#52215,#39302,#39303);
#34563=AXIS2_PLACEMENT_3D('',#52289,#39304,#39305);
#34564=AXIS2_PLACEMENT_3D('',#52424,#39306,#39307);
#34565=AXIS2_PLACEMENT_3D('',#52480,#39308,#39309);
#34566=AXIS2_PLACEMENT_3D('',#52561,#39310,#39311);
#34567=AXIS2_PLACEMENT_3D('',#52727,#39312,#39313);
#34568=AXIS2_PLACEMENT_3D('',#52793,#39314,#39315);
#34569=AXIS2_PLACEMENT_3D('',#52943,#39316,#39317);
#34570=AXIS2_PLACEMENT_3D('',#53006,#39318,#39319);
#34571=AXIS2_PLACEMENT_3D('',#53099,#39320,#39321);
#34572=AXIS2_PLACEMENT_3D('',#53237,#39322,#39323);
#34573=AXIS2_PLACEMENT_3D('',#53457,#39326,#39327);
#34574=AXIS2_PLACEMENT_3D('',#53538,#39329,#39330);
#34575=AXIS2_PLACEMENT_3D('',#53576,#39331,#39332);
#34576=AXIS2_PLACEMENT_3D('',#53577,#39333,#39334);
#34577=AXIS2_PLACEMENT_3D('',#53651,#39335,#39336);
#34578=AXIS2_PLACEMENT_3D('',#53725,#39337,#39338);
#34579=AXIS2_PLACEMENT_3D('',#53737,#39339,#39340);
#34580=AXIS2_PLACEMENT_3D('',#53801,#39341,#39342);
#34581=AXIS2_PLACEMENT_3D('',#53839,#39343,#39344);
#34582=AXIS2_PLACEMENT_3D('',#53883,#39345,#39346);
#34583=AXIS2_PLACEMENT_3D('',#53884,#39347,#39348);
#34584=AXIS2_PLACEMENT_3D('',#53885,#39349,#39350);
#34585=AXIS2_PLACEMENT_3D('',#53940,#39351,#39352);
#34586=AXIS2_PLACEMENT_3D('',#53977,#39353,#39354);
#34587=AXIS2_PLACEMENT_3D('',#54159,#39356,#39357);
#34588=AXIS2_PLACEMENT_3D('',#54196,#39358,#39359);
#34589=AXIS2_PLACEMENT_3D('',#54269,#39360,#39361);
#34590=AXIS2_PLACEMENT_3D('',#54324,#39362,#39363);
#34591=AXIS2_PLACEMENT_3D('',#54361,#39364,#39365);
#34592=AXIS2_PLACEMENT_3D('',#54416,#39366,#39367);
#34593=AXIS2_PLACEMENT_3D('',#54453,#39368,#39369);
#34594=AXIS2_PLACEMENT_3D('',#54508,#39370,#39371);
#34595=AXIS2_PLACEMENT_3D('',#54563,#39372,#39373);
#34596=AXIS2_PLACEMENT_3D('',#54636,#39374,#39375);
#34597=AXIS2_PLACEMENT_3D('',#54673,#39376,#39377);
#34598=AXIS2_PLACEMENT_3D('',#54710,#39378,#39379);
#34599=AXIS2_PLACEMENT_3D('',#54711,#39380,#39381);
#34600=AXIS2_PLACEMENT_3D('',#54766,#39382,#39383);
#34601=AXIS2_PLACEMENT_3D('',#54803,#39384,#39385);
#34602=AXIS2_PLACEMENT_3D('',#54804,#39386,#39387);
#34603=AXIS2_PLACEMENT_3D('',#54806,#39388,#39389);
#34604=AXIS2_PLACEMENT_3D('',#54808,#39390,#39391);
#34605=AXIS2_PLACEMENT_3D('',#54809,#39392,#39393);
#34606=AXIS2_PLACEMENT_3D('',#54810,#39394,#39395);
#34607=AXIS2_PLACEMENT_3D('',#54812,#39396,#39397);
#34608=AXIS2_PLACEMENT_3D('',#54813,#39398,#39399);
#34609=AXIS2_PLACEMENT_3D('',#54814,#39400,#39401);
#34610=AXIS2_PLACEMENT_3D('',#54816,#39402,#39403);
#34611=AXIS2_PLACEMENT_3D('',#54818,#39405,#39406);
#34612=AXIS2_PLACEMENT_3D('',#54820,#39407,#39408);
#34613=AXIS2_PLACEMENT_3D('',#54821,#39409,#39410);
#34614=AXIS2_PLACEMENT_3D('',#54822,#39411,#39412);
#34615=AXIS2_PLACEMENT_3D('',#54824,#39413,#39414);
#34616=AXIS2_PLACEMENT_3D('',#54826,#39416,#39417);
#34617=AXIS2_PLACEMENT_3D('',#54828,#39418,#39419);
#34618=AXIS2_PLACEMENT_3D('',#54829,#39420,#39421);
#34619=AXIS2_PLACEMENT_3D('',#54830,#39422,#39423);
#34620=AXIS2_PLACEMENT_3D('',#54832,#39424,#39425);
#34621=AXIS2_PLACEMENT_3D('',#54834,#39427,#39428);
#34622=AXIS2_PLACEMENT_3D('',#54836,#39429,#39430);
#34623=AXIS2_PLACEMENT_3D('',#54837,#39431,#39432);
#34624=AXIS2_PLACEMENT_3D('',#54838,#39433,#39434);
#34625=AXIS2_PLACEMENT_3D('',#54840,#39435,#39436);
#34626=AXIS2_PLACEMENT_3D('',#54841,#39437,#39438);
#34627=AXIS2_PLACEMENT_3D('',#54842,#39439,#39440);
#34628=AXIS2_PLACEMENT_3D('',#54844,#39441,#39442);
#34629=AXIS2_PLACEMENT_3D('',#54845,#39443,#39444);
#34630=AXIS2_PLACEMENT_3D('',#54846,#39445,#39446);
#34631=AXIS2_PLACEMENT_3D('',#54848,#39447,#39448);
#34632=AXIS2_PLACEMENT_3D('',#54850,#39450,#39451);
#34633=AXIS2_PLACEMENT_3D('',#54852,#39452,#39453);
#34634=AXIS2_PLACEMENT_3D('',#54853,#39454,#39455);
#34635=AXIS2_PLACEMENT_3D('',#54854,#39456,#39457);
#34636=AXIS2_PLACEMENT_3D('',#54856,#39458,#39459);
#34637=AXIS2_PLACEMENT_3D('',#54857,#39460,#39461);
#34638=AXIS2_PLACEMENT_3D('',#54858,#39462,#39463);
#34639=AXIS2_PLACEMENT_3D('',#54860,#39464,#39465);
#34640=AXIS2_PLACEMENT_3D('',#54861,#39466,#39467);
#34641=AXIS2_PLACEMENT_3D('',#54862,#39468,#39469);
#34642=AXIS2_PLACEMENT_3D('',#54864,#39470,#39471);
#34643=AXIS2_PLACEMENT_3D('',#54866,#39473,#39474);
#34644=AXIS2_PLACEMENT_3D('',#54868,#39475,#39476);
#34645=AXIS2_PLACEMENT_3D('',#54869,#39477,#39478);
#34646=AXIS2_PLACEMENT_3D('',#54870,#39479,#39480);
#34647=AXIS2_PLACEMENT_3D('',#54872,#39481,#39482);
#34648=AXIS2_PLACEMENT_3D('',#54874,#39484,#39485);
#34649=AXIS2_PLACEMENT_3D('',#54876,#39486,#39487);
#34650=AXIS2_PLACEMENT_3D('',#54877,#39488,#39489);
#34651=AXIS2_PLACEMENT_3D('',#54878,#39490,#39491);
#34652=AXIS2_PLACEMENT_3D('',#54880,#39492,#39493);
#34653=AXIS2_PLACEMENT_3D('',#54882,#39495,#39496);
#34654=AXIS2_PLACEMENT_3D('',#54884,#39497,#39498);
#34655=AXIS2_PLACEMENT_3D('',#54885,#39499,#39500);
#34656=AXIS2_PLACEMENT_3D('',#54886,#39501,#39502);
#34657=AXIS2_PLACEMENT_3D('',#54888,#39503,#39504);
#34658=AXIS2_PLACEMENT_3D('',#54889,#39505,#39506);
#34659=AXIS2_PLACEMENT_3D('',#54890,#39507,#39508);
#34660=AXIS2_PLACEMENT_3D('',#54892,#39509,#39510);
#34661=AXIS2_PLACEMENT_3D('',#54893,#39511,#39512);
#34662=AXIS2_PLACEMENT_3D('',#54894,#39513,#39514);
#34663=AXIS2_PLACEMENT_3D('',#54896,#39515,#39516);
#34664=AXIS2_PLACEMENT_3D('',#54898,#39518,#39519);
#34665=AXIS2_PLACEMENT_3D('',#54900,#39520,#39521);
#34666=AXIS2_PLACEMENT_3D('',#54901,#39522,#39523);
#34667=AXIS2_PLACEMENT_3D('',#54902,#39524,#39525);
#34668=AXIS2_PLACEMENT_3D('',#54904,#39526,#39527);
#34669=AXIS2_PLACEMENT_3D('',#54906,#39529,#39530);
#34670=AXIS2_PLACEMENT_3D('',#54908,#39531,#39532);
#34671=AXIS2_PLACEMENT_3D('',#54909,#39533,#39534);
#34672=AXIS2_PLACEMENT_3D('',#54910,#39535,#39536);
#34673=AXIS2_PLACEMENT_3D('',#54912,#39537,#39538);
#34674=AXIS2_PLACEMENT_3D('',#54914,#39540,#39541);
#34675=AXIS2_PLACEMENT_3D('',#54916,#39542,#39543);
#34676=AXIS2_PLACEMENT_3D('',#54917,#39544,#39545);
#34677=AXIS2_PLACEMENT_3D('',#54918,#39546,#39547);
#34678=AXIS2_PLACEMENT_3D('',#54920,#39548,#39549);
#34679=AXIS2_PLACEMENT_3D('',#54921,#39550,#39551);
#34680=AXIS2_PLACEMENT_3D('',#54922,#39552,#39553);
#34681=AXIS2_PLACEMENT_3D('',#54924,#39554,#39555);
#34682=AXIS2_PLACEMENT_3D('',#54925,#39556,#39557);
#34683=AXIS2_PLACEMENT_3D('',#54926,#39558,#39559);
#34684=AXIS2_PLACEMENT_3D('',#54928,#39560,#39561);
#34685=AXIS2_PLACEMENT_3D('',#54930,#39563,#39564);
#34686=AXIS2_PLACEMENT_3D('',#54932,#39565,#39566);
#34687=AXIS2_PLACEMENT_3D('',#54933,#39567,#39568);
#34688=AXIS2_PLACEMENT_3D('',#54934,#39569,#39570);
#34689=AXIS2_PLACEMENT_3D('',#54936,#39571,#39572);
#34690=AXIS2_PLACEMENT_3D('',#54937,#39573,#39574);
#34691=AXIS2_PLACEMENT_3D('',#54938,#39575,#39576);
#34692=AXIS2_PLACEMENT_3D('',#54940,#39577,#39578);
#34693=AXIS2_PLACEMENT_3D('',#54941,#39579,#39580);
#34694=AXIS2_PLACEMENT_3D('',#54942,#39581,#39582);
#34695=AXIS2_PLACEMENT_3D('',#54944,#39583,#39584);
#34696=AXIS2_PLACEMENT_3D('',#54946,#39586,#39587);
#34697=AXIS2_PLACEMENT_3D('',#54948,#39588,#39589);
#34698=AXIS2_PLACEMENT_3D('',#54949,#39590,#39591);
#34699=AXIS2_PLACEMENT_3D('',#54950,#39592,#39593);
#34700=AXIS2_PLACEMENT_3D('',#54952,#39594,#39595);
#34701=AXIS2_PLACEMENT_3D('',#54954,#39597,#39598);
#34702=AXIS2_PLACEMENT_3D('',#54956,#39599,#39600);
#34703=AXIS2_PLACEMENT_3D('',#54957,#39601,#39602);
#34704=AXIS2_PLACEMENT_3D('',#54958,#39603,#39604);
#34705=AXIS2_PLACEMENT_3D('',#54960,#39605,#39606);
#34706=AXIS2_PLACEMENT_3D('',#54961,#39607,#39608);
#34707=AXIS2_PLACEMENT_3D('',#54962,#39609,#39610);
#34708=AXIS2_PLACEMENT_3D('',#54964,#39612,#39613);
#34709=AXIS2_PLACEMENT_3D('',#54968,#39615,#39616);
#34710=AXIS2_PLACEMENT_3D('',#54972,#39618,#39619);
#34711=AXIS2_PLACEMENT_3D('',#54976,#39621,#39622);
#34712=AXIS2_PLACEMENT_3D('',#54980,#39624,#39625);
#34713=AXIS2_PLACEMENT_3D('',#54983,#39627,#39628);
#34714=AXIS2_PLACEMENT_3D('',#54985,#39629,#39630);
#34715=AXIS2_PLACEMENT_3D('',#54989,#39632,#39633);
#34716=AXIS2_PLACEMENT_3D('',#54993,#39635,#39636);
#34717=AXIS2_PLACEMENT_3D('',#54997,#39638,#39639);
#34718=AXIS2_PLACEMENT_3D('',#55000,#39641,#39642);
#34719=AXIS2_PLACEMENT_3D('',#55001,#39643,#39644);
#34720=AXIS2_PLACEMENT_3D('',#55006,#39647,#39648);
#34721=AXIS2_PLACEMENT_3D('',#55007,#39649,#39650);
#34722=AXIS2_PLACEMENT_3D('',#55011,#39653,#39654);
#34723=AXIS2_PLACEMENT_3D('',#55015,#39657,#39658);
#34724=AXIS2_PLACEMENT_3D('',#55017,#39659,#39660);
#34725=AXIS2_PLACEMENT_3D('',#55019,#39662,#39663);
#34726=AXIS2_PLACEMENT_3D('',#55023,#39666,#39667);
#34727=AXIS2_PLACEMENT_3D('',#55024,#39668,#39669);
#34728=AXIS2_PLACEMENT_3D('',#55025,#39670,#39671);
#34729=AXIS2_PLACEMENT_3D('',#55031,#39675,#39676);
#34730=AXIS2_PLACEMENT_3D('',#55032,#39677,#39678);
#34731=AXIS2_PLACEMENT_3D('',#55033,#39679,#39680);
#34732=AXIS2_PLACEMENT_3D('',#55035,#39681,#39682);
#34733=AXIS2_PLACEMENT_3D('',#55037,#39684,#39685);
#34734=AXIS2_PLACEMENT_3D('',#55041,#39688,#39689);
#34735=AXIS2_PLACEMENT_3D('',#55043,#39690,#39691);
#34736=AXIS2_PLACEMENT_3D('',#55045,#39693,#39694);
#34737=AXIS2_PLACEMENT_3D('',#55049,#39697,#39698);
#34738=AXIS2_PLACEMENT_3D('',#55051,#39699,#39700);
#34739=AXIS2_PLACEMENT_3D('',#55053,#39702,#39703);
#34740=AXIS2_PLACEMENT_3D('',#55057,#39706,#39707);
#34741=AXIS2_PLACEMENT_3D('',#55059,#39708,#39709);
#34742=AXIS2_PLACEMENT_3D('',#55061,#39711,#39712);
#34743=AXIS2_PLACEMENT_3D('',#55065,#39715,#39716);
#34744=AXIS2_PLACEMENT_3D('',#55067,#39717,#39718);
#34745=AXIS2_PLACEMENT_3D('',#55069,#39720,#39721);
#34746=AXIS2_PLACEMENT_3D('',#55133,#39726,#39727);
#34747=AXIS2_PLACEMENT_3D('',#55410,#39737,#39738);
#34748=AXIS2_PLACEMENT_3D('',#55502,#39739,#39740);
#34749=AXIS2_PLACEMENT_3D('',#55503,#39741,#39742);
#34750=AXIS2_PLACEMENT_3D('',#55516,#39743,#39744);
#34751=AXIS2_PLACEMENT_3D('',#55738,#39746,#39747);
#34752=AXIS2_PLACEMENT_3D('',#55851,#39748,#39749);
#34753=AXIS2_PLACEMENT_3D('',#55933,#39750,#39751);
#34754=AXIS2_PLACEMENT_3D('',#56065,#39752,#39753);
#34755=AXIS2_PLACEMENT_3D('',#56066,#39754,#39755);
#34756=AXIS2_PLACEMENT_3D('',#56068,#39757,#39758);
#34757=AXIS2_PLACEMENT_3D('',#56156,#39759,#39760);
#34758=AXIS2_PLACEMENT_3D('',#56158,#39762,#39763);
#34759=AXIS2_PLACEMENT_3D('',#56160,#39764,#39765);
#34760=AXIS2_PLACEMENT_3D('',#56162,#39767,#39768);
#34761=AXIS2_PLACEMENT_3D('',#56164,#39769,#39770);
#34762=AXIS2_PLACEMENT_3D('',#56189,#39772,#39773);
#34763=AXIS2_PLACEMENT_3D('',#56191,#39774,#39775);
#34764=AXIS2_PLACEMENT_3D('',#56222,#39777,#39778);
#34765=AXIS2_PLACEMENT_3D('',#56224,#39779,#39780);
#34766=AXIS2_PLACEMENT_3D('',#56328,#39781,#39782);
#34767=AXIS2_PLACEMENT_3D('',#56330,#39784,#39785);
#34768=AXIS2_PLACEMENT_3D('',#56361,#39786,#39787);
#34769=AXIS2_PLACEMENT_3D('',#56363,#39789,#39790);
#34770=AXIS2_PLACEMENT_3D('',#56387,#39791,#39792);
#34771=AXIS2_PLACEMENT_3D('',#56425,#39793,#39794);
#34772=AXIS2_PLACEMENT_3D('',#56469,#39795,#39796);
#34773=AXIS2_PLACEMENT_3D('',#56523,#39797,#39798);
#34774=AXIS2_PLACEMENT_3D('',#56524,#39799,#39800);
#34775=AXIS2_PLACEMENT_3D('',#56580,#39801,#39802);
#34776=AXIS2_PLACEMENT_3D('',#56621,#39803,#39804);
#34777=AXIS2_PLACEMENT_3D('',#56690,#39805,#39806);
#34778=AXIS2_PLACEMENT_3D('',#56746,#39807,#39808);
#34779=AXIS2_PLACEMENT_3D('',#56875,#39809,#39810);
#34780=AXIS2_PLACEMENT_3D('',#56935,#39811,#39812);
#34781=AXIS2_PLACEMENT_3D('',#56995,#39813,#39814);
#34782=AXIS2_PLACEMENT_3D('',#56996,#39815,#39816);
#34783=AXIS2_PLACEMENT_3D('',#57034,#39817,#39818);
#34784=AXIS2_PLACEMENT_3D('',#57076,#39819,#39820);
#34785=AXIS2_PLACEMENT_3D('',#57090,#39821,#39822);
#34786=AXIS2_PLACEMENT_3D('',#57091,#39823,#39824);
#34787=AXIS2_PLACEMENT_3D('',#57147,#39825,#39826);
#34788=AXIS2_PLACEMENT_3D('',#57219,#39827,#39828);
#34789=AXIS2_PLACEMENT_3D('',#57324,#39829,#39830);
#34790=AXIS2_PLACEMENT_3D('',#57688,#39834,#39835);
#34791=AXIS2_PLACEMENT_3D('',#57703,#39837,#39838);
#34792=AXIS2_PLACEMENT_3D('',#57718,#39840,#39841);
#34793=AXIS2_PLACEMENT_3D('',#57753,#39844,#39845);
#34794=AXIS2_PLACEMENT_3D('',#57768,#39847,#39848);
#34795=AXIS2_PLACEMENT_3D('',#57783,#39850,#39851);
#34796=AXIS2_PLACEMENT_3D('',#57798,#39853,#39854);
#34797=AXIS2_PLACEMENT_3D('',#57833,#39857,#39858);
#34798=AXIS2_PLACEMENT_3D('',#57848,#39860,#39861);
#34799=AXIS2_PLACEMENT_3D('',#57861,#39862,#39863);
#34800=AXIS2_PLACEMENT_3D('',#57862,#39864,#39865);
#34801=AXIS2_PLACEMENT_3D('',#57865,#39866,#39867);
#34802=AXIS2_PLACEMENT_3D('',#57867,#39868,#39869);
#34803=AXIS2_PLACEMENT_3D('',#57869,#39870,#39871);
#34804=AXIS2_PLACEMENT_3D('',#57871,#39872,#39873);
#34805=AXIS2_PLACEMENT_3D('',#57873,#39874,#39875);
#34806=AXIS2_PLACEMENT_3D('',#57875,#39876,#39877);
#34807=AXIS2_PLACEMENT_3D('',#57876,#39878,#39879);
#34808=AXIS2_PLACEMENT_3D('',#57877,#39880,#39881);
#34809=AXIS2_PLACEMENT_3D('',#57880,#39882,#39883);
#34810=AXIS2_PLACEMENT_3D('',#57883,#39886,#39887);
#34811=AXIS2_PLACEMENT_3D('',#57886,#39889,#39890);
#34812=AXIS2_PLACEMENT_3D('',#57887,#39891,#39892);
#34813=AXIS2_PLACEMENT_3D('',#57890,#39894,#39895);
#34814=AXIS2_PLACEMENT_3D('',#57891,#39896,#39897);
#34815=AXIS2_PLACEMENT_3D('',#57893,#39898,#39899);
#34816=AXIS2_PLACEMENT_3D('',#57895,#39901,#39902);
#34817=AXIS2_PLACEMENT_3D('',#57897,#39903,#39904);
#34818=AXIS2_PLACEMENT_3D('',#57899,#39906,#39907);
#34819=AXIS2_PLACEMENT_3D('',#57901,#39908,#39909);
#34820=AXIS2_PLACEMENT_3D('',#57903,#39911,#39912);
#34821=AXIS2_PLACEMENT_3D('',#57904,#39913,#39914);
#34822=AXIS2_PLACEMENT_3D('',#57905,#39915,#39916);
#34823=AXIS2_PLACEMENT_3D('',#57906,#39917,#39918);
#34824=AXIS2_PLACEMENT_3D('',#57907,#39919,#39920);
#34825=AXIS2_PLACEMENT_3D('',#58116,#39921,#39922);
#34826=AXIS2_PLACEMENT_3D('',#59282,#39923,#39924);
#34827=AXIS2_PLACEMENT_3D('',#59383,#39926,#39927);
#34828=AXIS2_PLACEMENT_3D('',#59537,#39928,#39929);
#34829=AXIS2_PLACEMENT_3D('',#59635,#39931,#39932);
#34830=AXIS2_PLACEMENT_3D('',#60368,#39933,#39934);
#34831=AXIS2_PLACEMENT_3D('',#60608,#39935,#39936);
#34832=AXIS2_PLACEMENT_3D('',#61448,#39937,#39938);
#34833=AXIS2_PLACEMENT_3D('',#61948,#39940,#39941);
#34834=AXIS2_PLACEMENT_3D('',#62762,#39942,#39943);
#34835=AXIS2_PLACEMENT_3D('',#63138,#39945,#39946);
#34836=AXIS2_PLACEMENT_3D('',#63451,#39947,#39948);
#34837=AXIS2_PLACEMENT_3D('',#63453,#39949,#39950);
#34838=AXIS2_PLACEMENT_3D('',#63454,#39951,#39952);
#34839=AXIS2_PLACEMENT_3D('',#63492,#39953,#39954);
#34840=AXIS2_PLACEMENT_3D('',#63494,#39955,#39956);
#34841=AXIS2_PLACEMENT_3D('',#63495,#39957,#39958);
#34842=AXIS2_PLACEMENT_3D('',#63496,#39959,#39960);
#34843=AXIS2_PLACEMENT_3D('',#63608,#39963,#39964);
#34844=AXIS2_PLACEMENT_3D('',#63863,#39965,#39966);
#34845=AXIS2_PLACEMENT_3D('',#63968,#39968,#39969);
#34846=AXIS2_PLACEMENT_3D('',#64088,#39970,#39971);
#34847=AXIS2_PLACEMENT_3D('',#64205,#39973,#39974);
#34848=AXIS2_PLACEMENT_3D('',#64421,#39975,#39976);
#34849=AXIS2_PLACEMENT_3D('',#64616,#39978,#39979);
#34850=AXIS2_PLACEMENT_3D('',#64880,#39980,#39981);
#34851=AXIS2_PLACEMENT_3D('',#64973,#39983,#39984);
#34852=AXIS2_PLACEMENT_3D('',#64974,#39985,#39986);
#34853=AXIS2_PLACEMENT_3D('',#65030,#39987,#39988);
#34854=AXIS2_PLACEMENT_3D('',#65031,#39989,#39990);
#34855=AXIS2_PLACEMENT_3D('',#65100,#39992,#39993);
#34856=AXIS2_PLACEMENT_3D('',#65171,#39994,#39995);
#34857=AXIS2_PLACEMENT_3D('',#65185,#39997,#39998);
#34858=AXIS2_PLACEMENT_3D('',#65219,#40000,#40001);
#34859=AXIS2_PLACEMENT_3D('',#65253,#40003,#40004);
#34860=AXIS2_PLACEMENT_3D('',#65495,#40006,#40007);
#34861=AXIS2_PLACEMENT_3D('',#65582,#40008,#40009);
#34862=AXIS2_PLACEMENT_3D('',#65674,#40012,#40013);
#34863=AXIS2_PLACEMENT_3D('',#65816,#40015,#40016);
#34864=AXIS2_PLACEMENT_3D('',#65982,#40017,#40018);
#34865=AXIS2_PLACEMENT_3D('',#66081,#40020,#40021);
#34866=AXIS2_PLACEMENT_3D('',#66341,#40023,#40024);
#34867=AXIS2_PLACEMENT_3D('',#66536,#40025,#40026);
#34868=AXIS2_PLACEMENT_3D('',#66629,#40028,#40029);
#34869=AXIS2_PLACEMENT_3D('',#66630,#40030,#40031);
#34870=AXIS2_PLACEMENT_3D('',#66686,#40032,#40033);
#34871=AXIS2_PLACEMENT_3D('',#66687,#40034,#40035);
#34872=AXIS2_PLACEMENT_3D('',#67044,#40037,#40038);
#34873=AXIS2_PLACEMENT_3D('',#67046,#40039,#40040);
#34874=AXIS2_PLACEMENT_3D('',#67144,#40041,#40042);
#34875=AXIS2_PLACEMENT_3D('',#67158,#40043,#40044);
#34876=AXIS2_PLACEMENT_3D('',#67264,#40047,#40048);
#34877=AXIS2_PLACEMENT_3D('',#67381,#40049,#40050);
#34878=AXIS2_PLACEMENT_3D('',#67516,#40052,#40053);
#34879=AXIS2_PLACEMENT_3D('',#67774,#40054,#40055);
#34880=AXIS2_PLACEMENT_3D('',#67879,#40057,#40058);
#34881=AXIS2_PLACEMENT_3D('',#67880,#40059,#40060);
#34882=AXIS2_PLACEMENT_3D('',#67918,#40061,#40062);
#34883=AXIS2_PLACEMENT_3D('',#67919,#40063,#40064);
#34884=AXIS2_PLACEMENT_3D('',#67920,#40065,#40066);
#34885=AXIS2_PLACEMENT_3D('',#68119,#40069,#40070);
#34886=AXIS2_PLACEMENT_3D('',#68121,#40071,#40072);
#34887=AXIS2_PLACEMENT_3D('',#68123,#40074,#40075);
#34888=AXIS2_PLACEMENT_3D('',#68126,#40077,#40078);
#34889=AXIS2_PLACEMENT_3D('',#68127,#40079,#40080);
#34890=AXIS2_PLACEMENT_3D('',#68184,#40082,#40083);
#34891=AXIS2_PLACEMENT_3D('',#68255,#40084,#40085);
#34892=AXIS2_PLACEMENT_3D('',#68324,#40087,#40088);
#34893=AXIS2_PLACEMENT_3D('',#68325,#40089,#40090);
#34894=AXIS2_PLACEMENT_3D('',#68381,#40091,#40092);
#34895=AXIS2_PLACEMENT_3D('',#68382,#40093,#40094);
#34896=AXIS2_PLACEMENT_3D('',#68796,#40096,#40097);
#34897=AXIS2_PLACEMENT_3D('',#68810,#40098,#40099);
#34898=AXIS2_PLACEMENT_3D('',#68884,#40100,#40101);
#34899=AXIS2_PLACEMENT_3D('',#68886,#40102,#40103);
#34900=AXIS2_PLACEMENT_3D('',#69007,#40106,#40107);
#34901=AXIS2_PLACEMENT_3D('',#69069,#40108,#40109);
#34902=AXIS2_PLACEMENT_3D('',#69181,#40111,#40112);
#34903=AXIS2_PLACEMENT_3D('',#69246,#40113,#40114);
#34904=AXIS2_PLACEMENT_3D('',#69321,#40116,#40117);
#34905=AXIS2_PLACEMENT_3D('',#69386,#40118,#40119);
#34906=AXIS2_PLACEMENT_3D('',#69461,#40121,#40122);
#34907=AXIS2_PLACEMENT_3D('',#69523,#40123,#40124);
#34908=AXIS2_PLACEMENT_3D('',#69653,#40126,#40127);
#34909=AXIS2_PLACEMENT_3D('',#69748,#40128,#40129);
#34910=AXIS2_PLACEMENT_3D('',#69904,#40131,#40132);
#34911=AXIS2_PLACEMENT_3D('',#70011,#40133,#40134);
#34912=AXIS2_PLACEMENT_3D('',#70315,#40136,#40137);
#34913=AXIS2_PLACEMENT_3D('',#70536,#40138,#40139);
#34914=AXIS2_PLACEMENT_3D('',#70710,#40141,#40142);
#34915=AXIS2_PLACEMENT_3D('',#70711,#40143,#40144);
#34916=AXIS2_PLACEMENT_3D('',#70767,#40145,#40146);
#34917=AXIS2_PLACEMENT_3D('',#70768,#40147,#40148);
#34918=AXIS2_PLACEMENT_3D('',#70963,#40150,#40151);
#34919=AXIS2_PLACEMENT_3D('',#71166,#40152,#40153);
#34920=AXIS2_PLACEMENT_3D('',#71740,#40155,#40156);
#34921=AXIS2_PLACEMENT_3D('',#71741,#40157,#40158);
#34922=AXIS2_PLACEMENT_3D('',#72777,#40163,#40164);
#34923=AXIS2_PLACEMENT_3D('',#72779,#40165,#40166);
#34924=AXIS2_PLACEMENT_3D('',#72780,#40167,#40168);
#34925=AXIS2_PLACEMENT_3D('',#72860,#40171,#40172);
#34926=AXIS2_PLACEMENT_3D('',#72862,#40173,#40174);
#34927=AXIS2_PLACEMENT_3D('',#72916,#40177,#40178);
#34928=AXIS2_PLACEMENT_3D('',#72918,#40179,#40180);
#34929=AXIS2_PLACEMENT_3D('',#72919,#40181,#40182);
#34930=AXIS2_PLACEMENT_3D('',#72920,#40183,#40184);
#34931=AXIS2_PLACEMENT_3D('',#72922,#40186,#40187);
#34932=AXIS2_PLACEMENT_3D('',#72924,#40188,#40189);
#34933=AXIS2_PLACEMENT_3D('',#72925,#40190,#40191);
#34934=AXIS2_PLACEMENT_3D('',#72926,#40192,#40193);
#34935=AXIS2_PLACEMENT_3D('',#72983,#40195,#40196);
#34936=AXIS2_PLACEMENT_3D('',#72985,#40197,#40198);
#34937=AXIS2_PLACEMENT_3D('',#73006,#40201,#40202);
#34938=AXIS2_PLACEMENT_3D('',#73008,#40203,#40204);
#34939=AXIS2_PLACEMENT_3D('',#73010,#40206,#40207);
#34940=AXIS2_PLACEMENT_3D('',#73067,#40209,#40210);
#34941=AXIS2_PLACEMENT_3D('',#73142,#40212,#40213);
#34942=AXIS2_PLACEMENT_3D('',#73214,#40215,#40216);
#34943=AXIS2_PLACEMENT_3D('',#73216,#40217,#40218);
#34944=AXIS2_PLACEMENT_3D('',#73218,#40220,#40221);
#34945=AXIS2_PLACEMENT_3D('',#73275,#40223,#40224);
#34946=AXIS2_PLACEMENT_3D('',#73350,#40226,#40227);
#34947=AXIS2_PLACEMENT_3D('',#73425,#40229,#40230);
#34948=AXIS2_PLACEMENT_3D('',#73618,#40232,#40233);
#34949=AXIS2_PLACEMENT_3D('',#73626,#40234,#40235);
#34950=AXIS2_PLACEMENT_3D('',#73732,#40238,#40239);
#34951=AXIS2_PLACEMENT_3D('',#73834,#40241,#40242);
#34952=AXIS2_PLACEMENT_3D('',#73909,#40244,#40245);
#34953=AXIS2_PLACEMENT_3D('',#74020,#40247,#40248);
#34954=AXIS2_PLACEMENT_3D('',#74122,#40250,#40251);
#34955=AXIS2_PLACEMENT_3D('',#74142,#40253,#40254);
#34956=AXIS2_PLACEMENT_3D('',#74144,#40255,#40256);
#34957=AXIS2_PLACEMENT_3D('',#74146,#40258,#40259);
#34958=AXIS2_PLACEMENT_3D('',#74203,#40261,#40262);
#34959=AXIS2_PLACEMENT_3D('',#74278,#40264,#40265);
#34960=AXIS2_PLACEMENT_3D('',#74298,#40267,#40268);
#34961=AXIS2_PLACEMENT_3D('',#74300,#40270,#40271);
#34962=AXIS2_PLACEMENT_3D('',#74301,#40272,#40273);
#34963=AXIS2_PLACEMENT_3D('',#74302,#40274,#40275);
#34964=AXIS2_PLACEMENT_3D('',#74311,#40277,#40278);
#34965=AXIS2_PLACEMENT_3D('',#74312,#40279,#40280);
#34966=AXIS2_PLACEMENT_3D('',#74317,#40283,#40284);
#34967=AXIS2_PLACEMENT_3D('',#74318,#40285,#40286);
#34968=AXIS2_PLACEMENT_3D('',#74334,#40289,#40290);
#34969=AXIS2_PLACEMENT_3D('',#74335,#40291,#40292);
#34970=AXIS2_PLACEMENT_3D('',#74343,#40293,#40294);
#34971=AXIS2_PLACEMENT_3D('',#74345,#40296,#40297);
#34972=AXIS2_PLACEMENT_3D('',#74351,#40301,#40302);
#34973=AXIS2_PLACEMENT_3D('',#74354,#40304,#40305);
#34974=AXIS2_PLACEMENT_3D('',#74367,#40306,#40307);
#34975=AXIS2_PLACEMENT_3D('',#74368,#40308,#40309);
#34976=AXIS2_PLACEMENT_3D('',#74371,#40310,#40311);
#34977=AXIS2_PLACEMENT_3D('',#74375,#40313,#40314);
#34978=AXIS2_PLACEMENT_3D('',#74377,#40315,#40316);
#34979=AXIS2_PLACEMENT_3D('',#74379,#40318,#40319);
#34980=AXIS2_PLACEMENT_3D('',#74382,#40320,#40321);
#34981=AXIS2_PLACEMENT_3D('',#74386,#40323,#40324);
#34982=AXIS2_PLACEMENT_3D('',#74388,#40326,#40327);
#34983=AXIS2_PLACEMENT_3D('',#74399,#40333,#40334);
#34984=AXIS2_PLACEMENT_3D('',#74412,#40337,#40338);
#34985=AXIS2_PLACEMENT_3D('',#74424,#40341,#40342);
#34986=AXIS2_PLACEMENT_3D('',#74436,#40345,#40346);
#34987=AXIS2_PLACEMENT_3D('',#74447,#40349,#40350);
#34988=AXIS2_PLACEMENT_3D('',#74452,#40352,#40353);
#34989=AXIS2_PLACEMENT_3D('',#74454,#40354,#40355);
#34990=AXIS2_PLACEMENT_3D('',#74456,#40356,#40357);
#34991=AXIS2_PLACEMENT_3D('',#74459,#40359,#40360);
#34992=AXIS2_PLACEMENT_3D('',#74462,#40361,#40362);
#34993=AXIS2_PLACEMENT_3D('',#74464,#40363,#40364);
#34994=AXIS2_PLACEMENT_3D('',#74470,#40367,#40368);
#34995=AXIS2_PLACEMENT_3D('',#74480,#40373,#40374);
#34996=AXIS2_PLACEMENT_3D('',#74482,#40375,#40376);
#34997=AXIS2_PLACEMENT_3D('',#74484,#40378,#40379);
#34998=AXIS2_PLACEMENT_3D('',#74487,#40380,#40381);
#34999=AXIS2_PLACEMENT_3D('',#74489,#40382,#40383);
#35000=AXIS2_PLACEMENT_3D('',#74495,#40386,#40387);
#35001=AXIS2_PLACEMENT_3D('',#74498,#40389,#40390);
#35002=AXIS2_PLACEMENT_3D('',#74503,#40392,#40393);
#35003=AXIS2_PLACEMENT_3D('',#74505,#40394,#40395);
#35004=AXIS2_PLACEMENT_3D('',#74507,#40396,#40397);
#35005=AXIS2_PLACEMENT_3D('',#74509,#40398,#40399);
#35006=AXIS2_PLACEMENT_3D('',#74511,#40400,#40401);
#35007=AXIS2_PLACEMENT_3D('',#74513,#40402,#40403);
#35008=AXIS2_PLACEMENT_3D('',#74515,#40405,#40406);
#35009=AXIS2_PLACEMENT_3D('',#74518,#40407,#40408);
#35010=AXIS2_PLACEMENT_3D('',#74520,#40409,#40410);
#35011=AXIS2_PLACEMENT_3D('',#74524,#40412,#40413);
#35012=AXIS2_PLACEMENT_3D('',#74529,#40416,#40417);
#35013=AXIS2_PLACEMENT_3D('',#74530,#40418,#40419);
#35014=AXIS2_PLACEMENT_3D('',#74532,#40420,#40421);
#35015=AXIS2_PLACEMENT_3D('',#74534,#40423,#40424);
#35016=AXIS2_PLACEMENT_3D('',#74536,#40425,#40426);
#35017=AXIS2_PLACEMENT_3D('',#74538,#40428,#40429);
#35018=AXIS2_PLACEMENT_3D('',#74542,#40431,#40432);
#35019=AXIS2_PLACEMENT_3D('',#74551,#40433,#40434);
#35020=AXIS2_PLACEMENT_3D('',#74555,#40437,#40438);
#35021=AXIS2_PLACEMENT_3D('',#74559,#40441,#40442);
#35022=AXIS2_PLACEMENT_3D('',#74564,#40444,#40445);
#35023=AXIS2_PLACEMENT_3D('',#74568,#40447,#40448);
#35024=AXIS2_PLACEMENT_3D('',#74572,#40450,#40451);
#35025=AXIS2_PLACEMENT_3D('',#74576,#40453,#40454);
#35026=AXIS2_PLACEMENT_3D('',#74580,#40456,#40457);
#35027=AXIS2_PLACEMENT_3D('',#74584,#40459,#40460);
#35028=AXIS2_PLACEMENT_3D('',#74588,#40462,#40463);
#35029=AXIS2_PLACEMENT_3D('',#74593,#40466,#40467);
#35030=AXIS2_PLACEMENT_3D('',#74596,#40469,#40470);
#35031=AXIS2_PLACEMENT_3D('',#74597,#40471,#40472);
#35032=AXIS2_PLACEMENT_3D('',#74618,#40476,#40477);
#35033=AXIS2_PLACEMENT_3D('',#74622,#40480,#40481);
#35034=AXIS2_PLACEMENT_3D('',#74626,#40483,#40484);
#35035=AXIS2_PLACEMENT_3D('',#74641,#40486,#40487);
#35036=AXIS2_PLACEMENT_3D('',#74655,#40489,#40490);
#35037=AXIS2_PLACEMENT_3D('',#74656,#40491,#40492);
#35038=AXIS2_PLACEMENT_3D('',#74677,#40496,#40497);
#35039=AXIS2_PLACEMENT_3D('',#74681,#40500,#40501);
#35040=AXIS2_PLACEMENT_3D('',#74686,#40503,#40504);
#35041=AXIS2_PLACEMENT_3D('',#74690,#40506,#40507);
#35042=AXIS2_PLACEMENT_3D('',#74694,#40509,#40510);
#35043=AXIS2_PLACEMENT_3D('',#74698,#40512,#40513);
#35044=AXIS2_PLACEMENT_3D('',#74702,#40515,#40516);
#35045=AXIS2_PLACEMENT_3D('',#74706,#40518,#40519);
#35046=AXIS2_PLACEMENT_3D('',#74709,#40521,#40522);
#35047=AXIS2_PLACEMENT_3D('',#74713,#40524,#40525);
#35048=AXIS2_PLACEMENT_3D('',#74716,#40527,#40528);
#35049=AXIS2_PLACEMENT_3D('',#74717,#40529,#40530);
#35050=AXIS2_PLACEMENT_3D('',#74738,#40534,#40535);
#35051=AXIS2_PLACEMENT_3D('',#74742,#40538,#40539);
#35052=AXIS2_PLACEMENT_3D('',#74746,#40541,#40542);
#35053=AXIS2_PLACEMENT_3D('',#74761,#40544,#40545);
#35054=AXIS2_PLACEMENT_3D('',#74775,#40547,#40548);
#35055=AXIS2_PLACEMENT_3D('',#74776,#40549,#40550);
#35056=AXIS2_PLACEMENT_3D('',#74797,#40554,#40555);
#35057=AXIS2_PLACEMENT_3D('',#74799,#40557,#40558);
#35058=AXIS2_PLACEMENT_3D('',#74805,#40561,#40562);
#35059=AXIS2_PLACEMENT_3D('',#74807,#40563,#40564);
#35060=AXIS2_PLACEMENT_3D('',#74808,#40565,#40566);
#35061=AXIS2_PLACEMENT_3D('',#74809,#40567,#40568);
#35062=AXIS2_PLACEMENT_3D('',#74815,#40572,#40573);
#35063=AXIS2_PLACEMENT_3D('',#74819,#40575,#40576);
#35064=AXIS2_PLACEMENT_3D('',#74821,#40577,#40578);
#35065=AXIS2_PLACEMENT_3D('',#74823,#40579,#40580);
#35066=AXIS2_PLACEMENT_3D('',#74824,#40581,#40582);
#35067=AXIS2_PLACEMENT_3D('',#74825,#40583,#40584);
#35068=AXIS2_PLACEMENT_3D('',#74828,#40586,#40587);
#35069=AXIS2_PLACEMENT_3D('',#74829,#40588,#40589);
#35070=AXIS2_PLACEMENT_3D('',#74832,#40590,#40591);
#35071=AXIS2_PLACEMENT_3D('',#74834,#40592,#40593);
#35072=AXIS2_PLACEMENT_3D('',#74836,#40594,#40595);
#35073=AXIS2_PLACEMENT_3D('',#74837,#40596,#40597);
#35074=AXIS2_PLACEMENT_3D('',#74839,#40599,#40600);
#35075=AXIS2_PLACEMENT_3D('',#74843,#40603,#40604);
#35076=AXIS2_PLACEMENT_3D('',#74851,#40609,#40610);
#35077=AXIS2_PLACEMENT_3D('',#74857,#40614,#40615);
#35078=AXIS2_PLACEMENT_3D('',#74860,#40617,#40618);
#35079=AXIS2_PLACEMENT_3D('',#74861,#40619,#40620);
#35080=AXIS2_PLACEMENT_3D('',#74867,#40624,#40625);
#35081=AXIS2_PLACEMENT_3D('',#74871,#40628,#40629);
#35082=AXIS2_PLACEMENT_3D('',#74875,#40631,#40632);
#35083=AXIS2_PLACEMENT_3D('',#74876,#40633,#40634);
#35084=AXIS2_PLACEMENT_3D('',#74877,#40635,#40636);
#35085=AXIS2_PLACEMENT_3D('',#74878,#40637,#40638);
#35086=AXIS2_PLACEMENT_3D('',#74879,#40639,#40640);
#35087=AXIS2_PLACEMENT_3D('',#74882,#40642,#40643);
#35088=AXIS2_PLACEMENT_3D('',#74883,#40644,#40645);
#35089=AXIS2_PLACEMENT_3D('',#74884,#40646,#40647);
#35090=AXIS2_PLACEMENT_3D('',#74886,#40649,#40650);
#35091=AXIS2_PLACEMENT_3D('',#74888,#40652,#40653);
#35092=AXIS2_PLACEMENT_3D('',#74889,#40654,#40655);
#35093=AXIS2_PLACEMENT_3D('',#74893,#40657,#40658);
#35094=AXIS2_PLACEMENT_3D('',#74895,#40660,#40661);
#35095=AXIS2_PLACEMENT_3D('',#74899,#40664,#40665);
#35096=AXIS2_PLACEMENT_3D('',#74903,#40667,#40668);
#35097=AXIS2_PLACEMENT_3D('',#74904,#40669,#40670);
#35098=AXIS2_PLACEMENT_3D('',#74905,#40671,#40672);
#35099=AXIS2_PLACEMENT_3D('',#74911,#40676,#40677);
#35100=AXIS2_PLACEMENT_3D('',#74915,#40680,#40681);
#35101=AXIS2_PLACEMENT_3D('',#74917,#40682,#40683);
#35102=AXIS2_PLACEMENT_3D('',#74919,#40685,#40686);
#35103=AXIS2_PLACEMENT_3D('',#74921,#40687,#40688);
#35104=AXIS2_PLACEMENT_3D('',#74924,#40690,#40691);
#35105=AXIS2_PLACEMENT_3D('',#74926,#40692,#40693);
#35106=AXIS2_PLACEMENT_3D('',#74928,#40694,#40695);
#35107=AXIS2_PLACEMENT_3D('',#74929,#40696,#40697);
#35108=AXIS2_PLACEMENT_3D('',#74930,#40698,#40699);
#35109=AXIS2_PLACEMENT_3D('',#74933,#40701,#40702);
#35110=AXIS2_PLACEMENT_3D('',#74934,#40703,#40704);
#35111=AXIS2_PLACEMENT_3D('',#74938,#40707,#40708);
#35112=AXIS2_PLACEMENT_3D('',#74940,#40709,#40710);
#35113=AXIS2_PLACEMENT_3D('',#74942,#40712,#40713);
#35114=AXIS2_PLACEMENT_3D('',#74944,#40714,#40715);
#35115=AXIS2_PLACEMENT_3D('',#74946,#40717,#40718);
#35116=AXIS2_PLACEMENT_3D('',#74948,#40719,#40720);
#35117=AXIS2_PLACEMENT_3D('',#74950,#40722,#40723);
#35118=AXIS2_PLACEMENT_3D('',#74952,#40724,#40725);
#35119=AXIS2_PLACEMENT_3D('',#74954,#40727,#40728);
#35120=AXIS2_PLACEMENT_3D('',#74957,#40730,#40731);
#35121=AXIS2_PLACEMENT_3D('',#74958,#40732,#40733);
#35122=AXIS2_PLACEMENT_3D('',#74960,#40734,#40735);
#35123=AXIS2_PLACEMENT_3D('',#74962,#40737,#40738);
#35124=AXIS2_PLACEMENT_3D('',#74964,#40740,#40741);
#35125=AXIS2_PLACEMENT_3D('',#74968,#40743,#40744);
#35126=AXIS2_PLACEMENT_3D('',#74970,#40746,#40747);
#35127=AXIS2_PLACEMENT_3D('',#74974,#40750,#40751);
#35128=AXIS2_PLACEMENT_3D('',#74980,#40755,#40756);
#35129=AXIS2_PLACEMENT_3D('',#74984,#40758,#40759);
#35130=AXIS2_PLACEMENT_3D('',#74985,#40760,#40761);
#35131=AXIS2_PLACEMENT_3D('',#74986,#40762,#40763);
#35132=AXIS2_PLACEMENT_3D('',#74990,#40766,#40767);
#35133=AXIS2_PLACEMENT_3D('',#74992,#40768,#40769);
#35134=AXIS2_PLACEMENT_3D('',#74994,#40771,#40772);
#35135=AXIS2_PLACEMENT_3D('',#74997,#40773,#40774);
#35136=AXIS2_PLACEMENT_3D('',#74999,#40775,#40776);
#35137=AXIS2_PLACEMENT_3D('',#75000,#40777,#40778);
#35138=AXIS2_PLACEMENT_3D('',#75001,#40779,#40780);
#35139=AXIS2_PLACEMENT_3D('',#75005,#40782,#40783);
#35140=AXIS2_PLACEMENT_3D('',#75006,#40784,#40785);
#35141=AXIS2_PLACEMENT_3D('',#75007,#40786,#40787);
#35142=AXIS2_PLACEMENT_3D('',#75008,#40788,#40789);
#35143=AXIS2_PLACEMENT_3D('',#75010,#40791,#40792);
#35144=AXIS2_PLACEMENT_3D('',#75014,#40795,#40796);
#35145=AXIS2_PLACEMENT_3D('',#75028,#40804,#40805);
#35146=AXIS2_PLACEMENT_3D('',#75030,#40806,#40807);
#35147=AXIS2_PLACEMENT_3D('',#75032,#40809,#40810);
#35148=AXIS2_PLACEMENT_3D('',#75044,#40817,#40818);
#35149=AXIS2_PLACEMENT_3D('',#75049,#40822,#40823);
#35150=AXIS2_PLACEMENT_3D('',#75050,#40824,#40825);
#35151=AXIS2_PLACEMENT_3D('',#75052,#40827,#40828);
#35152=AXIS2_PLACEMENT_3D('',#75056,#40831,#40832);
#35153=AXIS2_PLACEMENT_3D('',#75058,#40834,#40835);
#35154=AXIS2_PLACEMENT_3D('',#75062,#40838,#40839);
#35155=AXIS2_PLACEMENT_3D('',#75076,#40847,#40848);
#35156=AXIS2_PLACEMENT_3D('',#75078,#40849,#40850);
#35157=AXIS2_PLACEMENT_3D('',#75080,#40852,#40853);
#35158=AXIS2_PLACEMENT_3D('',#75092,#40860,#40861);
#35159=AXIS2_PLACEMENT_3D('',#75097,#40864,#40865);
#35160=AXIS2_PLACEMENT_3D('',#75098,#40866,#40867);
#35161=AXIS2_PLACEMENT_3D('',#75109,#40868,#40869);
#35162=AXIS2_PLACEMENT_3D('',#75120,#40870,#40871);
#35163=AXIS2_PLACEMENT_3D('',#75129,#40873,#40874);
#35164=AXIS2_PLACEMENT_3D('',#75138,#40875,#40876);
#35165=AXIS2_PLACEMENT_3D('',#75153,#40878,#40879);
#35166=AXIS2_PLACEMENT_3D('',#75154,#40880,#40881);
#35167=AXIS2_PLACEMENT_3D('',#75169,#40884,#40885);
#35168=AXIS2_PLACEMENT_3D('',#75170,#40886,#40887);
#35169=AXIS2_PLACEMENT_3D('',#75171,#40888,#40889);
#35170=AXIS2_PLACEMENT_3D('',#75179,#40890,#40891);
#35171=AXIS2_PLACEMENT_3D('',#75180,#40892,#40893);
#35172=AXIS2_PLACEMENT_3D('',#75181,#40894,#40895);
#35173=AXIS2_PLACEMENT_3D('',#75182,#40896,#40897);
#35174=AXIS2_PLACEMENT_3D('',#75183,#40898,#40899);
#35175=AXIS2_PLACEMENT_3D('',#75186,#40901,#40902);
#35176=AXIS2_PLACEMENT_3D('',#75187,#40903,#40904);
#35177=AXIS2_PLACEMENT_3D('',#75188,#40905,#40906);
#35178=AXIS2_PLACEMENT_3D('',#75189,#40907,#40908);
#35179=AXIS2_PLACEMENT_3D('',#75190,#40909,#40910);
#35180=AXIS2_PLACEMENT_3D('',#75192,#40911,#40912);
#35181=AXIS2_PLACEMENT_3D('',#75193,#40913,#40914);
#35182=AXIS2_PLACEMENT_3D('',#75194,#40915,#40916);
#35183=AXIS2_PLACEMENT_3D('',#75197,#40917,#40918);
#35184=AXIS2_PLACEMENT_3D('',#75199,#40919,#40920);
#35185=AXIS2_PLACEMENT_3D('',#75201,#40921,#40922);
#35186=AXIS2_PLACEMENT_3D('',#75203,#40923,#40924);
#35187=AXIS2_PLACEMENT_3D('',#75205,#40925,#40926);
#35188=AXIS2_PLACEMENT_3D('',#75209,#40928,#40929);
#35189=AXIS2_PLACEMENT_3D('',#75211,#40930,#40931);
#35190=AXIS2_PLACEMENT_3D('',#75214,#40933,#40934);
#35191=AXIS2_PLACEMENT_3D('',#75216,#40935,#40936);
#35192=AXIS2_PLACEMENT_3D('',#75217,#40937,#40938);
#35193=AXIS2_PLACEMENT_3D('',#75218,#40939,#40940);
#35194=AXIS2_PLACEMENT_3D('',#75219,#40941,#40942);
#35195=AXIS2_PLACEMENT_3D('',#75222,#40944,#40945);
#35196=AXIS2_PLACEMENT_3D('',#75223,#40946,#40947);
#35197=AXIS2_PLACEMENT_3D('',#75224,#40948,#40949);
#35198=AXIS2_PLACEMENT_3D('',#75226,#40950,#40951);
#35199=AXIS2_PLACEMENT_3D('',#75227,#40952,#40953);
#35200=AXIS2_PLACEMENT_3D('',#75228,#40954,#40955);
#35201=AXIS2_PLACEMENT_3D('',#75241,#40957,#40958);
#35202=AXIS2_PLACEMENT_3D('',#75243,#40959,#40960);
#35203=AXIS2_PLACEMENT_3D('',#75254,#40961,#40962);
#35204=AXIS2_PLACEMENT_3D('',#75255,#40963,#40964);
#35205=AXIS2_PLACEMENT_3D('',#75259,#40966,#40967);
#35206=AXIS2_PLACEMENT_3D('',#75260,#40968,#40969);
#35207=AXIS2_PLACEMENT_3D('',#75261,#40970,#40971);
#35208=AXIS2_PLACEMENT_3D('',#75264,#40972,#40973);
#35209=AXIS2_PLACEMENT_3D('',#75268,#40975,#40976);
#35210=AXIS2_PLACEMENT_3D('',#75270,#40978,#40979);
#35211=AXIS2_PLACEMENT_3D('',#75275,#40981,#40982);
#35212=AXIS2_PLACEMENT_3D('',#75278,#40984,#40985);
#35213=AXIS2_PLACEMENT_3D('',#75279,#40986,#40987);
#35214=AXIS2_PLACEMENT_3D('',#75284,#40989,#40990);
#35215=AXIS2_PLACEMENT_3D('',#75287,#40992,#40993);
#35216=AXIS2_PLACEMENT_3D('',#75288,#40994,#40995);
#35217=AXIS2_PLACEMENT_3D('',#75291,#40996,#40997);
#35218=AXIS2_PLACEMENT_3D('',#75295,#40999,#41000);
#35219=AXIS2_PLACEMENT_3D('',#75297,#41002,#41003);
#35220=AXIS2_PLACEMENT_3D('',#75301,#41005,#41006);
#35221=AXIS2_PLACEMENT_3D('',#75302,#41007,#41008);
#35222=AXIS2_PLACEMENT_3D('',#75303,#41009,#41010);
#35223=AXIS2_PLACEMENT_3D('',#75306,#41013,#41014);
#35224=AXIS2_PLACEMENT_3D('',#75307,#41015,#41016);
#35225=AXIS2_PLACEMENT_3D('',#75308,#41017,#41018);
#35226=AXIS2_PLACEMENT_3D('',#75309,#41019,#41020);
#35227=AXIS2_PLACEMENT_3D('',#75324,#41022,#41023);
#35228=AXIS2_PLACEMENT_3D('',#75327,#41025,#41026);
#35229=AXIS2_PLACEMENT_3D('',#75328,#41027,#41028);
#35230=AXIS2_PLACEMENT_3D('',#75331,#41029,#41030);
#35231=AXIS2_PLACEMENT_3D('',#75333,#41031,#41032);
#35232=AXIS2_PLACEMENT_3D('',#75367,#41035,#41036);
#35233=AXIS2_PLACEMENT_3D('',#75368,#41037,#41038);
#35234=AXIS2_PLACEMENT_3D('',#75372,#41040,#41041);
#35235=AXIS2_PLACEMENT_3D('',#75376,#41043,#41044);
#35236=AXIS2_PLACEMENT_3D('',#75380,#41046,#41047);
#35237=AXIS2_PLACEMENT_3D('',#75383,#41049,#41050);
#35238=AXIS2_PLACEMENT_3D('',#75385,#41051,#41052);
#35239=AXIS2_PLACEMENT_3D('',#75389,#41054,#41055);
#35240=AXIS2_PLACEMENT_3D('',#75393,#41057,#41058);
#35241=AXIS2_PLACEMENT_3D('',#75398,#41061,#41062);
#35242=AXIS2_PLACEMENT_3D('',#75400,#41063,#41064);
#35243=AXIS2_PLACEMENT_3D('',#75439,#41065,#41066);
#35244=AXIS2_PLACEMENT_3D('',#75442,#41068,#41069);
#35245=AXIS2_PLACEMENT_3D('',#75443,#41070,#41071);
#35246=AXIS2_PLACEMENT_3D('',#75447,#41073,#41074);
#35247=AXIS2_PLACEMENT_3D('',#75449,#41076,#41077);
#35248=AXIS2_PLACEMENT_3D('',#75454,#41080,#41081);
#35249=AXIS2_PLACEMENT_3D('',#75455,#41082,#41083);
#35250=AXIS2_PLACEMENT_3D('',#75460,#41085,#41086);
#35251=AXIS2_PLACEMENT_3D('',#75463,#41088,#41089);
#35252=AXIS2_PLACEMENT_3D('',#75464,#41090,#41091);
#35253=AXIS2_PLACEMENT_3D('',#75467,#41092,#41093);
#35254=AXIS2_PLACEMENT_3D('',#75471,#41095,#41096);
#35255=AXIS2_PLACEMENT_3D('',#75473,#41098,#41099);
#35256=AXIS2_PLACEMENT_3D('',#75477,#41101,#41102);
#35257=AXIS2_PLACEMENT_3D('',#75478,#41103,#41104);
#35258=AXIS2_PLACEMENT_3D('',#75479,#41105,#41106);
#35259=AXIS2_PLACEMENT_3D('',#75480,#41107,#41108);
#35260=AXIS2_PLACEMENT_3D('',#75481,#41109,#41110);
#35261=AXIS2_PLACEMENT_3D('',#75483,#41112,#41113);
#35262=AXIS2_PLACEMENT_3D('',#75484,#41114,#41115);
#35263=AXIS2_PLACEMENT_3D('',#75485,#41116,#41117);
#35264=AXIS2_PLACEMENT_3D('',#75486,#41118,#41119);
#35265=AXIS2_PLACEMENT_3D('',#75488,#41121,#41122);
#35266=AXIS2_PLACEMENT_3D('',#75490,#41124,#41125);
#35267=AXIS2_PLACEMENT_3D('',#75494,#41127,#41128);
#35268=AXIS2_PLACEMENT_3D('',#75506,#41130,#41131);
#35269=AXIS2_PLACEMENT_3D('',#75510,#41133,#41134);
#35270=AXIS2_PLACEMENT_3D('',#75512,#41135,#41136);
#35271=AXIS2_PLACEMENT_3D('',#75543,#41138,#41139);
#35272=AXIS2_PLACEMENT_3D('',#75545,#41140,#41141);
#35273=AXIS2_PLACEMENT_3D('',#75549,#41143,#41144);
#35274=AXIS2_PLACEMENT_3D('',#75553,#41146,#41147);
#35275=AXIS2_PLACEMENT_3D('',#75597,#41150,#41151);
#35276=AXIS2_PLACEMENT_3D('',#75599,#41152,#41153);
#35277=AXIS2_PLACEMENT_3D('',#75604,#41156,#41157);
#35278=AXIS2_PLACEMENT_3D('',#75608,#41159,#41160);
#35279=AXIS2_PLACEMENT_3D('',#75611,#41162,#41163);
#35280=AXIS2_PLACEMENT_3D('',#75612,#41164,#41165);
#35281=AXIS2_PLACEMENT_3D('',#75614,#41166,#41167);
#35282=AXIS2_PLACEMENT_3D('',#75615,#41168,#41169);
#35283=AXIS2_PLACEMENT_3D('',#75619,#41171,#41172);
#35284=AXIS2_PLACEMENT_3D('',#75621,#41174,#41175);
#35285=AXIS2_PLACEMENT_3D('',#75623,#41176,#41177);
#35286=AXIS2_PLACEMENT_3D('',#75625,#41179,#41180);
#35287=AXIS2_PLACEMENT_3D('',#75627,#41181,#41182);
#35288=AXIS2_PLACEMENT_3D('',#75629,#41184,#41185);
#35289=AXIS2_PLACEMENT_3D('',#75632,#41187,#41188);
#35290=AXIS2_PLACEMENT_3D('',#75633,#41189,#41190);
#35291=AXIS2_PLACEMENT_3D('',#75635,#41191,#41192);
#35292=AXIS2_PLACEMENT_3D('',#75637,#41194,#41195);
#35293=AXIS2_PLACEMENT_3D('',#75641,#41198,#41199);
#35294=AXIS2_PLACEMENT_3D('',#75643,#41200,#41201);
#35295=AXIS2_PLACEMENT_3D('',#75645,#41203,#41204);
#35296=AXIS2_PLACEMENT_3D('',#75647,#41205,#41206);
#35297=AXIS2_PLACEMENT_3D('',#75649,#41208,#41209);
#35298=AXIS2_PLACEMENT_3D('',#75651,#41211,#41212);
#35299=AXIS2_PLACEMENT_3D('',#75654,#41214,#41215);
#35300=AXIS2_PLACEMENT_3D('',#75655,#41216,#41217);
#35301=AXIS2_PLACEMENT_3D('',#75657,#41218,#41219);
#35302=AXIS2_PLACEMENT_3D('',#75659,#41221,#41222);
#35303=AXIS2_PLACEMENT_3D('',#75661,#41223,#41224);
#35304=AXIS2_PLACEMENT_3D('',#75662,#41225,#41226);
#35305=AXIS2_PLACEMENT_3D('',#75665,#41227,#41228);
#35306=AXIS2_PLACEMENT_3D('',#75668,#41231,#41232);
#35307=AXIS2_PLACEMENT_3D('',#75670,#41233,#41234);
#35308=AXIS2_PLACEMENT_3D('',#75867,#41243,#41244);
#35309=AXIS2_PLACEMENT_3D('',#75869,#41245,#41246);
#35310=AXIS2_PLACEMENT_3D('',#75871,#41248,#41249);
#35311=AXIS2_PLACEMENT_3D('',#75874,#41250,#41251);
#35312=AXIS2_PLACEMENT_3D('',#76072,#41261,#41262);
#35313=AXIS2_PLACEMENT_3D('',#76074,#41263,#41264);
#35314=AXIS2_PLACEMENT_3D('',#76076,#41266,#41267);
#35315=AXIS2_PLACEMENT_3D('',#76078,#41268,#41269);
#35316=AXIS2_PLACEMENT_3D('',#76080,#41271,#41272);
#35317=AXIS2_PLACEMENT_3D('',#76082,#41273,#41274);
#35318=AXIS2_PLACEMENT_3D('',#76084,#41276,#41277);
#35319=AXIS2_PLACEMENT_3D('',#76086,#41278,#41279);
#35320=AXIS2_PLACEMENT_3D('',#76090,#41281,#41282);
#35321=AXIS2_PLACEMENT_3D('',#76092,#41283,#41284);
#35322=AXIS2_PLACEMENT_3D('',#76094,#41286,#41287);
#35323=AXIS2_PLACEMENT_3D('',#76096,#41288,#41289);
#35324=AXIS2_PLACEMENT_3D('',#76097,#41290,#41291);
#35325=AXIS2_PLACEMENT_3D('',#76099,#41292,#41293);
#35326=AXIS2_PLACEMENT_3D('',#76100,#41294,#41295);
#35327=AXIS2_PLACEMENT_3D('',#76103,#41297,#41298);
#35328=AXIS2_PLACEMENT_3D('',#76104,#41299,#41300);
#35329=AXIS2_PLACEMENT_3D('',#76105,#41301,#41302);
#35330=AXIS2_PLACEMENT_3D('',#76109,#41304,#41305);
#35331=AXIS2_PLACEMENT_3D('',#76110,#41306,#41307);
#35332=AXIS2_PLACEMENT_3D('',#76111,#41308,#41309);
#35333=AXIS2_PLACEMENT_3D('',#76124,#41313,#41314);
#35334=AXIS2_PLACEMENT_3D('',#76126,#41315,#41316);
#35335=AXIS2_PLACEMENT_3D('',#76128,#41317,#41318);
#35336=AXIS2_PLACEMENT_3D('',#76130,#41320,#41321);
#35337=AXIS2_PLACEMENT_3D('',#76132,#41322,#41323);
#35338=AXIS2_PLACEMENT_3D('',#76134,#41324,#41325);
#35339=AXIS2_PLACEMENT_3D('',#76136,#41327,#41328);
#35340=AXIS2_PLACEMENT_3D('',#76142,#41332,#41333);
#35341=AXIS2_PLACEMENT_3D('',#76146,#41335,#41336);
#35342=AXIS2_PLACEMENT_3D('',#76148,#41337,#41338);
#35343=AXIS2_PLACEMENT_3D('',#76150,#41339,#41340);
#35344=AXIS2_PLACEMENT_3D('',#76152,#41341,#41342);
#35345=AXIS2_PLACEMENT_3D('',#76154,#41343,#41344);
#35346=AXIS2_PLACEMENT_3D('',#76156,#41345,#41346);
#35347=AXIS2_PLACEMENT_3D('',#76157,#41347,#41348);
#35348=AXIS2_PLACEMENT_3D('',#76158,#41349,#41350);
#35349=AXIS2_PLACEMENT_3D('',#76161,#41351,#41352);
#35350=AXIS2_PLACEMENT_3D('',#76164,#41354,#41355);
#35351=AXIS2_PLACEMENT_3D('',#76166,#41356,#41357);
#35352=AXIS2_PLACEMENT_3D('',#76168,#41358,#41359);
#35353=AXIS2_PLACEMENT_3D('',#76170,#41360,#41361);
#35354=AXIS2_PLACEMENT_3D('',#76172,#41362,#41363);
#35355=AXIS2_PLACEMENT_3D('',#76173,#41364,#41365);
#35356=AXIS2_PLACEMENT_3D('',#76174,#41366,#41367);
#35357=AXIS2_PLACEMENT_3D('',#76175,#41368,#41369);
#35358=AXIS2_PLACEMENT_3D('',#76178,#41370,#41371);
#35359=AXIS2_PLACEMENT_3D('',#76182,#41373,#41374);
#35360=AXIS2_PLACEMENT_3D('',#76184,#41376,#41377);
#35361=AXIS2_PLACEMENT_3D('',#76188,#41379,#41380);
#35362=AXIS2_PLACEMENT_3D('',#76189,#41381,#41382);
#35363=AXIS2_PLACEMENT_3D('',#76367,#41386,#41387);
#35364=AXIS2_PLACEMENT_3D('',#76369,#41388,#41389);
#35365=AXIS2_PLACEMENT_3D('',#76371,#41390,#41391);
#35366=AXIS2_PLACEMENT_3D('',#76550,#41396,#41397);
#35367=AXIS2_PLACEMENT_3D('',#76554,#41399,#41400);
#35368=AXIS2_PLACEMENT_3D('',#76555,#41401,#41402);
#35369=AXIS2_PLACEMENT_3D('',#76556,#41403,#41404);
#35370=AXIS2_PLACEMENT_3D('',#76557,#41405,#41406);
#35371=AXIS2_PLACEMENT_3D('',#76558,#41407,#41408);
#35372=AXIS2_PLACEMENT_3D('',#76559,#41409,#41410);
#35373=AXIS2_PLACEMENT_3D('',#76561,#41411,#41412);
#35374=AXIS2_PLACEMENT_3D('',#76562,#41413,#41414);
#35375=AXIS2_PLACEMENT_3D('',#76563,#41415,#41416);
#35376=AXIS2_PLACEMENT_3D('',#76572,#41417,#41418);
#35377=AXIS2_PLACEMENT_3D('',#76574,#41419,#41420);
#35378=AXIS2_PLACEMENT_3D('',#76581,#41421,#41422);
#35379=AXIS2_PLACEMENT_3D('',#76617,#41425,#41426);
#35380=AXIS2_PLACEMENT_3D('',#76633,#41427,#41428);
#35381=AXIS2_PLACEMENT_3D('',#76659,#41429,#41430);
#35382=AXIS2_PLACEMENT_3D('',#76688,#41433,#41434);
#35383=AXIS2_PLACEMENT_3D('',#76690,#41435,#41436);
#35384=AXIS2_PLACEMENT_3D('',#76692,#41437,#41438);
#35385=AXIS2_PLACEMENT_3D('',#76713,#41439,#41440);
#35386=AXIS2_PLACEMENT_3D('',#76718,#41441,#41442);
#35387=AXIS2_PLACEMENT_3D('',#76719,#41443,#41444);
#35388=AXIS2_PLACEMENT_3D('',#76757,#41445,#41446);
#35389=AXIS2_PLACEMENT_3D('',#76758,#41447,#41448);
#35390=AXIS2_PLACEMENT_3D('',#76774,#41449,#41450);
#35391=AXIS2_PLACEMENT_3D('',#76783,#41451,#41452);
#35392=AXIS2_PLACEMENT_3D('',#76787,#41454,#41455);
#35393=AXIS2_PLACEMENT_3D('',#76788,#41456,#41457);
#35394=AXIS2_PLACEMENT_3D('',#76789,#41458,#41459);
#35395=AXIS2_PLACEMENT_3D('',#76805,#41460,#41461);
#35396=AXIS2_PLACEMENT_3D('',#76807,#41462,#41463);
#35397=AXIS2_PLACEMENT_3D('',#76809,#41464,#41465);
#35398=AXIS2_PLACEMENT_3D('',#76813,#41467,#41468);
#35399=AXIS2_PLACEMENT_3D('',#76820,#41469,#41470);
#35400=AXIS2_PLACEMENT_3D('',#76835,#41471,#41472);
#35401=AXIS2_PLACEMENT_3D('',#76836,#41473,#41474);
#35402=AXIS2_PLACEMENT_3D('',#76843,#41475,#41476);
#35403=AXIS2_PLACEMENT_3D('',#76850,#41477,#41478);
#35404=AXIS2_PLACEMENT_3D('',#76851,#41479,#41480);
#35405=AXIS2_PLACEMENT_3D('',#76853,#41481,#41482);
#35406=AXIS2_PLACEMENT_3D('',#76890,#41483,#41484);
#35407=AXIS2_PLACEMENT_3D('',#76916,#41485,#41486);
#35408=AXIS2_PLACEMENT_3D('',#76918,#41487,#41488);
#35409=AXIS2_PLACEMENT_3D('',#76922,#41490,#41491);
#35410=AXIS2_PLACEMENT_3D('',#76924,#41492,#41493);
#35411=AXIS2_PLACEMENT_3D('',#76980,#41494,#41495);
#35412=AXIS2_PLACEMENT_3D('',#77010,#41496,#41497);
#35413=AXIS2_PLACEMENT_3D('',#77011,#41498,#41499);
#35414=AXIS2_PLACEMENT_3D('',#77014,#41500,#41501);
#35415=AXIS2_PLACEMENT_3D('',#77016,#41502,#41503);
#35416=AXIS2_PLACEMENT_3D('',#77020,#41505,#41506);
#35417=AXIS2_PLACEMENT_3D('',#77022,#41507,#41508);
#35418=AXIS2_PLACEMENT_3D('',#77071,#41509,#41510);
#35419=AXIS2_PLACEMENT_3D('',#77073,#41511,#41512);
#35420=AXIS2_PLACEMENT_3D('',#77075,#41514,#41515);
#35421=AXIS2_PLACEMENT_3D('',#77076,#41516,#41517);
#35422=AXIS2_PLACEMENT_3D('',#77133,#41519,#41520);
#35423=AXIS2_PLACEMENT_3D('',#77164,#41521,#41522);
#35424=AXIS2_PLACEMENT_3D('',#77166,#41523,#41524);
#35425=AXIS2_PLACEMENT_3D('',#77195,#41525,#41526);
#35426=AXIS2_PLACEMENT_3D('',#77197,#41527,#41528);
#35427=AXIS2_PLACEMENT_3D('',#77216,#41529,#41530);
#35428=AXIS2_PLACEMENT_3D('',#77294,#41534,#41535);
#35429=AXIS2_PLACEMENT_3D('',#77296,#41536,#41537);
#35430=AXIS2_PLACEMENT_3D('',#77461,#41544,#41545);
#35431=AXIS2_PLACEMENT_3D('',#77463,#41546,#41547);
#35432=AXIS2_PLACEMENT_3D('',#77465,#41549,#41550);
#35433=AXIS2_PLACEMENT_3D('',#77469,#41553,#41554);
#35434=AXIS2_PLACEMENT_3D('',#77470,#41555,#41556);
#35435=AXIS2_PLACEMENT_3D('',#77551,#41561,#41562);
#35436=AXIS2_PLACEMENT_3D('',#77553,#41563,#41564);
#35437=AXIS2_PLACEMENT_3D('',#77555,#41566,#41567);
#35438=AXIS2_PLACEMENT_3D('',#77559,#41570,#41571);
#35439=AXIS2_PLACEMENT_3D('',#77560,#41572,#41573);
#35440=AXIS2_PLACEMENT_3D('',#77561,#41574,#41575);
#35441=AXIS2_PLACEMENT_3D('',#77563,#41576,#41577);
#35442=AXIS2_PLACEMENT_3D('',#77757,#41585,#41586);
#35443=AXIS2_PLACEMENT_3D('',#77759,#41587,#41588);
#35444=AXIS2_PLACEMENT_3D('',#77761,#41590,#41591);
#35445=AXIS2_PLACEMENT_3D('',#77764,#41593,#41594);
#35446=AXIS2_PLACEMENT_3D('',#77765,#41595,#41596);
#35447=AXIS2_PLACEMENT_3D('',#77769,#41599,#41600);
#35448=AXIS2_PLACEMENT_3D('',#77772,#41602,#41603);
#35449=AXIS2_PLACEMENT_3D('',#77773,#41604,#41605);
#35450=AXIS2_PLACEMENT_3D('',#77775,#41606,#41607);
#35451=AXIS2_PLACEMENT_3D('',#77906,#41613,#41614);
#35452=AXIS2_PLACEMENT_3D('',#77962,#41618,#41619);
#35453=AXIS2_PLACEMENT_3D('',#77964,#41621,#41622);
#35454=AXIS2_PLACEMENT_3D('',#77965,#41623,#41624);
#35455=AXIS2_PLACEMENT_3D('',#77968,#41625,#41626);
#35456=AXIS2_PLACEMENT_3D('',#77971,#41629,#41630);
#35457=AXIS2_PLACEMENT_3D('',#77973,#41631,#41632);
#35458=AXIS2_PLACEMENT_3D('',#77975,#41634,#41635);
#35459=AXIS2_PLACEMENT_3D('',#77979,#41638,#41639);
#35460=AXIS2_PLACEMENT_3D('',#77981,#41640,#41641);
#35461=AXIS2_PLACEMENT_3D('',#77983,#41643,#41644);
#35462=AXIS2_PLACEMENT_3D('',#77985,#41645,#41646);
#35463=AXIS2_PLACEMENT_3D('',#78128,#41651,#41652);
#35464=AXIS2_PLACEMENT_3D('',#78129,#41653,#41654);
#35465=AXIS2_PLACEMENT_3D('',#78130,#41655,#41656);
#35466=AXIS2_PLACEMENT_3D('',#78132,#41658,#41659);
#35467=AXIS2_PLACEMENT_3D('',#78134,#41661,#41662);
#35468=AXIS2_PLACEMENT_3D('',#78136,#41664,#41665);
#35469=AXIS2_PLACEMENT_3D('',#78138,#41667,#41668);
#35470=AXIS2_PLACEMENT_3D('',#78146,#41673,#41674);
#35471=AXIS2_PLACEMENT_3D('',#78156,#41680,#41681);
#35472=AXIS2_PLACEMENT_3D('',#78166,#41687,#41688);
#35473=AXIS2_PLACEMENT_3D('',#78174,#41693,#41694);
#35474=AXIS2_PLACEMENT_3D('',#78182,#41699,#41700);
#35475=AXIS2_PLACEMENT_3D('',#78192,#41706,#41707);
#35476=AXIS2_PLACEMENT_3D('',#78202,#41713,#41714);
#35477=AXIS2_PLACEMENT_3D('',#78210,#41719,#41720);
#35478=AXIS2_PLACEMENT_3D('',#78211,#41721,#41722);
#35479=AXIS2_PLACEMENT_3D('',#78212,#41723,#41724);
#35480=AXIS2_PLACEMENT_3D('',#78215,#41726,#41727);
#35481=AXIS2_PLACEMENT_3D('',#78216,#41728,#41729);
#35482=AXIS2_PLACEMENT_3D('',#78218,#41730,#41731);
#35483=AXIS2_PLACEMENT_3D('',#78221,#41733,#41734);
#35484=AXIS2_PLACEMENT_3D('',#78222,#41735,#41736);
#35485=AXIS2_PLACEMENT_3D('',#78223,#41737,#41738);
#35486=AXIS2_PLACEMENT_3D('',#78225,#41739,#41740);
#35487=AXIS2_PLACEMENT_3D('',#78228,#41742,#41743);
#35488=AXIS2_PLACEMENT_3D('',#78230,#41744,#41745);
#35489=AXIS2_PLACEMENT_3D('',#78233,#41747,#41748);
#35490=AXIS2_PLACEMENT_3D('',#78236,#41750,#41751);
#35491=AXIS2_PLACEMENT_3D('',#78238,#41752,#41753);
#35492=AXIS2_PLACEMENT_3D('',#78241,#41755,#41756);
#35493=AXIS2_PLACEMENT_3D('',#78244,#41758,#41759);
#35494=AXIS2_PLACEMENT_3D('',#78245,#41760,#41761);
#35495=AXIS2_PLACEMENT_3D('',#78246,#41762,#41763);
#35496=AXIS2_PLACEMENT_3D('',#78247,#41764,#41765);
#35497=AXIS2_PLACEMENT_3D('',#78249,#41766,#41767);
#35498=AXIS2_PLACEMENT_3D('',#78251,#41769,#41770);
#35499=AXIS2_PLACEMENT_3D('',#78253,#41771,#41772);
#35500=AXIS2_PLACEMENT_3D('',#78255,#41773,#41774);
#35501=AXIS2_PLACEMENT_3D('',#78257,#41776,#41777);
#35502=AXIS2_PLACEMENT_3D('',#78258,#41778,#41779);
#35503=AXIS2_PLACEMENT_3D('',#78259,#41780,#41781);
#35504=AXIS2_PLACEMENT_3D('',#78260,#41782,#41783);
#35505=AXIS2_PLACEMENT_3D('',#78261,#41784,#41785);
#35506=AXIS2_PLACEMENT_3D('',#78263,#41786,#41787);
#35507=AXIS2_PLACEMENT_3D('',#78265,#41789,#41790);
#35508=AXIS2_PLACEMENT_3D('',#78266,#41791,#41792);
#35509=AXIS2_PLACEMENT_3D('',#78267,#41793,#41794);
#35510=AXIS2_PLACEMENT_3D('',#78269,#41795,#41796);
#35511=AXIS2_PLACEMENT_3D('',#78270,#41797,#41798);
#35512=AXIS2_PLACEMENT_3D('',#78271,#41799,#41800);
#35513=AXIS2_PLACEMENT_3D('',#78272,#41801,#41802);
#35514=AXIS2_PLACEMENT_3D('',#78273,#41803,#41804);
#35515=AXIS2_PLACEMENT_3D('',#78274,#41805,#41806);
#35516=AXIS2_PLACEMENT_3D('',#78275,#41807,#41808);
#35517=AXIS2_PLACEMENT_3D('',#78283,#41812,#41813);
#35518=AXIS2_PLACEMENT_3D('',#78285,#41814,#41815);
#35519=AXIS2_PLACEMENT_3D('',#78287,#41816,#41817);
#35520=AXIS2_PLACEMENT_3D('',#78291,#41820,#41821);
#35521=AXIS2_PLACEMENT_3D('',#78293,#41822,#41823);
#35522=AXIS2_PLACEMENT_3D('',#78295,#41825,#41826);
#35523=AXIS2_PLACEMENT_3D('',#78296,#41827,#41828);
#35524=AXIS2_PLACEMENT_3D('',#78297,#41829,#41830);
#35525=AXIS2_PLACEMENT_3D('',#78298,#41831,#41832);
#35526=AXIS2_PLACEMENT_3D('',#78299,#41833,#41834);
#35527=AXIS2_PLACEMENT_3D('',#78300,#41835,#41836);
#35528=AXIS2_PLACEMENT_3D('',#78302,#41837,#41838);
#35529=AXIS2_PLACEMENT_3D('',#78303,#41839,#41840);
#35530=AXIS2_PLACEMENT_3D('',#78304,#41841,#41842);
#35531=AXIS2_PLACEMENT_3D('',#78307,#41844,#41845);
#35532=AXIS2_PLACEMENT_3D('',#78308,#41846,#41847);
#35533=AXIS2_PLACEMENT_3D('',#78309,#41848,#41849);
#35534=AXIS2_PLACEMENT_3D('',#78310,#41850,#41851);
#35535=AXIS2_PLACEMENT_3D('',#78311,#41852,#41853);
#35536=AXIS2_PLACEMENT_3D('',#78312,#41854,#41855);
#35537=AXIS2_PLACEMENT_3D('',#78313,#41856,#41857);
#35538=AXIS2_PLACEMENT_3D('',#78314,#41858,#41859);
#35539=AXIS2_PLACEMENT_3D('',#78315,#41860,#41861);
#35540=AXIS2_PLACEMENT_3D('',#78316,#41862,#41863);
#35541=AXIS2_PLACEMENT_3D('',#78317,#41864,#41865);
#35542=AXIS2_PLACEMENT_3D('',#78318,#41866,#41867);
#35543=AXIS2_PLACEMENT_3D('',#78319,#41868,#41869);
#35544=AXIS2_PLACEMENT_3D('',#78320,#41870,#41871);
#35545=AXIS2_PLACEMENT_3D('',#78321,#41872,#41873);
#35546=AXIS2_PLACEMENT_3D('',#78322,#41874,#41875);
#35547=AXIS2_PLACEMENT_3D('',#78324,#41877,#41878);
#35548=AXIS2_PLACEMENT_3D('',#78325,#41879,#41880);
#35549=AXIS2_PLACEMENT_3D('',#78327,#41882,#41883);
#35550=AXIS2_PLACEMENT_3D('',#78329,#41885,#41886);
#35551=AXIS2_PLACEMENT_3D('',#78330,#41887,#41888);
#35552=AXIS2_PLACEMENT_3D('',#78331,#41889,#41890);
#35553=AXIS2_PLACEMENT_3D('',#78332,#41891,#41892);
#35554=AXIS2_PLACEMENT_3D('',#78338,#41896,#41897);
#35555=AXIS2_PLACEMENT_3D('',#78340,#41898,#41899);
#35556=AXIS2_PLACEMENT_3D('',#78342,#41900,#41901);
#35557=AXIS2_PLACEMENT_3D('',#78344,#41903,#41904);
#35558=AXIS2_PLACEMENT_3D('',#78345,#41905,#41906);
#35559=AXIS2_PLACEMENT_3D('',#78346,#41907,#41908);
#35560=AXIS2_PLACEMENT_3D('',#78347,#41909,#41910);
#35561=AXIS2_PLACEMENT_3D('',#78348,#41911,#41912);
#35562=AXIS2_PLACEMENT_3D('',#78351,#41914,#41915);
#35563=AXIS2_PLACEMENT_3D('',#78352,#41916,#41917);
#35564=AXIS2_PLACEMENT_3D('',#78353,#41918,#41919);
#35565=AXIS2_PLACEMENT_3D('',#78354,#41920,#41921);
#35566=AXIS2_PLACEMENT_3D('',#78356,#41922,#41923);
#35567=AXIS2_PLACEMENT_3D('',#78357,#41924,#41925);
#35568=AXIS2_PLACEMENT_3D('',#78358,#41926,#41927);
#35569=AXIS2_PLACEMENT_3D('',#78361,#41929,#41930);
#35570=AXIS2_PLACEMENT_3D('',#78362,#41931,#41932);
#35571=AXIS2_PLACEMENT_3D('',#78363,#41933,#41934);
#35572=AXIS2_PLACEMENT_3D('',#78364,#41935,#41936);
#35573=AXIS2_PLACEMENT_3D('',#78372,#41940,#41941);
#35574=AXIS2_PLACEMENT_3D('',#78374,#41942,#41943);
#35575=AXIS2_PLACEMENT_3D('',#78376,#41944,#41945);
#35576=AXIS2_PLACEMENT_3D('',#78380,#41948,#41949);
#35577=AXIS2_PLACEMENT_3D('',#78382,#41950,#41951);
#35578=AXIS2_PLACEMENT_3D('',#78384,#41953,#41954);
#35579=AXIS2_PLACEMENT_3D('',#78386,#41955,#41956);
#35580=AXIS2_PLACEMENT_3D('',#78387,#41957,#41958);
#35581=AXIS2_PLACEMENT_3D('',#78388,#41959,#41960);
#35582=AXIS2_PLACEMENT_3D('',#78391,#41962,#41963);
#35583=AXIS2_PLACEMENT_3D('',#78392,#41964,#41965);
#35584=AXIS2_PLACEMENT_3D('',#78394,#41966,#41967);
#35585=AXIS2_PLACEMENT_3D('',#78395,#41968,#41969);
#35586=AXIS2_PLACEMENT_3D('',#78396,#41970,#41971);
#35587=AXIS2_PLACEMENT_3D('',#78399,#41973,#41974);
#35588=AXIS2_PLACEMENT_3D('',#78400,#41975,#41976);
#35589=AXIS2_PLACEMENT_3D('',#78402,#41977,#41978);
#35590=AXIS2_PLACEMENT_3D('',#78403,#41979,#41980);
#35591=AXIS2_PLACEMENT_3D('',#78404,#41981,#41982);
#35592=AXIS2_PLACEMENT_3D('',#78407,#41984,#41985);
#35593=AXIS2_PLACEMENT_3D('',#78408,#41986,#41987);
#35594=AXIS2_PLACEMENT_3D('',#78409,#41988,#41989);
#35595=AXIS2_PLACEMENT_3D('',#78410,#41990,#41991);
#35596=AXIS2_PLACEMENT_3D('',#78411,#41992,#41993);
#35597=AXIS2_PLACEMENT_3D('',#78412,#41994,#41995);
#35598=AXIS2_PLACEMENT_3D('',#78413,#41996,#41997);
#35599=AXIS2_PLACEMENT_3D('',#78415,#41998,#41999);
#35600=AXIS2_PLACEMENT_3D('',#78416,#42000,#42001);
#35601=AXIS2_PLACEMENT_3D('',#78417,#42002,#42003);
#35602=AXIS2_PLACEMENT_3D('',#78419,#42005,#42006);
#35603=AXIS2_PLACEMENT_3D('',#78421,#42008,#42009);
#35604=AXIS2_PLACEMENT_3D('',#78423,#42011,#42012);
#35605=AXIS2_PLACEMENT_3D('',#78425,#42014,#42015);
#35606=AXIS2_PLACEMENT_3D('',#78427,#42017,#42018);
#35607=AXIS2_PLACEMENT_3D('',#78429,#42020,#42021);
#35608=AXIS2_PLACEMENT_3D('',#78431,#42023,#42024);
#35609=AXIS2_PLACEMENT_3D('',#78433,#42026,#42027);
#35610=AXIS2_PLACEMENT_3D('',#78434,#42028,#42029);
#35611=AXIS2_PLACEMENT_3D('',#78436,#42031,#42032);
#35612=AXIS2_PLACEMENT_3D('',#78437,#42033,#42034);
#35613=AXIS2_PLACEMENT_3D('',#78439,#42035,#42036);
#35614=AXIS2_PLACEMENT_3D('',#78442,#42038,#42039);
#35615=AXIS2_PLACEMENT_3D('',#78443,#42040,#42041);
#35616=AXIS2_PLACEMENT_3D('',#78444,#42042,#42043);
#35617=AXIS2_PLACEMENT_3D('',#78445,#42044,#42045);
#35618=AXIS2_PLACEMENT_3D('',#78446,#42046,#42047);
#35619=AXIS2_PLACEMENT_3D('',#78447,#42048,#42049);
#35620=AXIS2_PLACEMENT_3D('',#78450,#42051,#42052);
#35621=AXIS2_PLACEMENT_3D('',#78451,#42053,#42054);
#35622=AXIS2_PLACEMENT_3D('',#78452,#42055,#42056);
#35623=AXIS2_PLACEMENT_3D('',#78453,#42057,#42058);
#35624=AXIS2_PLACEMENT_3D('',#78455,#42059,#42060);
#35625=AXIS2_PLACEMENT_3D('',#78456,#42061,#42062);
#35626=AXIS2_PLACEMENT_3D('',#78457,#42063,#42064);
#35627=AXIS2_PLACEMENT_3D('',#78458,#42065,#42066);
#35628=AXIS2_PLACEMENT_3D('',#78459,#42067,#42068);
#35629=AXIS2_PLACEMENT_3D('',#78460,#42069,#42070);
#35630=AXIS2_PLACEMENT_3D('',#78461,#42071,#42072);
#35631=AXIS2_PLACEMENT_3D('',#78467,#42075,#42076);
#35632=AXIS2_PLACEMENT_3D('',#78469,#42077,#42078);
#35633=AXIS2_PLACEMENT_3D('',#78471,#42079,#42080);
#35634=AXIS2_PLACEMENT_3D('',#78477,#42084,#42085);
#35635=AXIS2_PLACEMENT_3D('',#78479,#42086,#42087);
#35636=AXIS2_PLACEMENT_3D('',#78481,#42089,#42090);
#35637=AXIS2_PLACEMENT_3D('',#78482,#42091,#42092);
#35638=AXIS2_PLACEMENT_3D('',#78483,#42093,#42094);
#35639=AXIS2_PLACEMENT_3D('',#78484,#42095,#42096);
#35640=AXIS2_PLACEMENT_3D('',#78485,#42097,#42098);
#35641=AXIS2_PLACEMENT_3D('',#78486,#42099,#42100);
#35642=AXIS2_PLACEMENT_3D('',#78488,#42101,#42102);
#35643=AXIS2_PLACEMENT_3D('',#78489,#42103,#42104);
#35644=AXIS2_PLACEMENT_3D('',#78490,#42105,#42106);
#35645=AXIS2_PLACEMENT_3D('',#78492,#42107,#42108);
#35646=AXIS2_PLACEMENT_3D('',#78494,#42110,#42111);
#35647=AXIS2_PLACEMENT_3D('',#78495,#42112,#42113);
#35648=AXIS2_PLACEMENT_3D('',#78496,#42114,#42115);
#35649=AXIS2_PLACEMENT_3D('',#78497,#42116,#42117);
#35650=AXIS2_PLACEMENT_3D('',#78498,#42118,#42119);
#35651=AXIS2_PLACEMENT_3D('',#78499,#42120,#42121);
#35652=AXIS2_PLACEMENT_3D('',#78500,#42122,#42123);
#35653=AXIS2_PLACEMENT_3D('',#78501,#42124,#42125);
#35654=AXIS2_PLACEMENT_3D('',#78502,#42126,#42127);
#35655=AXIS2_PLACEMENT_3D('',#78503,#42128,#42129);
#35656=AXIS2_PLACEMENT_3D('',#78504,#42130,#42131);
#35657=AXIS2_PLACEMENT_3D('',#78505,#42132,#42133);
#35658=AXIS2_PLACEMENT_3D('',#78506,#42134,#42135);
#35659=AXIS2_PLACEMENT_3D('',#78507,#42136,#42137);
#35660=AXIS2_PLACEMENT_3D('',#78508,#42138,#42139);
#35661=AXIS2_PLACEMENT_3D('',#78510,#42141,#42142);
#35662=AXIS2_PLACEMENT_3D('',#78511,#42143,#42144);
#35663=AXIS2_PLACEMENT_3D('',#78513,#42146,#42147);
#35664=AXIS2_PLACEMENT_3D('',#78515,#42149,#42150);
#35665=AXIS2_PLACEMENT_3D('',#78516,#42151,#42152);
#35666=AXIS2_PLACEMENT_3D('',#78517,#42153,#42154);
#35667=AXIS2_PLACEMENT_3D('',#78518,#42155,#42156);
#35668=AXIS2_PLACEMENT_3D('',#78524,#42160,#42161);
#35669=AXIS2_PLACEMENT_3D('',#78526,#42162,#42163);
#35670=AXIS2_PLACEMENT_3D('',#78529,#42165,#42166);
#35671=AXIS2_PLACEMENT_3D('',#78530,#42167,#42168);
#35672=AXIS2_PLACEMENT_3D('',#78533,#42170,#42171);
#35673=AXIS2_PLACEMENT_3D('',#78534,#42172,#42173);
#35674=AXIS2_PLACEMENT_3D('',#78535,#42174,#42175);
#35675=AXIS2_PLACEMENT_3D('',#78536,#42176,#42177);
#35676=AXIS2_PLACEMENT_3D('',#78537,#42178,#42179);
#35677=AXIS2_PLACEMENT_3D('',#78538,#42180,#42181);
#35678=AXIS2_PLACEMENT_3D('',#78539,#42182,#42183);
#35679=AXIS2_PLACEMENT_3D('',#78540,#42184,#42185);
#35680=AXIS2_PLACEMENT_3D('',#78546,#42188,#42189);
#35681=AXIS2_PLACEMENT_3D('',#78548,#42190,#42191);
#35682=AXIS2_PLACEMENT_3D('',#78550,#42192,#42193);
#35683=AXIS2_PLACEMENT_3D('',#78557,#42197,#42198);
#35684=AXIS2_PLACEMENT_3D('',#78558,#42199,#42200);
#35685=AXIS2_PLACEMENT_3D('',#78560,#42201,#42202);
#35686=AXIS2_PLACEMENT_3D('',#78562,#42204,#42205);
#35687=AXIS2_PLACEMENT_3D('',#78564,#42206,#42207);
#35688=AXIS2_PLACEMENT_3D('',#78565,#42208,#42209);
#35689=AXIS2_PLACEMENT_3D('',#78566,#42210,#42211);
#35690=AXIS2_PLACEMENT_3D('',#78567,#42212,#42213);
#35691=AXIS2_PLACEMENT_3D('',#78568,#42214,#42215);
#35692=AXIS2_PLACEMENT_3D('',#78570,#42216,#42217);
#35693=AXIS2_PLACEMENT_3D('',#78571,#42218,#42219);
#35694=AXIS2_PLACEMENT_3D('',#78572,#42220,#42221);
#35695=AXIS2_PLACEMENT_3D('',#78574,#42222,#42223);
#35696=AXIS2_PLACEMENT_3D('',#78576,#42224,#42225);
#35697=AXIS2_PLACEMENT_3D('',#78578,#42227,#42228);
#35698=AXIS2_PLACEMENT_3D('',#78580,#42229,#42230);
#35699=AXIS2_PLACEMENT_3D('',#78581,#42231,#42232);
#35700=AXIS2_PLACEMENT_3D('',#78582,#42233,#42234);
#35701=AXIS2_PLACEMENT_3D('',#78584,#42235,#42236);
#35702=AXIS2_PLACEMENT_3D('',#78585,#42237,#42238);
#35703=AXIS2_PLACEMENT_3D('',#78586,#42239,#42240);
#35704=AXIS2_PLACEMENT_3D('',#78588,#42242,#42243);
#35705=AXIS2_PLACEMENT_3D('',#78590,#42244,#42245);
#35706=AXIS2_PLACEMENT_3D('',#78592,#42247,#42248);
#35707=AXIS2_PLACEMENT_3D('',#78593,#42249,#42250);
#35708=AXIS2_PLACEMENT_3D('',#78594,#42251,#42252);
#35709=AXIS2_PLACEMENT_3D('',#78595,#42253,#42254);
#35710=AXIS2_PLACEMENT_3D('',#78596,#42255,#42256);
#35711=AXIS2_PLACEMENT_3D('',#78597,#42257,#42258);
#35712=AXIS2_PLACEMENT_3D('',#78599,#42259,#42260);
#35713=AXIS2_PLACEMENT_3D('',#78600,#42261,#42262);
#35714=AXIS2_PLACEMENT_3D('',#78601,#42263,#42264);
#35715=AXIS2_PLACEMENT_3D('',#78603,#42266,#42267);
#35716=AXIS2_PLACEMENT_3D('',#78605,#42269,#42270);
#35717=AXIS2_PLACEMENT_3D('',#78607,#42272,#42273);
#35718=AXIS2_PLACEMENT_3D('',#78609,#42275,#42276);
#35719=AXIS2_PLACEMENT_3D('',#78612,#42279,#42280);
#35720=AXIS2_PLACEMENT_3D('',#78614,#42282,#42283);
#35721=AXIS2_PLACEMENT_3D('',#78616,#42285,#42286);
#35722=AXIS2_PLACEMENT_3D('',#78617,#42287,#42288);
#35723=AXIS2_PLACEMENT_3D('',#78619,#42290,#42291);
#35724=AXIS2_PLACEMENT_3D('',#78620,#42292,#42293);
#35725=AXIS2_PLACEMENT_3D('',#78622,#42295,#42296);
#35726=AXIS2_PLACEMENT_3D('',#78623,#42297,#42298);
#35727=AXIS2_PLACEMENT_3D('',#78624,#42299,#42300);
#35728=AXIS2_PLACEMENT_3D('',#78634,#42301,#42302);
#35729=AXIS2_PLACEMENT_3D('',#78636,#42303,#42304);
#35730=AXIS2_PLACEMENT_3D('',#78638,#42305,#42306);
#35731=AXIS2_PLACEMENT_3D('',#78646,#42307,#42308);
#35732=AXIS2_PLACEMENT_3D('',#78647,#42309,#42310);
#35733=AXIS2_PLACEMENT_3D('',#78650,#42311,#42312);
#35734=AXIS2_PLACEMENT_3D('',#78652,#42313,#42314);
#35735=AXIS2_PLACEMENT_3D('',#78654,#42315,#42316);
#35736=AXIS2_PLACEMENT_3D('',#78656,#42317,#42318);
#35737=AXIS2_PLACEMENT_3D('',#78658,#42319,#42320);
#35738=AXIS2_PLACEMENT_3D('',#78659,#42321,#42322);
#35739=AXIS2_PLACEMENT_3D('',#78660,#42323,#42324);
#35740=AXIS2_PLACEMENT_3D('',#78663,#42325,#42326);
#35741=AXIS2_PLACEMENT_3D('',#78665,#42327,#42328);
#35742=AXIS2_PLACEMENT_3D('',#78667,#42329,#42330);
#35743=AXIS2_PLACEMENT_3D('',#78669,#42331,#42332);
#35744=AXIS2_PLACEMENT_3D('',#78671,#42333,#42334);
#35745=AXIS2_PLACEMENT_3D('',#78672,#42335,#42336);
#35746=AXIS2_PLACEMENT_3D('',#78673,#42337,#42338);
#35747=AXIS2_PLACEMENT_3D('',#78676,#42339,#42340);
#35748=AXIS2_PLACEMENT_3D('',#78685,#42341,#42342);
#35749=AXIS2_PLACEMENT_3D('',#78687,#42343,#42344);
#35750=AXIS2_PLACEMENT_3D('',#78689,#42345,#42346);
#35751=AXIS2_PLACEMENT_3D('',#78690,#42347,#42348);
#35752=AXIS2_PLACEMENT_3D('',#78691,#42349,#42350);
#35753=AXIS2_PLACEMENT_3D('',#78694,#42351,#42352);
#35754=AXIS2_PLACEMENT_3D('',#78703,#42353,#42354);
#35755=AXIS2_PLACEMENT_3D('',#78712,#42355,#42356);
#35756=AXIS2_PLACEMENT_3D('',#78713,#42357,#42358);
#35757=AXIS2_PLACEMENT_3D('',#78714,#42359,#42360);
#35758=AXIS2_PLACEMENT_3D('',#78717,#42361,#42362);
#35759=AXIS2_PLACEMENT_3D('',#78726,#42363,#42364);
#35760=AXIS2_PLACEMENT_3D('',#78992,#42365,#42366);
#35761=AXIS2_PLACEMENT_3D('',#78993,#42367,#42368);
#35762=AXIS2_PLACEMENT_3D('',#78997,#42370,#42371);
#35763=AXIS2_PLACEMENT_3D('',#78998,#42372,#42373);
#35764=AXIS2_PLACEMENT_3D('',#79136,#42375,#42376);
#35765=AXIS2_PLACEMENT_3D('',#79140,#42378,#42379);
#35766=AXIS2_PLACEMENT_3D('',#79141,#42380,#42381);
#35767=AXIS2_PLACEMENT_3D('',#79142,#42382,#42383);
#35768=AXIS2_PLACEMENT_3D('',#79185,#42385,#42386);
#35769=AXIS2_PLACEMENT_3D('',#79186,#42387,#42388);
#35770=AXIS2_PLACEMENT_3D('',#79188,#42389,#42390);
#35771=AXIS2_PLACEMENT_3D('',#79189,#42391,#42392);
#35772=AXIS2_PLACEMENT_3D('',#79190,#42393,#42394);
#35773=AXIS2_PLACEMENT_3D('',#79192,#42395,#42396);
#35774=AXIS2_PLACEMENT_3D('',#79193,#42397,#42398);
#35775=AXIS2_PLACEMENT_3D('',#79252,#42399,#42400);
#35776=AXIS2_PLACEMENT_3D('',#79353,#42401,#42402);
#35777=AXIS2_PLACEMENT_3D('',#79377,#42403,#42404);
#35778=AXIS2_PLACEMENT_3D('',#79378,#42405,#42406);
#35779=AXIS2_PLACEMENT_3D('',#79381,#42407,#42408);
#35780=AXIS2_PLACEMENT_3D('',#79393,#42409,#42410);
#35781=AXIS2_PLACEMENT_3D('',#79430,#42411,#42412);
#35782=AXIS2_PLACEMENT_3D('',#79432,#42413,#42414);
#35783=AXIS2_PLACEMENT_3D('',#79503,#42415,#42416);
#35784=AXIS2_PLACEMENT_3D('',#79589,#42417,#42418);
#35785=AXIS2_PLACEMENT_3D('',#79660,#42419,#42420);
#35786=AXIS2_PLACEMENT_3D('',#79662,#42421,#42422);
#35787=AXIS2_PLACEMENT_3D('',#79699,#42423,#42424);
#35788=AXIS2_PLACEMENT_3D('',#79709,#42425,#42426);
#35789=AXIS2_PLACEMENT_3D('',#79710,#42427,#42428);
#35790=AXIS2_PLACEMENT_3D('',#79711,#42429,#42430);
#35791=AXIS2_PLACEMENT_3D('',#79712,#42431,#42432);
#35792=AXIS2_PLACEMENT_3D('',#79713,#42433,#42434);
#35793=AXIS2_PLACEMENT_3D('',#79750,#42435,#42436);
#35794=AXIS2_PLACEMENT_3D('',#79751,#42437,#42438);
#35795=AXIS2_PLACEMENT_3D('',#79753,#42439,#42440);
#35796=AXIS2_PLACEMENT_3D('',#79754,#42441,#42442);
#35797=AXIS2_PLACEMENT_3D('',#79757,#42444,#42445);
#35798=AXIS2_PLACEMENT_3D('',#79758,#42446,#42447);
#35799=AXIS2_PLACEMENT_3D('',#79761,#42448,#42449);
#35800=AXIS2_PLACEMENT_3D('',#79765,#42451,#42452);
#35801=AXIS2_PLACEMENT_3D('',#79769,#42454,#42455);
#35802=AXIS2_PLACEMENT_3D('',#79773,#42457,#42458);
#35803=AXIS2_PLACEMENT_3D('',#79775,#42460,#42461);
#35804=AXIS2_PLACEMENT_3D('',#79777,#42462,#42463);
#35805=AXIS2_PLACEMENT_3D('',#79780,#42465,#42466);
#35806=AXIS2_PLACEMENT_3D('',#79781,#42467,#42468);
#35807=AXIS2_PLACEMENT_3D('',#79783,#42469,#42470);
#35808=AXIS2_PLACEMENT_3D('',#79784,#42471,#42472);
#35809=AXIS2_PLACEMENT_3D('',#79785,#42473,#42474);
#35810=AXIS2_PLACEMENT_3D('',#79787,#42475,#42476);
#35811=AXIS2_PLACEMENT_3D('',#79799,#42478,#42479);
#35812=AXIS2_PLACEMENT_3D('',#79800,#42480,#42481);
#35813=AXIS2_PLACEMENT_3D('',#79801,#42482,#42483);
#35814=AXIS2_PLACEMENT_3D('',#79803,#42484,#42485);
#35815=AXIS2_PLACEMENT_3D('',#79815,#42487,#42488);
#35816=AXIS2_PLACEMENT_3D('',#79816,#42489,#42490);
#35817=AXIS2_PLACEMENT_3D('',#79817,#42491,#42492);
#35818=AXIS2_PLACEMENT_3D('',#79819,#42493,#42494);
#35819=AXIS2_PLACEMENT_3D('',#79821,#42496,#42497);
#35820=AXIS2_PLACEMENT_3D('',#79876,#42498,#42499);
#35821=AXIS2_PLACEMENT_3D('',#79878,#42500,#42501);
#35822=AXIS2_PLACEMENT_3D('',#79879,#42502,#42503);
#35823=AXIS2_PLACEMENT_3D('',#79880,#42504,#42505);
#35824=AXIS2_PLACEMENT_3D('',#79960,#42509,#42510);
#35825=AXIS2_PLACEMENT_3D('',#79961,#42511,#42512);
#35826=AXIS2_PLACEMENT_3D('',#79964,#42514,#42515);
#35827=AXIS2_PLACEMENT_3D('',#79965,#42516,#42517);
#35828=AXIS2_PLACEMENT_3D('',#79969,#42520,#42521);
#35829=AXIS2_PLACEMENT_3D('',#79971,#42522,#42523);
#35830=AXIS2_PLACEMENT_3D('',#79973,#42525,#42526);
#35831=AXIS2_PLACEMENT_3D('',#79977,#42529,#42530);
#35832=AXIS2_PLACEMENT_3D('',#79979,#42531,#42532);
#35833=AXIS2_PLACEMENT_3D('',#80018,#42534,#42535);
#35834=AXIS2_PLACEMENT_3D('',#80029,#42536,#42537);
#35835=AXIS2_PLACEMENT_3D('',#80130,#42542,#42543);
#35836=AXIS2_PLACEMENT_3D('',#80138,#42544,#42545);
#35837=AXIS2_PLACEMENT_3D('',#80198,#42546,#42547);
#35838=AXIS2_PLACEMENT_3D('',#80208,#42548,#42549);
#35839=AXIS2_PLACEMENT_3D('',#80211,#42550,#42551);
#35840=AXIS2_PLACEMENT_3D('',#80224,#42554,#42555);
#35841=AXIS2_PLACEMENT_3D('',#80234,#42556,#42557);
#35842=AXIS2_PLACEMENT_3D('',#80236,#42558,#42559);
#35843=AXIS2_PLACEMENT_3D('',#80239,#42561,#42562);
#35844=AXIS2_PLACEMENT_3D('',#80240,#42563,#42564);
#35845=AXIS2_PLACEMENT_3D('',#80242,#42565,#42566);
#35846=AXIS2_PLACEMENT_3D('',#80244,#42568,#42569);
#35847=AXIS2_PLACEMENT_3D('',#80246,#42570,#42571);
#35848=AXIS2_PLACEMENT_3D('',#80247,#42572,#42573);
#35849=AXIS2_PLACEMENT_3D('',#80248,#42574,#42575);
#35850=AXIS2_PLACEMENT_3D('',#80250,#42576,#42577);
#35851=AXIS2_PLACEMENT_3D('',#80252,#42579,#42580);
#35852=AXIS2_PLACEMENT_3D('',#80254,#42581,#42582);
#35853=AXIS2_PLACEMENT_3D('',#80255,#42583,#42584);
#35854=AXIS2_PLACEMENT_3D('',#80256,#42585,#42586);
#35855=AXIS2_PLACEMENT_3D('',#80258,#42587,#42588);
#35856=AXIS2_PLACEMENT_3D('',#80260,#42590,#42591);
#35857=AXIS2_PLACEMENT_3D('',#80262,#42592,#42593);
#35858=AXIS2_PLACEMENT_3D('',#80263,#42594,#42595);
#35859=AXIS2_PLACEMENT_3D('',#80318,#42596,#42597);
#35860=AXIS2_PLACEMENT_3D('',#80319,#42598,#42599);
#35861=AXIS2_PLACEMENT_3D('',#80321,#42600,#42601);
#35862=AXIS2_PLACEMENT_3D('',#80323,#42603,#42604);
#35863=AXIS2_PLACEMENT_3D('',#80327,#42606,#42607);
#35864=AXIS2_PLACEMENT_3D('',#80328,#42608,#42609);
#35865=AXIS2_PLACEMENT_3D('',#80329,#42610,#42611);
#35866=AXIS2_PLACEMENT_3D('',#80331,#42612,#42613);
#35867=AXIS2_PLACEMENT_3D('',#80333,#42614,#42615);
#35868=AXIS2_PLACEMENT_3D('',#80335,#42617,#42618);
#35869=AXIS2_PLACEMENT_3D('',#80337,#42619,#42620);
#35870=AXIS2_PLACEMENT_3D('',#80339,#42622,#42623);
#35871=AXIS2_PLACEMENT_3D('',#80457,#42628,#42629);
#35872=AXIS2_PLACEMENT_3D('',#80458,#42630,#42631);
#35873=AXIS2_PLACEMENT_3D('',#80461,#42633,#42634);
#35874=AXIS2_PLACEMENT_3D('',#80462,#42635,#42636);
#35875=AXIS2_PLACEMENT_3D('',#80465,#42637,#42638);
#35876=AXIS2_PLACEMENT_3D('',#80466,#42639,#42640);
#35877=AXIS2_PLACEMENT_3D('',#80467,#42641,#42642);
#35878=AXIS2_PLACEMENT_3D('',#80468,#42643,#42644);
#35879=AXIS2_PLACEMENT_3D('',#80469,#42645,#42646);
#35880=AXIS2_PLACEMENT_3D('',#80470,#42647,#42648);
#35881=AXIS2_PLACEMENT_3D('',#80472,#42649,#42650);
#35882=AXIS2_PLACEMENT_3D('',#80473,#42651,#42652);
#35883=AXIS2_PLACEMENT_3D('',#80474,#42653,#42654);
#35884=AXIS2_PLACEMENT_3D('',#80479,#42656,#42657);
#35885=AXIS2_PLACEMENT_3D('',#80487,#42661,#42662);
#35886=AXIS2_PLACEMENT_3D('',#80495,#42666,#42667);
#35887=AXIS2_PLACEMENT_3D('',#80499,#42669,#42670);
#35888=AXIS2_PLACEMENT_3D('',#80503,#42672,#42673);
#35889=AXIS2_PLACEMENT_3D('',#80507,#42675,#42676);
#35890=AXIS2_PLACEMENT_3D('',#80511,#42678,#42679);
#35891=AXIS2_PLACEMENT_3D('',#80513,#42680,#42681);
#35892=AXIS2_PLACEMENT_3D('',#80517,#42683,#42684);
#35893=AXIS2_PLACEMENT_3D('',#80521,#42686,#42687);
#35894=AXIS2_PLACEMENT_3D('',#80524,#42689,#42690);
#35895=AXIS2_PLACEMENT_3D('',#80528,#42692,#42693);
#35896=AXIS2_PLACEMENT_3D('',#80532,#42695,#42696);
#35897=AXIS2_PLACEMENT_3D('',#80534,#42697,#42698);
#35898=AXIS2_PLACEMENT_3D('',#80538,#42700,#42701);
#35899=AXIS2_PLACEMENT_3D('',#80540,#42703,#42704);
#35900=AXIS2_PLACEMENT_3D('',#80541,#42705,#42706);
#35901=AXIS2_PLACEMENT_3D('',#80542,#42707,#42708);
#35902=AXIS2_PLACEMENT_3D('',#80544,#42709,#42710);
#35903=AXIS2_PLACEMENT_3D('',#80546,#42711,#42712);
#35904=AXIS2_PLACEMENT_3D('',#80547,#42713,#42714);
#35905=AXIS2_PLACEMENT_3D('',#80548,#42715,#42716);
#35906=AXIS2_PLACEMENT_3D('',#80550,#42717,#42718);
#35907=AXIS2_PLACEMENT_3D('',#80553,#42720,#42721);
#35908=AXIS2_PLACEMENT_3D('',#80554,#42722,#42723);
#35909=AXIS2_PLACEMENT_3D('',#80556,#42724,#42725);
#35910=AXIS2_PLACEMENT_3D('',#80560,#42727,#42728);
#35911=AXIS2_PLACEMENT_3D('',#80563,#42730,#42731);
#35912=AXIS2_PLACEMENT_3D('',#80564,#42732,#42733);
#35913=AXIS2_PLACEMENT_3D('',#80565,#42734,#42735);
#35914=AXIS2_PLACEMENT_3D('',#80566,#42736,#42737);
#35915=AXIS2_PLACEMENT_3D('',#80572,#42741,#42742);
#35916=AXIS2_PLACEMENT_3D('',#80573,#42743,#42744);
#35917=AXIS2_PLACEMENT_3D('',#80574,#42745,#42746);
#35918=AXIS2_PLACEMENT_3D('',#80575,#42747,#42748);
#35919=AXIS2_PLACEMENT_3D('',#80576,#42749,#42750);
#35920=AXIS2_PLACEMENT_3D('',#80577,#42751,#42752);
#35921=AXIS2_PLACEMENT_3D('',#80578,#42753,#42754);
#35922=AXIS2_PLACEMENT_3D('',#80579,#42755,#42756);
#35923=AXIS2_PLACEMENT_3D('',#80581,#42757,#42758);
#35924=AXIS2_PLACEMENT_3D('',#80584,#42760,#42761);
#35925=AXIS2_PLACEMENT_3D('',#80585,#42762,#42763);
#35926=AXIS2_PLACEMENT_3D('',#80586,#42764,#42765);
#35927=AXIS2_PLACEMENT_3D('',#80587,#42766,#42767);
#35928=AXIS2_PLACEMENT_3D('',#80588,#42768,#42769);
#35929=AXIS2_PLACEMENT_3D('',#80589,#42770,#42771);
#35930=AXIS2_PLACEMENT_3D('',#80590,#42772,#42773);
#35931=AXIS2_PLACEMENT_3D('',#80592,#42774,#42775);
#35932=AXIS2_PLACEMENT_3D('',#80595,#42777,#42778);
#35933=AXIS2_PLACEMENT_3D('',#80596,#42779,#42780);
#35934=AXIS2_PLACEMENT_3D('',#80598,#42781,#42782);
#35935=AXIS2_PLACEMENT_3D('',#80599,#42783,#42784);
#35936=AXIS2_PLACEMENT_3D('',#80600,#42785,#42786);
#35937=AXIS2_PLACEMENT_3D('',#80602,#42787,#42788);
#35938=AXIS2_PLACEMENT_3D('',#80604,#42790,#42791);
#35939=AXIS2_PLACEMENT_3D('',#80606,#42792,#42793);
#35940=AXIS2_PLACEMENT_3D('',#80607,#42794,#42795);
#35941=AXIS2_PLACEMENT_3D('',#80608,#42796,#42797);
#35942=AXIS2_PLACEMENT_3D('',#80610,#42798,#42799);
#35943=AXIS2_PLACEMENT_3D('',#80611,#42800,#42801);
#35944=AXIS2_PLACEMENT_3D('',#80612,#42802,#42803);
#35945=AXIS2_PLACEMENT_3D('',#80614,#42804,#42805);
#35946=AXIS2_PLACEMENT_3D('',#80616,#42806,#42807);
#35947=AXIS2_PLACEMENT_3D('',#80618,#42809,#42810);
#35948=AXIS2_PLACEMENT_3D('',#80619,#42811,#42812);
#35949=AXIS2_PLACEMENT_3D('',#80620,#42813,#42814);
#35950=AXIS2_PLACEMENT_3D('',#80621,#42815,#42816);
#35951=AXIS2_PLACEMENT_3D('',#80622,#42817,#42818);
#35952=AXIS2_PLACEMENT_3D('',#80623,#42819,#42820);
#35953=AXIS2_PLACEMENT_3D('',#80624,#42821,#42822);
#35954=AXIS2_PLACEMENT_3D('',#80626,#42823,#42824);
#35955=AXIS2_PLACEMENT_3D('',#80628,#42826,#42827);
#35956=AXIS2_PLACEMENT_3D('',#80630,#42828,#42829);
#35957=AXIS2_PLACEMENT_3D('',#80631,#42830,#42831);
#35958=AXIS2_PLACEMENT_3D('',#80632,#42832,#42833);
#35959=AXIS2_PLACEMENT_3D('',#80634,#42834,#42835);
#35960=AXIS2_PLACEMENT_3D('',#80636,#42837,#42838);
#35961=AXIS2_PLACEMENT_3D('',#80638,#42839,#42840);
#35962=AXIS2_PLACEMENT_3D('',#80640,#42841,#42842);
#35963=AXIS2_PLACEMENT_3D('',#80641,#42843,#42844);
#35964=AXIS2_PLACEMENT_3D('',#80642,#42845,#42846);
#35965=AXIS2_PLACEMENT_3D('',#80644,#42847,#42848);
#35966=AXIS2_PLACEMENT_3D('',#80645,#42849,#42850);
#35967=AXIS2_PLACEMENT_3D('',#80646,#42851,#42852);
#35968=AXIS2_PLACEMENT_3D('',#80648,#42853,#42854);
#35969=AXIS2_PLACEMENT_3D('',#80650,#42856,#42857);
#35970=AXIS2_PLACEMENT_3D('',#80652,#42858,#42859);
#35971=AXIS2_PLACEMENT_3D('',#80653,#42860,#42861);
#35972=AXIS2_PLACEMENT_3D('',#80654,#42862,#42863);
#35973=AXIS2_PLACEMENT_3D('',#80656,#42864,#42865);
#35974=AXIS2_PLACEMENT_3D('',#80658,#42867,#42868);
#35975=AXIS2_PLACEMENT_3D('',#80660,#42869,#42870);
#35976=AXIS2_PLACEMENT_3D('',#80661,#42871,#42872);
#35977=AXIS2_PLACEMENT_3D('',#80662,#42873,#42874);
#35978=AXIS2_PLACEMENT_3D('',#80664,#42875,#42876);
#35979=AXIS2_PLACEMENT_3D('',#80666,#42878,#42879);
#35980=AXIS2_PLACEMENT_3D('',#80668,#42880,#42881);
#35981=AXIS2_PLACEMENT_3D('',#80669,#42882,#42883);
#35982=AXIS2_PLACEMENT_3D('',#80670,#42884,#42885);
#35983=AXIS2_PLACEMENT_3D('',#80672,#42886,#42887);
#35984=AXIS2_PLACEMENT_3D('',#80674,#42889,#42890);
#35985=AXIS2_PLACEMENT_3D('',#80676,#42891,#42892);
#35986=AXIS2_PLACEMENT_3D('',#80677,#42893,#42894);
#35987=AXIS2_PLACEMENT_3D('',#80678,#42895,#42896);
#35988=AXIS2_PLACEMENT_3D('',#80680,#42897,#42898);
#35989=AXIS2_PLACEMENT_3D('',#80682,#42900,#42901);
#35990=AXIS2_PLACEMENT_3D('',#80684,#42902,#42903);
#35991=AXIS2_PLACEMENT_3D('',#80686,#42904,#42905);
#35992=AXIS2_PLACEMENT_3D('',#80688,#42907,#42908);
#35993=AXIS2_PLACEMENT_3D('',#80690,#42909,#42910);
#35994=AXIS2_PLACEMENT_3D('',#80692,#42911,#42912);
#35995=AXIS2_PLACEMENT_3D('',#80694,#42914,#42915);
#35996=AXIS2_PLACEMENT_3D('',#80696,#42916,#42917);
#35997=AXIS2_PLACEMENT_3D('',#80697,#42918,#42919);
#35998=AXIS2_PLACEMENT_3D('',#80698,#42920,#42921);
#35999=AXIS2_PLACEMENT_3D('',#80700,#42922,#42923);
#36000=AXIS2_PLACEMENT_3D('',#80702,#42925,#42926);
#36001=AXIS2_PLACEMENT_3D('',#80704,#42927,#42928);
#36002=AXIS2_PLACEMENT_3D('',#80706,#42929,#42930);
#36003=AXIS2_PLACEMENT_3D('',#80708,#42932,#42933);
#36004=AXIS2_PLACEMENT_3D('',#80710,#42934,#42935);
#36005=AXIS2_PLACEMENT_3D('',#80712,#42936,#42937);
#36006=AXIS2_PLACEMENT_3D('',#80714,#42939,#42940);
#36007=AXIS2_PLACEMENT_3D('',#80716,#42941,#42942);
#36008=AXIS2_PLACEMENT_3D('',#80717,#42943,#42944);
#36009=AXIS2_PLACEMENT_3D('',#80718,#42945,#42946);
#36010=AXIS2_PLACEMENT_3D('',#80720,#42948,#42949);
#36011=AXIS2_PLACEMENT_3D('',#80723,#42950,#42951);
#36012=AXIS2_PLACEMENT_3D('',#80724,#42952,#42953);
#36013=AXIS2_PLACEMENT_3D('',#80725,#42954,#42955);
#36014=AXIS2_PLACEMENT_3D('',#80726,#42956,#42957);
#36015=AXIS2_PLACEMENT_3D('',#80727,#42958,#42959);
#36016=AXIS2_PLACEMENT_3D('',#80728,#42960,#42961);
#36017=AXIS2_PLACEMENT_3D('',#80730,#42962,#42963);
#36018=AXIS2_PLACEMENT_3D('',#80732,#42964,#42965);
#36019=AXIS2_PLACEMENT_3D('',#80733,#42966,#42967);
#36020=AXIS2_PLACEMENT_3D('',#80734,#42968,#42969);
#36021=AXIS2_PLACEMENT_3D('',#80737,#42972,#42973);
#36022=AXIS2_PLACEMENT_3D('',#80739,#42974,#42975);
#36023=AXIS2_PLACEMENT_3D('',#80741,#42976,#42977);
#36024=AXIS2_PLACEMENT_3D('',#80742,#42978,#42979);
#36025=AXIS2_PLACEMENT_3D('',#80743,#42980,#42981);
#36026=AXIS2_PLACEMENT_3D('',#80747,#42983,#42984);
#36027=AXIS2_PLACEMENT_3D('',#80749,#42986,#42987);
#36028=AXIS2_PLACEMENT_3D('',#80751,#42988,#42989);
#36029=AXIS2_PLACEMENT_3D('',#80753,#42990,#42991);
#36030=AXIS2_PLACEMENT_3D('',#80760,#42992,#42993);
#36031=AXIS2_PLACEMENT_3D('',#80763,#42996,#42997);
#36032=AXIS2_PLACEMENT_3D('',#80776,#42998,#42999);
#36033=AXIS2_PLACEMENT_3D('',#80777,#43000,#43001);
#36034=AXIS2_PLACEMENT_3D('',#80778,#43002,#43003);
#36035=AXIS2_PLACEMENT_3D('',#80782,#43005,#43006);
#36036=AXIS2_PLACEMENT_3D('',#80784,#43008,#43009);
#36037=AXIS2_PLACEMENT_3D('',#80786,#43010,#43011);
#36038=AXIS2_PLACEMENT_3D('',#80787,#43012,#43013);
#36039=AXIS2_PLACEMENT_3D('',#80788,#43014,#43015);
#36040=AXIS2_PLACEMENT_3D('',#80790,#43017,#43018);
#36041=AXIS2_PLACEMENT_3D('',#80823,#43019,#43020);
#36042=AXIS2_PLACEMENT_3D('',#80824,#43021,#43022);
#36043=AXIS2_PLACEMENT_3D('',#80825,#43023,#43024);
#36044=AXIS2_PLACEMENT_3D('',#80826,#43025,#43026);
#36045=AXIS2_PLACEMENT_3D('',#80827,#43027,#43028);
#36046=AXIS2_PLACEMENT_3D('',#80877,#43029,#43030);
#36047=AXIS2_PLACEMENT_3D('',#80879,#43032,#43033);
#36048=AXIS2_PLACEMENT_3D('',#80880,#43034,#43035);
#36049=AXIS2_PLACEMENT_3D('',#80882,#43036,#43037);
#36050=AXIS2_PLACEMENT_3D('',#80883,#43038,#43039);
#36051=AXIS2_PLACEMENT_3D('',#80884,#43040,#43041);
#36052=AXIS2_PLACEMENT_3D('',#80886,#43043,#43044);
#36053=AXIS2_PLACEMENT_3D('',#80892,#43048,#43049);
#36054=AXIS2_PLACEMENT_3D('',#80895,#43051,#43052);
#36055=AXIS2_PLACEMENT_3D('',#80896,#43053,#43054);
#36056=AXIS2_PLACEMENT_3D('',#80898,#43055,#43056);
#36057=AXIS2_PLACEMENT_3D('',#80900,#43057,#43058);
#36058=AXIS2_PLACEMENT_3D('',#80901,#43059,#43060);
#36059=AXIS2_PLACEMENT_3D('',#80902,#43061,#43062);
#36060=AXIS2_PLACEMENT_3D('',#81067,#43066,#43067);
#36061=AXIS2_PLACEMENT_3D('',#81068,#43068,#43069);
#36062=AXIS2_PLACEMENT_3D('',#81238,#43070,#43071);
#36063=AXIS2_PLACEMENT_3D('',#81239,#43072,#43073);
#36064=AXIS2_PLACEMENT_3D('',#81240,#43074,#43075);
#36065=AXIS2_PLACEMENT_3D('',#81241,#43076,#43077);
#36066=AXIS2_PLACEMENT_3D('',#81379,#43079,#43080);
#36067=AXIS2_PLACEMENT_3D('',#81381,#43082,#43083);
#36068=AXIS2_PLACEMENT_3D('',#81383,#43085,#43086);
#36069=AXIS2_PLACEMENT_3D('',#81384,#43087,#43088);
#36070=AXIS2_PLACEMENT_3D('',#81521,#43089,#43090);
#36071=AXIS2_PLACEMENT_3D('',#81647,#43092,#43093);
#36072=AXIS2_PLACEMENT_3D('',#81650,#43095,#43096);
#36073=AXIS2_PLACEMENT_3D('',#81651,#43097,#43098);
#36074=AXIS2_PLACEMENT_3D('',#81655,#43101,#43102);
#36075=AXIS2_PLACEMENT_3D('',#81658,#43104,#43105);
#36076=AXIS2_PLACEMENT_3D('',#81659,#43106,#43107);
#36077=AXIS2_PLACEMENT_3D('',#81663,#43110,#43111);
#36078=AXIS2_PLACEMENT_3D('',#81666,#43113,#43114);
#36079=AXIS2_PLACEMENT_3D('',#81667,#43115,#43116);
#36080=AXIS2_PLACEMENT_3D('',#81671,#43119,#43120);
#36081=AXIS2_PLACEMENT_3D('',#81674,#43122,#43123);
#36082=AXIS2_PLACEMENT_3D('',#81675,#43124,#43125);
#36083=AXIS2_PLACEMENT_3D('',#81679,#43128,#43129);
#36084=AXIS2_PLACEMENT_3D('',#81682,#43131,#43132);
#36085=AXIS2_PLACEMENT_3D('',#81683,#43133,#43134);
#36086=AXIS2_PLACEMENT_3D('',#81687,#43137,#43138);
#36087=AXIS2_PLACEMENT_3D('',#81688,#43139,#43140);
#36088=AXIS2_PLACEMENT_3D('',#81689,#43141,#43142);
#36089=AXIS2_PLACEMENT_3D('',#81695,#43146,#43147);
#36090=AXIS2_PLACEMENT_3D('',#81696,#43148,#43149);
#36091=AXIS2_PLACEMENT_3D('',#81697,#43150,#43151);
#36092=AXIS2_PLACEMENT_3D('',#81703,#43155,#43156);
#36093=AXIS2_PLACEMENT_3D('',#81706,#43158,#43159);
#36094=AXIS2_PLACEMENT_3D('',#81707,#43160,#43161);
#36095=AXIS2_PLACEMENT_3D('',#81711,#43164,#43165);
#36096=AXIS2_PLACEMENT_3D('',#81712,#43166,#43167);
#36097=AXIS2_PLACEMENT_3D('',#81713,#43168,#43169);
#36098=AXIS2_PLACEMENT_3D('',#81719,#43173,#43174);
#36099=AXIS2_PLACEMENT_3D('',#81720,#43175,#43176);
#36100=AXIS2_PLACEMENT_3D('',#81721,#43177,#43178);
#36101=AXIS2_PLACEMENT_3D('',#81727,#43182,#43183);
#36102=AXIS2_PLACEMENT_3D('',#81730,#43185,#43186);
#36103=AXIS2_PLACEMENT_3D('',#81731,#43187,#43188);
#36104=AXIS2_PLACEMENT_3D('',#81733,#43190,#43191);
#36105=AXIS2_PLACEMENT_3D('',#81735,#43192,#43193);
#36106=AXIS2_PLACEMENT_3D('',#81737,#43195,#43196);
#36107=AXIS2_PLACEMENT_3D('',#81739,#43197,#43198);
#36108=AXIS2_PLACEMENT_3D('',#81741,#43199,#43200);
#36109=AXIS2_PLACEMENT_3D('',#81742,#43201,#43202);
#36110=AXIS2_PLACEMENT_3D('',#81810,#43203,#43204);
#36111=AXIS2_PLACEMENT_3D('',#81812,#43205,#43206);
#36112=AXIS2_PLACEMENT_3D('',#81814,#43208,#43209);
#36113=AXIS2_PLACEMENT_3D('',#81816,#43210,#43211);
#36114=AXIS2_PLACEMENT_3D('',#81818,#43212,#43213);
#36115=AXIS2_PLACEMENT_3D('',#81819,#43214,#43215);
#36116=AXIS2_PLACEMENT_3D('',#81820,#43216,#43217);
#36117=AXIS2_PLACEMENT_3D('',#81824,#43219,#43220);
#36118=AXIS2_PLACEMENT_3D('',#81828,#43222,#43223);
#36119=AXIS2_PLACEMENT_3D('',#81830,#43224,#43225);
#36120=AXIS2_PLACEMENT_3D('',#81832,#43226,#43227);
#36121=AXIS2_PLACEMENT_3D('',#81836,#43229,#43230);
#36122=AXIS2_PLACEMENT_3D('',#81839,#43232,#43233);
#36123=AXIS2_PLACEMENT_3D('',#81841,#43234,#43235);
#36124=AXIS2_PLACEMENT_3D('',#81888,#43236,#43237);
#36125=AXIS2_PLACEMENT_3D('',#81891,#43239,#43240);
#36126=AXIS2_PLACEMENT_3D('',#81892,#43241,#43242);
#36127=AXIS2_PLACEMENT_3D('',#81894,#43243,#43244);
#36128=AXIS2_PLACEMENT_3D('',#81896,#43245,#43246);
#36129=AXIS2_PLACEMENT_3D('',#81897,#43247,#43248);
#36130=AXIS2_PLACEMENT_3D('',#81965,#43249,#43250);
#36131=AXIS2_PLACEMENT_3D('',#82012,#43251,#43252);
#36132=AXIS2_PLACEMENT_3D('',#82013,#43253,#43254);
#36133=AXIS2_PLACEMENT_3D('',#82015,#43255,#43256);
#36134=AXIS2_PLACEMENT_3D('',#82017,#43257,#43258);
#36135=AXIS2_PLACEMENT_3D('',#82019,#43260,#43261);
#36136=AXIS2_PLACEMENT_3D('',#82021,#43262,#43263);
#36137=AXIS2_PLACEMENT_3D('',#82022,#43264,#43265);
#36138=AXIS2_PLACEMENT_3D('',#82023,#43266,#43267);
#36139=AXIS2_PLACEMENT_3D('',#82025,#43268,#43269);
#36140=AXIS2_PLACEMENT_3D('',#82027,#43271,#43272);
#36141=AXIS2_PLACEMENT_3D('',#82029,#43273,#43274);
#36142=AXIS2_PLACEMENT_3D('',#82030,#43275,#43276);
#36143=AXIS2_PLACEMENT_3D('',#82031,#43277,#43278);
#36144=AXIS2_PLACEMENT_3D('',#82033,#43279,#43280);
#36145=AXIS2_PLACEMENT_3D('',#82034,#43281,#43282);
#36146=AXIS2_PLACEMENT_3D('',#82035,#43283,#43284);
#36147=AXIS2_PLACEMENT_3D('',#82037,#43285,#43286);
#36148=AXIS2_PLACEMENT_3D('',#82039,#43288,#43289);
#36149=AXIS2_PLACEMENT_3D('',#82041,#43290,#43291);
#36150=AXIS2_PLACEMENT_3D('',#82042,#43292,#43293);
#36151=AXIS2_PLACEMENT_3D('',#82043,#43294,#43295);
#36152=AXIS2_PLACEMENT_3D('',#82045,#43296,#43297);
#36153=AXIS2_PLACEMENT_3D('',#82047,#43299,#43300);
#36154=AXIS2_PLACEMENT_3D('',#82049,#43301,#43302);
#36155=AXIS2_PLACEMENT_3D('',#82050,#43303,#43304);
#36156=AXIS2_PLACEMENT_3D('',#82051,#43305,#43306);
#36157=AXIS2_PLACEMENT_3D('',#82053,#43307,#43308);
#36158=AXIS2_PLACEMENT_3D('',#82055,#43310,#43311);
#36159=AXIS2_PLACEMENT_3D('',#82057,#43312,#43313);
#36160=AXIS2_PLACEMENT_3D('',#82058,#43314,#43315);
#36161=AXIS2_PLACEMENT_3D('',#82059,#43316,#43317);
#36162=AXIS2_PLACEMENT_3D('',#82061,#43318,#43319);
#36163=AXIS2_PLACEMENT_3D('',#82063,#43321,#43322);
#36164=AXIS2_PLACEMENT_3D('',#82065,#43323,#43324);
#36165=AXIS2_PLACEMENT_3D('',#82066,#43325,#43326);
#36166=AXIS2_PLACEMENT_3D('',#82067,#43327,#43328);
#36167=AXIS2_PLACEMENT_3D('',#82069,#43329,#43330);
#36168=AXIS2_PLACEMENT_3D('',#82071,#43332,#43333);
#36169=AXIS2_PLACEMENT_3D('',#82072,#43334,#43335);
#36170=AXIS2_PLACEMENT_3D('',#82073,#43336,#43337);
#36171=AXIS2_PLACEMENT_3D('',#82075,#43338,#43339);
#36172=AXIS2_PLACEMENT_3D('',#82077,#43341,#43342);
#36173=AXIS2_PLACEMENT_3D('',#82078,#43343,#43344);
#36174=AXIS2_PLACEMENT_3D('',#82079,#43345,#43346);
#36175=AXIS2_PLACEMENT_3D('',#82080,#43347,#43348);
#36176=AXIS2_PLACEMENT_3D('',#82082,#43349,#43350);
#36177=AXIS2_PLACEMENT_3D('',#82084,#43352,#43353);
#36178=AXIS2_PLACEMENT_3D('',#82085,#43354,#43355);
#36179=AXIS2_PLACEMENT_3D('',#82087,#43356,#43357);
#36180=AXIS2_PLACEMENT_3D('',#82088,#43358,#43359);
#36181=AXIS2_PLACEMENT_3D('',#82089,#43360,#43361);
#36182=AXIS2_PLACEMENT_3D('',#82091,#43362,#43363);
#36183=AXIS2_PLACEMENT_3D('',#82093,#43365,#43366);
#36184=AXIS2_PLACEMENT_3D('',#82094,#43367,#43368);
#36185=AXIS2_PLACEMENT_3D('',#82095,#43369,#43370);
#36186=AXIS2_PLACEMENT_3D('',#82097,#43371,#43372);
#36187=AXIS2_PLACEMENT_3D('',#82099,#43374,#43375);
#36188=AXIS2_PLACEMENT_3D('',#82100,#43376,#43377);
#36189=AXIS2_PLACEMENT_3D('',#82101,#43378,#43379);
#36190=AXIS2_PLACEMENT_3D('',#82102,#43380,#43381);
#36191=AXIS2_PLACEMENT_3D('',#82104,#43382,#43383);
#36192=AXIS2_PLACEMENT_3D('',#82106,#43385,#43386);
#36193=AXIS2_PLACEMENT_3D('',#82107,#43387,#43388);
#36194=AXIS2_PLACEMENT_3D('',#82109,#43389,#43390);
#36195=AXIS2_PLACEMENT_3D('',#82110,#43391,#43392);
#36196=AXIS2_PLACEMENT_3D('',#82111,#43393,#43394);
#36197=AXIS2_PLACEMENT_3D('',#82113,#43396,#43397);
#36198=AXIS2_PLACEMENT_3D('',#82115,#43398,#43399);
#36199=AXIS2_PLACEMENT_3D('',#82116,#43400,#43401);
#36200=AXIS2_PLACEMENT_3D('',#82117,#43402,#43403);
#36201=AXIS2_PLACEMENT_3D('',#82118,#43404,#43405);
#36202=AXIS2_PLACEMENT_3D('',#82120,#43406,#43407);
#36203=AXIS2_PLACEMENT_3D('',#82124,#43409,#43410);
#36204=AXIS2_PLACEMENT_3D('',#82125,#43411,#43412);
#36205=AXIS2_PLACEMENT_3D('',#82126,#43413,#43414);
#36206=AXIS2_PLACEMENT_3D('',#82130,#43417,#43418);
#36207=AXIS2_PLACEMENT_3D('',#82132,#43419,#43420);
#36208=AXIS2_PLACEMENT_3D('',#82133,#43421,#43422);
#36209=AXIS2_PLACEMENT_3D('',#82134,#43423,#43424);
#36210=AXIS2_PLACEMENT_3D('',#82136,#43425,#43426);
#36211=AXIS2_PLACEMENT_3D('',#82139,#43428,#43429);
#36212=AXIS2_PLACEMENT_3D('',#82140,#43430,#43431);
#36213=AXIS2_PLACEMENT_3D('',#82142,#43432,#43433);
#36214=AXIS2_PLACEMENT_3D('',#82143,#43434,#43435);
#36215=AXIS2_PLACEMENT_3D('',#82144,#43436,#43437);
#36216=AXIS2_PLACEMENT_3D('',#82146,#43438,#43439);
#36217=AXIS2_PLACEMENT_3D('',#82148,#43440,#43441);
#36218=AXIS2_PLACEMENT_3D('',#82149,#43442,#43443);
#36219=AXIS2_PLACEMENT_3D('',#82150,#43444,#43445);
#36220=AXIS2_PLACEMENT_3D('',#82152,#43447,#43448);
#36221=AXIS2_PLACEMENT_3D('',#82154,#43449,#43450);
#36222=AXIS2_PLACEMENT_3D('',#82155,#43451,#43452);
#36223=AXIS2_PLACEMENT_3D('',#82156,#43453,#43454);
#36224=AXIS2_PLACEMENT_3D('',#82158,#43455,#43456);
#36225=AXIS2_PLACEMENT_3D('',#82159,#43457,#43458);
#36226=AXIS2_PLACEMENT_3D('',#82160,#43459,#43460);
#36227=AXIS2_PLACEMENT_3D('',#82162,#43462,#43463);
#36228=AXIS2_PLACEMENT_3D('',#82164,#43464,#43465);
#36229=AXIS2_PLACEMENT_3D('',#82196,#43466,#43467);
#36230=AXIS2_PLACEMENT_3D('',#82198,#43468,#43469);
#36231=AXIS2_PLACEMENT_3D('',#82199,#43470,#43471);
#36232=AXIS2_PLACEMENT_3D('',#82200,#43472,#43473);
#36233=AXIS2_PLACEMENT_3D('',#82202,#43475,#43476);
#36234=AXIS2_PLACEMENT_3D('',#82204,#43477,#43478);
#36235=AXIS2_PLACEMENT_3D('',#82206,#43479,#43480);
#36236=AXIS2_PLACEMENT_3D('',#82207,#43481,#43482);
#36237=AXIS2_PLACEMENT_3D('',#82208,#43483,#43484);
#36238=AXIS2_PLACEMENT_3D('',#82209,#43485,#43486);
#36239=AXIS2_PLACEMENT_3D('',#82210,#43487,#43488);
#36240=AXIS2_PLACEMENT_3D('',#82214,#43491,#43492);
#36241=AXIS2_PLACEMENT_3D('',#82216,#43493,#43494);
#36242=AXIS2_PLACEMENT_3D('',#82218,#43495,#43496);
#36243=AXIS2_PLACEMENT_3D('',#82220,#43497,#43498);
#36244=AXIS2_PLACEMENT_3D('',#82221,#43499,#43500);
#36245=AXIS2_PLACEMENT_3D('',#82222,#43501,#43502);
#36246=AXIS2_PLACEMENT_3D('',#82223,#43503,#43504);
#36247=AXIS2_PLACEMENT_3D('',#82224,#43505,#43506);
#36248=AXIS2_PLACEMENT_3D('',#82225,#43507,#43508);
#36249=AXIS2_PLACEMENT_3D('',#82226,#43509,#43510);
#36250=AXIS2_PLACEMENT_3D('',#82228,#43511,#43512);
#36251=AXIS2_PLACEMENT_3D('',#82230,#43514,#43515);
#36252=AXIS2_PLACEMENT_3D('',#82233,#43517,#43518);
#36253=AXIS2_PLACEMENT_3D('',#82234,#43519,#43520);
#36254=AXIS2_PLACEMENT_3D('',#82236,#43521,#43522);
#36255=AXIS2_PLACEMENT_3D('',#82238,#43523,#43524);
#36256=AXIS2_PLACEMENT_3D('',#82239,#43525,#43526);
#36257=AXIS2_PLACEMENT_3D('',#82240,#43527,#43528);
#36258=AXIS2_PLACEMENT_3D('',#82245,#43531,#43532);
#36259=AXIS2_PLACEMENT_3D('',#82246,#43533,#43534);
#36260=AXIS2_PLACEMENT_3D('',#82248,#43535,#43536);
#36261=AXIS2_PLACEMENT_3D('',#82250,#43537,#43538);
#36262=AXIS2_PLACEMENT_3D('',#82251,#43539,#43540);
#36263=AXIS2_PLACEMENT_3D('',#82252,#43541,#43542);
#36264=AXIS2_PLACEMENT_3D('',#82257,#43545,#43546);
#36265=AXIS2_PLACEMENT_3D('',#82258,#43547,#43548);
#36266=AXIS2_PLACEMENT_3D('',#82259,#43549,#43550);
#36267=AXIS2_PLACEMENT_3D('',#82260,#43551,#43552);
#36268=AXIS2_PLACEMENT_3D('',#82263,#43555,#43556);
#36269=AXIS2_PLACEMENT_3D('',#82265,#43557,#43558);
#36270=AXIS2_PLACEMENT_3D('',#82266,#43559,#43560);
#36271=AXIS2_PLACEMENT_3D('',#82267,#43561,#43562);
#36272=AXIS2_PLACEMENT_3D('',#82269,#43564,#43565);
#36273=AXIS2_PLACEMENT_3D('',#82271,#43566,#43567);
#36274=AXIS2_PLACEMENT_3D('',#82272,#43568,#43569);
#36275=AXIS2_PLACEMENT_3D('',#82273,#43570,#43571);
#36276=AXIS2_PLACEMENT_3D('',#82274,#43572,#43573);
#36277=AXIS2_PLACEMENT_3D('',#82277,#43574,#43575);
#36278=AXIS2_PLACEMENT_3D('',#82279,#43576,#43577);
#36279=AXIS2_PLACEMENT_3D('',#82281,#43578,#43579);
#36280=AXIS2_PLACEMENT_3D('',#82282,#43580,#43581);
#36281=AXIS2_PLACEMENT_3D('',#82283,#43582,#43583);
#36282=AXIS2_PLACEMENT_3D('',#82287,#43585,#43586);
#36283=AXIS2_PLACEMENT_3D('',#82300,#43588,#43589);
#36284=AXIS2_PLACEMENT_3D('',#82302,#43590,#43591);
#36285=AXIS2_PLACEMENT_3D('',#82304,#43592,#43593);
#36286=AXIS2_PLACEMENT_3D('',#82305,#43594,#43595);
#36287=AXIS2_PLACEMENT_3D('',#82306,#43596,#43597);
#36288=AXIS2_PLACEMENT_3D('',#82436,#43600,#43601);
#36289=AXIS2_PLACEMENT_3D('',#82437,#43602,#43603);
#36290=AXIS2_PLACEMENT_3D('',#82439,#43605,#43606);
#36291=AXIS2_PLACEMENT_3D('',#82443,#43608,#43609);
#36292=AXIS2_PLACEMENT_3D('',#82445,#43611,#43612);
#36293=AXIS2_PLACEMENT_3D('',#82448,#43613,#43614);
#36294=AXIS2_PLACEMENT_3D('',#82450,#43615,#43616);
#36295=AXIS2_PLACEMENT_3D('',#82452,#43617,#43618);
#36296=AXIS2_PLACEMENT_3D('',#82453,#43619,#43620);
#36297=AXIS2_PLACEMENT_3D('',#82454,#43621,#43622);
#36298=AXIS2_PLACEMENT_3D('',#82459,#43625,#43626);
#36299=AXIS2_PLACEMENT_3D('',#82460,#43627,#43628);
#36300=AXIS2_PLACEMENT_3D('',#82462,#43629,#43630);
#36301=AXIS2_PLACEMENT_3D('',#82465,#43632,#43633);
#36302=AXIS2_PLACEMENT_3D('',#82469,#43635,#43636);
#36303=AXIS2_PLACEMENT_3D('',#82473,#43638,#43639);
#36304=AXIS2_PLACEMENT_3D('',#82477,#43641,#43642);
#36305=AXIS2_PLACEMENT_3D('',#82480,#43644,#43645);
#36306=AXIS2_PLACEMENT_3D('',#82481,#43646,#43647);
#36307=AXIS2_PLACEMENT_3D('',#82482,#43648,#43649);
#36308=AXIS2_PLACEMENT_3D('',#82483,#43650,#43651);
#36309=AXIS2_PLACEMENT_3D('',#82484,#43652,#43653);
#36310=AXIS2_PLACEMENT_3D('',#82485,#43654,#43655);
#36311=AXIS2_PLACEMENT_3D('',#82486,#43656,#43657);
#36312=AXIS2_PLACEMENT_3D('',#82487,#43658,#43659);
#36313=AXIS2_PLACEMENT_3D('',#82488,#43660,#43661);
#36314=AXIS2_PLACEMENT_3D('',#82538,#43662,#43663);
#36315=AXIS2_PLACEMENT_3D('',#82540,#43665,#43666);
#36316=AXIS2_PLACEMENT_3D('',#82542,#43668,#43669);
#36317=AXIS2_PLACEMENT_3D('',#82544,#43671,#43672);
#36318=AXIS2_PLACEMENT_3D('',#82617,#43676,#43677);
#36319=AXIS2_PLACEMENT_3D('',#82618,#43678,#43679);
#36320=AXIS2_PLACEMENT_3D('',#82619,#43680,#43681);
#36321=AXIS2_PLACEMENT_3D('',#82621,#43682,#43683);
#36322=AXIS2_PLACEMENT_3D('',#82622,#43684,#43685);
#36323=AXIS2_PLACEMENT_3D('',#82623,#43686,#43687);
#36324=AXIS2_PLACEMENT_3D('',#82626,#43689,#43690);
#36325=AXIS2_PLACEMENT_3D('',#82627,#43691,#43692);
#36326=AXIS2_PLACEMENT_3D('',#82629,#43693,#43694);
#36327=AXIS2_PLACEMENT_3D('',#82630,#43695,#43696);
#36328=AXIS2_PLACEMENT_3D('',#82631,#43697,#43698);
#36329=AXIS2_PLACEMENT_3D('',#82634,#43700,#43701);
#36330=AXIS2_PLACEMENT_3D('',#82635,#43702,#43703);
#36331=AXIS2_PLACEMENT_3D('',#82637,#43704,#43705);
#36332=AXIS2_PLACEMENT_3D('',#82638,#43706,#43707);
#36333=AXIS2_PLACEMENT_3D('',#82639,#43708,#43709);
#36334=AXIS2_PLACEMENT_3D('',#82642,#43711,#43712);
#36335=AXIS2_PLACEMENT_3D('',#82643,#43713,#43714);
#36336=AXIS2_PLACEMENT_3D('',#82644,#43715,#43716);
#36337=AXIS2_PLACEMENT_3D('',#82645,#43717,#43718);
#36338=AXIS2_PLACEMENT_3D('',#82666,#43721,#43722);
#36339=AXIS2_PLACEMENT_3D('',#82707,#43725,#43726);
#36340=AXIS2_PLACEMENT_3D('',#82709,#43728,#43729);
#36341=AXIS2_PLACEMENT_3D('',#82711,#43731,#43732);
#36342=AXIS2_PLACEMENT_3D('',#82713,#43734,#43735);
#36343=AXIS2_PLACEMENT_3D('',#82715,#43737,#43738);
#36344=AXIS2_PLACEMENT_3D('',#82716,#43739,#43740);
#36345=AXIS2_PLACEMENT_3D('',#82727,#43741,#43742);
#36346=AXIS2_PLACEMENT_3D('',#82728,#43743,#43744);
#36347=AXIS2_PLACEMENT_3D('',#82729,#43745,#43746);
#36348=AXIS2_PLACEMENT_3D('',#82731,#43747,#43748);
#36349=AXIS2_PLACEMENT_3D('',#82770,#43750,#43751);
#36350=AXIS2_PLACEMENT_3D('',#82912,#43752,#43753);
#36351=AXIS2_PLACEMENT_3D('',#82913,#43754,#43755);
#36352=AXIS2_PLACEMENT_3D('',#82914,#43756,#43757);
#36353=AXIS2_PLACEMENT_3D('',#82916,#43759,#43760);
#36354=AXIS2_PLACEMENT_3D('',#82919,#43762,#43763);
#36355=AXIS2_PLACEMENT_3D('',#82920,#43764,#43765);
#36356=AXIS2_PLACEMENT_3D('',#82923,#43767,#43768);
#36357=AXIS2_PLACEMENT_3D('',#82924,#43769,#43770);
#36358=AXIS2_PLACEMENT_3D('',#82927,#43772,#43773);
#36359=AXIS2_PLACEMENT_3D('',#82928,#43774,#43775);
#36360=AXIS2_PLACEMENT_3D('',#83028,#43776,#43777);
#36361=AXIS2_PLACEMENT_3D('',#83030,#43778,#43779);
#36362=AXIS2_PLACEMENT_3D('',#83165,#43780,#43781);
#36363=AXIS2_PLACEMENT_3D('',#83166,#43782,#43783);
#36364=AXIS2_PLACEMENT_3D('',#83203,#43784,#43785);
#36365=AXIS2_PLACEMENT_3D('',#83240,#43786,#43787);
#36366=AXIS2_PLACEMENT_3D('',#83277,#43788,#43789);
#36367=AXIS2_PLACEMENT_3D('',#83278,#43790,#43791);
#36368=AXIS2_PLACEMENT_3D('',#83280,#43793,#43794);
#36369=AXIS2_PLACEMENT_3D('',#83281,#43795,#43796);
#36370=AXIS2_PLACEMENT_3D('',#83312,#43797,#43798);
#36371=AXIS2_PLACEMENT_3D('',#83319,#43799,#43800);
#36372=AXIS2_PLACEMENT_3D('',#83326,#43801,#43802);
#36373=AXIS2_PLACEMENT_3D('',#83359,#43803,#43804);
#36374=AXIS2_PLACEMENT_3D('',#83396,#43805,#43806);
#36375=AXIS2_PLACEMENT_3D('',#83427,#43807,#43808);
#36376=AXIS2_PLACEMENT_3D('',#83430,#43809,#43810);
#36377=AXIS2_PLACEMENT_3D('',#83431,#43811,#43812);
#36378=AXIS2_PLACEMENT_3D('',#83434,#43814,#43815);
#36379=AXIS2_PLACEMENT_3D('',#83435,#43816,#43817);
#36380=AXIS2_PLACEMENT_3D('',#83438,#43818,#43819);
#36381=AXIS2_PLACEMENT_3D('',#83455,#43822,#43823);
#36382=AXIS2_PLACEMENT_3D('',#83470,#43826,#43827);
#36383=AXIS2_PLACEMENT_3D('',#83471,#43828,#43829);
#36384=AXIS2_PLACEMENT_3D('',#83473,#43830,#43831);
#36385=AXIS2_PLACEMENT_3D('',#83474,#43832,#43833);
#36386=AXIS2_PLACEMENT_3D('',#83479,#43835,#43836);
#36387=AXIS2_PLACEMENT_3D('',#83482,#43838,#43839);
#36388=AXIS2_PLACEMENT_3D('',#83483,#43840,#43841);
#36389=AXIS2_PLACEMENT_3D('',#83489,#43845,#43846);
#36390=AXIS2_PLACEMENT_3D('',#83495,#43850,#43851);
#36391=AXIS2_PLACEMENT_3D('',#83496,#43852,#43853);
#36392=AXIS2_PLACEMENT_3D('',#83497,#43854,#43855);
#36393=AXIS2_PLACEMENT_3D('',#83498,#43856,#43857);
#36394=AXIS2_PLACEMENT_3D('',#83503,#43859,#43860);
#36395=AXIS2_PLACEMENT_3D('',#83506,#43862,#43863);
#36396=AXIS2_PLACEMENT_3D('',#83507,#43864,#43865);
#36397=AXIS2_PLACEMENT_3D('',#83513,#43869,#43870);
#36398=AXIS2_PLACEMENT_3D('',#83519,#43874,#43875);
#36399=AXIS2_PLACEMENT_3D('',#83520,#43876,#43877);
#36400=AXIS2_PLACEMENT_3D('',#83521,#43878,#43879);
#36401=AXIS2_PLACEMENT_3D('',#83522,#43880,#43881);
#36402=AXIS2_PLACEMENT_3D('',#83525,#43882,#43883);
#36403=AXIS2_PLACEMENT_3D('',#83529,#43885,#43886);
#36404=AXIS2_PLACEMENT_3D('',#83533,#43888,#43889);
#36405=AXIS2_PLACEMENT_3D('',#83537,#43891,#43892);
#36406=AXIS2_PLACEMENT_3D('',#83541,#43894,#43895);
#36407=AXIS2_PLACEMENT_3D('',#83545,#43897,#43898);
#36408=AXIS2_PLACEMENT_3D('',#83560,#43900,#43901);
#36409=AXIS2_PLACEMENT_3D('',#83575,#43903,#43904);
#36410=AXIS2_PLACEMENT_3D('',#83590,#43906,#43907);
#36411=AXIS2_PLACEMENT_3D('',#83605,#43909,#43910);
#36412=AXIS2_PLACEMENT_3D('',#83620,#43912,#43913);
#36413=AXIS2_PLACEMENT_3D('',#83635,#43915,#43916);
#36414=AXIS2_PLACEMENT_3D('',#83639,#43918,#43919);
#36415=AXIS2_PLACEMENT_3D('',#83643,#43921,#43922);
#36416=AXIS2_PLACEMENT_3D('',#83647,#43924,#43925);
#36417=AXIS2_PLACEMENT_3D('',#83650,#43927,#43928);
#36418=AXIS2_PLACEMENT_3D('',#83652,#43929,#43930);
#36419=AXIS2_PLACEMENT_3D('',#83678,#43932,#43933);
#36420=AXIS2_PLACEMENT_3D('',#83704,#43935,#43936);
#36421=AXIS2_PLACEMENT_3D('',#83730,#43938,#43939);
#36422=AXIS2_PLACEMENT_3D('',#83754,#43941,#43942);
#36423=AXIS2_PLACEMENT_3D('',#83758,#43944,#43945);
#36424=AXIS2_PLACEMENT_3D('',#83784,#43947,#43948);
#36425=AXIS2_PLACEMENT_3D('',#83810,#43950,#43951);
#36426=AXIS2_PLACEMENT_3D('',#83836,#43953,#43954);
#36427=AXIS2_PLACEMENT_3D('',#83861,#43956,#43957);
#36428=AXIS2_PLACEMENT_3D('',#83862,#43958,#43959);
#36429=AXIS2_PLACEMENT_3D('',#83868,#43963,#43964);
#36430=AXIS2_PLACEMENT_3D('',#83874,#43968,#43969);
#36431=AXIS2_PLACEMENT_3D('',#83876,#43970,#43971);
#36432=AXIS2_PLACEMENT_3D('',#83878,#43972,#43973);
#36433=AXIS2_PLACEMENT_3D('',#83880,#43975,#43976);
#36434=AXIS2_PLACEMENT_3D('',#83881,#43977,#43978);
#36435=AXIS2_PLACEMENT_3D('',#83882,#43979,#43980);
#36436=AXIS2_PLACEMENT_3D('',#83883,#43981,#43982);
#36437=AXIS2_PLACEMENT_3D('',#83888,#43984,#43985);
#36438=AXIS2_PLACEMENT_3D('',#83891,#43987,#43988);
#36439=AXIS2_PLACEMENT_3D('',#83892,#43989,#43990);
#36440=AXIS2_PLACEMENT_3D('',#83896,#43992,#43993);
#36441=AXIS2_PLACEMENT_3D('',#83897,#43994,#43995);
#36442=AXIS2_PLACEMENT_3D('',#83898,#43996,#43997);
#36443=AXIS2_PLACEMENT_3D('',#83900,#43998,#43999);
#36444=AXIS2_PLACEMENT_3D('',#83903,#44001,#44002);
#36445=AXIS2_PLACEMENT_3D('',#83904,#44003,#44004);
#36446=AXIS2_PLACEMENT_3D('',#83907,#44007,#44008);
#36447=AXIS2_PLACEMENT_3D('',#83909,#44009,#44010);
#36448=AXIS2_PLACEMENT_3D('',#83911,#44011,#44012);
#36449=AXIS2_PLACEMENT_3D('',#83913,#44014,#44015);
#36450=AXIS2_PLACEMENT_3D('',#83915,#44017,#44018);
#36451=AXIS2_PLACEMENT_3D('',#83917,#44020,#44021);
#36452=AXIS2_PLACEMENT_3D('',#83920,#44022,#44023);
#36453=AXIS2_PLACEMENT_3D('',#83924,#44025,#44026);
#36454=AXIS2_PLACEMENT_3D('',#83926,#44028,#44029);
#36455=AXIS2_PLACEMENT_3D('',#83932,#44033,#44034);
#36456=AXIS2_PLACEMENT_3D('',#83934,#44035,#44036);
#36457=AXIS2_PLACEMENT_3D('',#83936,#44037,#44038);
#36458=AXIS2_PLACEMENT_3D('',#83965,#44040,#44041);
#36459=AXIS2_PLACEMENT_3D('',#83966,#44042,#44043);
#36460=AXIS2_PLACEMENT_3D('',#83967,#44044,#44045);
#36461=AXIS2_PLACEMENT_3D('',#83968,#44046,#44047);
#36462=AXIS2_PLACEMENT_3D('',#83971,#44050,#44051);
#36463=AXIS2_PLACEMENT_3D('',#83975,#44053,#44054);
#36464=AXIS2_PLACEMENT_3D('',#83979,#44057,#44058);
#36465=AXIS2_PLACEMENT_3D('',#83989,#44060,#44061);
#36466=AXIS2_PLACEMENT_3D('',#83990,#44062,#44063);
#36467=AXIS2_PLACEMENT_3D('',#83993,#44066,#44067);
#36468=AXIS2_PLACEMENT_3D('',#83995,#44068,#44069);
#36469=AXIS2_PLACEMENT_3D('',#83998,#44071,#44072);
#36470=AXIS2_PLACEMENT_3D('',#84054,#44073,#44074);
#36471=AXIS2_PLACEMENT_3D('',#84110,#44075,#44076);
#36472=AXIS2_PLACEMENT_3D('',#84131,#44078,#44079);
#36473=AXIS2_PLACEMENT_3D('',#84132,#44080,#44081);
#36474=AXIS2_PLACEMENT_3D('',#84133,#44082,#44083);
#36475=AXIS2_PLACEMENT_3D('',#84135,#44084,#44085);
#36476=AXIS2_PLACEMENT_3D('',#84177,#44086,#44087);
#36477=AXIS2_PLACEMENT_3D('',#84186,#44089,#44090);
#36478=AXIS2_PLACEMENT_3D('',#84274,#44092,#44093);
#36479=AXIS2_PLACEMENT_3D('',#84275,#44094,#44095);
#36480=AXIS2_PLACEMENT_3D('',#84277,#44096,#44097);
#36481=AXIS2_PLACEMENT_3D('',#84383,#44099,#44100);
#36482=AXIS2_PLACEMENT_3D('',#84415,#44101,#44102);
#36483=AXIS2_PLACEMENT_3D('',#84416,#44103,#44104);
#36484=AXIS2_PLACEMENT_3D('',#84417,#44105,#44106);
#36485=AXIS2_PLACEMENT_3D('',#84419,#44108,#44109);
#36486=AXIS2_PLACEMENT_3D('',#84421,#44111,#44112);
#36487=AXIS2_PLACEMENT_3D('',#84425,#44114,#44115);
#36488=AXIS2_PLACEMENT_3D('',#84426,#44116,#44117);
#36489=AXIS2_PLACEMENT_3D('',#84427,#44118,#44119);
#36490=AXIS2_PLACEMENT_3D('',#84429,#44120,#44121);
#36491=AXIS2_PLACEMENT_3D('',#84432,#44123,#44124);
#36492=AXIS2_PLACEMENT_3D('',#84433,#44125,#44126);
#36493=AXIS2_PLACEMENT_3D('',#84439,#44130,#44131);
#36494=AXIS2_PLACEMENT_3D('',#84443,#44133,#44134);
#36495=AXIS2_PLACEMENT_3D('',#84444,#44135,#44136);
#36496=AXIS2_PLACEMENT_3D('',#84471,#44137,#44138);
#36497=AXIS2_PLACEMENT_3D('',#84473,#44139,#44140);
#36498=AXIS2_PLACEMENT_3D('',#84474,#44141,#44142);
#36499=AXIS2_PLACEMENT_3D('',#84475,#44143,#44144);
#36500=AXIS2_PLACEMENT_3D('',#84477,#44146,#44147);
#36501=AXIS2_PLACEMENT_3D('',#84479,#44148,#44149);
#36502=AXIS2_PLACEMENT_3D('',#84480,#44150,#44151);
#36503=AXIS2_PLACEMENT_3D('',#84481,#44152,#44153);
#36504=AXIS2_PLACEMENT_3D('',#84483,#44155,#44156);
#36505=AXIS2_PLACEMENT_3D('',#84489,#44159,#44160);
#36506=AXIS2_PLACEMENT_3D('',#84491,#44162,#44163);
#36507=AXIS2_PLACEMENT_3D('',#84493,#44164,#44165);
#36508=AXIS2_PLACEMENT_3D('',#84496,#44167,#44168);
#36509=AXIS2_PLACEMENT_3D('',#84497,#44169,#44170);
#36510=AXIS2_PLACEMENT_3D('',#84500,#44173,#44174);
#36511=AXIS2_PLACEMENT_3D('',#84503,#44176,#44177);
#36512=AXIS2_PLACEMENT_3D('',#84504,#44178,#44179);
#36513=AXIS2_PLACEMENT_3D('',#84505,#44180,#44181);
#36514=AXIS2_PLACEMENT_3D('',#84506,#44182,#44183);
#36515=AXIS2_PLACEMENT_3D('',#84562,#44184,#44185);
#36516=AXIS2_PLACEMENT_3D('',#84563,#44186,#44187);
#36517=AXIS2_PLACEMENT_3D('',#84564,#44188,#44189);
#36518=AXIS2_PLACEMENT_3D('',#84585,#44191,#44192);
#36519=AXIS2_PLACEMENT_3D('',#84586,#44193,#44194);
#36520=AXIS2_PLACEMENT_3D('',#84587,#44195,#44196);
#36521=AXIS2_PLACEMENT_3D('',#84667,#44197,#44198);
#36522=AXIS2_PLACEMENT_3D('',#84668,#44199,#44200);
#36523=AXIS2_PLACEMENT_3D('',#84677,#44202,#44203);
#36524=AXIS2_PLACEMENT_3D('',#84734,#44205,#44206);
#36525=AXIS2_PLACEMENT_3D('',#84763,#44207,#44208);
#36526=AXIS2_PLACEMENT_3D('',#84766,#44210,#44211);
#36527=AXIS2_PLACEMENT_3D('',#84822,#44212,#44213);
#36528=AXIS2_PLACEMENT_3D('',#84903,#44214,#44215);
#36529=AXIS2_PLACEMENT_3D('',#84904,#44216,#44217);
#36530=AXIS2_PLACEMENT_3D('',#84905,#44218,#44219);
#36531=AXIS2_PLACEMENT_3D('',#84907,#44221,#44222);
#36532=AXIS2_PLACEMENT_3D('',#84909,#44224,#44225);
#36533=AXIS2_PLACEMENT_3D('',#84915,#44229,#44230);
#36534=AXIS2_PLACEMENT_3D('',#84921,#44234,#44235);
#36535=AXIS2_PLACEMENT_3D('',#84923,#44236,#44237);
#36536=AXIS2_PLACEMENT_3D('',#84925,#44238,#44239);
#36537=AXIS2_PLACEMENT_3D('',#84927,#44241,#44242);
#36538=AXIS2_PLACEMENT_3D('',#84928,#44243,#44244);
#36539=AXIS2_PLACEMENT_3D('',#84929,#44245,#44246);
#36540=AXIS2_PLACEMENT_3D('',#84930,#44247,#44248);
#36541=AXIS2_PLACEMENT_3D('',#84935,#44250,#44251);
#36542=AXIS2_PLACEMENT_3D('',#84938,#44253,#44254);
#36543=AXIS2_PLACEMENT_3D('',#84939,#44255,#44256);
#36544=AXIS2_PLACEMENT_3D('',#84943,#44258,#44259);
#36545=AXIS2_PLACEMENT_3D('',#84944,#44260,#44261);
#36546=AXIS2_PLACEMENT_3D('',#84945,#44262,#44263);
#36547=AXIS2_PLACEMENT_3D('',#84947,#44264,#44265);
#36548=AXIS2_PLACEMENT_3D('',#84950,#44267,#44268);
#36549=AXIS2_PLACEMENT_3D('',#84951,#44269,#44270);
#36550=AXIS2_PLACEMENT_3D('',#84954,#44273,#44274);
#36551=AXIS2_PLACEMENT_3D('',#84956,#44275,#44276);
#36552=AXIS2_PLACEMENT_3D('',#84958,#44277,#44278);
#36553=AXIS2_PLACEMENT_3D('',#84960,#44280,#44281);
#36554=AXIS2_PLACEMENT_3D('',#84962,#44283,#44284);
#36555=AXIS2_PLACEMENT_3D('',#84964,#44286,#44287);
#36556=AXIS2_PLACEMENT_3D('',#84967,#44290,#44291);
#36557=AXIS2_PLACEMENT_3D('',#84969,#44293,#44294);
#36558=AXIS2_PLACEMENT_3D('',#84971,#44296,#44297);
#36559=AXIS2_PLACEMENT_3D('',#84973,#44299,#44300);
#36560=AXIS2_PLACEMENT_3D('',#84975,#44302,#44303);
#36561=AXIS2_PLACEMENT_3D('',#84978,#44306,#44307);
#36562=AXIS2_PLACEMENT_3D('',#84980,#44309,#44310);
#36563=AXIS2_PLACEMENT_3D('',#84982,#44312,#44313);
#36564=AXIS2_PLACEMENT_3D('',#84984,#44315,#44316);
#36565=AXIS2_PLACEMENT_3D('',#84986,#44318,#44319);
#36566=AXIS2_PLACEMENT_3D('',#84988,#44321,#44322);
#36567=AXIS2_PLACEMENT_3D('',#84990,#44324,#44325);
#36568=AXIS2_PLACEMENT_3D('',#84991,#44326,#44327);
#36569=AXIS2_PLACEMENT_3D('',#84993,#44329,#44330);
#36570=AXIS2_PLACEMENT_3D('',#84995,#44332,#44333);
#36571=AXIS2_PLACEMENT_3D('',#84996,#44334,#44335);
#36572=AXIS2_PLACEMENT_3D('',#84998,#44336,#44337);
#36573=AXIS2_PLACEMENT_3D('',#85000,#44339,#44340);
#36574=AXIS2_PLACEMENT_3D('',#85001,#44341,#44342);
#36575=AXIS2_PLACEMENT_3D('',#85002,#44343,#44344);
#36576=AXIS2_PLACEMENT_3D('',#85003,#44345,#44346);
#36577=AXIS2_PLACEMENT_3D('',#85004,#44347,#44348);
#36578=AXIS2_PLACEMENT_3D('',#85005,#44349,#44350);
#36579=AXIS2_PLACEMENT_3D('',#85006,#44351,#44352);
#36580=AXIS2_PLACEMENT_3D('',#85009,#44353,#44354);
#36581=AXIS2_PLACEMENT_3D('',#85013,#44356,#44357);
#36582=AXIS2_PLACEMENT_3D('',#85017,#44359,#44360);
#36583=AXIS2_PLACEMENT_3D('',#85021,#44362,#44363);
#36584=AXIS2_PLACEMENT_3D('',#85025,#44365,#44366);
#36585=AXIS2_PLACEMENT_3D('',#85029,#44368,#44369);
#36586=AXIS2_PLACEMENT_3D('',#85031,#44371,#44372);
#36587=AXIS2_PLACEMENT_3D('',#85034,#44375,#44376);
#36588=AXIS2_PLACEMENT_3D('',#85036,#44378,#44379);
#36589=AXIS2_PLACEMENT_3D('',#85038,#44381,#44382);
#36590=AXIS2_PLACEMENT_3D('',#85041,#44384,#44385);
#36591=AXIS2_PLACEMENT_3D('',#85042,#44386,#44387);
#36592=AXIS2_PLACEMENT_3D('',#85075,#44389,#44390);
#36593=AXIS2_PLACEMENT_3D('',#85078,#44392,#44393);
#36594=AXIS2_PLACEMENT_3D('',#85079,#44394,#44395);
#36595=AXIS2_PLACEMENT_3D('',#85116,#44397,#44398);
#36596=AXIS2_PLACEMENT_3D('',#85119,#44400,#44401);
#36597=AXIS2_PLACEMENT_3D('',#85120,#44402,#44403);
#36598=AXIS2_PLACEMENT_3D('',#85153,#44405,#44406);
#36599=AXIS2_PLACEMENT_3D('',#85155,#44408,#44409);
#36600=AXIS2_PLACEMENT_3D('',#85156,#44410,#44411);
#36601=AXIS2_PLACEMENT_3D('',#85158,#44413,#44414);
#36602=AXIS2_PLACEMENT_3D('',#85187,#44415,#44416);
#36603=AXIS2_PLACEMENT_3D('',#85188,#44417,#44418);
#36604=AXIS2_PLACEMENT_3D('',#85210,#44419,#44420);
#36605=AXIS2_PLACEMENT_3D('',#85214,#44422,#44423);
#36606=AXIS2_PLACEMENT_3D('',#85216,#44425,#44426);
#36607=AXIS2_PLACEMENT_3D('',#85220,#44428,#44429);
#36608=AXIS2_PLACEMENT_3D('',#85222,#44430,#44431);
#36609=AXIS2_PLACEMENT_3D('',#85223,#44432,#44433);
#36610=AXIS2_PLACEMENT_3D('',#85224,#44434,#44435);
#36611=AXIS2_PLACEMENT_3D('',#85277,#44437,#44438);
#36612=AXIS2_PLACEMENT_3D('',#85278,#44439,#44440);
#36613=AXIS2_PLACEMENT_3D('',#85283,#44442,#44443);
#36614=AXIS2_PLACEMENT_3D('',#85301,#44445,#44446);
#36615=AXIS2_PLACEMENT_3D('',#85306,#44448,#44449);
#36616=AXIS2_PLACEMENT_3D('',#85309,#44451,#44452);
#36617=AXIS2_PLACEMENT_3D('',#85310,#44453,#44454);
#36618=AXIS2_PLACEMENT_3D('',#85316,#44458,#44459);
#36619=AXIS2_PLACEMENT_3D('',#85318,#44460,#44461);
#36620=AXIS2_PLACEMENT_3D('',#85321,#44463,#44464);
#36621=AXIS2_PLACEMENT_3D('',#85322,#44465,#44466);
#36622=AXIS2_PLACEMENT_3D('',#85326,#44468,#44469);
#36623=AXIS2_PLACEMENT_3D('',#85327,#44470,#44471);
#36624=AXIS2_PLACEMENT_3D('',#85328,#44472,#44473);
#36625=AXIS2_PLACEMENT_3D('',#85330,#44474,#44475);
#36626=AXIS2_PLACEMENT_3D('',#85391,#44478,#44479);
#36627=AXIS2_PLACEMENT_3D('',#85392,#44480,#44481);
#36628=AXIS2_PLACEMENT_3D('',#85398,#44484,#44485);
#36629=AXIS2_PLACEMENT_3D('',#85400,#44487,#44488);
#36630=AXIS2_PLACEMENT_3D('',#85457,#44490,#44491);
#36631=AXIS2_PLACEMENT_3D('',#85459,#44493,#44494);
#36632=AXIS2_PLACEMENT_3D('',#85460,#44495,#44496);
#36633=AXIS2_PLACEMENT_3D('',#85461,#44497,#44498);
#36634=AXIS2_PLACEMENT_3D('',#85463,#44499,#44500);
#36635=AXIS2_PLACEMENT_3D('',#85464,#44501,#44502);
#36636=AXIS2_PLACEMENT_3D('',#85465,#44503,#44504);
#36637=AXIS2_PLACEMENT_3D('',#85466,#44505,#44506);
#36638=AXIS2_PLACEMENT_3D('',#85467,#44507,#44508);
#36639=AXIS2_PLACEMENT_3D('',#85472,#44511,#44512);
#36640=AXIS2_PLACEMENT_3D('',#85473,#44513,#44514);
#36641=AXIS2_PLACEMENT_3D('',#85475,#44515,#44516);
#36642=AXIS2_PLACEMENT_3D('',#85477,#44517,#44518);
#36643=AXIS2_PLACEMENT_3D('',#85478,#44519,#44520);
#36644=AXIS2_PLACEMENT_3D('',#85479,#44521,#44522);
#36645=AXIS2_PLACEMENT_3D('',#85481,#44523,#44524);
#36646=AXIS2_PLACEMENT_3D('',#85482,#44525,#44526);
#36647=AXIS2_PLACEMENT_3D('',#85483,#44527,#44528);
#36648=AXIS2_PLACEMENT_3D('',#85484,#44529,#44530);
#36649=AXIS2_PLACEMENT_3D('',#85486,#44531,#44532);
#36650=AXIS2_PLACEMENT_3D('',#85487,#44533,#44534);
#36651=AXIS2_PLACEMENT_3D('',#85488,#44535,#44536);
#36652=AXIS2_PLACEMENT_3D('',#85490,#44537,#44538);
#36653=AXIS2_PLACEMENT_3D('',#85491,#44539,#44540);
#36654=AXIS2_PLACEMENT_3D('',#85492,#44541,#44542);
#36655=AXIS2_PLACEMENT_3D('',#85493,#44543,#44544);
#36656=AXIS2_PLACEMENT_3D('',#85495,#44545,#44546);
#36657=AXIS2_PLACEMENT_3D('',#85496,#44547,#44548);
#36658=AXIS2_PLACEMENT_3D('',#85497,#44549,#44550);
#36659=AXIS2_PLACEMENT_3D('',#85500,#44552,#44553);
#36660=AXIS2_PLACEMENT_3D('',#85501,#44554,#44555);
#36661=AXIS2_PLACEMENT_3D('',#85502,#44556,#44557);
#36662=AXIS2_PLACEMENT_3D('',#85503,#44558,#44559);
#36663=AXIS2_PLACEMENT_3D('',#85505,#44560,#44561);
#36664=AXIS2_PLACEMENT_3D('',#85506,#44562,#44563);
#36665=AXIS2_PLACEMENT_3D('',#85507,#44564,#44565);
#36666=AXIS2_PLACEMENT_3D('',#85508,#44566,#44567);
#36667=AXIS2_PLACEMENT_3D('',#85509,#44568,#44569);
#36668=AXIS2_PLACEMENT_3D('',#85555,#44571,#44572);
#36669=AXIS2_PLACEMENT_3D('',#85557,#44573,#44574);
#36670=AXIS2_PLACEMENT_3D('',#85558,#44575,#44576);
#36671=AXIS2_PLACEMENT_3D('',#85559,#44577,#44578);
#36672=AXIS2_PLACEMENT_3D('',#85616,#44585,#44586);
#36673=AXIS2_PLACEMENT_3D('',#85618,#44587,#44588);
#36674=AXIS2_PLACEMENT_3D('',#85621,#44590,#44591);
#36675=AXIS2_PLACEMENT_3D('',#85622,#44592,#44593);
#36676=AXIS2_PLACEMENT_3D('',#85626,#44595,#44596);
#36677=AXIS2_PLACEMENT_3D('',#85627,#44597,#44598);
#36678=AXIS2_PLACEMENT_3D('',#85628,#44599,#44600);
#36679=AXIS2_PLACEMENT_3D('',#85630,#44601,#44602);
#36680=AXIS2_PLACEMENT_3D('',#85633,#44604,#44605);
#36681=AXIS2_PLACEMENT_3D('',#85634,#44606,#44607);
#36682=AXIS2_PLACEMENT_3D('',#85640,#44611,#44612);
#36683=AXIS2_PLACEMENT_3D('',#85644,#44614,#44615);
#36684=AXIS2_PLACEMENT_3D('',#85682,#44616,#44617);
#36685=AXIS2_PLACEMENT_3D('',#85684,#44618,#44619);
#36686=AXIS2_PLACEMENT_3D('',#85686,#44620,#44621);
#36687=AXIS2_PLACEMENT_3D('',#85688,#44623,#44624);
#36688=AXIS2_PLACEMENT_3D('',#85692,#44626,#44627);
#36689=AXIS2_PLACEMENT_3D('',#85693,#44628,#44629);
#36690=AXIS2_PLACEMENT_3D('',#85694,#44630,#44631);
#36691=AXIS2_PLACEMENT_3D('',#85695,#44632,#44633);
#36692=AXIS2_PLACEMENT_3D('',#85696,#44634,#44635);
#36693=AXIS2_PLACEMENT_3D('',#85698,#44636,#44637);
#36694=AXIS2_PLACEMENT_3D('',#85699,#44638,#44639);
#36695=AXIS2_PLACEMENT_3D('',#85700,#44640,#44641);
#36696=AXIS2_PLACEMENT_3D('',#85701,#44642,#44643);
#36697=AXIS2_PLACEMENT_3D('',#85702,#44644,#44645);
#36698=AXIS2_PLACEMENT_3D('',#85705,#44647,#44648);
#36699=AXIS2_PLACEMENT_3D('',#85706,#44649,#44650);
#36700=AXIS2_PLACEMENT_3D('',#85708,#44651,#44652);
#36701=AXIS2_PLACEMENT_3D('',#85709,#44653,#44654);
#36702=AXIS2_PLACEMENT_3D('',#85710,#44655,#44656);
#36703=AXIS2_PLACEMENT_3D('',#85719,#44657,#44658);
#36704=AXIS2_PLACEMENT_3D('',#85720,#44659,#44660);
#36705=AXIS2_PLACEMENT_3D('',#85721,#44661,#44662);
#36706=AXIS2_PLACEMENT_3D('',#85722,#44663,#44664);
#36707=AXIS2_PLACEMENT_3D('',#85723,#44665,#44666);
#36708=AXIS2_PLACEMENT_3D('',#85820,#44667,#44668);
#36709=AXIS2_PLACEMENT_3D('',#85821,#44669,#44670);
#36710=AXIS2_PLACEMENT_3D('',#85822,#44671,#44672);
#36711=AXIS2_PLACEMENT_3D('',#85960,#44675,#44676);
#36712=AXIS2_PLACEMENT_3D('',#85962,#44677,#44678);
#36713=AXIS2_PLACEMENT_3D('',#86023,#44679,#44680);
#36714=AXIS2_PLACEMENT_3D('',#86024,#44681,#44682);
#36715=AXIS2_PLACEMENT_3D('',#86025,#44683,#44684);
#36716=AXIS2_PLACEMENT_3D('',#86077,#44687,#44688);
#36717=AXIS2_PLACEMENT_3D('',#86078,#44689,#44690);
#36718=AXIS2_PLACEMENT_3D('',#86081,#44691,#44692);
#36719=AXIS2_PLACEMENT_3D('',#86191,#44693,#44694);
#36720=AXIS2_PLACEMENT_3D('',#86192,#44695,#44696);
#36721=AXIS2_PLACEMENT_3D('',#86193,#44697,#44698);
#36722=AXIS2_PLACEMENT_3D('',#86194,#44699,#44700);
#36723=AXIS2_PLACEMENT_3D('',#86195,#44701,#44702);
#36724=AXIS2_PLACEMENT_3D('',#86201,#44706,#44707);
#36725=AXIS2_PLACEMENT_3D('',#86202,#44708,#44709);
#36726=AXIS2_PLACEMENT_3D('',#86203,#44710,#44711);
#36727=AXIS2_PLACEMENT_3D('',#86206,#44712,#44713);
#36728=AXIS2_PLACEMENT_3D('',#86209,#44716,#44717);
#36729=AXIS2_PLACEMENT_3D('',#86210,#44718,#44719);
#36730=AXIS2_PLACEMENT_3D('',#86211,#44720,#44721);
#36731=AXIS2_PLACEMENT_3D('',#86217,#44725,#44726);
#36732=AXIS2_PLACEMENT_3D('',#86218,#44727,#44728);
#36733=AXIS2_PLACEMENT_3D('',#86219,#44729,#44730);
#36734=AXIS2_PLACEMENT_3D('',#86224,#44733,#44734);
#36735=AXIS2_PLACEMENT_3D('',#86225,#44735,#44736);
#36736=AXIS2_PLACEMENT_3D('',#86226,#44737,#44738);
#36737=AXIS2_PLACEMENT_3D('',#86227,#44739,#44740);
#36738=AXIS2_PLACEMENT_3D('',#86229,#44741,#44742);
#36739=AXIS2_PLACEMENT_3D('',#86232,#44744,#44745);
#36740=AXIS2_PLACEMENT_3D('',#86233,#44746,#44747);
#36741=AXIS2_PLACEMENT_3D('',#86234,#44748,#44749);
#36742=AXIS2_PLACEMENT_3D('',#86235,#44750,#44751);
#36743=AXIS2_PLACEMENT_3D('',#86237,#44752,#44753);
#36744=AXIS2_PLACEMENT_3D('',#86239,#44754,#44755);
#36745=AXIS2_PLACEMENT_3D('',#86240,#44756,#44757);
#36746=AXIS2_PLACEMENT_3D('',#86241,#44758,#44759);
#36747=AXIS2_PLACEMENT_3D('',#86242,#44760,#44761);
#36748=AXIS2_PLACEMENT_3D('',#86243,#44762,#44763);
#36749=AXIS2_PLACEMENT_3D('',#86245,#44764,#44765);
#36750=AXIS2_PLACEMENT_3D('',#86248,#44767,#44768);
#36751=AXIS2_PLACEMENT_3D('',#86249,#44769,#44770);
#36752=AXIS2_PLACEMENT_3D('',#86250,#44771,#44772);
#36753=AXIS2_PLACEMENT_3D('',#86251,#44773,#44774);
#36754=AXIS2_PLACEMENT_3D('',#86253,#44775,#44776);
#36755=AXIS2_PLACEMENT_3D('',#86255,#44777,#44778);
#36756=AXIS2_PLACEMENT_3D('',#86256,#44779,#44780);
#36757=AXIS2_PLACEMENT_3D('',#86257,#44781,#44782);
#36758=AXIS2_PLACEMENT_3D('',#86258,#44783,#44784);
#36759=AXIS2_PLACEMENT_3D('',#86259,#44785,#44786);
#36760=AXIS2_PLACEMENT_3D('',#86262,#44787,#44788);
#36761=AXIS2_PLACEMENT_3D('',#86264,#44789,#44790);
#36762=AXIS2_PLACEMENT_3D('',#86265,#44791,#44792);
#36763=AXIS2_PLACEMENT_3D('',#86266,#44793,#44794);
#36764=AXIS2_PLACEMENT_3D('',#86267,#44795,#44796);
#36765=AXIS2_PLACEMENT_3D('',#86268,#44797,#44798);
#36766=AXIS2_PLACEMENT_3D('',#86269,#44799,#44800);
#36767=AXIS2_PLACEMENT_3D('',#86270,#44801,#44802);
#36768=AXIS2_PLACEMENT_3D('',#86271,#44803,#44804);
#36769=AXIS2_PLACEMENT_3D('',#86272,#44805,#44806);
#36770=AXIS2_PLACEMENT_3D('',#86282,#44807,#44808);
#36771=AXIS2_PLACEMENT_3D('',#86284,#44809,#44810);
#36772=AXIS2_PLACEMENT_3D('',#86285,#44811,#44812);
#36773=AXIS2_PLACEMENT_3D('',#86286,#44813,#44814);
#36774=AXIS2_PLACEMENT_3D('',#86349,#44815,#44816);
#36775=AXIS2_PLACEMENT_3D('',#86426,#44817,#44818);
#36776=AXIS2_PLACEMENT_3D('',#86428,#44819,#44820);
#36777=AXIS2_PLACEMENT_3D('',#86430,#44821,#44822);
#36778=AXIS2_PLACEMENT_3D('',#86431,#44823,#44824);
#36779=AXIS2_PLACEMENT_3D('',#86432,#44825,#44826);
#36780=AXIS2_PLACEMENT_3D('',#86441,#44831,#44832);
#36781=AXIS2_PLACEMENT_3D('',#86444,#44833,#44834);
#36782=AXIS2_PLACEMENT_3D('',#86507,#44836,#44837);
#36783=AXIS2_PLACEMENT_3D('',#86570,#44839,#44840);
#36784=AXIS2_PLACEMENT_3D('',#86574,#44842,#44843);
#36785=AXIS2_PLACEMENT_3D('',#86576,#44844,#44845);
#36786=AXIS2_PLACEMENT_3D('',#86618,#44847,#44848);
#36787=AXIS2_PLACEMENT_3D('',#86625,#44851,#44852);
#36788=AXIS2_PLACEMENT_3D('',#86629,#44855,#44856);
#36789=AXIS2_PLACEMENT_3D('',#86631,#44857,#44858);
#36790=AXIS2_PLACEMENT_3D('',#86674,#44860,#44861);
#36791=AXIS2_PLACEMENT_3D('',#86680,#44864,#44865);
#36792=AXIS2_PLACEMENT_3D('',#86683,#44867,#44868);
#36793=AXIS2_PLACEMENT_3D('',#86684,#44869,#44870);
#36794=AXIS2_PLACEMENT_3D('',#86686,#44871,#44872);
#36795=AXIS2_PLACEMENT_3D('',#86729,#44874,#44875);
#36796=AXIS2_PLACEMENT_3D('',#86743,#44879,#44880);
#36797=AXIS2_PLACEMENT_3D('',#86744,#44881,#44882);
#36798=AXIS2_PLACEMENT_3D('',#86745,#44883,#44884);
#36799=AXIS2_PLACEMENT_3D('',#86746,#44885,#44886);
#36800=AXIS2_PLACEMENT_3D('',#86747,#44887,#44888);
#36801=AXIS2_PLACEMENT_3D('',#86749,#44889,#44890);
#36802=AXIS2_PLACEMENT_3D('',#86750,#44891,#44892);
#36803=AXIS2_PLACEMENT_3D('',#86751,#44893,#44894);
#36804=AXIS2_PLACEMENT_3D('',#86753,#44895,#44896);
#36805=AXIS2_PLACEMENT_3D('',#86754,#44897,#44898);
#36806=AXIS2_PLACEMENT_3D('',#86755,#44899,#44900);
#36807=AXIS2_PLACEMENT_3D('',#86760,#44903,#44904);
#36808=AXIS2_PLACEMENT_3D('',#86761,#44905,#44906);
#36809=AXIS2_PLACEMENT_3D('',#86765,#44908,#44909);
#36810=AXIS2_PLACEMENT_3D('',#86773,#44914,#44915);
#36811=AXIS2_PLACEMENT_3D('',#86775,#44916,#44917);
#36812=AXIS2_PLACEMENT_3D('',#86778,#44919,#44920);
#36813=AXIS2_PLACEMENT_3D('',#86779,#44921,#44922);
#36814=AXIS2_PLACEMENT_3D('',#86781,#44923,#44924);
#36815=AXIS2_PLACEMENT_3D('',#86783,#44925,#44926);
#36816=AXIS2_PLACEMENT_3D('',#86785,#44928,#44929);
#36817=AXIS2_PLACEMENT_3D('',#86787,#44930,#44931);
#36818=AXIS2_PLACEMENT_3D('',#86790,#44933,#44934);
#36819=AXIS2_PLACEMENT_3D('',#86791,#44935,#44936);
#36820=AXIS2_PLACEMENT_3D('',#86797,#44940,#44941);
#36821=AXIS2_PLACEMENT_3D('',#86801,#44943,#44944);
#36822=AXIS2_PLACEMENT_3D('',#86808,#44945,#44946);
#36823=AXIS2_PLACEMENT_3D('',#86810,#44947,#44948);
#36824=AXIS2_PLACEMENT_3D('',#86813,#44950,#44951);
#36825=AXIS2_PLACEMENT_3D('',#86814,#44952,#44953);
#36826=AXIS2_PLACEMENT_3D('',#86815,#44954,#44955);
#36827=AXIS2_PLACEMENT_3D('',#86816,#44956,#44957);
#36828=AXIS2_PLACEMENT_3D('',#86817,#44958,#44959);
#36829=AXIS2_PLACEMENT_3D('',#86822,#44961,#44962);
#36830=AXIS2_PLACEMENT_3D('',#86824,#44964,#44965);
#36831=AXIS2_PLACEMENT_3D('',#86825,#44966,#44967);
#36832=AXIS2_PLACEMENT_3D('',#86828,#44968,#44969);
#36833=AXIS2_PLACEMENT_3D('',#86830,#44970,#44971);
#36834=AXIS2_PLACEMENT_3D('',#86832,#44972,#44973);
#36835=AXIS2_PLACEMENT_3D('',#86833,#44974,#44975);
#36836=AXIS2_PLACEMENT_3D('',#86834,#44976,#44977);
#36837=AXIS2_PLACEMENT_3D('',#86836,#44978,#44979);
#36838=AXIS2_PLACEMENT_3D('',#86838,#44980,#44981);
#36839=AXIS2_PLACEMENT_3D('',#86839,#44982,#44983);
#36840=AXIS2_PLACEMENT_3D('',#86840,#44984,#44985);
#36841=AXIS2_PLACEMENT_3D('',#86845,#44988,#44989);
#36842=AXIS2_PLACEMENT_3D('',#86846,#44990,#44991);
#36843=AXIS2_PLACEMENT_3D('',#86848,#44992,#44993);
#36844=AXIS2_PLACEMENT_3D('',#86850,#44994,#44995);
#36845=AXIS2_PLACEMENT_3D('',#86851,#44996,#44997);
#36846=AXIS2_PLACEMENT_3D('',#86852,#44998,#44999);
#36847=AXIS2_PLACEMENT_3D('',#86854,#45000,#45001);
#36848=AXIS2_PLACEMENT_3D('',#86856,#45002,#45003);
#36849=AXIS2_PLACEMENT_3D('',#86857,#45004,#45005);
#36850=AXIS2_PLACEMENT_3D('',#86858,#45006,#45007);
#36851=AXIS2_PLACEMENT_3D('',#86860,#45008,#45009);
#36852=AXIS2_PLACEMENT_3D('',#86862,#45010,#45011);
#36853=AXIS2_PLACEMENT_3D('',#86863,#45012,#45013);
#36854=AXIS2_PLACEMENT_3D('',#86864,#45014,#45015);
#36855=AXIS2_PLACEMENT_3D('',#86866,#45016,#45017);
#36856=AXIS2_PLACEMENT_3D('',#86868,#45018,#45019);
#36857=AXIS2_PLACEMENT_3D('',#86869,#45020,#45021);
#36858=AXIS2_PLACEMENT_3D('',#86870,#45022,#45023);
#36859=AXIS2_PLACEMENT_3D('',#86873,#45026,#45027);
#36860=AXIS2_PLACEMENT_3D('',#86876,#45028,#45029);
#36861=AXIS2_PLACEMENT_3D('',#86878,#45030,#45031);
#36862=AXIS2_PLACEMENT_3D('',#86880,#45032,#45033);
#36863=AXIS2_PLACEMENT_3D('',#86881,#45034,#45035);
#36864=AXIS2_PLACEMENT_3D('',#86919,#45036,#45037);
#36865=AXIS2_PLACEMENT_3D('',#86925,#45038,#45039);
#36866=AXIS2_PLACEMENT_3D('',#86926,#45040,#45041);
#36867=AXIS2_PLACEMENT_3D('',#86927,#45042,#45043);
#36868=AXIS2_PLACEMENT_3D('',#86929,#45044,#45045);
#36869=AXIS2_PLACEMENT_3D('',#86930,#45046,#45047);
#36870=AXIS2_PLACEMENT_3D('',#86968,#45048,#45049);
#36871=AXIS2_PLACEMENT_3D('',#86970,#45050,#45051);
#36872=AXIS2_PLACEMENT_3D('',#86971,#45052,#45053);
#36873=AXIS2_PLACEMENT_3D('',#87009,#45054,#45055);
#36874=AXIS2_PLACEMENT_3D('',#87068,#45056,#45057);
#36875=AXIS2_PLACEMENT_3D('',#87069,#45058,#45059);
#36876=AXIS2_PLACEMENT_3D('',#87071,#45060,#45061);
#36877=AXIS2_PLACEMENT_3D('',#87073,#45062,#45063);
#36878=AXIS2_PLACEMENT_3D('',#87074,#45064,#45065);
#36879=AXIS2_PLACEMENT_3D('',#87075,#45066,#45067);
#36880=AXIS2_PLACEMENT_3D('',#87077,#45068,#45069);
#36881=AXIS2_PLACEMENT_3D('',#87079,#45070,#45071);
#36882=AXIS2_PLACEMENT_3D('',#87080,#45072,#45073);
#36883=AXIS2_PLACEMENT_3D('',#87081,#45074,#45075);
#36884=AXIS2_PLACEMENT_3D('',#87083,#45076,#45077);
#36885=AXIS2_PLACEMENT_3D('',#87085,#45078,#45079);
#36886=AXIS2_PLACEMENT_3D('',#87086,#45080,#45081);
#36887=AXIS2_PLACEMENT_3D('',#87087,#45082,#45083);
#36888=AXIS2_PLACEMENT_3D('',#87127,#45086,#45087);
#36889=AXIS2_PLACEMENT_3D('',#87129,#45088,#45089);
#36890=AXIS2_PLACEMENT_3D('',#87130,#45090,#45091);
#36891=AXIS2_PLACEMENT_3D('',#87168,#45092,#45093);
#36892=AXIS2_PLACEMENT_3D('',#87234,#45094,#45095);
#36893=AXIS2_PLACEMENT_3D('',#87235,#45096,#45097);
#36894=AXIS2_PLACEMENT_3D('',#87236,#45098,#45099);
#36895=AXIS2_PLACEMENT_3D('',#87238,#45100,#45101);
#36896=AXIS2_PLACEMENT_3D('',#87240,#45102,#45103);
#36897=AXIS2_PLACEMENT_3D('',#87242,#45104,#45105);
#36898=AXIS2_PLACEMENT_3D('',#87244,#45106,#45107);
#36899=AXIS2_PLACEMENT_3D('',#87245,#45108,#45109);
#36900=AXIS2_PLACEMENT_3D('',#87246,#45110,#45111);
#36901=AXIS2_PLACEMENT_3D('',#87248,#45112,#45113);
#36902=AXIS2_PLACEMENT_3D('',#87250,#45114,#45115);
#36903=AXIS2_PLACEMENT_3D('',#87251,#45116,#45117);
#36904=AXIS2_PLACEMENT_3D('',#87252,#45118,#45119);
#36905=AXIS2_PLACEMENT_3D('',#87257,#45122,#45123);
#36906=AXIS2_PLACEMENT_3D('',#87258,#45124,#45125);
#36907=AXIS2_PLACEMENT_3D('',#87260,#45126,#45127);
#36908=AXIS2_PLACEMENT_3D('',#87262,#45128,#45129);
#36909=AXIS2_PLACEMENT_3D('',#87263,#45130,#45131);
#36910=AXIS2_PLACEMENT_3D('',#87264,#45132,#45133);
#36911=AXIS2_PLACEMENT_3D('',#87266,#45134,#45135);
#36912=AXIS2_PLACEMENT_3D('',#87268,#45136,#45137);
#36913=AXIS2_PLACEMENT_3D('',#87269,#45138,#45139);
#36914=AXIS2_PLACEMENT_3D('',#87270,#45140,#45141);
#36915=AXIS2_PLACEMENT_3D('',#87272,#45142,#45143);
#36916=AXIS2_PLACEMENT_3D('',#87274,#45144,#45145);
#36917=AXIS2_PLACEMENT_3D('',#87275,#45146,#45147);
#36918=AXIS2_PLACEMENT_3D('',#87276,#45148,#45149);
#36919=AXIS2_PLACEMENT_3D('',#87278,#45150,#45151);
#36920=AXIS2_PLACEMENT_3D('',#87280,#45152,#45153);
#36921=AXIS2_PLACEMENT_3D('',#87281,#45154,#45155);
#36922=AXIS2_PLACEMENT_3D('',#87282,#45156,#45157);
#36923=AXIS2_PLACEMENT_3D('',#87285,#45160,#45161);
#36924=AXIS2_PLACEMENT_3D('',#87290,#45163,#45164);
#36925=AXIS2_PLACEMENT_3D('',#87372,#45166,#45167);
#36926=AXIS2_PLACEMENT_3D('',#87438,#45170,#45171);
#36927=AXIS2_PLACEMENT_3D('',#87441,#45172,#45173);
#36928=AXIS2_PLACEMENT_3D('',#87544,#45174,#45175);
#36929=AXIS2_PLACEMENT_3D('',#87545,#45176,#45177);
#36930=AXIS2_PLACEMENT_3D('',#87546,#45178,#45179);
#36931=AXIS2_PLACEMENT_3D('',#87548,#45180,#45181);
#36932=AXIS2_PLACEMENT_3D('',#87549,#45182,#45183);
#36933=AXIS2_PLACEMENT_3D('',#87550,#45184,#45185);
#36934=AXIS2_PLACEMENT_3D('',#87552,#45186,#45187);
#36935=AXIS2_PLACEMENT_3D('',#87554,#45188,#45189);
#36936=AXIS2_PLACEMENT_3D('',#87628,#45190,#45191);
#36937=AXIS2_PLACEMENT_3D('',#87630,#45192,#45193);
#36938=AXIS2_PLACEMENT_3D('',#87631,#45194,#45195);
#36939=AXIS2_PLACEMENT_3D('',#87632,#45196,#45197);
#36940=AXIS2_PLACEMENT_3D('',#87634,#45198,#45199);
#36941=AXIS2_PLACEMENT_3D('',#87635,#45200,#45201);
#36942=AXIS2_PLACEMENT_3D('',#87636,#45202,#45203);
#36943=AXIS2_PLACEMENT_3D('',#87638,#45204,#45205);
#36944=AXIS2_PLACEMENT_3D('',#87639,#45206,#45207);
#36945=AXIS2_PLACEMENT_3D('',#87640,#45208,#45209);
#36946=AXIS2_PLACEMENT_3D('',#87643,#45212,#45213);
#36947=AXIS2_PLACEMENT_3D('',#87645,#45214,#45215);
#36948=AXIS2_PLACEMENT_3D('',#87647,#45216,#45217);
#36949=AXIS2_PLACEMENT_3D('',#87648,#45218,#45219);
#36950=AXIS2_PLACEMENT_3D('',#87649,#45220,#45221);
#36951=AXIS2_PLACEMENT_3D('',#87651,#45222,#45223);
#36952=AXIS2_PLACEMENT_3D('',#87653,#45224,#45225);
#36953=AXIS2_PLACEMENT_3D('',#87654,#45226,#45227);
#36954=AXIS2_PLACEMENT_3D('',#87655,#45228,#45229);
#36955=AXIS2_PLACEMENT_3D('',#87657,#45230,#45231);
#36956=AXIS2_PLACEMENT_3D('',#87659,#45232,#45233);
#36957=AXIS2_PLACEMENT_3D('',#87660,#45234,#45235);
#36958=AXIS2_PLACEMENT_3D('',#87661,#45236,#45237);
#36959=AXIS2_PLACEMENT_3D('',#87663,#45238,#45239);
#36960=AXIS2_PLACEMENT_3D('',#87665,#45240,#45241);
#36961=AXIS2_PLACEMENT_3D('',#87666,#45242,#45243);
#36962=AXIS2_PLACEMENT_3D('',#87667,#45244,#45245);
#36963=AXIS2_PLACEMENT_3D('',#87669,#45246,#45247);
#36964=AXIS2_PLACEMENT_3D('',#87671,#45248,#45249);
#36965=AXIS2_PLACEMENT_3D('',#87672,#45250,#45251);
#36966=AXIS2_PLACEMENT_3D('',#87673,#45252,#45253);
#36967=AXIS2_PLACEMENT_3D('',#87675,#45254,#45255);
#36968=AXIS2_PLACEMENT_3D('',#87676,#45256,#45257);
#36969=AXIS2_PLACEMENT_3D('',#87677,#45258,#45259);
#36970=AXIS2_PLACEMENT_3D('',#87680,#45260,#45261);
#36971=AXIS2_PLACEMENT_3D('',#87683,#45264,#45265);
#36972=AXIS2_PLACEMENT_3D('',#87684,#45266,#45267);
#36973=AXIS2_PLACEMENT_3D('',#87685,#45268,#45269);
#36974=AXIS2_PLACEMENT_3D('',#87688,#45270,#45271);
#36975=AXIS2_PLACEMENT_3D('',#87725,#45272,#45273);
#36976=AXIS2_PLACEMENT_3D('',#87730,#45275,#45276);
#36977=AXIS2_PLACEMENT_3D('',#87733,#45278,#45279);
#36978=AXIS2_PLACEMENT_3D('',#87734,#45280,#45281);
#36979=AXIS2_PLACEMENT_3D('',#87736,#45282,#45283);
#36980=AXIS2_PLACEMENT_3D('',#87796,#45284,#45285);
#36981=AXIS2_PLACEMENT_3D('',#87797,#45286,#45287);
#36982=AXIS2_PLACEMENT_3D('',#87800,#45288,#45289);
#36983=AXIS2_PLACEMENT_3D('',#87801,#45290,#45291);
#36984=AXIS2_PLACEMENT_3D('',#87802,#45292,#45293);
#36985=AXIS2_PLACEMENT_3D('',#87805,#45294,#45295);
#36986=AXIS2_PLACEMENT_3D('',#87806,#45296,#45297);
#36987=AXIS2_PLACEMENT_3D('',#87807,#45298,#45299);
#36988=AXIS2_PLACEMENT_3D('',#87808,#45300,#45301);
#36989=AXIS2_PLACEMENT_3D('',#87811,#45302,#45303);
#36990=AXIS2_PLACEMENT_3D('',#87813,#45304,#45305);
#36991=AXIS2_PLACEMENT_3D('',#87815,#45306,#45307);
#36992=AXIS2_PLACEMENT_3D('',#87816,#45308,#45309);
#36993=AXIS2_PLACEMENT_3D('',#87817,#45310,#45311);
#36994=AXIS2_PLACEMENT_3D('',#87911,#45312,#45313);
#36995=AXIS2_PLACEMENT_3D('',#87912,#45314,#45315);
#36996=AXIS2_PLACEMENT_3D('',#87913,#45316,#45317);
#36997=AXIS2_PLACEMENT_3D('',#87974,#45318,#45319);
#36998=AXIS2_PLACEMENT_3D('',#87975,#45320,#45321);
#36999=AXIS2_PLACEMENT_3D('',#87976,#45322,#45323);
#37000=AXIS2_PLACEMENT_3D('',#87977,#45324,#45325);
#37001=AXIS2_PLACEMENT_3D('',#87979,#45326,#45327);
#37002=AXIS2_PLACEMENT_3D('',#87982,#45329,#45330);
#37003=AXIS2_PLACEMENT_3D('',#87983,#45331,#45332);
#37004=AXIS2_PLACEMENT_3D('',#87984,#45333,#45334);
#37005=AXIS2_PLACEMENT_3D('',#87985,#45335,#45336);
#37006=AXIS2_PLACEMENT_3D('',#87986,#45337,#45338);
#37007=AXIS2_PLACEMENT_3D('',#87987,#45339,#45340);
#37008=AXIS2_PLACEMENT_3D('',#87988,#45341,#45342);
#37009=AXIS2_PLACEMENT_3D('',#87989,#45343,#45344);
#37010=AXIS2_PLACEMENT_3D('',#87990,#45345,#45346);
#37011=AXIS2_PLACEMENT_3D('',#88124,#45348,#45349);
#37012=AXIS2_PLACEMENT_3D('',#88125,#45350,#45351);
#37013=AXIS2_PLACEMENT_3D('',#88126,#45352,#45353);
#37014=AXIS2_PLACEMENT_3D('',#88127,#45354,#45355);
#37015=AXIS2_PLACEMENT_3D('',#88223,#45356,#45357);
#37016=AXIS2_PLACEMENT_3D('',#88224,#45358,#45359);
#37017=AXIS2_PLACEMENT_3D('',#88225,#45360,#45361);
#37018=AXIS2_PLACEMENT_3D('',#88226,#45362,#45363);
#37019=AXIS2_PLACEMENT_3D('',#88228,#45365,#45366);
#37020=AXIS2_PLACEMENT_3D('',#88230,#45368,#45369);
#37021=AXIS2_PLACEMENT_3D('',#88231,#45370,#45371);
#37022=AXIS2_PLACEMENT_3D('',#88233,#45372,#45373);
#37023=AXIS2_PLACEMENT_3D('',#88234,#45374,#45375);
#37024=AXIS2_PLACEMENT_3D('',#88236,#45376,#45377);
#37025=AXIS2_PLACEMENT_3D('',#88237,#45378,#45379);
#37026=AXIS2_PLACEMENT_3D('',#88240,#45381,#45382);
#37027=AXIS2_PLACEMENT_3D('',#88242,#45384,#45385);
#37028=AXIS2_PLACEMENT_3D('',#88246,#45387,#45388);
#37029=AXIS2_PLACEMENT_3D('',#88248,#45390,#45391);
#37030=AXIS2_PLACEMENT_3D('',#88315,#45393,#45394);
#37031=AXIS2_PLACEMENT_3D('',#88356,#45395,#45396);
#37032=AXIS2_PLACEMENT_3D('',#88358,#45397,#45398);
#37033=AXIS2_PLACEMENT_3D('',#88360,#45399,#45400);
#37034=AXIS2_PLACEMENT_3D('',#88388,#45403,#45404);
#37035=AXIS2_PLACEMENT_3D('',#88390,#45405,#45406);
#37036=AXIS2_PLACEMENT_3D('',#88392,#45407,#45408);
#37037=AXIS2_PLACEMENT_3D('',#88394,#45410,#45411);
#37038=AXIS2_PLACEMENT_3D('',#88395,#45412,#45413);
#37039=AXIS2_PLACEMENT_3D('',#88396,#45414,#45415);
#37040=AXIS2_PLACEMENT_3D('',#88398,#45416,#45417);
#37041=AXIS2_PLACEMENT_3D('',#88399,#45418,#45419);
#37042=AXIS2_PLACEMENT_3D('',#88428,#45420,#45421);
#37043=AXIS2_PLACEMENT_3D('',#88429,#45422,#45423);
#37044=AXIS2_PLACEMENT_3D('',#88431,#45424,#45425);
#37045=AXIS2_PLACEMENT_3D('',#88432,#45426,#45427);
#37046=AXIS2_PLACEMENT_3D('',#88433,#45428,#45429);
#37047=AXIS2_PLACEMENT_3D('',#88436,#45431,#45432);
#37048=AXIS2_PLACEMENT_3D('',#88437,#45433,#45434);
#37049=AXIS2_PLACEMENT_3D('',#88438,#45435,#45436);
#37050=AXIS2_PLACEMENT_3D('',#88439,#45437,#45438);
#37051=AXIS2_PLACEMENT_3D('',#88441,#45439,#45440);
#37052=AXIS2_PLACEMENT_3D('',#88442,#45441,#45442);
#37053=AXIS2_PLACEMENT_3D('',#88443,#45443,#45444);
#37054=AXIS2_PLACEMENT_3D('',#88444,#45445,#45446);
#37055=AXIS2_PLACEMENT_3D('',#88445,#45447,#45448);
#37056=AXIS2_PLACEMENT_3D('',#88446,#45449,#45450);
#37057=AXIS2_PLACEMENT_3D('',#88447,#45451,#45452);
#37058=AXIS2_PLACEMENT_3D('',#88448,#45453,#45454);
#37059=AXIS2_PLACEMENT_3D('',#88449,#45455,#45456);
#37060=AXIS2_PLACEMENT_3D('',#88455,#45460,#45461);
#37061=AXIS2_PLACEMENT_3D('',#88458,#45464,#45465);
#37062=AXIS2_PLACEMENT_3D('',#88460,#45466,#45467);
#37063=AXIS2_PLACEMENT_3D('',#88462,#45469,#45470);
#37064=AXIS2_PLACEMENT_3D('',#88466,#45473,#45474);
#37065=AXIS2_PLACEMENT_3D('',#88468,#45475,#45476);
#37066=AXIS2_PLACEMENT_3D('',#88470,#45478,#45479);
#37067=AXIS2_PLACEMENT_3D('',#88471,#45480,#45481);
#37068=AXIS2_PLACEMENT_3D('',#88473,#45483,#45484);
#37069=AXIS2_PLACEMENT_3D('',#88475,#45486,#45487);
#37070=AXIS2_PLACEMENT_3D('',#88477,#45489,#45490);
#37071=AXIS2_PLACEMENT_3D('',#88478,#45491,#45492);
#37072=AXIS2_PLACEMENT_3D('',#88481,#45495,#45496);
#37073=AXIS2_PLACEMENT_3D('',#88483,#45498,#45499);
#37074=AXIS2_PLACEMENT_3D('',#88485,#45501,#45502);
#37075=AXIS2_PLACEMENT_3D('',#88487,#45504,#45505);
#37076=AXIS2_PLACEMENT_3D('',#88489,#45507,#45508);
#37077=AXIS2_PLACEMENT_3D('',#88490,#45509,#45510);
#37078=AXIS2_PLACEMENT_3D('',#88493,#45513,#45514);
#37079=AXIS2_PLACEMENT_3D('',#88495,#45516,#45517);
#37080=AXIS2_PLACEMENT_3D('',#88497,#45519,#45520);
#37081=AXIS2_PLACEMENT_3D('',#88499,#45521,#45522);
#37082=AXIS2_PLACEMENT_3D('',#88501,#45524,#45525);
#37083=AXIS2_PLACEMENT_3D('',#88503,#45526,#45527);
#37084=AXIS2_PLACEMENT_3D('',#88505,#45529,#45530);
#37085=AXIS2_PLACEMENT_3D('',#88508,#45532,#45533);
#37086=AXIS2_PLACEMENT_3D('',#88509,#45534,#45535);
#37087=AXIS2_PLACEMENT_3D('',#88511,#45536,#45537);
#37088=AXIS2_PLACEMENT_3D('',#88513,#45539,#45540);
#37089=AXIS2_PLACEMENT_3D('',#88515,#45542,#45543);
#37090=AXIS2_PLACEMENT_3D('',#88516,#45544,#45545);
#37091=AXIS2_PLACEMENT_3D('',#88517,#45546,#45547);
#37092=AXIS2_PLACEMENT_3D('',#88519,#45548,#45549);
#37093=AXIS2_PLACEMENT_3D('',#88578,#45550,#45551);
#37094=AXIS2_PLACEMENT_3D('',#88579,#45552,#45553);
#37095=AXIS2_PLACEMENT_3D('',#88580,#45554,#45555);
#37096=AXIS2_PLACEMENT_3D('',#88581,#45556,#45557);
#37097=AXIS2_PLACEMENT_3D('',#88582,#45558,#45559);
#37098=AXIS2_PLACEMENT_3D('',#88584,#45561,#45562);
#37099=AXIS2_PLACEMENT_3D('',#88587,#45564,#45565);
#37100=AXIS2_PLACEMENT_3D('',#88588,#45566,#45567);
#37101=AXIS2_PLACEMENT_3D('',#88589,#45568,#45569);
#37102=AXIS2_PLACEMENT_3D('',#88591,#45570,#45571);
#37103=AXIS2_PLACEMENT_3D('',#88593,#45572,#45573);
#37104=AXIS2_PLACEMENT_3D('',#88594,#45574,#45575);
#37105=AXIS2_PLACEMENT_3D('',#88595,#45576,#45577);
#37106=AXIS2_PLACEMENT_3D('',#88596,#45578,#45579);
#37107=AXIS2_PLACEMENT_3D('',#88597,#45580,#45581);
#37108=AXIS2_PLACEMENT_3D('',#88599,#45583,#45584);
#37109=AXIS2_PLACEMENT_3D('',#88600,#45585,#45586);
#37110=AXIS2_PLACEMENT_3D('',#88601,#45587,#45588);
#37111=AXIS2_PLACEMENT_3D('',#88602,#45589,#45590);
#37112=AXIS2_PLACEMENT_3D('',#88603,#45591,#45592);
#37113=AXIS2_PLACEMENT_3D('',#88683,#45593,#45594);
#37114=AXIS2_PLACEMENT_3D('',#88684,#45595,#45596);
#37115=AXIS2_PLACEMENT_3D('',#88770,#45597,#45598);
#37116=AXIS2_PLACEMENT_3D('',#88823,#45599,#45600);
#37117=AXIS2_PLACEMENT_3D('',#88825,#45602,#45603);
#37118=AXIS2_PLACEMENT_3D('',#88826,#45604,#45605);
#37119=AXIS2_PLACEMENT_3D('',#88827,#45606,#45607);
#37120=AXIS2_PLACEMENT_3D('',#88829,#45608,#45609);
#37121=AXIS2_PLACEMENT_3D('',#88830,#45610,#45611);
#37122=AXIS2_PLACEMENT_3D('',#88831,#45612,#45613);
#37123=AXIS2_PLACEMENT_3D('',#88834,#45614,#45615);
#37124=AXIS2_PLACEMENT_3D('',#88836,#45616,#45617);
#37125=AXIS2_PLACEMENT_3D('',#88837,#45618,#45619);
#37126=AXIS2_PLACEMENT_3D('',#88838,#45620,#45621);
#37127=AXIS2_PLACEMENT_3D('',#88841,#45624,#45625);
#37128=AXIS2_PLACEMENT_3D('',#88842,#45626,#45627);
#37129=AXIS2_PLACEMENT_3D('',#88843,#45628,#45629);
#37130=AXIS2_PLACEMENT_3D('',#88844,#45630,#45631);
#37131=AXIS2_PLACEMENT_3D('',#88845,#45632,#45633);
#37132=AXIS2_PLACEMENT_3D('',#88847,#45634,#45635);
#37133=AXIS2_PLACEMENT_3D('',#88849,#45636,#45637);
#37134=AXIS2_PLACEMENT_3D('',#88851,#45639,#45640);
#37135=AXIS2_PLACEMENT_3D('',#88853,#45641,#45642);
#37136=AXIS2_PLACEMENT_3D('',#88854,#45643,#45644);
#37137=AXIS2_PLACEMENT_3D('',#88855,#45645,#45646);
#37138=AXIS2_PLACEMENT_3D('',#88857,#45647,#45648);
#37139=AXIS2_PLACEMENT_3D('',#88858,#45649,#45650);
#37140=AXIS2_PLACEMENT_3D('',#88859,#45651,#45652);
#37141=AXIS2_PLACEMENT_3D('',#88861,#45653,#45654);
#37142=AXIS2_PLACEMENT_3D('',#88862,#45655,#45656);
#37143=AXIS2_PLACEMENT_3D('',#88863,#45657,#45658);
#37144=AXIS2_PLACEMENT_3D('',#88865,#45659,#45660);
#37145=AXIS2_PLACEMENT_3D('',#88867,#45662,#45663);
#37146=AXIS2_PLACEMENT_3D('',#88869,#45664,#45665);
#37147=AXIS2_PLACEMENT_3D('',#88870,#45666,#45667);
#37148=AXIS2_PLACEMENT_3D('',#88872,#45668,#45669);
#37149=AXIS2_PLACEMENT_3D('',#88873,#45670,#45671);
#37150=AXIS2_PLACEMENT_3D('',#88875,#45672,#45673);
#37151=AXIS2_PLACEMENT_3D('',#88953,#45674,#45675);
#37152=AXIS2_PLACEMENT_3D('',#88954,#45676,#45677);
#37153=AXIS2_PLACEMENT_3D('',#88955,#45678,#45679);
#37154=AXIS2_PLACEMENT_3D('',#88956,#45680,#45681);
#37155=AXIS2_PLACEMENT_3D('',#88958,#45682,#45683);
#37156=AXIS2_PLACEMENT_3D('',#88960,#45684,#45685);
#37157=AXIS2_PLACEMENT_3D('',#88966,#45686,#45687);
#37158=AXIS2_PLACEMENT_3D('',#88968,#45689,#45690);
#37159=AXIS2_PLACEMENT_3D('',#88970,#45692,#45693);
#37160=AXIS2_PLACEMENT_3D('',#88972,#45695,#45696);
#37161=AXIS2_PLACEMENT_3D('',#88975,#45698,#45699);
#37162=AXIS2_PLACEMENT_3D('',#88976,#45700,#45701);
#37163=AXIS2_PLACEMENT_3D('',#88977,#45702,#45703);
#37164=AXIS2_PLACEMENT_3D('',#88978,#45704,#45705);
#37165=AXIS2_PLACEMENT_3D('',#88981,#45708,#45709);
#37166=AXIS2_PLACEMENT_3D('',#88983,#45711,#45712);
#37167=AXIS2_PLACEMENT_3D('',#89094,#45714,#45715);
#37168=AXIS2_PLACEMENT_3D('',#89159,#45716,#45717);
#37169=AXIS2_PLACEMENT_3D('',#89161,#45718,#45719);
#37170=AXIS2_PLACEMENT_3D('',#89163,#45721,#45722);
#37171=AXIS2_PLACEMENT_3D('',#89165,#45723,#45724);
#37172=AXIS2_PLACEMENT_3D('',#89166,#45725,#45726);
#37173=AXIS2_PLACEMENT_3D('',#89167,#45727,#45728);
#37174=AXIS2_PLACEMENT_3D('',#89169,#45729,#45730);
#37175=AXIS2_PLACEMENT_3D('',#89170,#45731,#45732);
#37176=AXIS2_PLACEMENT_3D('',#89171,#45733,#45734);
#37177=AXIS2_PLACEMENT_3D('',#89173,#45735,#45736);
#37178=AXIS2_PLACEMENT_3D('',#89174,#45737,#45738);
#37179=AXIS2_PLACEMENT_3D('',#89175,#45739,#45740);
#37180=AXIS2_PLACEMENT_3D('',#89177,#45741,#45742);
#37181=AXIS2_PLACEMENT_3D('',#89234,#45744,#45745);
#37182=AXIS2_PLACEMENT_3D('',#89314,#45746,#45747);
#37183=AXIS2_PLACEMENT_3D('',#89316,#45748,#45749);
#37184=AXIS2_PLACEMENT_3D('',#89317,#45750,#45751);
#37185=AXIS2_PLACEMENT_3D('',#89318,#45752,#45753);
#37186=AXIS2_PLACEMENT_3D('',#89320,#45754,#45755);
#37187=AXIS2_PLACEMENT_3D('',#89321,#45756,#45757);
#37188=AXIS2_PLACEMENT_3D('',#89322,#45758,#45759);
#37189=AXIS2_PLACEMENT_3D('',#89323,#45760,#45761);
#37190=AXIS2_PLACEMENT_3D('',#89324,#45762,#45763);
#37191=AXIS2_PLACEMENT_3D('',#89326,#45764,#45765);
#37192=AXIS2_PLACEMENT_3D('',#89327,#45766,#45767);
#37193=AXIS2_PLACEMENT_3D('',#89328,#45768,#45769);
#37194=AXIS2_PLACEMENT_3D('',#89330,#45770,#45771);
#37195=AXIS2_PLACEMENT_3D('',#89331,#45772,#45773);
#37196=AXIS2_PLACEMENT_3D('',#89370,#45774,#45775);
#37197=AXIS2_PLACEMENT_3D('',#89371,#45776,#45777);
#37198=AXIS2_PLACEMENT_3D('',#89372,#45778,#45779);
#37199=AXIS2_PLACEMENT_3D('',#89436,#45780,#45781);
#37200=AXIS2_PLACEMENT_3D('',#89438,#45782,#45783);
#37201=AXIS2_PLACEMENT_3D('',#89504,#45785,#45786);
#37202=AXIS2_PLACEMENT_3D('',#89505,#45787,#45788);
#37203=AXIS2_PLACEMENT_3D('',#89622,#45790,#45791);
#37204=AXIS2_PLACEMENT_3D('',#89623,#45792,#45793);
#37205=AXIS2_PLACEMENT_3D('',#89625,#45795,#45796);
#37206=AXIS2_PLACEMENT_3D('',#89626,#45797,#45798);
#37207=AXIS2_PLACEMENT_3D('',#89627,#45799,#45800);
#37208=AXIS2_PLACEMENT_3D('',#89650,#45801,#45802);
#37209=AXIS2_PLACEMENT_3D('',#89706,#45803,#45804);
#37210=AXIS2_PLACEMENT_3D('',#89784,#45805,#45806);
#37211=AXIS2_PLACEMENT_3D('',#89785,#45807,#45808);
#37212=AXIS2_PLACEMENT_3D('',#89787,#45809,#45810);
#37213=AXIS2_PLACEMENT_3D('',#89789,#45811,#45812);
#37214=AXIS2_PLACEMENT_3D('',#89790,#45813,#45814);
#37215=AXIS2_PLACEMENT_3D('',#89791,#45815,#45816);
#37216=AXIS2_PLACEMENT_3D('',#89793,#45817,#45818);
#37217=AXIS2_PLACEMENT_3D('',#89795,#45819,#45820);
#37218=AXIS2_PLACEMENT_3D('',#89796,#45821,#45822);
#37219=AXIS2_PLACEMENT_3D('',#89797,#45823,#45824);
#37220=AXIS2_PLACEMENT_3D('',#89801,#45826,#45827);
#37221=AXIS2_PLACEMENT_3D('',#89803,#45829,#45830);
#37222=AXIS2_PLACEMENT_3D('',#89805,#45831,#45832);
#37223=AXIS2_PLACEMENT_3D('',#89807,#45833,#45834);
#37224=AXIS2_PLACEMENT_3D('',#89808,#45835,#45836);
#37225=AXIS2_PLACEMENT_3D('',#89809,#45837,#45838);
#37226=AXIS2_PLACEMENT_3D('',#89811,#45839,#45840);
#37227=AXIS2_PLACEMENT_3D('',#89813,#45841,#45842);
#37228=AXIS2_PLACEMENT_3D('',#89814,#45843,#45844);
#37229=AXIS2_PLACEMENT_3D('',#89815,#45845,#45846);
#37230=AXIS2_PLACEMENT_3D('',#89817,#45847,#45848);
#37231=AXIS2_PLACEMENT_3D('',#89819,#45849,#45850);
#37232=AXIS2_PLACEMENT_3D('',#89820,#45851,#45852);
#37233=AXIS2_PLACEMENT_3D('',#89858,#45853,#45854);
#37234=AXIS2_PLACEMENT_3D('',#89859,#45855,#45856);
#37235=AXIS2_PLACEMENT_3D('',#89960,#45857,#45858);
#37236=AXIS2_PLACEMENT_3D('',#89963,#45861,#45862);
#37237=AXIS2_PLACEMENT_3D('',#89967,#45864,#45865);
#37238=AXIS2_PLACEMENT_3D('',#89969,#45867,#45868);
#37239=AXIS2_PLACEMENT_3D('',#89971,#45869,#45870);
#37240=AXIS2_PLACEMENT_3D('',#89973,#45872,#45873);
#37241=AXIS2_PLACEMENT_3D('',#89974,#45874,#45875);
#37242=AXIS2_PLACEMENT_3D('',#89975,#45876,#45877);
#37243=AXIS2_PLACEMENT_3D('',#89977,#45878,#45879);
#37244=AXIS2_PLACEMENT_3D('',#89979,#45881,#45882);
#37245=AXIS2_PLACEMENT_3D('',#89981,#45883,#45884);
#37246=AXIS2_PLACEMENT_3D('',#89983,#45886,#45887);
#37247=AXIS2_PLACEMENT_3D('',#89985,#45888,#45889);
#37248=AXIS2_PLACEMENT_3D('',#89987,#45891,#45892);
#37249=AXIS2_PLACEMENT_3D('',#89991,#45895,#45896);
#37250=AXIS2_PLACEMENT_3D('',#89993,#45897,#45898);
#37251=AXIS2_PLACEMENT_3D('',#89995,#45900,#45901);
#37252=AXIS2_PLACEMENT_3D('',#89997,#45902,#45903);
#37253=AXIS2_PLACEMENT_3D('',#89999,#45905,#45906);
#37254=AXIS2_PLACEMENT_3D('',#90001,#45907,#45908);
#37255=AXIS2_PLACEMENT_3D('',#90003,#45910,#45911);
#37256=AXIS2_PLACEMENT_3D('',#90007,#45914,#45915);
#37257=AXIS2_PLACEMENT_3D('',#90008,#45916,#45917);
#37258=AXIS2_PLACEMENT_3D('',#90009,#45918,#45919);
#37259=AXIS2_PLACEMENT_3D('',#90011,#45920,#45921);
#37260=AXIS2_PLACEMENT_3D('',#90012,#45922,#45923);
#37261=AXIS2_PLACEMENT_3D('',#90013,#45924,#45925);
#37262=AXIS2_PLACEMENT_3D('',#90015,#45926,#45927);
#37263=AXIS2_PLACEMENT_3D('',#90016,#45928,#45929);
#37264=AXIS2_PLACEMENT_3D('',#90017,#45930,#45931);
#37265=AXIS2_PLACEMENT_3D('',#90019,#45932,#45933);
#37266=AXIS2_PLACEMENT_3D('',#90020,#45934,#45935);
#37267=AXIS2_PLACEMENT_3D('',#90021,#45936,#45937);
#37268=AXIS2_PLACEMENT_3D('',#90023,#45938,#45939);
#37269=AXIS2_PLACEMENT_3D('',#90024,#45940,#45941);
#37270=AXIS2_PLACEMENT_3D('',#90025,#45942,#45943);
#37271=AXIS2_PLACEMENT_3D('',#90026,#45944,#45945);
#37272=AXIS2_PLACEMENT_3D('',#90027,#45946,#45947);
#37273=AXIS2_PLACEMENT_3D('',#90029,#45948,#45949);
#37274=AXIS2_PLACEMENT_3D('',#90030,#45950,#45951);
#37275=AXIS2_PLACEMENT_3D('',#90031,#45952,#45953);
#37276=AXIS2_PLACEMENT_3D('',#90033,#45954,#45955);
#37277=AXIS2_PLACEMENT_3D('',#90089,#45956,#45957);
#37278=AXIS2_PLACEMENT_3D('',#90090,#45958,#45959);
#37279=AXIS2_PLACEMENT_3D('',#90091,#45960,#45961);
#37280=AXIS2_PLACEMENT_3D('',#90149,#45963,#45964);
#37281=AXIS2_PLACEMENT_3D('',#90150,#45965,#45966);
#37282=AXIS2_PLACEMENT_3D('',#90151,#45967,#45968);
#37283=AXIS2_PLACEMENT_3D('',#90153,#45969,#45970);
#37284=AXIS2_PLACEMENT_3D('',#90209,#45971,#45972);
#37285=AXIS2_PLACEMENT_3D('',#90210,#45973,#45974);
#37286=AXIS2_PLACEMENT_3D('',#90211,#45975,#45976);
#37287=AXIS2_PLACEMENT_3D('',#90213,#45978,#45979);
#37288=AXIS2_PLACEMENT_3D('',#90216,#45981,#45982);
#37289=AXIS2_PLACEMENT_3D('',#90217,#45983,#45984);
#37290=AXIS2_PLACEMENT_3D('',#90219,#45985,#45986);
#37291=AXIS2_PLACEMENT_3D('',#90220,#45987,#45988);
#37292=AXIS2_PLACEMENT_3D('',#90221,#45989,#45990);
#37293=AXIS2_PLACEMENT_3D('',#90223,#45991,#45992);
#37294=AXIS2_PLACEMENT_3D('',#90224,#45993,#45994);
#37295=AXIS2_PLACEMENT_3D('',#90225,#45995,#45996);
#37296=AXIS2_PLACEMENT_3D('',#90226,#45997,#45998);
#37297=AXIS2_PLACEMENT_3D('',#90227,#45999,#46000);
#37298=AXIS2_PLACEMENT_3D('',#90228,#46001,#46002);
#37299=AXIS2_PLACEMENT_3D('',#90233,#46004,#46005);
#37300=AXIS2_PLACEMENT_3D('',#90237,#46007,#46008);
#37301=AXIS2_PLACEMENT_3D('',#90302,#46009,#46010);
#37302=AXIS2_PLACEMENT_3D('',#90305,#46011,#46012);
#37303=AXIS2_PLACEMENT_3D('',#90306,#46013,#46014);
#37304=AXIS2_PLACEMENT_3D('',#90308,#46015,#46016);
#37305=AXIS2_PLACEMENT_3D('',#90310,#46018,#46019);
#37306=AXIS2_PLACEMENT_3D('',#90312,#46020,#46021);
#37307=AXIS2_PLACEMENT_3D('',#90388,#46023,#46024);
#37308=AXIS2_PLACEMENT_3D('',#90409,#46026,#46027);
#37309=AXIS2_PLACEMENT_3D('',#90411,#46029,#46030);
#37310=AXIS2_PLACEMENT_3D('',#90451,#46032,#46033);
#37311=AXIS2_PLACEMENT_3D('',#90453,#46035,#46036);
#37312=AXIS2_PLACEMENT_3D('',#90459,#46040,#46041);
#37313=AXIS2_PLACEMENT_3D('',#90461,#46042,#46043);
#37314=AXIS2_PLACEMENT_3D('',#90464,#46045,#46046);
#37315=AXIS2_PLACEMENT_3D('',#90465,#46047,#46048);
#37316=AXIS2_PLACEMENT_3D('',#90467,#46049,#46050);
#37317=AXIS2_PLACEMENT_3D('',#90469,#46051,#46052);
#37318=AXIS2_PLACEMENT_3D('',#90471,#46054,#46055);
#37319=AXIS2_PLACEMENT_3D('',#90473,#46056,#46057);
#37320=AXIS2_PLACEMENT_3D('',#90488,#46060,#46061);
#37321=AXIS2_PLACEMENT_3D('',#90489,#46062,#46063);
#37322=AXIS2_PLACEMENT_3D('',#90493,#46065,#46066);
#37323=AXIS2_PLACEMENT_3D('',#90497,#46069,#46070);
#37324=AXIS2_PLACEMENT_3D('',#90501,#46072,#46073);
#37325=AXIS2_PLACEMENT_3D('',#90504,#46075,#46076);
#37326=AXIS2_PLACEMENT_3D('',#90505,#46077,#46078);
#37327=AXIS2_PLACEMENT_3D('',#90506,#46079,#46080);
#37328=AXIS2_PLACEMENT_3D('',#90507,#46081,#46082);
#37329=AXIS2_PLACEMENT_3D('',#90509,#46083,#46084);
#37330=AXIS2_PLACEMENT_3D('',#90510,#46085,#46086);
#37331=AXIS2_PLACEMENT_3D('',#90511,#46087,#46088);
#37332=AXIS2_PLACEMENT_3D('',#90512,#46089,#46090);
#37333=AXIS2_PLACEMENT_3D('',#90513,#46091,#46092);
#37334=AXIS2_PLACEMENT_3D('',#90516,#46093,#46094);
#37335=AXIS2_PLACEMENT_3D('',#90519,#46097,#46098);
#37336=AXIS2_PLACEMENT_3D('',#90522,#46099,#46100);
#37337=AXIS2_PLACEMENT_3D('',#90523,#46101,#46102);
#37338=AXIS2_PLACEMENT_3D('',#90524,#46103,#46104);
#37339=AXIS2_PLACEMENT_3D('',#90525,#46105,#46106);
#37340=AXIS2_PLACEMENT_3D('',#90527,#46107,#46108);
#37341=AXIS2_PLACEMENT_3D('',#90528,#46109,#46110);
#37342=AXIS2_PLACEMENT_3D('',#90529,#46111,#46112);
#37343=AXIS2_PLACEMENT_3D('',#90530,#46113,#46114);
#37344=AXIS2_PLACEMENT_3D('',#90532,#46115,#46116);
#37345=AXIS2_PLACEMENT_3D('',#90533,#46117,#46118);
#37346=AXIS2_PLACEMENT_3D('',#90534,#46119,#46120);
#37347=AXIS2_PLACEMENT_3D('',#90536,#46121,#46122);
#37348=AXIS2_PLACEMENT_3D('',#90537,#46123,#46124);
#37349=AXIS2_PLACEMENT_3D('',#90538,#46125,#46126);
#37350=AXIS2_PLACEMENT_3D('',#90539,#46127,#46128);
#37351=AXIS2_PLACEMENT_3D('',#90541,#46129,#46130);
#37352=AXIS2_PLACEMENT_3D('',#90542,#46131,#46132);
#37353=AXIS2_PLACEMENT_3D('',#90543,#46133,#46134);
#37354=AXIS2_PLACEMENT_3D('',#90545,#46135,#46136);
#37355=AXIS2_PLACEMENT_3D('',#90547,#46138,#46139);
#37356=AXIS2_PLACEMENT_3D('',#90548,#46140,#46141);
#37357=AXIS2_PLACEMENT_3D('',#90549,#46142,#46143);
#37358=AXIS2_PLACEMENT_3D('',#90551,#46144,#46145);
#37359=AXIS2_PLACEMENT_3D('',#90552,#46146,#46147);
#37360=AXIS2_PLACEMENT_3D('',#90553,#46148,#46149);
#37361=AXIS2_PLACEMENT_3D('',#90554,#46150,#46151);
#37362=AXIS2_PLACEMENT_3D('',#90555,#46152,#46153);
#37363=AXIS2_PLACEMENT_3D('',#90558,#46155,#46156);
#37364=AXIS2_PLACEMENT_3D('',#90559,#46157,#46158);
#37365=AXIS2_PLACEMENT_3D('',#90561,#46159,#46160);
#37366=AXIS2_PLACEMENT_3D('',#90562,#46161,#46162);
#37367=AXIS2_PLACEMENT_3D('',#90563,#46163,#46164);
#37368=AXIS2_PLACEMENT_3D('',#90620,#46171,#46172);
#37369=AXIS2_PLACEMENT_3D('',#90622,#46173,#46174);
#37370=AXIS2_PLACEMENT_3D('',#90625,#46176,#46177);
#37371=AXIS2_PLACEMENT_3D('',#90626,#46178,#46179);
#37372=AXIS2_PLACEMENT_3D('',#90628,#46180,#46181);
#37373=AXIS2_PLACEMENT_3D('',#90630,#46182,#46183);
#37374=AXIS2_PLACEMENT_3D('',#90632,#46185,#46186);
#37375=AXIS2_PLACEMENT_3D('',#90634,#46187,#46188);
#37376=AXIS2_PLACEMENT_3D('',#90637,#46190,#46191);
#37377=AXIS2_PLACEMENT_3D('',#90638,#46192,#46193);
#37378=AXIS2_PLACEMENT_3D('',#90644,#46197,#46198);
#37379=AXIS2_PLACEMENT_3D('',#90646,#46199,#46200);
#37380=AXIS2_PLACEMENT_3D('',#90648,#46201,#46202);
#37381=AXIS2_PLACEMENT_3D('',#90650,#46204,#46205);
#37382=AXIS2_PLACEMENT_3D('',#90654,#46207,#46208);
#37383=AXIS2_PLACEMENT_3D('',#90655,#46209,#46210);
#37384=AXIS2_PLACEMENT_3D('',#90656,#46211,#46212);
#37385=AXIS2_PLACEMENT_3D('',#90658,#46213,#46214);
#37386=AXIS2_PLACEMENT_3D('',#90660,#46215,#46216);
#37387=AXIS2_PLACEMENT_3D('',#90662,#46218,#46219);
#37388=AXIS2_PLACEMENT_3D('',#90663,#46220,#46221);
#37389=AXIS2_PLACEMENT_3D('',#90664,#46222,#46223);
#37390=AXIS2_PLACEMENT_3D('',#90666,#46224,#46225);
#37391=AXIS2_PLACEMENT_3D('',#90667,#46226,#46227);
#37392=AXIS2_PLACEMENT_3D('',#90668,#46228,#46229);
#37393=AXIS2_PLACEMENT_3D('',#90669,#46230,#46231);
#37394=AXIS2_PLACEMENT_3D('',#90670,#46232,#46233);
#37395=AXIS2_PLACEMENT_3D('',#90672,#46234,#46235);
#37396=AXIS2_PLACEMENT_3D('',#90674,#46237,#46238);
#37397=AXIS2_PLACEMENT_3D('',#90676,#46239,#46240);
#37398=AXIS2_PLACEMENT_3D('',#90677,#46241,#46242);
#37399=AXIS2_PLACEMENT_3D('',#90715,#46243,#46244);
#37400=AXIS2_PLACEMENT_3D('',#90771,#46245,#46246);
#37401=AXIS2_PLACEMENT_3D('',#90772,#46247,#46248);
#37402=AXIS2_PLACEMENT_3D('',#90773,#46249,#46250);
#37403=AXIS2_PLACEMENT_3D('',#90774,#46251,#46252);
#37404=AXIS2_PLACEMENT_3D('',#90775,#46253,#46254);
#37405=AXIS2_PLACEMENT_3D('',#90907,#46255,#46256);
#37406=AXIS2_PLACEMENT_3D('',#90908,#46257,#46258);
#37407=AXIS2_PLACEMENT_3D('',#90909,#46259,#46260);
#37408=AXIS2_PLACEMENT_3D('',#90910,#46261,#46262);
#37409=AXIS2_PLACEMENT_3D('',#90911,#46263,#46264);
#37410=AXIS2_PLACEMENT_3D('',#90912,#46265,#46266);
#37411=AXIS2_PLACEMENT_3D('',#90915,#46267,#46268);
#37412=AXIS2_PLACEMENT_3D('',#91059,#46271,#46272);
#37413=AXIS2_PLACEMENT_3D('',#91117,#46273,#46274);
#37414=AXIS2_PLACEMENT_3D('',#91119,#46275,#46276);
#37415=AXIS2_PLACEMENT_3D('',#91120,#46277,#46278);
#37416=AXIS2_PLACEMENT_3D('',#91121,#46279,#46280);
#37417=AXIS2_PLACEMENT_3D('',#91252,#46283,#46284);
#37418=AXIS2_PLACEMENT_3D('',#91312,#46285,#46286);
#37419=AXIS2_PLACEMENT_3D('',#91314,#46287,#46288);
#37420=AXIS2_PLACEMENT_3D('',#91315,#46289,#46290);
#37421=AXIS2_PLACEMENT_3D('',#91316,#46291,#46292);
#37422=AXIS2_PLACEMENT_3D('',#91317,#46293,#46294);
#37423=AXIS2_PLACEMENT_3D('',#91318,#46295,#46296);
#37424=AXIS2_PLACEMENT_3D('',#91324,#46300,#46301);
#37425=AXIS2_PLACEMENT_3D('',#91325,#46302,#46303);
#37426=AXIS2_PLACEMENT_3D('',#91326,#46304,#46305);
#37427=AXIS2_PLACEMENT_3D('',#91331,#46308,#46309);
#37428=AXIS2_PLACEMENT_3D('',#91332,#46310,#46311);
#37429=AXIS2_PLACEMENT_3D('',#91333,#46312,#46313);
#37430=AXIS2_PLACEMENT_3D('',#91334,#46314,#46315);
#37431=AXIS2_PLACEMENT_3D('',#91340,#46319,#46320);
#37432=AXIS2_PLACEMENT_3D('',#91341,#46321,#46322);
#37433=AXIS2_PLACEMENT_3D('',#91342,#46323,#46324);
#37434=AXIS2_PLACEMENT_3D('',#91345,#46325,#46326);
#37435=AXIS2_PLACEMENT_3D('',#91348,#46329,#46330);
#37436=AXIS2_PLACEMENT_3D('',#91349,#46331,#46332);
#37437=AXIS2_PLACEMENT_3D('',#91350,#46333,#46334);
#37438=AXIS2_PLACEMENT_3D('',#91352,#46335,#46336);
#37439=AXIS2_PLACEMENT_3D('',#91355,#46338,#46339);
#37440=AXIS2_PLACEMENT_3D('',#91356,#46340,#46341);
#37441=AXIS2_PLACEMENT_3D('',#91357,#46342,#46343);
#37442=AXIS2_PLACEMENT_3D('',#91358,#46344,#46345);
#37443=AXIS2_PLACEMENT_3D('',#91360,#46346,#46347);
#37444=AXIS2_PLACEMENT_3D('',#91362,#46348,#46349);
#37445=AXIS2_PLACEMENT_3D('',#91363,#46350,#46351);
#37446=AXIS2_PLACEMENT_3D('',#91364,#46352,#46353);
#37447=AXIS2_PLACEMENT_3D('',#91365,#46354,#46355);
#37448=AXIS2_PLACEMENT_3D('',#91366,#46356,#46357);
#37449=AXIS2_PLACEMENT_3D('',#91368,#46358,#46359);
#37450=AXIS2_PLACEMENT_3D('',#91371,#46361,#46362);
#37451=AXIS2_PLACEMENT_3D('',#91372,#46363,#46364);
#37452=AXIS2_PLACEMENT_3D('',#91373,#46365,#46366);
#37453=AXIS2_PLACEMENT_3D('',#91374,#46367,#46368);
#37454=AXIS2_PLACEMENT_3D('',#91376,#46369,#46370);
#37455=AXIS2_PLACEMENT_3D('',#91378,#46371,#46372);
#37456=AXIS2_PLACEMENT_3D('',#91379,#46373,#46374);
#37457=AXIS2_PLACEMENT_3D('',#91380,#46375,#46376);
#37458=AXIS2_PLACEMENT_3D('',#91381,#46377,#46378);
#37459=AXIS2_PLACEMENT_3D('',#91382,#46379,#46380);
#37460=AXIS2_PLACEMENT_3D('',#91385,#46381,#46382);
#37461=AXIS2_PLACEMENT_3D('',#91387,#46383,#46384);
#37462=AXIS2_PLACEMENT_3D('',#91388,#46385,#46386);
#37463=AXIS2_PLACEMENT_3D('',#91389,#46387,#46388);
#37464=AXIS2_PLACEMENT_3D('',#91390,#46389,#46390);
#37465=AXIS2_PLACEMENT_3D('',#91391,#46391,#46392);
#37466=AXIS2_PLACEMENT_3D('',#91392,#46393,#46394);
#37467=AXIS2_PLACEMENT_3D('',#91393,#46395,#46396);
#37468=AXIS2_PLACEMENT_3D('',#91394,#46397,#46398);
#37469=AXIS2_PLACEMENT_3D('',#91432,#46399,#46400);
#37470=AXIS2_PLACEMENT_3D('',#91488,#46401,#46402);
#37471=AXIS2_PLACEMENT_3D('',#91490,#46403,#46404);
#37472=AXIS2_PLACEMENT_3D('',#91492,#46405,#46406);
#37473=AXIS2_PLACEMENT_3D('',#91493,#46407,#46408);
#37474=AXIS2_PLACEMENT_3D('',#91494,#46409,#46410);
#37475=AXIS2_PLACEMENT_3D('',#91560,#46411,#46412);
#37476=AXIS2_PLACEMENT_3D('',#91598,#46413,#46414);
#37477=AXIS2_PLACEMENT_3D('',#91600,#46415,#46416);
#37478=AXIS2_PLACEMENT_3D('',#91602,#46417,#46418);
#37479=AXIS2_PLACEMENT_3D('',#91603,#46419,#46420);
#37480=AXIS2_PLACEMENT_3D('',#91604,#46421,#46422);
#37481=AXIS2_PLACEMENT_3D('',#91606,#46423,#46424);
#37482=AXIS2_PLACEMENT_3D('',#91609,#46426,#46427);
#37483=AXIS2_PLACEMENT_3D('',#91610,#46428,#46429);
#37484=AXIS2_PLACEMENT_3D('',#91616,#46433,#46434);
#37485=AXIS2_PLACEMENT_3D('',#91619,#46436,#46437);
#37486=AXIS2_PLACEMENT_3D('',#91620,#46438,#46439);
#37487=AXIS2_PLACEMENT_3D('',#91663,#46440,#46441);
#37488=AXIS2_PLACEMENT_3D('',#91665,#46442,#46443);
#37489=AXIS2_PLACEMENT_3D('',#91669,#46445,#46446);
#37490=AXIS2_PLACEMENT_3D('',#91732,#46448,#46449);
#37491=AXIS2_PLACEMENT_3D('',#91794,#46451,#46452);
#37492=AXIS2_PLACEMENT_3D('',#91795,#46453,#46454);
#37493=AXIS2_PLACEMENT_3D('',#91797,#46455,#46456);
#37494=AXIS2_PLACEMENT_3D('',#91799,#46457,#46458);
#37495=AXIS2_PLACEMENT_3D('',#91801,#46460,#46461);
#37496=AXIS2_PLACEMENT_3D('',#91805,#46463,#46464);
#37497=AXIS2_PLACEMENT_3D('',#91809,#46467,#46468);
#37498=AXIS2_PLACEMENT_3D('',#91811,#46469,#46470);
#37499=AXIS2_PLACEMENT_3D('',#91851,#46472,#46473);
#37500=AXIS2_PLACEMENT_3D('',#91853,#46474,#46475);
#37501=AXIS2_PLACEMENT_3D('',#91857,#46477,#46478);
#37502=AXIS2_PLACEMENT_3D('',#91861,#46481,#46482);
#37503=AXIS2_PLACEMENT_3D('',#91863,#46483,#46484);
#37504=AXIS2_PLACEMENT_3D('',#91903,#46486,#46487);
#37505=AXIS2_PLACEMENT_3D('',#91919,#46491,#46492);
#37506=AXIS2_PLACEMENT_3D('',#91920,#46493,#46494);
#37507=AXIS2_PLACEMENT_3D('',#91921,#46495,#46496);
#37508=AXIS2_PLACEMENT_3D('',#91922,#46497,#46498);
#37509=AXIS2_PLACEMENT_3D('',#91924,#46499,#46500);
#37510=AXIS2_PLACEMENT_3D('',#91925,#46501,#46502);
#37511=AXIS2_PLACEMENT_3D('',#91926,#46503,#46504);
#37512=AXIS2_PLACEMENT_3D('',#91928,#46505,#46506);
#37513=AXIS2_PLACEMENT_3D('',#91929,#46507,#46508);
#37514=AXIS2_PLACEMENT_3D('',#91930,#46509,#46510);
#37515=AXIS2_PLACEMENT_3D('',#91933,#46511,#46512);
#37516=AXIS2_PLACEMENT_3D('',#91944,#46515,#46516);
#37517=AXIS2_PLACEMENT_3D('',#91946,#46517,#46518);
#37518=AXIS2_PLACEMENT_3D('',#91989,#46520,#46521);
#37519=AXIS2_PLACEMENT_3D('',#91991,#46522,#46523);
#37520=AXIS2_PLACEMENT_3D('',#91993,#46525,#46526);
#37521=AXIS2_PLACEMENT_3D('',#92003,#46531,#46532);
#37522=AXIS2_PLACEMENT_3D('',#92005,#46534,#46535);
#37523=AXIS2_PLACEMENT_3D('',#92007,#46536,#46537);
#37524=AXIS2_PLACEMENT_3D('',#92010,#46539,#46540);
#37525=AXIS2_PLACEMENT_3D('',#92011,#46541,#46542);
#37526=AXIS2_PLACEMENT_3D('',#92015,#46544,#46545);
#37527=AXIS2_PLACEMENT_3D('',#92016,#46546,#46547);
#37528=AXIS2_PLACEMENT_3D('',#92017,#46548,#46549);
#37529=AXIS2_PLACEMENT_3D('',#92019,#46550,#46551);
#37530=AXIS2_PLACEMENT_3D('',#92022,#46553,#46554);
#37531=AXIS2_PLACEMENT_3D('',#92023,#46555,#46556);
#37532=AXIS2_PLACEMENT_3D('',#92029,#46560,#46561);
#37533=AXIS2_PLACEMENT_3D('',#92063,#46562,#46563);
#37534=AXIS2_PLACEMENT_3D('',#92065,#46565,#46566);
#37535=AXIS2_PLACEMENT_3D('',#92067,#46567,#46568);
#37536=AXIS2_PLACEMENT_3D('',#92070,#46570,#46571);
#37537=AXIS2_PLACEMENT_3D('',#92071,#46572,#46573);
#37538=AXIS2_PLACEMENT_3D('',#92072,#46574,#46575);
#37539=AXIS2_PLACEMENT_3D('',#92073,#46576,#46577);
#37540=AXIS2_PLACEMENT_3D('',#92074,#46578,#46579);
#37541=AXIS2_PLACEMENT_3D('',#92076,#46580,#46581);
#37542=AXIS2_PLACEMENT_3D('',#92080,#46583,#46584);
#37543=AXIS2_PLACEMENT_3D('',#92082,#46586,#46587);
#37544=AXIS2_PLACEMENT_3D('',#92085,#46588,#46589);
#37545=AXIS2_PLACEMENT_3D('',#92087,#46590,#46591);
#37546=AXIS2_PLACEMENT_3D('',#92089,#46592,#46593);
#37547=AXIS2_PLACEMENT_3D('',#92090,#46594,#46595);
#37548=AXIS2_PLACEMENT_3D('',#92091,#46596,#46597);
#37549=AXIS2_PLACEMENT_3D('',#92094,#46598,#46599);
#37550=AXIS2_PLACEMENT_3D('',#92095,#46600,#46601);
#37551=AXIS2_PLACEMENT_3D('',#92096,#46602,#46603);
#37552=AXIS2_PLACEMENT_3D('',#92097,#46604,#46605);
#37553=AXIS2_PLACEMENT_3D('',#92100,#46606,#46607);
#37554=AXIS2_PLACEMENT_3D('',#92103,#46610,#46611);
#37555=AXIS2_PLACEMENT_3D('',#92106,#46612,#46613);
#37556=AXIS2_PLACEMENT_3D('',#92107,#46614,#46615);
#37557=AXIS2_PLACEMENT_3D('',#92108,#46616,#46617);
#37558=AXIS2_PLACEMENT_3D('',#92109,#46618,#46619);
#37559=AXIS2_PLACEMENT_3D('',#92112,#46620,#46621);
#37560=AXIS2_PLACEMENT_3D('',#92113,#46622,#46623);
#37561=AXIS2_PLACEMENT_3D('',#92114,#46624,#46625);
#37562=AXIS2_PLACEMENT_3D('',#92115,#46626,#46627);
#37563=AXIS2_PLACEMENT_3D('',#92117,#46628,#46629);
#37564=AXIS2_PLACEMENT_3D('',#92119,#46630,#46631);
#37565=AXIS2_PLACEMENT_3D('',#92120,#46632,#46633);
#37566=AXIS2_PLACEMENT_3D('',#92121,#46634,#46635);
#37567=AXIS2_PLACEMENT_3D('',#92124,#46636,#46637);
#37568=AXIS2_PLACEMENT_3D('',#92125,#46638,#46639);
#37569=AXIS2_PLACEMENT_3D('',#92126,#46640,#46641);
#37570=AXIS2_PLACEMENT_3D('',#92127,#46642,#46643);
#37571=AXIS2_PLACEMENT_3D('',#92130,#46646,#46647);
#37572=AXIS2_PLACEMENT_3D('',#92133,#46648,#46649);
#37573=AXIS2_PLACEMENT_3D('',#92135,#46650,#46651);
#37574=AXIS2_PLACEMENT_3D('',#92137,#46652,#46653);
#37575=AXIS2_PLACEMENT_3D('',#92138,#46654,#46655);
#37576=AXIS2_PLACEMENT_3D('',#92170,#46656,#46657);
#37577=AXIS2_PLACEMENT_3D('',#92176,#46658,#46659);
#37578=AXIS2_PLACEMENT_3D('',#92177,#46660,#46661);
#37579=AXIS2_PLACEMENT_3D('',#92179,#46662,#46663);
#37580=AXIS2_PLACEMENT_3D('',#92180,#46664,#46665);
#37581=AXIS2_PLACEMENT_3D('',#92181,#46666,#46667);
#37582=AXIS2_PLACEMENT_3D('',#92219,#46668,#46669);
#37583=AXIS2_PLACEMENT_3D('',#92221,#46670,#46671);
#37584=AXIS2_PLACEMENT_3D('',#92222,#46672,#46673);
#37585=AXIS2_PLACEMENT_3D('',#92288,#46674,#46675);
#37586=AXIS2_PLACEMENT_3D('',#92317,#46676,#46677);
#37587=AXIS2_PLACEMENT_3D('',#92319,#46678,#46679);
#37588=AXIS2_PLACEMENT_3D('',#92321,#46680,#46681);
#37589=AXIS2_PLACEMENT_3D('',#92322,#46682,#46683);
#37590=AXIS2_PLACEMENT_3D('',#92323,#46684,#46685);
#37591=AXIS2_PLACEMENT_3D('',#92326,#46686,#46687);
#37592=AXIS2_PLACEMENT_3D('',#92327,#46688,#46689);
#37593=AXIS2_PLACEMENT_3D('',#92328,#46690,#46691);
#37594=AXIS2_PLACEMENT_3D('',#92329,#46692,#46693);
#37595=AXIS2_PLACEMENT_3D('',#92331,#46694,#46695);
#37596=AXIS2_PLACEMENT_3D('',#92333,#46696,#46697);
#37597=AXIS2_PLACEMENT_3D('',#92334,#46698,#46699);
#37598=AXIS2_PLACEMENT_3D('',#92335,#46700,#46701);
#37599=AXIS2_PLACEMENT_3D('',#92375,#46704,#46705);
#37600=AXIS2_PLACEMENT_3D('',#92377,#46706,#46707);
#37601=AXIS2_PLACEMENT_3D('',#92378,#46708,#46709);
#37602=AXIS2_PLACEMENT_3D('',#92444,#46710,#46711);
#37603=AXIS2_PLACEMENT_3D('',#92482,#46712,#46713);
#37604=AXIS2_PLACEMENT_3D('',#92483,#46714,#46715);
#37605=AXIS2_PLACEMENT_3D('',#92484,#46716,#46717);
#37606=AXIS2_PLACEMENT_3D('',#92486,#46718,#46719);
#37607=AXIS2_PLACEMENT_3D('',#92488,#46720,#46721);
#37608=AXIS2_PLACEMENT_3D('',#92490,#46722,#46723);
#37609=AXIS2_PLACEMENT_3D('',#92492,#46724,#46725);
#37610=AXIS2_PLACEMENT_3D('',#92493,#46726,#46727);
#37611=AXIS2_PLACEMENT_3D('',#92494,#46728,#46729);
#37612=AXIS2_PLACEMENT_3D('',#92497,#46730,#46731);
#37613=AXIS2_PLACEMENT_3D('',#92498,#46732,#46733);
#37614=AXIS2_PLACEMENT_3D('',#92499,#46734,#46735);
#37615=AXIS2_PLACEMENT_3D('',#92500,#46736,#46737);
#37616=AXIS2_PLACEMENT_3D('',#92503,#46738,#46739);
#37617=AXIS2_PLACEMENT_3D('',#92506,#46742,#46743);
#37618=AXIS2_PLACEMENT_3D('',#92509,#46744,#46745);
#37619=AXIS2_PLACEMENT_3D('',#92510,#46746,#46747);
#37620=AXIS2_PLACEMENT_3D('',#92511,#46748,#46749);
#37621=AXIS2_PLACEMENT_3D('',#92512,#46750,#46751);
#37622=AXIS2_PLACEMENT_3D('',#92515,#46752,#46753);
#37623=AXIS2_PLACEMENT_3D('',#92516,#46754,#46755);
#37624=AXIS2_PLACEMENT_3D('',#92517,#46756,#46757);
#37625=AXIS2_PLACEMENT_3D('',#92518,#46758,#46759);
#37626=AXIS2_PLACEMENT_3D('',#92520,#46760,#46761);
#37627=AXIS2_PLACEMENT_3D('',#92522,#46762,#46763);
#37628=AXIS2_PLACEMENT_3D('',#92523,#46764,#46765);
#37629=AXIS2_PLACEMENT_3D('',#92524,#46766,#46767);
#37630=AXIS2_PLACEMENT_3D('',#92527,#46768,#46769);
#37631=AXIS2_PLACEMENT_3D('',#92528,#46770,#46771);
#37632=AXIS2_PLACEMENT_3D('',#92529,#46772,#46773);
#37633=AXIS2_PLACEMENT_3D('',#92530,#46774,#46775);
#37634=AXIS2_PLACEMENT_3D('',#92533,#46778,#46779);
#37635=AXIS2_PLACEMENT_3D('',#92674,#46782,#46783);
#37636=AXIS2_PLACEMENT_3D('',#92678,#46785,#46786);
#37637=AXIS2_PLACEMENT_3D('',#92680,#46788,#46789);
#37638=AXIS2_PLACEMENT_3D('',#92757,#46790,#46791);
#37639=AXIS2_PLACEMENT_3D('',#92826,#46792,#46793);
#37640=AXIS2_PLACEMENT_3D('',#92827,#46794,#46795);
#37641=AXIS2_PLACEMENT_3D('',#92829,#46796,#46797);
#37642=AXIS2_PLACEMENT_3D('',#92830,#46798,#46799);
#37643=AXIS2_PLACEMENT_3D('',#92831,#46800,#46801);
#37644=AXIS2_PLACEMENT_3D('',#92946,#46802,#46803);
#37645=AXIS2_PLACEMENT_3D('',#92947,#46804,#46805);
#37646=AXIS2_PLACEMENT_3D('',#92948,#46806,#46807);
#37647=AXIS2_PLACEMENT_3D('',#92950,#46808,#46809);
#37648=AXIS2_PLACEMENT_3D('',#92951,#46810,#46811);
#37649=AXIS2_PLACEMENT_3D('',#92952,#46812,#46813);
#37650=AXIS2_PLACEMENT_3D('',#92954,#46814,#46815);
#37651=AXIS2_PLACEMENT_3D('',#92955,#46816,#46817);
#37652=AXIS2_PLACEMENT_3D('',#92956,#46818,#46819);
#37653=AXIS2_PLACEMENT_3D('',#92958,#46820,#46821);
#37654=AXIS2_PLACEMENT_3D('',#92959,#46822,#46823);
#37655=AXIS2_PLACEMENT_3D('',#92960,#46824,#46825);
#37656=AXIS2_PLACEMENT_3D('',#92963,#46828,#46829);
#37657=AXIS2_PLACEMENT_3D('',#93024,#46830,#46831);
#37658=AXIS2_PLACEMENT_3D('',#93025,#46832,#46833);
#37659=AXIS2_PLACEMENT_3D('',#93026,#46834,#46835);
#37660=AXIS2_PLACEMENT_3D('',#93028,#46836,#46837);
#37661=AXIS2_PLACEMENT_3D('',#93030,#46838,#46839);
#37662=AXIS2_PLACEMENT_3D('',#93031,#46840,#46841);
#37663=AXIS2_PLACEMENT_3D('',#93032,#46842,#46843);
#37664=AXIS2_PLACEMENT_3D('',#93034,#46844,#46845);
#37665=AXIS2_PLACEMENT_3D('',#93036,#46846,#46847);
#37666=AXIS2_PLACEMENT_3D('',#93037,#46848,#46849);
#37667=AXIS2_PLACEMENT_3D('',#93038,#46850,#46851);
#37668=AXIS2_PLACEMENT_3D('',#93041,#46852,#46853);
#37669=AXIS2_PLACEMENT_3D('',#93042,#46854,#46855);
#37670=AXIS2_PLACEMENT_3D('',#93043,#46856,#46857);
#37671=AXIS2_PLACEMENT_3D('',#93044,#46858,#46859);
#37672=AXIS2_PLACEMENT_3D('',#93046,#46860,#46861);
#37673=AXIS2_PLACEMENT_3D('',#93048,#46862,#46863);
#37674=AXIS2_PLACEMENT_3D('',#93049,#46864,#46865);
#37675=AXIS2_PLACEMENT_3D('',#93050,#46866,#46867);
#37676=AXIS2_PLACEMENT_3D('',#93052,#46868,#46869);
#37677=AXIS2_PLACEMENT_3D('',#93053,#46870,#46871);
#37678=AXIS2_PLACEMENT_3D('',#93054,#46872,#46873);
#37679=AXIS2_PLACEMENT_3D('',#93056,#46874,#46875);
#37680=AXIS2_PLACEMENT_3D('',#93058,#46877,#46878);
#37681=AXIS2_PLACEMENT_3D('',#93061,#46880,#46881);
#37682=AXIS2_PLACEMENT_3D('',#93062,#46882,#46883);
#37683=AXIS2_PLACEMENT_3D('',#93063,#46884,#46885);
#37684=AXIS2_PLACEMENT_3D('',#93164,#46886,#46887);
#37685=AXIS2_PLACEMENT_3D('',#93215,#46888,#46889);
#37686=AXIS2_PLACEMENT_3D('',#93216,#46890,#46891);
#37687=AXIS2_PLACEMENT_3D('',#93219,#46892,#46893);
#37688=AXIS2_PLACEMENT_3D('',#93223,#46895,#46896);
#37689=AXIS2_PLACEMENT_3D('',#93225,#46898,#46899);
#37690=AXIS2_PLACEMENT_3D('',#93227,#46900,#46901);
#37691=AXIS2_PLACEMENT_3D('',#93229,#46902,#46903);
#37692=AXIS2_PLACEMENT_3D('',#93230,#46904,#46905);
#37693=AXIS2_PLACEMENT_3D('',#93231,#46906,#46907);
#37694=AXIS2_PLACEMENT_3D('',#93234,#46908,#46909);
#37695=AXIS2_PLACEMENT_3D('',#93235,#46910,#46911);
#37696=AXIS2_PLACEMENT_3D('',#93236,#46912,#46913);
#37697=AXIS2_PLACEMENT_3D('',#93238,#46914,#46915);
#37698=AXIS2_PLACEMENT_3D('',#93240,#46916,#46917);
#37699=AXIS2_PLACEMENT_3D('',#93241,#46918,#46919);
#37700=AXIS2_PLACEMENT_3D('',#93242,#46920,#46921);
#37701=AXIS2_PLACEMENT_3D('',#93244,#46922,#46923);
#37702=AXIS2_PLACEMENT_3D('',#93246,#46924,#46925);
#37703=AXIS2_PLACEMENT_3D('',#93247,#46926,#46927);
#37704=AXIS2_PLACEMENT_3D('',#93248,#46928,#46929);
#37705=AXIS2_PLACEMENT_3D('',#93250,#46930,#46931);
#37706=AXIS2_PLACEMENT_3D('',#93253,#46933,#46934);
#37707=AXIS2_PLACEMENT_3D('',#93254,#46935,#46936);
#37708=AXIS2_PLACEMENT_3D('',#93256,#46937,#46938);
#37709=AXIS2_PLACEMENT_3D('',#93259,#46940,#46941);
#37710=AXIS2_PLACEMENT_3D('',#93260,#46942,#46943);
#37711=AXIS2_PLACEMENT_3D('',#93262,#46944,#46945);
#37712=AXIS2_PLACEMENT_3D('',#93263,#46946,#46947);
#37713=AXIS2_PLACEMENT_3D('',#93264,#46948,#46949);
#37714=AXIS2_PLACEMENT_3D('',#93267,#46951,#46952);
#37715=AXIS2_PLACEMENT_3D('',#93268,#46953,#46954);
#37716=AXIS2_PLACEMENT_3D('',#93270,#46955,#46956);
#37717=AXIS2_PLACEMENT_3D('',#93271,#46957,#46958);
#37718=AXIS2_PLACEMENT_3D('',#93272,#46959,#46960);
#37719=AXIS2_PLACEMENT_3D('',#93275,#46962,#46963);
#37720=AXIS2_PLACEMENT_3D('',#93276,#46964,#46965);
#37721=AXIS2_PLACEMENT_3D('',#93277,#46966,#46967);
#37722=AXIS2_PLACEMENT_3D('',#93278,#46968,#46969);
#37723=AXIS2_PLACEMENT_3D('',#93280,#46970,#46971);
#37724=AXIS2_PLACEMENT_3D('',#93281,#46972,#46973);
#37725=AXIS2_PLACEMENT_3D('',#93282,#46974,#46975);
#37726=AXIS2_PLACEMENT_3D('',#93285,#46977,#46978);
#37727=AXIS2_PLACEMENT_3D('',#93286,#46979,#46980);
#37728=AXIS2_PLACEMENT_3D('',#93288,#46981,#46982);
#37729=AXIS2_PLACEMENT_3D('',#93289,#46983,#46984);
#37730=AXIS2_PLACEMENT_3D('',#93290,#46985,#46986);
#37731=AXIS2_PLACEMENT_3D('',#93292,#46987,#46988);
#37732=AXIS2_PLACEMENT_3D('',#93294,#46990,#46991);
#37733=AXIS2_PLACEMENT_3D('',#93296,#46992,#46993);
#37734=AXIS2_PLACEMENT_3D('',#93297,#46994,#46995);
#37735=AXIS2_PLACEMENT_3D('',#93298,#46996,#46997);
#37736=AXIS2_PLACEMENT_3D('',#93300,#46998,#46999);
#37737=AXIS2_PLACEMENT_3D('',#93302,#47001,#47002);
#37738=AXIS2_PLACEMENT_3D('',#93304,#47003,#47004);
#37739=AXIS2_PLACEMENT_3D('',#93305,#47005,#47006);
#37740=AXIS2_PLACEMENT_3D('',#93306,#47007,#47008);
#37741=AXIS2_PLACEMENT_3D('',#93308,#47009,#47010);
#37742=AXIS2_PLACEMENT_3D('',#93310,#47012,#47013);
#37743=AXIS2_PLACEMENT_3D('',#93311,#47014,#47015);
#37744=AXIS2_PLACEMENT_3D('',#93312,#47016,#47017);
#37745=AXIS2_PLACEMENT_3D('',#93313,#47018,#47019);
#37746=AXIS2_PLACEMENT_3D('',#93317,#47021,#47022);
#37747=AXIS2_PLACEMENT_3D('',#93320,#47024,#47025);
#37748=AXIS2_PLACEMENT_3D('',#93321,#47026,#47027);
#37749=AXIS2_PLACEMENT_3D('',#93476,#47028,#47029);
#37750=AXIS2_PLACEMENT_3D('',#93523,#47030,#47031);
#37751=AXIS2_PLACEMENT_3D('',#93525,#47032,#47033);
#37752=AXIS2_PLACEMENT_3D('',#93527,#47034,#47035);
#37753=AXIS2_PLACEMENT_3D('',#93528,#47036,#47037);
#37754=AXIS2_PLACEMENT_3D('',#93529,#47038,#47039);
#37755=AXIS2_PLACEMENT_3D('',#93531,#47040,#47041);
#37756=AXIS2_PLACEMENT_3D('',#93534,#47043,#47044);
#37757=AXIS2_PLACEMENT_3D('',#93535,#47045,#47046);
#37758=AXIS2_PLACEMENT_3D('',#93536,#47047,#47048);
#37759=AXIS2_PLACEMENT_3D('',#93537,#47049,#47050);
#37760=AXIS2_PLACEMENT_3D('',#93538,#47051,#47052);
#37761=AXIS2_PLACEMENT_3D('',#93539,#47053,#47054);
#37762=AXIS2_PLACEMENT_3D('',#93540,#47055,#47056);
#37763=AXIS2_PLACEMENT_3D('',#93541,#47057,#47058);
#37764=AXIS2_PLACEMENT_3D('',#93631,#47059,#47060);
#37765=AXIS2_PLACEMENT_3D('',#93632,#47061,#47062);
#37766=AXIS2_PLACEMENT_3D('',#93694,#47063,#47064);
#37767=AXIS2_PLACEMENT_3D('',#93695,#47065,#47066);
#37768=AXIS2_PLACEMENT_3D('',#93751,#47067,#47068);
#37769=AXIS2_PLACEMENT_3D('',#93810,#47069,#47070);
#37770=AXIS2_PLACEMENT_3D('',#93811,#47071,#47072);
#37771=AXIS2_PLACEMENT_3D('',#93812,#47073,#47074);
#37772=AXIS2_PLACEMENT_3D('',#93814,#47076,#47077);
#37773=AXIS2_PLACEMENT_3D('',#93815,#47078,#47079);
#37774=AXIS2_PLACEMENT_3D('',#93817,#47081,#47082);
#37775=AXIS2_PLACEMENT_3D('',#93818,#47083,#47084);
#37776=AXIS2_PLACEMENT_3D('',#93820,#47086,#47087);
#37777=AXIS2_PLACEMENT_3D('',#93822,#47089,#47090);
#37778=AXIS2_PLACEMENT_3D('',#93824,#47091,#47092);
#37779=AXIS2_PLACEMENT_3D('',#93839,#47094,#47095);
#37780=AXIS2_PLACEMENT_3D('',#93841,#47096,#47097);
#37781=AXIS2_PLACEMENT_3D('',#93842,#47098,#47099);
#37782=AXIS2_PLACEMENT_3D('',#93843,#47100,#47101);
#37783=AXIS2_PLACEMENT_3D('',#93845,#47102,#47103);
#37784=AXIS2_PLACEMENT_3D('',#93847,#47104,#47105);
#37785=AXIS2_PLACEMENT_3D('',#93851,#47107,#47108);
#37786=AXIS2_PLACEMENT_3D('',#93853,#47109,#47110);
#37787=AXIS2_PLACEMENT_3D('',#93855,#47112,#47113);
#37788=AXIS2_PLACEMENT_3D('',#93857,#47114,#47115);
#37789=AXIS2_PLACEMENT_3D('',#93858,#47116,#47117);
#37790=AXIS2_PLACEMENT_3D('',#93860,#47118,#47119);
#37791=AXIS2_PLACEMENT_3D('',#93861,#47120,#47121);
#37792=AXIS2_PLACEMENT_3D('',#93863,#47123,#47124);
#37793=AXIS2_PLACEMENT_3D('',#93864,#47125,#47126);
#37794=AXIS2_PLACEMENT_3D('',#93873,#47128,#47129);
#37795=AXIS2_PLACEMENT_3D('',#93993,#47131,#47132);
#37796=AXIS2_PLACEMENT_3D('',#94021,#47134,#47135);
#37797=AXIS2_PLACEMENT_3D('',#94022,#47136,#47137);
#37798=AXIS2_PLACEMENT_3D('',#94023,#47138,#47139);
#37799=AXIS2_PLACEMENT_3D('',#94027,#47141,#47142);
#37800=AXIS2_PLACEMENT_3D('',#94028,#47143,#47144);
#37801=AXIS2_PLACEMENT_3D('',#94029,#47145,#47146);
#37802=AXIS2_PLACEMENT_3D('',#94030,#47147,#47148);
#37803=AXIS2_PLACEMENT_3D('',#94031,#47149,#47150);
#37804=AXIS2_PLACEMENT_3D('',#94048,#47151,#47152);
#37805=AXIS2_PLACEMENT_3D('',#94049,#47153,#47154);
#37806=AXIS2_PLACEMENT_3D('',#94050,#47155,#47156);
#37807=AXIS2_PLACEMENT_3D('',#94051,#47157,#47158);
#37808=AXIS2_PLACEMENT_3D('',#94052,#47159,#47160);
#37809=AXIS2_PLACEMENT_3D('',#94053,#47161,#47162);
#37810=AXIS2_PLACEMENT_3D('',#94054,#47163,#47164);
#37811=AXIS2_PLACEMENT_3D('',#94055,#47165,#47166);
#37812=AXIS2_PLACEMENT_3D('',#94056,#47167,#47168);
#37813=AXIS2_PLACEMENT_3D('',#94057,#47169,#47170);
#37814=AXIS2_PLACEMENT_3D('',#94058,#47171,#47172);
#37815=AXIS2_PLACEMENT_3D('',#94059,#47173,#47174);
#37816=AXIS2_PLACEMENT_3D('',#94060,#47175,#47176);
#37817=AXIS2_PLACEMENT_3D('',#94061,#47177,#47178);
#37818=AXIS2_PLACEMENT_3D('',#94062,#47179,#47180);
#37819=AXIS2_PLACEMENT_3D('',#94068,#47184,#47185);
#37820=AXIS2_PLACEMENT_3D('',#94071,#47188,#47189);
#37821=AXIS2_PLACEMENT_3D('',#94074,#47191,#47192);
#37822=AXIS2_PLACEMENT_3D('',#94075,#47193,#47194);
#37823=AXIS2_PLACEMENT_3D('',#94079,#47197,#47198);
#37824=AXIS2_PLACEMENT_3D('',#94082,#47200,#47201);
#37825=AXIS2_PLACEMENT_3D('',#94083,#47202,#47203);
#37826=AXIS2_PLACEMENT_3D('',#94085,#47205,#47206);
#37827=AXIS2_PLACEMENT_3D('',#94086,#47207,#47208);
#37828=AXIS2_PLACEMENT_3D('',#94088,#47210,#47211);
#37829=AXIS2_PLACEMENT_3D('',#94090,#47213,#47214);
#37830=AXIS2_PLACEMENT_3D('',#94091,#47215,#47216);
#37831=AXIS2_PLACEMENT_3D('',#94094,#47219,#47220);
#37832=AXIS2_PLACEMENT_3D('',#94096,#47222,#47223);
#37833=AXIS2_PLACEMENT_3D('',#94098,#47225,#47226);
#37834=AXIS2_PLACEMENT_3D('',#94100,#47228,#47229);
#37835=AXIS2_PLACEMENT_3D('',#94102,#47231,#47232);
#37836=AXIS2_PLACEMENT_3D('',#94103,#47233,#47234);
#37837=AXIS2_PLACEMENT_3D('',#94106,#47237,#47238);
#37838=AXIS2_PLACEMENT_3D('',#94108,#47240,#47241);
#37839=AXIS2_PLACEMENT_3D('',#94110,#47243,#47244);
#37840=AXIS2_PLACEMENT_3D('',#94113,#47246,#47247);
#37841=AXIS2_PLACEMENT_3D('',#94114,#47248,#47249);
#37842=AXIS2_PLACEMENT_3D('',#94117,#47251,#47252);
#37843=AXIS2_PLACEMENT_3D('',#94118,#47253,#47254);
#37844=AXIS2_PLACEMENT_3D('',#94120,#47255,#47256);
#37845=AXIS2_PLACEMENT_3D('',#94122,#47258,#47259);
#37846=AXIS2_PLACEMENT_3D('',#94125,#47261,#47262);
#37847=AXIS2_PLACEMENT_3D('',#94126,#47263,#47264);
#37848=AXIS2_PLACEMENT_3D('',#94128,#47266,#47267);
#37849=AXIS2_PLACEMENT_3D('',#94129,#47268,#47269);
#37850=AXIS2_PLACEMENT_3D('',#94130,#47270,#47271);
#37851=AXIS2_PLACEMENT_3D('',#94205,#47272,#47273);
#37852=AXIS2_PLACEMENT_3D('',#94206,#47274,#47275);
#37853=AXIS2_PLACEMENT_3D('',#94207,#47276,#47277);
#37854=AXIS2_PLACEMENT_3D('',#94208,#47278,#47279);
#37855=AXIS2_PLACEMENT_3D('',#94209,#47280,#47281);
#37856=AXIS2_PLACEMENT_3D('',#94210,#47282,#47283);
#37857=AXIS2_PLACEMENT_3D('',#94212,#47285,#47286);
#37858=AXIS2_PLACEMENT_3D('',#94214,#47287,#47288);
#37859=AXIS2_PLACEMENT_3D('',#94216,#47290,#47291);
#37860=AXIS2_PLACEMENT_3D('',#94217,#47292,#47293);
#37861=AXIS2_PLACEMENT_3D('',#94220,#47294,#47295);
#37862=AXIS2_PLACEMENT_3D('',#94221,#47296,#47297);
#37863=AXIS2_PLACEMENT_3D('',#94222,#47298,#47299);
#37864=AXIS2_PLACEMENT_3D('',#94223,#47300,#47301);
#37865=AXIS2_PLACEMENT_3D('',#94224,#47302,#47303);
#37866=AXIS2_PLACEMENT_3D('',#94225,#47304,#47305);
#37867=AXIS2_PLACEMENT_3D('',#94227,#47307,#47308);
#37868=AXIS2_PLACEMENT_3D('',#94228,#47309,#47310);
#37869=AXIS2_PLACEMENT_3D('',#94229,#47311,#47312);
#37870=AXIS2_PLACEMENT_3D('',#94230,#47313,#47314);
#37871=AXIS2_PLACEMENT_3D('',#94231,#47315,#47316);
#37872=AXIS2_PLACEMENT_3D('',#94272,#47317,#47318);
#37873=AXIS2_PLACEMENT_3D('',#94273,#47319,#47320);
#37874=AXIS2_PLACEMENT_3D('',#94332,#47321,#47322);
#37875=AXIS2_PLACEMENT_3D('',#94403,#47323,#47324);
#37876=AXIS2_PLACEMENT_3D('',#94405,#47326,#47327);
#37877=AXIS2_PLACEMENT_3D('',#94406,#47328,#47329);
#37878=AXIS2_PLACEMENT_3D('',#94407,#47330,#47331);
#37879=AXIS2_PLACEMENT_3D('',#94408,#47332,#47333);
#37880=AXIS2_PLACEMENT_3D('',#94411,#47334,#47335);
#37881=AXIS2_PLACEMENT_3D('',#94413,#47336,#47337);
#37882=AXIS2_PLACEMENT_3D('',#94414,#47338,#47339);
#37883=AXIS2_PLACEMENT_3D('',#94415,#47340,#47341);
#37884=AXIS2_PLACEMENT_3D('',#94418,#47344,#47345);
#37885=AXIS2_PLACEMENT_3D('',#94419,#47346,#47347);
#37886=AXIS2_PLACEMENT_3D('',#94420,#47348,#47349);
#37887=AXIS2_PLACEMENT_3D('',#94421,#47350,#47351);
#37888=AXIS2_PLACEMENT_3D('',#94422,#47352,#47353);
#37889=AXIS2_PLACEMENT_3D('',#94426,#47355,#47356);
#37890=AXIS2_PLACEMENT_3D('',#94427,#47357,#47358);
#37891=AXIS2_PLACEMENT_3D('',#94428,#47359,#47360);
#37892=AXIS2_PLACEMENT_3D('',#94430,#47361,#47362);
#37893=AXIS2_PLACEMENT_3D('',#94431,#47363,#47364);
#37894=AXIS2_PLACEMENT_3D('',#94432,#47365,#47366);
#37895=AXIS2_PLACEMENT_3D('',#94434,#47367,#47368);
#37896=AXIS2_PLACEMENT_3D('',#94435,#47369,#47370);
#37897=AXIS2_PLACEMENT_3D('',#94436,#47371,#47372);
#37898=AXIS2_PLACEMENT_3D('',#94438,#47373,#47374);
#37899=AXIS2_PLACEMENT_3D('',#94439,#47375,#47376);
#37900=AXIS2_PLACEMENT_3D('',#94440,#47377,#47378);
#37901=AXIS2_PLACEMENT_3D('',#94443,#47380,#47381);
#37902=AXIS2_PLACEMENT_3D('',#94444,#47382,#47383);
#37903=AXIS2_PLACEMENT_3D('',#94445,#47384,#47385);
#37904=AXIS2_PLACEMENT_3D('',#94448,#47387,#47388);
#37905=AXIS2_PLACEMENT_3D('',#94449,#47389,#47390);
#37906=AXIS2_PLACEMENT_3D('',#94451,#47391,#47392);
#37907=AXIS2_PLACEMENT_3D('',#94452,#47393,#47394);
#37908=AXIS2_PLACEMENT_3D('',#94454,#47395,#47396);
#37909=AXIS2_PLACEMENT_3D('',#94455,#47397,#47398);
#37910=AXIS2_PLACEMENT_3D('',#94590,#47399,#47400);
#37911=AXIS2_PLACEMENT_3D('',#94591,#47401,#47402);
#37912=AXIS2_PLACEMENT_3D('',#94592,#47403,#47404);
#37913=AXIS2_PLACEMENT_3D('',#94679,#47405,#47406);
#37914=AXIS2_PLACEMENT_3D('',#94680,#47407,#47408);
#37915=AXIS2_PLACEMENT_3D('',#94681,#47409,#47410);
#37916=AXIS2_PLACEMENT_3D('',#94682,#47411,#47412);
#37917=AXIS2_PLACEMENT_3D('',#94684,#47414,#47415);
#37918=AXIS2_PLACEMENT_3D('',#94686,#47417,#47418);
#37919=AXIS2_PLACEMENT_3D('',#94688,#47420,#47421);
#37920=AXIS2_PLACEMENT_3D('',#94689,#47422,#47423);
#37921=AXIS2_PLACEMENT_3D('',#94691,#47424,#47425);
#37922=AXIS2_PLACEMENT_3D('',#94693,#47427,#47428);
#37923=AXIS2_PLACEMENT_3D('',#94694,#47429,#47430);
#37924=AXIS2_PLACEMENT_3D('',#94695,#47431,#47432);
#37925=AXIS2_PLACEMENT_3D('',#94697,#47434,#47435);
#37926=AXIS2_PLACEMENT_3D('',#94699,#47437,#47438);
#37927=AXIS2_PLACEMENT_3D('',#94828,#47440,#47441);
#37928=AXIS2_PLACEMENT_3D('',#94829,#47442,#47443);
#37929=AXIS2_PLACEMENT_3D('',#94832,#47445,#47446);
#37930=AXIS2_PLACEMENT_3D('',#94833,#47447,#47448);
#37931=AXIS2_PLACEMENT_3D('',#94835,#47449,#47450);
#37932=AXIS2_PLACEMENT_3D('',#94836,#47451,#47452);
#37933=AXIS2_PLACEMENT_3D('',#94837,#47453,#47454);
#37934=AXIS2_PLACEMENT_3D('',#94839,#47455,#47456);
#37935=AXIS2_PLACEMENT_3D('',#94840,#47457,#47458);
#37936=AXIS2_PLACEMENT_3D('',#94841,#47459,#47460);
#37937=AXIS2_PLACEMENT_3D('',#94843,#47461,#47462);
#37938=AXIS2_PLACEMENT_3D('',#94844,#47463,#47464);
#37939=AXIS2_PLACEMENT_3D('',#94845,#47465,#47466);
#37940=AXIS2_PLACEMENT_3D('',#94848,#47468,#47469);
#37941=AXIS2_PLACEMENT_3D('',#94913,#47470,#47471);
#37942=AXIS2_PLACEMENT_3D('',#94914,#47472,#47473);
#37943=AXIS2_PLACEMENT_3D('',#94916,#47474,#47475);
#37944=AXIS2_PLACEMENT_3D('',#94917,#47476,#47477);
#37945=AXIS2_PLACEMENT_3D('',#94918,#47478,#47479);
#37946=AXIS2_PLACEMENT_3D('',#94920,#47480,#47481);
#37947=AXIS2_PLACEMENT_3D('',#94921,#47482,#47483);
#37948=AXIS2_PLACEMENT_3D('',#94922,#47484,#47485);
#37949=AXIS2_PLACEMENT_3D('',#94923,#47486,#47487);
#37950=AXIS2_PLACEMENT_3D('',#94924,#47488,#47489);
#37951=AXIS2_PLACEMENT_3D('',#94926,#47490,#47491);
#37952=AXIS2_PLACEMENT_3D('',#94927,#47492,#47493);
#37953=AXIS2_PLACEMENT_3D('',#94928,#47494,#47495);
#37954=AXIS2_PLACEMENT_3D('',#94930,#47496,#47497);
#37955=AXIS2_PLACEMENT_3D('',#94931,#47498,#47499);
#37956=AXIS2_PLACEMENT_3D('',#94969,#47500,#47501);
#37957=AXIS2_PLACEMENT_3D('',#94971,#47502,#47503);
#37958=AXIS2_PLACEMENT_3D('',#94972,#47504,#47505);
#37959=AXIS2_PLACEMENT_3D('',#95055,#47506,#47507);
#37960=AXIS2_PLACEMENT_3D('',#95058,#47509,#47510);
#37961=AXIS2_PLACEMENT_3D('',#95114,#47511,#47512);
#37962=AXIS2_PLACEMENT_3D('',#95158,#47513,#47514);
#37963=AXIS2_PLACEMENT_3D('',#95197,#47516,#47517);
#37964=AXIS2_PLACEMENT_3D('',#95241,#47518,#47519);
#37965=AXIS2_PLACEMENT_3D('',#95243,#47521,#47522);
#37966=AXIS2_PLACEMENT_3D('',#95244,#47523,#47524);
#37967=AXIS2_PLACEMENT_3D('',#95245,#47525,#47526);
#37968=AXIS2_PLACEMENT_3D('',#95246,#47527,#47528);
#37969=AXIS2_PLACEMENT_3D('',#95247,#47529,#47530);
#37970=AXIS2_PLACEMENT_3D('',#95249,#47531,#47532);
#37971=AXIS2_PLACEMENT_3D('',#95252,#47534,#47535);
#37972=AXIS2_PLACEMENT_3D('',#95253,#47536,#47537);
#37973=AXIS2_PLACEMENT_3D('',#95256,#47539,#47540);
#37974=AXIS2_PLACEMENT_3D('',#95257,#47541,#47542);
#37975=AXIS2_PLACEMENT_3D('',#95259,#47544,#47545);
#37976=AXIS2_PLACEMENT_3D('',#95261,#47546,#47547);
#37977=AXIS2_PLACEMENT_3D('',#95263,#47549,#47550);
#37978=AXIS2_PLACEMENT_3D('',#95264,#47551,#47552);
#37979=AXIS2_PLACEMENT_3D('',#95265,#47553,#47554);
#37980=AXIS2_PLACEMENT_3D('',#95267,#47555,#47556);
#37981=AXIS2_PLACEMENT_3D('',#95268,#47557,#47558);
#37982=AXIS2_PLACEMENT_3D('',#95269,#47559,#47560);
#37983=AXIS2_PLACEMENT_3D('',#95271,#47561,#47562);
#37984=AXIS2_PLACEMENT_3D('',#95273,#47564,#47565);
#37985=AXIS2_PLACEMENT_3D('',#95275,#47566,#47567);
#37986=AXIS2_PLACEMENT_3D('',#95276,#47568,#47569);
#37987=AXIS2_PLACEMENT_3D('',#95277,#47570,#47571);
#37988=AXIS2_PLACEMENT_3D('',#95279,#47573,#47574);
#37989=AXIS2_PLACEMENT_3D('',#95281,#47576,#47577);
#37990=AXIS2_PLACEMENT_3D('',#95284,#47579,#47580);
#37991=AXIS2_PLACEMENT_3D('',#95285,#47581,#47582);
#37992=AXIS2_PLACEMENT_3D('',#95286,#47583,#47584);
#37993=AXIS2_PLACEMENT_3D('',#95287,#47585,#47586);
#37994=AXIS2_PLACEMENT_3D('',#95291,#47588,#47589);
#37995=AXIS2_PLACEMENT_3D('',#95293,#47590,#47591);
#37996=AXIS2_PLACEMENT_3D('',#95295,#47592,#47593);
#37997=AXIS2_PLACEMENT_3D('',#95299,#47595,#47596);
#37998=AXIS2_PLACEMENT_3D('',#95300,#47597,#47598);
#37999=AXIS2_PLACEMENT_3D('',#95301,#47599,#47600);
#38000=AXIS2_PLACEMENT_3D('',#95304,#47601,#47602);
#38001=AXIS2_PLACEMENT_3D('',#95503,#47603,#47604);
#38002=AXIS2_PLACEMENT_3D('',#95540,#47605,#47606);
#38003=AXIS2_PLACEMENT_3D('',#95541,#47607,#47608);
#38004=AXIS2_PLACEMENT_3D('',#95543,#47609,#47610);
#38005=AXIS2_PLACEMENT_3D('',#95544,#47611,#47612);
#38006=AXIS2_PLACEMENT_3D('',#95545,#47613,#47614);
#38007=AXIS2_PLACEMENT_3D('',#95547,#47615,#47616);
#38008=AXIS2_PLACEMENT_3D('',#95548,#47617,#47618);
#38009=AXIS2_PLACEMENT_3D('',#95549,#47619,#47620);
#38010=AXIS2_PLACEMENT_3D('',#95551,#47621,#47622);
#38011=AXIS2_PLACEMENT_3D('',#95553,#47624,#47625);
#38012=AXIS2_PLACEMENT_3D('',#95555,#47626,#47627);
#38013=AXIS2_PLACEMENT_3D('',#95556,#47628,#47629);
#38014=AXIS2_PLACEMENT_3D('',#95557,#47630,#47631);
#38015=AXIS2_PLACEMENT_3D('',#95559,#47632,#47633);
#38016=AXIS2_PLACEMENT_3D('',#95560,#47634,#47635);
#38017=AXIS2_PLACEMENT_3D('',#95561,#47636,#47637);
#38018=AXIS2_PLACEMENT_3D('',#95563,#47638,#47639);
#38019=AXIS2_PLACEMENT_3D('',#95564,#47640,#47641);
#38020=AXIS2_PLACEMENT_3D('',#95602,#47642,#47643);
#38021=AXIS2_PLACEMENT_3D('',#95603,#47644,#47645);
#38022=AXIS2_PLACEMENT_3D('',#95689,#47646,#47647);
#38023=AXIS2_PLACEMENT_3D('',#95691,#47649,#47650);
#38024=AXIS2_PLACEMENT_3D('',#95695,#47652,#47653);
#38025=AXIS2_PLACEMENT_3D('',#95697,#47655,#47656);
#38026=AXIS2_PLACEMENT_3D('',#95700,#47658,#47659);
#38027=AXIS2_PLACEMENT_3D('',#95701,#47660,#47661);
#38028=AXIS2_PLACEMENT_3D('',#95702,#47662,#47663);
#38029=AXIS2_PLACEMENT_3D('',#95703,#47664,#47665);
#38030=AXIS2_PLACEMENT_3D('',#95706,#47667,#47668);
#38031=AXIS2_PLACEMENT_3D('',#95707,#47669,#47670);
#38032=AXIS2_PLACEMENT_3D('',#95710,#47672,#47673);
#38033=AXIS2_PLACEMENT_3D('',#95711,#47674,#47675);
#38034=AXIS2_PLACEMENT_3D('',#95714,#47677,#47678);
#38035=AXIS2_PLACEMENT_3D('',#95715,#47679,#47680);
#38036=AXIS2_PLACEMENT_3D('',#95719,#47683,#47684);
#38037=AXIS2_PLACEMENT_3D('',#95722,#47686,#47687);
#38038=AXIS2_PLACEMENT_3D('',#95723,#47688,#47689);
#38039=AXIS2_PLACEMENT_3D('',#95726,#47691,#47692);
#38040=AXIS2_PLACEMENT_3D('',#95727,#47693,#47694);
#38041=AXIS2_PLACEMENT_3D('',#95730,#47696,#47697);
#38042=AXIS2_PLACEMENT_3D('',#95731,#47698,#47699);
#38043=AXIS2_PLACEMENT_3D('',#95735,#47702,#47703);
#38044=AXIS2_PLACEMENT_3D('',#95736,#47704,#47705);
#38045=AXIS2_PLACEMENT_3D('',#95737,#47706,#47707);
#38046=AXIS2_PLACEMENT_3D('',#95739,#47708,#47709);
#38047=AXIS2_PLACEMENT_3D('',#95740,#47710,#47711);
#38048=AXIS2_PLACEMENT_3D('',#95741,#47712,#47713);
#38049=AXIS2_PLACEMENT_3D('',#95743,#47714,#47715);
#38050=AXIS2_PLACEMENT_3D('',#95744,#47716,#47717);
#38051=AXIS2_PLACEMENT_3D('',#95745,#47718,#47719);
#38052=AXIS2_PLACEMENT_3D('',#95747,#47720,#47721);
#38053=AXIS2_PLACEMENT_3D('',#95748,#47722,#47723);
#38054=AXIS2_PLACEMENT_3D('',#95749,#47724,#47725);
#38055=AXIS2_PLACEMENT_3D('',#95751,#47726,#47727);
#38056=AXIS2_PLACEMENT_3D('',#95752,#47728,#47729);
#38057=AXIS2_PLACEMENT_3D('',#95753,#47730,#47731);
#38058=AXIS2_PLACEMENT_3D('',#95754,#47732,#47733);
#38059=AXIS2_PLACEMENT_3D('',#95755,#47734,#47735);
#38060=AXIS2_PLACEMENT_3D('',#95757,#47736,#47737);
#38061=AXIS2_PLACEMENT_3D('',#95758,#47738,#47739);
#38062=AXIS2_PLACEMENT_3D('',#95759,#47740,#47741);
#38063=AXIS2_PLACEMENT_3D('',#95761,#47742,#47743);
#38064=AXIS2_PLACEMENT_3D('',#95762,#47744,#47745);
#38065=AXIS2_PLACEMENT_3D('',#95763,#47746,#47747);
#38066=AXIS2_PLACEMENT_3D('',#95764,#47748,#47749);
#38067=AXIS2_PLACEMENT_3D('',#95765,#47750,#47751);
#38068=AXIS2_PLACEMENT_3D('',#95767,#47752,#47753);
#38069=AXIS2_PLACEMENT_3D('',#95769,#47755,#47756);
#38070=AXIS2_PLACEMENT_3D('',#95770,#47757,#47758);
#38071=AXIS2_PLACEMENT_3D('',#95771,#47759,#47760);
#38072=AXIS2_PLACEMENT_3D('',#95773,#47761,#47762);
#38073=AXIS2_PLACEMENT_3D('',#95774,#47763,#47764);
#38074=AXIS2_PLACEMENT_3D('',#95775,#47765,#47766);
#38075=AXIS2_PLACEMENT_3D('',#95776,#47767,#47768);
#38076=AXIS2_PLACEMENT_3D('',#95777,#47769,#47770);
#38077=AXIS2_PLACEMENT_3D('',#95779,#47772,#47773);
#38078=AXIS2_PLACEMENT_3D('',#95781,#47774,#47775);
#38079=AXIS2_PLACEMENT_3D('',#95783,#47777,#47778);
#38080=AXIS2_PLACEMENT_3D('',#95785,#47779,#47780);
#38081=AXIS2_PLACEMENT_3D('',#95786,#47781,#47782);
#38082=AXIS2_PLACEMENT_3D('',#95787,#47783,#47784);
#38083=AXIS2_PLACEMENT_3D('',#95789,#47785,#47786);
#38084=AXIS2_PLACEMENT_3D('',#95790,#47787,#47788);
#38085=AXIS2_PLACEMENT_3D('',#95791,#47789,#47790);
#38086=AXIS2_PLACEMENT_3D('',#95792,#47791,#47792);
#38087=AXIS2_PLACEMENT_3D('',#95793,#47793,#47794);
#38088=AXIS2_PLACEMENT_3D('',#95794,#47795,#47796);
#38089=AXIS2_PLACEMENT_3D('',#95795,#47797,#47798);
#38090=AXIS2_PLACEMENT_3D('',#95798,#47799,#47800);
#38091=AXIS2_PLACEMENT_3D('',#95800,#47801,#47802);
#38092=AXIS2_PLACEMENT_3D('',#95802,#47803,#47804);
#38093=AXIS2_PLACEMENT_3D('',#95803,#47805,#47806);
#38094=AXIS2_PLACEMENT_3D('',#95804,#47807,#47808);
#38095=AXIS2_PLACEMENT_3D('',#95807,#47809,#47810);
#38096=AXIS2_PLACEMENT_3D('',#95811,#47812,#47813);
#38097=AXIS2_PLACEMENT_3D('',#95813,#47815,#47816);
#38098=AXIS2_PLACEMENT_3D('',#95815,#47817,#47818);
#38099=AXIS2_PLACEMENT_3D('',#95817,#47819,#47820);
#38100=AXIS2_PLACEMENT_3D('',#95819,#47822,#47823);
#38101=AXIS2_PLACEMENT_3D('',#95821,#47824,#47825);
#38102=AXIS2_PLACEMENT_3D('',#95823,#47826,#47827);
#38103=AXIS2_PLACEMENT_3D('',#95825,#47829,#47830);
#38104=AXIS2_PLACEMENT_3D('',#95883,#47831,#47832);
#38105=AXIS2_PLACEMENT_3D('',#95884,#47833,#47834);
#38106=AXIS2_PLACEMENT_3D('',#95946,#47835,#47836);
#38107=AXIS2_PLACEMENT_3D('',#95948,#47837,#47838);
#38108=AXIS2_PLACEMENT_3D('',#95949,#47839,#47840);
#38109=AXIS2_PLACEMENT_3D('',#95950,#47841,#47842);
#38110=AXIS2_PLACEMENT_3D('',#95953,#47843,#47844);
#38111=AXIS2_PLACEMENT_3D('',#95954,#47845,#47846);
#38112=AXIS2_PLACEMENT_3D('',#95956,#47847,#47848);
#38113=AXIS2_PLACEMENT_3D('',#95957,#47849,#47850);
#38114=AXIS2_PLACEMENT_3D('',#95958,#47851,#47852);
#38115=AXIS2_PLACEMENT_3D('',#95960,#47853,#47854);
#38116=AXIS2_PLACEMENT_3D('',#95961,#47855,#47856);
#38117=AXIS2_PLACEMENT_3D('',#95962,#47857,#47858);
#38118=AXIS2_PLACEMENT_3D('',#95965,#47860,#47861);
#38119=AXIS2_PLACEMENT_3D('',#95966,#47862,#47863);
#38120=AXIS2_PLACEMENT_3D('',#95973,#47864,#47865);
#38121=AXIS2_PLACEMENT_3D('',#95974,#47866,#47867);
#38122=AXIS2_PLACEMENT_3D('',#95977,#47869,#47870);
#38123=AXIS2_PLACEMENT_3D('',#95978,#47871,#47872);
#38124=AXIS2_PLACEMENT_3D('',#95980,#47873,#47874);
#38125=AXIS2_PLACEMENT_3D('',#95981,#47875,#47876);
#38126=AXIS2_PLACEMENT_3D('',#95982,#47877,#47878);
#38127=AXIS2_PLACEMENT_3D('',#95984,#47879,#47880);
#38128=AXIS2_PLACEMENT_3D('',#95986,#47882,#47883);
#38129=AXIS2_PLACEMENT_3D('',#95988,#47884,#47885);
#38130=AXIS2_PLACEMENT_3D('',#95991,#47887,#47888);
#38131=AXIS2_PLACEMENT_3D('',#95992,#47889,#47890);
#38132=AXIS2_PLACEMENT_3D('',#96048,#47891,#47892);
#38133=AXIS2_PLACEMENT_3D('',#96079,#47893,#47894);
#38134=AXIS2_PLACEMENT_3D('',#96080,#47895,#47896);
#38135=AXIS2_PLACEMENT_3D('',#96081,#47897,#47898);
#38136=AXIS2_PLACEMENT_3D('',#96086,#47900,#47901);
#38137=AXIS2_PLACEMENT_3D('',#96090,#47903,#47904);
#38138=AXIS2_PLACEMENT_3D('',#96091,#47905,#47906);
#38139=AXIS2_PLACEMENT_3D('',#96092,#47907,#47908);
#38140=AXIS2_PLACEMENT_3D('',#96124,#47909,#47910);
#38141=AXIS2_PLACEMENT_3D('',#96126,#47912,#47913);
#38142=AXIS2_PLACEMENT_3D('',#96132,#47917,#47918);
#38143=AXIS2_PLACEMENT_3D('',#96134,#47919,#47920);
#38144=AXIS2_PLACEMENT_3D('',#96136,#47921,#47922);
#38145=AXIS2_PLACEMENT_3D('',#96137,#47923,#47924);
#38146=AXIS2_PLACEMENT_3D('',#96138,#47925,#47926);
#38147=AXIS2_PLACEMENT_3D('',#96139,#47927,#47928);
#38148=AXIS2_PLACEMENT_3D('',#96140,#47929,#47930);
#38149=AXIS2_PLACEMENT_3D('',#96142,#47931,#47932);
#38150=AXIS2_PLACEMENT_3D('',#96144,#47934,#47935);
#38151=AXIS2_PLACEMENT_3D('',#96147,#47937,#47938);
#38152=AXIS2_PLACEMENT_3D('',#96148,#47939,#47940);
#38153=AXIS2_PLACEMENT_3D('',#96189,#47942,#47943);
#38154=AXIS2_PLACEMENT_3D('',#96190,#47944,#47945);
#38155=AXIS2_PLACEMENT_3D('',#96191,#47946,#47947);
#38156=AXIS2_PLACEMENT_3D('',#96192,#47948,#47949);
#38157=AXIS2_PLACEMENT_3D('',#96194,#47950,#47951);
#38158=AXIS2_PLACEMENT_3D('',#96196,#47953,#47954);
#38159=AXIS2_PLACEMENT_3D('',#96200,#47957,#47958);
#38160=AXIS2_PLACEMENT_3D('',#96205,#47960,#47961);
#38161=AXIS2_PLACEMENT_3D('',#96209,#47963,#47964);
#38162=AXIS2_PLACEMENT_3D('',#96210,#47965,#47966);
#38163=AXIS2_PLACEMENT_3D('',#96211,#47967,#47968);
#38164=AXIS2_PLACEMENT_3D('',#96223,#47969,#47970);
#38165=AXIS2_PLACEMENT_3D('',#96225,#47972,#47973);
#38166=AXIS2_PLACEMENT_3D('',#96231,#47977,#47978);
#38167=AXIS2_PLACEMENT_3D('',#96233,#47979,#47980);
#38168=AXIS2_PLACEMENT_3D('',#96234,#47981,#47982);
#38169=AXIS2_PLACEMENT_3D('',#96235,#47983,#47984);
#38170=AXIS2_PLACEMENT_3D('',#96236,#47985,#47986);
#38171=AXIS2_PLACEMENT_3D('',#96238,#47988,#47989);
#38172=AXIS2_PLACEMENT_3D('',#96240,#47990,#47991);
#38173=AXIS2_PLACEMENT_3D('',#96242,#47993,#47994);
#38174=AXIS2_PLACEMENT_3D('',#96243,#47995,#47996);
#38175=AXIS2_PLACEMENT_3D('',#96244,#47997,#47998);
#38176=AXIS2_PLACEMENT_3D('',#96274,#48000,#48001);
#38177=AXIS2_PLACEMENT_3D('',#96275,#48002,#48003);
#38178=AXIS2_PLACEMENT_3D('',#96276,#48004,#48005);
#38179=AXIS2_PLACEMENT_3D('',#96277,#48006,#48007);
#38180=AXIS2_PLACEMENT_3D('',#96279,#48008,#48009);
#38181=AXIS2_PLACEMENT_3D('',#96281,#48011,#48012);
#38182=AXIS2_PLACEMENT_3D('',#96285,#48015,#48016);
#38183=AXIS2_PLACEMENT_3D('',#96294,#48021,#48022);
#38184=AXIS2_PLACEMENT_3D('',#96332,#48024,#48025);
#38185=AXIS2_PLACEMENT_3D('',#96333,#48026,#48027);
#38186=AXIS2_PLACEMENT_3D('',#96338,#48029,#48030);
#38187=AXIS2_PLACEMENT_3D('',#96340,#48031,#48032);
#38188=AXIS2_PLACEMENT_3D('',#96341,#48033,#48034);
#38189=AXIS2_PLACEMENT_3D('',#96343,#48035,#48036);
#38190=AXIS2_PLACEMENT_3D('',#96345,#48037,#48038);
#38191=AXIS2_PLACEMENT_3D('',#96346,#48039,#48040);
#38192=AXIS2_PLACEMENT_3D('',#96347,#48041,#48042);
#38193=AXIS2_PLACEMENT_3D('',#96349,#48043,#48044);
#38194=AXIS2_PLACEMENT_3D('',#96351,#48045,#48046);
#38195=AXIS2_PLACEMENT_3D('',#96353,#48048,#48049);
#38196=AXIS2_PLACEMENT_3D('',#96354,#48050,#48051);
#38197=AXIS2_PLACEMENT_3D('',#96355,#48052,#48053);
#38198=AXIS2_PLACEMENT_3D('',#96357,#48054,#48055);
#38199=AXIS2_PLACEMENT_3D('',#96358,#48056,#48057);
#38200=AXIS2_PLACEMENT_3D('',#96359,#48058,#48059);
#38201=AXIS2_PLACEMENT_3D('',#96362,#48061,#48062);
#38202=AXIS2_PLACEMENT_3D('',#96363,#48063,#48064);
#38203=AXIS2_PLACEMENT_3D('',#96365,#48065,#48066);
#38204=AXIS2_PLACEMENT_3D('',#96366,#48067,#48068);
#38205=AXIS2_PLACEMENT_3D('',#96367,#48069,#48070);
#38206=AXIS2_PLACEMENT_3D('',#96370,#48072,#48073);
#38207=AXIS2_PLACEMENT_3D('',#96371,#48074,#48075);
#38208=AXIS2_PLACEMENT_3D('',#96373,#48076,#48077);
#38209=AXIS2_PLACEMENT_3D('',#96374,#48078,#48079);
#38210=AXIS2_PLACEMENT_3D('',#96375,#48080,#48081);
#38211=AXIS2_PLACEMENT_3D('',#96378,#48083,#48084);
#38212=AXIS2_PLACEMENT_3D('',#96379,#48085,#48086);
#38213=AXIS2_PLACEMENT_3D('',#96404,#48088,#48089);
#38214=AXIS2_PLACEMENT_3D('',#96405,#48090,#48091);
#38215=AXIS2_PLACEMENT_3D('',#96406,#48092,#48093);
#38216=AXIS2_PLACEMENT_3D('',#96407,#48094,#48095);
#38217=AXIS2_PLACEMENT_3D('',#96409,#48096,#48097);
#38218=AXIS2_PLACEMENT_3D('',#96411,#48099,#48100);
#38219=AXIS2_PLACEMENT_3D('',#96415,#48103,#48104);
#38220=AXIS2_PLACEMENT_3D('',#96418,#48105,#48106);
#38221=AXIS2_PLACEMENT_3D('',#96420,#48107,#48108);
#38222=AXIS2_PLACEMENT_3D('',#96422,#48109,#48110);
#38223=AXIS2_PLACEMENT_3D('',#96424,#48111,#48112);
#38224=AXIS2_PLACEMENT_3D('',#96426,#48113,#48114);
#38225=AXIS2_PLACEMENT_3D('',#96427,#48115,#48116);
#38226=AXIS2_PLACEMENT_3D('',#96428,#48117,#48118);
#38227=AXIS2_PLACEMENT_3D('',#96430,#48119,#48120);
#38228=AXIS2_PLACEMENT_3D('',#96432,#48121,#48122);
#38229=AXIS2_PLACEMENT_3D('',#96434,#48124,#48125);
#38230=AXIS2_PLACEMENT_3D('',#96436,#48126,#48127);
#38231=AXIS2_PLACEMENT_3D('',#96437,#48128,#48129);
#38232=AXIS2_PLACEMENT_3D('',#96438,#48130,#48131);
#38233=AXIS2_PLACEMENT_3D('',#96440,#48132,#48133);
#38234=AXIS2_PLACEMENT_3D('',#96441,#48134,#48135);
#38235=AXIS2_PLACEMENT_3D('',#96442,#48136,#48137);
#38236=AXIS2_PLACEMENT_3D('',#96444,#48138,#48139);
#38237=AXIS2_PLACEMENT_3D('',#96445,#48140,#48141);
#38238=AXIS2_PLACEMENT_3D('',#96446,#48142,#48143);
#38239=AXIS2_PLACEMENT_3D('',#96448,#48144,#48145);
#38240=AXIS2_PLACEMENT_3D('',#96450,#48147,#48148);
#38241=AXIS2_PLACEMENT_3D('',#96452,#48149,#48150);
#38242=AXIS2_PLACEMENT_3D('',#96454,#48151,#48152);
#38243=AXIS2_PLACEMENT_3D('',#96456,#48154,#48155);
#38244=AXIS2_PLACEMENT_3D('',#96457,#48156,#48157);
#38245=AXIS2_PLACEMENT_3D('',#96458,#48158,#48159);
#38246=AXIS2_PLACEMENT_3D('',#96460,#48160,#48161);
#38247=AXIS2_PLACEMENT_3D('',#96461,#48162,#48163);
#38248=AXIS2_PLACEMENT_3D('',#96462,#48164,#48165);
#38249=AXIS2_PLACEMENT_3D('',#96464,#48166,#48167);
#38250=AXIS2_PLACEMENT_3D('',#96466,#48169,#48170);
#38251=AXIS2_PLACEMENT_3D('',#96468,#48171,#48172);
#38252=AXIS2_PLACEMENT_3D('',#96471,#48174,#48175);
#38253=AXIS2_PLACEMENT_3D('',#96472,#48176,#48177);
#38254=AXIS2_PLACEMENT_3D('',#96474,#48178,#48179);
#38255=AXIS2_PLACEMENT_3D('',#96475,#48180,#48181);
#38256=AXIS2_PLACEMENT_3D('',#96476,#48182,#48183);
#38257=AXIS2_PLACEMENT_3D('',#96478,#48184,#48185);
#38258=AXIS2_PLACEMENT_3D('',#96479,#48186,#48187);
#38259=AXIS2_PLACEMENT_3D('',#96480,#48188,#48189);
#38260=AXIS2_PLACEMENT_3D('',#96482,#48190,#48191);
#38261=AXIS2_PLACEMENT_3D('',#96483,#48192,#48193);
#38262=AXIS2_PLACEMENT_3D('',#96484,#48194,#48195);
#38263=AXIS2_PLACEMENT_3D('',#96486,#48196,#48197);
#38264=AXIS2_PLACEMENT_3D('',#96487,#48198,#48199);
#38265=AXIS2_PLACEMENT_3D('',#96488,#48200,#48201);
#38266=AXIS2_PLACEMENT_3D('',#96490,#48202,#48203);
#38267=AXIS2_PLACEMENT_3D('',#96491,#48204,#48205);
#38268=AXIS2_PLACEMENT_3D('',#96492,#48206,#48207);
#38269=AXIS2_PLACEMENT_3D('',#96494,#48208,#48209);
#38270=AXIS2_PLACEMENT_3D('',#96496,#48211,#48212);
#38271=AXIS2_PLACEMENT_3D('',#96497,#48213,#48214);
#38272=AXIS2_PLACEMENT_3D('',#96498,#48215,#48216);
#38273=AXIS2_PLACEMENT_3D('',#96499,#48217,#48218);
#38274=AXIS2_PLACEMENT_3D('',#96500,#48219,#48220);
#38275=AXIS2_PLACEMENT_3D('',#96502,#48221,#48222);
#38276=AXIS2_PLACEMENT_3D('',#96503,#48223,#48224);
#38277=AXIS2_PLACEMENT_3D('',#96505,#48225,#48226);
#38278=AXIS2_PLACEMENT_3D('',#96506,#48227,#48228);
#38279=AXIS2_PLACEMENT_3D('',#96508,#48229,#48230);
#38280=AXIS2_PLACEMENT_3D('',#96510,#48231,#48232);
#38281=AXIS2_PLACEMENT_3D('',#96512,#48233,#48234);
#38282=AXIS2_PLACEMENT_3D('',#96513,#48235,#48236);
#38283=AXIS2_PLACEMENT_3D('',#96514,#48237,#48238);
#38284=AXIS2_PLACEMENT_3D('',#96515,#48239,#48240);
#38285=AXIS2_PLACEMENT_3D('',#96598,#48241,#48242);
#38286=AXIS2_PLACEMENT_3D('',#96600,#48243,#48244);
#38287=AXIS2_PLACEMENT_3D('',#96610,#48245,#48246);
#38288=AXIS2_PLACEMENT_3D('',#96612,#48248,#48249);
#38289=AXIS2_PLACEMENT_3D('',#96685,#48251,#48252);
#38290=AXIS2_PLACEMENT_3D('',#96686,#48253,#48254);
#38291=AXIS2_PLACEMENT_3D('',#96688,#48255,#48256);
#38292=AXIS2_PLACEMENT_3D('',#96689,#48257,#48258);
#38293=AXIS2_PLACEMENT_3D('',#96690,#48259,#48260);
#38294=AXIS2_PLACEMENT_3D('',#96693,#48263,#48264);
#38295=AXIS2_PLACEMENT_3D('',#96695,#48265,#48266);
#38296=AXIS2_PLACEMENT_3D('',#96696,#48267,#48268);
#38297=AXIS2_PLACEMENT_3D('',#96697,#48269,#48270);
#38298=AXIS2_PLACEMENT_3D('',#96699,#48272,#48273);
#38299=AXIS2_PLACEMENT_3D('',#96702,#48274,#48275);
#38300=AXIS2_PLACEMENT_3D('',#96704,#48276,#48277);
#38301=AXIS2_PLACEMENT_3D('',#96705,#48278,#48279);
#38302=AXIS2_PLACEMENT_3D('',#96706,#48280,#48281);
#38303=AXIS2_PLACEMENT_3D('',#96707,#48282,#48283);
#38304=AXIS2_PLACEMENT_3D('',#96709,#48284,#48285);
#38305=AXIS2_PLACEMENT_3D('',#96710,#48286,#48287);
#38306=AXIS2_PLACEMENT_3D('',#96712,#48288,#48289);
#38307=AXIS2_PLACEMENT_3D('',#96713,#48290,#48291);
#38308=AXIS2_PLACEMENT_3D('',#96714,#48292,#48293);
#38309=AXIS2_PLACEMENT_3D('',#96797,#48294,#48295);
#38310=AXIS2_PLACEMENT_3D('',#96799,#48296,#48297);
#38311=AXIS2_PLACEMENT_3D('',#96834,#48298,#48299);
#38312=AXIS2_PLACEMENT_3D('',#96836,#48301,#48302);
#38313=AXIS2_PLACEMENT_3D('',#96838,#48303,#48304);
#38314=AXIS2_PLACEMENT_3D('',#96839,#48305,#48306);
#38315=AXIS2_PLACEMENT_3D('',#96941,#48307,#48308);
#38316=AXIS2_PLACEMENT_3D('',#96943,#48310,#48311);
#38317=AXIS2_PLACEMENT_3D('',#96945,#48313,#48314);
#38318=AXIS2_PLACEMENT_3D('',#96947,#48315,#48316);
#38319=AXIS2_PLACEMENT_3D('',#96949,#48317,#48318);
#38320=AXIS2_PLACEMENT_3D('',#96950,#48319,#48320);
#38321=AXIS2_PLACEMENT_3D('',#97000,#48321,#48322);
#38322=AXIS2_PLACEMENT_3D('',#97002,#48324,#48325);
#38323=AXIS2_PLACEMENT_3D('',#97004,#48326,#48327);
#38324=AXIS2_PLACEMENT_3D('',#97006,#48328,#48329);
#38325=AXIS2_PLACEMENT_3D('',#97007,#48330,#48331);
#38326=AXIS2_PLACEMENT_3D('',#97057,#48332,#48333);
#38327=AXIS2_PLACEMENT_3D('',#97059,#48335,#48336);
#38328=AXIS2_PLACEMENT_3D('',#97061,#48337,#48338);
#38329=AXIS2_PLACEMENT_3D('',#97062,#48339,#48340);
#38330=AXIS2_PLACEMENT_3D('',#97064,#48341,#48342);
#38331=AXIS2_PLACEMENT_3D('',#97065,#48343,#48344);
#38332=AXIS2_PLACEMENT_3D('',#97068,#48345,#48346);
#38333=AXIS2_PLACEMENT_3D('',#97070,#48347,#48348);
#38334=AXIS2_PLACEMENT_3D('',#97071,#48349,#48350);
#38335=AXIS2_PLACEMENT_3D('',#97072,#48351,#48352);
#38336=AXIS2_PLACEMENT_3D('',#97073,#48353,#48354);
#38337=AXIS2_PLACEMENT_3D('',#97074,#48355,#48356);
#38338=AXIS2_PLACEMENT_3D('',#97075,#48357,#48358);
#38339=AXIS2_PLACEMENT_3D('',#97077,#48359,#48360);
#38340=AXIS2_PLACEMENT_3D('',#97078,#48361,#48362);
#38341=AXIS2_PLACEMENT_3D('',#97180,#48363,#48364);
#38342=AXIS2_PLACEMENT_3D('',#97182,#48366,#48367);
#38343=AXIS2_PLACEMENT_3D('',#97184,#48368,#48369);
#38344=AXIS2_PLACEMENT_3D('',#97185,#48370,#48371);
#38345=AXIS2_PLACEMENT_3D('',#97327,#48372,#48373);
#38346=AXIS2_PLACEMENT_3D('',#97329,#48375,#48376);
#38347=AXIS2_PLACEMENT_3D('',#97330,#48377,#48378);
#38348=AXIS2_PLACEMENT_3D('',#97331,#48379,#48380);
#38349=AXIS2_PLACEMENT_3D('',#97334,#48381,#48382);
#38350=AXIS2_PLACEMENT_3D('',#97336,#48383,#48384);
#38351=AXIS2_PLACEMENT_3D('',#97338,#48385,#48386);
#38352=AXIS2_PLACEMENT_3D('',#97340,#48387,#48388);
#38353=AXIS2_PLACEMENT_3D('',#97342,#48389,#48390);
#38354=AXIS2_PLACEMENT_3D('',#97343,#48391,#48392);
#38355=AXIS2_PLACEMENT_3D('',#97344,#48393,#48394);
#38356=AXIS2_PLACEMENT_3D('',#97347,#48395,#48396);
#38357=AXIS2_PLACEMENT_3D('',#97351,#48398,#48399);
#38358=AXIS2_PLACEMENT_3D('',#97355,#48402,#48403);
#38359=AXIS2_PLACEMENT_3D('',#97361,#48407,#48408);
#38360=AXIS2_PLACEMENT_3D('',#97365,#48411,#48412);
#38361=AXIS2_PLACEMENT_3D('',#97368,#48414,#48415);
#38362=AXIS2_PLACEMENT_3D('',#97369,#48416,#48417);
#38363=AXIS2_PLACEMENT_3D('',#97373,#48420,#48421);
#38364=AXIS2_PLACEMENT_3D('',#97380,#48424,#48425);
#38365=AXIS2_PLACEMENT_3D('',#97382,#48427,#48428);
#38366=AXIS2_PLACEMENT_3D('',#97388,#48432,#48433);
#38367=AXIS2_PLACEMENT_3D('',#97392,#48436,#48437);
#38368=AXIS2_PLACEMENT_3D('',#97396,#48440,#48441);
#38369=AXIS2_PLACEMENT_3D('',#97398,#48442,#48443);
#38370=AXIS2_PLACEMENT_3D('',#97399,#48444,#48445);
#38371=AXIS2_PLACEMENT_3D('',#97402,#48447,#48448);
#38372=AXIS2_PLACEMENT_3D('',#97403,#48449,#48450);
#38373=AXIS2_PLACEMENT_3D('',#97407,#48452,#48453);
#38374=AXIS2_PLACEMENT_3D('',#97411,#48455,#48456);
#38375=AXIS2_PLACEMENT_3D('',#97415,#48458,#48459);
#38376=AXIS2_PLACEMENT_3D('',#97417,#48460,#48461);
#38377=AXIS2_PLACEMENT_3D('',#97421,#48463,#48464);
#38378=AXIS2_PLACEMENT_3D('',#97423,#48465,#48466);
#38379=AXIS2_PLACEMENT_3D('',#97427,#48468,#48469);
#38380=AXIS2_PLACEMENT_3D('',#97429,#48470,#48471);
#38381=AXIS2_PLACEMENT_3D('',#97431,#48472,#48473);
#38382=AXIS2_PLACEMENT_3D('',#97433,#48474,#48475);
#38383=AXIS2_PLACEMENT_3D('',#97435,#48476,#48477);
#38384=AXIS2_PLACEMENT_3D('',#97437,#48478,#48479);
#38385=AXIS2_PLACEMENT_3D('',#97439,#48480,#48481);
#38386=AXIS2_PLACEMENT_3D('',#97443,#48483,#48484);
#38387=AXIS2_PLACEMENT_3D('',#97445,#48485,#48486);
#38388=AXIS2_PLACEMENT_3D('',#97449,#48488,#48489);
#38389=AXIS2_PLACEMENT_3D('',#97451,#48490,#48491);
#38390=AXIS2_PLACEMENT_3D('',#97455,#48493,#48494);
#38391=AXIS2_PLACEMENT_3D('',#97459,#48496,#48497);
#38392=AXIS2_PLACEMENT_3D('',#97461,#48499,#48500);
#38393=AXIS2_PLACEMENT_3D('',#97464,#48501,#48502);
#38394=AXIS2_PLACEMENT_3D('',#97478,#48503,#48504);
#38395=AXIS2_PLACEMENT_3D('',#97480,#48505,#48506);
#38396=AXIS2_PLACEMENT_3D('',#97484,#48508,#48509);
#38397=AXIS2_PLACEMENT_3D('',#97496,#48515,#48516);
#38398=AXIS2_PLACEMENT_3D('',#97500,#48518,#48519);
#38399=AXIS2_PLACEMENT_3D('',#97502,#48521,#48522);
#38400=AXIS2_PLACEMENT_3D('',#97504,#48523,#48524);
#38401=AXIS2_PLACEMENT_3D('',#97505,#48525,#48526);
#38402=AXIS2_PLACEMENT_3D('',#97506,#48527,#48528);
#38403=AXIS2_PLACEMENT_3D('',#97517,#48535,#48536);
#38404=AXIS2_PLACEMENT_3D('',#97559,#48538,#48539);
#38405=AXIS2_PLACEMENT_3D('',#97560,#48540,#48541);
#38406=AXIS2_PLACEMENT_3D('',#97569,#48545,#48546);
#38407=AXIS2_PLACEMENT_3D('',#97573,#48549,#48550);
#38408=AXIS2_PLACEMENT_3D('',#97576,#48552,#48553);
#38409=AXIS2_PLACEMENT_3D('',#97577,#48554,#48555);
#38410=AXIS2_PLACEMENT_3D('',#97581,#48558,#48559);
#38411=AXIS2_PLACEMENT_3D('',#97594,#48561,#48562);
#38412=AXIS2_PLACEMENT_3D('',#97598,#48565,#48566);
#38413=AXIS2_PLACEMENT_3D('',#97599,#48567,#48568);
#38414=AXIS2_PLACEMENT_3D('',#97600,#48569,#48570);
#38415=AXIS2_PLACEMENT_3D('',#97603,#48571,#48572);
#38416=AXIS2_PLACEMENT_3D('',#97607,#48575,#48576);
#38417=AXIS2_PLACEMENT_3D('',#97613,#48579,#48580);
#38418=AXIS2_PLACEMENT_3D('',#97615,#48582,#48583);
#38419=AXIS2_PLACEMENT_3D('',#97619,#48586,#48587);
#38420=AXIS2_PLACEMENT_3D('',#97632,#48589,#48590);
#38421=AXIS2_PLACEMENT_3D('',#97633,#48591,#48592);
#38422=AXIS2_PLACEMENT_3D('',#97634,#48593,#48594);
#38423=AXIS2_PLACEMENT_3D('',#97643,#48598,#48599);
#38424=AXIS2_PLACEMENT_3D('',#97645,#48601,#48602);
#38425=AXIS2_PLACEMENT_3D('',#97647,#48603,#48604);
#38426=AXIS2_PLACEMENT_3D('',#97649,#48606,#48607);
#38427=AXIS2_PLACEMENT_3D('',#97662,#48609,#48610);
#38428=AXIS2_PLACEMENT_3D('',#97666,#48613,#48614);
#38429=AXIS2_PLACEMENT_3D('',#97667,#48615,#48616);
#38430=AXIS2_PLACEMENT_3D('',#97668,#48617,#48618);
#38431=AXIS2_PLACEMENT_3D('',#97671,#48619,#48620);
#38432=AXIS2_PLACEMENT_3D('',#97675,#48623,#48624);
#38433=AXIS2_PLACEMENT_3D('',#97683,#48628,#48629);
#38434=AXIS2_PLACEMENT_3D('',#97685,#48631,#48632);
#38435=AXIS2_PLACEMENT_3D('',#97689,#48635,#48636);
#38436=AXIS2_PLACEMENT_3D('',#97702,#48638,#48639);
#38437=AXIS2_PLACEMENT_3D('',#97706,#48642,#48643);
#38438=AXIS2_PLACEMENT_3D('',#97707,#48644,#48645);
#38439=AXIS2_PLACEMENT_3D('',#97708,#48646,#48647);
#38440=AXIS2_PLACEMENT_3D('',#97711,#48648,#48649);
#38441=AXIS2_PLACEMENT_3D('',#97713,#48651,#48652);
#38442=AXIS2_PLACEMENT_3D('',#97716,#48653,#48654);
#38443=AXIS2_PLACEMENT_3D('',#97718,#48656,#48657);
#38444=AXIS2_PLACEMENT_3D('',#97721,#48660,#48661);
#38445=AXIS2_PLACEMENT_3D('',#97724,#48664,#48665);
#38446=AXIS2_PLACEMENT_3D('',#97727,#48666,#48667);
#38447=AXIS2_PLACEMENT_3D('',#97729,#48668,#48669);
#38448=AXIS2_PLACEMENT_3D('',#97732,#48671,#48672);
#38449=AXIS2_PLACEMENT_3D('',#97733,#48673,#48674);
#38450=AXIS2_PLACEMENT_3D('',#97735,#48676,#48677);
#38451=AXIS2_PLACEMENT_3D('',#97737,#48679,#48680);
#38452=AXIS2_PLACEMENT_3D('',#97740,#48681,#48682);
#38453=AXIS2_PLACEMENT_3D('',#97743,#48685,#48686);
#38454=AXIS2_PLACEMENT_3D('',#97745,#48687,#48688);
#38455=AXIS2_PLACEMENT_3D('',#97747,#48690,#48691);
#38456=AXIS2_PLACEMENT_3D('',#97751,#48694,#48695);
#38457=AXIS2_PLACEMENT_3D('',#97752,#48696,#48697);
#38458=AXIS2_PLACEMENT_3D('',#97753,#48698,#48699);
#38459=AXIS2_PLACEMENT_3D('',#97755,#48700,#48701);
#38460=AXIS2_PLACEMENT_3D('',#97796,#48703,#48704);
#38461=AXIS2_PLACEMENT_3D('',#97799,#48705,#48706);
#38462=AXIS2_PLACEMENT_3D('',#97803,#48709,#48710);
#38463=AXIS2_PLACEMENT_3D('',#97809,#48714,#48715);
#38464=AXIS2_PLACEMENT_3D('',#97823,#48717,#48718);
#38465=AXIS2_PLACEMENT_3D('',#97824,#48719,#48720);
#38466=AXIS2_PLACEMENT_3D('',#97830,#48724,#48725);
#38467=AXIS2_PLACEMENT_3D('',#97839,#48730,#48731);
#38468=AXIS2_PLACEMENT_3D('',#97853,#48733,#48734);
#38469=AXIS2_PLACEMENT_3D('',#97854,#48735,#48736);
#38470=AXIS2_PLACEMENT_3D('',#97860,#48740,#48741);
#38471=AXIS2_PLACEMENT_3D('',#97862,#48742,#48743);
#38472=AXIS2_PLACEMENT_3D('',#97864,#48745,#48746);
#38473=AXIS2_PLACEMENT_3D('',#97869,#48748,#48749);
#38474=AXIS2_PLACEMENT_3D('',#97871,#48751,#48752);
#38475=AXIS2_PLACEMENT_3D('',#97885,#48754,#48755);
#38476=AXIS2_PLACEMENT_3D('',#97886,#48756,#48757);
#38477=AXIS2_PLACEMENT_3D('',#97892,#48761,#48762);
#38478=AXIS2_PLACEMENT_3D('',#97898,#48765,#48766);
#38479=AXIS2_PLACEMENT_3D('',#97899,#48767,#48768);
#38480=AXIS2_PLACEMENT_3D('',#97913,#48770,#48771);
#38481=AXIS2_PLACEMENT_3D('',#97914,#48772,#48773);
#38482=AXIS2_PLACEMENT_3D('',#97920,#48777,#48778);
#38483=AXIS2_PLACEMENT_3D('',#97922,#48779,#48780);
#38484=AXIS2_PLACEMENT_3D('',#97924,#48781,#48782);
#38485=AXIS2_PLACEMENT_3D('',#97926,#48784,#48785);
#38486=AXIS2_PLACEMENT_3D('',#97931,#48787,#48788);
#38487=AXIS2_PLACEMENT_3D('',#97933,#48789,#48790);
#38488=AXIS2_PLACEMENT_3D('',#97937,#48792,#48793);
#38489=AXIS2_PLACEMENT_3D('',#97939,#48794,#48795);
#38490=AXIS2_PLACEMENT_3D('',#97941,#48796,#48797);
#38491=AXIS2_PLACEMENT_3D('',#97943,#48798,#48799);
#38492=AXIS2_PLACEMENT_3D('',#97945,#48800,#48801);
#38493=AXIS2_PLACEMENT_3D('',#97947,#48802,#48803);
#38494=AXIS2_PLACEMENT_3D('',#97951,#48805,#48806);
#38495=AXIS2_PLACEMENT_3D('',#97953,#48807,#48808);
#38496=AXIS2_PLACEMENT_3D('',#97955,#48809,#48810);
#38497=AXIS2_PLACEMENT_3D('',#97959,#48812,#48813);
#38498=AXIS2_PLACEMENT_3D('',#97961,#48814,#48815);
#38499=AXIS2_PLACEMENT_3D('',#97963,#48816,#48817);
#38500=AXIS2_PLACEMENT_3D('',#97965,#48818,#48819);
#38501=AXIS2_PLACEMENT_3D('',#97967,#48820,#48821);
#38502=AXIS2_PLACEMENT_3D('',#97969,#48822,#48823);
#38503=AXIS2_PLACEMENT_3D('',#97973,#48825,#48826);
#38504=AXIS2_PLACEMENT_3D('',#97975,#48827,#48828);
#38505=AXIS2_PLACEMENT_3D('',#97978,#48830,#48831);
#38506=AXIS2_PLACEMENT_3D('',#97979,#48832,#48833);
#38507=AXIS2_PLACEMENT_3D('',#97981,#48834,#48835);
#38508=AXIS2_PLACEMENT_3D('',#97985,#48837,#48838);
#38509=AXIS2_PLACEMENT_3D('',#97988,#48840,#48841);
#38510=AXIS2_PLACEMENT_3D('',#97989,#48842,#48843);
#38511=AXIS2_PLACEMENT_3D('',#97994,#48846,#48847);
#38512=AXIS2_PLACEMENT_3D('',#97995,#48848,#48849);
#38513=AXIS2_PLACEMENT_3D('',#97999,#48852,#48853);
#38514=AXIS2_PLACEMENT_3D('',#98001,#48854,#48855);
#38515=AXIS2_PLACEMENT_3D('',#98003,#48857,#48858);
#38516=AXIS2_PLACEMENT_3D('',#98007,#48861,#48862);
#38517=AXIS2_PLACEMENT_3D('',#98010,#48864,#48865);
#38518=AXIS2_PLACEMENT_3D('',#98011,#48866,#48867);
#38519=AXIS2_PLACEMENT_3D('',#98014,#48869,#48870);
#38520=AXIS2_PLACEMENT_3D('',#98015,#48871,#48872);
#38521=AXIS2_PLACEMENT_3D('',#98019,#48875,#48876);
#38522=AXIS2_PLACEMENT_3D('',#98021,#48877,#48878);
#38523=AXIS2_PLACEMENT_3D('',#98023,#48880,#48881);
#38524=AXIS2_PLACEMENT_3D('',#98025,#48882,#48883);
#38525=AXIS2_PLACEMENT_3D('',#98027,#48885,#48886);
#38526=AXIS2_PLACEMENT_3D('',#98029,#48887,#48888);
#38527=AXIS2_PLACEMENT_3D('',#98031,#48890,#48891);
#38528=AXIS2_PLACEMENT_3D('',#98034,#48893,#48894);
#38529=AXIS2_PLACEMENT_3D('',#98035,#48895,#48896);
#38530=AXIS2_PLACEMENT_3D('',#98038,#48898,#48899);
#38531=AXIS2_PLACEMENT_3D('',#98039,#48900,#48901);
#38532=AXIS2_PLACEMENT_3D('',#98042,#48903,#48904);
#38533=AXIS2_PLACEMENT_3D('',#98043,#48905,#48906);
#38534=AXIS2_PLACEMENT_3D('',#98047,#48909,#48910);
#38535=AXIS2_PLACEMENT_3D('',#98049,#48911,#48912);
#38536=AXIS2_PLACEMENT_3D('',#98051,#48914,#48915);
#38537=AXIS2_PLACEMENT_3D('',#98054,#48917,#48918);
#38538=AXIS2_PLACEMENT_3D('',#98055,#48919,#48920);
#38539=AXIS2_PLACEMENT_3D('',#98057,#48921,#48922);
#38540=AXIS2_PLACEMENT_3D('',#98059,#48924,#48925);
#38541=AXIS2_PLACEMENT_3D('',#98063,#48928,#48929);
#38542=AXIS2_PLACEMENT_3D('',#98066,#48931,#48932);
#38543=AXIS2_PLACEMENT_3D('',#98067,#48933,#48934);
#38544=AXIS2_PLACEMENT_3D('',#98070,#48936,#48937);
#38545=AXIS2_PLACEMENT_3D('',#98071,#48938,#48939);
#38546=AXIS2_PLACEMENT_3D('',#98074,#48941,#48942);
#38547=AXIS2_PLACEMENT_3D('',#98075,#48943,#48944);
#38548=AXIS2_PLACEMENT_3D('',#98077,#48945,#48946);
#38549=AXIS2_PLACEMENT_3D('',#98079,#48948,#48949);
#38550=AXIS2_PLACEMENT_3D('',#98082,#48951,#48952);
#38551=AXIS2_PLACEMENT_3D('',#98083,#48953,#48954);
#38552=AXIS2_PLACEMENT_3D('',#98085,#48955,#48956);
#38553=AXIS2_PLACEMENT_3D('',#98087,#48958,#48959);
#38554=AXIS2_PLACEMENT_3D('',#98091,#48962,#48963);
#38555=AXIS2_PLACEMENT_3D('',#98092,#48964,#48965);
#38556=AXIS2_PLACEMENT_3D('',#98093,#48966,#48967);
#38557=AXIS2_PLACEMENT_3D('',#98095,#48968,#48969);
#38558=AXIS2_PLACEMENT_3D('',#98097,#48971,#48972);
#38559=AXIS2_PLACEMENT_3D('',#98099,#48974,#48975);
#38560=AXIS2_PLACEMENT_3D('',#98103,#48978,#48979);
#38561=AXIS2_PLACEMENT_3D('',#98104,#48980,#48981);
#38562=AXIS2_PLACEMENT_3D('',#98105,#48982,#48983);
#38563=AXIS2_PLACEMENT_3D('',#98107,#48984,#48985);
#38564=AXIS2_PLACEMENT_3D('',#98109,#48987,#48988);
#38565=AXIS2_PLACEMENT_3D('',#98111,#48990,#48991);
#38566=AXIS2_PLACEMENT_3D('',#98114,#48993,#48994);
#38567=AXIS2_PLACEMENT_3D('',#98116,#48995,#48996);
#38568=AXIS2_PLACEMENT_3D('',#98118,#48998,#48999);
#38569=AXIS2_PLACEMENT_3D('',#98120,#49001,#49002);
#38570=AXIS2_PLACEMENT_3D('',#98121,#49003,#49004);
#38571=AXIS2_PLACEMENT_3D('',#98123,#49005,#49006);
#38572=AXIS2_PLACEMENT_3D('',#98124,#49007,#49008);
#38573=AXIS2_PLACEMENT_3D('',#98125,#49009,#49010);
#38574=AXIS2_PLACEMENT_3D('',#98127,#49012,#49013);
#38575=AXIS2_PLACEMENT_3D('',#98130,#49015,#49016);
#38576=AXIS2_PLACEMENT_3D('',#98131,#49017,#49018);
#38577=AXIS2_PLACEMENT_3D('',#98133,#49020,#49021);
#38578=AXIS2_PLACEMENT_3D('',#98135,#49022,#49023);
#38579=AXIS2_PLACEMENT_3D('',#98136,#49024,#49025);
#38580=AXIS2_PLACEMENT_3D('',#98137,#49026,#49027);
#38581=AXIS2_PLACEMENT_3D('',#98139,#49029,#49030);
#38582=AXIS2_PLACEMENT_3D('',#98142,#49032,#49033);
#38583=AXIS2_PLACEMENT_3D('',#98143,#49034,#49035);
#38584=AXIS2_PLACEMENT_3D('',#98182,#49037,#49038);
#38585=AXIS2_PLACEMENT_3D('',#98194,#49039,#49040);
#38586=AXIS2_PLACEMENT_3D('',#98195,#49041,#49042);
#38587=AXIS2_PLACEMENT_3D('',#98196,#49043,#49044);
#38588=AXIS2_PLACEMENT_3D('',#98197,#49045,#49046);
#38589=AXIS2_PLACEMENT_3D('',#98198,#49047,#49048);
#38590=AXIS2_PLACEMENT_3D('',#98199,#49049,#49050);
#38591=AXIS2_PLACEMENT_3D('',#98201,#49052,#49053);
#38592=AXIS2_PLACEMENT_3D('',#98203,#49054,#49055);
#38593=AXIS2_PLACEMENT_3D('',#98204,#49056,#49057);
#38594=AXIS2_PLACEMENT_3D('',#98205,#49058,#49059);
#38595=AXIS2_PLACEMENT_3D('',#98251,#49061,#49062);
#38596=AXIS2_PLACEMENT_3D('',#98252,#49063,#49064);
#38597=AXIS2_PLACEMENT_3D('',#98253,#49065,#49066);
#38598=AXIS2_PLACEMENT_3D('',#98254,#49067,#49068);
#38599=AXIS2_PLACEMENT_3D('',#98255,#49069,#49070);
#38600=AXIS2_PLACEMENT_3D('',#98256,#49071,#49072);
#38601=AXIS2_PLACEMENT_3D('',#98257,#49073,#49074);
#38602=AXIS2_PLACEMENT_3D('',#98258,#49075,#49076);
#38603=AXIS2_PLACEMENT_3D('',#98262,#49079,#49080);
#38604=AXIS2_PLACEMENT_3D('',#98266,#49083,#49084);
#38605=AXIS2_PLACEMENT_3D('',#98268,#49086,#49087);
#38606=AXIS2_PLACEMENT_3D('',#98269,#49088,#49089);
#38607=AXIS2_PLACEMENT_3D('',#98270,#49090,#49091);
#38608=AXIS2_PLACEMENT_3D('',#98271,#49092,#49093);
#38609=AXIS2_PLACEMENT_3D('',#98272,#49094,#49095);
#38610=AXIS2_PLACEMENT_3D('',#98273,#49096,#49097);
#38611=AXIS2_PLACEMENT_3D('',#98274,#49098,#49099);
#38612=AXIS2_PLACEMENT_3D('',#98275,#49100,#49101);
#38613=AXIS2_PLACEMENT_3D('',#98276,#49102,#49103);
#38614=AXIS2_PLACEMENT_3D('',#98277,#49104,#49105);
#38615=AXIS2_PLACEMENT_3D('',#98278,#49106,#49107);
#38616=DIRECTION('axis',(0.,0.,1.));
#38617=DIRECTION('refdir',(1.,0.,0.));
#38618=DIRECTION('axis',(0.,0.,1.));
#38619=DIRECTION('refdir',(1.,0.,0.));
#38620=DIRECTION('center_axis',(1.,-1.7744788353171E-14,4.9634756259259E-15));
#38621=DIRECTION('ref_axis',(-1.3170890159705E-14,-0.50000000000019,0.866025403784329));
#38622=DIRECTION('center_axis',(1.,0.,0.));
#38623=DIRECTION('ref_axis',(0.,1.,0.));
#38624=DIRECTION('',(-0.707106781186874,-0.353553390593237,0.612372435695439));
#38625=DIRECTION('center_axis',(1.,0.,0.));
#38626=DIRECTION('ref_axis',(0.,1.,0.));
#38627=DIRECTION('center_axis',(1.,0.,0.));
#38628=DIRECTION('ref_axis',(0.,1.,0.));
#38629=DIRECTION('center_axis',(1.,0.,0.));
#38630=DIRECTION('ref_axis',(0.,1.,0.));
#38631=DIRECTION('center_axis',(1.,1.11593432733E-14,6.44284984283E-15));
#38632=DIRECTION('ref_axis',(-1.11593432733E-14,1.,-4.86402894982592E-32));
#38633=DIRECTION('',(-1.,0.,0.));
#38634=DIRECTION('center_axis',(1.,1.11593432733E-14,6.44284984283E-15));
#38635=DIRECTION('ref_axis',(-1.11593432733E-14,1.,-4.86402894982592E-32));
#38636=DIRECTION('center_axis',(1.,0.,0.));
#38637=DIRECTION('ref_axis',(0.,1.,0.));
#38638=DIRECTION('center_axis',(-1.,-1.7744788353171E-14,4.9634756259259E-15));
#38639=DIRECTION('ref_axis',(1.3170890159705E-14,-0.50000000000019,0.866025403784329));
#38640=DIRECTION('',(0.707106781186874,-0.353553390593237,0.612372435695439));
#38641=DIRECTION('center_axis',(1.,0.,0.));
#38642=DIRECTION('ref_axis',(0.,1.,0.));
#38643=DIRECTION('center_axis',(1.,0.,0.));
#38644=DIRECTION('ref_axis',(0.,1.,0.));
#38645=DIRECTION('axis',(0.,0.,1.));
#38646=DIRECTION('refdir',(1.,0.,0.));
#38647=DIRECTION('center_axis',(2.44929359829375E-16,1.,-1.22464679914625E-16));
#38648=DIRECTION('ref_axis',(0.70655827709904,-8.63941405564051E-17,0.707654860128041));
#38649=DIRECTION('',(0.,-1.,0.));
#38650=DIRECTION('center_axis',(-1.56278055360592E-9,-1.,3.44451669369109E-9));
#38651=DIRECTION('ref_axis',(0.706558277096871,1.33333344365384E-9,0.707654860130206));
#38652=DIRECTION('',(-2.96059473233E-16,-1.,0.));
#38653=DIRECTION('center_axis',(-2.44929359829E-16,-1.,1.22464679915E-16));
#38654=DIRECTION('ref_axis',(1.,-2.44929359829E-16,2.99951956532444E-32));
#38655=DIRECTION('center_axis',(-2.44929359829E-16,-1.,1.22464679915E-16));
#38656=DIRECTION('ref_axis',(-1.,2.44929359829E-16,0.));
#38657=DIRECTION('',(3.9900198549E-16,0.,-1.));
#38658=DIRECTION('center_axis',(-2.44929359829E-16,-1.,1.22464679915E-16));
#38659=DIRECTION('ref_axis',(1.,-2.44929359829E-16,2.99951956532444E-32));
#38660=DIRECTION('center_axis',(-2.44929359829E-16,-1.,1.22464679915E-16));
#38661=DIRECTION('ref_axis',(1.,-2.44929359829E-16,5.91180967883826E-34));
#38662=DIRECTION('center_axis',(-2.44929359829E-16,-1.,1.22464679915E-16));
#38663=DIRECTION('ref_axis',(1.,-2.44929359829E-16,2.99951956532443E-32));
#38664=DIRECTION('',(0.716064653814028,0.,0.698033961608027));
#38665=DIRECTION('center_axis',(2.44929359829E-16,1.,-1.22464679915E-16));
#38666=DIRECTION('ref_axis',(1.,-2.44929359829E-16,2.99951956532444E-32));
#38667=DIRECTION('',(0.698033961608027,-4.30707715433016E-16,-0.716064653814028));
#38668=DIRECTION('center_axis',(2.44929359829E-16,1.,-1.22464679915E-16));
#38669=DIRECTION('ref_axis',(1.,-2.44929359829E-16,2.99951956532444E-32));
#38670=DIRECTION('',(-0.716064653814028,0.,-0.698033961608027));
#38671=DIRECTION('center_axis',(-2.44929359829E-16,-1.,1.22464679915E-16));
#38672=DIRECTION('ref_axis',(1.,-2.44929359829E-16,2.99951956532443E-32));
#38673=DIRECTION('center_axis',(-2.44929359829E-16,-1.,1.22464679915E-16));
#38674=DIRECTION('ref_axis',(1.,-2.44929359829E-16,5.91180967883826E-34));
#38675=DIRECTION('center_axis',(-2.44929359829E-16,-1.,1.22464679915E-16));
#38676=DIRECTION('ref_axis',(1.,-2.44929359829E-16,2.99951956532443E-32));
#38677=DIRECTION('',(-0.716064653814028,2.5912401877601E-16,0.698033961608027));
#38678=DIRECTION('center_axis',(2.44929359829E-16,1.,-1.22464679915E-16));
#38679=DIRECTION('ref_axis',(1.,-2.44929359829E-16,2.99951956532444E-32));
#38680=DIRECTION('',(0.698033961608027,0.,0.716064653814028));
#38681=DIRECTION('center_axis',(2.44929359829E-16,1.,-1.22464679915E-16));
#38682=DIRECTION('ref_axis',(1.,-2.44929359829E-16,2.99951956532444E-32));
#38683=DIRECTION('',(0.716064653814028,-2.6102542122301E-16,-0.698033961608027));
#38684=DIRECTION('center_axis',(-2.44929359829E-16,-1.,1.22464679915E-16));
#38685=DIRECTION('ref_axis',(1.,-2.44929359829E-16,2.99951956532443E-32));
#38686=DIRECTION('center_axis',(-2.44929359829E-16,-1.,1.22464679915E-16));
#38687=DIRECTION('ref_axis',(1.,-2.44929359829E-16,6.68589598176748E-33));
#38688=DIRECTION('center_axis',(-2.44929359829E-16,-1.,1.22464679915E-16));
#38689=DIRECTION('ref_axis',(1.,-2.44929359829E-16,2.99951956532444E-32));
#38690=DIRECTION('',(-3.9900198549E-16,0.,1.));
#38691=DIRECTION('center_axis',(-2.44929359829E-16,-1.,1.22464679915E-16));
#38692=DIRECTION('ref_axis',(1.,-2.44929359829E-16,2.99951956532444E-32));
#38693=DIRECTION('center_axis',(-2.44929359829E-16,-1.,1.22464679915E-16));
#38694=DIRECTION('ref_axis',(1.,-2.44929359829E-16,-2.37876790876508E-32));
#38695=DIRECTION('center_axis',(-2.44929359829E-16,-1.,1.22464679915E-16));
#38696=DIRECTION('ref_axis',(1.,-2.44929359829E-16,2.99951956532443E-32));
#38697=DIRECTION('',(-0.716064653814028,0.,-0.698033961608027));
#38698=DIRECTION('center_axis',(2.44929359829E-16,1.,-1.22464679915E-16));
#38699=DIRECTION('ref_axis',(1.,-2.44929359829E-16,2.99951956532444E-32));
#38700=DIRECTION('',(-0.698033961608027,4.30707715433016E-16,0.716064653814028));
#38701=DIRECTION('center_axis',(2.44929359829E-16,1.,-1.22464679915E-16));
#38702=DIRECTION('ref_axis',(1.,-2.44929359829E-16,2.99951956532444E-32));
#38703=DIRECTION('',(0.716064653814028,0.,0.698033961608027));
#38704=DIRECTION('center_axis',(-2.44929359829E-16,-1.,1.22464679915E-16));
#38705=DIRECTION('ref_axis',(1.,-2.44929359829E-16,2.99951956532443E-32));
#38706=DIRECTION('center_axis',(-2.44929359829E-16,-1.,1.22464679915E-16));
#38707=DIRECTION('ref_axis',(1.,-2.44929359829E-16,5.91180967883826E-34));
#38708=DIRECTION('center_axis',(-2.44929359829E-16,-1.,1.22464679915E-16));
#38709=DIRECTION('ref_axis',(1.,-2.44929359829E-16,2.99951956532443E-32));
#38710=DIRECTION('',(0.716064653814028,-2.6393829599301E-16,-0.698033961608027));
#38711=DIRECTION('center_axis',(2.44929359829E-16,1.,-1.22464679915E-16));
#38712=DIRECTION('ref_axis',(1.,-2.44929359829E-16,2.99951956532443E-32));
#38713=DIRECTION('',(-0.698033961608027,0.,-0.716064653814028));
#38714=DIRECTION('center_axis',(2.44929359829E-16,1.,-1.22464679915E-16));
#38715=DIRECTION('ref_axis',(1.,-2.44929359829E-16,2.99951956532444E-32));
#38716=DIRECTION('',(-0.716064653814028,2.6591127623201E-16,0.698033961608027));
#38717=DIRECTION('center_axis',(-2.44929359829E-16,-1.,1.22464679915E-16));
#38718=DIRECTION('ref_axis',(1.,-2.44929359829E-16,2.99951956532443E-32));
#38719=DIRECTION('center_axis',(-2.44929359829E-16,-1.,1.22464679915E-16));
#38720=DIRECTION('ref_axis',(1.,-2.44929359829E-16,-2.37876790876508E-32));
#38721=DIRECTION('center_axis',(-2.44929359829E-16,-1.,1.22464679915E-16));
#38722=DIRECTION('ref_axis',(1.,-2.44929359829E-16,2.99951956532444E-32));
#38723=DIRECTION('center_axis',(2.44929359829E-16,1.,-1.22464679915E-16));
#38724=DIRECTION('ref_axis',(1.,-2.44929359829E-16,2.99951956532444E-32));
#38725=DIRECTION('center_axis',(2.44929359829E-16,1.,-1.22464679915E-16));
#38726=DIRECTION('ref_axis',(1.,-2.44929359829E-16,2.99951956532443E-32));
#38727=DIRECTION('',(4.20437734738E-16,0.,-1.));
#38728=DIRECTION('center_axis',(2.44929359829E-16,1.,-1.22464679915E-16));
#38729=DIRECTION('ref_axis',(1.,-2.44929359829E-16,2.99951956532443E-32));
#38730=DIRECTION('center_axis',(2.44929359829E-16,1.,-1.22464679915E-16));
#38731=DIRECTION('ref_axis',(1.,-2.44929359829E-16,2.99951956532444E-32));
#38732=DIRECTION('center_axis',(-2.44929359829E-16,-1.,1.22464679915E-16));
#38733=DIRECTION('ref_axis',(1.,-2.44929359829E-16,2.99951956532443E-32));
#38734=DIRECTION('center_axis',(-2.44929359829E-16,-1.,1.22464679915E-16));
#38735=DIRECTION('ref_axis',(1.,-2.44929359829E-16,2.99951956532444E-32));
#38736=DIRECTION('',(-0.0656339938339316,0.,0.99784376475148));
#38737=DIRECTION('center_axis',(-2.44929359829E-16,-1.,1.22464679915E-16));
#38738=DIRECTION('ref_axis',(1.,-2.44929359829E-16,2.99951956532443E-32));
#38739=DIRECTION('center_axis',(2.44929359829E-16,1.,-1.22464679915E-16));
#38740=DIRECTION('ref_axis',(1.,-2.44929359829E-16,2.99951956532443E-32));
#38741=DIRECTION('center_axis',(2.44929359829E-16,1.,-1.22464679915E-16));
#38742=DIRECTION('ref_axis',(1.,-2.44929359829E-16,2.99951956532444E-32));
#38743=DIRECTION('',(0.0656339938339316,0.,0.99784376475148));
#38744=DIRECTION('',(4.20437734738E-16,0.,-1.));
#38745=DIRECTION('center_axis',(-2.44929359829E-16,-1.,1.22464679915E-16));
#38746=DIRECTION('ref_axis',(1.,-2.44929359829E-16,2.99951956532444E-32));
#38747=DIRECTION('center_axis',(-2.44929359829E-16,-1.,1.22464679915E-16));
#38748=DIRECTION('ref_axis',(1.,-2.44929359829E-16,2.99951956532444E-32));
#38749=DIRECTION('center_axis',(-2.44929359829E-16,-1.,1.22464679915E-16));
#38750=DIRECTION('ref_axis',(1.,-2.44929359829E-16,2.99951956532444E-32));
#38751=DIRECTION('',(-0.288070798801296,0.943889906160958,0.161514890723551));
#38752=DIRECTION('',(-0.185892369076962,0.87281982032212,0.451253352754101));
#38753=DIRECTION('center_axis',(0.631948690569006,-0.772532669185509,-0.0619203321150045));
#38754=DIRECTION('ref_axis',(-0.212600461685972,-0.249632918685971,0.944713951203874));
#38755=DIRECTION('center_axis',(-0.0594793302428471,-0.422789452293976,
0.904273901150986));
#38756=DIRECTION('ref_axis',(0.74528916761046,0.583836479538853,0.321992269786383));
#38757=DIRECTION('center_axis',(-0.629470113233292,0.456900095359148,0.628497954974293));
#38758=DIRECTION('ref_axis',(0.745284573628305,0.583834639915972,0.322006238364825));
#38759=DIRECTION('center_axis',(-1.,2.44929359829E-16,-4.93371725307E-16));
#38760=DIRECTION('ref_axis',(-4.93371725307E-16,0.,1.));
#38761=DIRECTION('',(3.93680872405E-16,0.,-1.));
#38762=DIRECTION('',(0.,-1.,0.));
#38763=DIRECTION('',(3.70074341542E-16,0.,-1.));
#38764=DIRECTION('',(0.,-1.,0.));
#38765=DIRECTION('',(2.1147105231E-16,1.,0.));
#38766=DIRECTION('',(4.22942104619E-16,1.,0.));
#38767=DIRECTION('center_axis',(2.44929359829E-16,1.,-1.22464679915E-16));
#38768=DIRECTION('ref_axis',(-1.,2.44929359829E-16,-2.99951956532444E-32));
#38769=DIRECTION('',(2.67621944414E-16,1.,-1.07048777765E-15));
#38770=DIRECTION('center_axis',(-0.455243749742543,-0.0346073179899924,
0.889694027102514));
#38771=DIRECTION('ref_axis',(0.0631992828870565,-0.997979881587316,-0.00648124907159732));
#38772=DIRECTION('center_axis',(1.,-2.44929359829E-16,3.67394039744E-16));
#38773=DIRECTION('ref_axis',(-3.67394039744E-16,0.,1.));
#38774=DIRECTION('',(2.1147105231E-16,1.,0.));
#38775=DIRECTION('',(0.,0.,-1.));
#38776=DIRECTION('center_axis',(2.44929359829009E-16,1.,-1.22464679915049E-16));
#38777=DIRECTION('ref_axis',(0.17719394991793,-1.63926793636935E-16,-0.984175951805612));
#38778=DIRECTION('',(2.96059473233E-16,1.,0.));
#38779=DIRECTION('center_axis',(0.164797595711241,-0.072937415919611,-0.983626903763192));
#38780=DIRECTION('ref_axis',(-0.00994679585199009,0.997088453026087,-0.0756021037691614));
#38781=DIRECTION('center_axis',(-0.996740111917573,-0.0806792990324772,
-1.47358394346062E-6));
#38782=DIRECTION('ref_axis',(0.080679298682933,-0.996740105534059,-0.000113066272843588));
#38783=DIRECTION('',(1.18423789293E-15,1.,-1.48029736617E-16));
#38784=DIRECTION('center_axis',(-0.815291085828504,-0.452356370985093,0.361488808952332));
#38785=DIRECTION('ref_axis',(0.410559632229298,-0.0113482213864199,0.911763130563585));
#38786=DIRECTION('center_axis',(-0.181645839985608,-0.207917305089807,0.961132240152267));
#38787=DIRECTION('ref_axis',(0.0696529687957434,-0.977657575872474,-0.198328334529125));
#38788=DIRECTION('',(1.18423789293E-15,1.,0.));
#38789=DIRECTION('',(0.,1.,0.));
#38790=DIRECTION('center_axis',(0.062548597995711,-0.99472870449491,-0.0812556296058808));
#38791=DIRECTION('ref_axis',(0.441715695037133,0.100598146276716,-0.891497200064897));
#38792=DIRECTION('',(0.,1.,0.));
#38793=DIRECTION('',(4.22942104619E-16,1.,0.));
#38794=DIRECTION('center_axis',(2.44929359828923E-16,1.,-1.22464679914962E-16));
#38795=DIRECTION('ref_axis',(-0.898888448298522,2.73825444514855E-16,0.438177541089767));
#38796=DIRECTION('center_axis',(-0.891374682075179,-0.0362585643310429,
0.451814666282565));
#38797=DIRECTION('ref_axis',(0.0137554448307947,-0.998500150383736,-0.0529928053717017));
#38798=DIRECTION('center_axis',(-2.44929359829E-16,-1.,1.22464679915E-16));
#38799=DIRECTION('ref_axis',(1.,-2.44929359829E-16,2.99951956532444E-32));
#38800=DIRECTION('',(2.96059473233E-16,1.,-5.92118946467E-16));
#38801=DIRECTION('center_axis',(-0.455243749742543,0.0346073179899924,-0.889694027102514));
#38802=DIRECTION('ref_axis',(0.0631992828870565,0.997979881587316,0.00648124907159732));
#38803=DIRECTION('',(2.67621944414E-16,1.,-1.07048777765E-15));
#38804=DIRECTION('',(4.22942104619E-16,1.,0.));
#38805=DIRECTION('center_axis',(-2.44929359828974E-16,-1.,1.22464679915013E-16));
#38806=DIRECTION('ref_axis',(0.898888448298522,-1.66502899883911E-16,0.438177541089767));
#38807=DIRECTION('',(0.,1.,0.));
#38808=DIRECTION('center_axis',(-0.891374682075179,0.0362585643310429,-0.451814666282565));
#38809=DIRECTION('ref_axis',(0.0137554448307947,0.998500150383736,0.0529928053717017));
#38810=DIRECTION('',(0.,1.,0.));
#38811=DIRECTION('',(0.,1.,0.));
#38812=DIRECTION('',(1.18423789293E-15,1.,0.));
#38813=DIRECTION('center_axis',(0.062548597995711,0.99472870449491,0.0812556296058808));
#38814=DIRECTION('ref_axis',(0.441715695037133,-0.100598146276716,0.891497200064897));
#38815=DIRECTION('',(1.18423789293E-15,1.,-1.48029736617E-16));
#38816=DIRECTION('',(2.1147105231E-16,1.,0.));
#38817=DIRECTION('center_axis',(-0.181645839985592,0.207917305090092,-0.961132240152208));
#38818=DIRECTION('ref_axis',(-0.0696529687957387,-0.977657575872416,-0.198328334529416));
#38819=DIRECTION('center_axis',(-0.815291085828504,0.452356370985093,-0.361488808952332));
#38820=DIRECTION('ref_axis',(0.410559632229298,0.0113482213864199,-0.911763130563585));
#38821=DIRECTION('center_axis',(-2.44929359829084E-16,-1.,1.22464679914533E-16));
#38822=DIRECTION('ref_axis',(-0.17719394991793,-7.71267921984697E-17,-0.984175951805612));
#38823=DIRECTION('',(2.67621944414E-16,1.,-1.07048777765E-15));
#38824=DIRECTION('center_axis',(-0.996740111917573,0.0806792990324772,1.47358394346062E-6));
#38825=DIRECTION('ref_axis',(0.080679298682933,0.996740105534059,0.000113066272843588));
#38826=DIRECTION('center_axis',(0.164797595711241,0.072937415919611,0.983626903763192));
#38827=DIRECTION('ref_axis',(-0.00994679585199009,-0.997088453026087,0.0756021037691614));
#38828=DIRECTION('center_axis',(1.,-2.44929359829E-16,3.67394039744E-16));
#38829=DIRECTION('ref_axis',(-3.67394039744E-16,0.,1.));
#38830=DIRECTION('',(0.,0.,-1.));
#38831=DIRECTION('center_axis',(-2.44929359829E-16,-1.,1.22464679915E-16));
#38832=DIRECTION('ref_axis',(-7.42634721754E-16,1.22464679915E-16,1.));
#38833=DIRECTION('center_axis',(-2.44929359829E-16,-1.,1.22464679915E-16));
#38834=DIRECTION('ref_axis',(1.,-2.44929359829E-16,6.54860237547756E-33));
#38835=DIRECTION('',(0.,-1.,0.));
#38836=DIRECTION('center_axis',(-2.44929359829E-16,-1.,1.22464679915E-16));
#38837=DIRECTION('ref_axis',(1.,-2.44929359829E-16,6.83249535077049E-33));
#38838=DIRECTION('',(0.,-1.,0.));
#38839=DIRECTION('center_axis',(-2.18773443555785E-16,-1.,1.58554584738017E-16));
#38840=DIRECTION('ref_axis',(0.586831315816962,0.,0.809709211245947));
#38841=DIRECTION('center_axis',(-0.809709211245947,2.70187668013982E-16,
0.586831315816962));
#38842=DIRECTION('ref_axis',(0.586831315816962,-1.3944828999061E-30,0.809709211245947));
#38843=DIRECTION('center_axis',(-0.828419399070054,1.34310750335009E-16,
-0.560108292426036));
#38844=DIRECTION('ref_axis',(0.560108292426036,6.83578973261393E-31,-0.828419399070054));
#38845=DIRECTION('center_axis',(-6.43747505554034E-17,-1.,-6.27537777746355E-17));
#38846=DIRECTION('ref_axis',(0.698033961608026,0.,-0.716064653814029));
#38847=DIRECTION('center_axis',(0.716064653814028,-8.99007515774035E-17,
0.698033961608027));
#38848=DIRECTION('ref_axis',(0.698033961608027,-7.96736102322353E-31,-0.716064653814028));
#38849=DIRECTION('center_axis',(-2.44929359829E-16,-1.,1.22464679915E-16));
#38850=DIRECTION('ref_axis',(1.,-2.44929359829E-16,2.99951956532444E-32));
#38851=DIRECTION('center_axis',(2.44929359829294E-16,1.,-1.22464679914594E-16));
#38852=DIRECTION('ref_axis',(0.586831315816961,-4.4571439131697E-17,0.809709211245947));
#38853=DIRECTION('',(-4.80096443081E-16,-1.,0.));
#38854=DIRECTION('center_axis',(-2.44929359829E-16,-1.,1.22464679915E-16));
#38855=DIRECTION('ref_axis',(1.,-2.44929359829E-16,2.99951956532444E-32));
#38856=DIRECTION('center_axis',(0.716064653814028,-8.990075157705E-17,0.698033961608027));
#38857=DIRECTION('ref_axis',(-3.28514270034646E-16,-1.,2.08208645226189E-16));
#38858=DIRECTION('center_axis',(0.716064653814028,-8.99007515774035E-17,
0.698033961608027));
#38859=DIRECTION('ref_axis',(0.698033961608027,-7.96736102322353E-31,-0.716064653814028));
#38860=DIRECTION('',(0.716064653814028,0.,0.698033961608027));
#38861=DIRECTION('center_axis',(0.698033961608027,-2.5866163998301E-16,
-0.716064653814028));
#38862=DIRECTION('ref_axis',(-5.0987642944624E-33,-1.,3.6122665544973E-16));
#38863=DIRECTION('',(0.,1.,0.));
#38864=DIRECTION('',(0.716064653814028,0.,0.698033961608027));
#38865=DIRECTION('center_axis',(-6.43747505554034E-17,-1.,-6.27537777746355E-17));
#38866=DIRECTION('ref_axis',(-0.698033961608025,0.,0.71606465381403));
#38867=DIRECTION('center_axis',(-0.698033961608027,2.5866163998301E-16,
0.716064653814028));
#38868=DIRECTION('ref_axis',(0.716064653814028,2.30891390163356E-30,0.698033961608027));
#38869=DIRECTION('center_axis',(2.44929359829E-16,1.,-1.22464679915E-16));
#38870=DIRECTION('ref_axis',(1.,-2.44929359829E-16,2.99951956532444E-32));
#38871=DIRECTION('center_axis',(-2.44929359828773E-16,-1.,1.22464679914767E-16));
#38872=DIRECTION('ref_axis',(-0.698033961608027,2.5866163998301E-16,0.716064653814028));
#38873=DIRECTION('',(4.80096443081E-16,1.,0.));
#38874=DIRECTION('center_axis',(2.44929359829E-16,1.,-1.22464679915E-16));
#38875=DIRECTION('ref_axis',(1.,-2.44929359829E-16,2.99951956532444E-32));
#38876=DIRECTION('center_axis',(-0.698033961608027,2.58661639983637E-16,
0.716064653814028));
#38877=DIRECTION('ref_axis',(-1.80554609273807E-16,-1.,1.85218457689851E-16));
#38878=DIRECTION('center_axis',(-0.698033961608027,2.5866163998301E-16,
0.716064653814028));
#38879=DIRECTION('ref_axis',(0.716064653814028,2.30891390163356E-30,0.698033961608027));
#38880=DIRECTION('',(-0.698033961608027,0.,0.716064653814028));
#38881=DIRECTION('center_axis',(0.716064653814028,-8.99007515774035E-17,
0.698033961608027));
#38882=DIRECTION('ref_axis',(-2.12219958443594E-33,-1.,-1.28791371941708E-16));
#38883=DIRECTION('',(0.,1.,0.));
#38884=DIRECTION('',(-0.698033961608027,4.30707715433016E-16,0.716064653814028));
#38885=DIRECTION('center_axis',(-1.80554609273596E-16,-1.,1.85218457689635E-16));
#38886=DIRECTION('ref_axis',(-0.71606465381403,0.,-0.698033961608025));
#38887=DIRECTION('center_axis',(-0.716064653814028,8.99007515774035E-17,
-0.698033961608027));
#38888=DIRECTION('ref_axis',(0.698033961608027,-2.36964484828339E-31,-0.716064653814028));
#38889=DIRECTION('center_axis',(2.44929359829E-16,1.,-1.22464679915E-16));
#38890=DIRECTION('ref_axis',(1.,-2.44929359829E-16,2.99951956532444E-32));
#38891=DIRECTION('center_axis',(-2.44929359829491E-16,-1.,1.22464679914521E-16));
#38892=DIRECTION('ref_axis',(-0.716064653814027,8.99007515774033E-17,-0.698033961608028));
#38893=DIRECTION('',(4.80096443081E-16,1.,-2.40048221541E-16));
#38894=DIRECTION('center_axis',(2.44929359829E-16,1.,-1.22464679915E-16));
#38895=DIRECTION('ref_axis',(1.,-2.44929359829E-16,2.99951956532444E-32));
#38896=DIRECTION('center_axis',(0.716064653814028,-8.99007515774036E-17,
0.698033961608027));
#38897=DIRECTION('ref_axis',(-0.698033961608027,4.9741364910786E-33,0.716064653814028));
#38898=DIRECTION('center_axis',(-0.716064653814028,8.99007515774035E-17,
-0.698033961608027));
#38899=DIRECTION('ref_axis',(0.698033961608027,-7.96736102322353E-31,-0.716064653814028));
#38900=DIRECTION('',(-0.716064653814028,0.,-0.698033961608027));
#38901=DIRECTION('center_axis',(0.698033961608027,-2.5866163998301E-16,
-0.716064653814028));
#38902=DIRECTION('ref_axis',(-5.0987642944624E-33,-1.,3.6122665544973E-16));
#38903=DIRECTION('',(0.,-1.,0.));
#38904=DIRECTION('',(-0.716064653814028,0.,-0.698033961608027));
#38905=DIRECTION('center_axis',(-1.32057957382078E-16,-1.,1.9781552453987E-16));
#38906=DIRECTION('ref_axis',(0.831699011544245,0.,0.555226759258166));
#38907=DIRECTION('center_axis',(-0.555226759258164,2.37845087940071E-16,
0.831699011544246));
#38908=DIRECTION('ref_axis',(0.831699011544246,1.10558455272238E-30,0.555226759258164));
#38909=DIRECTION('center_axis',(-2.44929359829E-16,-1.,1.22464679915E-16));
#38910=DIRECTION('ref_axis',(1.,-2.44929359829E-16,2.99951956532444E-32));
#38911=DIRECTION('center_axis',(-2.4492935982974E-16,-1.,1.22464679914506E-16));
#38912=DIRECTION('ref_axis',(0.831699011544246,-1.3571183911604E-16,0.555226759258164));
#38913=DIRECTION('',(-4.55476112667E-16,-1.,0.));
#38914=DIRECTION('center_axis',(-2.44929359829E-16,-1.,1.22464679915E-16));
#38915=DIRECTION('ref_axis',(1.,-2.44929359829E-16,2.99951956532444E-32));
#38916=DIRECTION('center_axis',(-9.88589466193077E-17,-1.,1.96101782897063E-16));
#38917=DIRECTION('ref_axis',(0.892950553792926,0.,0.450154760588963));
#38918=DIRECTION('center_axis',(-0.450154760588963,2.19611021084982E-16,
0.892950553792926));
#38919=DIRECTION('ref_axis',(0.892950553792926,5.80220876798355E-31,0.450154760588963));
#38920=DIRECTION('center_axis',(-2.44929359829E-16,-1.,1.22464679915E-16));
#38921=DIRECTION('ref_axis',(1.,-2.44929359829E-16,6.83249535077049E-33));
#38922=DIRECTION('center_axis',(2.44929359829E-16,1.,-1.22464679915E-16));
#38923=DIRECTION('ref_axis',(7.84664226532002E-18,1.22464679915E-16,1.));
#38924=DIRECTION('',(0.,-1.,0.));
#38925=DIRECTION('center_axis',(-2.44929359829E-16,-1.,1.22464679915E-16));
#38926=DIRECTION('ref_axis',(1.,-2.44929359829E-16,-2.34494220138087E-32));
#38927=DIRECTION('center_axis',(-8.70163887007781E-31,-1.,1.22464679915002E-16));
#38928=DIRECTION('ref_axis',(1.,0.,7.105427357601E-15));
#38929=DIRECTION('center_axis',(-3.67394039744E-16,1.22464679915E-16,1.));
#38930=DIRECTION('ref_axis',(1.,4.49927934799277E-32,3.67394039744E-16));
#38931=DIRECTION('center_axis',(-2.44929359829E-16,-1.,1.22464679915E-16));
#38932=DIRECTION('ref_axis',(1.,-2.44929359829E-16,2.99951956532443E-32));
#38933=DIRECTION('center_axis',(-2.44929359829001E-16,-1.,1.22464679915E-16));
#38934=DIRECTION('ref_axis',(1.,-2.44929359829E-16,6.93889390390722E-15));
#38935=DIRECTION('',(-4.80096443081E-16,-1.,2.40048221541E-16));
#38936=DIRECTION('center_axis',(-2.44929359829E-16,-1.,1.22464679915E-16));
#38937=DIRECTION('ref_axis',(1.,-2.44929359829E-16,2.99951956532443E-32));
#38938=DIRECTION('center_axis',(3.67394039744E-16,-1.22464679915E-16,-1.));
#38939=DIRECTION('ref_axis',(1.,-4.87061678881549E-46,3.67394039744E-16));
#38940=DIRECTION('center_axis',(-3.33066907388E-16,1.22464679915E-16,1.));
#38941=DIRECTION('ref_axis',(1.,4.07889322035504E-32,3.33066907388E-16));
#38942=DIRECTION('',(-5.12480847979E-16,0.,1.));
#38943=DIRECTION('center_axis',(-1.,2.44929359829E-16,-4.93371725307E-16));
#38944=DIRECTION('ref_axis',(-4.93371725307E-16,0.,1.));
#38945=DIRECTION('',(0.,-1.,0.));
#38946=DIRECTION('',(-4.78802382588E-16,0.,1.));
#38947=DIRECTION('center_axis',(-4.05685585531587E-19,-1.,-8.04739169685281E-19));
#38948=DIRECTION('ref_axis',(0.892950553792926,0.,-0.450154760588964));
#38949=DIRECTION('center_axis',(0.450154760588963,-9.01213585416925E-19,
0.892950553792926));
#38950=DIRECTION('ref_axis',(0.892950553792926,2.40393060631611E-33,-0.450154760588963));
#38951=DIRECTION('center_axis',(-2.44929359829E-16,-1.,1.22464679915E-16));
#38952=DIRECTION('ref_axis',(1.,-2.44929359829E-16,2.99951956532443E-32));
#38953=DIRECTION('center_axis',(-2.44929359828808E-16,-1.,1.22464679914903E-16));
#38954=DIRECTION('ref_axis',(0.892950553792926,-2.73837866166978E-16,-0.450154760588963));
#38955=DIRECTION('',(0.,-1.,2.27738056333E-16));
#38956=DIRECTION('center_axis',(-2.44929359829E-16,-1.,1.22464679915E-16));
#38957=DIRECTION('ref_axis',(1.,-2.44929359829E-16,2.99951956532443E-32));
#38958=DIRECTION('center_axis',(-3.90625602496874E-16,-1.,2.19728776096112E-16));
#38959=DIRECTION('ref_axis',(0.831699011544246,-4.46882223748491E-16,-0.555226759258164));
#38960=DIRECTION('center_axis',(0.555226759258164,-3.41375814712101E-17,
0.831699011544246));
#38961=DIRECTION('ref_axis',(0.831699011544246,1.57834305747204E-31,-0.555226759258164));
#38962=DIRECTION('center_axis',(-2.44929359829E-16,-1.,1.22464679915E-16));
#38963=DIRECTION('ref_axis',(1.,-2.44929359829E-16,6.83249535077049E-33));
#38964=DIRECTION('center_axis',(2.44929359829E-16,1.,-1.22464679915E-16));
#38965=DIRECTION('ref_axis',(7.84664226532002E-18,1.22464679915E-16,1.));
#38966=DIRECTION('',(0.,-1.,0.));
#38967=DIRECTION('center_axis',(-2.44929359829E-16,-1.,1.22464679915E-16));
#38968=DIRECTION('ref_axis',(1.,-2.44929359829E-16,6.54860237547756E-33));
#38969=DIRECTION('center_axis',(-1.86799616485145E-16,-1.,1.82095954083848E-16));
#38970=DIRECTION('ref_axis',(-0.698033961608026,0.,-0.716064653814029));
#38971=DIRECTION('center_axis',(0.716064653814028,-2.6086976293301E-16,
-0.698033961608027));
#38972=DIRECTION('ref_axis',(0.698033961608027,-2.32071020223926E-30,0.716064653814028));
#38973=DIRECTION('center_axis',(-2.44929359829E-16,-1.,1.22464679915E-16));
#38974=DIRECTION('ref_axis',(1.,-2.44929359829E-16,2.99951956532444E-32));
#38975=DIRECTION('center_axis',(2.44929359829285E-16,1.,-1.2246467991519E-16));
#38976=DIRECTION('ref_axis',(0.831699011544246,-2.7170317382108E-16,-0.555226759258164));
#38977=DIRECTION('',(-4.80096443081E-16,-1.,0.));
#38978=DIRECTION('center_axis',(-2.44929359829E-16,-1.,1.22464679915E-16));
#38979=DIRECTION('ref_axis',(1.,-2.44929359829E-16,2.99951956532444E-32));
#38980=DIRECTION('center_axis',(0.716064653814028,-2.60869762933355E-16,
-0.698033961608027));
#38981=DIRECTION('ref_axis',(-1.8679961648542E-16,-1.,1.82095954084116E-16));
#38982=DIRECTION('center_axis',(0.716064653814028,-2.6086976293301E-16,
-0.698033961608027));
#38983=DIRECTION('ref_axis',(0.698033961608027,-7.02188537105379E-31,0.716064653814028));
#38984=DIRECTION('',(0.716064653814028,0.,-0.698033961608027));
#38985=DIRECTION('center_axis',(-0.698033961608027,8.32763827281032E-17,
-0.716064653814028));
#38986=DIRECTION('ref_axis',(-0.716064653814028,-6.03301243078373E-33,0.698033961608027));
#38987=DIRECTION('',(0.,1.,0.));
#38988=DIRECTION('',(0.716064653814028,-2.6102542122301E-16,-0.698033961608027));
#38989=DIRECTION('center_axis',(-1.86799616485145E-16,-1.,1.82095954083848E-16));
#38990=DIRECTION('ref_axis',(0.698033961608026,0.,0.716064653814029));
#38991=DIRECTION('center_axis',(0.698033961608027,-8.32763827281032E-17,
0.716064653814028));
#38992=DIRECTION('ref_axis',(0.716064653814028,7.37176741734741E-31,-0.698033961608027));
#38993=DIRECTION('center_axis',(2.44929359829E-16,1.,-1.22464679915E-16));
#38994=DIRECTION('ref_axis',(1.,-2.44929359829E-16,2.99951956532444E-32));
#38995=DIRECTION('center_axis',(-2.44929359829229E-16,-1.,1.22464679914765E-16));
#38996=DIRECTION('ref_axis',(0.698033961608028,-8.32763827281037E-17,0.716064653814027));
#38997=DIRECTION('',(4.80096443081E-16,1.,-2.40048221541E-16));
#38998=DIRECTION('center_axis',(2.44929359829E-16,1.,-1.22464679915E-16));
#38999=DIRECTION('ref_axis',(1.,-2.44929359829E-16,2.99951956532444E-32));
#39000=DIRECTION('center_axis',(-0.698033961608027,8.32763827281032E-17,
-0.716064653814028));
#39001=DIRECTION('ref_axis',(0.716064653814028,7.37176741734741E-31,-0.698033961608027));
#39002=DIRECTION('center_axis',(0.698033961608027,-8.32763827281032E-17,
0.716064653814028));
#39003=DIRECTION('ref_axis',(0.716064653814028,7.37176741734741E-31,-0.698033961608027));
#39004=DIRECTION('',(0.698033961608027,0.,0.716064653814028));
#39005=DIRECTION('center_axis',(-0.716064653814028,2.6086976293301E-16,
0.698033961608027));
#39006=DIRECTION('ref_axis',(3.64310347597135E-16,1.,-2.26745038145461E-32));
#39007=DIRECTION('',(0.,1.,0.));
#39008=DIRECTION('',(0.698033961608027,0.,0.716064653814028));
#39009=DIRECTION('center_axis',(-5.81297433438548E-17,-1.,-5.96312741688484E-17));
#39010=DIRECTION('ref_axis',(-0.71606465381403,0.,0.698033961608025));
#39011=DIRECTION('center_axis',(-0.716064653814028,2.6086976293301E-16,
0.698033961608027));
#39012=DIRECTION('ref_axis',(0.698033961608027,-2.32071020223926E-30,0.716064653814028));
#39013=DIRECTION('center_axis',(2.44929359829E-16,1.,-1.22464679915E-16));
#39014=DIRECTION('ref_axis',(1.,-2.44929359829E-16,2.99951956532444E-32));
#39015=DIRECTION('center_axis',(-2.44929359829028E-16,-1.,1.22464679915027E-16));
#39016=DIRECTION('ref_axis',(-0.716064653814028,2.6086976293301E-16,0.698033961608027));
#39017=DIRECTION('',(4.80096443081E-16,1.,0.));
#39018=DIRECTION('center_axis',(2.44929359829E-16,1.,-1.22464679915E-16));
#39019=DIRECTION('ref_axis',(1.,-2.44929359829E-16,2.99951956532444E-32));
#39020=DIRECTION('center_axis',(0.716064653814028,-2.6086976293301E-16,
-0.698033961608027));
#39021=DIRECTION('ref_axis',(0.698033961608027,-1.10143058876371E-32,0.716064653814028));
#39022=DIRECTION('center_axis',(-0.716064653814028,2.6086976293301E-16,
0.698033961608027));
#39023=DIRECTION('ref_axis',(0.698033961608027,-2.32071020223926E-30,0.716064653814028));
#39024=DIRECTION('',(-0.716064653814028,0.,0.698033961608027));
#39025=DIRECTION('center_axis',(-0.698033961608027,8.32763827281032E-17,
-0.716064653814028));
#39026=DIRECTION('ref_axis',(-0.716064653814028,-6.03301243078373E-33,0.698033961608027));
#39027=DIRECTION('',(0.,-1.,0.));
#39028=DIRECTION('',(-0.716064653814028,2.5912401877601E-16,0.698033961608027));
#39029=DIRECTION('center_axis',(-1.02392142274414E-16,-1.,-7.42080178237726E-17));
#39030=DIRECTION('ref_axis',(0.586831315816962,0.,-0.809709211245946));
#39031=DIRECTION('center_axis',(0.809709211245947,-1.26455449502992E-16,
0.586831315816962));
#39032=DIRECTION('ref_axis',(0.586831315816962,-6.48713419669698E-31,-0.809709211245947));
#39033=DIRECTION('center_axis',(-2.44929359829E-16,-1.,1.22464679915E-16));
#39034=DIRECTION('ref_axis',(1.,-2.44929359829E-16,2.99951956532444E-32));
#39035=DIRECTION('center_axis',(-2.4492935982892E-16,-1.,1.2246467991489E-16));
#39036=DIRECTION('ref_axis',(0.586831315816961,-2.42892997889984E-16,-0.809709211245947));
#39037=DIRECTION('',(0.,-1.,0.));
#39038=DIRECTION('center_axis',(-2.44929359829E-16,-1.,1.22464679915E-16));
#39039=DIRECTION('ref_axis',(1.,-2.44929359829E-16,2.99951956532444E-32));
#39040=DIRECTION('center_axis',(2.44929359829E-16,1.,-1.22464679915E-16));
#39041=DIRECTION('ref_axis',(1.14618037649415E-16,-1.22464679915E-16,-1.));
#39042=DIRECTION('center_axis',(-2.44929359829E-16,-1.,1.22464679915E-16));
#39043=DIRECTION('ref_axis',(1.,-2.44929359829E-16,7.76111877854652E-34));
#39044=DIRECTION('center_axis',(-2.44929359829E-16,-1.,1.22464679915E-16));
#39045=DIRECTION('ref_axis',(1.,-2.44929359829E-16,6.83249535077049E-33));
#39046=DIRECTION('',(0.,-1.,0.));
#39047=DIRECTION('center_axis',(-2.18773443555785E-16,-1.,1.58554584738017E-16));
#39048=DIRECTION('ref_axis',(-0.586831315816962,0.,-0.809709211245947));
#39049=DIRECTION('center_axis',(0.809709211245947,-2.70187668013982E-16,
-0.586831315816962));
#39050=DIRECTION('ref_axis',(0.586831315816962,-1.3944828999061E-30,0.809709211245947));
#39051=DIRECTION('center_axis',(-6.43747505554034E-17,-1.,-6.27537777746355E-17));
#39052=DIRECTION('ref_axis',(-0.698033961608026,0.,0.716064653814029));
#39053=DIRECTION('center_axis',(-0.716064653814028,8.99007515774035E-17,
-0.698033961608027));
#39054=DIRECTION('ref_axis',(0.698033961608027,-7.96736102322353E-31,-0.716064653814028));
#39055=DIRECTION('center_axis',(-2.44929359829E-16,-1.,1.22464679915E-16));
#39056=DIRECTION('ref_axis',(1.,-2.44929359829E-16,2.99951956532444E-32));
#39057=DIRECTION('center_axis',(2.44929359829294E-16,1.,-1.22464679914594E-16));
#39058=DIRECTION('ref_axis',(-0.586831315816961,4.4571439131697E-17,-0.809709211245947));
#39059=DIRECTION('',(-4.80096443081E-16,-1.,0.));
#39060=DIRECTION('center_axis',(-2.44929359829E-16,-1.,1.22464679915E-16));
#39061=DIRECTION('ref_axis',(1.,-2.44929359829E-16,2.99951956532444E-32));
#39062=DIRECTION('center_axis',(-0.716064653814028,8.99007515776184E-17,
-0.698033961608027));
#39063=DIRECTION('ref_axis',(-6.43747505560482E-17,-1.,-6.27537777752641E-17));
#39064=DIRECTION('center_axis',(-0.716064653814028,8.99007515774035E-17,
-0.698033961608027));
#39065=DIRECTION('ref_axis',(0.698033961608027,-7.96736102322353E-31,-0.716064653814028));
#39066=DIRECTION('',(-0.716064653814028,0.,-0.698033961608027));
#39067=DIRECTION('center_axis',(-0.698033961608027,2.5866163998301E-16,
0.716064653814028));
#39068=DIRECTION('ref_axis',(3.70557385756911E-16,1.,-1.7912467654698E-32));
#39069=DIRECTION('',(0.,1.,0.));
#39070=DIRECTION('',(-0.716064653814028,0.,-0.698033961608027));
#39071=DIRECTION('center_axis',(-6.43747505554034E-17,-1.,-6.27537777746355E-17));
#39072=DIRECTION('ref_axis',(0.698033961608025,0.,-0.71606465381403));
#39073=DIRECTION('center_axis',(0.698033961608027,-2.5866163998301E-16,
-0.716064653814028));
#39074=DIRECTION('ref_axis',(0.716064653814028,2.30891390163356E-30,0.698033961608027));
#39075=DIRECTION('center_axis',(2.44929359829E-16,1.,-1.22464679915E-16));
#39076=DIRECTION('ref_axis',(1.,-2.44929359829E-16,2.99951956532444E-32));
#39077=DIRECTION('center_axis',(-2.44929359828773E-16,-1.,1.22464679914767E-16));
#39078=DIRECTION('ref_axis',(0.698033961608027,-2.5866163998301E-16,-0.716064653814028));
#39079=DIRECTION('',(4.80096443081E-16,1.,0.));
#39080=DIRECTION('center_axis',(2.44929359829E-16,1.,-1.22464679915E-16));
#39081=DIRECTION('ref_axis',(1.,-2.44929359829E-16,2.99951956532444E-32));
#39082=DIRECTION('center_axis',(0.698033961608027,-2.58661639983667E-16,
-0.716064653814028));
#39083=DIRECTION('ref_axis',(-1.80554609273828E-16,-1.,1.85218457689873E-16));
#39084=DIRECTION('center_axis',(0.698033961608027,-2.5866163998301E-16,
-0.716064653814028));
#39085=DIRECTION('ref_axis',(0.716064653814028,2.30891390163356E-30,0.698033961608027));
#39086=DIRECTION('',(0.698033961608027,0.,-0.716064653814028));
#39087=DIRECTION('center_axis',(-0.716064653814028,8.99007515774035E-17,
-0.698033961608027));
#39088=DIRECTION('ref_axis',(-0.698033961608027,-3.69855194764065E-33,0.716064653814028));
#39089=DIRECTION('',(0.,1.,0.));
#39090=DIRECTION('',(0.698033961608027,-4.30707715433016E-16,-0.716064653814028));
#39091=DIRECTION('center_axis',(-1.80554609273596E-16,-1.,1.85218457689635E-16));
#39092=DIRECTION('ref_axis',(0.71606465381403,0.,0.698033961608025));
#39093=DIRECTION('center_axis',(0.716064653814028,-8.99007515774035E-17,
0.698033961608027));
#39094=DIRECTION('ref_axis',(0.698033961608027,-2.36964484828339E-31,-0.716064653814028));
#39095=DIRECTION('center_axis',(2.44929359829E-16,1.,-1.22464679915E-16));
#39096=DIRECTION('ref_axis',(1.,-2.44929359829E-16,2.99951956532444E-32));
#39097=DIRECTION('center_axis',(-2.44929359829491E-16,-1.,1.22464679914521E-16));
#39098=DIRECTION('ref_axis',(0.716064653814027,-8.99007515774033E-17,0.698033961608028));
#39099=DIRECTION('',(4.80096443081E-16,1.,-2.40048221541E-16));
#39100=DIRECTION('center_axis',(2.44929359829E-16,1.,-1.22464679915E-16));
#39101=DIRECTION('ref_axis',(1.,-2.44929359829E-16,2.99951956532444E-32));
#39102=DIRECTION('center_axis',(-0.716064653814028,8.99007515774036E-17,
-0.698033961608027));
#39103=DIRECTION('ref_axis',(0.698033961608027,-4.9741364910786E-33,-0.716064653814028));
#39104=DIRECTION('center_axis',(0.716064653814028,-8.99007515774035E-17,
0.698033961608027));
#39105=DIRECTION('ref_axis',(0.698033961608027,-7.96736102322353E-31,-0.716064653814028));
#39106=DIRECTION('',(0.716064653814028,0.,0.698033961608027));
#39107=DIRECTION('center_axis',(-0.698033961608027,2.5866163998301E-16,
0.716064653814028));
#39108=DIRECTION('ref_axis',(3.70557385756911E-16,1.,-1.7912467654698E-32));
#39109=DIRECTION('',(0.,-1.,0.));
#39110=DIRECTION('',(0.716064653814028,0.,0.698033961608027));
#39111=DIRECTION('center_axis',(-1.32057957382078E-16,-1.,1.9781552453987E-16));
#39112=DIRECTION('ref_axis',(-0.831699011544245,0.,-0.555226759258166));
#39113=DIRECTION('center_axis',(0.555226759258164,-2.37845087940071E-16,
-0.831699011544246));
#39114=DIRECTION('ref_axis',(0.831699011544246,1.10558455272238E-30,0.555226759258164));
#39115=DIRECTION('center_axis',(-2.44929359829E-16,-1.,1.22464679915E-16));
#39116=DIRECTION('ref_axis',(1.,-2.44929359829E-16,2.99951956532444E-32));
#39117=DIRECTION('center_axis',(-2.4492935982974E-16,-1.,1.22464679914506E-16));
#39118=DIRECTION('ref_axis',(-0.831699011544246,1.3571183911604E-16,-0.555226759258164));
#39119=DIRECTION('',(0.,-1.,0.));
#39120=DIRECTION('center_axis',(-2.44929359829E-16,-1.,1.22464679915E-16));
#39121=DIRECTION('ref_axis',(1.,-2.44929359829E-16,2.99951956532444E-32));
#39122=DIRECTION('center_axis',(-9.88589466193077E-17,-1.,1.96101782897063E-16));
#39123=DIRECTION('ref_axis',(-0.892950553792926,0.,-0.450154760588963));
#39124=DIRECTION('center_axis',(0.450154760588963,-2.19611021084982E-16,
-0.892950553792926));
#39125=DIRECTION('ref_axis',(0.892950553792926,5.80220876798355E-31,0.450154760588963));
#39126=DIRECTION('center_axis',(-2.44929359829E-16,-1.,1.22464679915E-16));
#39127=DIRECTION('ref_axis',(1.,-2.44929359829E-16,6.83249535077049E-33));
#39128=DIRECTION('center_axis',(-2.44929359829E-16,-1.,1.22464679915E-16));
#39129=DIRECTION('ref_axis',(-7.42634721754E-16,1.22464679915E-16,1.));
#39130=DIRECTION('',(0.,-1.,0.));
#39131=DIRECTION('center_axis',(-2.44929359829E-16,-1.,1.22464679915E-16));
#39132=DIRECTION('ref_axis',(1.,-2.44929359829E-16,6.54860237547756E-33));
#39133=DIRECTION('center_axis',(-1.74032777401559E-30,-1.,1.22464679915003E-16));
#39134=DIRECTION('ref_axis',(-1.,0.,-1.4210854715202E-14));
#39135=DIRECTION('center_axis',(3.67394039744E-16,-1.22464679915E-16,-1.));
#39136=DIRECTION('ref_axis',(1.,4.49927934799277E-32,3.67394039744E-16));
#39137=DIRECTION('center_axis',(-2.44929359829E-16,-1.,1.22464679915E-16));
#39138=DIRECTION('ref_axis',(1.,-2.44929359829E-16,2.99951956532443E-32));
#39139=DIRECTION('center_axis',(2.44929359829246E-16,1.,-1.22464679914876E-16));
#39140=DIRECTION('ref_axis',(-0.892950553792926,1.63581748831987E-16,-0.450154760588963));
#39141=DIRECTION('',(-4.80096443081E-16,-1.,2.40048221541E-16));
#39142=DIRECTION('center_axis',(-2.44929359829E-16,-1.,1.22464679915E-16));
#39143=DIRECTION('ref_axis',(1.,-2.44929359829E-16,2.99951956532443E-32));
#39144=DIRECTION('center_axis',(3.67394039744E-16,-1.22464679915E-16,-1.));
#39145=DIRECTION('ref_axis',(-1.82825659017378E-45,-1.,1.22464679915E-16));
#39146=DIRECTION('center_axis',(2.05391259556E-15,-1.22464679915E-16,-1.));
#39147=DIRECTION('ref_axis',(1.,2.51531748588642E-31,2.05391259556E-15));
#39148=DIRECTION('',(2.5624042399E-16,0.,-1.));
#39149=DIRECTION('center_axis',(-1.,2.44929359829E-16,-2.41416354181E-16));
#39150=DIRECTION('ref_axis',(-2.41416354181E-16,0.,1.));
#39151=DIRECTION('',(0.,-1.,0.));
#39152=DIRECTION('',(3.19201588392E-16,0.,-1.));
#39153=DIRECTION('center_axis',(-4.05685585531587E-19,-1.,-8.04739169685281E-19));
#39154=DIRECTION('ref_axis',(-0.892950553792926,0.,0.450154760588964));
#39155=DIRECTION('center_axis',(-0.450154760588963,9.01213585422925E-19,
-0.892950553792926));
#39156=DIRECTION('ref_axis',(0.892950553792926,2.37605947729967E-33,-0.450154760588963));
#39157=DIRECTION('center_axis',(-2.44929359829E-16,-1.,1.22464679915E-16));
#39158=DIRECTION('ref_axis',(1.,-2.44929359829E-16,2.99951956532443E-32));
#39159=DIRECTION('center_axis',(2.44929359829E-16,1.,-1.22464679915E-16));
#39160=DIRECTION('ref_axis',(-1.,2.44929359829E-16,-2.99951956532443E-32));
#39161=DIRECTION('',(0.,-1.,2.27738056333E-16));
#39162=DIRECTION('center_axis',(-2.44929359829E-16,-1.,1.22464679915E-16));
#39163=DIRECTION('ref_axis',(1.,-2.44929359829E-16,2.99951956532443E-32));
#39164=DIRECTION('center_axis',(-3.92903534935981E-16,-1.,2.14399869159323E-16));
#39165=DIRECTION('ref_axis',(-0.849410790431843,4.46882223748491E-16,0.527732232384902));
#39166=DIRECTION('center_axis',(-0.527732232384902,2.52342972731953E-17,
-0.849410790431843));
#39167=DIRECTION('ref_axis',(0.849410790431843,-6.27761689185242E-32,-0.527732232384902));
#39168=DIRECTION('center_axis',(-2.44929359829E-16,-1.,1.22464679915E-16));
#39169=DIRECTION('ref_axis',(1.,-2.44929359829E-16,6.83249535077049E-33));
#39170=DIRECTION('center_axis',(-2.44929359829E-16,-1.,1.22464679915E-16));
#39171=DIRECTION('ref_axis',(-7.42634721754E-16,1.22464679915E-16,1.));
#39172=DIRECTION('',(0.,-1.,0.));
#39173=DIRECTION('center_axis',(-2.44929359829E-16,-1.,1.22464679915E-16));
#39174=DIRECTION('ref_axis',(1.,-2.44929359829E-16,-2.34494220138087E-32));
#39175=DIRECTION('center_axis',(-1.86799616485145E-16,-1.,1.82095954083848E-16));
#39176=DIRECTION('ref_axis',(0.698033961608023,0.,0.716064653814032));
#39177=DIRECTION('center_axis',(-0.716064653814028,2.6086976293301E-16,
0.698033961608027));
#39178=DIRECTION('ref_axis',(0.698033961608027,-2.32071020223926E-30,0.716064653814028));
#39179=DIRECTION('center_axis',(-2.44929359829E-16,-1.,1.22464679915E-16));
#39180=DIRECTION('ref_axis',(1.,-2.44929359829E-16,2.99951956532444E-32));
#39181=DIRECTION('center_axis',(2.4492935982882E-16,1.,-1.22464679914888E-16));
#39182=DIRECTION('ref_axis',(-0.849410790431843,2.7267420005195E-16,0.527732232384902));
#39183=DIRECTION('',(-4.55476112667E-16,-1.,0.));
#39184=DIRECTION('center_axis',(-2.44929359829E-16,-1.,1.22464679915E-16));
#39185=DIRECTION('ref_axis',(1.,-2.44929359829E-16,2.99951956532444E-32));
#39186=DIRECTION('center_axis',(-0.716064653814028,2.60869762932787E-16,
0.698033961608027));
#39187=DIRECTION('ref_axis',(-1.86799616485013E-16,-1.,1.8209595408372E-16));
#39188=DIRECTION('center_axis',(-0.716064653814028,2.6086976293301E-16,
0.698033961608027));
#39189=DIRECTION('ref_axis',(0.698033961608027,-7.02188537105379E-31,0.716064653814028));
#39190=DIRECTION('',(-0.716064653814028,0.,0.698033961608027));
#39191=DIRECTION('center_axis',(0.698033961608027,-8.32763827281032E-17,
0.716064653814028));
#39192=DIRECTION('ref_axis',(-1.19301333901095E-16,-1.,6.93490090905032E-33));
#39193=DIRECTION('',(0.,1.,0.));
#39194=DIRECTION('',(-0.716064653814028,2.6591127623201E-16,0.698033961608027));
#39195=DIRECTION('center_axis',(-1.86799616485145E-16,-1.,1.82095954083848E-16));
#39196=DIRECTION('ref_axis',(-0.698033961608026,0.,-0.716064653814029));
#39197=DIRECTION('center_axis',(-0.698033961608027,8.32763827281032E-17,
-0.716064653814028));
#39198=DIRECTION('ref_axis',(0.716064653814028,7.37176741734741E-31,-0.698033961608027));
#39199=DIRECTION('center_axis',(2.44929359829E-16,1.,-1.22464679915E-16));
#39200=DIRECTION('ref_axis',(1.,-2.44929359829E-16,2.99951956532444E-32));
#39201=DIRECTION('center_axis',(-2.44929359829229E-16,-1.,1.22464679914765E-16));
#39202=DIRECTION('ref_axis',(-0.698033961608028,8.32763827281037E-17,-0.716064653814027));
#39203=DIRECTION('',(4.80096443081E-16,1.,-2.40048221541E-16));
#39204=DIRECTION('center_axis',(2.44929359829E-16,1.,-1.22464679915E-16));
#39205=DIRECTION('ref_axis',(1.,-2.44929359829E-16,2.99951956532444E-32));
#39206=DIRECTION('center_axis',(0.698033961608027,-8.32763827281032E-17,
0.716064653814028));
#39207=DIRECTION('ref_axis',(-0.716064653814028,-7.37176741734741E-31,0.698033961608027));
#39208=DIRECTION('center_axis',(-0.698033961608027,8.32763827281032E-17,
-0.716064653814028));
#39209=DIRECTION('ref_axis',(0.716064653814028,2.22654728542614E-31,-0.698033961608027));
#39210=DIRECTION('',(-0.698033961608027,0.,-0.716064653814028));
#39211=DIRECTION('center_axis',(0.716064653814028,-2.6086976293301E-16,
-0.698033961608027));
#39212=DIRECTION('ref_axis',(-1.38053841875249E-32,-1.,3.73720731770783E-16));
#39213=DIRECTION('',(0.,1.,0.));
#39214=DIRECTION('',(-0.698033961608027,0.,-0.716064653814028));
#39215=DIRECTION('center_axis',(-1.11265631080723E-16,-1.,-7.52285650242949E-17));
#39216=DIRECTION('ref_axis',(-0.560108292426038,0.,0.828419399070053));
#39217=DIRECTION('center_axis',(-2.44929359829E-16,-1.,1.22464679915E-16));
#39218=DIRECTION('ref_axis',(1.,-2.44929359829E-16,2.99951956532444E-32));
#39219=DIRECTION('center_axis',(0.716064653814028,-2.6086976293301E-16,
-0.698033961608027));
#39220=DIRECTION('ref_axis',(0.698033961608027,-2.32071020223926E-30,0.716064653814028));
#39221=DIRECTION('center_axis',(-2.44929359828833E-16,-1.,1.22464679914753E-16));
#39222=DIRECTION('ref_axis',(-0.560108292426038,2.38639082041016E-16,0.828419399070053));
#39223=DIRECTION('center_axis',(-2.44929359829E-16,-1.,1.22464679915E-16));
#39224=DIRECTION('ref_axis',(1.,-2.44929359829E-16,2.99951956532444E-32));
#39225=DIRECTION('',(-4.55476112667E-16,-1.,0.));
#39226=DIRECTION('center_axis',(-5.81297433438548E-17,-1.,-5.96312741688484E-17));
#39227=DIRECTION('ref_axis',(0.716064653814029,0.,-0.698033961608026));
#39228=DIRECTION('center_axis',(0.716064653814028,-2.6086976293301E-16,
-0.698033961608027));
#39229=DIRECTION('ref_axis',(0.698033961608027,-2.32071020223926E-30,0.716064653814028));
#39230=DIRECTION('center_axis',(2.44929359829E-16,1.,-1.22464679915E-16));
#39231=DIRECTION('ref_axis',(1.,-2.44929359829E-16,2.99951956532444E-32));
#39232=DIRECTION('center_axis',(-2.44929359829028E-16,-1.,1.22464679915027E-16));
#39233=DIRECTION('ref_axis',(0.716064653814026,-2.6086976293301E-16,-0.69803396160803));
#39234=DIRECTION('',(2.27738056333E-16,1.,0.));
#39235=DIRECTION('center_axis',(2.44929359829E-16,1.,-1.22464679915E-16));
#39236=DIRECTION('ref_axis',(1.,-2.44929359829E-16,2.99951956532444E-32));
#39237=DIRECTION('center_axis',(-0.716064653814028,2.6086976293301E-16,
0.698033961608027));
#39238=DIRECTION('ref_axis',(-0.698033961608027,-1.0524566385888E-31,-0.716064653814028));
#39239=DIRECTION('',(0.716064653814028,0.,-0.698033961608027));
#39240=DIRECTION('center_axis',(0.698033961608027,-8.32763827281032E-17,
0.716064653814028));
#39241=DIRECTION('ref_axis',(-1.19301333901095E-16,-1.,6.93490090905032E-33));
#39242=DIRECTION('',(0.716064653814028,-2.6393829599301E-16,-0.698033961608027));
#39243=DIRECTION('center_axis',(-1.,2.44929359829E-16,-2.41416354181E-16));
#39244=DIRECTION('ref_axis',(-2.41416354181E-16,0.,1.));
#39245=DIRECTION('',(0.,-1.,0.));
#39246=DIRECTION('',(-3.70074341542E-16,0.,1.));
#39247=DIRECTION('',(0.,-1.,0.));
#39248=DIRECTION('',(4.15092802552E-16,0.,-1.));
#39249=DIRECTION('',(0.323037326387015,0.920901128992761,-0.21814673130851));
#39250=DIRECTION('',(0.310424970358247,0.909870545905898,-0.27526701122907));
#39251=DIRECTION('center_axis',(-0.943627470111708,0.331009361877541,0.));
#39252=DIRECTION('ref_axis',(0.,0.,1.));
#39253=DIRECTION('',(0.330975706838633,0.943531527766579,0.0142596491237413));
#39254=DIRECTION('',(-1.64651774315771E-16,0.,-1.));
#39255=DIRECTION('center_axis',(-0.943627482809182,0.331009325680119,1.49146681070121E-9));
#39256=DIRECTION('ref_axis',(0.331009318664928,0.943627462811498,-0.000205875969548059));
#39257=DIRECTION('',(8.57762605026367E-7,2.44526964337894E-6,-0.999999999996642));
#39258=DIRECTION('',(0.294062932800905,0.911816425322849,-0.286562031790662));
#39259=DIRECTION('center_axis',(0.160589675912942,0.276008879795742,0.947644476723247));
#39260=DIRECTION('ref_axis',(-0.0609933906817373,0.961045570864355,-0.269575994879275));
#39261=DIRECTION('',(-0.288992183012555,0.946290745989702,0.144973591429235));
#39262=DIRECTION('',(0.117824078681733,0.966071698379208,0.229832460878599));
#39263=DIRECTION('center_axis',(-1.48089814433846E-9,1.,-1.36711158136743E-9));
#39264=DIRECTION('ref_axis',(-0.738412059057248,-2.01542449026607E-9,-0.674349783894705));
#39265=DIRECTION('',(0.128571714532246,0.968939478859869,0.211247723133303));
#39266=DIRECTION('',(-0.255328810234173,0.774608545951679,0.578609366674121));
#39267=DIRECTION('',(-0.181492548576796,0.738445189679448,0.649429870463611));
#39268=DIRECTION('',(-0.225419688153596,0.803501199046223,0.550973490581913));
#39269=DIRECTION('center_axis',(-4.57218787640431E-10,1.,8.71360109757879E-11));
#39270=DIRECTION('ref_axis',(-0.980286226483734,-4.65421893024152E-10,0.197582676786912));
#39271=DIRECTION('center_axis',(-0.698033961608027,8.32763827281032E-17,
-0.716064653814028));
#39272=DIRECTION('ref_axis',(-0.716064653814028,-6.03301243078373E-33,0.698033961608027));
#39273=DIRECTION('',(0.,-1.,0.));
#39274=DIRECTION('',(0.716064653824126,0.,-0.698033961597667));
#39275=DIRECTION('',(0.716064653814028,0.,-0.698033961608027));
#39276=DIRECTION('center_axis',(-0.698033961608027,2.5866163998301E-16,
0.716064653814028));
#39277=DIRECTION('ref_axis',(3.70557385756911E-16,1.,-1.7912467654698E-32));
#39278=DIRECTION('',(-0.716064653814028,0.,-0.698033961608027));
#39279=DIRECTION('',(0.716064653824126,0.,0.698033961597667));
#39280=DIRECTION('',(0.,-1.,0.));
#39281=DIRECTION('center_axis',(0.892620224620875,-0.100404069962798,0.439486242483976));
#39282=DIRECTION('ref_axis',(0.450785404329455,0.208856364443758,-0.867854560554282));
#39283=DIRECTION('center_axis',(0.436083773086294,0.0976415951931109,0.894593238147353));
#39284=DIRECTION('ref_axis',(0.867935375388418,0.216985732657287,-0.446772174572843));
#39285=DIRECTION('center_axis',(0.00186553655657051,-0.00532586126953934,
0.999984077360782));
#39286=DIRECTION('ref_axis',(0.943629829775382,0.331002634962083,2.49821012154569E-6));
#39287=DIRECTION('center_axis',(0.880062092697831,0.092955957006382,0.465671453981606));
#39288=DIRECTION('ref_axis',(0.441468068374835,0.201070817369295,-0.874457815453573));
#39289=DIRECTION('center_axis',(-2.14201187043523E-15,6.10635672184588E-15,
-1.));
#39290=DIRECTION('ref_axis',(0.943627470093642,0.331009361929045,0.));
#39291=DIRECTION('center_axis',(1.54815906928092E-5,2.538769952355E-6,0.999999999876938));
#39292=DIRECTION('ref_axis',(0.943627561740588,0.331009100305164,-1.54492116365672E-5));
#39293=DIRECTION('',(-8.57762605026367E-7,2.44526964337894E-6,-0.999999999996642));
#39294=DIRECTION('center_axis',(-0.983486256238949,0.0374328207462225,-0.177069386738866));
#39295=DIRECTION('ref_axis',(-0.163009880779526,0.24184812435891,0.956523530035891));
#39296=DIRECTION('center_axis',(0.160588996966396,-0.276000094097635,-0.947647150637527));
#39297=DIRECTION('ref_axis',(0.061024966583606,0.961047601642055,-0.269561608600934));
#39298=DIRECTION('center_axis',(-0.984719314308431,-0.119059960726394,-0.127092870688182));
#39299=DIRECTION('ref_axis',(-0.152586230961459,0.238117387003548,0.959175454297898));
#39300=DIRECTION('center_axis',(-0.0289008325901315,0.0823889103331479,
0.996181112714808));
#39301=DIRECTION('ref_axis',(0.9436275874899,0.331009027260539,1.50441563718168E-7));
#39302=DIRECTION('center_axis',(-0.943627482815775,-0.331009325661324,-1.49233941105659E-9));
#39303=DIRECTION('ref_axis',(0.331008843413436,-0.943626108051448,0.00170698148083177));
#39304=DIRECTION('center_axis',(-0.430110758359808,0.046153110977895,-0.901595599972744));
#39305=DIRECTION('ref_axis',(-0.879739108301929,0.202744349618919,0.430062588493499));
#39306=DIRECTION('center_axis',(-0.980966495583046,-0.0283022044444621,
-0.19210340904602));
#39307=DIRECTION('ref_axis',(-0.19328796736646,0.236890927961216,0.952114725188628));
#39308=DIRECTION('center_axis',(-0.388851273388422,-0.0301047308393102,
-0.920808553590428));
#39309=DIRECTION('ref_axis',(-0.902832709485492,0.211566053131498,0.37434329678177));
#39310=DIRECTION('center_axis',(0.154792429944213,0.0260186560475965,-0.987604340396215));
#39311=DIRECTION('ref_axis',(-0.95105813490232,0.274540052803893,-0.141831531905127));
#39312=DIRECTION('center_axis',(0.158571788614755,0.0251030524526189,-0.987028279540702));
#39313=DIRECTION('ref_axis',(-0.949647192915505,0.277483911944001,-0.145509063635074));
#39314=DIRECTION('center_axis',(0.519128585308313,0.0837939298473311,-0.85057867903947));
#39315=DIRECTION('ref_axis',(-0.763413574425517,0.492955180837497,-0.417366630276459));
#39316=DIRECTION('center_axis',(0.53027158586854,0.0827827349147078,-0.843776667146292));
#39317=DIRECTION('ref_axis',(-0.753475381714833,0.502288029862624,-0.424242364935906));
#39318=DIRECTION('center_axis',(0.648542405801268,0.0976477666270568,-0.754889171700224));
#39319=DIRECTION('ref_axis',(-0.653871091131623,0.579173686319672,-0.4868371773573));
#39320=DIRECTION('center_axis',(0.494563463497324,-0.191710317879514,0.847734707672198));
#39321=DIRECTION('ref_axis',(0.865846793003873,0.193521564619003,-0.461366161603039));
#39322=DIRECTION('center_axis',(0.464395725684733,-0.198543507192818,0.863085792790801));
#39323=DIRECTION('ref_axis',(0.883803239974284,0.166419749377341,-0.437259991341698));
#39324=DIRECTION('',(0.113178938997705,0.763679548992658,0.635597415206925));
#39325=DIRECTION('',(0.181492548576796,0.738445189679448,0.649429870463611));
#39326=DIRECTION('center_axis',(-0.396005905940162,-0.201097924900932,0.8959570006764));
#39327=DIRECTION('ref_axis',(0.891702233585015,0.148696398124815,0.427500301525276));
#39328=DIRECTION('',(-0.117824078681021,0.96607169838126,0.229832460870341));
#39329=DIRECTION('center_axis',(0.922778105750095,-0.103279309791534,0.371233015392289));
#39330=DIRECTION('ref_axis',(0.385281285161793,0.262890595038936,-0.884560267219906));
#39331=DIRECTION('center_axis',(-0.878226997877743,-0.135323395232607,0.458699159473141));
#39332=DIRECTION('ref_axis',(0.477362666720091,-0.189841514555233,0.857954010290329));
#39333=DIRECTION('center_axis',(0.456738059260596,-0.0359334235885344,0.888875207378444));
#39334=DIRECTION('ref_axis',(0.872740846734216,0.211709714743671,-0.439889089572357));
#39335=DIRECTION('center_axis',(0.920065996825176,-0.0139599992294347,0.391514597311019));
#39336=DIRECTION('ref_axis',(0.381633312533999,0.257729359286959,-0.887655108770214));
#39337=DIRECTION('center_axis',(0.892620455906449,0.100404015839207,-0.439485785095176));
#39338=DIRECTION('ref_axis',(-0.450784946851557,0.208856415901993,-0.867854785795764));
#39339=DIRECTION('center_axis',(0.880062092716156,-0.092955957010435,-0.465671453946163));
#39340=DIRECTION('ref_axis',(-0.441468068339719,0.201070817365602,-0.874457815472151));
#39341=DIRECTION('center_axis',(0.00186854672551137,0.0053252415770575,
-0.999984075040838));
#39342=DIRECTION('ref_axis',(-0.943627592819709,0.33100901206617,-5.09303340548844E-7));
#39343=DIRECTION('center_axis',(0.436083773086294,-0.0976415951931109,-0.894593238147353));
#39344=DIRECTION('ref_axis',(-0.867935375388418,0.216985732657287,-0.446772174572843));
#39345=DIRECTION('center_axis',(0.922778105089071,0.103279310020637,-0.371233016971665));
#39346=DIRECTION('ref_axis',(-0.38528128674108,0.262890594935205,-0.884560266562856));
#39347=DIRECTION('center_axis',(-0.396017498125805,0.201038848453509,-0.895965134695913));
#39348=DIRECTION('ref_axis',(0.888623240590356,-0.161920158177116,-0.429104414634237));
#39349=DIRECTION('center_axis',(0.919974181323324,0.0139905959715904,-0.391729203561387));
#39350=DIRECTION('ref_axis',(-0.381848078164205,0.257725957261476,-0.88756373075738));
#39351=DIRECTION('center_axis',(0.456738059260626,0.0359334235885297,-0.888875207378428));
#39352=DIRECTION('ref_axis',(-0.872740846734205,0.211709714743646,-0.43988908957239));
#39353=DIRECTION('center_axis',(-0.878226997877743,0.135323395232607,-0.458699159473141));
#39354=DIRECTION('ref_axis',(0.477362666720091,0.189841514555233,-0.857954010290329));
#39355=DIRECTION('',(-0.113178938997705,0.763679548992658,0.635597415206925));
#39356=DIRECTION('center_axis',(0.464395555049772,0.198543523260408,-0.8630858809072));
#39357=DIRECTION('ref_axis',(-0.883803329144551,0.16641971123809,-0.437259825623666));
#39358=DIRECTION('center_axis',(0.495307295122513,0.191627071871079,-0.847319153993663));
#39359=DIRECTION('ref_axis',(-0.865425172209434,0.193684803027571,-0.462088160833452));
#39360=DIRECTION('center_axis',(0.648543686882833,-0.0976472412892305,0.754888139046458));
#39361=DIRECTION('ref_axis',(0.65387002449902,0.579173846918327,-0.486838418890166));
#39362=DIRECTION('center_axis',(0.530204044384788,-0.0828039354466806,0.843817029688638));
#39363=DIRECTION('ref_axis',(0.753516762104764,0.502282247298617,-0.424175710379322));
#39364=DIRECTION('center_axis',(0.519038701925307,-0.0838213303629659,0.850630830901323));
#39365=DIRECTION('ref_axis',(0.763467531439435,0.492946409813472,-0.41727828303158));
#39366=DIRECTION('center_axis',(0.158462664464082,-0.0251186847944935,0.987045407083757));
#39367=DIRECTION('ref_axis',(0.949664686103619,0.277481196947328,-0.1454000320096));
#39368=DIRECTION('center_axis',(0.154792396107517,-0.0260186608384927,0.987604345573401));
#39369=DIRECTION('ref_axis',(0.951058139598754,0.274540054077438,-0.141831497947794));
#39370=DIRECTION('center_axis',(-0.388296589591557,0.0301690890474203,0.92104049019444));
#39371=DIRECTION('ref_axis',(0.903066320863432,0.211547985251654,0.373789606674866));
#39372=DIRECTION('center_axis',(-0.430257355733273,-0.0461697877906974,
0.901524796404832));
#39373=DIRECTION('ref_axis',(0.879669075246814,0.202736833246679,0.430209361241156));
#39374=DIRECTION('center_axis',(-0.980966495583046,0.0283022044444621,0.19210340904602));
#39375=DIRECTION('ref_axis',(0.19328796736646,0.236890927961216,0.952114725188628));
#39376=DIRECTION('center_axis',(-0.983486190287356,-0.0374327738616832,
0.177069762961054));
#39377=DIRECTION('ref_axis',(0.16301025642708,0.24184813865655,0.95652346240327));
#39378=DIRECTION('center_axis',(1.52856649600948E-5,-2.50540282491327E-6,
-0.999999999880036));
#39379=DIRECTION('ref_axis',(-0.943627561743776,0.331009100305162,-1.52532858923899E-5));
#39380=DIRECTION('center_axis',(-0.0289009651132723,-0.0823888877589006,
-0.996181110737085));
#39381=DIRECTION('ref_axis',(-0.943627583659813,0.331009038179116,2.82460236826103E-7));
#39382=DIRECTION('center_axis',(-0.984716782786941,0.119056590783676,0.127115639827304));
#39383=DIRECTION('ref_axis',(0.152607474441606,0.238116529713297,0.959172287455101));
#39384=DIRECTION('center_axis',(-2.14201187043523E-15,-6.10635672184588E-15,
1.));
#39385=DIRECTION('ref_axis',(-0.943627470093642,0.331009361929045,0.));
#39386=DIRECTION('center_axis',(-2.18773443555785E-16,-1.,1.58554584738017E-16));
#39387=DIRECTION('ref_axis',(0.586831315816962,0.,0.809709211245947));
#39388=DIRECTION('center_axis',(-0.809709211245947,2.70187668013982E-16,
0.586831315816962));
#39389=DIRECTION('ref_axis',(0.586831315816962,-1.3944828999061E-30,0.809709211245947));
#39390=DIRECTION('center_axis',(-2.44929359829E-16,-1.,1.22464679915E-16));
#39391=DIRECTION('ref_axis',(1.,-2.44929359829E-16,5.91180967883826E-34));
#39392=DIRECTION('center_axis',(-0.828419399070054,1.34310750335009E-16,
-0.560108292426036));
#39393=DIRECTION('ref_axis',(0.560108292426036,6.83578973261393E-31,-0.828419399070054));
#39394=DIRECTION('center_axis',(-6.43747505554034E-17,-1.,-6.27537777746355E-17));
#39395=DIRECTION('ref_axis',(0.698033961608026,0.,-0.716064653814029));
#39396=DIRECTION('center_axis',(0.716064653814028,-8.99007515774035E-17,
0.698033961608027));
#39397=DIRECTION('ref_axis',(0.698033961608027,-7.96736102322353E-31,-0.716064653814028));
#39398=DIRECTION('center_axis',(-2.44929359829E-16,-1.,1.22464679915E-16));
#39399=DIRECTION('ref_axis',(1.,-2.44929359829E-16,2.99951956532443E-32));
#39400=DIRECTION('center_axis',(0.716064653814028,-8.99007515774036E-17,
0.698033961608027));
#39401=DIRECTION('ref_axis',(0.698033961608027,-4.9741364910786E-33,-0.716064653814028));
#39402=DIRECTION('center_axis',(0.716064653814028,-8.99007515774035E-17,
0.698033961608027));
#39403=DIRECTION('ref_axis',(0.698033961608027,-7.96736102322353E-31,-0.716064653814028));
#39404=DIRECTION('',(0.716064653814028,0.,0.698033961608027));
#39405=DIRECTION('center_axis',(-6.43747505554034E-17,-1.,-6.27537777746355E-17));
#39406=DIRECTION('ref_axis',(-0.698033961608025,0.,0.71606465381403));
#39407=DIRECTION('center_axis',(-0.698033961608027,2.5866163998301E-16,
0.716064653814028));
#39408=DIRECTION('ref_axis',(0.716064653814028,2.30891390163356E-30,0.698033961608027));
#39409=DIRECTION('center_axis',(2.44929359829E-16,1.,-1.22464679915E-16));
#39410=DIRECTION('ref_axis',(1.,-2.44929359829E-16,2.99951956532444E-32));
#39411=DIRECTION('center_axis',(-0.698033961608027,2.5866163998301E-16,
0.716064653814028));
#39412=DIRECTION('ref_axis',(0.716064653814028,2.30891390163356E-30,0.698033961608027));
#39413=DIRECTION('center_axis',(-0.698033961608027,2.5866163998301E-16,
0.716064653814028));
#39414=DIRECTION('ref_axis',(0.716064653814028,2.30891390163356E-30,0.698033961608027));
#39415=DIRECTION('',(-0.698033961608027,0.,0.716064653814028));
#39416=DIRECTION('center_axis',(-1.80554609273596E-16,-1.,1.85218457689635E-16));
#39417=DIRECTION('ref_axis',(-0.71606465381403,0.,-0.698033961608025));
#39418=DIRECTION('center_axis',(-0.716064653814028,8.99007515774035E-17,
-0.698033961608027));
#39419=DIRECTION('ref_axis',(0.698033961608027,-2.36964484828339E-31,-0.716064653814028));
#39420=DIRECTION('center_axis',(2.44929359829E-16,1.,-1.22464679915E-16));
#39421=DIRECTION('ref_axis',(1.,-2.44929359829E-16,2.99951956532444E-32));
#39422=DIRECTION('center_axis',(0.716064653814028,-8.99007515767179E-17,
0.698033961608027));
#39423=DIRECTION('ref_axis',(6.43747505554034E-17,1.,6.27537777746355E-17));
#39424=DIRECTION('center_axis',(-0.716064653814028,8.99007515773035E-17,
-0.698033961608027));
#39425=DIRECTION('ref_axis',(0.698033961608027,-8.0031308366142E-31,-0.716064653814028));
#39426=DIRECTION('',(-0.716064653814028,0.,-0.698033961608027));
#39427=DIRECTION('center_axis',(-1.32057957382078E-16,-1.,1.9781552453987E-16));
#39428=DIRECTION('ref_axis',(0.831699011544245,0.,0.555226759258166));
#39429=DIRECTION('center_axis',(-0.555226759258164,2.37845087940071E-16,
0.831699011544246));
#39430=DIRECTION('ref_axis',(0.831699011544246,1.10558455272238E-30,0.555226759258164));
#39431=DIRECTION('center_axis',(-2.44929359829E-16,-1.,1.22464679915E-16));
#39432=DIRECTION('ref_axis',(1.,-2.44929359829E-16,2.99951956532443E-32));
#39433=DIRECTION('center_axis',(-9.88589466193077E-17,-1.,1.96101782897063E-16));
#39434=DIRECTION('ref_axis',(0.892950553792926,0.,0.450154760588963));
#39435=DIRECTION('center_axis',(-0.450154760588963,2.19611021084982E-16,
0.892950553792926));
#39436=DIRECTION('ref_axis',(0.892950553792926,5.80220876798355E-31,0.450154760588963));
#39437=DIRECTION('center_axis',(-2.44929359829E-16,-1.,1.22464679915E-16));
#39438=DIRECTION('ref_axis',(1.,-2.44929359829E-16,6.68589598176748E-33));
#39439=DIRECTION('center_axis',(-4.0788932203553E-30,-1.,1.22464679915008E-16));
#39440=DIRECTION('ref_axis',(1.,0.,3.37507799486048E-14));
#39441=DIRECTION('center_axis',(-4.47194436842E-16,1.22464679915E-16,1.));
#39442=DIRECTION('ref_axis',(1.,5.47655235676242E-32,4.47194436842E-16));
#39443=DIRECTION('center_axis',(-2.44929359829E-16,-1.,1.22464679915E-16));
#39444=DIRECTION('ref_axis',(1.,-2.44929359829E-16,2.99951956532444E-32));
#39445=DIRECTION('center_axis',(4.47194436842E-16,-1.22464679915E-16,-1.));
#39446=DIRECTION('ref_axis',(2.22237178326514E-45,1.,-1.22464679915E-16));
#39447=DIRECTION('center_axis',(2.62012633812E-14,1.22464679915E-16,1.));
#39448=DIRECTION('ref_axis',(1.,-2.2094004949211E-32,-2.62012633812E-14));
#39449=DIRECTION('',(-3.84360635984E-16,0.,1.));
#39450=DIRECTION('center_axis',(-4.05685585531587E-19,-1.,-8.04739169685281E-19));
#39451=DIRECTION('ref_axis',(0.892950553792926,0.,-0.450154760588964));
#39452=DIRECTION('center_axis',(0.450154760588963,-9.01213585416925E-19,
0.892950553792926));
#39453=DIRECTION('ref_axis',(0.892950553792926,2.40393060631611E-33,-0.450154760588963));
#39454=DIRECTION('center_axis',(-2.44929359829E-16,-1.,1.22464679915E-16));
#39455=DIRECTION('ref_axis',(1.,-2.44929359829E-16,2.99951956532444E-32));
#39456=DIRECTION('center_axis',(-3.92977953786766E-16,-1.,2.21299161975131E-16));
#39457=DIRECTION('ref_axis',(0.831699011544246,-4.46882223748491E-16,-0.555226759258164));
#39458=DIRECTION('center_axis',(0.555226759258164,-3.41375814712101E-17,
0.831699011544246));
#39459=DIRECTION('ref_axis',(0.831699011544246,1.57834305747204E-31,-0.555226759258164));
#39460=DIRECTION('center_axis',(-2.44929359829E-16,-1.,1.22464679915E-16));
#39461=DIRECTION('ref_axis',(1.,-2.44929359829E-16,6.68589598176748E-33));
#39462=DIRECTION('center_axis',(-1.86799616485145E-16,-1.,1.82095954083848E-16));
#39463=DIRECTION('ref_axis',(-0.698033961608026,0.,-0.716064653814029));
#39464=DIRECTION('center_axis',(0.716064653814028,-2.6086976293301E-16,
-0.698033961608027));
#39465=DIRECTION('ref_axis',(0.698033961608027,-2.32071020223926E-30,0.716064653814028));
#39466=DIRECTION('center_axis',(-2.44929359829E-16,-1.,1.22464679915E-16));
#39467=DIRECTION('ref_axis',(1.,-2.44929359829E-16,2.99951956532443E-32));
#39468=DIRECTION('center_axis',(0.716064653814028,-2.6086976293301E-16,
-0.698033961608027));
#39469=DIRECTION('ref_axis',(-0.698033961608027,1.10143058876371E-32,-0.716064653814028));
#39470=DIRECTION('center_axis',(0.716064653814515,-2.60869762932824E-16,
-0.698033961607527));
#39471=DIRECTION('ref_axis',(0.698033961607527,-1.04004355553456E-30,0.716064653814515));
#39472=DIRECTION('',(0.716064653814028,0.,-0.698033961608027));
#39473=DIRECTION('center_axis',(-1.86799616485145E-16,-1.,1.82095954083848E-16));
#39474=DIRECTION('ref_axis',(0.698033961608026,0.,0.716064653814029));
#39475=DIRECTION('center_axis',(0.698033961608027,-8.32763827281032E-17,
0.716064653814028));
#39476=DIRECTION('ref_axis',(0.716064653814028,7.37176741734741E-31,-0.698033961608027));
#39477=DIRECTION('center_axis',(2.44929359829E-16,1.,-1.22464679915E-16));
#39478=DIRECTION('ref_axis',(1.,-2.44929359829E-16,2.99951956532444E-32));
#39479=DIRECTION('center_axis',(-0.698033961608027,8.32763827277746E-17,
-0.716064653814028));
#39480=DIRECTION('ref_axis',(5.81297433438548E-17,1.,5.96312741688484E-17));
#39481=DIRECTION('center_axis',(0.698033961608027,-8.32763827281032E-17,
0.716064653814028));
#39482=DIRECTION('ref_axis',(0.716064653814028,7.37176741734741E-31,-0.698033961608027));
#39483=DIRECTION('',(0.698033961608027,0.,0.716064653814028));
#39484=DIRECTION('center_axis',(-5.81297433438548E-17,-1.,-5.96312741688484E-17));
#39485=DIRECTION('ref_axis',(-0.71606465381403,0.,0.698033961608025));
#39486=DIRECTION('center_axis',(-0.716064653814028,2.6086976293301E-16,
0.698033961608027));
#39487=DIRECTION('ref_axis',(0.698033961608027,-2.32071020223926E-30,0.716064653814028));
#39488=DIRECTION('center_axis',(2.44929359829E-16,1.,-1.22464679915E-16));
#39489=DIRECTION('ref_axis',(1.,-2.44929359829E-16,2.99951956532444E-32));
#39490=DIRECTION('center_axis',(0.716064653814028,-2.60869762932971E-16,
-0.698033961608027));
#39491=DIRECTION('ref_axis',(1.86799616485145E-16,1.,-1.82095954083849E-16));
#39492=DIRECTION('center_axis',(-0.716064653814515,2.60869762932824E-16,
0.698033961607527));
#39493=DIRECTION('ref_axis',(0.698033961607527,-2.6232605074812E-30,0.716064653814515));
#39494=DIRECTION('',(-0.716064653814028,0.,0.698033961608027));
#39495=DIRECTION('center_axis',(-1.02392142274414E-16,-1.,-7.42080178237726E-17));
#39496=DIRECTION('ref_axis',(0.586831315816962,0.,-0.809709211245946));
#39497=DIRECTION('center_axis',(0.809709211245947,-1.26455449502992E-16,
0.586831315816962));
#39498=DIRECTION('ref_axis',(0.586831315816962,-6.48713419669698E-31,-0.809709211245947));
#39499=DIRECTION('center_axis',(-2.44929359829E-16,-1.,1.22464679915E-16));
#39500=DIRECTION('ref_axis',(1.,-2.44929359829E-16,2.99951956532443E-32));
#39501=DIRECTION('center_axis',(-2.18773443555785E-16,-1.,1.58554584738017E-16));
#39502=DIRECTION('ref_axis',(-0.586831315816962,0.,-0.809709211245947));
#39503=DIRECTION('center_axis',(0.809709211245947,-2.70187668013982E-16,
-0.586831315816962));
#39504=DIRECTION('ref_axis',(0.586831315816962,-1.3944828999061E-30,0.809709211245947));
#39505=DIRECTION('center_axis',(-2.44929359829E-16,-1.,1.22464679915E-16));
#39506=DIRECTION('ref_axis',(1.,-2.44929359829E-16,6.68589598176748E-33));
#39507=DIRECTION('center_axis',(-6.43747505554034E-17,-1.,-6.27537777746355E-17));
#39508=DIRECTION('ref_axis',(-0.698033961608026,0.,0.716064653814029));
#39509=DIRECTION('center_axis',(-0.716064653814028,8.99007515774035E-17,
-0.698033961608027));
#39510=DIRECTION('ref_axis',(0.698033961608027,-7.96736102322353E-31,-0.716064653814028));
#39511=DIRECTION('center_axis',(-2.44929359829E-16,-1.,1.22464679915E-16));
#39512=DIRECTION('ref_axis',(1.,-2.44929359829E-16,2.99951956532443E-32));
#39513=DIRECTION('center_axis',(-0.716064653814028,8.99007515774035E-17,
-0.698033961608027));
#39514=DIRECTION('ref_axis',(-0.698033961608027,2.4644238743985E-33,0.716064653814028));
#39515=DIRECTION('center_axis',(-0.716064653814028,8.99007515774035E-17,
-0.698033961608027));
#39516=DIRECTION('ref_axis',(0.698033961608027,-7.96736102322353E-31,-0.716064653814028));
#39517=DIRECTION('',(-0.716064653814028,0.,-0.698033961608027));
#39518=DIRECTION('center_axis',(-6.43747505554034E-17,-1.,-6.27537777746355E-17));
#39519=DIRECTION('ref_axis',(0.698033961608025,0.,-0.71606465381403));
#39520=DIRECTION('center_axis',(0.698033961608027,-2.5866163998301E-16,
-0.716064653814028));
#39521=DIRECTION('ref_axis',(0.716064653814028,2.30891390163356E-30,0.698033961608027));
#39522=DIRECTION('center_axis',(2.44929359829E-16,1.,-1.22464679915E-16));
#39523=DIRECTION('ref_axis',(1.,-2.44929359829E-16,2.99951956532444E-32));
#39524=DIRECTION('center_axis',(0.698033961608027,-2.5866163998301E-16,
-0.716064653814028));
#39525=DIRECTION('ref_axis',(-0.716064653814028,-2.30891390163356E-30,-0.698033961608027));
#39526=DIRECTION('center_axis',(0.698033961608027,-2.5866163998301E-16,
-0.716064653814028));
#39527=DIRECTION('ref_axis',(0.716064653814028,2.30891390163356E-30,0.698033961608027));
#39528=DIRECTION('',(0.698033961608027,0.,-0.716064653814028));
#39529=DIRECTION('center_axis',(-1.80554609273596E-16,-1.,1.85218457689635E-16));
#39530=DIRECTION('ref_axis',(0.71606465381403,0.,0.698033961608025));
#39531=DIRECTION('center_axis',(0.716064653814028,-8.99007515774035E-17,
0.698033961608027));
#39532=DIRECTION('ref_axis',(0.698033961608027,-2.36964484828339E-31,-0.716064653814028));
#39533=DIRECTION('center_axis',(2.44929359829E-16,1.,-1.22464679915E-16));
#39534=DIRECTION('ref_axis',(1.,-2.44929359829E-16,2.99951956532444E-32));
#39535=DIRECTION('center_axis',(-0.716064653814028,8.99007515767179E-17,
-0.698033961608027));
#39536=DIRECTION('ref_axis',(6.43747505554034E-17,1.,6.27537777746355E-17));
#39537=DIRECTION('center_axis',(0.716064653814028,-8.99007515774035E-17,
0.698033961608027));
#39538=DIRECTION('ref_axis',(0.698033961608027,-7.96736102322353E-31,-0.716064653814028));
#39539=DIRECTION('',(0.716064653814028,0.,0.698033961608027));
#39540=DIRECTION('center_axis',(-1.32057957382078E-16,-1.,1.9781552453987E-16));
#39541=DIRECTION('ref_axis',(-0.831699011544245,0.,-0.555226759258166));
#39542=DIRECTION('center_axis',(0.555226759258164,-2.37845087940071E-16,
-0.831699011544246));
#39543=DIRECTION('ref_axis',(0.831699011544246,1.10558455272238E-30,0.555226759258164));
#39544=DIRECTION('center_axis',(-2.44929359829E-16,-1.,1.22464679915E-16));
#39545=DIRECTION('ref_axis',(1.,-2.44929359829E-16,2.99951956532443E-32));
#39546=DIRECTION('center_axis',(-9.88589466193077E-17,-1.,1.96101782897063E-16));
#39547=DIRECTION('ref_axis',(-0.892950553792926,0.,-0.450154760588963));
#39548=DIRECTION('center_axis',(0.450154760588963,-2.19611021084982E-16,
-0.892950553792926));
#39549=DIRECTION('ref_axis',(0.892950553792926,5.80220876798355E-31,0.450154760588963));
#39550=DIRECTION('center_axis',(-2.44929359829E-16,-1.,1.22464679915E-16));
#39551=DIRECTION('ref_axis',(1.,-2.44929359829E-16,5.91180967883826E-34));
#39552=DIRECTION('center_axis',(-1.35963107345579E-30,-1.,1.22464679915003E-16));
#39553=DIRECTION('ref_axis',(-1.,0.,-1.06581410364015E-14));
#39554=DIRECTION('center_axis',(2.87593642646E-16,-1.22464679915E-16,-1.));
#39555=DIRECTION('ref_axis',(1.,3.52200633922313E-32,2.87593642646E-16));
#39556=DIRECTION('center_axis',(-2.44929359829E-16,-1.,1.22464679915E-16));
#39557=DIRECTION('ref_axis',(1.,-2.44929359829E-16,2.99951956532444E-32));
#39558=DIRECTION('center_axis',(2.87593642646E-16,-1.22464679915E-16,-1.));
#39559=DIRECTION('ref_axis',(-1.,-1.10148049272531E-46,-2.87593642646E-16));
#39560=DIRECTION('center_axis',(-1.74860126378E-14,-1.22464679915E-16,-1.));
#39561=DIRECTION('ref_axis',(1.,-1.6995388412451E-32,-1.74860126378E-14));
#39562=DIRECTION('',(3.84360635984E-16,0.,-1.));
#39563=DIRECTION('center_axis',(-4.05685585531587E-19,-1.,-8.04739169685281E-19));
#39564=DIRECTION('ref_axis',(-0.892950553792926,0.,0.450154760588964));
#39565=DIRECTION('center_axis',(-0.450154760588963,9.01213585422925E-19,
-0.892950553792926));
#39566=DIRECTION('ref_axis',(0.892950553792926,2.37605947729967E-33,-0.450154760588963));
#39567=DIRECTION('center_axis',(-2.44929359829E-16,-1.,1.22464679915E-16));
#39568=DIRECTION('ref_axis',(1.,-2.44929359829E-16,2.99951956532444E-32));
#39569=DIRECTION('center_axis',(-3.95305981663445E-16,-1.,2.15892490384474E-16));
#39570=DIRECTION('ref_axis',(-0.849410790431843,4.46882223748491E-16,0.527732232384902));
#39571=DIRECTION('center_axis',(-0.527732232384902,2.52342972731953E-17,
-0.849410790431843));
#39572=DIRECTION('ref_axis',(0.849410790431843,-6.27761689185242E-32,-0.527732232384902));
#39573=DIRECTION('center_axis',(-2.44929359829E-16,-1.,1.22464679915E-16));
#39574=DIRECTION('ref_axis',(1.,-2.44929359829E-16,5.91180967883826E-34));
#39575=DIRECTION('center_axis',(-1.86799616485314E-16,-1.,1.82095954083758E-16));
#39576=DIRECTION('ref_axis',(0.698033961607525,0.,0.716064653814517));
#39577=DIRECTION('center_axis',(-0.716064653814028,2.6086976293301E-16,
0.698033961608027));
#39578=DIRECTION('ref_axis',(0.698033961608027,-2.32071020223926E-30,0.716064653814028));
#39579=DIRECTION('center_axis',(-2.44929359829E-16,-1.,1.22464679915E-16));
#39580=DIRECTION('ref_axis',(1.,-2.44929359829E-16,2.99951956532443E-32));
#39581=DIRECTION('center_axis',(-0.716064653814028,2.6086976293301E-16,
0.698033961608027));
#39582=DIRECTION('ref_axis',(0.698033961608027,1.0524566385888E-31,0.716064653814028));
#39583=DIRECTION('center_axis',(-0.716064653814028,2.6086976293301E-16,
0.698033961608027));
#39584=DIRECTION('ref_axis',(0.698033961608027,-7.02188537105379E-31,0.716064653814028));
#39585=DIRECTION('',(-0.716064653814028,0.,0.698033961608027));
#39586=DIRECTION('center_axis',(-1.86799616485145E-16,-1.,1.82095954083848E-16));
#39587=DIRECTION('ref_axis',(-0.698033961608026,0.,-0.716064653814029));
#39588=DIRECTION('center_axis',(-0.698033961608027,8.32763827281032E-17,
-0.716064653814028));
#39589=DIRECTION('ref_axis',(0.716064653814028,7.37176741734741E-31,-0.698033961608027));
#39590=DIRECTION('center_axis',(2.44929359829E-16,1.,-1.22464679915E-16));
#39591=DIRECTION('ref_axis',(1.,-2.44929359829E-16,2.99951956532444E-32));
#39592=DIRECTION('center_axis',(0.698033961608027,-8.32763827277746E-17,
0.716064653814028));
#39593=DIRECTION('ref_axis',(5.81297433438548E-17,1.,5.96312741688484E-17));
#39594=DIRECTION('center_axis',(-0.698033961607527,8.32763827280436E-17,
-0.716064653814515));
#39595=DIRECTION('ref_axis',(0.716064653814515,3.35409891176131E-31,-0.698033961607527));
#39596=DIRECTION('',(-0.698033961608027,0.,-0.716064653814028));
#39597=DIRECTION('center_axis',(-1.11265631080723E-16,-1.,-7.52285650242949E-17));
#39598=DIRECTION('ref_axis',(-0.560108292426038,0.,0.828419399070053));
#39599=DIRECTION('center_axis',(-2.44929359829E-16,-1.,1.22464679915E-16));
#39600=DIRECTION('ref_axis',(1.,-2.44929359829E-16,2.99951956532443E-32));
#39601=DIRECTION('center_axis',(0.716064653814028,-2.6086976293301E-16,
-0.698033961608027));
#39602=DIRECTION('ref_axis',(0.698033961608027,-2.32071020223926E-30,0.716064653814028));
#39603=DIRECTION('center_axis',(-5.81297433438548E-17,-1.,-5.96312741688484E-17));
#39604=DIRECTION('ref_axis',(0.716064653814029,0.,-0.698033961608026));
#39605=DIRECTION('center_axis',(0.716064653814028,-2.6086976293301E-16,
-0.698033961608027));
#39606=DIRECTION('ref_axis',(0.698033961608027,-2.32071020223926E-30,0.716064653814028));
#39607=DIRECTION('center_axis',(2.44929359829E-16,1.,-1.22464679915E-16));
#39608=DIRECTION('ref_axis',(1.,-2.44929359829E-16,2.99951956532443E-32));
#39609=DIRECTION('center_axis',(-0.716064653814028,2.60869762932971E-16,
0.698033961608027));
#39610=DIRECTION('ref_axis',(1.86799616485145E-16,1.,-1.82095954083849E-16));
#39611=DIRECTION('',(0.716064653814028,0.,-0.698033961608027));
#39612=DIRECTION('center_axis',(-2.44929359829E-16,-1.,1.22464679915E-16));
#39613=DIRECTION('ref_axis',(-1.,2.44929359829E-16,0.));
#39614=DIRECTION('',(0.716064653814028,0.,0.698033961608027));
#39615=DIRECTION('center_axis',(-2.44929359829E-16,-1.,1.22464679915E-16));
#39616=DIRECTION('ref_axis',(1.,-2.44929359829E-16,2.99951956532444E-32));
#39617=DIRECTION('',(-0.698033961608027,0.,0.716064653814028));
#39618=DIRECTION('center_axis',(-2.44929359829E-16,-1.,1.22464679915E-16));
#39619=DIRECTION('ref_axis',(1.,-2.44929359829E-16,2.99951956532444E-32));
#39620=DIRECTION('',(0.716064653814028,0.,0.698033961608027));
#39621=DIRECTION('center_axis',(2.44929359829E-16,1.,-1.22464679915E-16));
#39622=DIRECTION('ref_axis',(1.,-2.44929359829E-16,9.78625965784287E-34));
#39623=DIRECTION('',(-0.716064653814028,0.,0.698033961608027));
#39624=DIRECTION('center_axis',(-2.44929359829E-16,-1.,1.22464679915E-16));
#39625=DIRECTION('ref_axis',(1.,-2.44929359829E-16,2.99951956532444E-32));
#39626=DIRECTION('',(0.698033961608027,0.,0.716064653814028));
#39627=DIRECTION('center_axis',(-2.32604145439E-16,-1.,1.36266007238E-16));
#39628=DIRECTION('ref_axis',(1.,-2.32604145439E-16,3.16960381659796E-32));
#39629=DIRECTION('center_axis',(-2.44929359829E-16,-1.,1.22464679915E-16));
#39630=DIRECTION('ref_axis',(1.,-2.44929359829E-16,2.99951956532444E-32));
#39631=DIRECTION('',(0.698033961608027,0.,-0.716064653814028));
#39632=DIRECTION('center_axis',(-2.44929359829E-16,-1.,1.22464679915E-16));
#39633=DIRECTION('ref_axis',(1.,-2.44929359829E-16,2.99951956532444E-32));
#39634=DIRECTION('',(-0.716064653814028,0.,-0.698033961608027));
#39635=DIRECTION('center_axis',(-2.44929359829E-16,-1.,1.22464679915E-16));
#39636=DIRECTION('ref_axis',(1.,-2.44929359829E-16,9.78625965784287E-34));
#39637=DIRECTION('',(0.716064653814028,0.,-0.698033961608027));
#39638=DIRECTION('center_axis',(-2.44929359829E-16,-1.,1.22464679915E-16));
#39639=DIRECTION('ref_axis',(1.,-2.44929359829E-16,2.99951956532444E-32));
#39640=DIRECTION('',(-0.698033961608027,0.,-0.716064653814028));
#39641=DIRECTION('center_axis',(-2.44929359829E-16,-1.,1.22464679915E-16));
#39642=DIRECTION('ref_axis',(1.,-2.44929359829E-16,2.99951956532444E-32));
#39643=DIRECTION('center_axis',(2.44929359828964E-16,1.,-1.22464679914979E-16));
#39644=DIRECTION('ref_axis',(-0.860090783657011,2.73135739791003E-16,0.510141003908006));
#39645=DIRECTION('',(-3.70074341542E-16,-1.,0.));
#39646=DIRECTION('',(-3.70074341542E-16,-1.,0.));
#39647=DIRECTION('center_axis',(0.,-1.,0.));
#39648=DIRECTION('ref_axis',(0.503074672515737,0.,-0.864242948408133));
#39649=DIRECTION('center_axis',(0.698033961608027,-2.5866163998301E-16,
-0.716064653814028));
#39650=DIRECTION('ref_axis',(-5.0987642944624E-33,-1.,3.6122665544973E-16));
#39651=DIRECTION('',(0.716064653824126,0.,0.698033961597667));
#39652=DIRECTION('',(0.,-1.,0.));
#39653=DIRECTION('center_axis',(-0.698033961608027,8.32763827281032E-17,
-0.716064653814028));
#39654=DIRECTION('ref_axis',(-0.716064653814028,-6.03301243078373E-33,0.698033961608027));
#39655=DIRECTION('',(0.716064653821144,0.,-0.698033961600728));
#39656=DIRECTION('',(0.,-1.,0.));
#39657=DIRECTION('center_axis',(-2.44929359829028E-16,-1.,1.22464679915027E-16));
#39658=DIRECTION('ref_axis',(-0.716064653814028,2.6086976293301E-16,0.698033961608027));
#39659=DIRECTION('center_axis',(0.,1.,0.));
#39660=DIRECTION('ref_axis',(-0.716064653820949,0.,0.698033961600927));
#39661=DIRECTION('',(-3.70074341542E-16,-1.,0.));
#39662=DIRECTION('center_axis',(-0.716064653814028,2.6086976293301E-16,
0.698033961608027));
#39663=DIRECTION('ref_axis',(3.64310347597135E-16,1.,-2.26745038145461E-32));
#39664=DIRECTION('',(-0.698033961612045,0.,-0.716064653810111));
#39665=DIRECTION('',(0.,-1.,0.));
#39666=DIRECTION('center_axis',(-2.44929359829229E-16,-1.,1.22464679914765E-16));
#39667=DIRECTION('ref_axis',(0.698033961608027,-8.32763827281033E-17,0.716064653814028));
#39668=DIRECTION('center_axis',(0.,1.,0.));
#39669=DIRECTION('ref_axis',(0.698033961600926,0.,0.71606465382095));
#39670=DIRECTION('center_axis',(0.716064653814028,-8.99007515774035E-17,
0.698033961608027));
#39671=DIRECTION('ref_axis',(-2.12219958443594E-33,-1.,-1.28791371941708E-16));
#39672=DIRECTION('',(0.,-1.,0.));
#39673=DIRECTION('',(-0.698033961612045,0.,0.716064653810111));
#39674=DIRECTION('',(0.,-1.,0.));
#39675=DIRECTION('center_axis',(-2.44929359829491E-16,-1.,1.22464679914521E-16));
#39676=DIRECTION('ref_axis',(-0.716064653814028,8.99007515774037E-17,-0.698033961608027));
#39677=DIRECTION('center_axis',(0.,1.,0.));
#39678=DIRECTION('ref_axis',(-0.716064653804541,0.,-0.698033961617759));
#39679=DIRECTION('center_axis',(-2.44929359828773E-16,-1.,1.22464679914767E-16));
#39680=DIRECTION('ref_axis',(-0.698033961608027,2.5866163998301E-16,0.716064653814028));
#39681=DIRECTION('center_axis',(0.,1.,0.));
#39682=DIRECTION('ref_axis',(-0.698033961584438,0.,0.716064653837023));
#39683=DIRECTION('',(-3.70074341542E-16,-1.,0.));
#39684=DIRECTION('center_axis',(0.698033961608027,-2.5866163998301E-16,
-0.716064653814028));
#39685=DIRECTION('ref_axis',(-5.0987642944624E-33,-1.,3.6122665544973E-16));
#39686=DIRECTION('',(0.716064653821144,0.,0.698033961600728));
#39687=DIRECTION('',(-3.70074341542E-16,-1.,0.));
#39688=DIRECTION('center_axis',(2.44929359828964E-16,1.,-1.22464679914979E-16));
#39689=DIRECTION('ref_axis',(-0.860090783657011,2.73135739791003E-16,0.510141003908006));
#39690=DIRECTION('center_axis',(0.,-1.,0.));
#39691=DIRECTION('ref_axis',(-4.52175312758849E-15,0.,1.));
#39692=DIRECTION('',(-3.70074341542E-16,-1.,0.));
#39693=DIRECTION('center_axis',(-0.698033961608027,2.5866163998301E-16,
0.716064653814028));
#39694=DIRECTION('ref_axis',(3.70557385756911E-16,1.,-1.7912467654698E-32));
#39695=DIRECTION('',(0.,-1.,0.));
#39696=DIRECTION('',(-0.716064653821144,0.,-0.698033961600728));
#39697=DIRECTION('center_axis',(-2.44929359828773E-16,-1.,1.22464679914767E-16));
#39698=DIRECTION('ref_axis',(0.698033961608027,-2.5866163998301E-16,-0.716064653814028));
#39699=DIRECTION('center_axis',(0.,1.,0.));
#39700=DIRECTION('ref_axis',(0.698033961584438,0.,-0.716064653837023));
#39701=DIRECTION('',(-3.70074341542E-16,-1.,0.));
#39702=DIRECTION('center_axis',(-0.716064653814028,8.99007515774035E-17,
-0.698033961608027));
#39703=DIRECTION('ref_axis',(-0.698033961608027,-3.69855194764065E-33,0.716064653814028));
#39704=DIRECTION('',(0.,-1.,0.));
#39705=DIRECTION('',(0.698033961612045,0.,-0.716064653810111));
#39706=DIRECTION('center_axis',(-2.32604145438773E-16,-1.,1.36266007238254E-16));
#39707=DIRECTION('ref_axis',(-0.666093971259166,5.32997876968134E-17,-0.745867831088185));
#39708=DIRECTION('center_axis',(0.,1.,0.));
#39709=DIRECTION('ref_axis',(-0.666093971264093,0.,-0.745867831083785));
#39710=DIRECTION('',(0.,-1.,0.));
#39711=DIRECTION('center_axis',(0.716064653814028,-2.6086976293301E-16,
-0.698033961608027));
#39712=DIRECTION('ref_axis',(-1.38053841875249E-32,-1.,3.73720731770783E-16));
#39713=DIRECTION('',(0.,-1.,0.));
#39714=DIRECTION('',(0.698033961610687,0.,0.716064653811435));
#39715=DIRECTION('center_axis',(-2.44929359829028E-16,-1.,1.22464679915027E-16));
#39716=DIRECTION('ref_axis',(0.716064653814028,-2.6086976293301E-16,-0.698033961608027));
#39717=DIRECTION('center_axis',(0.,1.,0.));
#39718=DIRECTION('ref_axis',(0.7160646538177,0.,-0.69803396160426));
#39719=DIRECTION('',(0.,-1.,0.));
#39720=DIRECTION('center_axis',(0.698033961608027,-8.32763827281032E-17,
0.716064653814028));
#39721=DIRECTION('ref_axis',(-1.19301333901095E-16,-1.,6.93490090905032E-33));
#39722=DIRECTION('',(-0.716064653924687,0.,0.698033961494509));
#39723=DIRECTION('',(-0.326298438494934,0.943819486756767,0.0522886742417565));
#39724=DIRECTION('',(-0.128571714532246,0.968939478859869,0.211247723133303));
#39725=DIRECTION('',(-0.330975706838633,0.943531527766579,0.0142596491237413));
#39726=DIRECTION('center_axis',(-0.943627470111708,-0.331009361877541,0.));
#39727=DIRECTION('ref_axis',(0.,0.,1.));
#39728=DIRECTION('',(-0.323037326396155,0.920901128988691,-0.218146731312158));
#39729=DIRECTION('',(1.64651774315771E-16,0.,-1.));
#39730=DIRECTION('',(-0.294062932800905,0.911816425322849,-0.286562031790662));
#39731=DIRECTION('',(-0.310424970358247,0.909870545905898,-0.27526701122907));
#39732=DIRECTION('',(0.288992183012555,0.946290745989702,0.144973591429235));
#39733=DIRECTION('',(0.288070798801296,0.943889906160958,0.161514890723551));
#39734=DIRECTION('',(0.185892369076962,0.87281982032212,0.451253352754101));
#39735=DIRECTION('',(0.225419688153596,0.803501199046223,0.550973490581913));
#39736=DIRECTION('',(0.25532881023728,0.774608545942306,0.578609366685298));
#39737=DIRECTION('center_axis',(-4.57218787640431E-10,-1.,-8.71360109757879E-11));
#39738=DIRECTION('ref_axis',(0.980286226483734,-4.65421893024152E-10,0.197582676786912));
#39739=DIRECTION('center_axis',(-2.44929359829491E-16,-1.,1.22464679914521E-16));
#39740=DIRECTION('ref_axis',(0.716064653814028,-8.99007515774037E-17,0.698033961608027));
#39741=DIRECTION('center_axis',(0.,1.,0.));
#39742=DIRECTION('ref_axis',(0.716064653804541,0.,0.698033961617759));
#39743=DIRECTION('center_axis',(-1.48089814433846E-9,-1.,1.36711158136743E-9));
#39744=DIRECTION('ref_axis',(0.738412059057248,-2.01542449026607E-9,-0.674349783894705));
#39745=DIRECTION('',(0.326298438494934,0.943819486756767,0.0522886742417565));
#39746=DIRECTION('center_axis',(0.33738697816179,0.0208183480491995,0.941135815571461));
#39747=DIRECTION('ref_axis',(0.637783973074513,0.730279477783167,-0.244792745027368));
#39748=DIRECTION('center_axis',(0.126791036026689,-0.0184132777306928,0.991758531289997));
#39749=DIRECTION('ref_axis',(0.674495541553173,0.734701613202815,-0.0725899716357153));
#39750=DIRECTION('center_axis',(-0.703555295639302,0.00327031186878069,
0.710632993209699));
#39751=DIRECTION('ref_axis',(0.595284509769511,0.548878148649461,0.586829728595623));
#39752=DIRECTION('center_axis',(0.71100199103497,0.0109882068305169,0.703104137418461));
#39753=DIRECTION('ref_axis',(0.587718788382872,-0.558268880784424,-0.585595835478255));
#39754=DIRECTION('center_axis',(-2.44929359829021E-16,-1.,1.22464679914804E-16));
#39755=DIRECTION('ref_axis',(0.106227141118038,9.57536156315344E-17,0.994341890141358));
#39756=DIRECTION('',(2.22044604925E-16,1.,0.));
#39757=DIRECTION('center_axis',(2.44929359828927E-16,1.,-1.22464679914314E-16));
#39758=DIRECTION('ref_axis',(-0.106227141118038,1.47789906972053E-16,0.994341890141358));
#39759=DIRECTION('center_axis',(0.71100199103497,-0.0109882068305169,-0.703104137418461));
#39760=DIRECTION('ref_axis',(0.587718788382872,0.558268880784424,0.585595835478255));
#39761=DIRECTION('',(-4.22942104619E-16,-1.,0.));
#39762=DIRECTION('center_axis',(-2.44929359829277E-16,-1.,1.22464679915277E-16));
#39763=DIRECTION('ref_axis',(-0.70655827709904,2.59719592428015E-16,0.707654860128041));
#39764=DIRECTION('center_axis',(1.75424076978333E-8,1.,-1.21125590716001E-8));
#39765=DIRECTION('ref_axis',(-0.706558277096875,2.09662509575991E-8,0.707654860130201));
#39766=DIRECTION('',(0.,-1.,0.));
#39767=DIRECTION('center_axis',(-0.99784376475148,2.52439080557121E-16,
0.0656339938339316));
#39768=DIRECTION('ref_axis',(2.52984574814669E-16,1.,-1.76602436617594E-34));
#39769=DIRECTION('center_axis',(0.997843762826238,-1.07495452104656E-7,
-0.0656340231035873));
#39770=DIRECTION('ref_axis',(0.0543784369549279,-0.559973082837639,0.826724338635104));
#39771=DIRECTION('',(4.22942104619E-16,1.,-1.05735526155E-16));
#39772=DIRECTION('center_axis',(2.44929359829765E-16,1.,-1.2246467991505E-16));
#39773=DIRECTION('ref_axis',(0.99784376475148,-2.52439080557122E-16,-0.0656339938339316));
#39774=DIRECTION('center_axis',(0.992604832159675,-0.0967004534711314,-0.0733803071112495));
#39775=DIRECTION('ref_axis',(0.0892087136015431,0.991051361070216,-0.0992925230741472));
#39776=DIRECTION('',(2.96059473233E-16,1.,0.));
#39777=DIRECTION('center_axis',(-2.4492935982986E-16,-1.,1.22464679914313E-16));
#39778=DIRECTION('ref_axis',(-0.781375177526389,1.14956222701057E-16,-0.624061561022311));
#39779=DIRECTION('center_axis',(-0.762365462560859,-0.0521613879530353,
0.645041154579443));
#39780=DIRECTION('ref_axis',(0.181698336597197,-0.973905518778203,0.135991745967063));
#39781=DIRECTION('center_axis',(-0.762365462560859,0.0521613879530353,-0.645041154579443));
#39782=DIRECTION('ref_axis',(0.181698336597197,0.973905518778203,-0.135991745967063));
#39783=DIRECTION('',(4.22942104619E-16,1.,-1.05735526155E-16));
#39784=DIRECTION('center_axis',(-2.44929359829589E-16,-1.,1.22464679914961E-16));
#39785=DIRECTION('ref_axis',(-0.99784376475148,2.36363388464114E-16,-0.0656339938339316));
#39786=DIRECTION('center_axis',(0.992604832159675,0.0967004534711314,0.0733803071112495));
#39787=DIRECTION('ref_axis',(0.0892087136015431,-0.991051361070216,0.0992925230741472));
#39788=DIRECTION('',(0.,1.,-1.71536605105E-16));
#39789=DIRECTION('center_axis',(-0.99784376475148,2.36363388464114E-16,
-0.0656339938339316));
#39790=DIRECTION('ref_axis',(-0.0656339938339316,2.57699594238361E-34,0.99784376475148));
#39791=DIRECTION('center_axis',(0.997843762826238,1.07495452104656E-7,0.0656340231035873));
#39792=DIRECTION('ref_axis',(0.0543784369549279,0.559973082837639,-0.826724338635104));
#39793=DIRECTION('center_axis',(-0.065618044097648,-0.0267441093839493,
0.997486353241015));
#39794=DIRECTION('ref_axis',(0.827047674636938,0.557835994841529,0.0693624302976431));
#39795=DIRECTION('center_axis',(-0.0655782124791017,-0.0412186949466952,
0.996995745845958));
#39796=DIRECTION('ref_axis',(0.269397312004974,-0.962775872182078,-0.0220841171101169));
#39797=DIRECTION('center_axis',(-0.0856235883015126,0.0624824447695074,
0.994366403908538));
#39798=DIRECTION('ref_axis',(0.0924863865976304,-0.993223888733409,0.0703745347650614));
#39799=DIRECTION('center_axis',(0.979394141707147,0.188333569461664,0.0729217512375316));
#39800=DIRECTION('ref_axis',(-0.0989622241844842,0.132786699227001,0.986191751482874));
#39801=DIRECTION('center_axis',(-0.643311851218355,0.0453228721401247,0.764261538573663));
#39802=DIRECTION('ref_axis',(0.734064765060376,0.320083161313605,0.59891208915862));
#39803=DIRECTION('center_axis',(-0.645613117725507,0.00688651525632543,
0.763633602016291));
#39804=DIRECTION('ref_axis',(0.724253375877135,0.322609208678801,0.609409834188956));
#39805=DIRECTION('center_axis',(-1.,-3.05924483389283E-12,-3.74625528149392E-12));
#39806=DIRECTION('ref_axis',(-4.80001061146564E-12,0.722902978576062,0.690949552113508));
#39807=DIRECTION('center_axis',(-0.64561315170571,-0.00688562442483218,
-0.763633581320845));
#39808=DIRECTION('ref_axis',(-0.724253155294373,0.322609253942205,0.609410072379017));
#39809=DIRECTION('center_axis',(-0.643311852237848,-0.0453228719224639,
-0.76426153772842));
#39810=DIRECTION('ref_axis',(-0.734064763730816,0.320083163451923,0.598912089645409));
#39811=DIRECTION('center_axis',(-0.0855523090148687,-0.062489382877931,
-0.994372103113196));
#39812=DIRECTION('ref_axis',(0.0924776252402706,0.993224761345867,-0.0703737328792845));
#39813=DIRECTION('center_axis',(-0.065578227090674,0.0412186963935417,-0.996995744825052));
#39814=DIRECTION('ref_axis',(0.269393661471009,0.962776887229459,0.0220843966636586));
#39815=DIRECTION('center_axis',(0.979394141707147,-0.188333569461664,-0.0729217512375316));
#39816=DIRECTION('ref_axis',(-0.0989622241844842,-0.132786699227001,-0.986191751482874));
#39817=DIRECTION('center_axis',(-0.0656099521672813,0.0267416358010699,
-0.997486951840118));
#39818=DIRECTION('ref_axis',(-0.827048250379497,0.557836147395209,0.0693543380293116));
#39819=DIRECTION('center_axis',(-0.0594793722313762,0.422789020794831,-0.904274100134638));
#39820=DIRECTION('ref_axis',(0.998229534866085,0.025191826794196,-0.0538810503220736));
#39821=DIRECTION('center_axis',(-0.631948690569006,-0.772532669185509,-0.0619203321150045));
#39822=DIRECTION('ref_axis',(0.212600461685972,-0.249632918685971,0.944713951203874));
#39823=DIRECTION('center_axis',(-0.629471273307508,-0.456899628845233,-0.628497132246213));
#39824=DIRECTION('ref_axis',(-0.745283693861492,0.583835272272019,0.322007128050339));
#39825=DIRECTION('center_axis',(-0.703545043437849,-0.00327462087547922,
-0.710643123313071));
#39826=DIRECTION('ref_axis',(-0.595295187901339,0.548876942737332,0.58682002436252));
#39827=DIRECTION('center_axis',(0.126798015387979,0.0184102004931597,-0.991757696119103));
#39828=DIRECTION('ref_axis',(-0.674494684978775,0.734701710295614,-0.0725969477601046));
#39829=DIRECTION('center_axis',(0.337389367637308,-0.0208194531308848,-0.941134934521415));
#39830=DIRECTION('ref_axis',(-0.637783115038796,0.730279423602685,-0.244795142177984));
#39831=DIRECTION('',(0.70749274103932,0.681076592669504,0.188649665502934));
#39832=DIRECTION('',(-0.70749274103932,0.681076592669504,0.188649665502934));
#39833=DIRECTION('',(-0.724633338758358,0.67760887776062,0.125509892597787));
#39834=DIRECTION('center_axis',(4.6699357595302E-12,-1.,-1.22734079440797E-12));
#39835=DIRECTION('ref_axis',(-0.937281717636962,-3.94796067924408E-12,-0.348572778316818));
#39836=DIRECTION('',(-0.549972007288369,0.810772660219186,-0.20044571494623));
#39837=DIRECTION('center_axis',(0.,-1.,0.));
#39838=DIRECTION('ref_axis',(-0.845128221450091,0.,-0.534563643833553));
#39839=DIRECTION('',(-0.532777339634286,0.817212408304852,-0.219800332312754));
#39840=DIRECTION('center_axis',(0.,1.,0.));
#39841=DIRECTION('ref_axis',(-0.845112251565906,0.,-0.534588890880839));
#39842=DIRECTION('',(-0.158243927826022,0.930070177257986,-0.331554406819593));
#39843=DIRECTION('',(-0.126460756662279,0.930954528604445,-0.342536629713202));
#39844=DIRECTION('center_axis',(0.,-1.,0.));
#39845=DIRECTION('ref_axis',(0.633622560519774,0.,-0.773642327435854));
#39846=DIRECTION('',(-3.46493233997901E-14,0.690868651664906,-0.722980294438731));
#39847=DIRECTION('center_axis',(0.,-1.,0.));
#39848=DIRECTION('ref_axis',(-0.633782984477245,0.,-0.773510910451247));
#39849=DIRECTION('',(0.126460756667282,0.930954528602216,-0.342536629717412));
#39850=DIRECTION('center_axis',(-2.44519893085839E-16,1.,-2.75686781185422E-14));
#39851=DIRECTION('ref_axis',(0.633782984477227,-2.12111638737612E-14,-0.773510910451261));
#39852=DIRECTION('',(0.158243927826291,0.930070177257933,-0.331554406819613));
#39853=DIRECTION('center_axis',(0.,1.,0.));
#39854=DIRECTION('ref_axis',(0.633622560519774,0.,0.773642327435854));
#39855=DIRECTION('',(0.532777339638841,0.817212408301779,-0.219800332313137));
#39856=DIRECTION('',(0.54997200729065,0.810772660217083,-0.200445714948479));
#39857=DIRECTION('center_axis',(0.,-1.,0.));
#39858=DIRECTION('ref_axis',(0.845112251565906,0.,-0.534588890880839));
#39859=DIRECTION('',(0.724633338767814,0.677608877750319,0.125509892598804));
#39860=DIRECTION('center_axis',(0.,1.,0.));
#39861=DIRECTION('ref_axis',(0.845128221450091,0.,-0.534563643833553));
#39862=DIRECTION('center_axis',(4.6699357595302E-12,1.,1.22734079440797E-12));
#39863=DIRECTION('ref_axis',(0.937281717636962,-3.94796067924408E-12,-0.348572778316818));
#39864=DIRECTION('center_axis',(-2.44929359829E-16,-1.,1.22464679915E-16));
#39865=DIRECTION('ref_axis',(-1.,2.44929359829E-16,0.));
#39866=DIRECTION('center_axis',(-2.44929359829E-16,-1.,1.22464679915E-16));
#39867=DIRECTION('ref_axis',(1.,-2.44929359829E-16,2.99951956532443E-32));
#39868=DIRECTION('center_axis',(-2.44929359829E-16,-1.,1.22464679915E-16));
#39869=DIRECTION('ref_axis',(1.,-2.44929359829E-16,-2.25001164789147E-32));
#39870=DIRECTION('center_axis',(-2.44929359829E-16,-1.,1.22464679915E-16));
#39871=DIRECTION('ref_axis',(1.,-2.44929359829E-16,-2.35882174039441E-33));
#39872=DIRECTION('center_axis',(-2.44929359829E-16,-1.,1.22464679915E-16));
#39873=DIRECTION('ref_axis',(1.,-2.44929359829E-16,2.99951956532443E-32));
#39874=DIRECTION('center_axis',(2.44929359829E-16,1.,-1.22464679915E-16));
#39875=DIRECTION('ref_axis',(1.,-2.44929359829E-16,2.99951956532443E-32));
#39876=DIRECTION('center_axis',(2.44929359829E-16,1.,-1.22464679915E-16));
#39877=DIRECTION('ref_axis',(1.,-2.44929359829E-16,-2.35882174039442E-33));
#39878=DIRECTION('center_axis',(2.44929359829E-16,1.,-1.22464679915E-16));
#39879=DIRECTION('ref_axis',(1.,-2.44929359829E-16,-2.25001164789147E-32));
#39880=DIRECTION('center_axis',(-2.44929359829289E-16,-1.,1.22464679914817E-16));
#39881=DIRECTION('ref_axis',(-0.844952619998974,1.41454552433996E-16,-0.534841163296983));
#39882=DIRECTION('center_axis',(3.20197585381547E-15,-1.,5.00923523856943E-15));
#39883=DIRECTION('ref_axis',(-0.254396783383164,-5.76114676938621E-15,-0.967099931033138));
#39884=DIRECTION('',(0.,-1.,1.13869028167E-16));
#39885=DIRECTION('',(-3.9650822308E-16,-1.,0.));
#39886=DIRECTION('center_axis',(-2.44929359829546E-16,-1.,1.22464679915124E-16));
#39887=DIRECTION('ref_axis',(-0.975256647866936,2.65942952836982E-16,0.221075712802985));
#39888=DIRECTION('',(-4.55476112667E-16,-1.,2.27738056333E-16));
#39889=DIRECTION('center_axis',(1.27286491546545E-14,-1.,-7.63214849541229E-16));
#39890=DIRECTION('ref_axis',(-0.994685788780406,-1.25120668655344E-14,-0.102957183325405));
#39891=DIRECTION('center_axis',(-2.44929359828997E-16,-1.,1.22464679914357E-16));
#39892=DIRECTION('ref_axis',(-0.00535506551034943,1.23774536725987E-16,
0.999985661533894));
#39893=DIRECTION('',(-2.41971684854E-16,-1.,0.));
#39894=DIRECTION('center_axis',(1.42571546068487E-15,-1.,-2.56729319960534E-15));
#39895=DIRECTION('ref_axis',(-0.846038107384351,-2.53200862645747E-15,0.533122425764951));
#39896=DIRECTION('center_axis',(2.44929359829001E-16,1.,-1.22464679914941E-16));
#39897=DIRECTION('ref_axis',(0.00535506551034943,1.21151311191987E-16,0.999985661533894));
#39898=DIRECTION('center_axis',(0.,1.,0.));
#39899=DIRECTION('ref_axis',(0.846038107384351,0.,0.533122425764951));
#39900=DIRECTION('',(0.,-1.,0.));
#39901=DIRECTION('center_axis',(2.4492935982935E-16,1.,-1.22464679914921E-16));
#39902=DIRECTION('ref_axis',(0.975256647866936,-2.11795020025986E-16,0.221075712802985));
#39903=DIRECTION('center_axis',(-6.33314902666E-15,1.,-9.01543124247796E-16));
#39904=DIRECTION('ref_axis',(0.994685788780406,6.25603343276713E-15,-0.10295718332541));
#39905=DIRECTION('',(0.,-1.,0.));
#39906=DIRECTION('center_axis',(2.44929359829233E-16,1.,-1.22464679915147E-16));
#39907=DIRECTION('ref_axis',(0.844952619998974,-2.72452856170991E-16,-0.534841163296983));
#39908=DIRECTION('center_axis',(0.,1.,0.));
#39909=DIRECTION('ref_axis',(0.254396783383163,0.,-0.967099931033138));
#39910=DIRECTION('',(-3.9650822308E-16,-1.,0.));
#39911=DIRECTION('center_axis',(2.44929359828916E-16,1.,-1.22464679914681E-16));
#39912=DIRECTION('ref_axis',(0.254396783383044,-1.80744824796032E-16,-0.967099931033169));
#39913=DIRECTION('center_axis',(0.,1.,0.));
#39914=DIRECTION('ref_axis',(-0.254396783384328,0.,-0.967099931032832));
#39915=DIRECTION('center_axis',(-2.44929359829E-16,-1.,1.22464679915E-16));
#39916=DIRECTION('ref_axis',(-1.,2.44929359829E-16,0.));
#39917=DIRECTION('axis',(0.,0.,1.));
#39918=DIRECTION('refdir',(1.,0.,0.));
#39919=DIRECTION('center_axis',(0.,1.,0.));
#39920=DIRECTION('ref_axis',(1.,0.,0.));
#39921=DIRECTION('center_axis',(-4.53826900753912E-20,1.,-1.89783535791704E-12));
#39922=DIRECTION('ref_axis',(0.999999996595594,-1.56555493309401E-16,-8.25155224061155E-5));
#39923=DIRECTION('center_axis',(-3.6775085234444E-13,-1.,1.12427017219775E-12));
#39924=DIRECTION('ref_axis',(0.949453459673758,3.75489493260349E-15,0.313907833469525));
#39925=DIRECTION('',(6.70258519737E-14,0.,1.));
#39926=DIRECTION('center_axis',(1.50438405503027E-11,-1.,-7.96818632756709E-11));
#39927=DIRECTION('ref_axis',(0.982070554550592,-2.47012319048512E-13,0.188513728637183));
#39928=DIRECTION('center_axis',(0.,-1.,0.));
#39929=DIRECTION('ref_axis',(0.983200783709105,0.,-0.182527310049212));
#39930=DIRECTION('',(5.34758952088E-14,0.,-1.));
#39931=DIRECTION('center_axis',(4.23985864404906E-13,-1.,1.28365524709865E-12));
#39932=DIRECTION('ref_axis',(0.949639883258862,4.08975341799599E-16,-0.313343409255875));
#39933=DIRECTION('center_axis',(0.,1.,0.));
#39934=DIRECTION('ref_axis',(0.99999996092868,0.,0.000279540048092856));
#39935=DIRECTION('center_axis',(0.,1.,0.));
#39936=DIRECTION('ref_axis',(1.,0.,0.));
#39937=DIRECTION('center_axis',(0.,1.,0.));
#39938=DIRECTION('ref_axis',(0.999999972082516,0.,-0.000236294239609272));
#39939=DIRECTION('',(6.51345827468E-14,0.,1.));
#39940=DIRECTION('center_axis',(0.,-1.,0.));
#39941=DIRECTION('ref_axis',(0.94940501112193,0.,0.31405433424261));
#39942=DIRECTION('center_axis',(0.,-1.,0.));
#39943=DIRECTION('ref_axis',(0.949684781053655,0.,-0.313207306164895));
#39944=DIRECTION('',(5.92102704963E-14,0.,-1.));
#39945=DIRECTION('center_axis',(0.,1.,0.));
#39946=DIRECTION('ref_axis',(0.999999881236024,0.,0.000487368379934368));
#39947=DIRECTION('center_axis',(-0.981439111391386,-6.91947304276285E-7,
0.19177400926822));
#39948=DIRECTION('ref_axis',(0.135605174340565,-0.707106824297193,0.693982114844759));
#39949=DIRECTION('center_axis',(-0.983800902348753,2.55819041831388E-6,
0.179264565743584));
#39950=DIRECTION('ref_axis',(0.126757816828919,-0.707104514303595,0.695654843815698));
#39951=DIRECTION('center_axis',(0.,-1.,0.));
#39952=DIRECTION('ref_axis',(0.982643704634813,0.,-0.185502964239308));
#39953=DIRECTION('center_axis',(-0.981438226141561,-7.89143835502642E-7,
0.191778539642689));
#39954=DIRECTION('ref_axis',(-0.13560735839919,-0.70710678023174,-0.693981732971621));
#39955=DIRECTION('center_axis',(0.,-1.,0.));
#39956=DIRECTION('ref_axis',(0.982643702177,0.,-0.185502977258799));
#39957=DIRECTION('center_axis',(-0.983803848856482,2.10287653257285E-5,
0.179248393390189));
#39958=DIRECTION('ref_axis',(0.126755899045361,0.707142957839062,0.695616114847712));
#39959=DIRECTION('center_axis',(0.,1.,0.));
#39960=DIRECTION('ref_axis',(0.185521087284598,0.,0.98264028320273));
#39961=DIRECTION('',(0.,1.,0.));
#39962=DIRECTION('',(0.,1.,0.));
#39963=DIRECTION('center_axis',(0.154836917217659,-3.12361430976921E-6,
0.987940043249981));
#39964=DIRECTION('ref_axis',(0.698580542308629,-0.707104979136634,-0.109488695251894));
#39965=DIRECTION('center_axis',(0.154845223447756,-1.35064972128871E-7,
0.98793874140829));
#39966=DIRECTION('ref_axis',(-0.698578109459083,-0.707106871046533,0.109491999266408));
#39967=DIRECTION('',(0.,1.,0.));
#39968=DIRECTION('center_axis',(0.520972865596847,1.69414956570985E-6,0.853573238397819));
#39969=DIRECTION('ref_axis',(0.603568577001839,-0.707106162849763,-0.368382745681526));
#39970=DIRECTION('center_axis',(0.520969134614679,-1.13333766643287E-11,
0.85357551556897));
#39971=DIRECTION('ref_axis',(0.603569036189203,0.707106780165659,-0.368380808399938));
#39972=DIRECTION('',(0.,1.,0.));
#39973=DIRECTION('center_axis',(0.473837063552872,-1.24145995566389E-6,
-0.880612535228775));
#39974=DIRECTION('ref_axis',(0.622687803281783,0.707106449521282,0.335052784930248));
#39975=DIRECTION('center_axis',(0.473828846366866,-2.37517960535292E-6,
-0.88061695665312));
#39976=DIRECTION('ref_axis',(-0.622690007725239,0.707106120461181,-0.335049382457988));
#39977=DIRECTION('',(0.,1.,0.));
#39978=DIRECTION('center_axis',(0.904703679923686,3.52343105396791E-6,-0.426041373014554));
#39979=DIRECTION('ref_axis',(0.301254485151548,0.70710679235048,0.639723158395795));
#39980=DIRECTION('center_axis',(0.904707515904337,-3.36627255552488E-8,
-0.42603322718563));
#39981=DIRECTION('ref_axis',(0.301250989895463,-0.707106716692524,0.639724887975543));
#39982=DIRECTION('',(0.,1.,0.));
#39983=DIRECTION('center_axis',(0.980476419194366,4.59982314936753E-7,-0.196636699025342));
#39984=DIRECTION('ref_axis',(0.139042808353642,0.70710686281341,0.693301508730011));
#39985=DIRECTION('center_axis',(0.,-1.,0.));
#39986=DIRECTION('ref_axis',(0.949544989671707,0.,-0.313630854013693));
#39987=DIRECTION('center_axis',(0.,-1.,0.));
#39988=DIRECTION('ref_axis',(0.949544989671193,0.,-0.313630854015248));
#39989=DIRECTION('center_axis',(0.980477123615918,9.28542161123966E-7,-0.196633186580987));
#39990=DIRECTION('ref_axis',(0.139041425768334,-0.707106158854598,0.693302503983798));
#39991=DIRECTION('',(0.,1.,0.));
#39992=DIRECTION('center_axis',(-1.01620465039977E-5,4.17131142926177E-6,
-0.999999999939666));
#39993=DIRECTION('ref_axis',(0.707097475073845,0.707116087164088,-4.23595600861289E-6));
#39994=DIRECTION('center_axis',(-9.12499515000718E-8,-3.77832852281249E-8,
-0.999999999999995));
#39995=DIRECTION('ref_axis',(0.70710678547465,-0.707106776898444,-3.78066428416396E-8));
#39996=DIRECTION('',(2.51386213433E-14,1.,0.));
#39997=DIRECTION('center_axis',(5.34758952088E-14,0.,-1.));
#39998=DIRECTION('ref_axis',(-1.,2.31296463463574E-14,-5.34758952088E-14));
#39999=DIRECTION('',(5.3463780235E-14,0.,-1.));
#40000=DIRECTION('center_axis',(5.92118946467E-14,-1.35858726807196E-28,
-1.));
#40001=DIRECTION('ref_axis',(5.42101086242749E-16,-1.,1.67957559213664E-28));
#40002=DIRECTION('',(5.3463780235E-14,0.,-1.));
#40003=DIRECTION('center_axis',(1.,-2.51304279671E-14,5.34739473113E-14));
#40004=DIRECTION('ref_axis',(-5.34739473113E-14,0.,1.));
#40005=DIRECTION('',(0.,1.,0.));
#40006=DIRECTION('center_axis',(0.0335673088203785,9.76784545296555E-7,
0.999436459099628));
#40007=DIRECTION('ref_axis',(0.706708319465629,-0.707106782500715,-0.0237349813472152));
#40008=DIRECTION('center_axis',(0.033571208573789,-2.79700859966269E-6,
0.999436328110537));
#40009=DIRECTION('ref_axis',(0.70670899253357,0.707106059613177,-0.0237364767923099));
#40010=DIRECTION('',(0.,1.,0.));
#40011=DIRECTION('',(0.,1.,0.));
#40012=DIRECTION('center_axis',(0.999999978084788,-0.000101096238990269,
0.000183330234716788));
#40013=DIRECTION('ref_axis',(5.81481962535521E-5,-0.707106853629676,-0.707106706352533));
#40014=DIRECTION('',(0.,1.,0.));
#40015=DIRECTION('center_axis',(0.0335656369607943,-6.36312949534584E-7,
-0.999436515249974));
#40016=DIRECTION('ref_axis',(0.706708024598012,0.707107109174478,0.0237340288128194));
#40017=DIRECTION('center_axis',(0.0335621289194674,1.19749411790846E-10,
-0.999436633060042));
#40018=DIRECTION('ref_axis',(-0.706708201393549,0.707107000522345,-0.023732001504006));
#40019=DIRECTION('',(0.,1.,0.));
#40020=DIRECTION('center_axis',(-0.296880383254147,-5.5879869627127E-5,
-0.954914674154875));
#40021=DIRECTION('ref_axis',(0.675214504950974,0.707107206299133,-0.209963737592105));
#40022=DIRECTION('',(0.,1.,0.));
#40023=DIRECTION('center_axis',(-0.97943439723664,1.88767156221692E-7,-0.201762884370897));
#40024=DIRECTION('ref_axis',(0.142668223249667,0.707105845503049,-0.692565593521799));
#40025=DIRECTION('center_axis',(-0.979434890534362,-1.13639773389063E-6,
-0.201760489696696));
#40026=DIRECTION('ref_axis',(0.142667101613083,-0.707106265008557,-0.692565396264476));
#40027=DIRECTION('',(0.,1.,0.));
#40028=DIRECTION('center_axis',(-0.979434533515105,-4.50567798853205E-7,
0.201762222821431));
#40029=DIRECTION('ref_axis',(0.142667769468626,-0.707106674739596,0.692564840353275));
#40030=DIRECTION('center_axis',(0.,1.,0.));
#40031=DIRECTION('ref_axis',(1.,0.,4.53995751566807E-15));
#40032=DIRECTION('center_axis',(0.,1.,0.));
#40033=DIRECTION('ref_axis',(1.,0.,-1.77342090453718E-17));
#40034=DIRECTION('center_axis',(-0.979433511432438,-1.51283178385928E-6,
0.201767184350767));
#40035=DIRECTION('ref_axis',(-0.142669686404077,-0.707107822666436,-0.692563273430879));
#40036=DIRECTION('',(0.,1.,0.));
#40037=DIRECTION('center_axis',(0.473835002614585,-4.38921425069636E-12,
0.880613644169358));
#40038=DIRECTION('ref_axis',(0.62268754361935,-0.70710716248492,-0.335051762842439));
#40039=DIRECTION('center_axis',(0.520966517709422,1.18825474124969E-6,-0.853577112758014));
#40040=DIRECTION('ref_axis',(0.603569632363666,0.707106892020158,0.368379616898087));
#40041=DIRECTION('center_axis',(0.473834278771671,2.54149984160096E-8,0.880614033649777));
#40042=DIRECTION('ref_axis',(-0.622688145028847,-0.707106782614661,0.335051446827015));
#40043=DIRECTION('center_axis',(0.520965370835567,-1.29982441725717E-6,
-0.853577812732074));
#40044=DIRECTION('ref_axis',(-0.603570181217405,0.707106780728377,-0.368378931255765));
#40045=DIRECTION('',(0.,1.,0.));
#40046=DIRECTION('',(0.,1.,0.));
#40047=DIRECTION('center_axis',(0.154843595557673,1.07297464218487E-6,-0.987938996554757));
#40048=DIRECTION('ref_axis',(0.698578639261851,0.707106383509641,0.109491767576273));
#40049=DIRECTION('center_axis',(0.1548978156336,3.28185673290842E-5,-0.987930496358363));
#40050=DIRECTION('ref_axis',(-0.698568936199091,0.707113878525059,-0.109505270078283));
#40051=DIRECTION('',(0.,1.,0.));
#40052=DIRECTION('center_axis',(-0.983798505452903,-7.41074738031404E-6,
-0.179277719233919));
#40053=DIRECTION('ref_axis',(0.12676491018783,0.707097999012039,-0.695660173747384));
#40054=DIRECTION('center_axis',(-0.983801593483001,7.34382161735624E-7,
-0.17926077278582));
#40055=DIRECTION('ref_axis',(-0.126755910682294,0.70710726361168,0.695652396570805));
#40056=DIRECTION('',(0.,1.,0.));
#40057=DIRECTION('center_axis',(-0.981439661906731,1.44249277216099E-6,
-0.191771191878033));
#40058=DIRECTION('ref_axis',(0.135603711019434,0.707106782535524,-0.693982443329813));
#40059=DIRECTION('center_axis',(0.,-1.,0.));
#40060=DIRECTION('ref_axis',(0.982642715024755,0.,0.185508206311143));
#40061=DIRECTION('center_axis',(0.,-1.,0.));
#40062=DIRECTION('ref_axis',(0.982642715024755,0.,0.185508206311143));
#40063=DIRECTION('center_axis',(-0.981441652211516,-4.67297560071752E-6,
-0.191761005635902));
#40064=DIRECTION('ref_axis',(0.135598750250042,-0.707106782087573,-0.69398341309889));
#40065=DIRECTION('center_axis',(0.,1.,0.));
#40066=DIRECTION('ref_axis',(-0.185521087269691,0.,0.982640283205544));
#40067=DIRECTION('',(0.,1.,0.));
#40068=DIRECTION('',(-5.31321018928E-14,1.,0.));
#40069=DIRECTION('center_axis',(6.70258519737E-14,-4.98239453982157E-43,
1.));
#40070=DIRECTION('ref_axis',(1.,4.62592926927149E-14,-6.70258519737E-14));
#40071=DIRECTION('center_axis',(-1.10324427504723E-11,-1.10324427504724E-11,
1.));
#40072=DIRECTION('ref_axis',(0.707106778746433,-0.707106783626662,-5.38408906596044E-20));
#40073=DIRECTION('',(6.70203270059E-14,0.,1.));
#40074=DIRECTION('center_axis',(6.51330841113E-14,-8.98109190113476E-29,
1.));
#40075=DIRECTION('ref_axis',(-7.22801448323666E-16,-1.,-4.27326314819128E-29));
#40076=DIRECTION('',(6.70203270059E-14,0.,1.));
#40077=DIRECTION('center_axis',(-7.94004949271736E-11,7.94004949271753E-11,
1.));
#40078=DIRECTION('ref_axis',(-0.707106780907752,-0.707106781465343,4.42741533183115E-20));
#40079=DIRECTION('center_axis',(-1.,-5.30625513235E-14,6.70263256881E-14));
#40080=DIRECTION('ref_axis',(-5.30625513235E-14,1.,-1.81689879574742E-43));
#40081=DIRECTION('',(0.,1.,0.));
#40082=DIRECTION('center_axis',(0.980478566353175,3.7723498926218E-6,0.196625992452148));
#40083=DIRECTION('ref_axis',(0.139037044282546,-0.707112597974319,-0.693296815298601));
#40084=DIRECTION('center_axis',(0.980476663067875,-1.6843586153538E-12,
0.196635483011803));
#40085=DIRECTION('ref_axis',(0.139042284163302,0.70710677761346,-0.693301700753547));
#40086=DIRECTION('',(0.,1.,0.));
#40087=DIRECTION('center_axis',(0.904708058486416,4.59948929901095E-7,0.426032074977376));
#40088=DIRECTION('ref_axis',(0.301250429246376,-0.707106861495181,-0.639724991934275));
#40089=DIRECTION('center_axis',(0.,-1.,0.));
#40090=DIRECTION('ref_axis',(0.949544989671187,0.,0.313630854015266));
#40091=DIRECTION('center_axis',(0.,-1.,0.));
#40092=DIRECTION('ref_axis',(0.949544989671187,0.,0.313630854015266));
#40093=DIRECTION('center_axis',(0.904706532331394,9.28476887061025E-7,0.426035315855436));
#40094=DIRECTION('ref_axis',(-0.301252132655329,-0.707106157393727,0.639724968049938));
#40095=DIRECTION('',(0.,1.,0.));
#40096=DIRECTION('center_axis',(0.831646496536582,-3.85743040235925E-7,
0.555305415783314));
#40097=DIRECTION('ref_axis',(-0.392659665147305,-0.707108198105435,0.588061547406809));
#40098=DIRECTION('center_axis',(0.520955689889625,-6.10489755846883E-6,
-0.853583721221507));
#40099=DIRECTION('ref_axis',(-0.603570886687802,0.70710877515402,-0.368373947019984));
#40100=DIRECTION('center_axis',(0.831646480866685,3.73065313146438E-7,0.555305439251157));
#40101=DIRECTION('ref_axis',(0.392659054445677,-0.707109314315335,-0.588060613007131));
#40102=DIRECTION('center_axis',(0.520969129687222,5.06965085525085E-8,-0.85357551857638));
#40103=DIRECTION('ref_axis',(0.603569010894602,0.707106790406539,0.368380830186201));
#40104=DIRECTION('',(0.,1.,0.));
#40105=DIRECTION('',(0.,1.,0.));
#40106=DIRECTION('center_axis',(-0.160486455919009,-1.14494809085679E-8,
-0.987038042562978));
#40107=DIRECTION('ref_axis',(-0.697941290843371,0.707106784875672,0.113481052685807));
#40108=DIRECTION('center_axis',(-0.160486595636023,6.52250457089104E-13,
-0.987038019845821));
#40109=DIRECTION('ref_axis',(0.697941276113114,0.707106782208678,-0.113481159899282));
#40110=DIRECTION('',(0.,1.,0.));
#40111=DIRECTION('center_axis',(0.999999997768984,-1.78060155735714E-9,
6.67984466585521E-5));
#40112=DIRECTION('ref_axis',(4.72348957176867E-5,0.707106750687066,-0.707106810108377));
#40113=DIRECTION('center_axis',(0.999999997862801,4.18017746208693E-16,
6.53788750221213E-5));
#40114=DIRECTION('ref_axis',(4.6229822268084E-5,-0.707107142261732,-0.707106418599952));
#40115=DIRECTION('',(0.,1.,0.));
#40116=DIRECTION('center_axis',(-0.160485631761041,-3.83256429423384E-7,
0.987038176565685));
#40117=DIRECTION('ref_axis',(-0.697939946398453,-0.707108197591881,-0.113480518679139));
#40118=DIRECTION('center_axis',(-0.160485659064817,3.71132526604556E-7,
0.987038172126283));
#40119=DIRECTION('ref_axis',(0.697938843129776,-0.707109313555971,0.11348035042717));
#40120=DIRECTION('',(0.,1.,0.));
#40121=DIRECTION('center_axis',(0.831647339569147,-2.01970215594345E-7,
-0.555304153223726));
#40122=DIRECTION('ref_axis',(-0.392659211278407,0.70710678535694,-0.58806354920229));
#40123=DIRECTION('center_axis',(0.831642793947518,2.20503061757152E-6,-0.555310960877151));
#40124=DIRECTION('ref_axis',(0.392662307348694,0.707107757326728,0.588060313161809));
#40125=DIRECTION('',(0.,1.,0.));
#40126=DIRECTION('center_axis',(0.52097569735597,-2.97995712518636E-6,0.853571510042117));
#40127=DIRECTION('ref_axis',(0.603567201195272,0.707106897821364,-0.368383589068178));
#40128=DIRECTION('center_axis',(0.520966807973242,-7.72496346239503E-7,
0.853576935600755));
#40129=DIRECTION('ref_axis',(0.603569754740143,-0.707106781322477,-0.368379628875825));
#40130=DIRECTION('',(0.,1.,0.));
#40131=DIRECTION('center_axis',(0.154844796216802,-8.97906301415941E-8,
0.987938808370523));
#40132=DIRECTION('ref_axis',(-0.698578220064376,-0.707106802000707,0.109491739487604));
#40133=DIRECTION('center_axis',(0.154844863297137,1.72305380745362E-8,0.987938797856674));
#40134=DIRECTION('ref_axis',(0.698578206815753,-0.707106799844172,-0.109491837943393));
#40135=DIRECTION('',(0.,1.,0.));
#40136=DIRECTION('center_axis',(-0.990334650762026,-1.38749992122331E-10,
0.138698520179765));
#40137=DIRECTION('ref_axis',(0.0980746699601121,0.707106738665372,0.700272389321638));
#40138=DIRECTION('center_axis',(-0.990334159630947,1.08015952695937E-6,
0.138702026902633));
#40139=DIRECTION('ref_axis',(0.098076591555837,-0.707105309160556,0.700273563649053));
#40140=DIRECTION('',(0.,1.,0.));
#40141=DIRECTION('center_axis',(-0.990334489416453,-4.27056810582187E-7,
-0.138699672213279));
#40142=DIRECTION('ref_axis',(0.0980757788219265,-0.707106774008865,-0.700272198333797));
#40143=DIRECTION('center_axis',(0.,1.,0.));
#40144=DIRECTION('ref_axis',(1.,0.,5.1304900982414E-15));
#40145=DIRECTION('center_axis',(-0.990345075157185,2.9441547790821E-5,-0.138624064451688));
#40146=DIRECTION('ref_axis',(0.0980424742908994,0.707107928682427,-0.700275696015052));
#40147=DIRECTION('center_axis',(0.,1.,0.));
#40148=DIRECTION('ref_axis',(1.,0.,1.00009553569338E-17));
#40149=DIRECTION('',(0.,1.,0.));
#40150=DIRECTION('center_axis',(0.154794000275648,-2.07516415067679E-5,
-0.987946768327136));
#40151=DIRECTION('ref_axis',(-0.698579366791292,0.707109029425635,-0.109470036074784));
#40152=DIRECTION('center_axis',(0.154851124507597,-3.12677899154245E-6,
-0.987937816478829));
#40153=DIRECTION('ref_axis',(0.698577610398848,0.707107045772696,0.109494054943846));
#40154=DIRECTION('',(0.,1.,0.));
#40155=DIRECTION('axis',(0.,0.,1.));
#40156=DIRECTION('refdir',(1.,0.,0.));
#40157=DIRECTION('center_axis',(0.,-1.,0.));
#40158=DIRECTION('ref_axis',(0.,0.,-1.));
#40159=DIRECTION('',(0.,0.,1.));
#40160=DIRECTION('',(0.,0.,-1.));
#40161=DIRECTION('',(0.,0.,1.));
#40162=DIRECTION('',(0.,0.,-1.));
#40163=DIRECTION('center_axis',(0.,-1.,0.));
#40164=DIRECTION('ref_axis',(1.,0.,0.));
#40165=DIRECTION('center_axis',(0.,-1.,0.));
#40166=DIRECTION('ref_axis',(1.,0.,0.));
#40167=DIRECTION('center_axis',(0.,-1.,0.));
#40168=DIRECTION('ref_axis',(0.,0.,-1.));
#40169=DIRECTION('',(0.,0.,-1.));
#40170=DIRECTION('',(0.,0.,1.));
#40171=DIRECTION('center_axis',(0.,-1.,0.));
#40172=DIRECTION('ref_axis',(1.,0.,0.));
#40173=DIRECTION('center_axis',(0.,-1.,0.));
#40174=DIRECTION('ref_axis',(1.,0.,0.));
#40175=DIRECTION('',(0.,0.,1.));
#40176=DIRECTION('',(0.,0.,-1.));
#40177=DIRECTION('center_axis',(0.,-1.,0.));
#40178=DIRECTION('ref_axis',(-1.,0.,1.45603019622971E-16));
#40179=DIRECTION('center_axis',(0.,-1.,0.));
#40180=DIRECTION('ref_axis',(1.,0.,0.));
#40181=DIRECTION('center_axis',(0.,0.,1.));
#40182=DIRECTION('ref_axis',(1.,0.,0.));
#40183=DIRECTION('center_axis',(0.,-1.,0.));
#40184=DIRECTION('ref_axis',(-1.,0.,5.51957469628984E-16));
#40185=DIRECTION('',(0.,-1.,0.));
#40186=DIRECTION('center_axis',(0.,-1.,0.));
#40187=DIRECTION('ref_axis',(1.,0.,3.64007549057428E-16));
#40188=DIRECTION('center_axis',(0.,-1.,0.));
#40189=DIRECTION('ref_axis',(1.,0.,0.));
#40190=DIRECTION('center_axis',(4.55009436321785E-16,0.,-1.));
#40191=DIRECTION('ref_axis',(-1.,0.,-4.55009436321785E-16));
#40192=DIRECTION('center_axis',(0.,-1.,0.));
#40193=DIRECTION('ref_axis',(1.,0.,4.73106402539129E-16));
#40194=DIRECTION('',(0.,-1.,0.));
#40195=DIRECTION('center_axis',(0.954875323536579,7.50697958768155E-7,0.297006930054419));
#40196=DIRECTION('ref_axis',(0.210016056245524,-0.707106999787048,-0.675198450065784));
#40197=DIRECTION('center_axis',(3.24818764753068E-6,-1.23643017124277E-11,
0.999999999994725));
#40198=DIRECTION('ref_axis',(0.707106611008976,-0.707106951360347,-2.29682370226244E-6));
#40199=DIRECTION('',(0.,-1.,0.));
#40200=DIRECTION('',(0.,-1.,0.));
#40201=DIRECTION('center_axis',(0.,0.,1.));
#40202=DIRECTION('ref_axis',(-1.,0.,0.));
#40203=DIRECTION('center_axis',(0.,0.,1.));
#40204=DIRECTION('ref_axis',(3.70074341541716E-15,-1.,0.));
#40205=DIRECTION('',(0.,0.,1.));
#40206=DIRECTION('center_axis',(1.,0.,3.15544362088E-30));
#40207=DIRECTION('ref_axis',(-3.15544362088E-30,0.,1.));
#40208=DIRECTION('',(0.,-1.,0.));
#40209=DIRECTION('center_axis',(-0.999999999998532,6.19186184291188E-7,
1.59754516227631E-6));
#40210=DIRECTION('ref_axis',(6.91803843401809E-7,-0.707106972624542,0.707106589748163));
#40211=DIRECTION('',(0.,-1.,0.));
#40212=DIRECTION('center_axis',(-1.86759121106465E-6,5.22456588938859E-9,
-0.999999999998256));
#40213=DIRECTION('ref_axis',(0.70710691586452,0.707106646507323,-1.3168923360884E-6));
#40214=DIRECTION('',(0.,-1.,0.));
#40215=DIRECTION('center_axis',(0.,0.,-1.));
#40216=DIRECTION('ref_axis',(1.,0.,0.));
#40217=DIRECTION('center_axis',(-8.90823913776128E-12,8.90823913776095E-12,
-1.));
#40218=DIRECTION('ref_axis',(0.707106781186548,0.707106781186547,-2.33979865511361E-25));
#40219=DIRECTION('',(0.,0.,-1.));
#40220=DIRECTION('center_axis',(-1.,0.,0.));
#40221=DIRECTION('ref_axis',(0.,0.,1.));
#40222=DIRECTION('',(0.,-1.,0.));
#40223=DIRECTION('center_axis',(0.954873176751286,2.05613266315519E-6,-0.297013831860875));
#40224=DIRECTION('ref_axis',(0.21001907334242,0.707106892215597,0.675197624265364));
#40225=DIRECTION('',(0.,-1.,0.));
#40226=DIRECTION('center_axis',(0.223512880731291,7.41972707830334E-7,-0.974700975759566));
#40227=DIRECTION('ref_axis',(0.689217337981213,0.707107001090406,0.158047935877135));
#40228=DIRECTION('',(0.,-1.,0.));
#40229=DIRECTION('center_axis',(0.223525571185457,4.30435661235287E-6,0.974698065560658));
#40230=DIRECTION('ref_axis',(0.689215820938936,-0.707107264577136,-0.158053372471798));
#40231=DIRECTION('',(0.,-1.,0.));
#40232=DIRECTION('center_axis',(-0.999936197465094,6.12637967379869E-7,
-0.0112960612017118));
#40233=DIRECTION('ref_axis',(-0.00798708627314562,0.707106960926242,0.707061491146646));
#40234=DIRECTION('center_axis',(7.57660191412773E-6,-3.13873518338466E-6,
0.999999999966372));
#40235=DIRECTION('ref_axis',(-0.707106276301774,-0.707107286063998,3.13804024942857E-6));
#40236=DIRECTION('',(0.,-1.,0.));
#40237=DIRECTION('',(0.,-1.,0.));
#40238=DIRECTION('center_axis',(0.223393486583629,1.49897152312551E-6,-0.974728346848374));
#40239=DIRECTION('ref_axis',(0.689238163153829,-0.707105855285527,0.157962222930858));
#40240=DIRECTION('',(0.,-1.,0.));
#40241=DIRECTION('center_axis',(0.999999999997494,8.08987842812791E-7,2.08724718407666E-6));
#40242=DIRECTION('ref_axis',(-9.03865987698544E-7,-0.707106733063809,0.707106829308705));
#40243=DIRECTION('',(0.,-1.,0.));
#40244=DIRECTION('center_axis',(0.223400190145581,-3.77165381060116E-6,
0.974726810459573));
#40245=DIRECTION('ref_axis',(-0.689235920657423,-0.707107409693601,0.157965049399924));
#40246=DIRECTION('',(0.,-1.,0.));
#40247=DIRECTION('center_axis',(-0.999936145359499,-1.756468756071E-6,0.011300672568584));
#40248=DIRECTION('ref_axis',(-0.00798954026920954,-0.707106781570959,-0.707061642788411));
#40249=DIRECTION('',(0.,-1.,0.));
#40250=DIRECTION('center_axis',(0.,0.,-1.));
#40251=DIRECTION('ref_axis',(0.707106781635978,-0.707106780737117,0.));
#40252=DIRECTION('',(0.,-1.,0.));
#40253=DIRECTION('center_axis',(0.,0.,1.));
#40254=DIRECTION('ref_axis',(-1.,0.,0.));
#40255=DIRECTION('center_axis',(-3.91056427499541E-6,-3.975788198415E-10,
-0.999999999992354));
#40256=DIRECTION('ref_axis',(-0.707106338048842,0.70710722431857,2.76490365336202E-6));
#40257=DIRECTION('',(0.,0.,-1.));
#40258=DIRECTION('center_axis',(1.,0.,0.));
#40259=DIRECTION('ref_axis',(0.,1.,0.));
#40260=DIRECTION('',(0.,-1.,0.));
#40261=DIRECTION('center_axis',(-0.999999999976519,-2.47658205161019E-6,
6.38976095921973E-6));
#40262=DIRECTION('ref_axis',(-2.76704852940032E-6,-0.707105293783789,-0.707108268580764));
#40263=DIRECTION('',(0.,-1.,0.));
#40264=DIRECTION('center_axis',(0.,0.,1.));
#40265=DIRECTION('ref_axis',(0.707106781635978,0.707106780737117,0.));
#40266=DIRECTION('',(0.,-1.,0.));
#40267=DIRECTION('center_axis',(0.,0.,-1.));
#40268=DIRECTION('ref_axis',(1.,0.,0.));
#40269=DIRECTION('',(0.,0.,1.));
#40270=DIRECTION('center_axis',(-1.,0.,0.));
#40271=DIRECTION('ref_axis',(0.,0.,1.));
#40272=DIRECTION('axis',(0.,0.,1.));
#40273=DIRECTION('refdir',(1.,0.,0.));
#40274=DIRECTION('center_axis',(0.,1.,0.));
#40275=DIRECTION('ref_axis',(1.,0.,0.));
#40276=DIRECTION('',(0.,0.,-1.));
#40277=DIRECTION('center_axis',(0.,-1.,0.));
#40278=DIRECTION('ref_axis',(-0.256673183280288,0.,-0.966498255034516));
#40279=DIRECTION('center_axis',(0.,-1.,0.));
#40280=DIRECTION('ref_axis',(-0.280070575750354,0.,-0.959979412591158));
#40281=DIRECTION('',(0.,-1.,0.));
#40282=DIRECTION('',(0.,1.,0.));
#40283=DIRECTION('center_axis',(0.,-1.,0.));
#40284=DIRECTION('ref_axis',(1.,0.,0.));
#40285=DIRECTION('center_axis',(1.,0.,0.));
#40286=DIRECTION('ref_axis',(0.,1.,0.));
#40287=DIRECTION('',(0.,1.,0.));
#40288=DIRECTION('',(0.,0.,-1.));
#40289=DIRECTION('center_axis',(0.,1.,0.));
#40290=DIRECTION('ref_axis',(1.,0.,0.));
#40291=DIRECTION('center_axis',(0.,1.,0.));
#40292=DIRECTION('ref_axis',(1.,0.,0.));
#40293=DIRECTION('center_axis',(0.,1.,0.));
#40294=DIRECTION('ref_axis',(0.256673183280308,0.,-0.96649825503451));
#40295=DIRECTION('',(0.,0.,-1.));
#40296=DIRECTION('center_axis',(1.,0.,0.));
#40297=DIRECTION('ref_axis',(0.,1.,0.));
#40298=DIRECTION('',(0.,1.,0.));
#40299=DIRECTION('',(0.,0.,-1.));
#40300=DIRECTION('',(0.,1.,0.));
#40301=DIRECTION('center_axis',(0.,1.,0.));
#40302=DIRECTION('ref_axis',(0.280070575787534,0.,-0.959979412580311));
#40303=DIRECTION('',(0.,1.,0.));
#40304=DIRECTION('center_axis',(0.,1.,0.));
#40305=DIRECTION('ref_axis',(1.,0.,0.));
#40306=DIRECTION('center_axis',(0.,1.,0.));
#40307=DIRECTION('ref_axis',(1.,0.,0.));
#40308=DIRECTION('center_axis',(0.,1.,0.));
#40309=DIRECTION('ref_axis',(-6.12267139103014E-17,0.,1.));
#40310=DIRECTION('center_axis',(0.,-1.,0.));
#40311=DIRECTION('ref_axis',(1.,0.,0.));
#40312=DIRECTION('',(0.,1.,0.));
#40313=DIRECTION('center_axis',(0.,-1.,0.));
#40314=DIRECTION('ref_axis',(1.,0.,0.));
#40315=DIRECTION('center_axis',(0.,-1.,0.));
#40316=DIRECTION('ref_axis',(1.,0.,0.));
#40317=DIRECTION('',(0.,1.,0.));
#40318=DIRECTION('center_axis',(0.,-1.,0.));
#40319=DIRECTION('ref_axis',(2.83274710209661E-16,0.,1.));
#40320=DIRECTION('center_axis',(0.,-1.,0.));
#40321=DIRECTION('ref_axis',(1.,0.,0.));
#40322=DIRECTION('',(0.,1.,0.));
#40323=DIRECTION('center_axis',(0.,-1.,0.));
#40324=DIRECTION('ref_axis',(1.,0.,0.));
#40325=DIRECTION('',(0.,1.,0.));
#40326=DIRECTION('center_axis',(-0.341378619534878,0.,0.939925868419665));
#40327=DIRECTION('ref_axis',(0.,1.,0.));
#40328=DIRECTION('',(0.,1.,0.));
#40329=DIRECTION('',(0.939925868419665,0.,0.341378619534878));
#40330=DIRECTION('',(0.939925868419665,0.,0.341378619534878));
#40331=DIRECTION('',(0.,1.,0.));
#40332=DIRECTION('',(0.939925868419665,0.,0.341378619534878));
#40333=DIRECTION('center_axis',(0.,1.,0.));
#40334=DIRECTION('ref_axis',(1.,0.,0.));
#40335=DIRECTION('',(-1.,0.,0.));
#40336=DIRECTION('',(-1.,0.,0.));
#40337=DIRECTION('center_axis',(0.,1.,0.));
#40338=DIRECTION('ref_axis',(1.,0.,0.));
#40339=DIRECTION('',(1.,0.,0.));
#40340=DIRECTION('',(-1.,0.,0.));
#40341=DIRECTION('center_axis',(0.,-1.,0.));
#40342=DIRECTION('ref_axis',(1.,0.,0.));
#40343=DIRECTION('',(1.,0.,0.));
#40344=DIRECTION('',(-1.,0.,0.));
#40345=DIRECTION('center_axis',(0.,1.,0.));
#40346=DIRECTION('ref_axis',(1.,0.,0.));
#40347=DIRECTION('',(1.,0.,0.));
#40348=DIRECTION('',(1.,0.,0.));
#40349=DIRECTION('center_axis',(0.,1.,0.));
#40350=DIRECTION('ref_axis',(1.,0.,0.));
#40351=DIRECTION('',(-1.,0.,0.));
#40352=DIRECTION('center_axis',(0.,-1.,0.));
#40353=DIRECTION('ref_axis',(1.,0.,0.));
#40354=DIRECTION('center_axis',(0.,1.,0.));
#40355=DIRECTION('ref_axis',(1.,0.,0.));
#40356=DIRECTION('center_axis',(0.,1.,0.));
#40357=DIRECTION('ref_axis',(1.,0.,0.));
#40358=DIRECTION('',(1.,0.,0.));
#40359=DIRECTION('center_axis',(0.,1.,0.));
#40360=DIRECTION('ref_axis',(1.,0.,0.));
#40361=DIRECTION('center_axis',(0.,-1.,0.));
#40362=DIRECTION('ref_axis',(1.,0.,0.));
#40363=DIRECTION('center_axis',(0.,-1.,0.));
#40364=DIRECTION('ref_axis',(1.,0.,0.));
#40365=DIRECTION('',(0.,0.,-1.));
#40366=DIRECTION('',(1.,0.,0.));
#40367=DIRECTION('center_axis',(0.,1.,0.));
#40368=DIRECTION('ref_axis',(1.,0.,0.));
#40369=DIRECTION('',(-0.939925868419665,0.,0.341378619534878));
#40370=DIRECTION('',(0.,0.,-1.));
#40371=DIRECTION('',(-1.,0.,0.));
#40372=DIRECTION('',(0.,0.,-1.));
#40373=DIRECTION('center_axis',(0.,1.,0.));
#40374=DIRECTION('ref_axis',(1.,0.,0.));
#40375=DIRECTION('center_axis',(0.,1.,0.));
#40376=DIRECTION('ref_axis',(1.,0.,0.));
#40377=DIRECTION('',(0.,0.,-1.));
#40378=DIRECTION('center_axis',(0.,1.,0.));
#40379=DIRECTION('ref_axis',(1.,0.,0.));
#40380=DIRECTION('center_axis',(0.,1.,0.));
#40381=DIRECTION('ref_axis',(1.,0.,0.));
#40382=DIRECTION('center_axis',(0.,-1.,0.));
#40383=DIRECTION('ref_axis',(1.,0.,0.));
#40384=DIRECTION('',(0.,0.,-1.));
#40385=DIRECTION('',(-0.939925868419665,0.,0.341378619534878));
#40386=DIRECTION('center_axis',(0.,1.,0.));
#40387=DIRECTION('ref_axis',(1.,0.,0.));
#40388=DIRECTION('',(0.,0.,1.));
#40389=DIRECTION('center_axis',(0.,-1.,0.));
#40390=DIRECTION('ref_axis',(1.,0.,0.));
#40391=DIRECTION('',(0.,0.,-1.));
#40392=DIRECTION('center_axis',(0.,-1.,0.));
#40393=DIRECTION('ref_axis',(1.,0.,0.));
#40394=DIRECTION('center_axis',(0.,1.,0.));
#40395=DIRECTION('ref_axis',(1.,0.,0.));
#40396=DIRECTION('center_axis',(0.,-1.,0.));
#40397=DIRECTION('ref_axis',(1.,0.,0.));
#40398=DIRECTION('center_axis',(0.,-1.,0.));
#40399=DIRECTION('ref_axis',(1.,0.,0.));
#40400=DIRECTION('center_axis',(0.,-1.,0.));
#40401=DIRECTION('ref_axis',(1.,0.,0.));
#40402=DIRECTION('center_axis',(0.,-1.,0.));
#40403=DIRECTION('ref_axis',(1.,0.,0.));
#40404=DIRECTION('',(0.,0.,-1.));
#40405=DIRECTION('center_axis',(0.,1.,0.));
#40406=DIRECTION('ref_axis',(1.,0.,0.));
#40407=DIRECTION('center_axis',(0.,1.,0.));
#40408=DIRECTION('ref_axis',(1.,0.,0.));
#40409=DIRECTION('center_axis',(0.,1.,0.));
#40410=DIRECTION('ref_axis',(1.,0.,0.));
#40411=DIRECTION('',(0.,0.,1.));
#40412=DIRECTION('center_axis',(0.,1.,0.));
#40413=DIRECTION('ref_axis',(1.,0.,0.));
#40414=DIRECTION('',(0.939925868419665,0.,0.341378619534878));
#40415=DIRECTION('',(0.,0.,-1.));
#40416=DIRECTION('center_axis',(0.,1.,0.));
#40417=DIRECTION('ref_axis',(1.,0.,0.));
#40418=DIRECTION('center_axis',(0.,1.,0.));
#40419=DIRECTION('ref_axis',(0.,0.,1.));
#40420=DIRECTION('center_axis',(0.,1.,0.));
#40421=DIRECTION('ref_axis',(1.,0.,0.));
#40422=DIRECTION('',(0.,1.,0.));
#40423=DIRECTION('center_axis',(0.,1.,0.));
#40424=DIRECTION('ref_axis',(1.,0.,0.));
#40425=DIRECTION('center_axis',(0.,1.,0.));
#40426=DIRECTION('ref_axis',(-0.350308709236867,0.,0.936634298022873));
#40427=DIRECTION('',(-1.,0.,0.));
#40428=DIRECTION('center_axis',(0.,1.,0.));
#40429=DIRECTION('ref_axis',(1.,0.,0.));
#40430=DIRECTION('',(0.,0.,-1.));
#40431=DIRECTION('center_axis',(0.,1.,0.));
#40432=DIRECTION('ref_axis',(0.974839739501394,0.,0.222906891523915));
#40433=DIRECTION('center_axis',(-3.99809304065974E-15,1.,-3.3121011422878E-15));
#40434=DIRECTION('ref_axis',(0.977438775426633,4.67462326157961E-15,0.211218939237193));
#40435=DIRECTION('',(0.,0.,-1.));
#40436=DIRECTION('',(-1.,0.,0.));
#40437=DIRECTION('center_axis',(1.,0.,0.));
#40438=DIRECTION('ref_axis',(0.,1.,0.));
#40439=DIRECTION('',(0.,1.,0.));
#40440=DIRECTION('',(0.,0.,-1.));
#40441=DIRECTION('center_axis',(0.,1.,0.));
#40442=DIRECTION('ref_axis',(-5.05321549807E-16,0.,1.));
#40443=DIRECTION('',(0.,1.,0.));
#40444=DIRECTION('center_axis',(0.,-1.,0.));
#40445=DIRECTION('ref_axis',(1.,0.,0.));
#40446=DIRECTION('',(0.,1.,0.));
#40447=DIRECTION('center_axis',(0.,-1.,0.));
#40448=DIRECTION('ref_axis',(1.,0.,0.));
#40449=DIRECTION('',(0.,-1.,0.));
#40450=DIRECTION('center_axis',(0.,-1.,0.));
#40451=DIRECTION('ref_axis',(1.,0.,0.));
#40452=DIRECTION('',(0.,-1.,0.));
#40453=DIRECTION('center_axis',(0.,-1.,0.));
#40454=DIRECTION('ref_axis',(1.,0.,0.));
#40455=DIRECTION('',(0.,1.,0.));
#40456=DIRECTION('center_axis',(0.,-1.,0.));
#40457=DIRECTION('ref_axis',(1.,0.,0.));
#40458=DIRECTION('',(0.,1.,0.));
#40459=DIRECTION('center_axis',(0.,-1.,0.));
#40460=DIRECTION('ref_axis',(1.,0.,0.));
#40461=DIRECTION('',(0.,-1.,0.));
#40462=DIRECTION('center_axis',(0.,1.,0.));
#40463=DIRECTION('ref_axis',(1.,0.,0.));
#40464=DIRECTION('',(0.,-1.,0.));
#40465=DIRECTION('',(0.,-1.,0.));
#40466=DIRECTION('center_axis',(0.,1.,0.));
#40467=DIRECTION('ref_axis',(1.,0.,0.));
#40468=DIRECTION('',(0.,-1.,0.));
#40469=DIRECTION('center_axis',(0.,-1.,0.));
#40470=DIRECTION('ref_axis',(1.,0.,0.));
#40471=DIRECTION('center_axis',(0.,0.,1.));
#40472=DIRECTION('ref_axis',(1.,0.,0.));
#40473=DIRECTION('',(0.,1.,0.));
#40474=DIRECTION('',(1.,0.,0.));
#40475=DIRECTION('',(0.,1.,0.));
#40476=DIRECTION('center_axis',(0.,0.,1.));
#40477=DIRECTION('ref_axis',(1.,0.,0.));
#40478=DIRECTION('',(1.,0.,0.));
#40479=DIRECTION('',(0.,1.,0.));
#40480=DIRECTION('center_axis',(0.,1.,0.));
#40481=DIRECTION('ref_axis',(0.,0.,1.));
#40482=DIRECTION('',(0.,1.,0.));
#40483=DIRECTION('center_axis',(0.,-1.,0.));
#40484=DIRECTION('ref_axis',(1.,0.,0.));
#40485=DIRECTION('',(0.,-1.,0.));
#40486=DIRECTION('center_axis',(0.,-1.,0.));
#40487=DIRECTION('ref_axis',(1.,0.,0.));
#40488=DIRECTION('',(0.,-1.,0.));
#40489=DIRECTION('center_axis',(0.,-1.,0.));
#40490=DIRECTION('ref_axis',(1.,0.,0.));
#40491=DIRECTION('center_axis',(0.,0.,1.));
#40492=DIRECTION('ref_axis',(1.,0.,0.));
#40493=DIRECTION('',(0.,1.,0.));
#40494=DIRECTION('',(-1.,0.,0.));
#40495=DIRECTION('',(0.,1.,0.));
#40496=DIRECTION('center_axis',(0.,0.,1.));
#40497=DIRECTION('ref_axis',(1.,0.,0.));
#40498=DIRECTION('',(0.,-1.,0.));
#40499=DIRECTION('',(1.,0.,0.));
#40500=DIRECTION('center_axis',(0.,1.,0.));
#40501=DIRECTION('ref_axis',(-5.05321549807E-16,0.,1.));
#40502=DIRECTION('',(0.,1.,0.));
#40503=DIRECTION('center_axis',(0.,1.,0.));
#40504=DIRECTION('ref_axis',(1.,0.,0.));
#40505=DIRECTION('',(0.,1.,0.));
#40506=DIRECTION('center_axis',(0.,-1.,0.));
#40507=DIRECTION('ref_axis',(1.,0.,0.));
#40508=DIRECTION('',(0.,-1.,0.));
#40509=DIRECTION('center_axis',(0.,1.,0.));
#40510=DIRECTION('ref_axis',(1.,0.,0.));
#40511=DIRECTION('',(0.,-1.,0.));
#40512=DIRECTION('center_axis',(0.,-1.,0.));
#40513=DIRECTION('ref_axis',(1.,0.,0.));
#40514=DIRECTION('',(0.,1.,0.));
#40515=DIRECTION('center_axis',(0.,1.,0.));
#40516=DIRECTION('ref_axis',(1.,0.,0.));
#40517=DIRECTION('',(0.,1.,0.));
#40518=DIRECTION('center_axis',(0.,-1.,0.));
#40519=DIRECTION('ref_axis',(1.,0.,0.));
#40520=DIRECTION('',(0.,-1.,0.));
#40521=DIRECTION('center_axis',(0.,1.,0.));
#40522=DIRECTION('ref_axis',(1.,0.,0.));
#40523=DIRECTION('',(0.,-1.,0.));
#40524=DIRECTION('center_axis',(0.,1.,0.));
#40525=DIRECTION('ref_axis',(1.,0.,0.));
#40526=DIRECTION('',(0.,-1.,0.));
#40527=DIRECTION('center_axis',(0.,-1.,0.));
#40528=DIRECTION('ref_axis',(1.,0.,0.));
#40529=DIRECTION('center_axis',(4.93038065763E-32,0.,-1.));
#40530=DIRECTION('ref_axis',(0.,-1.,0.));
#40531=DIRECTION('',(0.,1.,0.));
#40532=DIRECTION('',(-1.,0.,0.));
#40533=DIRECTION('',(0.,1.,0.));
#40534=DIRECTION('center_axis',(4.93038065763E-32,0.,-1.));
#40535=DIRECTION('ref_axis',(0.,-1.,0.));
#40536=DIRECTION('',(1.,0.,0.));
#40537=DIRECTION('',(0.,1.,0.));
#40538=DIRECTION('center_axis',(0.,1.,0.));
#40539=DIRECTION('ref_axis',(1.22464679914735E-16,0.,-1.));
#40540=DIRECTION('',(0.,1.,0.));
#40541=DIRECTION('center_axis',(0.,-1.,0.));
#40542=DIRECTION('ref_axis',(1.,0.,0.));
#40543=DIRECTION('',(0.,-1.,0.));
#40544=DIRECTION('center_axis',(0.,-1.,0.));
#40545=DIRECTION('ref_axis',(1.,0.,0.));
#40546=DIRECTION('',(0.,-1.,0.));
#40547=DIRECTION('center_axis',(0.,-1.,0.));
#40548=DIRECTION('ref_axis',(1.,0.,0.));
#40549=DIRECTION('center_axis',(4.93038065763E-32,0.,-1.));
#40550=DIRECTION('ref_axis',(0.,-1.,0.));
#40551=DIRECTION('',(0.,1.,0.));
#40552=DIRECTION('',(-1.,0.,0.));
#40553=DIRECTION('',(0.,1.,0.));
#40554=DIRECTION('center_axis',(4.93038065763E-32,0.,-1.));
#40555=DIRECTION('ref_axis',(0.,-1.,0.));
#40556=DIRECTION('',(-1.,0.,0.));
#40557=DIRECTION('center_axis',(0.,1.,0.));
#40558=DIRECTION('ref_axis',(-1.22464679914735E-16,0.,-1.));
#40559=DIRECTION('',(0.,1.,0.));
#40560=DIRECTION('',(0.,1.,0.));
#40561=DIRECTION('center_axis',(0.,1.,0.));
#40562=DIRECTION('ref_axis',(1.,0.,0.));
#40563=DIRECTION('center_axis',(0.,1.,0.));
#40564=DIRECTION('ref_axis',(1.,0.,0.));
#40565=DIRECTION('center_axis',(0.,1.,0.));
#40566=DIRECTION('ref_axis',(1.,0.,0.));
#40567=DIRECTION('center_axis',(4.93038065763E-32,0.,-1.));
#40568=DIRECTION('ref_axis',(0.,-1.,0.));
#40569=DIRECTION('',(0.,1.,0.));
#40570=DIRECTION('',(-1.,0.,0.));
#40571=DIRECTION('',(-1.,0.,0.));
#40572=DIRECTION('center_axis',(0.,1.,0.));
#40573=DIRECTION('ref_axis',(0.260485490128613,0.,-0.965477762267188));
#40574=DIRECTION('',(0.,1.,0.));
#40575=DIRECTION('center_axis',(0.,1.,0.));
#40576=DIRECTION('ref_axis',(1.,0.,0.));
#40577=DIRECTION('center_axis',(0.,1.,0.));
#40578=DIRECTION('ref_axis',(1.,0.,0.));
#40579=DIRECTION('center_axis',(0.,1.,0.));
#40580=DIRECTION('ref_axis',(1.,0.,0.));
#40581=DIRECTION('center_axis',(0.,1.,0.));
#40582=DIRECTION('ref_axis',(1.,0.,0.));
#40583=DIRECTION('center_axis',(0.,1.,0.));
#40584=DIRECTION('ref_axis',(-3.50864490502111E-15,0.,1.));
#40585=DIRECTION('',(0.,1.,0.));
#40586=DIRECTION('center_axis',(0.,1.,0.));
#40587=DIRECTION('ref_axis',(1.,0.,0.));
#40588=DIRECTION('center_axis',(0.,-1.,0.));
#40589=DIRECTION('ref_axis',(-0.260485490128613,0.,-0.965477762267188));
#40590=DIRECTION('center_axis',(0.,1.,0.));
#40591=DIRECTION('ref_axis',(1.,0.,0.));
#40592=DIRECTION('center_axis',(0.,1.,0.));
#40593=DIRECTION('ref_axis',(1.,0.,0.));
#40594=DIRECTION('center_axis',(0.,1.,0.));
#40595=DIRECTION('ref_axis',(1.,0.,0.));
#40596=DIRECTION('center_axis',(0.,1.,0.));
#40597=DIRECTION('ref_axis',(1.,0.,0.));
#40598=DIRECTION('',(0.,1.,0.));
#40599=DIRECTION('center_axis',(4.93038065763E-32,0.,-1.));
#40600=DIRECTION('ref_axis',(0.,-1.,0.));
#40601=DIRECTION('',(-1.,0.,0.));
#40602=DIRECTION('',(-1.,0.,0.));
#40603=DIRECTION('center_axis',(1.,0.,0.));
#40604=DIRECTION('ref_axis',(0.,1.,0.));
#40605=DIRECTION('',(0.,1.,0.));
#40606=DIRECTION('',(0.,0.,-1.));
#40607=DIRECTION('',(0.,0.,-1.));
#40608=DIRECTION('',(0.,-1.,0.));
#40609=DIRECTION('center_axis',(-0.341378619534878,0.,-0.939925868419665));
#40610=DIRECTION('ref_axis',(-0.939925868419665,0.,0.341378619534878));
#40611=DIRECTION('',(0.,1.,0.));
#40612=DIRECTION('',(-0.939925868419665,0.,0.341378619534878));
#40613=DIRECTION('',(-0.939925868419665,0.,0.341378619534878));
#40614=DIRECTION('center_axis',(0.,1.,0.));
#40615=DIRECTION('ref_axis',(0.,0.,1.));
#40616=DIRECTION('',(0.,1.,0.));
#40617=DIRECTION('center_axis',(0.,1.,0.));
#40618=DIRECTION('ref_axis',(1.,0.,0.));
#40619=DIRECTION('center_axis',(0.,0.,1.));
#40620=DIRECTION('ref_axis',(1.,0.,0.));
#40621=DIRECTION('',(0.,1.,0.));
#40622=DIRECTION('',(-1.,0.,0.));
#40623=DIRECTION('',(-1.,0.,0.));
#40624=DIRECTION('center_axis',(1.,0.,0.));
#40625=DIRECTION('ref_axis',(0.,1.,0.));
#40626=DIRECTION('',(0.,1.,0.));
#40627=DIRECTION('',(0.,0.,-1.));
#40628=DIRECTION('center_axis',(0.,-1.,0.));
#40629=DIRECTION('ref_axis',(0.814642535600978,0.,0.579963394697984));
#40630=DIRECTION('',(0.,-1.,0.));
#40631=DIRECTION('center_axis',(0.,1.,0.));
#40632=DIRECTION('ref_axis',(1.,0.,0.));
#40633=DIRECTION('center_axis',(0.,1.,0.));
#40634=DIRECTION('ref_axis',(1.,0.,0.));
#40635=DIRECTION('center_axis',(0.,-1.,0.));
#40636=DIRECTION('ref_axis',(0.739062930406113,0.,-0.673636389233487));
#40637=DIRECTION('center_axis',(0.,-1.,0.));
#40638=DIRECTION('ref_axis',(1.,0.,0.));
#40639=DIRECTION('center_axis',(0.,1.,0.));
#40640=DIRECTION('ref_axis',(-0.739062931366045,0.,-0.673636388180322));
#40641=DIRECTION('',(0.,1.,0.));
#40642=DIRECTION('center_axis',(0.,1.,0.));
#40643=DIRECTION('ref_axis',(1.,0.,0.));
#40644=DIRECTION('center_axis',(0.,1.,0.));
#40645=DIRECTION('ref_axis',(-0.814642535600978,0.,0.579963394697984));
#40646=DIRECTION('center_axis',(0.,1.,0.));
#40647=DIRECTION('ref_axis',(1.,0.,0.));
#40648=DIRECTION('',(0.,1.,0.));
#40649=DIRECTION('center_axis',(1.,0.,0.));
#40650=DIRECTION('ref_axis',(0.,1.,0.));
#40651=DIRECTION('',(0.,1.,0.));
#40652=DIRECTION('center_axis',(0.,0.,1.));
#40653=DIRECTION('ref_axis',(1.,0.,0.));
#40654=DIRECTION('center_axis',(0.,-1.,0.));
#40655=DIRECTION('ref_axis',(-0.42050842009983,0.,0.907288635785297));
#40656=DIRECTION('',(0.,-1.,0.));
#40657=DIRECTION('center_axis',(0.,-1.,0.));
#40658=DIRECTION('ref_axis',(1.,0.,0.));
#40659=DIRECTION('',(0.,-1.,0.));
#40660=DIRECTION('center_axis',(-1.,0.,0.));
#40661=DIRECTION('ref_axis',(0.,0.,1.));
#40662=DIRECTION('',(0.,1.,0.));
#40663=DIRECTION('',(0.,0.,-1.));
#40664=DIRECTION('center_axis',(0.,1.,0.));
#40665=DIRECTION('ref_axis',(0.,0.,1.));
#40666=DIRECTION('',(0.,1.,0.));
#40667=DIRECTION('center_axis',(0.,1.,0.));
#40668=DIRECTION('ref_axis',(1.,0.,0.));
#40669=DIRECTION('center_axis',(0.,1.,0.));
#40670=DIRECTION('ref_axis',(1.,0.,0.));
#40671=DIRECTION('center_axis',(-0.341378619534878,0.,-0.939925868419665));
#40672=DIRECTION('ref_axis',(-0.939925868419665,0.,0.341378619534878));
#40673=DIRECTION('',(0.,1.,0.));
#40674=DIRECTION('',(-0.939925868419665,0.,0.341378619534878));
#40675=DIRECTION('',(-0.939925868419665,0.,0.341378619534878));
#40676=DIRECTION('center_axis',(1.,0.,0.));
#40677=DIRECTION('ref_axis',(0.,1.,0.));
#40678=DIRECTION('',(0.,1.,0.));
#40679=DIRECTION('',(0.,0.,-1.));
#40680=DIRECTION('center_axis',(0.,-1.,0.));
#40681=DIRECTION('ref_axis',(0.707106781186548,0.,-0.707106781186548));
#40682=DIRECTION('center_axis',(0.,-1.,0.));
#40683=DIRECTION('ref_axis',(1.,0.,0.));
#40684=DIRECTION('',(0.,-1.,0.));
#40685=DIRECTION('center_axis',(0.,-1.,0.));
#40686=DIRECTION('ref_axis',(1.,0.,0.));
#40687=DIRECTION('center_axis',(0.,1.,0.));
#40688=DIRECTION('ref_axis',(1.,0.,0.));
#40689=DIRECTION('',(0.,1.,0.));
#40690=DIRECTION('center_axis',(0.,-1.,0.));
#40691=DIRECTION('ref_axis',(1.,0.,0.));
#40692=DIRECTION('center_axis',(0.,-1.,0.));
#40693=DIRECTION('ref_axis',(1.,0.,0.));
#40694=DIRECTION('center_axis',(0.,-1.,0.));
#40695=DIRECTION('ref_axis',(1.,0.,0.));
#40696=DIRECTION('center_axis',(0.,-1.,0.));
#40697=DIRECTION('ref_axis',(1.,0.,0.));
#40698=DIRECTION('center_axis',(0.,1.,0.));
#40699=DIRECTION('ref_axis',(-2.83274710209661E-16,0.,1.));
#40700=DIRECTION('',(0.,1.,0.));
#40701=DIRECTION('center_axis',(0.,1.,0.));
#40702=DIRECTION('ref_axis',(1.,0.,0.));
#40703=DIRECTION('center_axis',(1.,0.,0.));
#40704=DIRECTION('ref_axis',(0.,1.,0.));
#40705=DIRECTION('',(0.,1.,0.));
#40706=DIRECTION('',(0.,0.,-1.));
#40707=DIRECTION('center_axis',(0.,1.,0.));
#40708=DIRECTION('ref_axis',(1.,0.,-1.73472347597681E-15));
#40709=DIRECTION('center_axis',(0.,-1.,0.));
#40710=DIRECTION('ref_axis',(1.,0.,0.));
#40711=DIRECTION('',(0.,1.,0.));
#40712=DIRECTION('center_axis',(0.,-1.,0.));
#40713=DIRECTION('ref_axis',(-0.785616163798045,0.,-0.618714185370954));
#40714=DIRECTION('center_axis',(0.,-1.,0.));
#40715=DIRECTION('ref_axis',(1.,0.,0.));
#40716=DIRECTION('',(0.,1.,0.));
#40717=DIRECTION('center_axis',(0.,1.,0.));
#40718=DIRECTION('ref_axis',(-0.974728984364045,0.,0.22339070491101));
#40719=DIRECTION('center_axis',(0.,-1.,0.));
#40720=DIRECTION('ref_axis',(1.,0.,0.));
#40721=DIRECTION('',(0.,1.,0.));
#40722=DIRECTION('center_axis',(0.,1.,0.));
#40723=DIRECTION('ref_axis',(-1.52656512918906E-15,0.,1.));
#40724=DIRECTION('center_axis',(0.,-1.,0.));
#40725=DIRECTION('ref_axis',(1.,0.,0.));
#40726=DIRECTION('',(0.,1.,0.));
#40727=DIRECTION('center_axis',(0.,1.,0.));
#40728=DIRECTION('ref_axis',(0.785616163798045,0.,-0.618714185370954));
#40729=DIRECTION('',(0.,1.,0.));
#40730=DIRECTION('center_axis',(0.,1.,0.));
#40731=DIRECTION('ref_axis',(1.,0.,0.));
#40732=DIRECTION('center_axis',(0.,-1.,0.));
#40733=DIRECTION('ref_axis',(-1.,0.,0.));
#40734=DIRECTION('center_axis',(0.,-1.,0.));
#40735=DIRECTION('ref_axis',(1.,0.,0.));
#40736=DIRECTION('',(0.,1.,0.));
#40737=DIRECTION('center_axis',(1.,0.,0.));
#40738=DIRECTION('ref_axis',(0.,1.,0.));
#40739=DIRECTION('',(0.,0.,-1.));
#40740=DIRECTION('center_axis',(0.,1.,0.));
#40741=DIRECTION('ref_axis',(-0.707106781186548,0.,-0.707106781186548));
#40742=DIRECTION('',(0.,1.,0.));
#40743=DIRECTION('center_axis',(0.,1.,0.));
#40744=DIRECTION('ref_axis',(1.,0.,0.));
#40745=DIRECTION('',(0.,-1.,0.));
#40746=DIRECTION('center_axis',(1.,0.,0.));
#40747=DIRECTION('ref_axis',(0.,1.,0.));
#40748=DIRECTION('',(0.,0.,-1.));
#40749=DIRECTION('',(0.,1.,0.));
#40750=DIRECTION('center_axis',(-0.341378619534878,0.,0.939925868419665));
#40751=DIRECTION('ref_axis',(0.,1.,0.));
#40752=DIRECTION('',(0.,1.,0.));
#40753=DIRECTION('',(0.939925868419665,0.,0.341378619534878));
#40754=DIRECTION('',(0.939925868419665,0.,0.341378619534878));
#40755=DIRECTION('center_axis',(0.,1.,0.));
#40756=DIRECTION('ref_axis',(0.,0.,1.));
#40757=DIRECTION('',(0.,1.,0.));
#40758=DIRECTION('center_axis',(0.,1.,0.));
#40759=DIRECTION('ref_axis',(1.,0.,0.));
#40760=DIRECTION('center_axis',(0.,1.,0.));
#40761=DIRECTION('ref_axis',(1.,0.,0.));
#40762=DIRECTION('center_axis',(-1.,0.,0.));
#40763=DIRECTION('ref_axis',(0.,0.,1.));
#40764=DIRECTION('',(0.,1.,0.));
#40765=DIRECTION('',(0.,0.,-1.));
#40766=DIRECTION('center_axis',(0.,1.,0.));
#40767=DIRECTION('ref_axis',(0.42050842009983,0.,0.907288635785297));
#40768=DIRECTION('center_axis',(0.,1.,0.));
#40769=DIRECTION('ref_axis',(1.,0.,0.));
#40770=DIRECTION('',(0.,-1.,0.));
#40771=DIRECTION('center_axis',(0.,1.,0.));
#40772=DIRECTION('ref_axis',(-1.,0.,0.));
#40773=DIRECTION('center_axis',(0.,1.,0.));
#40774=DIRECTION('ref_axis',(1.,0.,0.));
#40775=DIRECTION('center_axis',(0.,1.,0.));
#40776=DIRECTION('ref_axis',(1.,0.,0.));
#40777=DIRECTION('center_axis',(0.,1.,0.));
#40778=DIRECTION('ref_axis',(1.,0.,0.));
#40779=DIRECTION('center_axis',(0.,1.,0.));
#40780=DIRECTION('ref_axis',(1.,0.,0.));
#40781=DIRECTION('',(0.,-1.,0.));
#40782=DIRECTION('center_axis',(0.,-1.,0.));
#40783=DIRECTION('ref_axis',(1.,0.,0.));
#40784=DIRECTION('center_axis',(0.,-1.,0.));
#40785=DIRECTION('ref_axis',(1.,0.,0.));
#40786=DIRECTION('center_axis',(0.,1.,0.));
#40787=DIRECTION('ref_axis',(1.,0.,0.));
#40788=DIRECTION('center_axis',(0.,1.,0.));
#40789=DIRECTION('ref_axis',(1.,0.,0.));
#40790=DIRECTION('',(0.,0.,-1.));
#40791=DIRECTION('center_axis',(-1.,0.,0.));
#40792=DIRECTION('ref_axis',(0.,0.,1.));
#40793=DIRECTION('',(0.,0.,-1.));
#40794=DIRECTION('',(0.,-1.,0.));
#40795=DIRECTION('center_axis',(0.,0.,1.));
#40796=DIRECTION('ref_axis',(1.,0.,0.));
#40797=DIRECTION('',(0.,-1.,0.));
#40798=DIRECTION('',(-1.,0.,0.));
#40799=DIRECTION('',(0.,1.,0.));
#40800=DIRECTION('',(-1.,0.,0.));
#40801=DIRECTION('',(-1.,0.,0.));
#40802=DIRECTION('',(0.,1.,0.));
#40803=DIRECTION('',(-1.,0.,0.));
#40804=DIRECTION('center_axis',(0.,1.,0.));
#40805=DIRECTION('ref_axis',(1.,0.,0.));
#40806=DIRECTION('center_axis',(0.,1.,0.));
#40807=DIRECTION('ref_axis',(-0.989619470215645,0.,0.143712574850308));
#40808=DIRECTION('',(-1.,0.,0.));
#40809=DIRECTION('center_axis',(0.,0.,1.));
#40810=DIRECTION('ref_axis',(1.,0.,0.));
#40811=DIRECTION('',(-1.,0.,0.));
#40812=DIRECTION('',(0.,1.,0.));
#40813=DIRECTION('',(-1.,0.,0.));
#40814=DIRECTION('',(0.,1.,0.));
#40815=DIRECTION('',(-1.,0.,0.));
#40816=DIRECTION('',(0.,-1.,0.));
#40817=DIRECTION('center_axis',(-1.,0.,0.));
#40818=DIRECTION('ref_axis',(0.,0.,1.));
#40819=DIRECTION('',(0.,0.,-1.));
#40820=DIRECTION('',(0.,0.,-1.));
#40821=DIRECTION('',(0.,-1.,0.));
#40822=DIRECTION('center_axis',(0.,1.,0.));
#40823=DIRECTION('ref_axis',(1.,0.,0.));
#40824=DIRECTION('center_axis',(0.,1.,0.));
#40825=DIRECTION('ref_axis',(1.,0.,0.));
#40826=DIRECTION('',(0.,0.,-1.));
#40827=DIRECTION('center_axis',(-1.,0.,0.));
#40828=DIRECTION('ref_axis',(0.,0.,1.));
#40829=DIRECTION('',(0.,-1.,0.));
#40830=DIRECTION('',(0.,0.,-1.));
#40831=DIRECTION('center_axis',(0.,1.,0.));
#40832=DIRECTION('ref_axis',(1.,0.,0.));
#40833=DIRECTION('',(0.,0.,-1.));
#40834=DIRECTION('center_axis',(-1.,0.,0.));
#40835=DIRECTION('ref_axis',(0.,0.,1.));
#40836=DIRECTION('',(0.,-1.,0.));
#40837=DIRECTION('',(0.,0.,-1.));
#40838=DIRECTION('center_axis',(0.,0.,1.));
#40839=DIRECTION('ref_axis',(1.,0.,0.));
#40840=DIRECTION('',(-1.,0.,0.));
#40841=DIRECTION('',(0.,1.,0.));
#40842=DIRECTION('',(-1.,0.,0.));
#40843=DIRECTION('',(0.,-1.,0.));
#40844=DIRECTION('',(1.,0.,0.));
#40845=DIRECTION('',(0.,1.,0.));
#40846=DIRECTION('',(1.,0.,0.));
#40847=DIRECTION('center_axis',(0.,1.,0.));
#40848=DIRECTION('ref_axis',(1.,0.,0.));
#40849=DIRECTION('center_axis',(2.56173517218487E-14,-1.,0.));
#40850=DIRECTION('ref_axis',(0.989619470215645,2.526255984177E-14,0.143712574850308));
#40851=DIRECTION('',(1.,0.,0.));
#40852=DIRECTION('center_axis',(0.,0.,1.));
#40853=DIRECTION('ref_axis',(1.,0.,0.));
#40854=DIRECTION('',(0.,1.,0.));
#40855=DIRECTION('',(1.,0.,0.));
#40856=DIRECTION('',(0.,-1.,0.));
#40857=DIRECTION('',(-1.,0.,0.));
#40858=DIRECTION('',(0.,1.,0.));
#40859=DIRECTION('',(-1.,0.,0.));
#40860=DIRECTION('center_axis',(0.,1.,0.));
#40861=DIRECTION('ref_axis',(1.,0.,0.));
#40862=DIRECTION('',(0.,0.,-1.));
#40863=DIRECTION('',(0.,0.,-1.));
#40864=DIRECTION('center_axis',(0.,-1.,0.));
#40865=DIRECTION('ref_axis',(-7.00720136310847E-15,0.,-1.));
#40866=DIRECTION('center_axis',(0.,0.,-1.));
#40867=DIRECTION('ref_axis',(0.70710678118139,0.707106781191705,0.));
#40868=DIRECTION('center_axis',(0.,0.,-1.));
#40869=DIRECTION('ref_axis',(-0.70710678118139,0.707106781191705,0.));
#40870=DIRECTION('center_axis',(0.,1.,0.));
#40871=DIRECTION('ref_axis',(1.,0.,0.));
#40872=DIRECTION('',(0.,0.,-1.));
#40873=DIRECTION('center_axis',(0.,1.,0.));
#40874=DIRECTION('ref_axis',(1.,0.,0.));
#40875=DIRECTION('center_axis',(0.,1.,0.));
#40876=DIRECTION('ref_axis',(1.,0.,-8.24040019504512E-15));
#40877=DIRECTION('',(0.,0.,-1.));
#40878=DIRECTION('center_axis',(0.,1.,0.));
#40879=DIRECTION('ref_axis',(1.,0.,0.));
#40880=DIRECTION('center_axis',(0.,1.,0.));
#40881=DIRECTION('ref_axis',(1.,0.,0.));
#40882=DIRECTION('',(0.,0.,-1.));
#40883=DIRECTION('',(0.,0.,-1.));
#40884=DIRECTION('center_axis',(0.,1.,0.));
#40885=DIRECTION('ref_axis',(1.,0.,0.));
#40886=DIRECTION('center_axis',(0.,1.,0.));
#40887=DIRECTION('ref_axis',(1.,0.,0.));
#40888=DIRECTION('center_axis',(0.,1.,0.));
#40889=DIRECTION('ref_axis',(1.,0.,0.));
#40890=DIRECTION('center_axis',(0.,1.,0.));
#40891=DIRECTION('ref_axis',(0.974839739488413,0.,-0.222906891580687));
#40892=DIRECTION('center_axis',(0.,1.,0.));
#40893=DIRECTION('ref_axis',(1.,0.,0.));
#40894=DIRECTION('center_axis',(0.,1.,0.));
#40895=DIRECTION('ref_axis',(0.350308709237325,0.,0.936634298022702));
#40896=DIRECTION('center_axis',(0.,1.,0.));
#40897=DIRECTION('ref_axis',(1.,0.,0.));
#40898=DIRECTION('center_axis',(0.,1.,0.));
#40899=DIRECTION('ref_axis',(1.,0.,0.));
#40900=DIRECTION('',(0.,0.,-1.));
#40901=DIRECTION('center_axis',(0.,1.,0.));
#40902=DIRECTION('ref_axis',(0.949788039554192,0.,0.312894039444354));
#40903=DIRECTION('center_axis',(0.,1.,0.));
#40904=DIRECTION('ref_axis',(1.,0.,0.));
#40905=DIRECTION('center_axis',(0.,1.,0.));
#40906=DIRECTION('ref_axis',(0.662256581371297,0.,0.749277131928103));
#40907=DIRECTION('center_axis',(0.,1.,0.));
#40908=DIRECTION('ref_axis',(1.,0.,0.));
#40909=DIRECTION('center_axis',(0.,1.,0.));
#40910=DIRECTION('ref_axis',(1.,0.,7.89491928622333E-16));
#40911=DIRECTION('center_axis',(-9.86864910777917E-16,0.,1.));
#40912=DIRECTION('ref_axis',(-1.,0.,-9.86864910777917E-16));
#40913=DIRECTION('center_axis',(0.,1.,0.));
#40914=DIRECTION('ref_axis',(1.,0.,0.));
#40915=DIRECTION('center_axis',(0.,-1.,0.));
#40916=DIRECTION('ref_axis',(0.,0.,-1.));
#40917=DIRECTION('center_axis',(0.,-1.,0.));
#40918=DIRECTION('ref_axis',(1.,0.,0.));
#40919=DIRECTION('center_axis',(0.,1.,0.));
#40920=DIRECTION('ref_axis',(1.,0.,0.));
#40921=DIRECTION('center_axis',(0.,-1.,0.));
#40922=DIRECTION('ref_axis',(1.,0.,0.));
#40923=DIRECTION('center_axis',(0.,-1.,0.));
#40924=DIRECTION('ref_axis',(1.,0.,0.));
#40925=DIRECTION('center_axis',(0.,-1.,0.));
#40926=DIRECTION('ref_axis',(1.,0.,0.));
#40927=DIRECTION('',(0.,0.,-1.));
#40928=DIRECTION('center_axis',(0.,-1.,0.));
#40929=DIRECTION('ref_axis',(1.,0.,0.));
#40930=DIRECTION('center_axis',(0.,1.,0.));
#40931=DIRECTION('ref_axis',(1.,0.,0.));
#40932=DIRECTION('',(0.,0.,-1.));
#40933=DIRECTION('center_axis',(0.,1.,0.));
#40934=DIRECTION('ref_axis',(1.,0.,0.));
#40935=DIRECTION('center_axis',(0.,-1.,0.));
#40936=DIRECTION('ref_axis',(1.,0.,0.));
#40937=DIRECTION('center_axis',(0.,1.,0.));
#40938=DIRECTION('ref_axis',(1.,0.,0.));
#40939=DIRECTION('center_axis',(0.,1.,0.));
#40940=DIRECTION('ref_axis',(-0.662256581371391,0.,0.749277131928019));
#40941=DIRECTION('center_axis',(0.,1.,0.));
#40942=DIRECTION('ref_axis',(1.,0.,0.));
#40943=DIRECTION('',(0.,0.,-1.));
#40944=DIRECTION('center_axis',(0.,1.,0.));
#40945=DIRECTION('ref_axis',(0.949788039554207,0.,-0.312894039444309));
#40946=DIRECTION('center_axis',(0.,1.,0.));
#40947=DIRECTION('ref_axis',(1.,0.,0.));
#40948=DIRECTION('center_axis',(0.,1.,0.));
#40949=DIRECTION('ref_axis',(1.,0.,2.368475785867E-15));
#40950=DIRECTION('center_axis',(-1.97372982155583E-15,0.,1.));
#40951=DIRECTION('ref_axis',(-1.,0.,-1.97372982155583E-15));
#40952=DIRECTION('center_axis',(0.,-1.,0.));
#40953=DIRECTION('ref_axis',(1.,0.,0.));
#40954=DIRECTION('center_axis',(0.,0.,-1.));
#40955=DIRECTION('ref_axis',(-0.707106781186548,0.707106781186547,0.));
#40956=DIRECTION('',(0.,0.,-1.));
#40957=DIRECTION('center_axis',(0.,1.,0.));
#40958=DIRECTION('ref_axis',(0.,0.,1.));
#40959=DIRECTION('center_axis',(0.,-1.,0.));
#40960=DIRECTION('ref_axis',(1.,0.,0.));
#40961=DIRECTION('center_axis',(0.,-1.,0.));
#40962=DIRECTION('ref_axis',(1.,0.,0.));
#40963=DIRECTION('center_axis',(0.,1.,0.));
#40964=DIRECTION('ref_axis',(-1.,0.,0.));
#40965=DIRECTION('',(0.,1.,0.));
#40966=DIRECTION('center_axis',(0.,-1.,0.));
#40967=DIRECTION('ref_axis',(1.,0.,0.));
#40968=DIRECTION('center_axis',(0.,1.,0.));
#40969=DIRECTION('ref_axis',(1.,0.,0.));
#40970=DIRECTION('center_axis',(0.,-1.,0.));
#40971=DIRECTION('ref_axis',(0.720353042651791,0.,0.693607593630799));
#40972=DIRECTION('center_axis',(0.,-1.,0.));
#40973=DIRECTION('ref_axis',(1.,0.,0.));
#40974=DIRECTION('',(0.,-1.,0.));
#40975=DIRECTION('center_axis',(0.,1.,0.));
#40976=DIRECTION('ref_axis',(1.,0.,0.));
#40977=DIRECTION('',(0.,-1.,0.));
#40978=DIRECTION('center_axis',(0.,1.,0.));
#40979=DIRECTION('ref_axis',(-1.,0.,0.));
#40980=DIRECTION('',(0.,1.,0.));
#40981=DIRECTION('center_axis',(0.,1.,0.));
#40982=DIRECTION('ref_axis',(1.,0.,0.));
#40983=DIRECTION('',(0.,1.,0.));
#40984=DIRECTION('center_axis',(0.,-1.,0.));
#40985=DIRECTION('ref_axis',(1.,0.,0.));
#40986=DIRECTION('center_axis',(0.,1.,0.));
#40987=DIRECTION('ref_axis',(-1.,0.,0.));
#40988=DIRECTION('',(0.,1.,0.));
#40989=DIRECTION('center_axis',(0.,-1.,0.));
#40990=DIRECTION('ref_axis',(1.,0.,0.));
#40991=DIRECTION('',(0.,1.,0.));
#40992=DIRECTION('center_axis',(0.,1.,0.));
#40993=DIRECTION('ref_axis',(1.,0.,0.));
#40994=DIRECTION('center_axis',(0.,1.,0.));
#40995=DIRECTION('ref_axis',(-0.720353042651791,0.,0.693607593630799));
#40996=DIRECTION('center_axis',(0.,-1.,0.));
#40997=DIRECTION('ref_axis',(1.,0.,0.));
#40998=DIRECTION('',(0.,-1.,0.));
#40999=DIRECTION('center_axis',(0.,-1.,0.));
#41000=DIRECTION('ref_axis',(1.,0.,0.));
#41001=DIRECTION('',(0.,-1.,0.));
#41002=DIRECTION('center_axis',(0.,1.,0.));
#41003=DIRECTION('ref_axis',(-1.,0.,0.));
#41004=DIRECTION('',(0.,1.,0.));
#41005=DIRECTION('center_axis',(0.,1.,0.));
#41006=DIRECTION('ref_axis',(1.,0.,0.));
#41007=DIRECTION('center_axis',(0.,-1.,0.));
#41008=DIRECTION('ref_axis',(1.,0.,0.));
#41009=DIRECTION('center_axis',(1.,0.,0.));
#41010=DIRECTION('ref_axis',(0.,1.,0.));
#41011=DIRECTION('',(0.,0.,-1.));
#41012=DIRECTION('',(0.,0.,-1.));
#41013=DIRECTION('center_axis',(0.,1.,0.));
#41014=DIRECTION('ref_axis',(1.,0.,0.));
#41015=DIRECTION('center_axis',(0.,1.,0.));
#41016=DIRECTION('ref_axis',(1.,0.,0.));
#41017=DIRECTION('center_axis',(0.,1.,0.));
#41018=DIRECTION('ref_axis',(-1.,0.,-2.44929359829735E-16));
#41019=DIRECTION('center_axis',(0.,1.,0.));
#41020=DIRECTION('ref_axis',(1.,0.,0.));
#41021=DIRECTION('',(0.716064653815062,0.,0.698033961606966));
#41022=DIRECTION('center_axis',(0.,1.,0.));
#41023=DIRECTION('ref_axis',(-0.137277512281788,0.,-0.990532626732569));
#41024=DIRECTION('',(0.,0.,-1.));
#41025=DIRECTION('center_axis',(0.,-1.,0.));
#41026=DIRECTION('ref_axis',(-0.0324675324676818,0.,-0.999472790692903));
#41027=DIRECTION('center_axis',(0.,1.,0.));
#41028=DIRECTION('ref_axis',(1.,0.,0.));
#41029=DIRECTION('center_axis',(0.,-1.,0.));
#41030=DIRECTION('ref_axis',(-0.670496489123443,0.,-0.741912702461102));
#41031=DIRECTION('center_axis',(-5.55025254589126E-14,1.,2.83382379459511E-15));
#41032=DIRECTION('ref_axis',(-0.698033961645093,-4.44089209850066E-14,0.716064653777895));
#41033=DIRECTION('',(0.716064653810392,0.,0.698033961611757));
#41034=DIRECTION('',(0.71606465381051,0.,0.698033961611635));
#41035=DIRECTION('center_axis',(1.03196692270593E-15,1.,-5.46377092356529E-14));
#41036=DIRECTION('ref_axis',(-0.670496489136716,-4.44089209850059E-14,-0.741912702449107));
#41037=DIRECTION('center_axis',(0.,1.,0.));
#41038=DIRECTION('ref_axis',(1.,0.,0.));
#41039=DIRECTION('',(0.716064653808873,0.,0.698033961613315));
#41040=DIRECTION('center_axis',(0.,-1.,0.));
#41041=DIRECTION('ref_axis',(-0.818163015360923,0.,-0.574986330529276));
#41042=DIRECTION('',(-0.716064653796352,0.,0.69803396162616));
#41043=DIRECTION('center_axis',(0.,1.,0.));
#41044=DIRECTION('ref_axis',(-0.698033961628439,0.,-0.716064653794129));
#41045=DIRECTION('',(0.698033961547156,0.,0.716064653873366));
#41046=DIRECTION('center_axis',(0.,1.,0.));
#41047=DIRECTION('ref_axis',(0.716064653746231,0.,-0.698033961677575));
#41048=DIRECTION('',(-0.716064653813429,0.,0.698033961608642));
#41049=DIRECTION('center_axis',(-5.78811379739961E-14,1.,-3.92120274457636E-15));
#41050=DIRECTION('ref_axis',(-0.788233466082538,-4.44089209850063E-14,0.615376310031113));
#41051=DIRECTION('center_axis',(2.02347729834534E-15,1.,5.69830917539279E-14));
#41052=DIRECTION('ref_axis',(0.698033961510944,-4.44089209850061E-14,0.716064653908666));
#41053=DIRECTION('',(-0.716064653799089,0.,0.698033961623351));
#41054=DIRECTION('center_axis',(0.,1.,0.));
#41055=DIRECTION('ref_axis',(-0.698033961694648,0.,-0.716064653729587));
#41056=DIRECTION('',(0.698033961635916,0.,0.716064653786841));
#41057=DIRECTION('center_axis',(0.,1.,0.));
#41058=DIRECTION('ref_axis',(0.716064653777882,0.,-0.698033961645107));
#41059=DIRECTION('',(-0.716064653794199,0.,0.698033961628368));
#41060=DIRECTION('',(0.,0.,-1.));
#41061=DIRECTION('center_axis',(-3.40810699911546E-15,-1.,3.13651749681814E-15));
#41062=DIRECTION('ref_axis',(-0.999929890837095,3.15250835974135E-15,-0.0118411743723115));
#41063=DIRECTION('center_axis',(6.83821351836324E-14,1.,-8.83723547502582E-14));
#41064=DIRECTION('ref_axis',(-0.262414447485415,-8.88178419700126E-14,-0.964955262046342));
#41065=DIRECTION('center_axis',(0.,1.,0.));
#41066=DIRECTION('ref_axis',(-1.,0.,0.));
#41067=DIRECTION('',(0.,1.,0.));
#41068=DIRECTION('center_axis',(0.,1.,0.));
#41069=DIRECTION('ref_axis',(1.,0.,0.));
#41070=DIRECTION('center_axis',(0.,-1.,0.));
#41071=DIRECTION('ref_axis',(-0.720675546312773,0.,-0.693272498334375));
#41072=DIRECTION('',(0.,-1.,0.));
#41073=DIRECTION('center_axis',(0.,1.,0.));
#41074=DIRECTION('ref_axis',(1.,0.,0.));
#41075=DIRECTION('',(0.,-1.,0.));
#41076=DIRECTION('center_axis',(0.,1.,0.));
#41077=DIRECTION('ref_axis',(-1.,0.,0.));
#41078=DIRECTION('',(0.,1.,0.));
#41079=DIRECTION('',(0.,1.,0.));
#41080=DIRECTION('center_axis',(0.,1.,0.));
#41081=DIRECTION('ref_axis',(1.,0.,0.));
#41082=DIRECTION('center_axis',(0.,1.,0.));
#41083=DIRECTION('ref_axis',(-1.,0.,0.));
#41084=DIRECTION('',(0.,1.,0.));
#41085=DIRECTION('center_axis',(0.,1.,0.));
#41086=DIRECTION('ref_axis',(1.,0.,0.));
#41087=DIRECTION('',(0.,1.,0.));
#41088=DIRECTION('center_axis',(0.,-1.,0.));
#41089=DIRECTION('ref_axis',(1.,0.,0.));
#41090=DIRECTION('center_axis',(0.,1.,0.));
#41091=DIRECTION('ref_axis',(0.720675546312773,0.,-0.693272498334375));
#41092=DIRECTION('center_axis',(0.,-1.,0.));
#41093=DIRECTION('ref_axis',(1.,0.,0.));
#41094=DIRECTION('',(0.,-1.,0.));
#41095=DIRECTION('center_axis',(0.,-1.,0.));
#41096=DIRECTION('ref_axis',(1.,0.,0.));
#41097=DIRECTION('',(0.,-1.,0.));
#41098=DIRECTION('center_axis',(0.,1.,0.));
#41099=DIRECTION('ref_axis',(-1.,0.,0.));
#41100=DIRECTION('',(0.,1.,0.));
#41101=DIRECTION('center_axis',(0.,-1.,0.));
#41102=DIRECTION('ref_axis',(1.,0.,0.));
#41103=DIRECTION('center_axis',(0.,1.,0.));
#41104=DIRECTION('ref_axis',(1.,0.,0.));
#41105=DIRECTION('center_axis',(0.,1.,0.));
#41106=DIRECTION('ref_axis',(1.22464679914735E-16,0.,-1.));
#41107=DIRECTION('center_axis',(0.,-1.,0.));
#41108=DIRECTION('ref_axis',(1.,0.,0.));
#41109=DIRECTION('center_axis',(0.,1.,0.));
#41110=DIRECTION('ref_axis',(1.,0.,0.));
#41111=DIRECTION('',(0.,0.,-1.));
#41112=DIRECTION('center_axis',(0.,0.,-1.));
#41113=DIRECTION('ref_axis',(0.707106781186548,0.707106781186548,0.));
#41114=DIRECTION('center_axis',(0.,-1.,0.));
#41115=DIRECTION('ref_axis',(1.,0.,-2.44929359829735E-16));
#41116=DIRECTION('center_axis',(0.,-1.,0.));
#41117=DIRECTION('ref_axis',(1.,0.,0.));
#41118=DIRECTION('center_axis',(0.,1.,0.));
#41119=DIRECTION('ref_axis',(1.,0.,0.));
#41120=DIRECTION('',(0.,0.,-1.));
#41121=DIRECTION('center_axis',(1.,0.,0.));
#41122=DIRECTION('ref_axis',(0.,1.,0.));
#41123=DIRECTION('',(0.,0.,-1.));
#41124=DIRECTION('center_axis',(0.,1.,0.));
#41125=DIRECTION('ref_axis',(1.,0.,0.));
#41126=DIRECTION('',(0.,0.,-1.));
#41127=DIRECTION('center_axis',(0.,1.,0.));
#41128=DIRECTION('ref_axis',(0.0462962962962933,0.,-0.998927751616325));
#41129=DIRECTION('',(-0.716064653815062,0.,0.698033961606966));
#41130=DIRECTION('center_axis',(0.,1.,0.));
#41131=DIRECTION('ref_axis',(1.,0.,0.));
#41132=DIRECTION('',(-0.716064653810392,0.,0.698033961611757));
#41133=DIRECTION('center_axis',(5.55025254589126E-14,1.,2.83382379459511E-15));
#41134=DIRECTION('ref_axis',(0.767334963166091,-4.44089209850066E-14,-0.64124648482693));
#41135=DIRECTION('center_axis',(-1.03196692270593E-15,1.,-5.46377092356529E-14));
#41136=DIRECTION('ref_axis',(-0.698033961459682,-4.44089209850059E-14,-0.716064653958638));
#41137=DIRECTION('',(-0.71606465381051,0.,0.698033961611635));
#41138=DIRECTION('center_axis',(0.,1.,0.));
#41139=DIRECTION('ref_axis',(1.,0.,0.));
#41140=DIRECTION('center_axis',(5.55025254589126E-14,1.,-2.83382379459511E-15));
#41141=DIRECTION('ref_axis',(0.698033961645093,-4.44089209850066E-14,-0.716064653777895));
#41142=DIRECTION('',(0.716064653788584,0.,0.698033961634128));
#41143=DIRECTION('center_axis',(0.,1.,0.));
#41144=DIRECTION('ref_axis',(-0.698033961474199,0.,0.716064653944486));
#41145=DIRECTION('',(-0.698033961547149,0.,0.716064653873372));
#41146=DIRECTION('center_axis',(0.,1.,0.));
#41147=DIRECTION('ref_axis',(-0.716064653908654,0.,-0.698033961510957));
#41148=DIRECTION('',(0.716064653792681,0.,0.698033961629925));
#41149=DIRECTION('',(-0.716064653808873,0.,0.698033961613315));
#41150=DIRECTION('center_axis',(0.,-1.,0.));
#41151=DIRECTION('ref_axis',(0.262414447485428,0.,-0.964955262046338));
#41152=DIRECTION('center_axis',(0.,1.,0.));
#41153=DIRECTION('ref_axis',(0.999929890837095,0.,-0.0118411743723112));
#41154=DIRECTION('',(0.,0.,-1.));
#41155=DIRECTION('',(0.716064653815542,0.,0.698033961606474));
#41156=DIRECTION('center_axis',(0.,1.,0.));
#41157=DIRECTION('ref_axis',(-0.698033961677567,0.,0.716064653746239));
#41158=DIRECTION('',(-0.698033961510961,0.,0.71606465390865));
#41159=DIRECTION('center_axis',(0.,1.,0.));
#41160=DIRECTION('ref_axis',(-0.716064653794122,0.,-0.698033961628447));
#41161=DIRECTION('',(0.716064653808028,0.,0.698033961614182));
#41162=DIRECTION('center_axis',(-1.03196692270593E-15,1.,5.46377092356529E-14));
#41163=DIRECTION('ref_axis',(0.670496489136716,-4.44089209850059E-14,0.741912702449107));
#41164=DIRECTION('center_axis',(0.,1.,0.));
#41165=DIRECTION('ref_axis',(1.,0.,0.));
#41166=DIRECTION('center_axis',(0.,1.,0.));
#41167=DIRECTION('ref_axis',(-1.,0.,0.));
#41168=DIRECTION('center_axis',(0.,1.,0.));
#41169=DIRECTION('ref_axis',(1.,0.,8.67361737988404E-16));
#41170=DIRECTION('',(0.,1.,0.));
#41171=DIRECTION('center_axis',(0.,1.,0.));
#41172=DIRECTION('ref_axis',(1.,0.,0.));
#41173=DIRECTION('',(0.,1.,0.));
#41174=DIRECTION('center_axis',(0.,1.,0.));
#41175=DIRECTION('ref_axis',(-0.993447607883928,0.,0.114288452564992));
#41176=DIRECTION('center_axis',(0.,-1.,0.));
#41177=DIRECTION('ref_axis',(1.,0.,0.));
#41178=DIRECTION('',(0.,1.,0.));
#41179=DIRECTION('center_axis',(0.,-1.,0.));
#41180=DIRECTION('ref_axis',(-0.97470054788071,0.,-0.223514746629933));
#41181=DIRECTION('center_axis',(0.,1.,0.));
#41182=DIRECTION('ref_axis',(1.,0.,0.));
#41183=DIRECTION('',(0.,1.,0.));
#41184=DIRECTION('center_axis',(0.,-1.,0.));
#41185=DIRECTION('ref_axis',(0.993447607883928,0.,0.114288452564992));
#41186=DIRECTION('',(0.,1.,0.));
#41187=DIRECTION('center_axis',(0.,1.,0.));
#41188=DIRECTION('ref_axis',(1.,0.,0.));
#41189=DIRECTION('center_axis',(0.,-1.,0.));
#41190=DIRECTION('ref_axis',(-1.,0.,0.));
#41191=DIRECTION('center_axis',(0.,1.,0.));
#41192=DIRECTION('ref_axis',(1.,0.,0.));
#41193=DIRECTION('',(0.,1.,0.));
#41194=DIRECTION('center_axis',(1.,0.,0.));
#41195=DIRECTION('ref_axis',(0.,1.,0.));
#41196=DIRECTION('',(0.,0.,-1.));
#41197=DIRECTION('',(0.,1.,0.));
#41198=DIRECTION('center_axis',(0.,-1.,0.));
#41199=DIRECTION('ref_axis',(2.83273781220225E-16,0.,1.));
#41200=DIRECTION('center_axis',(0.,-1.,0.));
#41201=DIRECTION('ref_axis',(1.,0.,0.));
#41202=DIRECTION('',(0.,1.,0.));
#41203=DIRECTION('center_axis',(0.,1.,0.));
#41204=DIRECTION('ref_axis',(-2.83273781220225E-16,0.,1.));
#41205=DIRECTION('center_axis',(0.,1.,0.));
#41206=DIRECTION('ref_axis',(1.,0.,0.));
#41207=DIRECTION('',(0.,1.,0.));
#41208=DIRECTION('center_axis',(1.,0.,0.));
#41209=DIRECTION('ref_axis',(0.,1.,0.));
#41210=DIRECTION('',(0.,0.,-1.));
#41211=DIRECTION('center_axis',(0.,1.,0.));
#41212=DIRECTION('ref_axis',(-1.,0.,0.));
#41213=DIRECTION('',(0.,-1.,0.));
#41214=DIRECTION('center_axis',(0.,1.,0.));
#41215=DIRECTION('ref_axis',(1.,0.,0.));
#41216=DIRECTION('center_axis',(0.,-1.,0.));
#41217=DIRECTION('ref_axis',(1.,0.,0.));
#41218=DIRECTION('center_axis',(0.,-1.,0.));
#41219=DIRECTION('ref_axis',(1.,0.,0.));
#41220=DIRECTION('',(0.,1.,0.));
#41221=DIRECTION('center_axis',(0.,1.,0.));
#41222=DIRECTION('ref_axis',(1.,0.,0.));
#41223=DIRECTION('center_axis',(0.,-1.,0.));
#41224=DIRECTION('ref_axis',(-1.,0.,0.));
#41225=DIRECTION('center_axis',(0.,-1.,0.));
#41226=DIRECTION('ref_axis',(-5.9077376355796E-5,0.,0.999999998254932));
#41227=DIRECTION('center_axis',(0.,-1.,0.));
#41228=DIRECTION('ref_axis',(1.,0.,0.));
#41229=DIRECTION('',(0.,1.,0.));
#41230=DIRECTION('',(0.,1.,0.));
#41231=DIRECTION('center_axis',(0.,1.,0.));
#41232=DIRECTION('ref_axis',(0.999929890837101,0.,0.011841174371802));
#41233=DIRECTION('center_axis',(0.,-1.,0.));
#41234=DIRECTION('ref_axis',(1.,0.,0.));
#41235=DIRECTION('',(0.,1.,0.));
#41236=DIRECTION('',(0.,1.,0.));
#41237=DIRECTION('',(0.,1.,0.));
#41238=DIRECTION('',(0.,1.,0.));
#41239=DIRECTION('',(0.,1.,0.));
#41240=DIRECTION('',(0.,1.,0.));
#41241=DIRECTION('',(0.,1.,0.));
#41242=DIRECTION('',(0.,1.,0.));
#41243=DIRECTION('center_axis',(0.,1.,0.));
#41244=DIRECTION('ref_axis',(0.137277512281937,0.,-0.990532626732549));
#41245=DIRECTION('center_axis',(0.,-1.,0.));
#41246=DIRECTION('ref_axis',(1.,0.,0.));
#41247=DIRECTION('',(0.,1.,0.));
#41248=DIRECTION('center_axis',(0.,1.,0.));
#41249=DIRECTION('ref_axis',(0.137277512281937,0.,-0.990532626732549));
#41250=DIRECTION('center_axis',(0.,-1.,0.));
#41251=DIRECTION('ref_axis',(1.,0.,0.));
#41252=DIRECTION('',(0.,1.,0.));
#41253=DIRECTION('',(0.,1.,0.));
#41254=DIRECTION('',(0.,1.,0.));
#41255=DIRECTION('',(0.,1.,0.));
#41256=DIRECTION('',(0.,1.,0.));
#41257=DIRECTION('',(0.,1.,0.));
#41258=DIRECTION('',(0.,1.,0.));
#41259=DIRECTION('',(0.,1.,0.));
#41260=DIRECTION('',(0.,-1.,0.));
#41261=DIRECTION('center_axis',(0.,-1.,0.));
#41262=DIRECTION('ref_axis',(-0.999929890837101,0.,0.011841174371802));
#41263=DIRECTION('center_axis',(0.,-1.,0.));
#41264=DIRECTION('ref_axis',(1.,0.,0.));
#41265=DIRECTION('',(0.,-1.,0.));
#41266=DIRECTION('center_axis',(0.,1.,0.));
#41267=DIRECTION('ref_axis',(5.9077376355796E-5,0.,0.999999998254932));
#41268=DIRECTION('center_axis',(0.,1.,0.));
#41269=DIRECTION('ref_axis',(1.,0.,0.));
#41270=DIRECTION('',(0.,1.,0.));
#41271=DIRECTION('center_axis',(0.,-1.,0.));
#41272=DIRECTION('ref_axis',(1.,0.,0.));
#41273=DIRECTION('center_axis',(0.,-1.,0.));
#41274=DIRECTION('ref_axis',(1.,0.,0.));
#41275=DIRECTION('',(0.,-1.,0.));
#41276=DIRECTION('center_axis',(0.,1.,0.));
#41277=DIRECTION('ref_axis',(1.,0.,0.));
#41278=DIRECTION('center_axis',(0.,1.,0.));
#41279=DIRECTION('ref_axis',(1.,0.,0.));
#41280=DIRECTION('',(0.,0.,1.));
#41281=DIRECTION('center_axis',(0.,1.,0.));
#41282=DIRECTION('ref_axis',(1.,0.,0.));
#41283=DIRECTION('center_axis',(0.,-1.,0.));
#41284=DIRECTION('ref_axis',(1.,0.,0.));
#41285=DIRECTION('',(0.,0.,1.));
#41286=DIRECTION('center_axis',(0.,1.,0.));
#41287=DIRECTION('ref_axis',(1.,0.,0.));
#41288=DIRECTION('center_axis',(0.,1.,0.));
#41289=DIRECTION('ref_axis',(1.,0.,0.));
#41290=DIRECTION('center_axis',(0.,1.,0.));
#41291=DIRECTION('ref_axis',(1.,0.,0.));
#41292=DIRECTION('center_axis',(0.,-1.,0.));
#41293=DIRECTION('ref_axis',(1.,0.,0.));
#41294=DIRECTION('center_axis',(0.,1.,0.));
#41295=DIRECTION('ref_axis',(-1.,0.,0.));
#41296=DIRECTION('',(0.,1.,0.));
#41297=DIRECTION('center_axis',(0.,1.,0.));
#41298=DIRECTION('ref_axis',(1.,0.,0.));
#41299=DIRECTION('center_axis',(0.,-1.,0.));
#41300=DIRECTION('ref_axis',(0.,0.,-1.));
#41301=DIRECTION('center_axis',(0.,-1.,0.));
#41302=DIRECTION('ref_axis',(6.12267139103014E-17,0.,1.));
#41303=DIRECTION('',(0.,1.,0.));
#41304=DIRECTION('center_axis',(0.,1.,0.));
#41305=DIRECTION('ref_axis',(1.,0.,0.));
#41306=DIRECTION('center_axis',(0.,1.,0.));
#41307=DIRECTION('ref_axis',(1.,0.,0.));
#41308=DIRECTION('center_axis',(1.,0.,0.));
#41309=DIRECTION('ref_axis',(0.,1.,0.));
#41310=DIRECTION('',(0.,0.,1.));
#41311=DIRECTION('',(0.,0.,1.));
#41312=DIRECTION('',(0.,1.,0.));
#41313=DIRECTION('center_axis',(0.,1.,0.));
#41314=DIRECTION('ref_axis',(-0.934587360002009,0.,0.355733701699003));
#41315=DIRECTION('center_axis',(0.,1.,0.));
#41316=DIRECTION('ref_axis',(1.,0.,0.));
#41317=DIRECTION('center_axis',(0.,1.,0.));
#41318=DIRECTION('ref_axis',(1.,0.,0.));
#41319=DIRECTION('',(0.,1.,0.));
#41320=DIRECTION('center_axis',(0.,-1.,0.));
#41321=DIRECTION('ref_axis',(0.934587360002009,0.,0.355733701699003));
#41322=DIRECTION('center_axis',(0.,-1.,0.));
#41323=DIRECTION('ref_axis',(1.,0.,0.));
#41324=DIRECTION('center_axis',(0.,-1.,0.));
#41325=DIRECTION('ref_axis',(1.,0.,0.));
#41326=DIRECTION('',(0.,1.,0.));
#41327=DIRECTION('center_axis',(1.,0.,0.));
#41328=DIRECTION('ref_axis',(0.,1.,0.));
#41329=DIRECTION('',(0.,0.,1.));
#41330=DIRECTION('',(1.90171128996581E-6,0.,0.999999999998192));
#41331=DIRECTION('',(0.,0.,1.));
#41332=DIRECTION('center_axis',(0.,1.,0.));
#41333=DIRECTION('ref_axis',(-1.,0.,0.));
#41334=DIRECTION('',(0.,1.,0.));
#41335=DIRECTION('center_axis',(0.,-1.,0.));
#41336=DIRECTION('ref_axis',(1.,0.,0.));
#41337=DIRECTION('center_axis',(0.,-1.,0.));
#41338=DIRECTION('ref_axis',(1.,0.,0.));
#41339=DIRECTION('center_axis',(0.,-1.,0.));
#41340=DIRECTION('ref_axis',(1.,0.,0.));
#41341=DIRECTION('center_axis',(0.,-1.,0.));
#41342=DIRECTION('ref_axis',(1.,0.,0.));
#41343=DIRECTION('center_axis',(0.,-1.,0.));
#41344=DIRECTION('ref_axis',(1.,0.,0.));
#41345=DIRECTION('center_axis',(0.,-1.,0.));
#41346=DIRECTION('ref_axis',(1.,0.,0.));
#41347=DIRECTION('center_axis',(0.,-1.,0.));
#41348=DIRECTION('ref_axis',(1.,0.,0.));
#41349=DIRECTION('center_axis',(0.,-1.,0.));
#41350=DIRECTION('ref_axis',(1.,0.,0.));
#41351=DIRECTION('center_axis',(0.,1.,0.));
#41352=DIRECTION('ref_axis',(1.,0.,0.));
#41353=DIRECTION('',(0.,-1.,0.));
#41354=DIRECTION('center_axis',(0.,1.,0.));
#41355=DIRECTION('ref_axis',(1.,0.,0.));
#41356=DIRECTION('center_axis',(0.,1.,0.));
#41357=DIRECTION('ref_axis',(1.,0.,0.));
#41358=DIRECTION('center_axis',(0.,1.,0.));
#41359=DIRECTION('ref_axis',(1.,0.,0.));
#41360=DIRECTION('center_axis',(0.,1.,0.));
#41361=DIRECTION('ref_axis',(1.,0.,0.));
#41362=DIRECTION('center_axis',(0.,1.,0.));
#41363=DIRECTION('ref_axis',(1.,0.,0.));
#41364=DIRECTION('center_axis',(0.,1.,0.));
#41365=DIRECTION('ref_axis',(1.,0.,0.));
#41366=DIRECTION('center_axis',(0.,-1.,0.));
#41367=DIRECTION('ref_axis',(0.,0.,-1.));
#41368=DIRECTION('center_axis',(0.,-1.,0.));
#41369=DIRECTION('ref_axis',(-6.66472423784048E-5,0.,0.999999997779073));
#41370=DIRECTION('center_axis',(0.,-1.,0.));
#41371=DIRECTION('ref_axis',(1.,0.,0.));
#41372=DIRECTION('',(0.,1.,0.));
#41373=DIRECTION('center_axis',(0.,-1.,0.));
#41374=DIRECTION('ref_axis',(1.,0.,0.));
#41375=DIRECTION('',(0.,-1.,0.));
#41376=DIRECTION('center_axis',(0.,-1.,0.));
#41377=DIRECTION('ref_axis',(-0.55530622998795,0.,-0.831645952876926));
#41378=DIRECTION('',(0.,-1.,0.));
#41379=DIRECTION('center_axis',(0.,-1.,0.));
#41380=DIRECTION('ref_axis',(1.,0.,0.));
#41381=DIRECTION('center_axis',(0.,-1.,0.));
#41382=DIRECTION('ref_axis',(1.,0.,0.));
#41383=DIRECTION('',(0.,1.,0.));
#41384=DIRECTION('',(0.,1.,0.));
#41385=DIRECTION('',(0.,-1.,0.));
#41386=DIRECTION('center_axis',(0.,-1.,0.));
#41387=DIRECTION('ref_axis',(-0.138699292007931,0.,-0.990334542665507));
#41388=DIRECTION('center_axis',(0.,-1.,0.));
#41389=DIRECTION('ref_axis',(1.,0.,0.));
#41390=DIRECTION('center_axis',(0.,-1.,0.));
#41391=DIRECTION('ref_axis',(1.,0.,0.));
#41392=DIRECTION('',(0.,-1.,0.));
#41393=DIRECTION('',(0.,1.,0.));
#41394=DIRECTION('',(0.,1.,0.));
#41395=DIRECTION('',(0.,1.,0.));
#41396=DIRECTION('center_axis',(0.,1.,0.));
#41397=DIRECTION('ref_axis',(0.55530622998795,0.,-0.831645952876926));
#41398=DIRECTION('',(0.,1.,0.));
#41399=DIRECTION('center_axis',(0.,-1.,0.));
#41400=DIRECTION('ref_axis',(1.,0.,0.));
#41401=DIRECTION('center_axis',(0.,1.,0.));
#41402=DIRECTION('ref_axis',(1.,0.,0.));
#41403=DIRECTION('center_axis',(0.,1.,0.));
#41404=DIRECTION('ref_axis',(6.66472423784048E-5,0.,0.999999997779073));
#41405=DIRECTION('center_axis',(0.,1.,0.));
#41406=DIRECTION('ref_axis',(1.,0.,0.));
#41407=DIRECTION('center_axis',(0.,1.,0.));
#41408=DIRECTION('ref_axis',(1.,0.,0.));
#41409=DIRECTION('center_axis',(0.,1.,0.));
#41410=DIRECTION('ref_axis',(1.,0.,0.));
#41411=DIRECTION('center_axis',(0.,-1.,0.));
#41412=DIRECTION('ref_axis',(0.358624086674959,0.,-0.933482064346472));
#41413=DIRECTION('center_axis',(0.,1.,0.));
#41414=DIRECTION('ref_axis',(0.365247039092674,0.,0.930910629670773));
#41415=DIRECTION('center_axis',(0.,1.,0.));
#41416=DIRECTION('ref_axis',(1.,0.,0.));
#41417=DIRECTION('center_axis',(0.,-1.,0.));
#41418=DIRECTION('ref_axis',(-0.999436570354898,0.,0.033563996145276));
#41419=DIRECTION('center_axis',(-4.94340750637177E-15,1.,-5.11172940430608E-15));
#41420=DIRECTION('ref_axis',(0.999436570354898,4.99714829851786E-15,0.0335639961452762));
#41421=DIRECTION('center_axis',(0.,1.,0.));
#41422=DIRECTION('ref_axis',(1.,0.,0.));
#41423=DIRECTION('',(0.,-1.,0.));
#41424=DIRECTION('',(0.,-1.,0.));
#41425=DIRECTION('center_axis',(0.,1.,0.));
#41426=DIRECTION('ref_axis',(1.,0.,0.));
#41427=DIRECTION('center_axis',(0.,-1.,0.));
#41428=DIRECTION('ref_axis',(1.,0.,0.));
#41429=DIRECTION('center_axis',(0.,1.,0.));
#41430=DIRECTION('ref_axis',(1.,0.,0.));
#41431=DIRECTION('',(0.,-1.,0.));
#41432=DIRECTION('',(0.,-1.,0.));
#41433=DIRECTION('center_axis',(0.,1.,0.));
#41434=DIRECTION('ref_axis',(1.,0.,0.));
#41435=DIRECTION('center_axis',(1.50992280148742E-14,1.,-9.75211599539184E-15));
#41436=DIRECTION('ref_axis',(0.722348824225048,-1.76507793442358E-14,-0.691528868624217));
#41437=DIRECTION('center_axis',(0.,1.,0.));
#41438=DIRECTION('ref_axis',(-0.373228907029859,0.,0.927739286091355));
#41439=DIRECTION('center_axis',(0.,1.,0.));
#41440=DIRECTION('ref_axis',(0.731786637712586,0.,0.681533797302311));
#41441=DIRECTION('center_axis',(0.,1.,0.));
#41442=DIRECTION('ref_axis',(1.,0.,0.));
#41443=DIRECTION('center_axis',(0.,1.,0.));
#41444=DIRECTION('ref_axis',(1.,0.,0.));
#41445=DIRECTION('center_axis',(0.,-1.,0.));
#41446=DIRECTION('ref_axis',(0.188519518005548,0.,-0.982069443232481));
#41447=DIRECTION('center_axis',(0.,1.,0.));
#41448=DIRECTION('ref_axis',(1.,0.,0.));
#41449=DIRECTION('center_axis',(0.,1.,0.));
#41450=DIRECTION('ref_axis',(1.,0.,0.));
#41451=DIRECTION('center_axis',(0.,1.,0.));
#41452=DIRECTION('ref_axis',(1.,0.,0.));
#41453=DIRECTION('',(0.,0.,-1.));
#41454=DIRECTION('center_axis',(0.,1.,0.));
#41455=DIRECTION('ref_axis',(1.,0.,0.));
#41456=DIRECTION('center_axis',(7.97796769687341E-14,1.,-1.47631083777498E-13));
#41457=DIRECTION('ref_axis',(0.82647940397254,-1.49047681880818E-13,-0.562966957120215));
#41458=DIRECTION('center_axis',(0.,1.,0.));
#41459=DIRECTION('ref_axis',(1.,0.,0.));
#41460=DIRECTION('center_axis',(0.,1.,0.));
#41461=DIRECTION('ref_axis',(1.,0.,0.));
#41462=DIRECTION('center_axis',(7.97796769693144E-14,-1.,1.47631083778477E-13));
#41463=DIRECTION('ref_axis',(0.826479404012423,1.49047681876387E-13,0.562966957061665));
#41464=DIRECTION('center_axis',(0.,-1.,0.));
#41465=DIRECTION('ref_axis',(1.,0.,0.));
#41466=DIRECTION('',(0.,0.,-1.));
#41467=DIRECTION('center_axis',(0.,-1.,0.));
#41468=DIRECTION('ref_axis',(1.,0.,0.));
#41469=DIRECTION('center_axis',(0.,1.,0.));
#41470=DIRECTION('ref_axis',(1.,0.,0.));
#41471=DIRECTION('center_axis',(0.,-1.,0.));
#41472=DIRECTION('ref_axis',(0.373228907029852,0.,0.927739286091358));
#41473=DIRECTION('center_axis',(1.50992280148742E-14,-1.,9.75211599539184E-15));
#41474=DIRECTION('ref_axis',(0.722348824225048,1.76507793442358E-14,0.691528868624217));
#41475=DIRECTION('center_axis',(0.,-1.,0.));
#41476=DIRECTION('ref_axis',(0.731786637488438,0.,-0.681533797542987));
#41477=DIRECTION('center_axis',(0.,1.,0.));
#41478=DIRECTION('ref_axis',(1.,0.,0.));
#41479=DIRECTION('center_axis',(0.,1.,0.));
#41480=DIRECTION('ref_axis',(1.,0.,0.));
#41481=DIRECTION('center_axis',(0.,1.,0.));
#41482=DIRECTION('ref_axis',(0.188519616822252,0.,0.982069424263474));
#41483=DIRECTION('center_axis',(0.,1.,0.));
#41484=DIRECTION('ref_axis',(1.,0.,0.));
#41485=DIRECTION('center_axis',(0.,1.,0.));
#41486=DIRECTION('ref_axis',(0.196635535421533,0.,-0.980476652557055));
#41487=DIRECTION('center_axis',(0.,-1.,0.));
#41488=DIRECTION('ref_axis',(-1.,0.,1.11022302462516E-15));
#41489=DIRECTION('',(0.,0.,-1.));
#41490=DIRECTION('center_axis',(0.,1.,0.));
#41491=DIRECTION('ref_axis',(-0.999983860839812,0.,-0.00568137834545477));
#41492=DIRECTION('center_axis',(0.,-1.,0.));
#41493=DIRECTION('ref_axis',(0.182889314799161,0.,-0.983133510024093));
#41494=DIRECTION('center_axis',(0.,1.,0.));
#41495=DIRECTION('ref_axis',(-0.201763361402965,0.,-0.979434298968224));
#41496=DIRECTION('center_axis',(0.,1.,0.));
#41497=DIRECTION('ref_axis',(0.999436570354936,0.,0.0335639961441162));
#41498=DIRECTION('center_axis',(0.,-1.,0.));
#41499=DIRECTION('ref_axis',(-0.999436570354936,0.,0.0335639961441164));
#41500=DIRECTION('center_axis',(0.,1.,0.));
#41501=DIRECTION('ref_axis',(0.18615784526743,0.,0.98251985050959));
#41502=DIRECTION('center_axis',(0.,-1.,0.));
#41503=DIRECTION('ref_axis',(0.999983860839812,0.,-0.00568137834545072));
#41504=DIRECTION('',(0.,0.,-1.));
#41505=DIRECTION('center_axis',(0.,1.,0.));
#41506=DIRECTION('ref_axis',(1.,0.,0.));
#41507=DIRECTION('center_axis',(0.,-1.,0.));
#41508=DIRECTION('ref_axis',(-0.196635535421533,0.,-0.980476652557055));
#41509=DIRECTION('center_axis',(0.,1.,0.));
#41510=DIRECTION('ref_axis',(9.36455599968238E-5,0.,0.999999995615255));
#41511=DIRECTION('center_axis',(0.,1.,0.));
#41512=DIRECTION('ref_axis',(1.,0.,0.));
#41513=DIRECTION('',(0.,-1.,0.));
#41514=DIRECTION('center_axis',(0.,-1.,0.));
#41515=DIRECTION('ref_axis',(-9.36455599961238E-5,0.,0.999999995615255));
#41516=DIRECTION('center_axis',(0.,-1.,0.));
#41517=DIRECTION('ref_axis',(1.,0.,0.));
#41518=DIRECTION('',(0.,-1.,0.));
#41519=DIRECTION('center_axis',(0.,1.,0.));
#41520=DIRECTION('ref_axis',(1.,0.,0.));
#41521=DIRECTION('center_axis',(0.,-1.,0.));
#41522=DIRECTION('ref_axis',(1.,0.,0.));
#41523=DIRECTION('center_axis',(0.,1.,0.));
#41524=DIRECTION('ref_axis',(1.,0.,0.));
#41525=DIRECTION('center_axis',(0.,-1.,0.));
#41526=DIRECTION('ref_axis',(1.,0.,0.));
#41527=DIRECTION('center_axis',(0.,-1.,0.));
#41528=DIRECTION('ref_axis',(1.,0.,0.));
#41529=DIRECTION('center_axis',(0.,-1.,0.));
#41530=DIRECTION('ref_axis',(-0.257358836141954,0.,-0.966315905622824));
#41531=DIRECTION('',(0.,-1.,0.));
#41532=DIRECTION('',(0.,-1.,0.));
#41533=DIRECTION('',(0.,-1.,0.));
#41534=DIRECTION('center_axis',(0.,1.,0.));
#41535=DIRECTION('ref_axis',(-0.898888448298522,0.,0.438177541089767));
#41536=DIRECTION('center_axis',(0.,1.,0.));
#41537=DIRECTION('ref_axis',(1.,0.,0.));
#41538=DIRECTION('',(0.,-1.,0.));
#41539=DIRECTION('',(0.,-1.,0.));
#41540=DIRECTION('',(0.,-1.,0.));
#41541=DIRECTION('',(0.,-1.,0.));
#41542=DIRECTION('',(0.,-1.,0.));
#41543=DIRECTION('',(0.,-1.,0.));
#41544=DIRECTION('center_axis',(0.,1.,0.));
#41545=DIRECTION('ref_axis',(0.17719394991793,0.,-0.984175951805612));
#41546=DIRECTION('center_axis',(0.,1.,0.));
#41547=DIRECTION('ref_axis',(1.,0.,0.));
#41548=DIRECTION('',(0.,-1.,0.));
#41549=DIRECTION('center_axis',(1.,0.,3.3635018779E-16));
#41550=DIRECTION('ref_axis',(-3.3635018779E-16,0.,1.));
#41551=DIRECTION('',(3.3635018779E-16,0.,-1.));
#41552=DIRECTION('',(0.,-1.,0.));
#41553=DIRECTION('center_axis',(0.,1.,0.));
#41554=DIRECTION('ref_axis',(-1.,0.,0.));
#41555=DIRECTION('center_axis',(0.,1.,0.));
#41556=DIRECTION('ref_axis',(1.,0.,0.));
#41557=DIRECTION('',(0.,-1.,0.));
#41558=DIRECTION('',(0.,-1.,0.));
#41559=DIRECTION('',(0.,-1.,0.));
#41560=DIRECTION('',(0.,-1.,0.));
#41561=DIRECTION('center_axis',(0.,-1.,0.));
#41562=DIRECTION('ref_axis',(1.,0.,0.));
#41563=DIRECTION('center_axis',(0.,-1.,0.));
#41564=DIRECTION('ref_axis',(1.,0.,0.));
#41565=DIRECTION('',(0.,-1.,0.));
#41566=DIRECTION('center_axis',(1.,0.,-3.3635018779E-16));
#41567=DIRECTION('ref_axis',(-3.3635018779E-16,0.,-1.));
#41568=DIRECTION('',(-3.3635018779E-16,0.,-1.));
#41569=DIRECTION('',(0.,-1.,0.));
#41570=DIRECTION('center_axis',(0.,-1.,0.));
#41571=DIRECTION('ref_axis',(-0.17719394991793,0.,-0.984175951805612));
#41572=DIRECTION('center_axis',(0.,-1.,0.));
#41573=DIRECTION('ref_axis',(1.,0.,0.));
#41574=DIRECTION('center_axis',(0.,-1.,0.));
#41575=DIRECTION('ref_axis',(0.898888448298522,0.,0.438177541089767));
#41576=DIRECTION('center_axis',(0.,-1.,0.));
#41577=DIRECTION('ref_axis',(1.,0.,0.));
#41578=DIRECTION('',(0.,-1.,0.));
#41579=DIRECTION('',(0.,-1.,0.));
#41580=DIRECTION('',(0.,-1.,0.));
#41581=DIRECTION('',(0.,-1.,0.));
#41582=DIRECTION('',(0.,1.,0.));
#41583=DIRECTION('',(0.,1.,0.));
#41584=DIRECTION('',(0.,1.,0.));
#41585=DIRECTION('center_axis',(0.,1.,0.));
#41586=DIRECTION('ref_axis',(0.426033148631104,0.,-0.904707552896221));
#41587=DIRECTION('center_axis',(0.,1.,0.));
#41588=DIRECTION('ref_axis',(1.,0.,0.));
#41589=DIRECTION('',(0.,-1.,0.));
#41590=DIRECTION('center_axis',(0.,-1.,0.));
#41591=DIRECTION('ref_axis',(-0.196635535421993,0.,0.980476652556962));
#41592=DIRECTION('',(0.,-1.,0.));
#41593=DIRECTION('center_axis',(0.,-1.,0.));
#41594=DIRECTION('ref_axis',(1.,0.,0.));
#41595=DIRECTION('center_axis',(1.,0.,0.));
#41596=DIRECTION('ref_axis',(0.,1.,0.));
#41597=DIRECTION('',(0.,0.,-1.));
#41598=DIRECTION('',(0.,1.,0.));
#41599=DIRECTION('center_axis',(0.,1.,0.));
#41600=DIRECTION('ref_axis',(0.204297691364974,0.,-0.978908807449878));
#41601=DIRECTION('',(0.,-1.,0.));
#41602=DIRECTION('center_axis',(0.,1.,0.));
#41603=DIRECTION('ref_axis',(1.,0.,0.));
#41604=DIRECTION('center_axis',(0.,-1.,0.));
#41605=DIRECTION('ref_axis',(-0.17925890877697,0.,0.983801933126831));
#41606=DIRECTION('center_axis',(0.,-1.,0.));
#41607=DIRECTION('ref_axis',(1.,0.,0.));
#41608=DIRECTION('',(0.,-1.,0.));
#41609=DIRECTION('',(0.,1.,0.));
#41610=DIRECTION('',(0.,1.,0.));
#41611=DIRECTION('',(0.,1.,0.));
#41612=DIRECTION('',(0.,1.,0.));
#41613=DIRECTION('center_axis',(0.,1.,0.));
#41614=DIRECTION('ref_axis',(0.201763361403043,0.,-0.979434298968208));
#41615=DIRECTION('',(0.,1.,0.));
#41616=DIRECTION('',(0.,1.,0.));
#41617=DIRECTION('',(0.,1.,0.));
#41618=DIRECTION('center_axis',(0.,1.,0.));
#41619=DIRECTION('ref_axis',(7.9357870457813E-5,0.,0.999999996851164));
#41620=DIRECTION('',(0.,1.,0.));
#41621=DIRECTION('center_axis',(0.,-1.,0.));
#41622=DIRECTION('ref_axis',(-7.9357870457813E-5,0.,0.999999996851164));
#41623=DIRECTION('center_axis',(0.,1.,0.));
#41624=DIRECTION('ref_axis',(0.17925890877697,0.,0.983801933126831));
#41625=DIRECTION('center_axis',(0.,-1.,0.));
#41626=DIRECTION('ref_axis',(1.,0.,0.));
#41627=DIRECTION('',(0.,1.,0.));
#41628=DIRECTION('',(0.,1.,0.));
#41629=DIRECTION('center_axis',(0.,-1.,0.));
#41630=DIRECTION('ref_axis',(-0.204297691364974,0.,-0.978908807449878));
#41631=DIRECTION('center_axis',(0.,-1.,0.));
#41632=DIRECTION('ref_axis',(1.,0.,0.));
#41633=DIRECTION('',(0.,1.,0.));
#41634=DIRECTION('center_axis',(1.,0.,0.));
#41635=DIRECTION('ref_axis',(0.,1.,0.));
#41636=DIRECTION('',(0.,0.,-1.));
#41637=DIRECTION('',(0.,1.,0.));
#41638=DIRECTION('center_axis',(0.,1.,0.));
#41639=DIRECTION('ref_axis',(0.196635535421993,0.,0.980476652556962));
#41640=DIRECTION('center_axis',(0.,-1.,0.));
#41641=DIRECTION('ref_axis',(1.,0.,0.));
#41642=DIRECTION('',(0.,1.,0.));
#41643=DIRECTION('center_axis',(0.,-1.,0.));
#41644=DIRECTION('ref_axis',(-0.426033148631104,0.,-0.904707552896221));
#41645=DIRECTION('center_axis',(0.,-1.,0.));
#41646=DIRECTION('ref_axis',(1.,0.,0.));
#41647=DIRECTION('',(0.,1.,0.));
#41648=DIRECTION('',(0.,1.,0.));
#41649=DIRECTION('',(0.,1.,0.));
#41650=DIRECTION('',(0.,1.,0.));
#41651=DIRECTION('center_axis',(0.,1.,0.));
#41652=DIRECTION('ref_axis',(1.,0.,0.));
#41653=DIRECTION('center_axis',(0.,1.,0.));
#41654=DIRECTION('ref_axis',(1.,0.,0.));
#41655=DIRECTION('center_axis',(-1.,0.,0.));
#41656=DIRECTION('ref_axis',(0.,0.,1.));
#41657=DIRECTION('',(0.,0.,1.));
#41658=DIRECTION('center_axis',(-1.,0.,0.));
#41659=DIRECTION('ref_axis',(0.,0.,1.));
#41660=DIRECTION('',(0.,0.,1.));
#41661=DIRECTION('center_axis',(-1.,0.,0.));
#41662=DIRECTION('ref_axis',(0.,0.,1.));
#41663=DIRECTION('',(0.,0.,1.));
#41664=DIRECTION('center_axis',(-1.,0.,0.));
#41665=DIRECTION('ref_axis',(0.,0.,1.));
#41666=DIRECTION('',(0.,0.,1.));
#41667=DIRECTION('center_axis',(-0.698033961608027,0.,0.716064653814028));
#41668=DIRECTION('ref_axis',(0.,1.,0.));
#41669=DIRECTION('',(0.,-1.,0.));
#41670=DIRECTION('',(0.716064653814028,0.,0.698033961608027));
#41671=DIRECTION('',(0.,1.,0.));
#41672=DIRECTION('',(0.716064653814028,0.,0.698033961608027));
#41673=DIRECTION('center_axis',(-0.698033961608027,0.,0.716064653814028));
#41674=DIRECTION('ref_axis',(0.,1.,0.));
#41675=DIRECTION('',(0.716064653814028,0.,0.698033961608027));
#41676=DIRECTION('',(0.,1.,0.));
#41677=DIRECTION('',(-0.716064653814028,0.,-0.698033961608027));
#41678=DIRECTION('',(0.,1.,0.));
#41679=DIRECTION('',(-0.716064653814028,0.,-0.698033961608027));
#41680=DIRECTION('center_axis',(-0.698033961608027,0.,0.716064653814028));
#41681=DIRECTION('ref_axis',(0.,1.,0.));
#41682=DIRECTION('',(-0.716064653814028,0.,-0.698033961608027));
#41683=DIRECTION('',(0.,1.,0.));
#41684=DIRECTION('',(0.716064653814028,0.,0.698033961608027));
#41685=DIRECTION('',(0.,1.,0.));
#41686=DIRECTION('',(0.716064653814028,0.,0.698033961608027));
#41687=DIRECTION('center_axis',(-0.698033961608027,0.,0.716064653814028));
#41688=DIRECTION('ref_axis',(0.,1.,0.));
#41689=DIRECTION('',(0.716064653814028,0.,0.698033961608027));
#41690=DIRECTION('',(0.,1.,0.));
#41691=DIRECTION('',(-0.716064653814028,0.,-0.698033961608027));
#41692=DIRECTION('',(0.,-1.,0.));
#41693=DIRECTION('center_axis',(-0.698033961608027,0.,-0.716064653814028));
#41694=DIRECTION('ref_axis',(-0.716064653814028,0.,0.698033961608027));
#41695=DIRECTION('',(0.,-1.,0.));
#41696=DIRECTION('',(0.716064653814028,0.,-0.698033961608027));
#41697=DIRECTION('',(0.,1.,0.));
#41698=DIRECTION('',(-0.716064653814028,0.,0.698033961608027));
#41699=DIRECTION('center_axis',(-0.698033961608027,0.,-0.716064653814028));
#41700=DIRECTION('ref_axis',(-0.716064653814028,0.,0.698033961608027));
#41701=DIRECTION('',(-0.716064653814028,0.,0.698033961608027));
#41702=DIRECTION('',(0.,1.,0.));
#41703=DIRECTION('',(-0.716064653814028,0.,0.698033961608027));
#41704=DIRECTION('',(0.,1.,0.));
#41705=DIRECTION('',(0.716064653814028,0.,-0.698033961608027));
#41706=DIRECTION('center_axis',(-0.698033961608027,0.,-0.716064653814028));
#41707=DIRECTION('ref_axis',(-0.716064653814028,0.,0.698033961608027));
#41708=DIRECTION('',(0.716064653814028,0.,-0.698033961608027));
#41709=DIRECTION('',(0.,1.,0.));
#41710=DIRECTION('',(0.716064653814028,0.,-0.698033961608027));
#41711=DIRECTION('',(0.,1.,0.));
#41712=DIRECTION('',(-0.716064653814028,0.,0.698033961608027));
#41713=DIRECTION('center_axis',(-0.698033961608027,0.,-0.716064653814028));
#41714=DIRECTION('ref_axis',(-0.716064653814028,0.,0.698033961608027));
#41715=DIRECTION('',(-0.716064653814028,0.,0.698033961608027));
#41716=DIRECTION('',(0.,1.,0.));
#41717=DIRECTION('',(-0.716064653814028,0.,0.698033961608027));
#41718=DIRECTION('',(0.,-1.,0.));
#41719=DIRECTION('center_axis',(0.,1.,0.));
#41720=DIRECTION('ref_axis',(1.,0.,0.));
#41721=DIRECTION('center_axis',(0.,1.,0.));
#41722=DIRECTION('ref_axis',(1.,0.,0.));
#41723=DIRECTION('center_axis',(0.,1.,0.));
#41724=DIRECTION('ref_axis',(1.,0.,0.));
#41725=DIRECTION('',(0.716064653814028,0.,0.698033961608027));
#41726=DIRECTION('center_axis',(0.,1.,0.));
#41727=DIRECTION('ref_axis',(1.,0.,0.));
#41728=DIRECTION('center_axis',(0.,1.,0.));
#41729=DIRECTION('ref_axis',(1.,0.,0.));
#41730=DIRECTION('center_axis',(0.,1.,0.));
#41731=DIRECTION('ref_axis',(1.,0.,0.));
#41732=DIRECTION('',(-0.698033961608027,0.,-0.716064653814028));
#41733=DIRECTION('center_axis',(0.,1.,0.));
#41734=DIRECTION('ref_axis',(1.,0.,0.));
#41735=DIRECTION('center_axis',(0.,1.,0.));
#41736=DIRECTION('ref_axis',(1.,0.,0.));
#41737=DIRECTION('center_axis',(0.,1.,0.));
#41738=DIRECTION('ref_axis',(1.,0.,0.));
#41739=DIRECTION('center_axis',(0.,1.,0.));
#41740=DIRECTION('ref_axis',(1.,0.,0.));
#41741=DIRECTION('',(0.698033961608027,0.,-0.716064653814028));
#41742=DIRECTION('center_axis',(0.,1.,0.));
#41743=DIRECTION('ref_axis',(1.,0.,0.));
#41744=DIRECTION('center_axis',(0.,1.,0.));
#41745=DIRECTION('ref_axis',(1.,0.,0.));
#41746=DIRECTION('',(0.698033961608027,0.,-0.716064653814028));
#41747=DIRECTION('center_axis',(0.,1.,0.));
#41748=DIRECTION('ref_axis',(1.,0.,0.));
#41749=DIRECTION('',(-0.716064653814028,0.,0.698033961608027));
#41750=DIRECTION('center_axis',(0.,1.,0.));
#41751=DIRECTION('ref_axis',(1.,0.,0.));
#41752=DIRECTION('center_axis',(0.,1.,0.));
#41753=DIRECTION('ref_axis',(1.,0.,0.));
#41754=DIRECTION('',(0.716064653814028,0.,0.698033961608027));
#41755=DIRECTION('center_axis',(0.,1.,0.));
#41756=DIRECTION('ref_axis',(1.,0.,0.));
#41757=DIRECTION('',(-0.698033961608027,0.,-0.716064653814028));
#41758=DIRECTION('center_axis',(0.,1.,0.));
#41759=DIRECTION('ref_axis',(1.,0.,0.));
#41760=DIRECTION('center_axis',(0.,1.,0.));
#41761=DIRECTION('ref_axis',(1.,0.,0.));
#41762=DIRECTION('center_axis',(0.,1.,0.));
#41763=DIRECTION('ref_axis',(1.,0.,0.));
#41764=DIRECTION('center_axis',(0.,1.,0.));
#41765=DIRECTION('ref_axis',(1.,0.,0.));
#41766=DIRECTION('center_axis',(0.,1.,0.));
#41767=DIRECTION('ref_axis',(1.,0.,0.));
#41768=DIRECTION('',(-0.716064653814028,0.,0.698033961608027));
#41769=DIRECTION('center_axis',(0.716064653814028,3.32064561166926E-28,
-0.698033961608027));
#41770=DIRECTION('ref_axis',(-2.37779695035902E-28,1.,2.31792341140981E-28));
#41771=DIRECTION('center_axis',(0.716064653814028,0.,-0.698033961608027));
#41772=DIRECTION('ref_axis',(0.698033961608027,0.,0.716064653814028));
#41773=DIRECTION('center_axis',(0.716064653814028,0.,-0.698033961608027));
#41774=DIRECTION('ref_axis',(0.698033961608027,0.,0.716064653814028));
#41775=DIRECTION('',(0.716064653814028,0.,-0.698033961608027));
#41776=DIRECTION('center_axis',(0.,-1.,0.));
#41777=DIRECTION('ref_axis',(0.803032113208901,0.,-0.595935755895925));
#41778=DIRECTION('center_axis',(0.,1.,0.));
#41779=DIRECTION('ref_axis',(1.,0.,0.));
#41780=DIRECTION('center_axis',(0.,0.,1.));
#41781=DIRECTION('ref_axis',(1.,0.,0.));
#41782=DIRECTION('center_axis',(-0.595935755895926,0.,-0.8030321132089));
#41783=DIRECTION('ref_axis',(0.8030321132089,0.,-0.595935755895926));
#41784=DIRECTION('center_axis',(0.,1.,0.));
#41785=DIRECTION('ref_axis',(-0.716064653814026,0.,0.69803396160803));
#41786=DIRECTION('center_axis',(0.,1.,0.));
#41787=DIRECTION('ref_axis',(1.,0.,0.));
#41788=DIRECTION('',(0.,1.,0.));
#41789=DIRECTION('center_axis',(1.,0.,0.));
#41790=DIRECTION('ref_axis',(0.,-1.,0.));
#41791=DIRECTION('center_axis',(0.698033961608027,0.,0.716064653814028));
#41792=DIRECTION('ref_axis',(0.716064653814028,0.,-0.698033961608027));
#41793=DIRECTION('center_axis',(0.,1.,0.));
#41794=DIRECTION('ref_axis',(0.8030321132089,0.,-0.595935755895926));
#41795=DIRECTION('center_axis',(-0.779809347293264,0.,-0.626017077941212));
#41796=DIRECTION('ref_axis',(0.626017077941212,0.,-0.779809347293264));
#41797=DIRECTION('center_axis',(0.,1.,0.));
#41798=DIRECTION('ref_axis',(1.,0.,0.));
#41799=DIRECTION('center_axis',(0.,1.,0.));
#41800=DIRECTION('ref_axis',(0.626017077941214,0.,-0.779809347293263));
#41801=DIRECTION('center_axis',(0.,1.,0.));
#41802=DIRECTION('ref_axis',(1.,0.,0.));
#41803=DIRECTION('center_axis',(1.,0.,0.));
#41804=DIRECTION('ref_axis',(0.,-1.,0.));
#41805=DIRECTION('center_axis',(-0.716064653814028,0.,0.698033961608027));
#41806=DIRECTION('ref_axis',(0.698033961608027,0.,0.716064653814028));
#41807=DIRECTION('center_axis',(0.,1.,0.));
#41808=DIRECTION('ref_axis',(1.,0.,0.));
#41809=DIRECTION('',(-0.716064653814028,0.,0.698033961608027));
#41810=DIRECTION('',(0.698033961608027,0.,0.716064653814028));
#41811=DIRECTION('',(0.716064653814028,0.,-0.698033961608027));
#41812=DIRECTION('center_axis',(0.,-1.,0.));
#41813=DIRECTION('ref_axis',(1.,0.,0.));
#41814=DIRECTION('center_axis',(0.,-1.,0.));
#41815=DIRECTION('ref_axis',(1.,0.,0.));
#41816=DIRECTION('center_axis',(0.,-1.,0.));
#41817=DIRECTION('ref_axis',(1.,0.,0.));
#41818=DIRECTION('',(-0.716064653814028,0.,0.698033961608027));
#41819=DIRECTION('',(0.698033961608027,0.,0.716064653814028));
#41820=DIRECTION('center_axis',(-0.698033961608027,0.,-0.716064653814028));
#41821=DIRECTION('ref_axis',(-0.716064653814028,0.,0.698033961608027));
#41822=DIRECTION('center_axis',(0.698033961608027,0.,0.716064653814028));
#41823=DIRECTION('ref_axis',(0.716064653814028,0.,-0.698033961608027));
#41824=DIRECTION('',(0.698033961608027,0.,0.716064653814028));
#41825=DIRECTION('center_axis',(0.,0.,1.));
#41826=DIRECTION('ref_axis',(1.,0.,0.));
#41827=DIRECTION('center_axis',(-0.716064653814028,0.,0.698033961608027));
#41828=DIRECTION('ref_axis',(0.698033961608027,0.,0.716064653814028));
#41829=DIRECTION('center_axis',(0.,1.,0.));
#41830=DIRECTION('ref_axis',(1.,0.,0.));
#41831=DIRECTION('center_axis',(0.716064653814028,0.,-0.698033961608027));
#41832=DIRECTION('ref_axis',(-0.698033961608027,0.,-0.716064653814028));
#41833=DIRECTION('center_axis',(-0.716064653814028,0.,0.698033961608027));
#41834=DIRECTION('ref_axis',(0.698033961608027,0.,0.716064653814028));
#41835=DIRECTION('center_axis',(0.,0.,1.));
#41836=DIRECTION('ref_axis',(1.,0.,0.));
#41837=DIRECTION('center_axis',(0.,1.,0.));
#41838=DIRECTION('ref_axis',(1.,0.,0.));
#41839=DIRECTION('center_axis',(0.698033961608027,0.,0.716064653814028));
#41840=DIRECTION('ref_axis',(0.716064653814028,0.,-0.698033961608027));
#41841=DIRECTION('center_axis',(-0.698033961608027,0.,-0.716064653814028));
#41842=DIRECTION('ref_axis',(-0.716064653814028,0.,0.698033961608027));
#41843=DIRECTION('',(0.698033961608027,0.,0.716064653814028));
#41844=DIRECTION('center_axis',(0.698033961608027,0.,0.716064653814028));
#41845=DIRECTION('ref_axis',(0.716064653814028,0.,-0.698033961608027));
#41846=DIRECTION('center_axis',(1.,0.,0.));
#41847=DIRECTION('ref_axis',(0.,-1.,0.));
#41848=DIRECTION('center_axis',(0.,1.,0.));
#41849=DIRECTION('ref_axis',(1.,0.,0.));
#41850=DIRECTION('center_axis',(0.716064653814028,0.,-0.698033961608027));
#41851=DIRECTION('ref_axis',(0.698033961608027,0.,0.716064653814028));
#41852=DIRECTION('center_axis',(0.716064653814028,3.32064561166926E-28,
-0.698033961608027));
#41853=DIRECTION('ref_axis',(-2.37779695035902E-28,1.,2.31792341140981E-28));
#41854=DIRECTION('center_axis',(0.716064653814028,0.,-0.698033961608027));
#41855=DIRECTION('ref_axis',(0.698033961608027,0.,0.716064653814028));
#41856=DIRECTION('center_axis',(0.,1.,0.));
#41857=DIRECTION('ref_axis',(0.67049648912325,0.,-0.741912702461277));
#41858=DIRECTION('center_axis',(0.,-1.,0.));
#41859=DIRECTION('ref_axis',(1.,0.,0.));
#41860=DIRECTION('center_axis',(0.741912702461277,0.,0.67049648912325));
#41861=DIRECTION('ref_axis',(0.67049648912325,0.,-0.741912702461277));
#41862=DIRECTION('center_axis',(0.,1.,0.));
#41863=DIRECTION('ref_axis',(0.767334963051732,0.,-0.641246484963776));
#41864=DIRECTION('center_axis',(0.641246484963776,0.,0.767334963051731));
#41865=DIRECTION('ref_axis',(0.767334963051731,0.,-0.641246484963776));
#41866=DIRECTION('center_axis',(0.,1.,0.));
#41867=DIRECTION('ref_axis',(0.698033961608026,0.,0.716064653814029));
#41868=DIRECTION('center_axis',(0.,-1.,0.));
#41869=DIRECTION('ref_axis',(1.,0.,0.));
#41870=DIRECTION('center_axis',(-0.716064653814028,0.,0.698033961608027));
#41871=DIRECTION('ref_axis',(0.698033961608027,0.,0.716064653814028));
#41872=DIRECTION('center_axis',(0.716064653814028,0.,-0.698033961608027));
#41873=DIRECTION('ref_axis',(-0.698033961608027,0.,-0.716064653814028));
#41874=DIRECTION('center_axis',(0.716064653814028,0.,-0.698033961608027));
#41875=DIRECTION('ref_axis',(0.,-1.,0.));
#41876=DIRECTION('',(0.,1.,0.));
#41877=DIRECTION('center_axis',(0.,1.,0.));
#41878=DIRECTION('ref_axis',(-0.69803396160803,0.,-0.716064653814026));
#41879=DIRECTION('center_axis',(0.,1.,0.));
#41880=DIRECTION('ref_axis',(-0.69803396160803,0.,-0.716064653814026));
#41881=DIRECTION('',(0.,1.,0.));
#41882=DIRECTION('center_axis',(0.716064653814028,0.,-0.698033961608027));
#41883=DIRECTION('ref_axis',(0.,-1.,0.));
#41884=DIRECTION('',(0.,1.,0.));
#41885=DIRECTION('center_axis',(0.,1.,0.));
#41886=DIRECTION('ref_axis',(-0.716064653814028,0.,0.698033961608027));
#41887=DIRECTION('center_axis',(0.,-1.,0.));
#41888=DIRECTION('ref_axis',(-0.698033961608027,0.,-0.716064653814028));
#41889=DIRECTION('center_axis',(0.,1.,0.));
#41890=DIRECTION('ref_axis',(0.698033961608027,0.,0.716064653814028));
#41891=DIRECTION('center_axis',(-0.698033961608027,0.,0.716064653814028));
#41892=DIRECTION('ref_axis',(0.,1.,0.));
#41893=DIRECTION('',(0.,1.,0.));
#41894=DIRECTION('',(0.716064653814028,0.,0.698033961608027));
#41895=DIRECTION('',(0.,1.,0.));
#41896=DIRECTION('center_axis',(0.716064653814028,-3.32064561166926E-28,
0.698033961608027));
#41897=DIRECTION('ref_axis',(2.37779695035902E-28,1.,2.31792341140981E-28));
#41898=DIRECTION('center_axis',(0.716064653814028,0.,0.698033961608027));
#41899=DIRECTION('ref_axis',(0.698033961608027,0.,-0.716064653814028));
#41900=DIRECTION('center_axis',(0.716064653814028,0.,0.698033961608027));
#41901=DIRECTION('ref_axis',(0.698033961608027,0.,-0.716064653814028));
#41902=DIRECTION('',(0.716064653814028,0.,0.698033961608027));
#41903=DIRECTION('center_axis',(0.,-1.,0.));
#41904=DIRECTION('ref_axis',(0.626017077941214,0.,0.779809347293263));
#41905=DIRECTION('center_axis',(0.,1.,0.));
#41906=DIRECTION('ref_axis',(1.,0.,0.));
#41907=DIRECTION('center_axis',(1.,0.,0.));
#41908=DIRECTION('ref_axis',(0.,-1.,0.));
#41909=DIRECTION('center_axis',(0.779809347293264,0.,-0.626017077941212));
#41910=DIRECTION('ref_axis',(0.626017077941212,0.,0.779809347293264));
#41911=DIRECTION('center_axis',(0.,1.,0.));
#41912=DIRECTION('ref_axis',(-0.716064653814026,0.,-0.69803396160803));
#41913=DIRECTION('',(0.,1.,0.));
#41914=DIRECTION('center_axis',(0.,1.,0.));
#41915=DIRECTION('ref_axis',(1.,0.,0.));
#41916=DIRECTION('center_axis',(0.,0.,1.));
#41917=DIRECTION('ref_axis',(1.,0.,0.));
#41918=DIRECTION('center_axis',(-0.698033961608027,0.,0.716064653814028));
#41919=DIRECTION('ref_axis',(0.716064653814028,0.,0.698033961608027));
#41920=DIRECTION('center_axis',(0.,1.,0.));
#41921=DIRECTION('ref_axis',(0.626017077941212,0.,0.779809347293264));
#41922=DIRECTION('center_axis',(0.595935755895926,0.,-0.8030321132089));
#41923=DIRECTION('ref_axis',(0.8030321132089,0.,0.595935755895926));
#41924=DIRECTION('center_axis',(0.,1.,0.));
#41925=DIRECTION('ref_axis',(1.,0.,0.));
#41926=DIRECTION('center_axis',(0.,1.,0.));
#41927=DIRECTION('ref_axis',(0.803032113208901,0.,0.595935755895925));
#41928=DIRECTION('',(0.,1.,0.));
#41929=DIRECTION('center_axis',(0.,1.,0.));
#41930=DIRECTION('ref_axis',(1.,0.,0.));
#41931=DIRECTION('center_axis',(0.,0.,1.));
#41932=DIRECTION('ref_axis',(1.,0.,0.));
#41933=DIRECTION('center_axis',(-0.716064653814028,0.,-0.698033961608027));
#41934=DIRECTION('ref_axis',(0.698033961608027,0.,-0.716064653814028));
#41935=DIRECTION('center_axis',(0.,1.,0.));
#41936=DIRECTION('ref_axis',(1.,0.,0.));
#41937=DIRECTION('',(-0.716064653814028,0.,-0.698033961608027));
#41938=DIRECTION('',(-0.698033961608027,0.,0.716064653814028));
#41939=DIRECTION('',(0.716064653814028,0.,0.698033961608027));
#41940=DIRECTION('center_axis',(0.,-1.,0.));
#41941=DIRECTION('ref_axis',(1.,0.,0.));
#41942=DIRECTION('center_axis',(0.,-1.,0.));
#41943=DIRECTION('ref_axis',(1.,0.,0.));
#41944=DIRECTION('center_axis',(0.,-1.,0.));
#41945=DIRECTION('ref_axis',(1.,0.,0.));
#41946=DIRECTION('',(-0.716064653814028,0.,-0.698033961608027));
#41947=DIRECTION('',(-0.698033961608027,0.,0.716064653814028));
#41948=DIRECTION('center_axis',(-0.698033961608027,-3.32064561166926E-28,
0.716064653814028));
#41949=DIRECTION('ref_axis',(-2.31792341140981E-28,1.,2.37779695035902E-28));
#41950=DIRECTION('center_axis',(-0.698033961608027,0.,0.716064653814028));
#41951=DIRECTION('ref_axis',(0.716064653814028,0.,0.698033961608027));
#41952=DIRECTION('',(-0.698033961608027,0.,0.716064653814028));
#41953=DIRECTION('center_axis',(1.,0.,0.));
#41954=DIRECTION('ref_axis',(0.,-1.,0.));
#41955=DIRECTION('center_axis',(-0.716064653814028,0.,-0.698033961608027));
#41956=DIRECTION('ref_axis',(0.698033961608027,0.,-0.716064653814028));
#41957=DIRECTION('center_axis',(0.,1.,0.));
#41958=DIRECTION('ref_axis',(1.,0.,0.));
#41959=DIRECTION('center_axis',(0.716064653814028,0.,0.698033961608027));
#41960=DIRECTION('ref_axis',(0.698033961608027,0.,-0.716064653814028));
#41961=DIRECTION('',(-0.716064653814028,0.,-0.698033961608027));
#41962=DIRECTION('center_axis',(-0.716064653814028,0.,-0.698033961608027));
#41963=DIRECTION('ref_axis',(0.698033961608027,0.,-0.716064653814028));
#41964=DIRECTION('center_axis',(1.,0.,0.));
#41965=DIRECTION('ref_axis',(0.,-1.,0.));
#41966=DIRECTION('center_axis',(0.,1.,0.));
#41967=DIRECTION('ref_axis',(1.,0.,0.));
#41968=DIRECTION('center_axis',(-0.698033961608027,0.,0.716064653814028));
#41969=DIRECTION('ref_axis',(0.716064653814028,0.,0.698033961608027));
#41970=DIRECTION('center_axis',(-0.698033961608027,-3.32064561166926E-28,
0.716064653814028));
#41971=DIRECTION('ref_axis',(-2.31792341140981E-28,1.,2.37779695035902E-28));
#41972=DIRECTION('',(-0.698033961608027,0.,0.716064653814028));
#41973=DIRECTION('center_axis',(-0.698033961608027,0.,0.716064653814028));
#41974=DIRECTION('ref_axis',(0.716064653814028,0.,0.698033961608027));
#41975=DIRECTION('center_axis',(0.,0.,1.));
#41976=DIRECTION('ref_axis',(1.,0.,0.));
#41977=DIRECTION('center_axis',(0.,1.,0.));
#41978=DIRECTION('ref_axis',(1.,0.,0.));
#41979=DIRECTION('center_axis',(0.716064653814028,0.,0.698033961608027));
#41980=DIRECTION('ref_axis',(0.698033961608027,0.,-0.716064653814028));
#41981=DIRECTION('center_axis',(0.716064653814028,-3.32064561166926E-28,
0.698033961608027));
#41982=DIRECTION('ref_axis',(2.37779695035902E-28,1.,2.31792341140981E-28));
#41983=DIRECTION('',(0.716064653814028,0.,0.698033961608027));
#41984=DIRECTION('center_axis',(0.716064653814028,0.,0.698033961608027));
#41985=DIRECTION('ref_axis',(0.698033961608027,0.,-0.716064653814028));
#41986=DIRECTION('center_axis',(0.,1.,0.));
#41987=DIRECTION('ref_axis',(0.767334963051732,0.,0.641246484963776));
#41988=DIRECTION('center_axis',(0.,-1.,0.));
#41989=DIRECTION('ref_axis',(1.,0.,0.));
#41990=DIRECTION('center_axis',(-0.641246484963776,0.,0.767334963051731));
#41991=DIRECTION('ref_axis',(0.767334963051731,0.,0.641246484963776));
#41992=DIRECTION('center_axis',(0.,1.,0.));
#41993=DIRECTION('ref_axis',(0.67049648912325,0.,0.741912702461277));
#41994=DIRECTION('center_axis',(-0.741912702461277,0.,0.67049648912325));
#41995=DIRECTION('ref_axis',(0.67049648912325,0.,0.741912702461277));
#41996=DIRECTION('center_axis',(0.,1.,0.));
#41997=DIRECTION('ref_axis',(-0.698033961608026,0.,0.716064653814029));
#41998=DIRECTION('center_axis',(0.,-1.,0.));
#41999=DIRECTION('ref_axis',(1.,0.,0.));
#42000=DIRECTION('center_axis',(-0.716064653814028,0.,-0.698033961608027));
#42001=DIRECTION('ref_axis',(0.698033961608027,0.,-0.716064653814028));
#42002=DIRECTION('center_axis',(0.716064653814028,0.,0.698033961608027));
#42003=DIRECTION('ref_axis',(0.698033961608027,0.,-0.716064653814028));
#42004=DIRECTION('',(-0.716064653814028,0.,-0.698033961608027));
#42005=DIRECTION('center_axis',(-0.716064653814028,0.,-0.698033961608027));
#42006=DIRECTION('ref_axis',(-0.698033961608027,0.,0.716064653814028));
#42007=DIRECTION('',(0.,1.,0.));
#42008=DIRECTION('center_axis',(0.,1.,0.));
#42009=DIRECTION('ref_axis',(0.69803396160803,0.,-0.716064653814026));
#42010=DIRECTION('',(0.,1.,0.));
#42011=DIRECTION('center_axis',(-0.698033961608027,0.,0.716064653814028));
#42012=DIRECTION('ref_axis',(0.,1.,0.));
#42013=DIRECTION('',(0.,1.,0.));
#42014=DIRECTION('center_axis',(0.,1.,0.));
#42015=DIRECTION('ref_axis',(0.69803396160803,0.,-0.716064653814026));
#42016=DIRECTION('',(0.,1.,0.));
#42017=DIRECTION('center_axis',(-0.716064653814028,0.,-0.698033961608027));
#42018=DIRECTION('ref_axis',(-0.698033961608027,0.,0.716064653814028));
#42019=DIRECTION('',(0.,1.,0.));
#42020=DIRECTION('center_axis',(0.,1.,0.));
#42021=DIRECTION('ref_axis',(-0.716064653814028,0.,-0.698033961608027));
#42022=DIRECTION('',(0.,1.,0.));
#42023=DIRECTION('center_axis',(-0.698033961608027,0.,0.716064653814028));
#42024=DIRECTION('ref_axis',(0.,1.,0.));
#42025=DIRECTION('',(0.,-1.,0.));
#42026=DIRECTION('center_axis',(0.,-1.,0.));
#42027=DIRECTION('ref_axis',(0.698033961608027,0.,-0.716064653814028));
#42028=DIRECTION('center_axis',(0.,1.,0.));
#42029=DIRECTION('ref_axis',(-0.698033961608027,0.,0.716064653814028));
#42030=DIRECTION('',(0.,-1.,0.));
#42031=DIRECTION('center_axis',(-0.698033961608027,0.,0.716064653814028));
#42032=DIRECTION('ref_axis',(0.,1.,0.));
#42033=DIRECTION('center_axis',(-0.716064653814028,0.,-0.698033961608027));
#42034=DIRECTION('ref_axis',(-0.698033961608027,0.,0.716064653814028));
#42035=DIRECTION('center_axis',(-0.716064653814028,0.,-0.698033961608027));
#42036=DIRECTION('ref_axis',(0.698033961608027,0.,-0.716064653814028));
#42037=DIRECTION('',(-0.716064653814028,0.,-0.698033961608027));
#42038=DIRECTION('center_axis',(-0.716064653814028,0.,-0.698033961608027));
#42039=DIRECTION('ref_axis',(0.698033961608027,0.,-0.716064653814028));
#42040=DIRECTION('center_axis',(0.,1.,0.));
#42041=DIRECTION('ref_axis',(-0.803032113208901,0.,-0.595935755895925));
#42042=DIRECTION('center_axis',(0.,-1.,0.));
#42043=DIRECTION('ref_axis',(1.,0.,0.));
#42044=DIRECTION('center_axis',(0.,0.,1.));
#42045=DIRECTION('ref_axis',(1.,0.,0.));
#42046=DIRECTION('center_axis',(0.595935755895926,0.,-0.8030321132089));
#42047=DIRECTION('ref_axis',(0.8030321132089,0.,0.595935755895926));
#42048=DIRECTION('center_axis',(0.,1.,0.));
#42049=DIRECTION('ref_axis',(-0.69803396160803,0.,0.716064653814026));
#42050=DIRECTION('',(0.,1.,0.));
#42051=DIRECTION('center_axis',(0.,-1.,0.));
#42052=DIRECTION('ref_axis',(1.,0.,0.));
#42053=DIRECTION('center_axis',(1.,0.,0.));
#42054=DIRECTION('ref_axis',(0.,-1.,0.));
#42055=DIRECTION('center_axis',(-0.698033961608027,0.,0.716064653814028));
#42056=DIRECTION('ref_axis',(0.716064653814028,0.,0.698033961608027));
#42057=DIRECTION('center_axis',(0.,1.,0.));
#42058=DIRECTION('ref_axis',(-0.626017077941212,0.,-0.779809347293264));
#42059=DIRECTION('center_axis',(0.,-1.,0.));
#42060=DIRECTION('ref_axis',(1.,0.,0.));
#42061=DIRECTION('center_axis',(0.779809347293264,0.,-0.626017077941212));
#42062=DIRECTION('ref_axis',(0.626017077941212,0.,0.779809347293264));
#42063=DIRECTION('center_axis',(0.,-1.,0.));
#42064=DIRECTION('ref_axis',(-0.626017077941214,0.,-0.779809347293263));
#42065=DIRECTION('center_axis',(0.,-1.,0.));
#42066=DIRECTION('ref_axis',(1.,0.,0.));
#42067=DIRECTION('center_axis',(1.,0.,0.));
#42068=DIRECTION('ref_axis',(0.,-1.,0.));
#42069=DIRECTION('center_axis',(0.716064653814028,0.,0.698033961608027));
#42070=DIRECTION('ref_axis',(0.698033961608027,0.,-0.716064653814028));
#42071=DIRECTION('center_axis',(0.,1.,0.));
#42072=DIRECTION('ref_axis',(1.,0.,0.));
#42073=DIRECTION('',(-0.698033961608027,0.,0.716064653814028));
#42074=DIRECTION('',(0.716064653814028,0.,0.698033961608027));
#42075=DIRECTION('center_axis',(0.,1.,0.));
#42076=DIRECTION('ref_axis',(1.,0.,0.));
#42077=DIRECTION('center_axis',(0.,1.,0.));
#42078=DIRECTION('ref_axis',(1.,0.,0.));
#42079=DIRECTION('center_axis',(0.,1.,0.));
#42080=DIRECTION('ref_axis',(1.,0.,0.));
#42081=DIRECTION('',(-0.716064653814028,0.,-0.698033961608027));
#42082=DIRECTION('',(-0.698033961608027,0.,0.716064653814028));
#42083=DIRECTION('',(0.716064653814028,0.,0.698033961608027));
#42084=DIRECTION('center_axis',(0.698033961608027,0.,-0.716064653814028));
#42085=DIRECTION('ref_axis',(0.,1.,0.));
#42086=DIRECTION('center_axis',(-0.698033961608027,0.,0.716064653814028));
#42087=DIRECTION('ref_axis',(0.716064653814028,0.,0.698033961608027));
#42088=DIRECTION('',(-0.698033961608027,0.,0.716064653814028));
#42089=DIRECTION('center_axis',(0.,0.,1.));
#42090=DIRECTION('ref_axis',(1.,0.,0.));
#42091=DIRECTION('center_axis',(0.716064653814028,0.,0.698033961608027));
#42092=DIRECTION('ref_axis',(0.698033961608027,0.,-0.716064653814028));
#42093=DIRECTION('center_axis',(0.,-1.,0.));
#42094=DIRECTION('ref_axis',(1.,0.,0.));
#42095=DIRECTION('center_axis',(-0.716064653814028,0.,-0.698033961608027));
#42096=DIRECTION('ref_axis',(0.,1.,0.));
#42097=DIRECTION('center_axis',(0.716064653814028,0.,0.698033961608027));
#42098=DIRECTION('ref_axis',(0.698033961608027,0.,-0.716064653814028));
#42099=DIRECTION('center_axis',(0.,0.,1.));
#42100=DIRECTION('ref_axis',(1.,0.,0.));
#42101=DIRECTION('center_axis',(-0.698033961608027,0.,0.716064653814028));
#42102=DIRECTION('ref_axis',(0.716064653814028,0.,0.698033961608027));
#42103=DIRECTION('center_axis',(0.,-1.,0.));
#42104=DIRECTION('ref_axis',(1.,0.,0.));
#42105=DIRECTION('center_axis',(0.698033961608027,0.,-0.716064653814028));
#42106=DIRECTION('ref_axis',(0.,1.,0.));
#42107=DIRECTION('center_axis',(-0.698033961608027,0.,0.716064653814028));
#42108=DIRECTION('ref_axis',(0.716064653814028,0.,0.698033961608027));
#42109=DIRECTION('',(-0.698033961608027,0.,0.716064653814028));
#42110=DIRECTION('center_axis',(1.,0.,0.));
#42111=DIRECTION('ref_axis',(0.,-1.,0.));
#42112=DIRECTION('center_axis',(-0.716064653814028,0.,-0.698033961608027));
#42113=DIRECTION('ref_axis',(0.698033961608027,0.,-0.716064653814028));
#42114=DIRECTION('center_axis',(0.,-1.,0.));
#42115=DIRECTION('ref_axis',(1.,0.,0.));
#42116=DIRECTION('center_axis',(-0.716064653814028,0.,-0.698033961608027));
#42117=DIRECTION('ref_axis',(-0.698033961608027,0.,0.716064653814028));
#42118=DIRECTION('center_axis',(-0.716064653814028,0.,-0.698033961608027));
#42119=DIRECTION('ref_axis',(0.698033961608027,0.,-0.716064653814028));
#42120=DIRECTION('center_axis',(0.,1.,0.));
#42121=DIRECTION('ref_axis',(0.698033961608026,0.,-0.716064653814029));
#42122=DIRECTION('center_axis',(-0.741912702461277,0.,0.67049648912325));
#42123=DIRECTION('ref_axis',(0.67049648912325,0.,0.741912702461277));
#42124=DIRECTION('center_axis',(0.,1.,0.));
#42125=DIRECTION('ref_axis',(1.,0.,0.));
#42126=DIRECTION('center_axis',(0.,1.,0.));
#42127=DIRECTION('ref_axis',(-0.67049648912325,0.,-0.741912702461277));
#42128=DIRECTION('center_axis',(-0.641246484963776,0.,0.767334963051731));
#42129=DIRECTION('ref_axis',(0.767334963051731,0.,0.641246484963776));
#42130=DIRECTION('center_axis',(0.,1.,0.));
#42131=DIRECTION('ref_axis',(-0.767334963051732,0.,-0.641246484963776));
#42132=DIRECTION('center_axis',(0.716064653814028,0.,0.698033961608027));
#42133=DIRECTION('ref_axis',(0.698033961608027,0.,-0.716064653814028));
#42134=DIRECTION('center_axis',(0.,1.,0.));
#42135=DIRECTION('ref_axis',(1.,0.,0.));
#42136=DIRECTION('center_axis',(-0.716064653814028,0.,-0.698033961608027));
#42137=DIRECTION('ref_axis',(0.,1.,0.));
#42138=DIRECTION('center_axis',(0.716064653814028,0.,0.698033961608027));
#42139=DIRECTION('ref_axis',(0.,-1.,0.));
#42140=DIRECTION('',(0.,1.,0.));
#42141=DIRECTION('center_axis',(0.,1.,0.));
#42142=DIRECTION('ref_axis',(0.716064653814028,0.,0.698033961608027));
#42143=DIRECTION('center_axis',(0.,1.,0.));
#42144=DIRECTION('ref_axis',(0.716064653814026,0.,0.69803396160803));
#42145=DIRECTION('',(0.,1.,0.));
#42146=DIRECTION('center_axis',(0.716064653814028,0.,0.698033961608027));
#42147=DIRECTION('ref_axis',(0.,-1.,0.));
#42148=DIRECTION('',(0.,1.,0.));
#42149=DIRECTION('center_axis',(0.,1.,0.));
#42150=DIRECTION('ref_axis',(-0.69803396160803,0.,0.716064653814026));
#42151=DIRECTION('center_axis',(0.,1.,0.));
#42152=DIRECTION('ref_axis',(0.698033961608027,0.,-0.716064653814028));
#42153=DIRECTION('center_axis',(0.,-1.,0.));
#42154=DIRECTION('ref_axis',(-0.698033961608027,0.,0.716064653814028));
#42155=DIRECTION('center_axis',(-0.698033961608027,0.,-0.716064653814028));
#42156=DIRECTION('ref_axis',(-0.716064653814028,0.,0.698033961608027));
#42157=DIRECTION('',(0.,1.,0.));
#42158=DIRECTION('',(-0.716064653814028,0.,0.698033961608027));
#42159=DIRECTION('',(0.,1.,0.));
#42160=DIRECTION('center_axis',(-0.716064653814028,0.,0.698033961608027));
#42161=DIRECTION('ref_axis',(0.698033961608027,0.,0.716064653814028));
#42162=DIRECTION('center_axis',(-0.716064653814028,0.,0.698033961608027));
#42163=DIRECTION('ref_axis',(0.698033961608027,0.,0.716064653814028));
#42164=DIRECTION('',(-0.716064653814028,0.,0.698033961608027));
#42165=DIRECTION('center_axis',(-0.716064653814028,0.,0.698033961608027));
#42166=DIRECTION('ref_axis',(0.698033961608027,0.,0.716064653814028));
#42167=DIRECTION('center_axis',(0.,1.,0.));
#42168=DIRECTION('ref_axis',(0.698033961608027,0.,0.716064653814028));
#42169=DIRECTION('',(0.,1.,0.));
#42170=DIRECTION('center_axis',(0.,-1.,0.));
#42171=DIRECTION('ref_axis',(1.,0.,0.));
#42172=DIRECTION('center_axis',(0.,0.,1.));
#42173=DIRECTION('ref_axis',(1.,0.,0.));
#42174=DIRECTION('center_axis',(0.698033961608027,0.,0.716064653814028));
#42175=DIRECTION('ref_axis',(0.716064653814028,0.,-0.698033961608027));
#42176=DIRECTION('center_axis',(0.,1.,0.));
#42177=DIRECTION('ref_axis',(-0.601264366509671,0.,0.799050162108565));
#42178=DIRECTION('center_axis',(0.,-1.,0.));
#42179=DIRECTION('ref_axis',(1.,0.,0.));
#42180=DIRECTION('center_axis',(1.,0.,0.));
#42181=DIRECTION('ref_axis',(0.,-1.,0.));
#42182=DIRECTION('center_axis',(-0.799050162108564,0.,-0.601264366509672));
#42183=DIRECTION('ref_axis',(0.601264366509672,0.,-0.799050162108564));
#42184=DIRECTION('center_axis',(0.,1.,0.));
#42185=DIRECTION('ref_axis',(1.,0.,0.));
#42186=DIRECTION('',(0.698033961608027,0.,0.716064653814028));
#42187=DIRECTION('',(0.716064653814028,0.,-0.698033961608027));
#42188=DIRECTION('center_axis',(0.,1.,0.));
#42189=DIRECTION('ref_axis',(1.,0.,0.));
#42190=DIRECTION('center_axis',(0.,1.,0.));
#42191=DIRECTION('ref_axis',(1.,0.,0.));
#42192=DIRECTION('center_axis',(0.,1.,0.));
#42193=DIRECTION('ref_axis',(1.,0.,0.));
#42194=DIRECTION('',(-0.716064653814028,0.,0.698033961608027));
#42195=DIRECTION('',(0.698033961608027,0.,0.716064653814028));
#42196=DIRECTION('',(0.716064653814028,0.,-0.698033961608027));
#42197=DIRECTION('center_axis',(0.,-1.,0.));
#42198=DIRECTION('ref_axis',(1.,0.,0.));
#42199=DIRECTION('center_axis',(0.698033961608027,0.,0.716064653814028));
#42200=DIRECTION('ref_axis',(0.716064653814028,0.,-0.698033961608027));
#42201=DIRECTION('center_axis',(0.698033961608027,0.,0.716064653814028));
#42202=DIRECTION('ref_axis',(0.716064653814028,0.,-0.698033961608027));
#42203=DIRECTION('',(0.698033961608027,0.,0.716064653814028));
#42204=DIRECTION('center_axis',(1.,0.,0.));
#42205=DIRECTION('ref_axis',(0.,-1.,0.));
#42206=DIRECTION('center_axis',(0.716064653814028,0.,-0.698033961608027));
#42207=DIRECTION('ref_axis',(0.698033961608027,0.,0.716064653814028));
#42208=DIRECTION('center_axis',(0.,-1.,0.));
#42209=DIRECTION('ref_axis',(1.,0.,0.));
#42210=DIRECTION('center_axis',(0.,1.,0.));
#42211=DIRECTION('ref_axis',(-0.821350998880235,0.,0.570423120708164));
#42212=DIRECTION('center_axis',(-0.570423120708163,0.,-0.821350998880235));
#42213=DIRECTION('ref_axis',(0.821350998880235,0.,-0.570423120708163));
#42214=DIRECTION('center_axis',(0.,0.,1.));
#42215=DIRECTION('ref_axis',(1.,0.,0.));
#42216=DIRECTION('center_axis',(0.716064653814028,0.,-0.698033961608027));
#42217=DIRECTION('ref_axis',(0.698033961608027,0.,0.716064653814028));
#42218=DIRECTION('center_axis',(0.,-1.,0.));
#42219=DIRECTION('ref_axis',(1.,0.,0.));
#42220=DIRECTION('center_axis',(0.698033961608027,0.,0.716064653814028));
#42221=DIRECTION('ref_axis',(0.716064653814028,0.,-0.698033961608027));
#42222=DIRECTION('center_axis',(0.698033961608027,0.,0.716064653814028));
#42223=DIRECTION('ref_axis',(0.716064653814028,0.,-0.698033961608027));
#42224=DIRECTION('center_axis',(0.698033961608027,0.,0.716064653814028));
#42225=DIRECTION('ref_axis',(0.716064653814028,0.,-0.698033961608027));
#42226=DIRECTION('',(0.698033961608027,0.,0.716064653814028));
#42227=DIRECTION('center_axis',(1.,0.,0.));
#42228=DIRECTION('ref_axis',(0.,-1.,0.));
#42229=DIRECTION('center_axis',(0.716064653814028,0.,-0.698033961608027));
#42230=DIRECTION('ref_axis',(0.698033961608027,0.,0.716064653814028));
#42231=DIRECTION('center_axis',(0.,-1.,0.));
#42232=DIRECTION('ref_axis',(1.,0.,0.));
#42233=DIRECTION('center_axis',(0.,0.,1.));
#42234=DIRECTION('ref_axis',(1.,0.,0.));
#42235=DIRECTION('center_axis',(-0.716064653814028,0.,0.698033961608027));
#42236=DIRECTION('ref_axis',(0.698033961608027,0.,0.716064653814028));
#42237=DIRECTION('center_axis',(0.,-1.,0.));
#42238=DIRECTION('ref_axis',(1.,0.,0.));
#42239=DIRECTION('center_axis',(-0.716064653814028,0.,0.698033961608027));
#42240=DIRECTION('ref_axis',(0.,1.,0.));
#42241=DIRECTION('',(0.716064653814028,0.,-0.698033961608027));
#42242=DIRECTION('center_axis',(-0.716064653814028,0.,0.698033961608027));
#42243=DIRECTION('ref_axis',(0.698033961608027,0.,0.716064653814028));
#42244=DIRECTION('center_axis',(-0.716064653814028,0.,0.698033961608027));
#42245=DIRECTION('ref_axis',(0.698033961608027,0.,0.716064653814028));
#42246=DIRECTION('',(-0.716064653814028,0.,0.698033961608027));
#42247=DIRECTION('center_axis',(0.,1.,0.));
#42248=DIRECTION('ref_axis',(-0.698033961608026,0.,-0.716064653814029));
#42249=DIRECTION('center_axis',(0.615376309981942,0.,0.788233466120926));
#42250=DIRECTION('ref_axis',(0.788233466120926,0.,-0.615376309981942));
#42251=DIRECTION('center_axis',(0.,1.,0.));
#42252=DIRECTION('ref_axis',(1.,0.,0.));
#42253=DIRECTION('center_axis',(0.,1.,0.));
#42254=DIRECTION('ref_axis',(-0.788233466120926,0.,0.615376309981942));
#42255=DIRECTION('center_axis',(0.763773184102633,0.,0.645484719606689));
#42256=DIRECTION('ref_axis',(0.645484719606689,0.,-0.763773184102633));
#42257=DIRECTION('center_axis',(0.,1.,0.));
#42258=DIRECTION('ref_axis',(-0.645484719606688,0.,0.763773184102634));
#42259=DIRECTION('center_axis',(0.716064653814028,0.,-0.698033961608027));
#42260=DIRECTION('ref_axis',(0.698033961608027,0.,0.716064653814028));
#42261=DIRECTION('center_axis',(0.,1.,0.));
#42262=DIRECTION('ref_axis',(1.,0.,0.));
#42263=DIRECTION('center_axis',(-0.716064653814028,0.,0.698033961608027));
#42264=DIRECTION('ref_axis',(0.,1.,0.));
#42265=DIRECTION('',(0.716064653814028,0.,-0.698033961608027));
#42266=DIRECTION('center_axis',(-0.716064653814028,0.,0.698033961608027));
#42267=DIRECTION('ref_axis',(0.,1.,0.));
#42268=DIRECTION('',(0.,1.,0.));
#42269=DIRECTION('center_axis',(0.,1.,0.));
#42270=DIRECTION('ref_axis',(0.716064653814028,0.,-0.698033961608027));
#42271=DIRECTION('',(0.,1.,0.));
#42272=DIRECTION('center_axis',(0.,-1.,0.));
#42273=DIRECTION('ref_axis',(-0.821350998880237,0.,0.570423120708161));
#42274=DIRECTION('',(0.,1.,0.));
#42275=DIRECTION('center_axis',(-0.716064653814028,0.,0.698033961608027));
#42276=DIRECTION('ref_axis',(0.,1.,0.));
#42277=DIRECTION('',(0.,1.,0.));
#42278=DIRECTION('',(0.,1.,0.));
#42279=DIRECTION('center_axis',(0.,1.,0.));
#42280=DIRECTION('ref_axis',(0.716064653814027,0.,-0.698033961608028));
#42281=DIRECTION('',(0.,1.,0.));
#42282=DIRECTION('center_axis',(0.,1.,0.));
#42283=DIRECTION('ref_axis',(0.69803396160803,0.,0.716064653814026));
#42284=DIRECTION('',(0.,1.,0.));
#42285=DIRECTION('center_axis',(-0.698033961608027,0.,-0.716064653814028));
#42286=DIRECTION('ref_axis',(-0.716064653814028,0.,0.698033961608027));
#42287=DIRECTION('center_axis',(-0.698033961608027,0.,-0.716064653814028));
#42288=DIRECTION('ref_axis',(-0.716064653814028,0.,0.698033961608027));
#42289=DIRECTION('',(0.,-1.,0.));
#42290=DIRECTION('center_axis',(0.,1.,0.));
#42291=DIRECTION('ref_axis',(-0.698033961608027,0.,-0.716064653814028));
#42292=DIRECTION('center_axis',(0.,-1.,0.));
#42293=DIRECTION('ref_axis',(0.69803396160803,0.,0.716064653814026));
#42294=DIRECTION('',(0.,-1.,0.));
#42295=DIRECTION('center_axis',(-0.698033961608027,0.,-0.716064653814028));
#42296=DIRECTION('ref_axis',(-0.716064653814028,0.,0.698033961608027));
#42297=DIRECTION('axis',(0.,0.,1.));
#42298=DIRECTION('refdir',(1.,0.,0.));
#42299=DIRECTION('center_axis',(6.63470718431993E-14,0.227955838450084,
-0.973671472169396));
#42300=DIRECTION('ref_axis',(-0.992732772338003,0.117171330149,0.0274321365777));
#42301=DIRECTION('center_axis',(0.406548496485063,0.889574707517134,0.208267039522679));
#42302=DIRECTION('ref_axis',(0.874920124951576,-0.444723758704906,0.191665211757637));
#42303=DIRECTION('center_axis',(2.91433543964118E-16,0.227955838450093,
-0.973671472169394));
#42304=DIRECTION('ref_axis',(1.,-6.06006121796129E-18,2.9789526130602E-16));
#42305=DIRECTION('center_axis',(0.749524872976688,0.644544805048453,0.150912090550531));
#42306=DIRECTION('ref_axis',(-0.160087197730326,-0.0447191178841713,0.986089392306049));
#42307=DIRECTION('center_axis',(6.30625906570168E-14,0.227955838450087,
-0.973671472169396));
#42308=DIRECTION('ref_axis',(-0.662066919314815,0.729712947738079,0.170840300434043));
#42309=DIRECTION('center_axis',(-9.09138157376714E-14,0.502994068288049,
0.864289862989864));
#42310=DIRECTION('ref_axis',(-0.633334126643349,0.668855315522369,-0.389256279238214));
#42311=DIRECTION('center_axis',(-0.596844579943065,-0.693468570092834,0.403581329704418));
#42312=DIRECTION('ref_axis',(0.437619919908321,-0.702944182108675,-0.560676629207069));
#42313=DIRECTION('center_axis',(-0.59683034801759,-0.69347971696906,0.403583222938857));
#42314=DIRECTION('ref_axis',(0.802367306415891,-0.515527629471871,0.300729062190571));
#42315=DIRECTION('center_axis',(0.,0.502994068287953,0.86428986298992));
#42316=DIRECTION('ref_axis',(1.,0.,0.));
#42317=DIRECTION('center_axis',(-0.483245158280883,-0.756672875743816,0.440363799728893));
#42318=DIRECTION('ref_axis',(0.875485075257188,-0.417663891641161,0.243069448144098));
#42319=DIRECTION('center_axis',(-0.483245158280883,-0.756672875743816,0.440363799728893));
#42320=DIRECTION('ref_axis',(0.875485075257188,-0.417663891641161,0.243069448144098));
#42321=DIRECTION('center_axis',(2.41831516884545E-10,0.50299406814986,0.864289863070286));
#42322=DIRECTION('ref_axis',(-0.875472610430908,0.417683408812711,-0.243080806292652));
#42323=DIRECTION('center_axis',(-2.46296037642308E-13,-0.687200931805762,
0.726467397289991));
#42324=DIRECTION('ref_axis',(0.402304300130036,0.66508526660206,0.629136581551056));
#42325=DIRECTION('center_axis',(0.648015366812002,-0.553297373850002,-0.523390963302002));
#42326=DIRECTION('ref_axis',(0.761627260788049,0.470762036932009,0.445316763897474));
#42327=DIRECTION('center_axis',(0.648015366812002,-0.553297373850002,-0.523390963302002));
#42328=DIRECTION('ref_axis',(0.761627260788049,0.470762036932009,0.445316763897474));
#42329=DIRECTION('center_axis',(0.,0.687200931805355,-0.726467397290375));
#42330=DIRECTION('ref_axis',(1.,0.,0.));
#42331=DIRECTION('center_axis',(0.648015366812002,0.553297373850002,0.523390963302002));
#42332=DIRECTION('ref_axis',(0.761627260788049,-0.470762036932009,-0.445316763897474));
#42333=DIRECTION('center_axis',(0.648015366812002,0.553297373850002,0.523390963302002));
#42334=DIRECTION('ref_axis',(0.761627260788049,-0.470762036932009,-0.445316763897474));
#42335=DIRECTION('center_axis',(2.63677968348136E-16,0.687200931805355,
-0.726467397290375));
#42336=DIRECTION('ref_axis',(1.,-8.33708823855768E-17,2.84094538938874E-16));
#42337=DIRECTION('center_axis',(-2.04246620832741E-13,-0.502994068288093,
-0.864289862989838));
#42338=DIRECTION('ref_axis',(0.784944791291048,0.535484366527033,-0.311637879325019));
#42339=DIRECTION('center_axis',(-0.596850310252312,0.693464160284547,-0.403580432568982));
#42340=DIRECTION('ref_axis',(-0.802352586377076,-0.51573478711129,0.300412976579389));
#42341=DIRECTION('center_axis',(-2.4182864330415E-10,0.502994068149861,
0.864289863070286));
#42342=DIRECTION('ref_axis',(0.802371434083077,0.515829798451751,-0.300199435037263));
#42343=DIRECTION('center_axis',(-0.483245250027863,0.756673054355651,-0.440363392140626));
#42344=DIRECTION('ref_axis',(3.76091608502762E-6,0.50299542602652,0.864289072812016));
#42345=DIRECTION('center_axis',(-0.483247714733613,0.756671625250094,-0.440363143037791));
#42346=DIRECTION('ref_axis',(-0.8754836638776,-0.417653389614233,0.243092575837265));
#42347=DIRECTION('center_axis',(1.38777878077987E-16,0.502994068287953,
0.86428986298992));
#42348=DIRECTION('ref_axis',(1.,-2.40819858205088E-17,-1.46553589810128E-16));
#42349=DIRECTION('center_axis',(7.08949205856751E-14,-0.227955838450084,
0.973671472169396));
#42350=DIRECTION('ref_axis',(0.992732772337252,0.117171330155029,0.027432136579107));
#42351=DIRECTION('center_axis',(0.406568830313121,-0.889565491389124,-0.20826671060793));
#42352=DIRECTION('ref_axis',(-0.220907270377139,0.125476294051318,-0.967189576828488));
#42353=DIRECTION('center_axis',(-8.35086727472959E-14,0.227955838450079,
-0.973671472169397));
#42354=DIRECTION('ref_axis',(0.913629160773151,0.395844764797068,0.0926751248593784));
#42355=DIRECTION('center_axis',(0.749427187004001,-0.644656140376395,-0.150921675230167));
#42356=DIRECTION('ref_axis',(0.634043326955048,0.764428974922688,-0.116779286872384));
#42357=DIRECTION('center_axis',(3.46944695195141E-16,0.227955838450093,
-0.973671472169394));
#42358=DIRECTION('ref_axis',(1.,-6.63936891038671E-18,3.54771832349934E-16));
#42359=DIRECTION('center_axis',(-2.12030478187416E-14,0.950202644287033,
-0.311632692107118));
#42360=DIRECTION('ref_axis',(0.198472765334091,0.305433196953141,0.93129969591943));
#42361=DIRECTION('center_axis',(-5.55111512313038E-16,0.950202644287065,
-0.311632692107021));
#42362=DIRECTION('ref_axis',(1.,5.54555085240923E-16,-9.04006692102742E-17));
#42363=DIRECTION('center_axis',(-5.55111512313038E-16,0.950202644287065,
-0.311632692107021));
#42364=DIRECTION('ref_axis',(1.,5.52729018384727E-16,-9.59685496007145E-17));
#42365=DIRECTION('center_axis',(-0.206241528410022,0.304933168374568,0.929774270876617));
#42366=DIRECTION('ref_axis',(2.47601291321785E-8,-0.950202565004139,0.311632933849352));
#42367=DIRECTION('center_axis',(0.,1.,-7.7733519678E-16));
#42368=DIRECTION('ref_axis',(0.,-7.7733519678E-16,-1.));
#42369=DIRECTION('',(-1.,0.,0.));
#42370=DIRECTION('center_axis',(3.58723488914E-17,1.,-1.34708140773E-15));
#42371=DIRECTION('ref_axis',(1.,-3.58723488914E-17,4.83229742432088E-32));
#42372=DIRECTION('center_axis',(-1.,0.,0.));
#42373=DIRECTION('ref_axis',(0.,-1.,1.0842021724855E-15));
#42374=DIRECTION('',(-1.,0.,0.));
#42375=DIRECTION('center_axis',(0.,0.284628947689001,-0.958637763776001));
#42376=DIRECTION('ref_axis',(-1.,0.,0.));
#42377=DIRECTION('',(1.,0.,0.));
#42378=DIRECTION('center_axis',(1.05471187339E-15,0.284628947689001,-0.958637763776001));
#42379=DIRECTION('ref_axis',(1.,-2.4268872593874E-17,1.09301374232827E-15));
#42380=DIRECTION('center_axis',(-3.33066907388001E-16,0.284628947689001,
-0.958637763776001));
#42381=DIRECTION('ref_axis',(1.,7.90711700759394E-18,-3.45090007399474E-16));
#42382=DIRECTION('center_axis',(-1.,0.,0.));
#42383=DIRECTION('ref_axis',(0.,0.950202644287065,-0.31163269210702));
#42384=DIRECTION('',(1.,0.,0.));
#42385=DIRECTION('center_axis',(0.,0.950202644287065,-0.311632692107021));
#42386=DIRECTION('ref_axis',(-1.,0.,0.));
#42387=DIRECTION('center_axis',(-0.296636433707077,-0.948406798699881,0.111943603557285));
#42388=DIRECTION('ref_axis',(0.387977737402026,-0.0125716202918961,0.921583002037061));
#42389=DIRECTION('center_axis',(-0.424818360062199,-0.867834261877406,-0.257668498008121));
#42390=DIRECTION('ref_axis',(0.90527860957501,-0.407246922701095,-0.1209156027832));
#42391=DIRECTION('center_axis',(-0.391875379580097,-1.2252820670103E-15,
-0.920018307904226));
#42392=DIRECTION('ref_axis',(0.920018307904226,-1.05621218979234E-31,-0.391875379580097));
#42393=DIRECTION('center_axis',(-6.84827429158807E-14,0.284628947688994,
-0.958637763776003));
#42394=DIRECTION('ref_axis',(0.996284914443996,0.0825562971465005,0.0245117737583));
#42395=DIRECTION('center_axis',(-0.193028156853976,-0.94060906825824,-0.279275332551807));
#42396=DIRECTION('ref_axis',(1.51496469073372E-7,-0.284628303088786,0.958637955163875));
#42397=DIRECTION('center_axis',(-4.98308895405631E-6,0.284630761188568,
-0.958637225315388));
#42398=DIRECTION('ref_axis',(0.905278651982129,-0.407245323311114,-0.120920671957466));
#42399=DIRECTION('center_axis',(0.877582561890373,-0.479425538604203,0.));
#42400=DIRECTION('ref_axis',(0.479425538604203,0.877582561890373,0.));
#42401=DIRECTION('center_axis',(3.15330923650249E-6,0.28462980062271,-0.958637510526024));
#42402=DIRECTION('ref_axis',(-0.981193104700328,-0.185043702214525,-0.0549446954607343));
#42403=DIRECTION('center_axis',(5.98055361294049E-17,1.09473299575306E-16,
-1.));
#42404=DIRECTION('ref_axis',(-0.479425538604203,-0.877582561890373,-1.24744160070242E-16));
#42405=DIRECTION('center_axis',(3.58723488914E-17,1.,-1.34708140773E-15));
#42406=DIRECTION('ref_axis',(1.,-3.58723488914E-17,4.83229742432088E-32));
#42407=DIRECTION('center_axis',(8.32667268468611E-17,0.419820362992804,
0.907607218358575));
#42408=DIRECTION('ref_axis',(1.,-5.3020129034611E-18,-8.92906449242453E-17));
#42409=DIRECTION('center_axis',(-1.,-6.06243811038E-15,2.950331972E-15));
#42410=DIRECTION('ref_axis',(6.06243811038E-15,-1.,1.52149577650908E-31));
#42411=DIRECTION('center_axis',(-1.,0.,0.));
#42412=DIRECTION('ref_axis',(0.,1.,0.));
#42413=DIRECTION('center_axis',(3.88578058619201E-16,-0.687200931805355,
0.726467397290375));
#42414=DIRECTION('ref_axis',(1.,1.21921474786958E-16,-4.19555658898608E-16));
#42415=DIRECTION('center_axis',(-1.,3.92975632019E-15,5.94636008283E-15));
#42416=DIRECTION('ref_axis',(-3.92975632019E-15,-1.,5.15343103553154E-31));
#42417=DIRECTION('center_axis',(1.,-8.01620055713E-15,-2.35928728678E-15));
#42418=DIRECTION('ref_axis',(8.01620055713E-15,1.,4.56601977004064E-32));
#42419=DIRECTION('center_axis',(0.,-0.687200931805355,0.726467397290375));
#42420=DIRECTION('ref_axis',(1.,0.,0.));
#42421=DIRECTION('center_axis',(1.,0.,0.));
#42422=DIRECTION('ref_axis',(0.,1.,0.));
#42423=DIRECTION('center_axis',(1.,0.,0.));
#42424=DIRECTION('ref_axis',(0.,1.,0.));
#42425=DIRECTION('center_axis',(0.,0.,1.));
#42426=DIRECTION('ref_axis',(1.,0.,0.));
#42427=DIRECTION('center_axis',(-0.391875379580097,1.25339704769031E-15,
0.920018307904226));
#42428=DIRECTION('ref_axis',(0.920018307904226,2.69771308214058E-31,0.391875379580097));
#42429=DIRECTION('center_axis',(-0.424818360062199,0.867834261877406,0.257668498008121));
#42430=DIRECTION('ref_axis',(0.90527860957501,0.407246922701095,0.1209156027832));
#42431=DIRECTION('center_axis',(2.92163435282501E-13,0.284628947689245,
-0.958637763775929));
#42432=DIRECTION('ref_axis',(-0.752005368733267,-0.631892774094225,-0.187615157820067));
#42433=DIRECTION('center_axis',(-0.193028626051129,0.940608766817842,0.279276023514787));
#42434=DIRECTION('ref_axis',(1.14724600190167E-8,-0.284629003337217,0.958637747253498));
#42435=DIRECTION('center_axis',(-3.34855995114163E-16,1.,-1.24757595645316E-15));
#42436=DIRECTION('ref_axis',(0.965815610620677,0.,-0.259230025809914));
#42437=DIRECTION('center_axis',(1.,0.,0.));
#42438=DIRECTION('ref_axis',(0.,1.,0.));
#42439=DIRECTION('center_axis',(-1.,0.,0.));
#42440=DIRECTION('ref_axis',(0.,1.,0.));
#42441=DIRECTION('center_axis',(1.,0.,0.));
#42442=DIRECTION('ref_axis',(0.,1.,0.));
#42443=DIRECTION('',(1.,0.,0.));
#42444=DIRECTION('center_axis',(1.,0.,0.));
#42445=DIRECTION('ref_axis',(0.,1.,0.));
#42446=DIRECTION('center_axis',(1.,0.,0.));
#42447=DIRECTION('ref_axis',(0.,1.,0.));
#42448=DIRECTION('center_axis',(-1.,0.,0.));
#42449=DIRECTION('ref_axis',(0.,1.,0.));
#42450=DIRECTION('',(0.,-1.,0.));
#42451=DIRECTION('center_axis',(-1.,0.,0.));
#42452=DIRECTION('ref_axis',(0.,1.,0.));
#42453=DIRECTION('',(0.,0.,-1.));
#42454=DIRECTION('center_axis',(-1.,0.,0.));
#42455=DIRECTION('ref_axis',(0.,1.,0.));
#42456=DIRECTION('',(0.,1.,0.));
#42457=DIRECTION('center_axis',(1.,0.,0.));
#42458=DIRECTION('ref_axis',(0.,1.,0.));
#42459=DIRECTION('',(0.,0.901003410349976,-0.433812003680988));
#42460=DIRECTION('center_axis',(8.58451173878204E-29,0.901003410349976,
-0.433812003680988));
#42461=DIRECTION('ref_axis',(-1.,7.73467435283202E-29,-3.724064238024E-29));
#42462=DIRECTION('center_axis',(0.,0.901003410349976,-0.433812003680988));
#42463=DIRECTION('ref_axis',(1.,0.,0.));
#42464=DIRECTION('',(0.,0.901003410349976,-0.433812003680988));
#42465=DIRECTION('center_axis',(-3.70762016608926E-8,0.901003426429784,
-0.433811970284118));
#42466=DIRECTION('ref_axis',(0.707106729560538,0.306751431965231,0.637105667842847));
#42467=DIRECTION('center_axis',(1.,0.,0.));
#42468=DIRECTION('ref_axis',(0.,-0.433812003680988,-0.901003410349975));
#42469=DIRECTION('center_axis',(0.,1.,0.));
#42470=DIRECTION('ref_axis',(1.,0.,0.));
#42471=DIRECTION('center_axis',(1.,0.,0.));
#42472=DIRECTION('ref_axis',(0.,1.,0.));
#42473=DIRECTION('center_axis',(0.,1.,0.));
#42474=DIRECTION('ref_axis',(-1.,0.,0.));
#42475=DIRECTION('center_axis',(0.,1.,-6.12323399574E-17));
#42476=DIRECTION('ref_axis',(1.,0.,0.));
#42477=DIRECTION('',(0.,1.,0.));
#42478=DIRECTION('center_axis',(0.,0.,-1.));
#42479=DIRECTION('ref_axis',(1.,0.,0.));
#42480=DIRECTION('center_axis',(-1.,0.,0.));
#42481=DIRECTION('ref_axis',(0.,1.,0.));
#42482=DIRECTION('center_axis',(0.,0.,-1.));
#42483=DIRECTION('ref_axis',(-1.,0.,0.));
#42484=DIRECTION('center_axis',(0.,-6.12323399574E-17,-1.));
#42485=DIRECTION('ref_axis',(1.,0.,0.));
#42486=DIRECTION('',(0.,0.,-1.));
#42487=DIRECTION('center_axis',(0.,-1.,0.));
#42488=DIRECTION('ref_axis',(1.,0.,0.));
#42489=DIRECTION('center_axis',(-1.,0.,0.));
#42490=DIRECTION('ref_axis',(0.,1.,0.));
#42491=DIRECTION('center_axis',(0.,-1.,0.));
#42492=DIRECTION('ref_axis',(-1.,0.,0.));
#42493=DIRECTION('center_axis',(0.,-1.,0.));
#42494=DIRECTION('ref_axis',(0.,0.,-1.));
#42495=DIRECTION('',(0.,-1.,0.));
#42496=DIRECTION('center_axis',(1.,0.,0.));
#42497=DIRECTION('ref_axis',(0.,0.107526881719979,-0.994202177480807));
#42498=DIRECTION('center_axis',(0.,0.994202177480807,-0.107526881719979));
#42499=DIRECTION('ref_axis',(1.,0.,0.));
#42500=DIRECTION('center_axis',(-1.,0.,0.));
#42501=DIRECTION('ref_axis',(0.,1.,0.));
#42502=DIRECTION('center_axis',(0.,-0.994202177480807,-0.107526881719979));
#42503=DIRECTION('ref_axis',(1.,0.,0.));
#42504=DIRECTION('center_axis',(0.,0.433812003680988,0.901003410349976));
#42505=DIRECTION('ref_axis',(1.,0.,0.));
#42506=DIRECTION('',(0.,-0.901003410349976,0.433812003680988));
#42507=DIRECTION('',(-1.,0.,0.));
#42508=DIRECTION('',(1.,0.,0.));
#42509=DIRECTION('center_axis',(-0.0103217669355549,0.900955491125921,-0.433788732146629));
#42510=DIRECTION('ref_axis',(0.72659105028404,0.304799044389358,0.615762119804774));
#42511=DIRECTION('center_axis',(1.,0.,0.));
#42512=DIRECTION('ref_axis',(0.,-0.433812003680988,-0.901003410349976));
#42513=DIRECTION('',(1.,0.,0.));
#42514=DIRECTION('center_axis',(-1.,0.,0.));
#42515=DIRECTION('ref_axis',(0.,1.,0.));
#42516=DIRECTION('center_axis',(0.,0.,1.));
#42517=DIRECTION('ref_axis',(1.,0.,0.));
#42518=DIRECTION('',(0.,-1.,0.));
#42519=DIRECTION('',(-1.,0.,0.));
#42520=DIRECTION('center_axis',(1.,0.,0.));
#42521=DIRECTION('ref_axis',(0.,1.,0.));
#42522=DIRECTION('center_axis',(1.,0.,0.));
#42523=DIRECTION('ref_axis',(0.,1.,0.));
#42524=DIRECTION('',(-1.,0.,0.));
#42525=DIRECTION('center_axis',(0.,1.,0.));
#42526=DIRECTION('ref_axis',(1.,0.,0.));
#42527=DIRECTION('',(0.,0.,1.));
#42528=DIRECTION('',(-1.,0.,0.));
#42529=DIRECTION('center_axis',(1.,0.,0.));
#42530=DIRECTION('ref_axis',(0.,0.,-1.));
#42531=DIRECTION('center_axis',(1.,0.,0.));
#42532=DIRECTION('ref_axis',(0.,1.,0.));
#42533=DIRECTION('',(-1.,0.,0.));
#42534=DIRECTION('center_axis',(-0.0173651268263312,-0.999849214817067,
1.68859670582999E-8));
#42535=DIRECTION('ref_axis',(0.760990240424013,-0.0132166958731909,-0.648628686483722));
#42536=DIRECTION('center_axis',(0.,0.,1.));
#42537=DIRECTION('ref_axis',(1.,0.,0.));
#42538=DIRECTION('',(-1.,0.,0.));
#42539=DIRECTION('',(0.,-1.,0.));
#42540=DIRECTION('',(-1.,0.,0.));
#42541=DIRECTION('',(0.,1.,0.));
#42542=DIRECTION('center_axis',(0.0118198477658594,0.999930143159405,-6.38623129917418E-8));
#42543=DIRECTION('ref_axis',(0.727757019739868,-0.00860253433416321,0.685781099639218));
#42544=DIRECTION('center_axis',(0.0173638215992654,0.999849237484397,1.1573889087489E-6));
#42545=DIRECTION('ref_axis',(0.761020343050589,-0.0132169647677628,0.64859336205784));
#42546=DIRECTION('center_axis',(1.,0.,0.));
#42547=DIRECTION('ref_axis',(0.,-1.,0.));
#42548=DIRECTION('center_axis',(1.,0.,0.));
#42549=DIRECTION('ref_axis',(0.,-2.09002828430941E-15,-1.));
#42550=DIRECTION('center_axis',(-1.,0.,0.));
#42551=DIRECTION('ref_axis',(0.,1.,0.));
#42552=DIRECTION('',(1.,0.,0.));
#42553=DIRECTION('',(1.,0.,0.));
#42554=DIRECTION('center_axis',(1.,0.,0.));
#42555=DIRECTION('ref_axis',(0.,-1.,0.));
#42556=DIRECTION('center_axis',(-9.62964972193618E-33,-0.901003410349976,
0.433812003680988));
#42557=DIRECTION('ref_axis',(-6.43494414306736E-48,-0.433812003680988,-0.901003410349976));
#42558=DIRECTION('center_axis',(0.,-0.901003410349976,0.433812003680988));
#42559=DIRECTION('ref_axis',(1.,0.,0.));
#42560=DIRECTION('',(0.,-0.901003410349976,0.433812003680988));
#42561=DIRECTION('center_axis',(0.,-0.901003410349976,0.433812003680988));
#42562=DIRECTION('ref_axis',(1.,0.,0.));
#42563=DIRECTION('center_axis',(1.,0.,0.));
#42564=DIRECTION('ref_axis',(0.,0.433812003680988,0.901003410349976));
#42565=DIRECTION('center_axis',(1.,0.,0.));
#42566=DIRECTION('ref_axis',(0.,1.,0.));
#42567=DIRECTION('',(-1.,0.,0.));
#42568=DIRECTION('center_axis',(1.,0.,0.));
#42569=DIRECTION('ref_axis',(0.,-0.433812003680988,-0.901003410349975));
#42570=DIRECTION('center_axis',(0.,-1.,0.));
#42571=DIRECTION('ref_axis',(1.,0.,0.));
#42572=DIRECTION('center_axis',(-1.,0.,0.));
#42573=DIRECTION('ref_axis',(0.,1.,0.));
#42574=DIRECTION('center_axis',(0.,-1.,0.));
#42575=DIRECTION('ref_axis',(0.,0.,-1.));
#42576=DIRECTION('center_axis',(0.,-1.,-2.50640329593E-15));
#42577=DIRECTION('ref_axis',(1.,0.,0.));
#42578=DIRECTION('',(0.,-1.,0.));
#42579=DIRECTION('center_axis',(1.,0.,0.));
#42580=DIRECTION('ref_axis',(0.,1.,-1.26882631385732E-15));
#42581=DIRECTION('center_axis',(0.,0.,1.));
#42582=DIRECTION('ref_axis',(1.,0.,0.));
#42583=DIRECTION('center_axis',(1.,0.,0.));
#42584=DIRECTION('ref_axis',(0.,1.,0.));
#42585=DIRECTION('center_axis',(0.,0.,1.));
#42586=DIRECTION('ref_axis',(0.,-1.,0.));
#42587=DIRECTION('center_axis',(0.,6.53351286424E-16,1.));
#42588=DIRECTION('ref_axis',(1.,0.,0.));
#42589=DIRECTION('',(0.,0.,1.));
#42590=DIRECTION('center_axis',(1.,0.,0.));
#42591=DIRECTION('ref_axis',(0.,6.34413156928661E-16,-1.));
#42592=DIRECTION('center_axis',(0.,1.,0.));
#42593=DIRECTION('ref_axis',(1.,0.,0.));
#42594=DIRECTION('center_axis',(1.,0.,0.));
#42595=DIRECTION('ref_axis',(0.,1.,0.));
#42596=DIRECTION('center_axis',(-1.,1.38625597078213E-8,-8.47275514856299E-9));
#42597=DIRECTION('ref_axis',(8.4755411535573E-9,0.000200933695293934,-0.999999979812825));
#42598=DIRECTION('center_axis',(1.,0.,0.));
#42599=DIRECTION('ref_axis',(0.,0.,-1.));
#42600=DIRECTION('center_axis',(-1.,0.,0.));
#42601=DIRECTION('ref_axis',(0.,-1.,0.));
#42602=DIRECTION('',(-1.,0.,0.));
#42603=DIRECTION('center_axis',(0.,1.,0.));
#42604=DIRECTION('ref_axis',(0.,0.,-1.));
#42605=DIRECTION('',(0.,-1.,0.));
#42606=DIRECTION('center_axis',(0.,-1.,1.11022302463E-16));
#42607=DIRECTION('ref_axis',(1.,0.,0.));
#42608=DIRECTION('center_axis',(0.,-1.,-9.25185853854E-17));
#42609=DIRECTION('ref_axis',(1.,0.,0.));
#42610=DIRECTION('center_axis',(1.,0.,0.));
#42611=DIRECTION('ref_axis',(0.,-0.419820362992804,-0.907607218358575));
#42612=DIRECTION('center_axis',(1.,0.,0.));
#42613=DIRECTION('ref_axis',(0.,1.,0.));
#42614=DIRECTION('center_axis',(-1.,0.,0.));
#42615=DIRECTION('ref_axis',(0.,1.,0.));
#42616=DIRECTION('',(-1.,0.,0.));
#42617=DIRECTION('center_axis',(0.,-1.,0.));
#42618=DIRECTION('ref_axis',(1.,0.,0.));
#42619=DIRECTION('center_axis',(0.,1.,-5.55111512313E-17));
#42620=DIRECTION('ref_axis',(1.,0.,0.));
#42621=DIRECTION('',(0.,1.,0.));
#42622=DIRECTION('center_axis',(0.,0.,1.));
#42623=DIRECTION('ref_axis',(1.,0.,0.));
#42624=DIRECTION('',(0.,-1.,0.));
#42625=DIRECTION('',(-1.,0.,0.));
#42626=DIRECTION('',(0.,1.,0.));
#42627=DIRECTION('',(1.,0.,0.));
#42628=DIRECTION('center_axis',(1.,-1.76684878881754E-8,-1.39105393592899E-8));
#42629=DIRECTION('ref_axis',(1.39140895830399E-8,0.00020093320508201,0.999999979812923));
#42630=DIRECTION('center_axis',(-1.,0.,0.));
#42631=DIRECTION('ref_axis',(0.,-0.107526881719978,-0.994202177480807));
#42632=DIRECTION('',(1.,0.,0.));
#42633=DIRECTION('center_axis',(1.,0.,0.));
#42634=DIRECTION('ref_axis',(0.,1.,0.));
#42635=DIRECTION('center_axis',(1.,0.,0.));
#42636=DIRECTION('ref_axis',(0.,0.107526881719979,-0.994202177480807));
#42637=DIRECTION('center_axis',(-1.,0.,0.));
#42638=DIRECTION('ref_axis',(0.,1.,0.));
#42639=DIRECTION('center_axis',(0.,-0.994202177480807,-0.107526881719979));
#42640=DIRECTION('ref_axis',(1.,0.,0.));
#42641=DIRECTION('center_axis',(0.,0.994202177480807,-0.107526881719979));
#42642=DIRECTION('ref_axis',(1.,0.,0.));
#42643=DIRECTION('center_axis',(-1.,0.,0.));
#42644=DIRECTION('ref_axis',(0.,-1.,0.));
#42645=DIRECTION('center_axis',(1.,0.,0.));
#42646=DIRECTION('ref_axis',(0.,1.,0.));
#42647=DIRECTION('center_axis',(1.,0.,0.));
#42648=DIRECTION('ref_axis',(0.,0.433812003680988,0.901003410349976));
#42649=DIRECTION('center_axis',(1.,0.,0.));
#42650=DIRECTION('ref_axis',(0.,1.,0.));
#42651=DIRECTION('center_axis',(0.,-1.,0.));
#42652=DIRECTION('ref_axis',(1.,0.,0.));
#42653=DIRECTION('center_axis',(1.,0.,0.));
#42654=DIRECTION('ref_axis',(0.,1.,0.));
#42655=DIRECTION('',(0.,0.,-1.));
#42656=DIRECTION('center_axis',(1.,0.,0.));
#42657=DIRECTION('ref_axis',(0.,1.,0.));
#42658=DIRECTION('',(0.,-1.,0.));
#42659=DIRECTION('',(0.,0.,-1.));
#42660=DIRECTION('',(0.,1.,0.));
#42661=DIRECTION('center_axis',(1.,0.,0.));
#42662=DIRECTION('ref_axis',(0.,1.,0.));
#42663=DIRECTION('',(0.,0.,-1.));
#42664=DIRECTION('',(0.,1.,0.));
#42665=DIRECTION('',(0.,0.57980236498199,0.814757152506986));
#42666=DIRECTION('center_axis',(1.,0.,0.));
#42667=DIRECTION('ref_axis',(0.,1.,0.));
#42668=DIRECTION('',(0.,1.,0.));
#42669=DIRECTION('center_axis',(1.,0.,0.));
#42670=DIRECTION('ref_axis',(0.,1.,0.));
#42671=DIRECTION('',(0.,0.908754086213215,-0.417332015056099));
#42672=DIRECTION('center_axis',(-1.,0.,0.));
#42673=DIRECTION('ref_axis',(0.,1.,0.));
#42674=DIRECTION('',(0.,1.,0.));
#42675=DIRECTION('center_axis',(-1.,0.,0.));
#42676=DIRECTION('ref_axis',(0.,1.,0.));
#42677=DIRECTION('',(0.,0.726467397290375,0.687200931805355));
#42678=DIRECTION('center_axis',(-1.,0.,0.));
#42679=DIRECTION('ref_axis',(0.,1.,0.));
#42680=DIRECTION('center_axis',(1.,0.,0.));
#42681=DIRECTION('ref_axis',(0.,1.,0.));
#42682=DIRECTION('',(0.,-0.86428986298992,0.502994068287953));
#42683=DIRECTION('center_axis',(-1.,0.,0.));
#42684=DIRECTION('ref_axis',(0.,1.,0.));
#42685=DIRECTION('',(0.,-0.726467397290375,-0.687200931805355));
#42686=DIRECTION('center_axis',(1.,0.,0.));
#42687=DIRECTION('ref_axis',(0.,1.,0.));
#42688=DIRECTION('',(0.,-1.,0.));
#42689=DIRECTION('center_axis',(1.,0.,0.));
#42690=DIRECTION('ref_axis',(0.,1.,0.));
#42691=DIRECTION('',(0.,0.907607218358575,-0.419820362992804));
#42692=DIRECTION('center_axis',(-1.,0.,0.));
#42693=DIRECTION('ref_axis',(0.,1.,0.));
#42694=DIRECTION('',(0.,0.973671472169394,0.227955838450093));
#42695=DIRECTION('center_axis',(1.,0.,0.));
#42696=DIRECTION('ref_axis',(0.,1.,0.));
#42697=DIRECTION('center_axis',(-1.,0.,0.));
#42698=DIRECTION('ref_axis',(0.,1.,0.));
#42699=DIRECTION('',(0.,-0.907607218358575,0.419820362992804));
#42700=DIRECTION('center_axis',(-1.,0.,0.));
#42701=DIRECTION('ref_axis',(0.,1.,0.));
#42702=DIRECTION('',(0.,-1.,0.));
#42703=DIRECTION('center_axis',(0.,0.,1.));
#42704=DIRECTION('ref_axis',(1.,0.,0.));
#42705=DIRECTION('center_axis',(0.,-0.367447999014073,-0.930044067784185));
#42706=DIRECTION('ref_axis',(1.,0.,0.));
#42707=DIRECTION('center_axis',(1.,0.,0.));
#42708=DIRECTION('ref_axis',(0.,0.925572441975634,-0.37857054118785));
#42709=DIRECTION('center_axis',(-4.71844785466072E-16,-0.319261680225049,
-0.947666597248145));
#42710=DIRECTION('ref_axis',(1.,-4.12988579863361E-17,-4.83988402678584E-16));
#42711=DIRECTION('center_axis',(-1.,0.,0.));
#42712=DIRECTION('ref_axis',(0.,1.,0.));
#42713=DIRECTION('center_axis',(1.11022302463028E-15,0.0845895878810212,
-0.996415877845249));
#42714=DIRECTION('ref_axis',(1.,2.79313681155602E-17,1.11658771431272E-15));
#42715=DIRECTION('center_axis',(1.,0.,0.));
#42716=DIRECTION('ref_axis',(0.,1.,0.));
#42717=DIRECTION('center_axis',(1.,0.,0.));
#42718=DIRECTION('ref_axis',(0.,1.,0.));
#42719=DIRECTION('',(0.,-0.907607218358575,0.419820362992804));
#42720=DIRECTION('center_axis',(-1.,0.,0.));
#42721=DIRECTION('ref_axis',(0.,1.,0.));
#42722=DIRECTION('center_axis',(1.,0.,0.));
#42723=DIRECTION('ref_axis',(0.,1.,0.));
#42724=DIRECTION('center_axis',(1.,0.,0.));
#42725=DIRECTION('ref_axis',(0.,1.,0.));
#42726=DIRECTION('',(0.,1.,0.));
#42727=DIRECTION('center_axis',(-1.,0.,0.));
#42728=DIRECTION('ref_axis',(0.,1.,0.));
#42729=DIRECTION('',(0.,0.726467397290375,0.687200931805355));
#42730=DIRECTION('center_axis',(-1.,0.,0.));
#42731=DIRECTION('ref_axis',(0.,1.,0.));
#42732=DIRECTION('center_axis',(1.,0.,0.));
#42733=DIRECTION('ref_axis',(0.,-0.419820362992804,-0.907607218358575));
#42734=DIRECTION('center_axis',(0.,-0.907607218358575,0.419820362992804));
#42735=DIRECTION('ref_axis',(1.,0.,0.));
#42736=DIRECTION('center_axis',(0.,0.419820362992804,0.907607218358575));
#42737=DIRECTION('ref_axis',(1.,0.,0.));
#42738=DIRECTION('',(0.,-0.907607218358575,0.419820362992804));
#42739=DIRECTION('',(-1.,0.,0.));
#42740=DIRECTION('',(0.,0.907607218358575,-0.419820362992804));
#42741=DIRECTION('center_axis',(1.,0.,0.));
#42742=DIRECTION('ref_axis',(0.,-0.419820362992804,-0.907607218358575));
#42743=DIRECTION('center_axis',(0.,0.907607218358575,-0.419820362992804));
#42744=DIRECTION('ref_axis',(1.,0.,0.));
#42745=DIRECTION('center_axis',(0.,-1.,0.));
#42746=DIRECTION('ref_axis',(0.,0.,1.));
#42747=DIRECTION('center_axis',(0.,1.,6.36065274525E-16));
#42748=DIRECTION('ref_axis',(1.,0.,0.));
#42749=DIRECTION('center_axis',(0.,1.,1.7763568394E-15));
#42750=DIRECTION('ref_axis',(1.,0.,0.));
#42751=DIRECTION('center_axis',(1.,0.,0.));
#42752=DIRECTION('ref_axis',(0.,0.930044067784185,0.367447999014073));
#42753=DIRECTION('center_axis',(-1.,0.,0.));
#42754=DIRECTION('ref_axis',(0.,-1.,0.));
#42755=DIRECTION('center_axis',(1.,0.,0.));
#42756=DIRECTION('ref_axis',(0.,0.,1.));
#42757=DIRECTION('center_axis',(1.,0.,0.));
#42758=DIRECTION('ref_axis',(0.,1.,0.));
#42759=DIRECTION('',(-1.,0.,0.));
#42760=DIRECTION('center_axis',(-1.,0.,0.));
#42761=DIRECTION('ref_axis',(0.,1.,0.));
#42762=DIRECTION('center_axis',(0.,-1.,0.));
#42763=DIRECTION('ref_axis',(0.,0.,-1.));
#42764=DIRECTION('center_axis',(0.,-1.,-1.614869854E-15));
#42765=DIRECTION('ref_axis',(1.,0.,0.));
#42766=DIRECTION('center_axis',(1.,0.,0.));
#42767=DIRECTION('ref_axis',(0.,-0.930044067784185,-0.367447999014073));
#42768=DIRECTION('center_axis',(0.,0.367447999014073,-0.930044067784185));
#42769=DIRECTION('ref_axis',(1.,0.,0.));
#42770=DIRECTION('center_axis',(1.,0.,0.));
#42771=DIRECTION('ref_axis',(0.,-0.107526881719979,0.994202177480807));
#42772=DIRECTION('center_axis',(0.,-1.,0.));
#42773=DIRECTION('ref_axis',(0.,0.,-1.));
#42774=DIRECTION('center_axis',(0.,-1.,-3.99680288865E-15));
#42775=DIRECTION('ref_axis',(1.,0.,0.));
#42776=DIRECTION('',(0.,-1.,0.));
#42777=DIRECTION('center_axis',(0.,0.707106781186548,0.707106781186548));
#42778=DIRECTION('ref_axis',(0.,0.707106781186548,-0.707106781186548));
#42779=DIRECTION('center_axis',(1.,0.,0.));
#42780=DIRECTION('ref_axis',(0.,-0.419820362992805,-0.907607218358575));
#42781=DIRECTION('center_axis',(0.,-0.907607218358575,0.419820362992804));
#42782=DIRECTION('ref_axis',(1.,0.,0.));
#42783=DIRECTION('center_axis',(-1.,0.,0.));
#42784=DIRECTION('ref_axis',(0.,1.,0.));
#42785=DIRECTION('center_axis',(1.92592994438724E-32,-0.907607218358575,
0.419820362992804));
#42786=DIRECTION('ref_axis',(2.4880840830811E-46,-0.419820362992804,-0.907607218358575));
#42787=DIRECTION('center_axis',(0.,-0.907607218358575,0.419820362992804));
#42788=DIRECTION('ref_axis',(1.,0.,0.));
#42789=DIRECTION('',(0.,-0.907607218358575,0.419820362992804));
#42790=DIRECTION('center_axis',(1.,0.,0.));
#42791=DIRECTION('ref_axis',(0.,-0.72739643298632,0.686217479578288));
#42792=DIRECTION('center_axis',(0.,0.686217479578295,0.727396432986313));
#42793=DIRECTION('ref_axis',(1.,0.,0.));
#42794=DIRECTION('center_axis',(-1.,0.,0.));
#42795=DIRECTION('ref_axis',(0.,-1.,0.));
#42796=DIRECTION('center_axis',(1.,0.,0.));
#42797=DIRECTION('ref_axis',(0.,0.727396432986313,-0.686217479578295));
#42798=DIRECTION('center_axis',(0.,0.672677186066802,0.739936080580782));
#42799=DIRECTION('ref_axis',(1.,0.,0.));
#42800=DIRECTION('center_axis',(1.,0.,0.));
#42801=DIRECTION('ref_axis',(0.,1.,0.));
#42802=DIRECTION('center_axis',(0.,0.973671472169394,0.227955838450093));
#42803=DIRECTION('ref_axis',(0.,-0.227955838450093,0.973671472169394));
#42804=DIRECTION('center_axis',(0.,0.973671472169394,0.227955838450093));
#42805=DIRECTION('ref_axis',(1.,0.,0.));
#42806=DIRECTION('center_axis',(0.,0.973671472169394,0.227955838450093));
#42807=DIRECTION('ref_axis',(1.,0.,0.));
#42808=DIRECTION('',(0.,0.973671472169394,0.227955838450093));
#42809=DIRECTION('center_axis',(1.,0.,0.));
#42810=DIRECTION('ref_axis',(0.,0.419820362992802,0.907607218358576));
#42811=DIRECTION('center_axis',(0.,0.907607218358575,-0.419820362992804));
#42812=DIRECTION('ref_axis',(1.,0.,0.));
#42813=DIRECTION('center_axis',(-1.,0.,0.));
#42814=DIRECTION('ref_axis',(0.,-1.,0.));
#42815=DIRECTION('center_axis',(0.,-0.907607218358575,0.419820362992804));
#42816=DIRECTION('ref_axis',(1.,0.,0.));
#42817=DIRECTION('center_axis',(1.,0.,0.));
#42818=DIRECTION('ref_axis',(0.,0.,1.));
#42819=DIRECTION('center_axis',(0.,-0.726467397290375,-0.687200931805355));
#42820=DIRECTION('ref_axis',(1.,0.,0.));
#42821=DIRECTION('center_axis',(1.92592994438724E-32,-0.726467397290375,
-0.687200931805355));
#42822=DIRECTION('ref_axis',(-2.06468201548131E-46,0.687200931805355,-0.726467397290375));
#42823=DIRECTION('center_axis',(0.,-0.726467397290375,-0.687200931805355));
#42824=DIRECTION('ref_axis',(1.,0.,0.));
#42825=DIRECTION('',(0.,-0.726467397290375,-0.687200931805355));
#42826=DIRECTION('center_axis',(1.,0.,0.));
#42827=DIRECTION('ref_axis',(0.,-0.502994068287954,-0.864289862989919));
#42828=DIRECTION('center_axis',(0.,-0.86428986298992,0.502994068287953));
#42829=DIRECTION('ref_axis',(1.,0.,0.));
#42830=DIRECTION('center_axis',(-1.,0.,0.));
#42831=DIRECTION('ref_axis',(0.,-1.,0.));
#42832=DIRECTION('center_axis',(-9.62964972193618E-33,-0.86428986298992,
0.502994068287953));
#42833=DIRECTION('ref_axis',(-4.62384107026404E-47,-0.502994068287953,-0.86428986298992));
#42834=DIRECTION('center_axis',(0.,-0.86428986298992,0.502994068287953));
#42835=DIRECTION('ref_axis',(1.,0.,0.));
#42836=DIRECTION('',(0.,-0.86428986298992,0.502994068287953));
#42837=DIRECTION('center_axis',(1.,0.,0.));
#42838=DIRECTION('ref_axis',(0.,0.96323191500603,0.268671319485009));
#42839=DIRECTION('center_axis',(0.,-0.268671319485009,0.96323191500603));
#42840=DIRECTION('ref_axis',(1.,0.,0.));
#42841=DIRECTION('center_axis',(0.,-0.403636513060188,0.914919431056425));
#42842=DIRECTION('ref_axis',(1.,0.,0.));
#42843=DIRECTION('center_axis',(1.,0.,0.));
#42844=DIRECTION('ref_axis',(0.,1.,0.));
#42845=DIRECTION('center_axis',(1.,0.,0.));
#42846=DIRECTION('ref_axis',(0.,-0.687200931805354,0.726467397290377));
#42847=DIRECTION('center_axis',(0.,0.726467397290375,0.687200931805355));
#42848=DIRECTION('ref_axis',(1.,0.,0.));
#42849=DIRECTION('center_axis',(-1.,0.,0.));
#42850=DIRECTION('ref_axis',(0.,1.,0.));
#42851=DIRECTION('center_axis',(0.,-0.726467397290375,-0.687200931805355));
#42852=DIRECTION('ref_axis',(1.,0.,0.));
#42853=DIRECTION('center_axis',(0.,0.726467397290375,0.687200931805355));
#42854=DIRECTION('ref_axis',(1.,0.,0.));
#42855=DIRECTION('',(0.,0.726467397290375,0.687200931805355));
#42856=DIRECTION('center_axis',(1.,0.,0.));
#42857=DIRECTION('ref_axis',(0.,-3.5527136788005E-15,1.));
#42858=DIRECTION('center_axis',(0.,1.,0.));
#42859=DIRECTION('ref_axis',(1.,0.,0.));
#42860=DIRECTION('center_axis',(-1.,0.,0.));
#42861=DIRECTION('ref_axis',(0.,1.,0.));
#42862=DIRECTION('center_axis',(0.,-1.,0.));
#42863=DIRECTION('ref_axis',(1.,0.,0.));
#42864=DIRECTION('center_axis',(0.,1.,-4.99600361081E-16));
#42865=DIRECTION('ref_axis',(1.,0.,0.));
#42866=DIRECTION('',(0.,1.,0.));
#42867=DIRECTION('center_axis',(1.,0.,0.));
#42868=DIRECTION('ref_axis',(0.,0.417332015056099,0.908754086213215));
#42869=DIRECTION('center_axis',(0.,0.908754086213215,-0.417332015056099));
#42870=DIRECTION('ref_axis',(1.,0.,0.));
#42871=DIRECTION('center_axis',(-1.,0.,0.));
#42872=DIRECTION('ref_axis',(0.,1.,0.));
#42873=DIRECTION('center_axis',(0.,-0.908754086213215,0.417332015056099));
#42874=DIRECTION('ref_axis',(1.,0.,0.));
#42875=DIRECTION('center_axis',(0.,0.908754086213215,-0.417332015056099));
#42876=DIRECTION('ref_axis',(1.,0.,0.));
#42877=DIRECTION('',(0.,0.908754086213215,-0.417332015056099));
#42878=DIRECTION('center_axis',(1.,0.,0.));
#42879=DIRECTION('ref_axis',(0.,-0.417332015056099,-0.908754086213215));
#42880=DIRECTION('center_axis',(0.,1.,0.));
#42881=DIRECTION('ref_axis',(1.,0.,0.));
#42882=DIRECTION('center_axis',(1.,0.,0.));
#42883=DIRECTION('ref_axis',(0.,1.,0.));
#42884=DIRECTION('center_axis',(0.,-1.,0.));
#42885=DIRECTION('ref_axis',(1.,0.,0.));
#42886=DIRECTION('center_axis',(0.,1.,7.40148683083E-16));
#42887=DIRECTION('ref_axis',(1.,0.,0.));
#42888=DIRECTION('',(0.,1.,0.));
#42889=DIRECTION('center_axis',(1.,0.,0.));
#42890=DIRECTION('ref_axis',(0.,-2.53765262771464E-15,-1.));
#42891=DIRECTION('center_axis',(0.,0.57980236498199,0.814757152506986));
#42892=DIRECTION('ref_axis',(1.,0.,0.));
#42893=DIRECTION('center_axis',(1.,0.,0.));
#42894=DIRECTION('ref_axis',(0.,1.,0.));
#42895=DIRECTION('center_axis',(0.,-0.57980236498199,-0.814757152506986));
#42896=DIRECTION('ref_axis',(1.,0.,0.));
#42897=DIRECTION('center_axis',(0.,0.57980236498199,0.814757152506986));
#42898=DIRECTION('ref_axis',(1.,0.,0.));
#42899=DIRECTION('',(0.,0.57980236498199,0.814757152506986));
#42900=DIRECTION('center_axis',(0.,-1.,0.));
#42901=DIRECTION('ref_axis',(1.,0.,0.));
#42902=DIRECTION('center_axis',(0.,1.,-1.38777878078E-16));
#42903=DIRECTION('ref_axis',(1.,0.,0.));
#42904=DIRECTION('center_axis',(0.,1.,6.93889390391E-17));
#42905=DIRECTION('ref_axis',(1.,0.,0.));
#42906=DIRECTION('',(0.,1.,0.));
#42907=DIRECTION('center_axis',(0.,0.,1.));
#42908=DIRECTION('ref_axis',(1.,0.,0.));
#42909=DIRECTION('center_axis',(0.,3.46944695195E-17,-1.));
#42910=DIRECTION('ref_axis',(1.,0.,0.));
#42911=DIRECTION('center_axis',(0.,-4.4408920985E-15,-1.));
#42912=DIRECTION('ref_axis',(1.,0.,0.));
#42913=DIRECTION('',(0.,0.,-1.));
#42914=DIRECTION('center_axis',(1.,0.,0.));
#42915=DIRECTION('ref_axis',(0.,-1.,-3.5527136788005E-14));
#42916=DIRECTION('center_axis',(0.,1.,0.));
#42917=DIRECTION('ref_axis',(1.,0.,0.));
#42918=DIRECTION('center_axis',(1.,0.,0.));
#42919=DIRECTION('ref_axis',(0.,1.,0.));
#42920=DIRECTION('center_axis',(0.,-1.,0.));
#42921=DIRECTION('ref_axis',(1.,0.,0.));
#42922=DIRECTION('center_axis',(0.,1.,6.93889390391E-17));
#42923=DIRECTION('ref_axis',(1.,0.,0.));
#42924=DIRECTION('',(0.,1.,0.));
#42925=DIRECTION('center_axis',(0.,0.,1.));
#42926=DIRECTION('ref_axis',(1.,0.,0.));
#42927=DIRECTION('center_axis',(0.,3.46944695195E-17,-1.));
#42928=DIRECTION('ref_axis',(1.,0.,0.));
#42929=DIRECTION('center_axis',(0.,6.93889390391E-17,-1.));
#42930=DIRECTION('ref_axis',(1.,0.,0.));
#42931=DIRECTION('',(0.,0.,-1.));
#42932=DIRECTION('center_axis',(0.,-1.,0.));
#42933=DIRECTION('ref_axis',(0.,0.,-1.));
#42934=DIRECTION('center_axis',(0.,-1.,-3.46944695195E-17));
#42935=DIRECTION('ref_axis',(1.,0.,0.));
#42936=DIRECTION('center_axis',(0.,-1.,4.4408920985E-15));
#42937=DIRECTION('ref_axis',(1.,0.,0.));
#42938=DIRECTION('',(0.,-1.,0.));
#42939=DIRECTION('center_axis',(1.,0.,0.));
#42940=DIRECTION('ref_axis',(0.,7.10542735760101E-14,1.));
#42941=DIRECTION('center_axis',(0.,0.,-1.));
#42942=DIRECTION('ref_axis',(1.,0.,0.));
#42943=DIRECTION('center_axis',(1.,0.,0.));
#42944=DIRECTION('ref_axis',(0.,1.,0.));
#42945=DIRECTION('center_axis',(0.,0.,1.));
#42946=DIRECTION('ref_axis',(1.,0.,0.));
#42947=DIRECTION('',(0.,0.,-1.));
#42948=DIRECTION('center_axis',(1.,0.,0.));
#42949=DIRECTION('ref_axis',(0.,-1.,-2.39124959150034E-16));
#42950=DIRECTION('center_axis',(-1.,0.,0.));
#42951=DIRECTION('ref_axis',(0.,1.,0.));
#42952=DIRECTION('center_axis',(-1.,0.,0.));
#42953=DIRECTION('ref_axis',(0.,1.,0.));
#42954=DIRECTION('center_axis',(0.,3.62957527281301E-16,-1.));
#42955=DIRECTION('ref_axis',(0.,1.,3.62957527281301E-16));
#42956=DIRECTION('center_axis',(1.,0.,0.));
#42957=DIRECTION('ref_axis',(0.,0.,1.));
#42958=DIRECTION('center_axis',(0.,0.726467397290375,0.687200931805355));
#42959=DIRECTION('ref_axis',(1.,0.,0.));
#42960=DIRECTION('center_axis',(-1.,3.93147962979832E-15,5.94795371774818E-15));
#42961=DIRECTION('ref_axis',(6.92478089935691E-15,0.734190003119643,0.678944061995669));
#42962=DIRECTION('center_axis',(-5.73224391576859E-9,0.268671312840191,
-0.963231916859449));
#42963=DIRECTION('ref_axis',(-5.18104078158404E-14,0.963231916859449,0.268671312840191));
#42964=DIRECTION('center_axis',(-1.,0.,0.));
#42965=DIRECTION('ref_axis',(0.,1.,0.));
#42966=DIRECTION('center_axis',(2.73676276537777E-8,0.403636572488003,-0.914919404838556));
#42967=DIRECTION('ref_axis',(-6.96173815432251E-8,0.914919404838555,0.403636572487999));
#42968=DIRECTION('center_axis',(1.,0.,0.));
#42969=DIRECTION('ref_axis',(0.,-0.985518026541958,0.169570691337993));
#42970=DIRECTION('',(-1.,0.,0.));
#42971=DIRECTION('',(-1.,0.,0.));
#42972=DIRECTION('center_axis',(1.,-8.02179867202313E-15,-2.35887717715673E-15));
#42973=DIRECTION('ref_axis',(7.82801319057738E-15,0.997327347392217,-0.0730627274580159));
#42974=DIRECTION('center_axis',(5.57830379642003E-8,-0.403636428026677,
0.914919468570793));
#42975=DIRECTION('ref_axis',(-7.95659834314697E-14,0.914919468570794,0.403636428026678));
#42976=DIRECTION('center_axis',(1.,0.,0.));
#42977=DIRECTION('ref_axis',(0.,1.,0.));
#42978=DIRECTION('center_axis',(1.05822780461189E-7,-0.268671045025511,
0.963231991560127));
#42979=DIRECTION('ref_axis',(2.79567437663786E-7,0.963231991560103,0.268671045025474));
#42980=DIRECTION('center_axis',(1.,0.,0.));
#42981=DIRECTION('ref_axis',(0.,-0.985518026541958,0.169570691337993));
#42982=DIRECTION('',(-1.,0.,0.));
#42983=DIRECTION('center_axis',(1.,0.,0.));
#42984=DIRECTION('ref_axis',(0.,1.,0.));
#42985=DIRECTION('',(1.,0.,0.));
#42986=DIRECTION('center_axis',(-1.,-6.091226037548E-15,2.96434183740151E-15));
#42987=DIRECTION('ref_axis',(-6.77424218415349E-15,0.899174530813553,-0.437590177147782));
#42988=DIRECTION('center_axis',(-9.0860756207758E-13,-0.686217479581265,
-0.727396432983511));
#42989=DIRECTION('ref_axis',(5.73615229389664E-14,0.727396432983511,-0.686217479581266));
#42990=DIRECTION('center_axis',(-1.,0.,0.));
#42991=DIRECTION('ref_axis',(0.,1.,0.));
#42992=DIRECTION('center_axis',(1.,0.,0.));
#42993=DIRECTION('ref_axis',(0.,-0.985518026541958,0.169570691337993));
#42994=DIRECTION('',(-1.,0.,0.));
#42995=DIRECTION('',(-1.,0.,0.));
#42996=DIRECTION('center_axis',(1.,0.,0.));
#42997=DIRECTION('ref_axis',(0.,0.509059777782153,-0.860731167464259));
#42998=DIRECTION('center_axis',(1.,0.,0.));
#42999=DIRECTION('ref_axis',(0.,1.,0.));
#43000=DIRECTION('center_axis',(-1.19474117133794E-8,0.686217506760235,
0.727396407343181));
#43001=DIRECTION('ref_axis',(5.90198613961689E-8,0.727396407343179,-0.686217506760235));
#43002=DIRECTION('center_axis',(1.,0.,0.));
#43003=DIRECTION('ref_axis',(0.,-0.985518026541958,0.169570691337993));
#43004=DIRECTION('',(1.,0.,0.));
#43005=DIRECTION('center_axis',(1.,0.,0.));
#43006=DIRECTION('ref_axis',(0.,1.,0.));
#43007=DIRECTION('',(-1.,0.,0.));
#43008=DIRECTION('center_axis',(-0.72158910718404,0.350067294611212,0.597295613274472));
#43009=DIRECTION('ref_axis',(0.494822520302078,-0.342622923784054,0.798598901514125));
#43010=DIRECTION('center_axis',(0.,-0.726467397290375,-0.687200931805355));
#43011=DIRECTION('ref_axis',(1.,0.,0.));
#43012=DIRECTION('center_axis',(-0.816269637465565,0.41965920741329,0.396976105811274));
#43013=DIRECTION('ref_axis',(0.577671081976444,0.592993279016696,0.560941255470831));
#43014=DIRECTION('center_axis',(0.,-0.726467397290375,-0.687200931805355));
#43015=DIRECTION('ref_axis',(0.,-0.687200931805355,0.726467397290375));
#43016=DIRECTION('',(0.,0.726467397290375,0.687200931805355));
#43017=DIRECTION('center_axis',(-0.258644806000509,-0.1693466143229,-0.951012401888814));
#43018=DIRECTION('ref_axis',(-0.0704066837757783,-0.978589379636601,0.193405596977311));
#43019=DIRECTION('center_axis',(0.,-0.977144298741099,0.212577090576022));
#43020=DIRECTION('ref_axis',(1.,0.,0.));
#43021=DIRECTION('center_axis',(1.,0.,0.));
#43022=DIRECTION('ref_axis',(0.,0.419820362992805,0.907607218358575));
#43023=DIRECTION('center_axis',(1.,0.,0.));
#43024=DIRECTION('ref_axis',(0.,-1.,0.));
#43025=DIRECTION('center_axis',(0.,-0.907607218358575,0.419820362992804));
#43026=DIRECTION('ref_axis',(1.,0.,0.));
#43027=DIRECTION('center_axis',(5.29416742490447E-29,-0.907607218358575,
0.419820362992804));
#43028=DIRECTION('ref_axis',(-1.,-4.80502457004213E-29,2.22259929006807E-29));
#43029=DIRECTION('center_axis',(-1.,0.,0.));
#43030=DIRECTION('ref_axis',(0.,-0.227955838450089,0.973671472169395));
#43031=DIRECTION('',(-1.,0.,0.));
#43032=DIRECTION('center_axis',(0.,0.,1.));
#43033=DIRECTION('ref_axis',(1.,0.,0.));
#43034=DIRECTION('center_axis',(-1.97947233792048E-13,-0.68720093180552,
0.726467397290219));
#43035=DIRECTION('ref_axis',(0.657142409811958,0.547586747279966,0.517989003193967));
#43036=DIRECTION('center_axis',(0.,-0.687200931805355,0.726467397290375));
#43037=DIRECTION('ref_axis',(1.,0.,0.));
#43038=DIRECTION('center_axis',(-0.809300823598924,0.426722876366013,0.403657978625494));
#43039=DIRECTION('ref_axis',(1.04962473897651E-8,-0.687200924844299,0.726467403875177));
#43040=DIRECTION('center_axis',(0.,-0.687200931805355,0.726467397290375));
#43041=DIRECTION('ref_axis',(-1.,0.,0.));
#43042=DIRECTION('',(-1.,0.,0.));
#43043=DIRECTION('center_axis',(0.,0.,1.));
#43044=DIRECTION('ref_axis',(1.,0.,0.));
#43045=DIRECTION('',(-1.,0.,0.));
#43046=DIRECTION('',(0.,-1.,0.));
#43047=DIRECTION('',(-1.,0.,0.));
#43048=DIRECTION('center_axis',(1.,0.,0.));
#43049=DIRECTION('ref_axis',(0.,-0.419820362992804,-0.907607218358575));
#43050=DIRECTION('',(-1.,0.,0.));
#43051=DIRECTION('center_axis',(-1.,0.,0.));
#43052=DIRECTION('ref_axis',(0.,1.,0.));
#43053=DIRECTION('center_axis',(-1.07495723694558E-13,0.419820362992774,
0.907607218358589));
#43054=DIRECTION('ref_axis',(0.958193364102501,0.259685881990864,-0.120119605745937));
#43055=DIRECTION('center_axis',(-0.690862062643962,-0.656187848545089,0.303524492950896));
#43056=DIRECTION('ref_axis',(-1.09708538548473E-11,0.419820362981223,0.907607218363932));
#43057=DIRECTION('center_axis',(0.,0.419820362992804,0.907607218358575));
#43058=DIRECTION('ref_axis',(1.,0.,0.));
#43059=DIRECTION('center_axis',(-0.690862033103006,0.656187879687057,-0.303524492864391));
#43060=DIRECTION('ref_axis',(1.47203652509396E-7,0.419820474127234,0.907607166952511));
#43061=DIRECTION('center_axis',(0.,0.419820362992804,0.907607218358575));
#43062=DIRECTION('ref_axis',(1.,0.,0.));
#43063=DIRECTION('',(-1.,0.,0.));
#43064=DIRECTION('',(0.,-0.907607218358575,0.419820362992804));
#43065=DIRECTION('',(-1.,0.,0.));
#43066=DIRECTION('center_axis',(-1.,0.,0.));
#43067=DIRECTION('ref_axis',(0.,-0.419820362992802,-0.907607218358576));
#43068=DIRECTION('center_axis',(-1.,0.,0.));
#43069=DIRECTION('ref_axis',(0.,1.,0.));
#43070=DIRECTION('center_axis',(-1.,0.,0.));
#43071=DIRECTION('ref_axis',(0.,-0.419820362992802,-0.907607218358576));
#43072=DIRECTION('center_axis',(0.,-0.86993736790158,0.493162220702754));
#43073=DIRECTION('ref_axis',(0.,0.493162220702747,0.869937367901583));
#43074=DIRECTION('center_axis',(-1.,0.,0.));
#43075=DIRECTION('ref_axis',(0.,-1.,0.));
#43076=DIRECTION('center_axis',(0.,-0.227955838450092,0.973671472169394));
#43077=DIRECTION('ref_axis',(-1.,0.,0.));
#43078=DIRECTION('',(-1.,0.,0.));
#43079=DIRECTION('center_axis',(-1.,0.,0.));
#43080=DIRECTION('ref_axis',(0.,0.687200931805355,-0.726467397290376));
#43081=DIRECTION('',(-1.,0.,0.));
#43082=DIRECTION('center_axis',(0.,-0.502994068287953,-0.86428986298992));
#43083=DIRECTION('ref_axis',(0.,-0.86428986298992,0.502994068287953));
#43084=DIRECTION('',(-1.,0.,0.));
#43085=DIRECTION('center_axis',(0.,-0.379561655995102,-0.925166444105198));
#43086=DIRECTION('ref_axis',(0.,-0.925166444105201,0.379561655995094));
#43087=DIRECTION('center_axis',(-1.,0.,0.));
#43088=DIRECTION('ref_axis',(0.,-1.,0.));
#43089=DIRECTION('center_axis',(1.,0.,0.));
#43090=DIRECTION('ref_axis',(0.,-0.687200931805354,0.726467397290376));
#43091=DIRECTION('',(-1.,0.,0.));
#43092=DIRECTION('center_axis',(1.,0.,0.));
#43093=DIRECTION('ref_axis',(0.,-0.687200931805354,0.726467397290376));
#43094=DIRECTION('',(-1.,0.,0.));
#43095=DIRECTION('center_axis',(-1.,0.,0.));
#43096=DIRECTION('ref_axis',(0.,1.,0.));
#43097=DIRECTION('center_axis',(0.,-0.687200931805355,0.726467397290375));
#43098=DIRECTION('ref_axis',(-1.,0.,0.));
#43099=DIRECTION('',(-1.,0.,0.));
#43100=DIRECTION('',(0.,0.726467397290375,0.687200931805355));
#43101=DIRECTION('center_axis',(1.,0.,0.));
#43102=DIRECTION('ref_axis',(0.,0.,1.));
#43103=DIRECTION('',(-1.,0.,0.));
#43104=DIRECTION('center_axis',(-1.,0.,0.));
#43105=DIRECTION('ref_axis',(0.,1.,0.));
#43106=DIRECTION('center_axis',(0.,0.,1.));
#43107=DIRECTION('ref_axis',(1.,0.,0.));
#43108=DIRECTION('',(-1.,0.,0.));
#43109=DIRECTION('',(0.,1.,0.));
#43110=DIRECTION('center_axis',(1.,0.,0.));
#43111=DIRECTION('ref_axis',(0.,0.417332015056099,0.908754086213216));
#43112=DIRECTION('',(-1.,0.,0.));
#43113=DIRECTION('center_axis',(-1.,0.,0.));
#43114=DIRECTION('ref_axis',(0.,1.,0.));
#43115=DIRECTION('center_axis',(0.,0.417332015056099,0.908754086213215));
#43116=DIRECTION('ref_axis',(1.,0.,0.));
#43117=DIRECTION('',(1.,0.,0.));
#43118=DIRECTION('',(0.,0.908754086213215,-0.417332015056099));
#43119=DIRECTION('center_axis',(1.,0.,0.));
#43120=DIRECTION('ref_axis',(0.,-0.417332015056099,-0.908754086213215));
#43121=DIRECTION('',(1.,0.,0.));
#43122=DIRECTION('center_axis',(1.,0.,0.));
#43123=DIRECTION('ref_axis',(0.,1.,0.));
#43124=DIRECTION('center_axis',(0.,0.,1.));
#43125=DIRECTION('ref_axis',(1.,0.,0.));
#43126=DIRECTION('',(1.,0.,0.));
#43127=DIRECTION('',(0.,1.,0.));
#43128=DIRECTION('center_axis',(1.,0.,0.));
#43129=DIRECTION('ref_axis',(0.,0.,-1.));
#43130=DIRECTION('',(1.,0.,0.));
#43131=DIRECTION('center_axis',(1.,0.,0.));
#43132=DIRECTION('ref_axis',(0.,1.,0.));
#43133=DIRECTION('center_axis',(0.,-0.814757152506986,0.57980236498199));
#43134=DIRECTION('ref_axis',(-1.,0.,0.));
#43135=DIRECTION('',(-1.,0.,0.));
#43136=DIRECTION('',(0.,0.57980236498199,0.814757152506986));
#43137=DIRECTION('center_axis',(0.,0.,1.));
#43138=DIRECTION('ref_axis',(1.,0.,0.));
#43139=DIRECTION('center_axis',(-1.,0.,0.));
#43140=DIRECTION('ref_axis',(0.,1.,0.));
#43141=DIRECTION('center_axis',(0.,0.,1.));
#43142=DIRECTION('ref_axis',(1.,0.,0.));
#43143=DIRECTION('',(-1.,0.,0.));
#43144=DIRECTION('',(0.,1.,0.));
#43145=DIRECTION('',(-1.,0.,0.));
#43146=DIRECTION('center_axis',(0.,0.,1.));
#43147=DIRECTION('ref_axis',(1.,0.,0.));
#43148=DIRECTION('center_axis',(-1.,0.,0.));
#43149=DIRECTION('ref_axis',(0.,1.,0.));
#43150=DIRECTION('center_axis',(0.,1.,0.));
#43151=DIRECTION('ref_axis',(1.,0.,0.));
#43152=DIRECTION('',(1.,0.,0.));
#43153=DIRECTION('',(0.,0.,-1.));
#43154=DIRECTION('',(-1.,0.,0.));
#43155=DIRECTION('center_axis',(1.,0.,0.));
#43156=DIRECTION('ref_axis',(0.,-1.,0.));
#43157=DIRECTION('',(1.,0.,0.));
#43158=DIRECTION('center_axis',(1.,0.,0.));
#43159=DIRECTION('ref_axis',(0.,1.,0.));
#43160=DIRECTION('center_axis',(0.,0.,1.));
#43161=DIRECTION('ref_axis',(1.,0.,0.));
#43162=DIRECTION('',(-1.,0.,0.));
#43163=DIRECTION('',(0.,1.,0.));
#43164=DIRECTION('center_axis',(0.,0.,1.));
#43165=DIRECTION('ref_axis',(1.,0.,0.));
#43166=DIRECTION('center_axis',(-1.,0.,0.));
#43167=DIRECTION('ref_axis',(0.,1.,0.));
#43168=DIRECTION('center_axis',(0.,1.,0.));
#43169=DIRECTION('ref_axis',(1.,0.,0.));
#43170=DIRECTION('',(-1.,0.,0.));
#43171=DIRECTION('',(0.,0.,-1.));
#43172=DIRECTION('',(-1.,0.,0.));
#43173=DIRECTION('center_axis',(0.,0.,1.));
#43174=DIRECTION('ref_axis',(1.,0.,0.));
#43175=DIRECTION('center_axis',(-1.,0.,0.));
#43176=DIRECTION('ref_axis',(0.,1.,0.));
#43177=DIRECTION('center_axis',(0.,0.,1.));
#43178=DIRECTION('ref_axis',(1.,0.,0.));
#43179=DIRECTION('',(1.,0.,0.));
#43180=DIRECTION('',(0.,-1.,0.));
#43181=DIRECTION('',(-1.,0.,0.));
#43182=DIRECTION('center_axis',(1.,0.,0.));
#43183=DIRECTION('ref_axis',(0.,0.,1.));
#43184=DIRECTION('',(1.,0.,0.));
#43185=DIRECTION('center_axis',(1.,0.,0.));
#43186=DIRECTION('ref_axis',(0.,1.,0.));
#43187=DIRECTION('center_axis',(0.,1.,0.));
#43188=DIRECTION('ref_axis',(1.,0.,0.));
#43189=DIRECTION('',(0.,0.,-1.));
#43190=DIRECTION('center_axis',(1.,0.,0.));
#43191=DIRECTION('ref_axis',(0.,1.,0.));
#43192=DIRECTION('center_axis',(-1.,0.,0.));
#43193=DIRECTION('ref_axis',(0.,-1.,1.30922526488816E-16));
#43194=DIRECTION('',(-1.,0.,0.));
#43195=DIRECTION('center_axis',(-1.,0.,0.));
#43196=DIRECTION('ref_axis',(0.,0.96323191500603,0.268671319485009));
#43197=DIRECTION('center_axis',(0.,0.403636513060188,-0.914919431056425));
#43198=DIRECTION('ref_axis',(1.,0.,0.));
#43199=DIRECTION('center_axis',(1.,0.,0.));
#43200=DIRECTION('ref_axis',(0.,1.,0.));
#43201=DIRECTION('center_axis',(0.,0.268671319485009,-0.96323191500603));
#43202=DIRECTION('ref_axis',(1.,0.,0.));
#43203=DIRECTION('center_axis',(-1.,0.,0.));
#43204=DIRECTION('ref_axis',(0.,-0.502994068287962,-0.864289862989915));
#43205=DIRECTION('center_axis',(-1.,0.,0.));
#43206=DIRECTION('ref_axis',(0.,1.,0.));
#43207=DIRECTION('',(1.,0.,0.));
#43208=DIRECTION('center_axis',(1.,0.,0.));
#43209=DIRECTION('ref_axis',(0.,0.925572659293396,-0.378570009864162));
#43210=DIRECTION('center_axis',(2.08166817117052E-15,-0.0845895878810212,
0.996415877845249));
#43211=DIRECTION('ref_axis',(1.,-6.67956163323103E-18,-2.08972301509199E-15));
#43212=DIRECTION('center_axis',(1.,0.,0.));
#43213=DIRECTION('ref_axis',(0.,1.,0.));
#43214=DIRECTION('center_axis',(-6.10622663544094E-16,0.319261680225049,
0.947666597248145));
#43215=DIRECTION('ref_axis',(1.,-2.37377845073976E-17,6.52340422576772E-16));
#43216=DIRECTION('center_axis',(1.,0.,0.));
#43217=DIRECTION('ref_axis',(0.,1.,0.));
#43218=DIRECTION('',(0.,0.726467397290375,0.687200931805355));
#43219=DIRECTION('center_axis',(-1.,0.,0.));
#43220=DIRECTION('ref_axis',(0.,1.,0.));
#43221=DIRECTION('',(0.,1.,0.));
#43222=DIRECTION('center_axis',(1.,0.,0.));
#43223=DIRECTION('ref_axis',(0.,1.,0.));
#43224=DIRECTION('center_axis',(-1.,0.,0.));
#43225=DIRECTION('ref_axis',(0.,1.,0.));
#43226=DIRECTION('center_axis',(1.,0.,0.));
#43227=DIRECTION('ref_axis',(0.,1.,0.));
#43228=DIRECTION('',(0.,-1.,0.));
#43229=DIRECTION('center_axis',(-1.,0.,0.));
#43230=DIRECTION('ref_axis',(0.,1.,0.));
#43231=DIRECTION('',(0.,-0.907607218358575,0.419820362992804));
#43232=DIRECTION('center_axis',(1.,0.,0.));
#43233=DIRECTION('ref_axis',(0.,1.,0.));
#43234=DIRECTION('center_axis',(-1.,0.,0.));
#43235=DIRECTION('ref_axis',(0.,1.,0.));
#43236=DIRECTION('center_axis',(-1.,0.,0.));
#43237=DIRECTION('ref_axis',(0.,-0.739936080580779,0.672677186066805));
#43238=DIRECTION('',(1.,0.,0.));
#43239=DIRECTION('center_axis',(-1.,0.,0.));
#43240=DIRECTION('ref_axis',(0.,1.,0.));
#43241=DIRECTION('center_axis',(0.,0.,1.));
#43242=DIRECTION('ref_axis',(1.,0.,0.));
#43243=DIRECTION('center_axis',(0.,0.367447999014073,0.930044067784185));
#43244=DIRECTION('ref_axis',(1.,0.,0.));
#43245=DIRECTION('center_axis',(-1.,0.,0.));
#43246=DIRECTION('ref_axis',(0.,1.,0.));
#43247=DIRECTION('center_axis',(0.,1.,0.));
#43248=DIRECTION('ref_axis',(1.,0.,0.));
#43249=DIRECTION('center_axis',(-1.,0.,0.));
#43250=DIRECTION('ref_axis',(0.,-0.502994068287962,-0.864289862989915));
#43251=DIRECTION('center_axis',(-1.,0.,0.));
#43252=DIRECTION('ref_axis',(0.,-0.739936080580779,0.672677186066805));
#43253=DIRECTION('center_axis',(0.,1.,0.));
#43254=DIRECTION('ref_axis',(0.,0.,-1.));
#43255=DIRECTION('center_axis',(0.,-0.707106781186548,-0.707106781186548));
#43256=DIRECTION('ref_axis',(0.,0.707106781186548,-0.707106781186548));
#43257=DIRECTION('center_axis',(0.,1.,3.99680288865E-15));
#43258=DIRECTION('ref_axis',(1.,0.,0.));
#43259=DIRECTION('',(0.,-1.,0.));
#43260=DIRECTION('center_axis',(-1.,0.,0.));
#43261=DIRECTION('ref_axis',(0.,-0.419820362992805,-0.907607218358575));
#43262=DIRECTION('center_axis',(0.,0.907607218358575,-0.419820362992804));
#43263=DIRECTION('ref_axis',(1.,0.,0.));
#43264=DIRECTION('center_axis',(-1.,0.,0.));
#43265=DIRECTION('ref_axis',(0.,1.,0.));
#43266=DIRECTION('center_axis',(1.92592994438724E-32,0.907607218358575,
-0.419820362992804));
#43267=DIRECTION('ref_axis',(-2.4880840830811E-46,-0.419820362992804,-0.907607218358575));
#43268=DIRECTION('center_axis',(0.,0.907607218358575,-0.419820362992804));
#43269=DIRECTION('ref_axis',(1.,0.,0.));
#43270=DIRECTION('',(0.,-0.907607218358575,0.419820362992804));
#43271=DIRECTION('center_axis',(-1.,0.,0.));
#43272=DIRECTION('ref_axis',(0.,-0.72739643298632,0.686217479578288));
#43273=DIRECTION('center_axis',(0.,-0.686217479578295,-0.727396432986313));
#43274=DIRECTION('ref_axis',(1.,0.,0.));
#43275=DIRECTION('center_axis',(-1.,0.,0.));
#43276=DIRECTION('ref_axis',(0.,1.,0.));
#43277=DIRECTION('center_axis',(-1.,0.,0.));
#43278=DIRECTION('ref_axis',(0.,-0.687200931805354,0.726467397290377));
#43279=DIRECTION('center_axis',(0.,-0.726467397290375,-0.687200931805355));
#43280=DIRECTION('ref_axis',(1.,0.,0.));
#43281=DIRECTION('center_axis',(-1.,0.,0.));
#43282=DIRECTION('ref_axis',(0.,1.,0.));
#43283=DIRECTION('center_axis',(0.,0.726467397290375,0.687200931805355));
#43284=DIRECTION('ref_axis',(-1.,0.,0.));
#43285=DIRECTION('center_axis',(0.,-0.726467397290375,-0.687200931805355));
#43286=DIRECTION('ref_axis',(1.,0.,0.));
#43287=DIRECTION('',(0.,0.726467397290375,0.687200931805355));
#43288=DIRECTION('center_axis',(-1.,0.,0.));
#43289=DIRECTION('ref_axis',(0.,-3.5527136788005E-15,1.));
#43290=DIRECTION('center_axis',(0.,-1.,0.));
#43291=DIRECTION('ref_axis',(1.,0.,0.));
#43292=DIRECTION('center_axis',(-1.,0.,0.));
#43293=DIRECTION('ref_axis',(0.,1.,0.));
#43294=DIRECTION('center_axis',(0.,1.,0.));
#43295=DIRECTION('ref_axis',(-1.,0.,0.));
#43296=DIRECTION('center_axis',(0.,-1.,4.99600361081E-16));
#43297=DIRECTION('ref_axis',(1.,0.,0.));
#43298=DIRECTION('',(0.,1.,0.));
#43299=DIRECTION('center_axis',(-1.,0.,0.));
#43300=DIRECTION('ref_axis',(0.,0.417332015056099,0.908754086213215));
#43301=DIRECTION('center_axis',(0.,-0.908754086213215,0.417332015056099));
#43302=DIRECTION('ref_axis',(1.,0.,0.));
#43303=DIRECTION('center_axis',(-1.,0.,0.));
#43304=DIRECTION('ref_axis',(0.,1.,0.));
#43305=DIRECTION('center_axis',(0.,0.908754086213215,-0.417332015056099));
#43306=DIRECTION('ref_axis',(-1.,0.,0.));
#43307=DIRECTION('center_axis',(0.,-0.908754086213215,0.417332015056099));
#43308=DIRECTION('ref_axis',(1.,0.,0.));
#43309=DIRECTION('',(0.,0.908754086213215,-0.417332015056099));
#43310=DIRECTION('center_axis',(-1.,0.,0.));
#43311=DIRECTION('ref_axis',(0.,-0.417332015056099,-0.908754086213215));
#43312=DIRECTION('center_axis',(0.,-1.,0.));
#43313=DIRECTION('ref_axis',(1.,0.,0.));
#43314=DIRECTION('center_axis',(1.,0.,0.));
#43315=DIRECTION('ref_axis',(0.,1.,0.));
#43316=DIRECTION('center_axis',(0.,1.,0.));
#43317=DIRECTION('ref_axis',(-1.,0.,0.));
#43318=DIRECTION('center_axis',(0.,-1.,-7.40148683083E-16));
#43319=DIRECTION('ref_axis',(1.,0.,0.));
#43320=DIRECTION('',(0.,1.,0.));
#43321=DIRECTION('center_axis',(-1.,0.,0.));
#43322=DIRECTION('ref_axis',(0.,-2.53765262771464E-15,-1.));
#43323=DIRECTION('center_axis',(0.,-0.57980236498199,-0.814757152506986));
#43324=DIRECTION('ref_axis',(1.,0.,0.));
#43325=DIRECTION('center_axis',(1.,0.,0.));
#43326=DIRECTION('ref_axis',(0.,1.,0.));
#43327=DIRECTION('center_axis',(0.,0.57980236498199,0.814757152506986));
#43328=DIRECTION('ref_axis',(-1.,0.,0.));
#43329=DIRECTION('center_axis',(0.,-0.57980236498199,-0.814757152506986));
#43330=DIRECTION('ref_axis',(1.,0.,0.));
#43331=DIRECTION('',(0.,0.57980236498199,0.814757152506986));
#43332=DIRECTION('center_axis',(1.,0.,0.));
#43333=DIRECTION('ref_axis',(0.,0.,1.));
#43334=DIRECTION('center_axis',(-1.,0.,0.));
#43335=DIRECTION('ref_axis',(0.,1.,0.));
#43336=DIRECTION('center_axis',(0.,1.,0.));
#43337=DIRECTION('ref_axis',(-1.,0.,0.));
#43338=DIRECTION('center_axis',(0.,-1.,-6.93889390391E-17));
#43339=DIRECTION('ref_axis',(1.,0.,0.));
#43340=DIRECTION('',(0.,1.,0.));
#43341=DIRECTION('center_axis',(0.,-1.,1.38777878078E-16));
#43342=DIRECTION('ref_axis',(1.,0.,0.));
#43343=DIRECTION('center_axis',(1.,0.,0.));
#43344=DIRECTION('ref_axis',(0.,1.,0.));
#43345=DIRECTION('center_axis',(-1.,0.,0.));
#43346=DIRECTION('ref_axis',(0.,1.,0.));
#43347=DIRECTION('center_axis',(0.,0.,-1.));
#43348=DIRECTION('ref_axis',(-1.,0.,0.));
#43349=DIRECTION('center_axis',(0.,4.4408920985E-15,1.));
#43350=DIRECTION('ref_axis',(1.,0.,0.));
#43351=DIRECTION('',(0.,0.,-1.));
#43352=DIRECTION('center_axis',(0.,-3.46944695195E-17,1.));
#43353=DIRECTION('ref_axis',(1.,0.,0.));
#43354=DIRECTION('center_axis',(-1.,0.,0.));
#43355=DIRECTION('ref_axis',(0.,-1.,-3.5527136788005E-14));
#43356=DIRECTION('center_axis',(0.,-1.,0.));
#43357=DIRECTION('ref_axis',(1.,0.,0.));
#43358=DIRECTION('center_axis',(1.,0.,0.));
#43359=DIRECTION('ref_axis',(0.,1.,0.));
#43360=DIRECTION('center_axis',(0.,1.,0.));
#43361=DIRECTION('ref_axis',(-1.,0.,0.));
#43362=DIRECTION('center_axis',(0.,-1.,-6.93889390391E-17));
#43363=DIRECTION('ref_axis',(1.,0.,0.));
#43364=DIRECTION('',(0.,1.,0.));
#43365=DIRECTION('center_axis',(1.,0.,0.));
#43366=DIRECTION('ref_axis',(0.,1.,0.));
#43367=DIRECTION('center_axis',(-1.,0.,0.));
#43368=DIRECTION('ref_axis',(0.,1.,0.));
#43369=DIRECTION('center_axis',(0.,0.,-1.));
#43370=DIRECTION('ref_axis',(-1.,0.,0.));
#43371=DIRECTION('center_axis',(0.,-6.93889390391E-17,1.));
#43372=DIRECTION('ref_axis',(1.,0.,0.));
#43373=DIRECTION('',(0.,0.,-1.));
#43374=DIRECTION('center_axis',(0.,-3.46944695195E-17,1.));
#43375=DIRECTION('ref_axis',(1.,0.,0.));
#43376=DIRECTION('center_axis',(1.,0.,0.));
#43377=DIRECTION('ref_axis',(0.,0.,-1.));
#43378=DIRECTION('center_axis',(-1.,0.,0.));
#43379=DIRECTION('ref_axis',(0.,1.,0.));
#43380=DIRECTION('center_axis',(0.,1.,0.));
#43381=DIRECTION('ref_axis',(0.,0.,-1.));
#43382=DIRECTION('center_axis',(0.,1.,-4.4408920985E-15));
#43383=DIRECTION('ref_axis',(1.,0.,0.));
#43384=DIRECTION('',(0.,-1.,0.));
#43385=DIRECTION('center_axis',(0.,1.,3.46944695195E-17));
#43386=DIRECTION('ref_axis',(1.,0.,0.));
#43387=DIRECTION('center_axis',(-1.,0.,0.));
#43388=DIRECTION('ref_axis',(0.,7.10542735760101E-14,1.));
#43389=DIRECTION('center_axis',(0.,0.,1.));
#43390=DIRECTION('ref_axis',(1.,0.,0.));
#43391=DIRECTION('center_axis',(1.,0.,0.));
#43392=DIRECTION('ref_axis',(0.,1.,0.));
#43393=DIRECTION('center_axis',(0.,0.,-1.));
#43394=DIRECTION('ref_axis',(-1.,0.,0.));
#43395=DIRECTION('',(0.,0.,-1.));
#43396=DIRECTION('center_axis',(1.,0.,0.));
#43397=DIRECTION('ref_axis',(0.,1.,0.));
#43398=DIRECTION('center_axis',(1.,0.,0.));
#43399=DIRECTION('ref_axis',(0.,1.,0.));
#43400=DIRECTION('center_axis',(0.,-0.379561655995102,-0.925166444105198));
#43401=DIRECTION('ref_axis',(0.,-0.925166444105201,0.379561655995094));
#43402=DIRECTION('center_axis',(0.,0.86428986298992,-0.502994068287953));
#43403=DIRECTION('ref_axis',(1.,0.,0.));
#43404=DIRECTION('center_axis',(1.,1.76988078022002E-14,4.55191440096E-13));
#43405=DIRECTION('ref_axis',(-1.76988078022E-14,1.,-4.16314649483351E-16));
#43406=DIRECTION('center_axis',(-1.,0.,0.));
#43407=DIRECTION('ref_axis',(0.,-1.,0.));
#43408=DIRECTION('',(-0.788010753606638,0.615661475325766,-3.58876661851124E-13));
#43409=DIRECTION('center_axis',(-1.,2.05025983117E-16,1.75613383407E-16));
#43410=DIRECTION('ref_axis',(2.05025983117E-16,1.,2.62770395016422E-32));
#43411=DIRECTION('center_axis',(-1.,2.05025983117E-16,1.75613383407E-16));
#43412=DIRECTION('ref_axis',(2.05025983117E-16,1.,2.62770395016422E-32));
#43413=DIRECTION('center_axis',(0.,0.502994068287953,0.86428986298992));
#43414=DIRECTION('ref_axis',(1.,0.,0.));
#43415=DIRECTION('',(0.,-0.86428986298992,0.502994068287953));
#43416=DIRECTION('',(1.,0.,0.));
#43417=DIRECTION('center_axis',(-1.,0.,0.));
#43418=DIRECTION('ref_axis',(0.,1.,0.));
#43419=DIRECTION('center_axis',(-1.,0.,0.));
#43420=DIRECTION('ref_axis',(0.,1.,0.));
#43421=DIRECTION('center_axis',(0.,-1.28102656687518E-16,-1.));
#43422=DIRECTION('ref_axis',(0.,-1.,1.28102656687518E-16));
#43423=DIRECTION('center_axis',(0.,1.,0.));
#43424=DIRECTION('ref_axis',(0.,0.,1.));
#43425=DIRECTION('center_axis',(0.,-1.,-1.7763568394E-15));
#43426=DIRECTION('ref_axis',(1.,0.,0.));
#43427=DIRECTION('',(0.,1.,0.));
#43428=DIRECTION('center_axis',(0.,-1.,-6.36065274525E-16));
#43429=DIRECTION('ref_axis',(1.,0.,0.));
#43430=DIRECTION('center_axis',(-1.,0.,0.));
#43431=DIRECTION('ref_axis',(0.,0.,1.));
#43432=DIRECTION('center_axis',(0.,-0.726467397290375,-0.687200931805355));
#43433=DIRECTION('ref_axis',(1.,0.,0.));
#43434=DIRECTION('center_axis',(-1.,0.,0.));
#43435=DIRECTION('ref_axis',(0.,1.,0.));
#43436=DIRECTION('center_axis',(-1.,0.,0.));
#43437=DIRECTION('ref_axis',(0.,-0.419820362992804,-0.907607218358575));
#43438=DIRECTION('center_axis',(0.,1.,0.));
#43439=DIRECTION('ref_axis',(1.,0.,0.));
#43440=DIRECTION('center_axis',(-1.,0.,0.));
#43441=DIRECTION('ref_axis',(0.,1.,0.));
#43442=DIRECTION('center_axis',(0.,0.907607218358575,-0.419820362992804));
#43443=DIRECTION('ref_axis',(1.,0.,0.));
#43444=DIRECTION('center_axis',(0.,-1.,0.));
#43445=DIRECTION('ref_axis',(0.,0.,-1.));
#43446=DIRECTION('',(0.,-1.,0.));
#43447=DIRECTION('center_axis',(-1.,0.,0.));
#43448=DIRECTION('ref_axis',(0.,-0.107526881719979,0.994202177480807));
#43449=DIRECTION('center_axis',(0.,0.994202177480807,0.107526881719979));
#43450=DIRECTION('ref_axis',(1.,0.,0.));
#43451=DIRECTION('center_axis',(1.,0.,0.));
#43452=DIRECTION('ref_axis',(0.,-1.,0.));
#43453=DIRECTION('center_axis',(0.187357668294215,0.0206872986033109,0.982073897325376));
#43454=DIRECTION('ref_axis',(0.854656229332195,0.48939719485811,-0.17335834369504));
#43455=DIRECTION('center_axis',(-0.816269637465565,-0.41965920741329,-0.396976105811274));
#43456=DIRECTION('ref_axis',(0.577671081976444,-0.592993279016696,-0.560941255470831));
#43457=DIRECTION('center_axis',(0.,-0.726467397290375,-0.687200931805355));
#43458=DIRECTION('ref_axis',(1.,0.,0.));
#43459=DIRECTION('center_axis',(0.,0.726467397290375,0.687200931805355));
#43460=DIRECTION('ref_axis',(0.,-0.687200931805355,0.726467397290375));
#43461=DIRECTION('',(0.,0.726467397290375,0.687200931805355));
#43462=DIRECTION('center_axis',(0.860803892811723,0.39426976223081,-0.321819845116245));
#43463=DIRECTION('ref_axis',(-0.15670617194301,-0.396284218850021,-0.904655732069054));
#43464=DIRECTION('center_axis',(0.,-0.977144298741099,0.212577090576022));
#43465=DIRECTION('ref_axis',(1.,0.,0.));
#43466=DIRECTION('center_axis',(-1.,0.,0.));
#43467=DIRECTION('ref_axis',(0.,0.419820362992805,0.907607218358575));
#43468=DIRECTION('center_axis',(0.,0.907607218358575,-0.419820362992804));
#43469=DIRECTION('ref_axis',(1.,0.,0.));
#43470=DIRECTION('center_axis',(1.,0.,0.));
#43471=DIRECTION('ref_axis',(0.,-1.,0.));
#43472=DIRECTION('center_axis',(5.29416742490447E-29,0.907607218358575,
-0.419820362992804));
#43473=DIRECTION('ref_axis',(1.,-4.80502457004213E-29,2.22259929006807E-29));
#43474=DIRECTION('',(0.,-0.907607218358575,0.419820362992804));
#43475=DIRECTION('center_axis',(-1.,0.,0.));
#43476=DIRECTION('ref_axis',(0.,-0.930044067784185,-0.367447999014073));
#43477=DIRECTION('center_axis',(0.,-0.367447999014073,0.930044067784185));
#43478=DIRECTION('ref_axis',(1.,0.,0.));
#43479=DIRECTION('center_axis',(1.,0.,0.));
#43480=DIRECTION('ref_axis',(0.,-1.,0.));
#43481=DIRECTION('center_axis',(0.,-0.994202177480807,0.107526881719979));
#43482=DIRECTION('ref_axis',(1.,0.,0.));
#43483=DIRECTION('center_axis',(-1.,0.,0.));
#43484=DIRECTION('ref_axis',(0.,0.107526881719979,-0.994202177480807));
#43485=DIRECTION('center_axis',(-1.,0.,0.));
#43486=DIRECTION('ref_axis',(0.,1.,0.));
#43487=DIRECTION('center_axis',(0.,0.227955838450092,-0.973671472169394));
#43488=DIRECTION('ref_axis',(-1.,0.,0.));
#43489=DIRECTION('',(1.,0.,0.));
#43490=DIRECTION('',(0.,0.973671472169394,0.227955838450093));
#43491=DIRECTION('center_axis',(1.,-3.93687335395956E-16,-1.5579751070446E-16));
#43492=DIRECTION('ref_axis',(-3.60046877990609E-16,-0.994529145503541,0.104459459810952));
#43493=DIRECTION('center_axis',(1.9606953158236E-16,0.104459459810952,0.994529145503541));
#43494=DIRECTION('ref_axis',(4.50058597488261E-16,0.994529145503542,-0.104459459810952));
#43495=DIRECTION('center_axis',(-1.,4.69073756832726E-16,-2.82798301772873E-22));
#43496=DIRECTION('ref_axis',(-4.69073756826505E-16,-0.999999999999273,1.20579937603916E-6));
#43497=DIRECTION('center_axis',(-1.,-4.69075046723531E-16,4.6907432243473E-16));
#43498=DIRECTION('ref_axis',(-4.69073756826505E-16,0.999999999977518,6.70552506222274E-6));
#43499=DIRECTION('center_axis',(-1.,4.69073756832726E-16,-2.82798301772873E-22));
#43500=DIRECTION('ref_axis',(-4.69073756826505E-16,-0.999999999999273,1.20579937603916E-6));
#43501=DIRECTION('center_axis',(0.,0.,1.));
#43502=DIRECTION('ref_axis',(1.,0.,0.));
#43503=DIRECTION('center_axis',(0.,0.,1.));
#43504=DIRECTION('ref_axis',(1.,0.,0.));
#43505=DIRECTION('center_axis',(0.,0.,1.));
#43506=DIRECTION('ref_axis',(1.,0.,0.));
#43507=DIRECTION('center_axis',(0.,0.,1.));
#43508=DIRECTION('ref_axis',(1.,0.,0.));
#43509=DIRECTION('center_axis',(1.,0.,0.));
#43510=DIRECTION('ref_axis',(0.,1.,-1.1229236786457E-15));
#43511=DIRECTION('center_axis',(-1.,0.,0.));
#43512=DIRECTION('ref_axis',(0.,1.,3.46944695195361E-16));
#43513=DIRECTION('',(1.,0.,0.));
#43514=DIRECTION('center_axis',(-9.62964972193618E-33,0.86428986298992,
-0.502994068287953));
#43515=DIRECTION('ref_axis',(4.62384107026404E-47,-0.502994068287953,-0.86428986298992));
#43516=DIRECTION('',(0.,-0.86428986298992,0.502994068287953));
#43517=DIRECTION('center_axis',(0.,0.86428986298992,-0.502994068287953));
#43518=DIRECTION('ref_axis',(1.,0.,0.));
#43519=DIRECTION('center_axis',(-1.,0.,0.));
#43520=DIRECTION('ref_axis',(0.,-0.502994068287954,-0.864289862989919));
#43521=DIRECTION('center_axis',(-1.,0.,0.));
#43522=DIRECTION('ref_axis',(0.,-1.,0.));
#43523=DIRECTION('center_axis',(-1.,0.,0.));
#43524=DIRECTION('ref_axis',(0.,1.,0.));
#43525=DIRECTION('center_axis',(0.,0.726467397290375,0.687200931805355));
#43526=DIRECTION('ref_axis',(1.,0.,0.));
#43527=DIRECTION('center_axis',(1.92592994438724E-32,0.726467397290375,
0.687200931805355));
#43528=DIRECTION('ref_axis',(2.06468201548131E-46,0.687200931805355,-0.726467397290375));
#43529=DIRECTION('',(0.,-0.726467397290375,-0.687200931805355));
#43530=DIRECTION('',(0.,-0.726467397290375,-0.687200931805355));
#43531=DIRECTION('center_axis',(0.,0.726467397290375,0.687200931805355));
#43532=DIRECTION('ref_axis',(1.,0.,0.));
#43533=DIRECTION('center_axis',(-1.,0.,0.));
#43534=DIRECTION('ref_axis',(0.,0.,1.));
#43535=DIRECTION('center_axis',(1.,0.,0.));
#43536=DIRECTION('ref_axis',(0.,1.,0.));
#43537=DIRECTION('center_axis',(1.,0.,0.));
#43538=DIRECTION('ref_axis',(0.,1.,0.));
#43539=DIRECTION('center_axis',(0.,1.,0.));
#43540=DIRECTION('ref_axis',(1.,0.,0.));
#43541=DIRECTION('center_axis',(0.,1.,0.));
#43542=DIRECTION('ref_axis',(0.,0.,-1.));
#43543=DIRECTION('',(0.,-1.,0.));
#43544=DIRECTION('',(0.,-1.,0.));
#43545=DIRECTION('center_axis',(0.,1.,-4.82947015712E-15));
#43546=DIRECTION('ref_axis',(1.,0.,0.));
#43547=DIRECTION('center_axis',(0.,0.,1.));
#43548=DIRECTION('ref_axis',(1.,0.,0.));
#43549=DIRECTION('center_axis',(-1.,0.,0.));
#43550=DIRECTION('ref_axis',(0.,1.,0.));
#43551=DIRECTION('center_axis',(1.,0.,0.));
#43552=DIRECTION('ref_axis',(0.,0.,1.));
#43553=DIRECTION('',(1.,0.,0.));
#43554=DIRECTION('',(1.,0.,0.));
#43555=DIRECTION('center_axis',(1.53432918126103E-13,-0.687200931805562,
0.72646739729018));
#43556=DIRECTION('ref_axis',(-0.474694932580992,0.63940056798499,0.60484017280799));
#43557=DIRECTION('center_axis',(-0.809300828659765,-0.426722873335083,-0.403657971683043));
#43558=DIRECTION('ref_axis',(4.78167372553401E-5,-0.687248789804423,0.726422121514699));
#43559=DIRECTION('center_axis',(0.,-0.687200931805355,0.726467397290375));
#43560=DIRECTION('ref_axis',(1.,0.,0.));
#43561=DIRECTION('center_axis',(0.,-0.687200931805355,0.726467397290375));
#43562=DIRECTION('ref_axis',(-1.,0.,0.));
#43563=DIRECTION('',(1.,0.,0.));
#43564=DIRECTION('center_axis',(-1.,0.,0.));
#43565=DIRECTION('ref_axis',(0.,1.,0.));
#43566=DIRECTION('center_axis',(0.,1.30922526488816E-16,1.));
#43567=DIRECTION('ref_axis',(0.,-1.,1.30922526488816E-16));
#43568=DIRECTION('center_axis',(-1.,0.,0.));
#43569=DIRECTION('ref_axis',(0.,1.,0.));
#43570=DIRECTION('center_axis',(1.,0.,0.));
#43571=DIRECTION('ref_axis',(0.,1.,0.));
#43572=DIRECTION('center_axis',(-1.,0.,0.));
#43573=DIRECTION('ref_axis',(0.,-0.433812003680988,-0.901003410349975));
#43574=DIRECTION('center_axis',(0.,-0.901003410349976,0.433812003680988));
#43575=DIRECTION('ref_axis',(1.,0.,0.));
#43576=DIRECTION('center_axis',(1.,0.,0.));
#43577=DIRECTION('ref_axis',(0.,1.,0.));
#43578=DIRECTION('center_axis',(0.,-1.,0.));
#43579=DIRECTION('ref_axis',(1.,0.,0.));
#43580=DIRECTION('center_axis',(1.,0.,0.));
#43581=DIRECTION('ref_axis',(0.,1.,0.));
#43582=DIRECTION('center_axis',(1.,0.,0.));
#43583=DIRECTION('ref_axis',(0.,0.,-1.));
#43584=DIRECTION('',(1.,0.,0.));
#43585=DIRECTION('center_axis',(-1.,-5.53814966532964E-9,-3.76666845086606E-9));
#43586=DIRECTION('ref_axis',(3.76666845861945E-9,-1.40000233628258E-9,-1.));
#43587=DIRECTION('',(1.,0.,0.));
#43588=DIRECTION('center_axis',(0.,-1.,0.));
#43589=DIRECTION('ref_axis',(1.,0.,0.));
#43590=DIRECTION('center_axis',(-1.,0.,0.));
#43591=DIRECTION('ref_axis',(0.,1.,0.));
#43592=DIRECTION('center_axis',(0.,0.,1.));
#43593=DIRECTION('ref_axis',(1.,0.,0.));
#43594=DIRECTION('center_axis',(-1.,0.,0.));
#43595=DIRECTION('ref_axis',(0.,1.,0.));
#43596=DIRECTION('center_axis',(0.,-1.,0.));
#43597=DIRECTION('ref_axis',(1.,0.,0.));
#43598=DIRECTION('',(0.,1.,0.));
#43599=DIRECTION('',(0.,1.,0.));
#43600=DIRECTION('center_axis',(-1.,0.,0.));
#43601=DIRECTION('ref_axis',(0.,0.687200931805355,-0.726467397290376));
#43602=DIRECTION('center_axis',(1.,0.,0.));
#43603=DIRECTION('ref_axis',(0.,1.,0.));
#43604=DIRECTION('',(-1.,0.,0.));
#43605=DIRECTION('center_axis',(0.,0.,1.));
#43606=DIRECTION('ref_axis',(1.,0.,0.));
#43607=DIRECTION('',(0.,0.,-1.));
#43608=DIRECTION('center_axis',(0.,6.12323399574E-17,1.));
#43609=DIRECTION('ref_axis',(1.,0.,0.));
#43610=DIRECTION('',(0.,0.,-1.));
#43611=DIRECTION('center_axis',(-1.,0.,0.));
#43612=DIRECTION('ref_axis',(0.,-0.419820362992804,-0.907607218358575));
#43613=DIRECTION('center_axis',(1.,0.,0.));
#43614=DIRECTION('ref_axis',(0.,1.,0.));
#43615=DIRECTION('center_axis',(0.,-1.,0.));
#43616=DIRECTION('ref_axis',(1.,0.,0.));
#43617=DIRECTION('center_axis',(1.,0.,0.));
#43618=DIRECTION('ref_axis',(0.,1.,0.));
#43619=DIRECTION('center_axis',(0.,-0.907607218358575,0.419820362992804));
#43620=DIRECTION('ref_axis',(1.,0.,0.));
#43621=DIRECTION('center_axis',(0.,0.907607218358575,-0.419820362992804));
#43622=DIRECTION('ref_axis',(-1.,0.,0.));
#43623=DIRECTION('',(0.,0.907607218358575,-0.419820362992804));
#43624=DIRECTION('',(0.,0.907607218358575,-0.419820362992804));
#43625=DIRECTION('center_axis',(0.,-0.907607218358575,0.419820362992804));
#43626=DIRECTION('ref_axis',(1.,0.,0.));
#43627=DIRECTION('center_axis',(1.,0.,0.));
#43628=DIRECTION('ref_axis',(0.,1.,0.));
#43629=DIRECTION('center_axis',(1.,0.,0.));
#43630=DIRECTION('ref_axis',(0.,1.,0.));
#43631=DIRECTION('',(0.,0.973671472169394,0.227955838450093));
#43632=DIRECTION('center_axis',(-1.,0.,0.));
#43633=DIRECTION('ref_axis',(0.,1.,0.));
#43634=DIRECTION('',(0.,1.,0.));
#43635=DIRECTION('center_axis',(1.,0.,0.));
#43636=DIRECTION('ref_axis',(0.,1.,0.));
#43637=DIRECTION('',(0.,0.,1.));
#43638=DIRECTION('center_axis',(1.,0.,0.));
#43639=DIRECTION('ref_axis',(0.,1.,0.));
#43640=DIRECTION('',(0.,-1.,0.));
#43641=DIRECTION('center_axis',(-1.,0.,0.));
#43642=DIRECTION('ref_axis',(0.,1.,0.));
#43643=DIRECTION('',(0.,-0.901003410349976,0.433812003680988));
#43644=DIRECTION('center_axis',(1.,0.,0.));
#43645=DIRECTION('ref_axis',(0.,1.,0.));
#43646=DIRECTION('center_axis',(-1.,0.,0.));
#43647=DIRECTION('ref_axis',(0.,0.727396432986313,-0.686217479578295));
#43648=DIRECTION('center_axis',(0.,-0.672677186066802,-0.739936080580782));
#43649=DIRECTION('ref_axis',(1.,0.,0.));
#43650=DIRECTION('center_axis',(0.,-0.86993736790158,0.493162220702754));
#43651=DIRECTION('ref_axis',(0.,0.493162220702747,0.869937367901583));
#43652=DIRECTION('center_axis',(0.,-0.973671472169394,-0.227955838450093));
#43653=DIRECTION('ref_axis',(1.,0.,0.));
#43654=DIRECTION('center_axis',(0.,-0.973671472169394,-0.227955838450093));
#43655=DIRECTION('ref_axis',(0.,-0.227955838450093,0.973671472169394));
#43656=DIRECTION('center_axis',(0.,-0.973671472169394,-0.227955838450093));
#43657=DIRECTION('ref_axis',(1.,0.,0.));
#43658=DIRECTION('center_axis',(-1.,0.,0.));
#43659=DIRECTION('ref_axis',(0.,0.419820362992802,0.907607218358576));
#43660=DIRECTION('center_axis',(-1.,0.,0.));
#43661=DIRECTION('ref_axis',(0.,-1.,0.));
#43662=DIRECTION('center_axis',(-1.,0.,0.));
#43663=DIRECTION('ref_axis',(0.,-0.227955838450089,0.973671472169395));
#43664=DIRECTION('',(1.,0.,0.));
#43665=DIRECTION('center_axis',(0.,0.419820362992804,0.907607218358575));
#43666=DIRECTION('ref_axis',(1.,0.,0.));
#43667=DIRECTION('',(1.,0.,0.));
#43668=DIRECTION('center_axis',(1.,0.,0.));
#43669=DIRECTION('ref_axis',(0.,-0.419820362992804,-0.907607218358575));
#43670=DIRECTION('',(1.,0.,0.));
#43671=DIRECTION('center_axis',(0.,0.,1.));
#43672=DIRECTION('ref_axis',(1.,0.,0.));
#43673=DIRECTION('',(0.,1.,0.));
#43674=DIRECTION('',(0.,-1.,0.));
#43675=DIRECTION('',(1.,0.,0.));
#43676=DIRECTION('center_axis',(0.,1.,0.));
#43677=DIRECTION('ref_axis',(-1.,0.,0.));
#43678=DIRECTION('center_axis',(0.,-1.,-1.48029736617E-15));
#43679=DIRECTION('ref_axis',(1.,0.,0.));
#43680=DIRECTION('center_axis',(-1.,0.,0.));
#43681=DIRECTION('ref_axis',(0.,6.34413156928661E-16,-1.));
#43682=DIRECTION('center_axis',(1.,0.,0.));
#43683=DIRECTION('ref_axis',(0.,1.,0.));
#43684=DIRECTION('center_axis',(0.,0.,-1.));
#43685=DIRECTION('ref_axis',(1.,0.,0.));
#43686=DIRECTION('center_axis',(0.,0.,-1.));
#43687=DIRECTION('ref_axis',(0.,-1.,0.));
#43688=DIRECTION('',(0.,0.,1.));
#43689=DIRECTION('center_axis',(0.,1.67945721619E-15,-1.));
#43690=DIRECTION('ref_axis',(1.,0.,0.));
#43691=DIRECTION('center_axis',(-1.,0.,0.));
#43692=DIRECTION('ref_axis',(0.,1.,-1.26882631385732E-15));
#43693=DIRECTION('center_axis',(1.,0.,0.));
#43694=DIRECTION('ref_axis',(0.,1.,0.));
#43695=DIRECTION('center_axis',(0.,1.,0.));
#43696=DIRECTION('ref_axis',(1.,0.,0.));
#43697=DIRECTION('center_axis',(0.,1.,0.));
#43698=DIRECTION('ref_axis',(0.,0.,-1.));
#43699=DIRECTION('',(0.,-1.,0.));
#43700=DIRECTION('center_axis',(0.,1.,-4.99600361081E-16));
#43701=DIRECTION('ref_axis',(1.,0.,0.));
#43702=DIRECTION('center_axis',(-1.,0.,0.));
#43703=DIRECTION('ref_axis',(0.,-0.433812003680988,-0.901003410349975));
#43704=DIRECTION('center_axis',(-1.,0.,0.));
#43705=DIRECTION('ref_axis',(0.,1.,0.));
#43706=DIRECTION('center_axis',(0.,0.901003410349976,-0.433812003680988));
#43707=DIRECTION('ref_axis',(1.,0.,0.));
#43708=DIRECTION('center_axis',(-9.62964972193618E-33,0.901003410349976,
-0.433812003680988));
#43709=DIRECTION('ref_axis',(6.43494414306736E-48,-0.433812003680988,-0.901003410349976));
#43710=DIRECTION('',(0.,-0.901003410349976,0.433812003680988));
#43711=DIRECTION('center_axis',(0.,0.901003410349976,-0.433812003680988));
#43712=DIRECTION('ref_axis',(1.,0.,0.));
#43713=DIRECTION('center_axis',(-1.,0.,0.));
#43714=DIRECTION('ref_axis',(0.,0.433812003680988,0.901003410349976));
#43715=DIRECTION('center_axis',(1.,0.,0.));
#43716=DIRECTION('ref_axis',(0.,1.,0.));
#43717=DIRECTION('center_axis',(1.,0.,0.));
#43718=DIRECTION('ref_axis',(0.,0.433812003680988,0.901003410349976));
#43719=DIRECTION('',(1.,0.,0.));
#43720=DIRECTION('',(1.,0.,0.));
#43721=DIRECTION('center_axis',(0.,0.433812003680988,0.901003410349976));
#43722=DIRECTION('ref_axis',(1.,0.,0.));
#43723=DIRECTION('',(-1.,0.,0.));
#43724=DIRECTION('',(0.,0.901003410349976,-0.433812003680988));
#43725=DIRECTION('center_axis',(1.,0.,0.));
#43726=DIRECTION('ref_axis',(0.,-0.433812003680988,-0.901003410349976));
#43727=DIRECTION('',(-1.,0.,0.));
#43728=DIRECTION('center_axis',(0.,0.,1.));
#43729=DIRECTION('ref_axis',(1.,0.,0.));
#43730=DIRECTION('',(1.,0.,0.));
#43731=DIRECTION('center_axis',(1.,0.,0.));
#43732=DIRECTION('ref_axis',(0.,1.,0.));
#43733=DIRECTION('',(1.,0.,0.));
#43734=DIRECTION('center_axis',(0.,1.,0.));
#43735=DIRECTION('ref_axis',(1.,0.,0.));
#43736=DIRECTION('',(1.,0.,0.));
#43737=DIRECTION('center_axis',(1.,0.,0.));
#43738=DIRECTION('ref_axis',(0.,0.,-1.));
#43739=DIRECTION('center_axis',(-1.,0.,0.));
#43740=DIRECTION('ref_axis',(0.,1.,0.));
#43741=DIRECTION('center_axis',(0.,1.,0.));
#43742=DIRECTION('ref_axis',(1.,0.,0.));
#43743=DIRECTION('center_axis',(-1.,0.,0.));
#43744=DIRECTION('ref_axis',(0.,1.,0.));
#43745=DIRECTION('center_axis',(0.,1.,0.));
#43746=DIRECTION('ref_axis',(1.,0.,0.));
#43747=DIRECTION('center_axis',(3.93130878897075E-8,0.999999999999998,-3.93130878897075E-8));
#43748=DIRECTION('ref_axis',(0.707106723310616,4.55056292462304E-15,0.707106839062474));
#43749=DIRECTION('',(0.,-1.,0.));
#43750=DIRECTION('center_axis',(-0.0173649780999165,0.99984921740008,-1.91423167460546E-7));
#43751=DIRECTION('ref_axis',(0.760990338834415,0.0132166975786665,0.648628570990977));
#43752=DIRECTION('center_axis',(1.,0.,0.));
#43753=DIRECTION('ref_axis',(0.,-1.,0.));
#43754=DIRECTION('center_axis',(0.,0.994202177480807,0.107526881719979));
#43755=DIRECTION('ref_axis',(1.,0.,0.));
#43756=DIRECTION('center_axis',(-1.,0.,0.));
#43757=DIRECTION('ref_axis',(0.,-1.,0.));
#43758=DIRECTION('',(-1.,0.,0.));
#43759=DIRECTION('center_axis',(1.,0.,0.));
#43760=DIRECTION('ref_axis',(0.,-2.09002828430941E-15,-1.));
#43761=DIRECTION('',(-1.,0.,0.));
#43762=DIRECTION('center_axis',(-1.,0.,0.));
#43763=DIRECTION('ref_axis',(0.,1.,0.));
#43764=DIRECTION('center_axis',(-1.,0.,0.));
#43765=DIRECTION('ref_axis',(0.,-0.107526881719978,-0.994202177480807));
#43766=DIRECTION('',(-1.,0.,0.));
#43767=DIRECTION('center_axis',(1.,0.,0.));
#43768=DIRECTION('ref_axis',(0.,1.,0.));
#43769=DIRECTION('center_axis',(1.,0.,0.));
#43770=DIRECTION('ref_axis',(0.,0.930044067784185,0.367447999014073));
#43771=DIRECTION('',(-1.,0.,0.));
#43772=DIRECTION('center_axis',(1.,8.3307817066003E-9,3.39356925084603E-10));
#43773=DIRECTION('ref_axis',(-3.41030038156647E-10,0.000200933687209084,
0.999999979812826));
#43774=DIRECTION('center_axis',(0.,0.,1.));
#43775=DIRECTION('ref_axis',(1.,0.,0.));
#43776=DIRECTION('center_axis',(0.0173652351998802,-0.999849212934857,-1.53755357850641E-12));
#43777=DIRECTION('ref_axis',(0.760979857924961,0.0132165871066167,-0.648640869555534));
#43778=DIRECTION('center_axis',(0.0118197508200445,-0.999930144305366,-3.90308482337882E-8));
#43779=DIRECTION('ref_axis',(0.727691598926711,0.00860176102447277,-0.685850527854842));
#43780=DIRECTION('center_axis',(0.,-0.994202177480807,0.107526881719979));
#43781=DIRECTION('ref_axis',(1.,0.,0.));
#43782=DIRECTION('center_axis',(-1.,0.,0.));
#43783=DIRECTION('ref_axis',(0.,0.107526881719979,-0.994202177480807));
#43784=DIRECTION('center_axis',(-1.,0.,0.));
#43785=DIRECTION('ref_axis',(0.,1.,0.));
#43786=DIRECTION('center_axis',(-0.0103216872828093,-0.900955413872221,
0.43378889449359));
#43787=DIRECTION('ref_axis',(0.726589340957755,-0.304799871633038,-0.615763727300544));
#43788=DIRECTION('center_axis',(-9.83007148257777E-8,-0.901003452989707,
0.433811915120616));
#43789=DIRECTION('ref_axis',(0.707106781770852,-0.306751409315773,-0.637105620801179));
#43790=DIRECTION('center_axis',(8.58451173878204E-29,-0.901003410349976,
0.433812003680988));
#43791=DIRECTION('ref_axis',(1.,7.73467435283202E-29,-3.724064238024E-29));
#43792=DIRECTION('',(0.,0.901003410349976,-0.433812003680988));
#43793=DIRECTION('center_axis',(1.,0.,0.));
#43794=DIRECTION('ref_axis',(0.,1.,0.));
#43795=DIRECTION('axis',(0.,0.,1.));
#43796=DIRECTION('refdir',(1.,0.,0.));
#43797=DIRECTION('center_axis',(0.,1.,0.));
#43798=DIRECTION('ref_axis',(0.,0.,1.));
#43799=DIRECTION('center_axis',(0.,1.,0.));
#43800=DIRECTION('ref_axis',(0.,0.,1.));
#43801=DIRECTION('center_axis',(0.,1.,0.));
#43802=DIRECTION('ref_axis',(0.,0.,1.));
#43803=DIRECTION('center_axis',(0.,-1.,0.));
#43804=DIRECTION('ref_axis',(0.,0.,-1.));
#43805=DIRECTION('center_axis',(0.,1.,0.));
#43806=DIRECTION('ref_axis',(0.,0.,1.));
#43807=DIRECTION('center_axis',(0.,-1.,0.));
#43808=DIRECTION('ref_axis',(0.,0.,-1.));
#43809=DIRECTION('center_axis',(0.,-1.,0.));
#43810=DIRECTION('ref_axis',(0.,0.,1.));
#43811=DIRECTION('center_axis',(0.,-1.,0.));
#43812=DIRECTION('ref_axis',(0.,0.,1.));
#43813=DIRECTION('',(8.65956056235493E-17,0.707106781186548,-0.707106781186547));
#43814=DIRECTION('center_axis',(0.,1.,0.));
#43815=DIRECTION('ref_axis',(0.,0.,1.));
#43816=DIRECTION('center_axis',(0.,-1.,0.));
#43817=DIRECTION('ref_axis',(-6.04901474818E-16,0.,1.));
#43818=DIRECTION('center_axis',(0.,1.,0.));
#43819=DIRECTION('ref_axis',(4.81230659094137E-15,0.,1.));
#43820=DIRECTION('',(0.,-1.,0.));
#43821=DIRECTION('',(0.,-1.,0.));
#43822=DIRECTION('center_axis',(0.,-1.,0.));
#43823=DIRECTION('ref_axis',(1.,0.,0.));
#43824=DIRECTION('',(0.,-1.,0.));
#43825=DIRECTION('',(0.,-1.,0.));
#43826=DIRECTION('center_axis',(0.,1.,0.));
#43827=DIRECTION('ref_axis',(1.,0.,0.));
#43828=DIRECTION('center_axis',(0.,1.,0.));
#43829=DIRECTION('ref_axis',(0.,0.,1.));
#43830=DIRECTION('center_axis',(0.,-1.,0.));
#43831=DIRECTION('ref_axis',(1.,0.,0.));
#43832=DIRECTION('center_axis',(0.,1.,0.));
#43833=DIRECTION('ref_axis',(1.,0.,0.));
#43834=DIRECTION('',(-1.,0.,0.));
#43835=DIRECTION('center_axis',(0.,1.,0.));
#43836=DIRECTION('ref_axis',(1.,0.,0.));
#43837=DIRECTION('',(-1.,0.,0.));
#43838=DIRECTION('center_axis',(0.,1.,0.));
#43839=DIRECTION('ref_axis',(1.,0.,0.));
#43840=DIRECTION('center_axis',(0.,0.,1.));
#43841=DIRECTION('ref_axis',(1.,0.,0.));
#43842=DIRECTION('',(0.,1.,0.));
#43843=DIRECTION('',(0.,1.,0.));
#43844=DIRECTION('',(-1.,0.,0.));
#43845=DIRECTION('center_axis',(0.,0.,1.));
#43846=DIRECTION('ref_axis',(1.,0.,0.));
#43847=DIRECTION('',(-1.,0.,0.));
#43848=DIRECTION('',(0.,1.,0.));
#43849=DIRECTION('',(0.,1.,0.));
#43850=DIRECTION('center_axis',(0.,-1.,0.));
#43851=DIRECTION('ref_axis',(0.,0.,-1.));
#43852=DIRECTION('center_axis',(0.,-1.,0.));
#43853=DIRECTION('ref_axis',(1.,0.,0.));
#43854=DIRECTION('center_axis',(0.,-1.,0.));
#43855=DIRECTION('ref_axis',(1.,0.,0.));
#43856=DIRECTION('center_axis',(0.,1.,0.));
#43857=DIRECTION('ref_axis',(1.,0.,0.));
#43858=DIRECTION('',(-1.,0.,0.));
#43859=DIRECTION('center_axis',(0.,1.,0.));
#43860=DIRECTION('ref_axis',(1.,0.,0.));
#43861=DIRECTION('',(-1.,0.,0.));
#43862=DIRECTION('center_axis',(0.,1.,0.));
#43863=DIRECTION('ref_axis',(1.,0.,0.));
#43864=DIRECTION('center_axis',(0.,0.,1.));
#43865=DIRECTION('ref_axis',(1.,0.,0.));
#43866=DIRECTION('',(0.,1.,0.));
#43867=DIRECTION('',(-1.,0.,0.));
#43868=DIRECTION('',(0.,1.,0.));
#43869=DIRECTION('center_axis',(0.,0.,1.));
#43870=DIRECTION('ref_axis',(1.,0.,0.));
#43871=DIRECTION('',(0.,1.,0.));
#43872=DIRECTION('',(-1.,0.,0.));
#43873=DIRECTION('',(0.,1.,0.));
#43874=DIRECTION('center_axis',(0.,-1.,0.));
#43875=DIRECTION('ref_axis',(0.,0.,-1.));
#43876=DIRECTION('center_axis',(0.,-1.,0.));
#43877=DIRECTION('ref_axis',(1.,0.,0.));
#43878=DIRECTION('center_axis',(0.,-1.,0.));
#43879=DIRECTION('ref_axis',(1.,0.,0.));
#43880=DIRECTION('center_axis',(0.,1.,0.));
#43881=DIRECTION('ref_axis',(0.479425538604204,0.,0.877582561890372));
#43882=DIRECTION('center_axis',(0.,-1.,0.));
#43883=DIRECTION('ref_axis',(1.,0.,0.));
#43884=DIRECTION('',(0.,1.,0.));
#43885=DIRECTION('center_axis',(0.,1.,0.));
#43886=DIRECTION('ref_axis',(-0.971277075433192,0.,-0.237951345316528));
#43887=DIRECTION('',(0.,-1.,0.));
#43888=DIRECTION('center_axis',(0.,-1.,0.));
#43889=DIRECTION('ref_axis',(1.,0.,0.));
#43890=DIRECTION('',(0.,-1.,0.));
#43891=DIRECTION('center_axis',(0.,1.,0.));
#43892=DIRECTION('ref_axis',(-0.989856436210018,0.,0.142071234574779));
#43893=DIRECTION('',(0.,-1.,0.));
#43894=DIRECTION('center_axis',(0.,-1.,0.));
#43895=DIRECTION('ref_axis',(1.,0.,0.));
#43896=DIRECTION('',(0.,-1.,0.));
#43897=DIRECTION('center_axis',(0.,1.,0.));
#43898=DIRECTION('ref_axis',(-0.456844166721239,0.,0.889546742635134));
#43899=DIRECTION('',(0.,-1.,0.));
#43900=DIRECTION('center_axis',(0.,-1.,0.));
#43901=DIRECTION('ref_axis',(1.,0.,0.));
#43902=DIRECTION('',(0.,-1.,0.));
#43903=DIRECTION('center_axis',(0.,1.,0.));
#43904=DIRECTION('ref_axis',(-0.0624652415091979,0.,0.998047139970451));
#43905=DIRECTION('',(0.,-1.,0.));
#43906=DIRECTION('center_axis',(0.,1.,0.));
#43907=DIRECTION('ref_axis',(1.,0.,0.));
#43908=DIRECTION('',(0.,-1.,0.));
#43909=DIRECTION('center_axis',(0.,1.,0.));
#43910=DIRECTION('ref_axis',(0.361068082792987,0.,0.932539457389443));
#43911=DIRECTION('',(0.,-1.,0.));
#43912=DIRECTION('center_axis',(0.,1.,0.));
#43913=DIRECTION('ref_axis',(1.,0.,0.));
#43914=DIRECTION('',(0.,-1.,0.));
#43915=DIRECTION('center_axis',(0.,1.,0.));
#43916=DIRECTION('ref_axis',(0.479425538604341,0.,0.877582561890297));
#43917=DIRECTION('',(0.,-1.,0.));
#43918=DIRECTION('center_axis',(0.,-1.,0.));
#43919=DIRECTION('ref_axis',(1.,0.,0.));
#43920=DIRECTION('',(0.,-1.,0.));
#43921=DIRECTION('center_axis',(0.,1.,0.));
#43922=DIRECTION('ref_axis',(0.989856436210018,0.,-0.142071234574783));
#43923=DIRECTION('',(0.,-1.,0.));
#43924=DIRECTION('center_axis',(0.,-1.,0.));
#43925=DIRECTION('ref_axis',(1.,0.,0.));
#43926=DIRECTION('',(0.,-1.,0.));
#43927=DIRECTION('center_axis',(0.,1.,0.));
#43928=DIRECTION('ref_axis',(-0.971277075433192,0.,-0.237951345316528));
#43929=DIRECTION('center_axis',(0.,-1.,0.));
#43930=DIRECTION('ref_axis',(1.,0.,0.));
#43931=DIRECTION('',(0.,1.,0.));
#43932=DIRECTION('center_axis',(0.,-1.,0.));
#43933=DIRECTION('ref_axis',(1.,0.,0.));
#43934=DIRECTION('',(0.,1.,0.));
#43935=DIRECTION('center_axis',(0.,-1.,0.));
#43936=DIRECTION('ref_axis',(1.,0.,0.));
#43937=DIRECTION('',(0.,1.,0.));
#43938=DIRECTION('center_axis',(0.,1.,0.));
#43939=DIRECTION('ref_axis',(1.,0.,0.));
#43940=DIRECTION('',(0.,1.,0.));
#43941=DIRECTION('center_axis',(0.,1.,0.));
#43942=DIRECTION('ref_axis',(0.479425538604204,0.,0.877582561890372));
#43943=DIRECTION('',(0.,-1.,0.));
#43944=DIRECTION('center_axis',(0.,-1.,0.));
#43945=DIRECTION('ref_axis',(1.,0.,0.));
#43946=DIRECTION('',(0.,1.,0.));
#43947=DIRECTION('center_axis',(0.,1.,0.));
#43948=DIRECTION('ref_axis',(1.,0.,0.));
#43949=DIRECTION('',(0.,1.,0.));
#43950=DIRECTION('center_axis',(0.,1.,0.));
#43951=DIRECTION('ref_axis',(1.,0.,0.));
#43952=DIRECTION('',(0.,1.,0.));
#43953=DIRECTION('center_axis',(0.,-1.,0.));
#43954=DIRECTION('ref_axis',(1.,0.,0.));
#43955=DIRECTION('',(0.,1.,0.));
#43956=DIRECTION('center_axis',(0.,-1.,0.));
#43957=DIRECTION('ref_axis',(1.,0.,0.));
#43958=DIRECTION('center_axis',(-0.52238673488493,0.,-0.852708683675886));
#43959=DIRECTION('ref_axis',(-0.852708683675886,0.,0.52238673488493));
#43960=DIRECTION('',(0.85270868367354,0.,-0.522386734888759));
#43961=DIRECTION('',(0.,-1.,0.));
#43962=DIRECTION('',(0.852708683675886,0.,-0.52238673488493));
#43963=DIRECTION('center_axis',(0.52238673488493,0.,-0.852708683675886));
#43964=DIRECTION('ref_axis',(0.,-1.,0.));
#43965=DIRECTION('',(0.852708683675886,0.,0.52238673488493));
#43966=DIRECTION('',(0.,1.,0.));
#43967=DIRECTION('',(0.85270868366004,0.,0.522386734910796));
#43968=DIRECTION('center_axis',(0.,-1.,0.));
#43969=DIRECTION('ref_axis',(0.99973889499905,0.,-0.0228504228861944));
#43970=DIRECTION('center_axis',(0.,-1.,0.));
#43971=DIRECTION('ref_axis',(1.,0.,0.));
#43972=DIRECTION('center_axis',(0.,-1.,0.));
#43973=DIRECTION('ref_axis',(0.998419029265298,0.,0.0562089138921914));
#43974=DIRECTION('',(0.,1.,0.));
#43975=DIRECTION('center_axis',(0.,1.,0.));
#43976=DIRECTION('ref_axis',(-0.727788421795868,0.,-0.685801730166876));
#43977=DIRECTION('center_axis',(0.,-1.,0.));
#43978=DIRECTION('ref_axis',(0.928397903310364,0.,0.371587584734636));
#43979=DIRECTION('center_axis',(0.,-1.,0.));
#43980=DIRECTION('ref_axis',(1.,0.,0.));
#43981=DIRECTION('center_axis',(0.,-1.,0.));
#43982=DIRECTION('ref_axis',(0.985455636737957,0.,-0.169932892699993));
#43983=DIRECTION('',(0.,1.,0.));
#43984=DIRECTION('center_axis',(0.,1.,0.));
#43985=DIRECTION('ref_axis',(0.989299838612263,0.,-0.145896639172227));
#43986=DIRECTION('',(0.,-1.,0.));
#43987=DIRECTION('center_axis',(0.,1.,0.));
#43988=DIRECTION('ref_axis',(1.,0.,0.));
#43989=DIRECTION('center_axis',(0.,1.,0.));
#43990=DIRECTION('ref_axis',(0.115367964260996,0.,0.99332282407195));
#43991=DIRECTION('',(0.,-1.,0.));
#43992=DIRECTION('center_axis',(-1.93875202872386E-14,-1.,-1.52293552293204E-14));
#43993=DIRECTION('ref_axis',(0.291057680790064,-2.2204460492503E-14,0.956705506649308));
#43994=DIRECTION('center_axis',(0.,1.,0.));
#43995=DIRECTION('ref_axis',(1.,0.,0.));
#43996=DIRECTION('center_axis',(0.,1.,0.));
#43997=DIRECTION('ref_axis',(-0.291057680714125,0.,-0.956705506672411));
#43998=DIRECTION('center_axis',(0.,1.,0.));
#43999=DIRECTION('ref_axis',(1.,0.,0.));
#44000=DIRECTION('',(0.,-1.,0.));
#44001=DIRECTION('center_axis',(0.,-1.,0.));
#44002=DIRECTION('ref_axis',(-0.291057680796176,0.,-0.956705506647449));
#44003=DIRECTION('center_axis',(0.52238673488493,0.,-0.852708683675886));
#44004=DIRECTION('ref_axis',(0.,-1.,0.));
#44005=DIRECTION('',(-0.852708683675886,0.,-0.52238673488493));
#44006=DIRECTION('',(-0.852708683677683,0.,-0.522386734881996));
#44007=DIRECTION('center_axis',(0.,-1.,0.));
#44008=DIRECTION('ref_axis',(-0.98929983861229,0.,0.145896639172043));
#44009=DIRECTION('center_axis',(0.,1.,0.));
#44010=DIRECTION('ref_axis',(1.,0.,0.));
#44011=DIRECTION('center_axis',(0.,-1.,0.));
#44012=DIRECTION('ref_axis',(-0.52238673496676,0.,-0.852708683625755));
#44013=DIRECTION('',(0.,-1.,0.));
#44014=DIRECTION('center_axis',(0.,-1.,0.));
#44015=DIRECTION('ref_axis',(0.,0.,-1.));
#44016=DIRECTION('',(0.852708683675886,0.,-0.52238673488493));
#44017=DIRECTION('center_axis',(-0.52238673488493,0.,-0.852708683675886));
#44018=DIRECTION('ref_axis',(-0.852708683675886,0.,0.52238673488493));
#44019=DIRECTION('',(0.852708683678698,0.,-0.52238673488034));
#44020=DIRECTION('center_axis',(0.,-1.,0.));
#44021=DIRECTION('ref_axis',(0.952171177670241,0.,0.305565129578075));
#44022=DIRECTION('center_axis',(0.,1.,0.));
#44023=DIRECTION('ref_axis',(0.952171177838408,0.,0.305565129054051));
#44024=DIRECTION('',(0.,1.,0.));
#44025=DIRECTION('center_axis',(0.,-1.,0.));
#44026=DIRECTION('ref_axis',(1.,0.,0.));
#44027=DIRECTION('',(0.,1.,0.));
#44028=DIRECTION('center_axis',(0.952171177670241,0.,0.305565129578077));
#44029=DIRECTION('ref_axis',(0.,-1.,0.));
#44030=DIRECTION('',(0.305565129583039,0.,-0.952171177668648));
#44031=DIRECTION('',(0.,1.,0.));
#44032=DIRECTION('',(-0.305565129578077,0.,0.952171177670241));
#44033=DIRECTION('center_axis',(0.,-1.,0.));
#44034=DIRECTION('ref_axis',(-0.184788912514002,0.,-0.982778234299016));
#44035=DIRECTION('center_axis',(0.,1.,0.));
#44036=DIRECTION('ref_axis',(1.,0.,0.));
#44037=DIRECTION('center_axis',(0.,1.,0.));
#44038=DIRECTION('ref_axis',(1.,0.,0.));
#44039=DIRECTION('',(0.,-1.,0.));
#44040=DIRECTION('center_axis',(0.,1.,0.));
#44041=DIRECTION('ref_axis',(1.,0.,0.));
#44042=DIRECTION('center_axis',(0.982778234299016,0.,-0.184788912514004));
#44043=DIRECTION('ref_axis',(0.184788912514004,0.,0.982778234299016));
#44044=DIRECTION('center_axis',(-0.305565129578077,0.,0.952171177670241));
#44045=DIRECTION('ref_axis',(0.952171177670241,0.,0.305565129578077));
#44046=DIRECTION('center_axis',(-0.305565129578077,7.88432920788926E-29,
0.952171177670241));
#44047=DIRECTION('ref_axis',(-2.4091760760449E-29,-1.,7.50723102701579E-29));
#44048=DIRECTION('',(0.305565129578077,0.,-0.952171177670241));
#44049=DIRECTION('',(0.305565129578077,0.,-0.952171177670241));
#44050=DIRECTION('center_axis',(0.952171177670241,0.,0.305565129578077));
#44051=DIRECTION('ref_axis',(0.,-1.,0.));
#44052=DIRECTION('',(0.305565129578077,0.,-0.952171177670241));
#44053=DIRECTION('center_axis',(0.952171177669702,-1.65558619039422E-11,
0.305565129579756));
#44054=DIRECTION('ref_axis',(0.305564047343791,0.00266148306317448,-0.952167805315211));
#44055=DIRECTION('',(0.,-1.,0.));
#44056=DIRECTION('',(0.305565129582466,0.,-0.952171177668832));
#44057=DIRECTION('center_axis',(0.,1.,0.));
#44058=DIRECTION('ref_axis',(0.593785833940128,0.,-0.80462313129317));
#44059=DIRECTION('',(0.,-1.,0.));
#44060=DIRECTION('center_axis',(0.,1.,0.));
#44061=DIRECTION('ref_axis',(-0.952171177741116,0.,-0.305565129357222));
#44062=DIRECTION('center_axis',(0.593785833940127,0.,-0.804623131293172));
#44063=DIRECTION('ref_axis',(0.,-1.,0.));
#44064=DIRECTION('',(0.804623131293172,0.,0.593785833940126));
#44065=DIRECTION('',(0.804623131286062,0.,0.59378583394976));
#44066=DIRECTION('center_axis',(0.,1.,0.));
#44067=DIRECTION('ref_axis',(0.952171177670241,0.,0.305565129578075));
#44068=DIRECTION('center_axis',(0.,1.,0.));
#44069=DIRECTION('ref_axis',(-0.0867961056866223,0.,-0.996226096846312));
#44070=DIRECTION('',(0.,1.,0.));
#44071=DIRECTION('center_axis',(0.,-1.,0.));
#44072=DIRECTION('ref_axis',(1.,0.,0.));
#44073=DIRECTION('center_axis',(-0.305565319408436,1.99282937676548E-7,
0.952171116750966));
#44074=DIRECTION('ref_axis',(0.673337440012041,0.70705348480321,0.216083459583719));
#44075=DIRECTION('center_axis',(-0.804623131293172,2.27430927210528E-28,
-0.593785833940127));
#44076=DIRECTION('ref_axis',(-1.82996184805045E-28,-1.,-1.3504526277748E-28));
#44077=DIRECTION('',(0.804623131293172,0.,0.593785833940126));
#44078=DIRECTION('center_axis',(-0.333863836923852,0.942595934464823,0.00691684356269561));
#44079=DIRECTION('ref_axis',(-0.166136836043399,-0.0516188462595087,-0.984750753449992));
#44080=DIRECTION('center_axis',(0.502343691929506,0.859201694775685,-0.097073492124394));
#44081=DIRECTION('ref_axis',(-0.189730325478445,-5.12579610074604E-7,-0.981836240721222));
#44082=DIRECTION('center_axis',(0.,-1.,0.));
#44083=DIRECTION('ref_axis',(0.952171177670241,0.,0.305565129578077));
#44084=DIRECTION('center_axis',(-0.305565129578077,0.,0.952171177670241));
#44085=DIRECTION('ref_axis',(0.952171177670241,0.,0.305565129578077));
#44086=DIRECTION('center_axis',(0.305565129578077,0.,-0.952171177670241));
#44087=DIRECTION('ref_axis',(-0.952171177670241,0.,-0.305565129578077));
#44088=DIRECTION('',(0.305565129578077,0.,-0.952171177670241));
#44089=DIRECTION('center_axis',(0.,-1.,0.));
#44090=DIRECTION('ref_axis',(0.,0.,-1.));
#44091=DIRECTION('',(-0.804623131293172,0.,-0.593785833940126));
#44092=DIRECTION('center_axis',(0.750531794611774,0.36046055254421,0.55386840976567));
#44093=DIRECTION('ref_axis',(0.593786291820652,-9.54831594281741E-7,-0.804622793391393));
#44094=DIRECTION('center_axis',(0.,-1.,0.));
#44095=DIRECTION('ref_axis',(-0.189730742490933,0.,-0.981836160137647));
#44096=DIRECTION('center_axis',(-1.16339964917462E-14,1.,5.14376914730547E-14));
#44097=DIRECTION('ref_axis',(-0.189730742488058,4.88498130835068E-14,-0.981836160138203));
#44098=DIRECTION('',(0.,1.,0.));
#44099=DIRECTION('center_axis',(0.802919848716691,0.065033315405924,0.592528804720985));
#44100=DIRECTION('ref_axis',(-0.377801654618901,-0.713357017301177,0.590243742562671));
#44101=DIRECTION('center_axis',(-0.593785832104614,-6.52095874072556E-8,
0.804623132647718));
#44102=DIRECTION('ref_axis',(0.799228849499735,-0.115599692127252,0.589805016346432));
#44103=DIRECTION('center_axis',(0.804623251118834,-2.01435901831212E-7,
0.593785671567542));
#44104=DIRECTION('ref_axis',(0.419901543670372,0.707053636580093,-0.568997230768397));
#44105=DIRECTION('center_axis',(-0.804623131293172,0.,-0.593785833940127));
#44106=DIRECTION('ref_axis',(0.593785833940127,0.,-0.804623131293172));
#44107=DIRECTION('',(-0.804623131293172,0.,-0.593785833940126));
#44108=DIRECTION('center_axis',(0.593785833940127,0.,-0.804623131293172));
#44109=DIRECTION('ref_axis',(0.,-1.,0.));
#44110=DIRECTION('',(-0.804623131292045,0.,-0.593785833941653));
#44111=DIRECTION('center_axis',(0.,-1.,0.));
#44112=DIRECTION('ref_axis',(0.0149833744096974,0.,-0.999887742944826));
#44113=DIRECTION('',(0.,1.,0.));
#44114=DIRECTION('center_axis',(0.,1.,0.));
#44115=DIRECTION('ref_axis',(0.0149833744096974,0.,-0.999887742944826));
#44116=DIRECTION('center_axis',(0.,-1.,0.));
#44117=DIRECTION('ref_axis',(1.,0.,0.));
#44118=DIRECTION('center_axis',(0.,1.,0.));
#44119=DIRECTION('ref_axis',(-0.952171177670241,0.,0.305565129578075));
#44120=DIRECTION('center_axis',(0.,1.,0.));
#44121=DIRECTION('ref_axis',(1.,0.,0.));
#44122=DIRECTION('',(0.,1.,0.));
#44123=DIRECTION('center_axis',(0.,-1.,0.));
#44124=DIRECTION('ref_axis',(-0.952171177838413,0.,0.305565129054036));
#44125=DIRECTION('center_axis',(0.952171177670241,0.,-0.305565129578077));
#44126=DIRECTION('ref_axis',(0.,-1.,0.));
#44127=DIRECTION('',(0.305565129578077,0.,0.952171177670241));
#44128=DIRECTION('',(0.,1.,0.));
#44129=DIRECTION('',(-0.305565129583039,0.,-0.952171177668648));
#44130=DIRECTION('center_axis',(0.,1.,0.));
#44131=DIRECTION('ref_axis',(0.184788912514002,0.,-0.982778234299016));
#44132=DIRECTION('',(0.,-1.,0.));
#44133=DIRECTION('center_axis',(0.,-1.,0.));
#44134=DIRECTION('ref_axis',(1.,0.,0.));
#44135=DIRECTION('center_axis',(0.,-1.,0.));
#44136=DIRECTION('ref_axis',(1.,0.,0.));
#44137=DIRECTION('center_axis',(-0.305565129578077,0.,-0.952171177670241));
#44138=DIRECTION('ref_axis',(0.952171177670241,0.,-0.305565129578077));
#44139=DIRECTION('center_axis',(0.982778234299016,0.,0.184788912514004));
#44140=DIRECTION('ref_axis',(0.184788912514004,0.,-0.982778234299016));
#44141=DIRECTION('center_axis',(0.,-1.,0.));
#44142=DIRECTION('ref_axis',(1.,0.,0.));
#44143=DIRECTION('center_axis',(0.,-1.,0.));
#44144=DIRECTION('ref_axis',(0.,0.,-1.));
#44145=DIRECTION('',(-0.305565129578077,0.,-0.952171177670241));
#44146=DIRECTION('center_axis',(0.,1.,0.));
#44147=DIRECTION('ref_axis',(1.,0.,0.));
#44148=DIRECTION('center_axis',(0.,-1.,0.));
#44149=DIRECTION('ref_axis',(1.,0.,0.));
#44150=DIRECTION('center_axis',(0.,1.,0.));
#44151=DIRECTION('ref_axis',(1.,0.,0.));
#44152=DIRECTION('center_axis',(-0.305565129578077,-7.88432920788926E-29,
-0.952171177670241));
#44153=DIRECTION('ref_axis',(2.4091760760449E-29,-1.,7.50723102701579E-29));
#44154=DIRECTION('',(-0.305565129578077,0.,-0.952171177670241));
#44155=DIRECTION('center_axis',(0.952171177670241,0.,-0.305565129578077));
#44156=DIRECTION('ref_axis',(0.,-1.,0.));
#44157=DIRECTION('',(-0.305565129582466,0.,-0.952171177668832));
#44158=DIRECTION('',(0.,-1.,0.));
#44159=DIRECTION('center_axis',(0.952171177669702,1.65558619039422E-11,
-0.305565129579756));
#44160=DIRECTION('ref_axis',(0.305564047343791,-0.00266148306317448,0.952167805315211));
#44161=DIRECTION('',(-0.305565129578077,0.,-0.952171177670241));
#44162=DIRECTION('center_axis',(0.,-1.,0.));
#44163=DIRECTION('ref_axis',(-0.593785833940128,0.,-0.80462313129317));
#44164=DIRECTION('center_axis',(0.,-1.,0.));
#44165=DIRECTION('ref_axis',(0.952171177741116,0.,-0.305565129357222));
#44166=DIRECTION('',(0.,-1.,0.));
#44167=DIRECTION('center_axis',(2.16551588832688E-7,-0.999999999999974,
6.99060910068197E-8));
#44168=DIRECTION('ref_axis',(0.952171197960148,1.84833326422045E-7,-0.305565066352654));
#44169=DIRECTION('center_axis',(0.593785833940127,0.,0.804623131293172));
#44170=DIRECTION('ref_axis',(0.,-1.,0.));
#44171=DIRECTION('',(-0.804623131286062,0.,0.59378583394976));
#44172=DIRECTION('',(-0.804623131293172,0.,0.593785833940126));
#44173=DIRECTION('center_axis',(0.,-1.,0.));
#44174=DIRECTION('ref_axis',(-0.952171177670241,0.,0.305565129578075));
#44175=DIRECTION('',(0.,1.,0.));
#44176=DIRECTION('center_axis',(-3.88771230906498E-14,-1.,-3.10280620461979E-14));
#44177=DIRECTION('ref_axis',(0.0867961056866264,2.22044604925032E-14,-0.996226096846311));
#44178=DIRECTION('center_axis',(0.,-1.,0.));
#44179=DIRECTION('ref_axis',(0.105128000466025,0.,-0.994458698749232));
#44180=DIRECTION('center_axis',(0.,1.,0.));
#44181=DIRECTION('ref_axis',(0.086796105653726,0.,0.996226096849178));
#44182=DIRECTION('center_axis',(0.,-1.,0.));
#44183=DIRECTION('ref_axis',(-3.7470027081099E-16,0.,1.));
#44184=DIRECTION('center_axis',(0.999100306362134,-5.17100303120544E-8,
-0.04240964309078));
#44185=DIRECTION('ref_axis',(0.0424096425034725,0.000167646473684586,0.999100292321741));
#44186=DIRECTION('center_axis',(-0.305565353050774,-2.34615214704492E-7,
-0.95217110595465));
#44187=DIRECTION('ref_axis',(0.673337494350081,-0.70705342772588,-0.216083477025519));
#44188=DIRECTION('center_axis',(-0.804623131293172,-2.27430927210528E-28,
0.593785833940127));
#44189=DIRECTION('ref_axis',(1.82996184805045E-28,-1.,-1.3504526277748E-28));
#44190=DIRECTION('',(-0.804623131293172,0.,0.593785833940126));
#44191=DIRECTION('center_axis',(0.502343691929506,-0.859201694775685,0.097073492124394));
#44192=DIRECTION('ref_axis',(0.189730325478445,-5.12579610074604E-7,-0.981836240721222));
#44193=DIRECTION('center_axis',(-0.329648236156166,-0.942184923461378,-0.0601631980633227));
#44194=DIRECTION('ref_axis',(-0.00298910007657989,0.0647664414184453,-0.997895973208993));
#44195=DIRECTION('center_axis',(0.,-1.,0.));
#44196=DIRECTION('ref_axis',(-0.952171177670241,0.,0.305565129578077));
#44197=DIRECTION('center_axis',(-0.305565129578077,0.,-0.952171177670241));
#44198=DIRECTION('ref_axis',(0.952171177670241,0.,-0.305565129578077));
#44199=DIRECTION('center_axis',(0.305565129578077,0.,0.952171177670241));
#44200=DIRECTION('ref_axis',(0.952171177670241,0.,-0.305565129578077));
#44201=DIRECTION('',(-0.305565129578077,0.,-0.952171177670241));
#44202=DIRECTION('center_axis',(0.,-1.,0.));
#44203=DIRECTION('ref_axis',(0.,0.,-1.));
#44204=DIRECTION('',(0.804623131293172,0.,-0.593785833940126));
#44205=DIRECTION('center_axis',(0.750531467332585,-0.360460652348641,-0.553868788299169));
#44206=DIRECTION('ref_axis',(-0.593786666268931,-7.74994065794043E-7,-0.80462251706041));
#44207=DIRECTION('center_axis',(0.,1.,0.));
#44208=DIRECTION('ref_axis',(0.189730742490933,0.,-0.981836160137647));
#44209=DIRECTION('',(0.,1.,0.));
#44210=DIRECTION('center_axis',(0.,-1.,0.));
#44211=DIRECTION('ref_axis',(0.18973074248807,0.,-0.9818361601382));
#44212=DIRECTION('center_axis',(0.802920300631341,-0.0650326313851214,-0.592528267417854));
#44213=DIRECTION('ref_axis',(-0.377872514273543,0.713249764055606,-0.590327991061929));
#44214=DIRECTION('center_axis',(0.804623014253252,-1.97471803256364E-7,
-0.593785992537691));
#44215=DIRECTION('ref_axis',(0.419901584175499,-0.707053568412025,0.568997285584675));
#44216=DIRECTION('center_axis',(-0.593785832104614,6.52095874072556E-8,
-0.804623132647718));
#44217=DIRECTION('ref_axis',(0.799228849499735,0.115599692127252,-0.589805016346432));
#44218=DIRECTION('center_axis',(-0.804623131293172,0.,0.593785833940127));
#44219=DIRECTION('ref_axis',(-0.593785833940127,0.,-0.804623131293172));
#44220=DIRECTION('',(0.804623131293172,0.,-0.593785833940126));
#44221=DIRECTION('center_axis',(0.593785833940127,0.,0.804623131293172));
#44222=DIRECTION('ref_axis',(0.,-1.,0.));
#44223=DIRECTION('',(0.804623131292045,0.,-0.593785833941653));
#44224=DIRECTION('center_axis',(0.52238673488493,0.,0.852708683675886));
#44225=DIRECTION('ref_axis',(0.,-1.,0.));
#44226=DIRECTION('',(-0.85270868367354,0.,0.522386734888759));
#44227=DIRECTION('',(0.,-1.,0.));
#44228=DIRECTION('',(-0.852708683675886,0.,0.52238673488493));
#44229=DIRECTION('center_axis',(-0.52238673488493,0.,0.852708683675886));
#44230=DIRECTION('ref_axis',(0.,1.,0.));
#44231=DIRECTION('',(-0.852708683675886,0.,-0.52238673488493));
#44232=DIRECTION('',(0.,1.,0.));
#44233=DIRECTION('',(-0.85270868366004,0.,-0.522386734910796));
#44234=DIRECTION('center_axis',(0.,-1.,0.));
#44235=DIRECTION('ref_axis',(-0.99973889499905,0.,0.0228504228861944));
#44236=DIRECTION('center_axis',(0.,-1.,0.));
#44237=DIRECTION('ref_axis',(1.,0.,0.));
#44238=DIRECTION('center_axis',(0.,-1.,0.));
#44239=DIRECTION('ref_axis',(-0.998419029265298,0.,-0.0562089138921914));
#44240=DIRECTION('',(0.,1.,0.));
#44241=DIRECTION('center_axis',(0.,1.,0.));
#44242=DIRECTION('ref_axis',(0.727788421795868,0.,0.685801730166876));
#44243=DIRECTION('center_axis',(0.,-1.,0.));
#44244=DIRECTION('ref_axis',(-0.928397903310364,0.,-0.371587584734636));
#44245=DIRECTION('center_axis',(0.,-1.,0.));
#44246=DIRECTION('ref_axis',(1.,0.,0.));
#44247=DIRECTION('center_axis',(0.,-1.,0.));
#44248=DIRECTION('ref_axis',(-0.985455636737957,0.,0.169932892699993));
#44249=DIRECTION('',(0.,1.,0.));
#44250=DIRECTION('center_axis',(0.,1.,0.));
#44251=DIRECTION('ref_axis',(-0.989299838612263,0.,0.145896639172227));
#44252=DIRECTION('',(0.,-1.,0.));
#44253=DIRECTION('center_axis',(0.,1.,0.));
#44254=DIRECTION('ref_axis',(1.,0.,0.));
#44255=DIRECTION('center_axis',(0.,1.,0.));
#44256=DIRECTION('ref_axis',(-0.115367964260996,0.,-0.99332282407195));
#44257=DIRECTION('',(0.,-1.,0.));
#44258=DIRECTION('center_axis',(1.93875202872386E-14,-1.,1.52293552293204E-14));
#44259=DIRECTION('ref_axis',(-0.291057680790064,-2.2204460492503E-14,-0.956705506649308));
#44260=DIRECTION('center_axis',(0.,1.,0.));
#44261=DIRECTION('ref_axis',(1.,0.,0.));
#44262=DIRECTION('center_axis',(0.,1.,0.));
#44263=DIRECTION('ref_axis',(0.291057680714125,0.,0.956705506672411));
#44264=DIRECTION('center_axis',(0.,1.,0.));
#44265=DIRECTION('ref_axis',(1.,0.,0.));
#44266=DIRECTION('',(0.,-1.,0.));
#44267=DIRECTION('center_axis',(0.,-1.,0.));
#44268=DIRECTION('ref_axis',(0.291057680796176,0.,0.956705506647449));
#44269=DIRECTION('center_axis',(-0.52238673488493,0.,0.852708683675886));
#44270=DIRECTION('ref_axis',(0.,1.,0.));
#44271=DIRECTION('',(0.852708683675886,0.,0.52238673488493));
#44272=DIRECTION('',(0.852708683677683,0.,0.522386734881996));
#44273=DIRECTION('center_axis',(0.,-1.,0.));
#44274=DIRECTION('ref_axis',(0.98929983861229,0.,-0.145896639172043));
#44275=DIRECTION('center_axis',(0.,1.,0.));
#44276=DIRECTION('ref_axis',(1.,0.,0.));
#44277=DIRECTION('center_axis',(0.,-1.,0.));
#44278=DIRECTION('ref_axis',(0.52238673496676,0.,0.852708683625755));
#44279=DIRECTION('',(0.,-1.,0.));
#44280=DIRECTION('center_axis',(0.,-1.,0.));
#44281=DIRECTION('ref_axis',(0.,0.,-1.));
#44282=DIRECTION('',(-0.852708683675886,0.,0.52238673488493));
#44283=DIRECTION('center_axis',(0.52238673488493,0.,0.852708683675886));
#44284=DIRECTION('ref_axis',(0.,-1.,0.));
#44285=DIRECTION('',(-0.852708683678698,0.,0.52238673488034));
#44286=DIRECTION('center_axis',(-1.,0.,0.));
#44287=DIRECTION('ref_axis',(0.,0.,1.));
#44288=DIRECTION('',(0.,0.,1.));
#44289=DIRECTION('',(0.,0.,-1.));
#44290=DIRECTION('center_axis',(0.,0.,-1.));
#44291=DIRECTION('ref_axis',(0.,1.,0.));
#44292=DIRECTION('',(0.,0.,1.));
#44293=DIRECTION('center_axis',(0.,-1.,0.));
#44294=DIRECTION('ref_axis',(0.,0.,-1.));
#44295=DIRECTION('',(0.,0.,1.));
#44296=DIRECTION('center_axis',(0.,0.,-1.));
#44297=DIRECTION('ref_axis',(-1.,0.,0.));
#44298=DIRECTION('',(0.,0.,1.));
#44299=DIRECTION('center_axis',(-1.,0.,0.));
#44300=DIRECTION('ref_axis',(0.,0.,1.));
#44301=DIRECTION('',(0.,0.,-1.));
#44302=DIRECTION('center_axis',(-1.,0.,0.));
#44303=DIRECTION('ref_axis',(0.,0.,1.));
#44304=DIRECTION('',(0.,0.,1.));
#44305=DIRECTION('',(0.,0.,-1.));
#44306=DIRECTION('center_axis',(0.,0.,-1.));
#44307=DIRECTION('ref_axis',(0.,1.,0.));
#44308=DIRECTION('',(0.,0.,1.));
#44309=DIRECTION('center_axis',(0.,-1.,0.));
#44310=DIRECTION('ref_axis',(0.,0.,-1.));
#44311=DIRECTION('',(0.,0.,1.));
#44312=DIRECTION('center_axis',(0.,0.,-1.));
#44313=DIRECTION('ref_axis',(-1.,0.,0.));
#44314=DIRECTION('',(0.,0.,1.));
#44315=DIRECTION('center_axis',(-1.,0.,0.));
#44316=DIRECTION('ref_axis',(0.,0.,1.));
#44317=DIRECTION('',(0.,0.,-1.));
#44318=DIRECTION('center_axis',(0.,0.,-1.));
#44319=DIRECTION('ref_axis',(1.,0.,0.));
#44320=DIRECTION('',(0.,0.,-1.));
#44321=DIRECTION('center_axis',(0.,0.,-1.));
#44322=DIRECTION('ref_axis',(1.,0.,0.));
#44323=DIRECTION('',(0.,0.,-1.));
#44324=DIRECTION('center_axis',(0.,1.,0.));
#44325=DIRECTION('ref_axis',(1.,0.,0.));
#44326=DIRECTION('center_axis',(0.,0.,-1.));
#44327=DIRECTION('ref_axis',(0.,-1.,0.));
#44328=DIRECTION('',(0.,0.,-1.));
#44329=DIRECTION('center_axis',(0.,0.,-1.));
#44330=DIRECTION('ref_axis',(0.,-1.,0.));
#44331=DIRECTION('',(0.,0.,-1.));
#44332=DIRECTION('center_axis',(0.,1.,0.));
#44333=DIRECTION('ref_axis',(1.,0.,0.));
#44334=DIRECTION('center_axis',(0.,1.,0.));
#44335=DIRECTION('ref_axis',(0.479425538604203,0.,0.877582561890373));
#44336=DIRECTION('center_axis',(2.12964451632837E-16,1.,-1.16343010175233E-16));
#44337=DIRECTION('ref_axis',(-0.479425538604191,0.,-0.877582561890379));
#44338=DIRECTION('',(0.,1.,0.));
#44339=DIRECTION('center_axis',(0.,1.,0.));
#44340=DIRECTION('ref_axis',(1.,0.,0.));
#44341=DIRECTION('center_axis',(0.,1.,0.));
#44342=DIRECTION('ref_axis',(1.,0.,0.));
#44343=DIRECTION('center_axis',(0.,1.,0.));
#44344=DIRECTION('ref_axis',(1.,0.,0.));
#44345=DIRECTION('center_axis',(0.,1.,0.));
#44346=DIRECTION('ref_axis',(1.,0.,0.));
#44347=DIRECTION('center_axis',(0.,1.,0.));
#44348=DIRECTION('ref_axis',(1.,0.,0.));
#44349=DIRECTION('center_axis',(0.,1.,0.));
#44350=DIRECTION('ref_axis',(1.,0.,0.));
#44351=DIRECTION('center_axis',(0.,1.,0.));
#44352=DIRECTION('ref_axis',(1.,0.,0.));
#44353=DIRECTION('center_axis',(0.,1.,0.));
#44354=DIRECTION('ref_axis',(0.,0.,1.));
#44355=DIRECTION('',(1.,0.,-3.55668670831951E-15));
#44356=DIRECTION('center_axis',(0.,1.,0.));
#44357=DIRECTION('ref_axis',(0.,0.,1.));
#44358=DIRECTION('',(0.500000000000001,0.,0.866025403784438));
#44359=DIRECTION('center_axis',(0.,1.,0.));
#44360=DIRECTION('ref_axis',(0.,0.,1.));
#44361=DIRECTION('',(-0.499999999999995,0.,0.866025403784442));
#44362=DIRECTION('center_axis',(0.,1.,0.));
#44363=DIRECTION('ref_axis',(0.,0.,1.));
#44364=DIRECTION('',(-1.,0.,1.05277926566258E-14));
#44365=DIRECTION('center_axis',(0.,1.,0.));
#44366=DIRECTION('ref_axis',(0.,0.,1.));
#44367=DIRECTION('',(-0.500000000000007,0.,-0.866025403784435));
#44368=DIRECTION('center_axis',(0.,1.,0.));
#44369=DIRECTION('ref_axis',(0.,0.,1.));
#44370=DIRECTION('',(0.499999999999995,0.,-0.866025403784442));
#44371=DIRECTION('center_axis',(-3.55668670831951E-15,0.,-1.));
#44372=DIRECTION('ref_axis',(-1.,0.,3.55668670831951E-15));
#44373=DIRECTION('',(0.,-1.,0.));
#44374=DIRECTION('',(0.,-1.,0.));
#44375=DIRECTION('center_axis',(0.,-1.,0.));
#44376=DIRECTION('ref_axis',(0.,0.,-1.));
#44377=DIRECTION('',(0.,-1.,0.));
#44378=DIRECTION('center_axis',(-0.866025403784442,0.,-0.499999999999995));
#44379=DIRECTION('ref_axis',(-0.499999999999995,0.,0.866025403784442));
#44380=DIRECTION('',(0.,-1.,0.));
#44381=DIRECTION('center_axis',(0.,-1.,0.));
#44382=DIRECTION('ref_axis',(0.,0.,-1.));
#44383=DIRECTION('',(0.,-1.,0.));
#44384=DIRECTION('center_axis',(0.,1.,0.));
#44385=DIRECTION('ref_axis',(0.,0.,1.));
#44386=DIRECTION('center_axis',(-0.866025403784435,0.,0.500000000000007));
#44387=DIRECTION('ref_axis',(0.500000000000007,0.,0.866025403784435));
#44388=DIRECTION('',(0.,-1.,0.));
#44389=DIRECTION('center_axis',(0.,-1.,0.));
#44390=DIRECTION('ref_axis',(0.,0.,-1.));
#44391=DIRECTION('',(0.,-1.,0.));
#44392=DIRECTION('center_axis',(0.,1.,0.));
#44393=DIRECTION('ref_axis',(0.,0.,1.));
#44394=DIRECTION('center_axis',(1.05277926566258E-14,0.,1.));
#44395=DIRECTION('ref_axis',(1.,0.,-1.05277926566258E-14));
#44396=DIRECTION('',(0.,-1.,0.));
#44397=DIRECTION('center_axis',(0.,-1.,0.));
#44398=DIRECTION('ref_axis',(0.,0.,-1.));
#44399=DIRECTION('',(0.,-1.,0.));
#44400=DIRECTION('center_axis',(0.,1.,0.));
#44401=DIRECTION('ref_axis',(0.,0.,1.));
#44402=DIRECTION('center_axis',(0.866025403784442,0.,0.499999999999995));
#44403=DIRECTION('ref_axis',(0.499999999999995,0.,-0.866025403784442));
#44404=DIRECTION('',(0.,-1.,0.));
#44405=DIRECTION('center_axis',(0.,-1.,0.));
#44406=DIRECTION('ref_axis',(0.,0.,-1.));
#44407=DIRECTION('',(0.,-1.,0.));
#44408=DIRECTION('center_axis',(0.,1.,0.));
#44409=DIRECTION('ref_axis',(0.,0.,1.));
#44410=DIRECTION('center_axis',(0.866025403784438,0.,-0.500000000000001));
#44411=DIRECTION('ref_axis',(-0.500000000000001,0.,-0.866025403784438));
#44412=DIRECTION('',(0.,-1.,0.));
#44413=DIRECTION('center_axis',(0.,-1.,0.));
#44414=DIRECTION('ref_axis',(0.,0.,-1.));
#44415=DIRECTION('axis',(0.,0.,1.));
#44416=DIRECTION('refdir',(1.,0.,0.));
#44417=DIRECTION('center_axis',(-1.224646799149E-16,-1.,-1.07595286226434E-28));
#44418=DIRECTION('ref_axis',(-0.67889125729581,8.31402005216767E-17,0.734238830876789));
#44419=DIRECTION('center_axis',(1.22464679915E-16,1.,1.23259516441E-32));
#44420=DIRECTION('ref_axis',(1.,-1.22464679915E-16,-1.50949372274247E-48));
#44421=DIRECTION('',(-2.85587916301E-16,-1.,0.));
#44422=DIRECTION('center_axis',(1.22464679915E-16,1.,0.));
#44423=DIRECTION('ref_axis',(1.,-1.22464679915E-16,0.));
#44424=DIRECTION('',(0.,-1.,0.));
#44425=DIRECTION('center_axis',(1.22464679914912E-16,1.,-1.26181562037188E-28));
#44426=DIRECTION('ref_axis',(0.572811155566786,-7.01491348180737E-17,0.819687367267694));
#44427=DIRECTION('',(0.,-1.,0.));
#44428=DIRECTION('center_axis',(-1.22464679915E-16,-1.,-1.23259516441E-32));
#44429=DIRECTION('ref_axis',(1.,-1.22464679915E-16,-1.50949372274247E-48));
#44430=DIRECTION('center_axis',(-1.22464679915E-16,-1.,-2.46519032882E-32));
#44431=DIRECTION('ref_axis',(1.,-1.22464679915E-16,-3.01898744548495E-48));
#44432=DIRECTION('center_axis',(-0.641370372756966,-0.046782002687993,-0.765803818986358));
#44433=DIRECTION('ref_axis',(0.766534261679224,-0.0816131667450425,-0.636996480905298));
#44434=DIRECTION('center_axis',(-1.22464679914824E-16,-1.,2.07760762711853E-28));
#44435=DIRECTION('ref_axis',(-0.646318112561793,7.91511407778746E-17,-0.763068081742751));
#44436=DIRECTION('',(0.,-1.,0.));
#44437=DIRECTION('center_axis',(1.22464679915E-16,1.,6.16297582204E-33));
#44438=DIRECTION('ref_axis',(1.,-1.22464679915E-16,-7.54746861370013E-49));
#44439=DIRECTION('center_axis',(1.22464679914844E-16,1.,-1.36792384183344E-28));
#44440=DIRECTION('ref_axis',(0.751089446707,-9.19819286783E-17,0.660200456713999));
#44441=DIRECTION('',(0.,1.,0.));
#44442=DIRECTION('center_axis',(-1.22464679915E-16,-1.,-1.23259516441E-32));
#44443=DIRECTION('ref_axis',(1.,-1.22464679915E-16,-1.50949372274247E-48));
#44444=DIRECTION('',(2.85587916301E-16,1.,0.));
#44445=DIRECTION('center_axis',(1.2246467991496E-16,1.,-1.2428667907779E-29));
#44446=DIRECTION('ref_axis',(0.953995514765253,-1.16830755356031E-16,0.299820876204076));
#44447=DIRECTION('',(0.,1.,0.));
#44448=DIRECTION('center_axis',(-1.22464679915E-16,-1.,0.));
#44449=DIRECTION('ref_axis',(1.,-1.22464679915E-16,0.));
#44450=DIRECTION('',(2.85587916301E-16,1.,0.));
#44451=DIRECTION('center_axis',(0.,1.,0.));
#44452=DIRECTION('ref_axis',(0.678891257321093,0.,-0.734238830853412));
#44453=DIRECTION('center_axis',(-0.678891257295808,8.31402005216763E-17,
0.734238830876792));
#44454=DIRECTION('ref_axis',(1.22464679914784E-16,1.,1.83887638005312E-34));
#44455=DIRECTION('',(0.,-1.,0.));
#44456=DIRECTION('',(0.734238830876791,0.,0.678891257295807));
#44457=DIRECTION('',(-0.734238830876791,0.,-0.678891257295807));
#44458=DIRECTION('center_axis',(-1.224646799149E-16,-1.,-1.07595286226434E-28));
#44459=DIRECTION('ref_axis',(-0.67889125729581,8.31402005216767E-17,0.734238830876789));
#44460=DIRECTION('center_axis',(-1.22464679915E-16,-1.,0.));
#44461=DIRECTION('ref_axis',(1.,-1.22464679915E-16,0.));
#44462=DIRECTION('',(0.,-1.,0.));
#44463=DIRECTION('center_axis',(1.22464679915E-16,1.,0.));
#44464=DIRECTION('ref_axis',(1.,-1.22464679915E-16,0.));
#44465=DIRECTION('center_axis',(1.22464679914912E-16,1.,-1.26181562037188E-28));
#44466=DIRECTION('ref_axis',(0.572811155566786,-7.01491348180737E-17,0.819687367267694));
#44467=DIRECTION('',(0.,-1.,0.));
#44468=DIRECTION('center_axis',(-1.22464679915E-16,-1.,-1.23259516441E-32));
#44469=DIRECTION('ref_axis',(1.,-1.22464679915E-16,-1.50949372274247E-48));
#44470=DIRECTION('center_axis',(1.22464679915E-16,1.,0.));
#44471=DIRECTION('ref_axis',(1.,-1.22464679915E-16,0.));
#44472=DIRECTION('center_axis',(1.224646799149E-16,1.,1.07586726537792E-28));
#44473=DIRECTION('ref_axis',(0.67889125729581,-8.31402005216767E-17,-0.734238830876789));
#44474=DIRECTION('center_axis',(-1.22464679915E-16,-1.,0.));
#44475=DIRECTION('ref_axis',(1.,-1.22464679915E-16,0.));
#44476=DIRECTION('',(0.,-1.,0.));
#44477=DIRECTION('',(0.,-1.,0.));
#44478=DIRECTION('center_axis',(1.22464679915E-16,1.,1.23259516441E-32));
#44479=DIRECTION('ref_axis',(1.,-1.22464679915E-16,-1.50949372274247E-48));
#44480=DIRECTION('center_axis',(-0.678891257295808,8.31402005216763E-17,
0.734238830876792));
#44481=DIRECTION('ref_axis',(1.22464679914784E-16,1.,1.83887638005312E-34));
#44482=DIRECTION('',(0.,1.,0.));
#44483=DIRECTION('',(-0.734238830876791,0.,-0.678891257295807));
#44484=DIRECTION('center_axis',(-0.678891258039564,-8.05580512386835E-9,
0.7342388301891));
#44485=DIRECTION('ref_axis',(1.90502136153082E-5,-0.999999999663608,1.76032200345041E-5));
#44486=DIRECTION('',(0.734238830876791,0.,0.678891257295807));
#44487=DIRECTION('center_axis',(0.734238830876792,-8.99183234042744E-17,
0.678891257295808));
#44488=DIRECTION('ref_axis',(-0.678891257295807,-3.46311205996404E-31,0.734238830876791));
#44489=DIRECTION('',(0.734238830876791,0.,0.678891257295807));
#44490=DIRECTION('center_axis',(-0.734238830876792,8.99183234042744E-17,
-0.678891257295808));
#44491=DIRECTION('ref_axis',(0.678891257295807,3.46311205996404E-31,-0.734238830876791));
#44492=DIRECTION('',(0.734238830876791,0.,0.678891257295807));
#44493=DIRECTION('center_axis',(0.,0.,1.));
#44494=DIRECTION('ref_axis',(1.,0.,0.));
#44495=DIRECTION('center_axis',(0.803996045360697,-9.84611183477626E-17,
-0.594634643326775));
#44496=DIRECTION('ref_axis',(0.594634643326775,4.97302608069436E-32,0.803996045360697));
#44497=DIRECTION('center_axis',(-7.91623497736024E-17,-1.,5.85483919904324E-17));
#44498=DIRECTION('ref_axis',(0.594634643326775,0.,0.803996045360696));
#44499=DIRECTION('center_axis',(-1.22464679915E-16,-1.,-5.47382212627E-48));
#44500=DIRECTION('ref_axis',(1.,-1.22464679915E-16,-6.703498746053E-64));
#44501=DIRECTION('center_axis',(0.763068081742753,-9.34488883837698E-17,
-0.646318112561791));
#44502=DIRECTION('ref_axis',(0.646318112561791,2.50438493602067E-31,0.763068081742753));
#44503=DIRECTION('center_axis',(1.,0.,0.));
#44504=DIRECTION('ref_axis',(0.,-1.,0.));
#44505=DIRECTION('center_axis',(0.734238830876792,-8.99183234042744E-17,
0.678891257295808));
#44506=DIRECTION('ref_axis',(0.678891257295807,3.46311205996404E-31,-0.734238830876791));
#44507=DIRECTION('center_axis',(-0.734238830876792,8.99183234042744E-17,
-0.678891257295808));
#44508=DIRECTION('ref_axis',(0.678891257295807,3.46311205996404E-31,-0.734238830876791));
#44509=DIRECTION('',(-0.734238830876791,0.,-0.678891257295807));
#44510=DIRECTION('',(-0.734238830876791,0.,-0.678891257295807));
#44511=DIRECTION('center_axis',(0.734238830876792,-8.99183234042744E-17,
0.678891257295808));
#44512=DIRECTION('ref_axis',(0.678891257295807,3.46311205996404E-31,-0.734238830876791));
#44513=DIRECTION('center_axis',(-6.60215246509141E-17,-1.,-6.10447636300053E-17));
#44514=DIRECTION('ref_axis',(-0.678891257295808,0.,0.734238830876791));
#44515=DIRECTION('center_axis',(-1.22464679915E-16,-1.,-5.47382212627E-48));
#44516=DIRECTION('ref_axis',(1.,-1.22464679915E-16,-6.703498746053E-64));
#44517=DIRECTION('center_axis',(-1.22464679915E-16,-1.,-1.23259516441E-32));
#44518=DIRECTION('ref_axis',(1.,-1.22464679915E-16,-1.50949372274247E-48));
#44519=DIRECTION('center_axis',(0.732027802944257,-8.96475505763315E-17,
-0.68127475787424));
#44520=DIRECTION('ref_axis',(0.68127475787424,-1.91888914560603E-31,0.732027802944257));
#44521=DIRECTION('center_axis',(-6.56244994878123E-17,-1.,6.10746133129891E-17));
#44522=DIRECTION('ref_axis',(0.681274757874239,0.,0.732027802944258));
#44523=DIRECTION('center_axis',(-1.22464679915E-16,-1.,-5.47382212627E-48));
#44524=DIRECTION('ref_axis',(1.,-1.22464679915E-16,5.9677926224237E-64));
#44525=DIRECTION('center_axis',(-1.22464679915E-16,-1.,-5.47382212627E-48));
#44526=DIRECTION('ref_axis',(1.,-1.22464679915E-16,6.22660996643423E-64));
#44527=DIRECTION('center_axis',(0.660200456714,-8.0851237611E-17,-0.751089446706999));
#44528=DIRECTION('ref_axis',(0.751089446706999,6.24086217807948E-32,0.660200456714));
#44529=DIRECTION('center_axis',(-5.33780239968174E-17,-1.,6.0726511322985E-17));
#44530=DIRECTION('ref_axis',(0.751089446706998,0.,0.660200456714001));
#44531=DIRECTION('center_axis',(-1.22464679915E-16,-1.,-5.47382212627E-48));
#44532=DIRECTION('ref_axis',(1.,-1.22464679915E-16,-6.703498746053E-64));
#44533=DIRECTION('center_axis',(0.315563048033822,-3.86453276703782E-17,
-0.948904612021463));
#44534=DIRECTION('ref_axis',(0.948904612021463,7.52823903108453E-32,0.315563048033822));
#44535=DIRECTION('center_axis',(-1.21950373919573E-17,-1.,3.66707296595837E-17));
#44536=DIRECTION('ref_axis',(0.948904612021463,0.,0.315563048033822));
#44537=DIRECTION('center_axis',(-1.22464679915E-16,-1.,-5.47382212627E-48));
#44538=DIRECTION('ref_axis',(1.,-1.22464679915E-16,5.9677926224237E-64));
#44539=DIRECTION('center_axis',(-1.22464679915E-16,-1.,-5.47382212627E-48));
#44540=DIRECTION('ref_axis',(1.,-1.22464679915E-16,6.22660996643423E-64));
#44541=DIRECTION('center_axis',(0.299820876204079,-3.67174676361097E-17,
-0.953995514765252));
#44542=DIRECTION('ref_axis',(0.953995514765252,-6.3869078326472E-32,0.299820876204079));
#44543=DIRECTION('center_axis',(-1.10086633186706E-17,-1.,3.5028299438442E-17));
#44544=DIRECTION('ref_axis',(0.953995514765252,0.,0.299820876204079));
#44545=DIRECTION('center_axis',(-1.22464679915E-16,-1.,-5.47382212627E-48));
#44546=DIRECTION('ref_axis',(1.,-1.22464679915E-16,-6.703498746053E-64));
#44547=DIRECTION('center_axis',(-0.734238830876792,8.99183234042744E-17,
-0.678891257295808));
#44548=DIRECTION('ref_axis',(0.678891257295807,3.46311205996404E-31,-0.734238830876791));
#44549=DIRECTION('center_axis',(0.734238830876792,-8.99183234042744E-17,
0.678891257295808));
#44550=DIRECTION('ref_axis',(-0.678891257295807,-3.46311205996404E-31,0.734238830876791));
#44551=DIRECTION('',(0.734238830876791,0.,0.678891257295807));
#44552=DIRECTION('center_axis',(-0.734238830876792,8.99183234042744E-17,
-0.678891257295808));
#44553=DIRECTION('ref_axis',(0.678891257295807,3.46311205996404E-31,-0.734238830876791));
#44554=DIRECTION('center_axis',(0.,0.,1.));
#44555=DIRECTION('ref_axis',(1.,0.,0.));
#44556=DIRECTION('center_axis',(0.613815420645987,-7.51707090161983E-17,
-0.789449573675983));
#44557=DIRECTION('ref_axis',(0.789449573675983,7.34020703099417E-32,0.613815420645987));
#44558=DIRECTION('center_axis',(-4.61409403750984E-17,-1.,5.93434841858408E-17));
#44559=DIRECTION('ref_axis',(0.789449573675983,0.,0.613815420645986));
#44560=DIRECTION('center_axis',(-1.22464679915E-16,-1.,-5.47382212627E-48));
#44561=DIRECTION('ref_axis',(1.,-1.22464679915E-16,-6.703498746053E-64));
#44562=DIRECTION('center_axis',(0.560738119471071,-6.86706143170087E-17,
-0.827993213361104));
#44563=DIRECTION('ref_axis',(0.827993213361104,-2.38131063616686E-32,0.560738119471071));
#44564=DIRECTION('center_axis',(1.,0.,0.));
#44565=DIRECTION('ref_axis',(0.,-1.,0.));
#44566=DIRECTION('center_axis',(0.734238830876792,-8.99183234042744E-17,
0.678891257295808));
#44567=DIRECTION('ref_axis',(0.678891257295807,3.46311205996404E-31,-0.734238830876791));
#44568=DIRECTION('center_axis',(0.734238830876792,-8.99183234044499E-17,
0.678891257295808));
#44569=DIRECTION('ref_axis',(-6.60215246508846E-17,-1.,-6.1044763629978E-17));
#44570=DIRECTION('',(-0.734238830876791,0.,-0.678891257295807));
#44571=DIRECTION('center_axis',(-1.22464679915E-16,-1.,-5.47382212627E-48));
#44572=DIRECTION('ref_axis',(-1.,1.22464679915E-16,0.));
#44573=DIRECTION('center_axis',(1.22464679915E-16,1.,1.23259516441E-32));
#44574=DIRECTION('ref_axis',(1.,-1.22464679915E-16,-1.50949372274247E-48));
#44575=DIRECTION('center_axis',(1.22464679915E-16,1.,0.));
#44576=DIRECTION('ref_axis',(1.,-1.22464679915E-16,0.));
#44577=DIRECTION('center_axis',(1.,-1.22464679915E-16,6.12323399574E-17));
#44578=DIRECTION('ref_axis',(-1.22464679915E-16,-1.,-6.67366607695787E-50));
#44579=DIRECTION('',(-1.26882631386E-16,-1.,0.));
#44580=DIRECTION('',(1.75377892382E-16,0.,-1.));
#44581=DIRECTION('',(-1.26882631386E-16,-1.,0.));
#44582=DIRECTION('',(2.21800239814E-16,0.,-1.));
#44583=DIRECTION('',(-1.34875042533E-16,-1.,0.));
#44584=DIRECTION('',(2.5585870064E-16,0.,-1.));
#44585=DIRECTION('center_axis',(-1.22464679915E-16,-1.,-7.60253073092891E-48));
#44586=DIRECTION('ref_axis',(1.,-1.22464679915E-16,-9.3104149250716E-64));
#44587=DIRECTION('center_axis',(1.22464679915E-16,1.,0.));
#44588=DIRECTION('ref_axis',(1.,-1.22464679915E-16,0.));
#44589=DIRECTION('',(-1.42793958151E-16,-1.,0.));
#44590=DIRECTION('center_axis',(1.22464679915E-16,1.,6.16297582204E-33));
#44591=DIRECTION('ref_axis',(1.,-1.22464679915E-16,-7.54746861370013E-49));
#44592=DIRECTION('center_axis',(1.22464679914955E-16,1.,8.72911003161552E-29));
#44593=DIRECTION('ref_axis',(0.457271150163836,-5.59995650390798E-17,-0.889327327381681));
#44594=DIRECTION('',(-1.26882631386E-16,-1.,0.));
#44595=DIRECTION('center_axis',(-1.22464679915E-16,-1.,0.));
#44596=DIRECTION('ref_axis',(1.,-1.22464679915E-16,0.));
#44597=DIRECTION('center_axis',(-1.22464679915E-16,-1.,6.16297582204E-33));
#44598=DIRECTION('ref_axis',(1.,-1.22464679915E-16,7.54746861370012E-49));
#44599=DIRECTION('center_axis',(1.22464679915E-16,1.,0.));
#44600=DIRECTION('ref_axis',(-1.,1.22464679915E-16,-2.89120579329468E-15));
#44601=DIRECTION('center_axis',(1.22464679915E-16,1.,0.));
#44602=DIRECTION('ref_axis',(1.,-1.22464679915E-16,0.));
#44603=DIRECTION('',(-2.0185873175E-16,-1.,0.));
#44604=DIRECTION('center_axis',(1.22464679915E-16,1.,6.16297582204E-33));
#44605=DIRECTION('ref_axis',(1.,-1.22464679915E-16,-7.54746861370013E-49));
#44606=DIRECTION('center_axis',(1.,-1.22464679915E-16,6.12323399574E-17));
#44607=DIRECTION('ref_axis',(-1.22464679915E-16,-1.,-6.67366607695787E-50));
#44608=DIRECTION('',(-2.58629566281E-16,0.,1.));
#44609=DIRECTION('',(1.26882631386E-16,1.,0.));
#44610=DIRECTION('',(-1.75377892382E-16,0.,1.));
#44611=DIRECTION('center_axis',(-1.22464679914969E-16,-1.,-8.28235472972929E-29));
#44612=DIRECTION('ref_axis',(0.345424032932988,-4.23022436279984E-17,-0.938446715307966));
#44613=DIRECTION('',(1.42793958151E-16,1.,0.));
#44614=DIRECTION('center_axis',(-1.22464679915E-16,-1.,0.));
#44615=DIRECTION('ref_axis',(1.,-1.22464679915E-16,0.));
#44616=DIRECTION('center_axis',(1.22464679915E-16,1.,6.16297582203999E-33));
#44617=DIRECTION('ref_axis',(1.,-1.22464679915E-16,-7.54746861370011E-49));
#44618=DIRECTION('center_axis',(0.,-1.,0.));
#44619=DIRECTION('ref_axis',(1.,0.,3.70074341541721E-15));
#44620=DIRECTION('center_axis',(1.22464679915E-16,1.,-6.16297582204E-33));
#44621=DIRECTION('ref_axis',(1.,-1.22464679915E-16,7.54746861370013E-49));
#44622=DIRECTION('',(0.,-1.,0.));
#44623=DIRECTION('center_axis',(2.17357452795E-16,-2.66186108837E-32,-1.));
#44624=DIRECTION('ref_axis',(1.,5.7857534586223E-48,2.17357452795E-16));
#44625=DIRECTION('',(2.0973706922E-16,0.,-1.));
#44626=DIRECTION('center_axis',(-4.62592926927E-17,5.6651294727E-33,1.));
#44627=DIRECTION('ref_axis',(1.,2.62064882419671E-49,4.62592926927E-17));
#44628=DIRECTION('center_axis',(-2.77555756156E-16,3.39907768362E-32,1.));
#44629=DIRECTION('ref_axis',(1.,9.43433576710134E-48,2.77555756156E-16));
#44630=DIRECTION('center_axis',(1.,0.,0.));
#44631=DIRECTION('ref_axis',(0.,-1.,0.));
#44632=DIRECTION('center_axis',(-0.904759192693671,1.1080104493296E-16,
-0.425923471102845));
#44633=DIRECTION('ref_axis',(0.425923471102845,3.65487816993661E-32,-0.904759192693671));
#44634=DIRECTION('center_axis',(-1.00248263963544E-16,-1.,-4.71927656598494E-17));
#44635=DIRECTION('ref_axis',(0.425923471102846,0.,-0.904759192693671));
#44636=DIRECTION('center_axis',(-1.22464679915E-16,-1.,-5.47382212627E-48));
#44637=DIRECTION('ref_axis',(1.,-1.22464679915E-16,-6.703498746053E-64));
#44638=DIRECTION('center_axis',(-0.916786704663777,1.12273990336973E-16,
-0.399377187820903));
#44639=DIRECTION('ref_axis',(0.399377187820903,3.93858763528754E-32,-0.916786704663777));
#44640=DIRECTION('center_axis',(0.,0.,1.));
#44641=DIRECTION('ref_axis',(1.,0.,0.));
#44642=DIRECTION('center_axis',(2.17357452795E-16,-2.66186108837E-32,-1.));
#44643=DIRECTION('ref_axis',(1.,5.7857534586223E-48,2.17357452795E-16));
#44644=DIRECTION('center_axis',(2.17357452795E-16,-2.66186108836821E-32,
-1.));
#44645=DIRECTION('ref_axis',(-5.78575345861839E-48,-1.,2.66186108836821E-32));
#44646=DIRECTION('',(0.,0.,1.));
#44647=DIRECTION('center_axis',(2.17357452795E-16,-2.66186108837E-32,-1.));
#44648=DIRECTION('ref_axis',(1.,5.7857534586223E-48,2.17357452795E-16));
#44649=DIRECTION('center_axis',(-1.07341775839004E-45,-1.,3.62568286252829E-31));
#44650=DIRECTION('ref_axis',(1.,0.,3.94745964311167E-15));
#44651=DIRECTION('center_axis',(-1.22464679915E-16,-1.,-5.47382212627E-48));
#44652=DIRECTION('ref_axis',(1.,-1.22464679915E-16,-6.703498746053E-64));
#44653=DIRECTION('center_axis',(-0.938446715307966,1.14926576606996E-16,
-0.345424032932987));
#44654=DIRECTION('ref_axis',(0.345424032932987,5.96953449650393E-32,-0.938446715307966));
#44655=DIRECTION('center_axis',(-1.07852468318872E-16,-1.,-3.96984015829353E-17));
#44656=DIRECTION('ref_axis',(0.345424032932988,0.,-0.938446715307966));
#44657=DIRECTION('center_axis',(-1.22464679915E-16,-1.,-5.47382212627E-48));
#44658=DIRECTION('ref_axis',(1.,-1.22464679915E-16,5.9677926224237E-64));
#44659=DIRECTION('center_axis',(-1.22464679915E-16,-1.,-5.47382212627E-48));
#44660=DIRECTION('ref_axis',(1.,-1.22464679915E-16,6.22660996643423E-64));
#44661=DIRECTION('center_axis',(0.,0.,1.));
#44662=DIRECTION('ref_axis',(1.,0.,0.));
#44663=DIRECTION('center_axis',(0.927477365469186,-1.13583218690023E-16,
0.373879307454075));
#44664=DIRECTION('ref_axis',(0.373879307454075,-5.54912062383212E-32,-0.927477365469186));
#44665=DIRECTION('center_axis',(-1.0534586443266E-16,-1.,-4.2466415142443E-17));
#44666=DIRECTION('ref_axis',(0.373879307454075,0.,-0.927477365469186));
#44667=DIRECTION('center_axis',(1.22464679915E-16,1.,5.47382212627E-48));
#44668=DIRECTION('ref_axis',(1.,-1.22464679915E-16,5.02845536814161E-64));
#44669=DIRECTION('center_axis',(1.22464679915E-16,1.,5.47382212627E-48));
#44670=DIRECTION('ref_axis',(1.,-1.22464679915E-16,5.24998673990483E-64));
#44671=DIRECTION('center_axis',(0.687199008140201,-8.41576065696246E-17,
-0.726469216974212));
#44672=DIRECTION('ref_axis',(-0.726469216974212,-1.50838013754883E-32,-0.687199008140201));
#44673=DIRECTION('',(-0.687199008140201,0.,0.726469216974212));
#44674=DIRECTION('',(-0.687199008140201,0.,0.726469216974212));
#44675=DIRECTION('center_axis',(1.68490994230906E-17,1.,-4.21844451941189E-17));
#44676=DIRECTION('ref_axis',(-0.928663912412966,0.,-0.370922279974987));
#44677=DIRECTION('center_axis',(-1.22464679915E-16,-1.,-5.47382212627E-48));
#44678=DIRECTION('ref_axis',(1.,-1.22464679915E-16,-6.703498746053E-64));
#44679=DIRECTION('center_axis',(-1.22464679915E-16,-1.,-5.47382212627E-48));
#44680=DIRECTION('ref_axis',(1.,-1.22464679915E-16,-6.703498746053E-64));
#44681=DIRECTION('center_axis',(-0.656401557315033,6.93091019571431E-12,
-0.754411688373397));
#44682=DIRECTION('ref_axis',(-9.95129904405703E-12,1.,1.78468351208498E-11));
#44683=DIRECTION('center_axis',(1.,-1.22464679915E-16,6.12323399574E-17));
#44684=DIRECTION('ref_axis',(1.22464679915E-16,1.,7.49879891332945E-33));
#44685=DIRECTION('',(1.,0.,2.21592204945E-16));
#44686=DIRECTION('',(1.,0.,1.4772813663E-16));
#44687=DIRECTION('center_axis',(-1.,0.,0.));
#44688=DIRECTION('ref_axis',(0.,1.,-3.70074341541716E-15));
#44689=DIRECTION('center_axis',(2.41898181523141E-16,1.,1.1741867647411E-17));
#44690=DIRECTION('ref_axis',(-0.99520202856178,2.41886400693281E-16,-0.0978413120645785));
#44691=DIRECTION('center_axis',(1.22464679915E-16,1.,5.47382212627E-48));
#44692=DIRECTION('ref_axis',(1.,-1.22464679915E-16,6.22660996643423E-64));
#44693=DIRECTION('center_axis',(1.22464679915E-16,1.,5.47382212627E-48));
#44694=DIRECTION('ref_axis',(1.,-1.22464679915E-16,6.49622071350503E-64));
#44695=DIRECTION('center_axis',(-0.668126653627122,3.01884491205213E-12,
-0.744047562130959));
#44696=DIRECTION('ref_axis',(0.744047562130959,1.48029736616688E-14,-0.668126653627122));
#44697=DIRECTION('center_axis',(0.,1.,0.));
#44698=DIRECTION('ref_axis',(0.0129687405446048,0.,-0.999915902348136));
#44699=DIRECTION('center_axis',(1.22464679915E-16,1.,0.));
#44700=DIRECTION('ref_axis',(1.,-1.22464679915E-16,0.));
#44701=DIRECTION('center_axis',(-0.726469216974212,8.89668201247259E-17,
-0.687199008140201));
#44702=DIRECTION('ref_axis',(-0.687199008140201,2.45619021304035E-33,0.726469216974212));
#44703=DIRECTION('',(-0.687199008140201,0.,0.726469216974212));
#44704=DIRECTION('',(0.,-1.,0.));
#44705=DIRECTION('',(0.,1.,0.));
#44706=DIRECTION('center_axis',(0.,0.,1.));
#44707=DIRECTION('ref_axis',(1.,0.,0.));
#44708=DIRECTION('center_axis',(-1.22464679915E-16,-1.,0.));
#44709=DIRECTION('ref_axis',(1.,-1.22464679915E-16,0.));
#44710=DIRECTION('center_axis',(1.22464679914998E-16,1.,-1.73663083545565E-29));
#44711=DIRECTION('ref_axis',(0.095298509688002,-1.16707014853003E-17,0.99544874004202));
#44712=DIRECTION('center_axis',(-1.22464679915E-16,-1.,0.));
#44713=DIRECTION('ref_axis',(1.,-1.22464679915E-16,0.));
#44714=DIRECTION('',(0.,1.,0.));
#44715=DIRECTION('',(0.,1.,0.));
#44716=DIRECTION('center_axis',(0.,0.,1.));
#44717=DIRECTION('ref_axis',(1.,0.,0.));
#44718=DIRECTION('center_axis',(-1.22464679915E-16,-1.,3.08148791102E-33));
#44719=DIRECTION('ref_axis',(1.,-1.22464679915E-16,3.77373430685006E-49));
#44720=DIRECTION('center_axis',(-2.17357452795E-16,2.66186108837E-32,1.));
#44721=DIRECTION('ref_axis',(1.,2.56447231488414E-65,2.17357452795E-16));
#44722=DIRECTION('',(0.,1.,0.));
#44723=DIRECTION('',(0.,-1.,0.));
#44724=DIRECTION('',(1.,0.,4.75520106567E-17));
#44725=DIRECTION('center_axis',(0.,1.,0.));
#44726=DIRECTION('ref_axis',(0.79266275948672,0.,0.609660356036784));
#44727=DIRECTION('center_axis',(1.22464679915E-16,1.,0.));
#44728=DIRECTION('ref_axis',(1.,-1.22464679915E-16,0.));
#44729=DIRECTION('center_axis',(1.22464679914586E-16,1.,-1.3947821589454E-28));
#44730=DIRECTION('ref_axis',(0.947590338356885,-1.16046347476986E-16,0.319487950715961));
#44731=DIRECTION('',(0.,-1.,0.));
#44732=DIRECTION('',(0.,-1.,0.));
#44733=DIRECTION('center_axis',(1.22464679915E-16,1.,0.));
#44734=DIRECTION('ref_axis',(1.,-1.22464679915E-16,0.));
#44735=DIRECTION('center_axis',(1.22464679914811E-16,1.,1.69670148256195E-28));
#44736=DIRECTION('ref_axis',(0.744047562132924,-9.11195465378906E-17,-0.668126653624934));
#44737=DIRECTION('center_axis',(1.22464679915E-16,1.,0.));
#44738=DIRECTION('ref_axis',(1.,-1.22464679915E-16,0.));
#44739=DIRECTION('center_axis',(0.687199008140201,-8.41576065696246E-17,
-0.726469216974212));
#44740=DIRECTION('ref_axis',(0.726469216974212,1.50838013754883E-32,0.687199008140201));
#44741=DIRECTION('center_axis',(0.687199008140201,-8.41576065696246E-17,
-0.726469216974212));
#44742=DIRECTION('ref_axis',(0.726469216974212,1.50838013754883E-32,0.687199008140201));
#44743=DIRECTION('',(-0.687199008140201,0.,0.726469216974212));
#44744=DIRECTION('center_axis',(0.687199008140201,-8.41576065696246E-17,
-0.726469216974212));
#44745=DIRECTION('ref_axis',(0.726469216974212,1.50838013754883E-32,0.687199008140201));
#44746=DIRECTION('center_axis',(1.22464679914912E-16,1.,-8.35682402091226E-29));
#44747=DIRECTION('ref_axis',(-0.726469216974212,8.89668201247259E-17,-0.687199008140201));
#44748=DIRECTION('center_axis',(1.22464679915E-16,1.,1.23259516441E-32));
#44749=DIRECTION('ref_axis',(1.,-1.22464679915E-16,-1.50949372274247E-48));
#44750=DIRECTION('center_axis',(-2.81810938552877E-18,-1.,-1.83623833789471E-17));
#44751=DIRECTION('ref_axis',(0.988427230781696,0.,-0.151695779272953));
#44752=DIRECTION('center_axis',(-0.151695779272953,1.85773750529943E-17,
-0.988427230781696));
#44753=DIRECTION('ref_axis',(0.988427230781695,3.4608594993322E-33,-0.151695779272953));
#44754=DIRECTION('center_axis',(-1.22464679915E-16,-1.,-5.47382212627E-48));
#44755=DIRECTION('ref_axis',(1.,-1.22464679915E-16,-6.703498746053E-64));
#44756=DIRECTION('center_axis',(-0.656401557320037,8.03860066128046E-17,
-0.754411688369043));
#44757=DIRECTION('ref_axis',(0.754411688369043,3.51059188021851E-32,-0.656401557320037));
#44758=DIRECTION('center_axis',(-1.22464679915E-16,-1.,3.04712758348345E-33));
#44759=DIRECTION('ref_axis',(3.73165504171468E-49,3.04712758348345E-33,
1.));
#44760=DIRECTION('center_axis',(1.22464679915E-16,1.,0.));
#44761=DIRECTION('ref_axis',(1.,-1.22464679915E-16,0.));
#44762=DIRECTION('center_axis',(1.,-1.22464679915E-16,6.12323399574E-17));
#44763=DIRECTION('ref_axis',(-1.22464679915E-16,-1.,-7.49879891332945E-33));
#44764=DIRECTION('center_axis',(-1.,1.22464679915E-16,5.91506623067E-14));
#44765=DIRECTION('ref_axis',(1.22464679915E-16,1.,-7.24386692615027E-30));
#44766=DIRECTION('',(1.,0.,1.4772813663E-16));
#44767=DIRECTION('center_axis',(-1.,1.22464679915E-16,6.05071548421E-15));
#44768=DIRECTION('ref_axis',(1.22464679915E-16,1.,-7.40998935030512E-31));
#44769=DIRECTION('center_axis',(-1.22464679914936E-16,-1.,-1.70680191515918E-29));
#44770=DIRECTION('ref_axis',(0.966510120331627,-1.18363352520954E-16,-0.2566285005539));
#44771=DIRECTION('center_axis',(1.22464679915E-16,1.,0.));
#44772=DIRECTION('ref_axis',(1.,-1.22464679915E-16,0.));
#44773=DIRECTION('center_axis',(-8.06530182705333E-18,-1.,-3.03754096780024E-17));
#44774=DIRECTION('ref_axis',(0.966510120331627,0.,-0.256628500553901));
#44775=DIRECTION('center_axis',(0.668126653624933,-8.18219167786918E-17,
0.744047562132925));
#44776=DIRECTION('ref_axis',(0.744047562132925,-1.50412683502806E-31,-0.668126653624933));
#44777=DIRECTION('center_axis',(1.22464679915E-16,1.,5.47382212627E-48));
#44778=DIRECTION('ref_axis',(1.,-1.22464679915E-16,5.9677926224237E-64));
#44779=DIRECTION('center_axis',(0.256628500553901,-3.14279271772879E-17,
0.966510120331627));
#44780=DIRECTION('ref_axis',(0.966510120331627,1.90417037848503E-32,-0.256628500553901));
#44781=DIRECTION('center_axis',(-5.46674034506358E-17,-1.,-6.0879397708352E-17));
#44782=DIRECTION('ref_axis',(0.744047562132925,0.,-0.668126653624934));
#44783=DIRECTION('center_axis',(1.22464679915E-16,1.,5.47382212627E-48));
#44784=DIRECTION('ref_axis',(1.,-1.22464679915E-16,-6.703498746053E-64));
#44785=DIRECTION('center_axis',(0.,1.,0.));
#44786=DIRECTION('ref_axis',(0.997344825668515,0.,0.0728237510173635));
#44787=DIRECTION('center_axis',(-1.22464679915E-16,-1.,0.));
#44788=DIRECTION('ref_axis',(1.,-1.22464679915E-16,0.));
#44789=DIRECTION('center_axis',(-0.825067330468845,1.01041606533981E-16,
0.565034423900893));
#44790=DIRECTION('ref_axis',(0.565034423900893,7.24547600115018E-32,0.825067330468845));
#44791=DIRECTION('center_axis',(0.734238830876792,-8.99183234042744E-17,
0.678891257295808));
#44792=DIRECTION('ref_axis',(0.678891257295808,1.51038693775819E-31,-0.734238830876792));
#44793=DIRECTION('center_axis',(-5.78330237622164E-17,-1.,6.11379105471829E-17));
#44794=DIRECTION('ref_axis',(-0.726469216974212,0.,-0.687199008140201));
#44795=DIRECTION('center_axis',(1.22464679915E-16,1.,5.47382212627E-48));
#44796=DIRECTION('ref_axis',(1.,-1.22464679915E-16,-6.703498746053E-64));
#44797=DIRECTION('center_axis',(-2.81810938552877E-18,-1.,-1.83623833789471E-17));
#44798=DIRECTION('ref_axis',(-0.988427230781696,0.,0.151695779272954));
#44799=DIRECTION('center_axis',(1.22464679915E-16,1.,5.47382212627E-48));
#44800=DIRECTION('ref_axis',(1.,-1.22464679915E-16,-6.703498746053E-64));
#44801=DIRECTION('center_axis',(-1.22464679915E-16,-1.,6.16366086630911E-30));
#44802=DIRECTION('ref_axis',(4.93432455388959E-14,0.,1.));
#44803=DIRECTION('center_axis',(1.22464679915E-16,1.,5.47382212627E-48));
#44804=DIRECTION('ref_axis',(1.,-1.22464679915E-16,-6.703498746053E-64));
#44805=DIRECTION('center_axis',(-1.13563209349214E-16,-1.,-3.17943322838876E-17));
#44806=DIRECTION('ref_axis',(0.269603455472075,0.,-0.962971430935268));
#44807=DIRECTION('center_axis',(1.22464679915E-16,1.,5.47382212627E-48));
#44808=DIRECTION('ref_axis',(1.,-1.22464679915E-16,-6.703498746053E-64));
#44809=DIRECTION('center_axis',(-0.962971430935267,1.17929988057033E-16,
-0.269603455472075));
#44810=DIRECTION('ref_axis',(0.269603455472075,3.05583905676118E-32,-0.962971430935268));
#44811=DIRECTION('center_axis',(1.22464679915E-16,1.,5.47382212627E-48));
#44812=DIRECTION('ref_axis',(1.,-1.22464679915E-16,-6.703498746053E-64));
#44813=DIRECTION('center_axis',(1.22464679915E-16,1.,5.47382212627E-48));
#44814=DIRECTION('ref_axis',(1.,-1.22464679915E-16,0.));
#44815=DIRECTION('center_axis',(0.,0.,1.));
#44816=DIRECTION('ref_axis',(-0.70710677910001,-0.707106783273086,0.));
#44817=DIRECTION('center_axis',(-7.24819500366175E-17,-1.,-6.01900799944532E-17));
#44818=DIRECTION('ref_axis',(0.638858327474962,0.,-0.769324403236954));
#44819=DIRECTION('center_axis',(1.22464679915E-16,1.,5.47382212627E-48));
#44820=DIRECTION('ref_axis',(1.,-1.22464679915E-16,5.9677926224237E-64));
#44821=DIRECTION('center_axis',(0.769324403236954,-9.42150667929943E-17,
0.638858327474961));
#44822=DIRECTION('ref_axis',(0.638858327474961,7.17307849792281E-32,-0.769324403236954));
#44823=DIRECTION('center_axis',(1.22464679915E-16,1.,5.47382212627E-48));
#44824=DIRECTION('ref_axis',(1.,-1.22464679915E-16,6.22660996643423E-64));
#44825=DIRECTION('center_axis',(0.382683432365114,-4.68652040533141E-17,
-0.923879532511277));
#44826=DIRECTION('ref_axis',(2.5429740769239E-34,-1.,5.07265313324192E-17));
#44827=DIRECTION('',(-0.923879532511277,1.79771717893054E-16,-0.382683432365114));
#44828=DIRECTION('',(-1.22604516347E-16,-1.,0.));
#44829=DIRECTION('',(0.923879532511277,-1.79771717893054E-16,0.382683432365114));
#44830=DIRECTION('',(-1.66950830771E-16,-1.,0.));
#44831=DIRECTION('center_axis',(-1.22464679914995E-16,-1.,-2.84643200354157E-29));
#44832=DIRECTION('ref_axis',(0.175818770215043,-2.15315894174053E-17,-0.984422551570244));
#44833=DIRECTION('center_axis',(-1.22464679915E-16,-1.,1.23259516441E-32));
#44834=DIRECTION('ref_axis',(1.,-1.22464679915E-16,-1.13230748611233E-48));
#44835=DIRECTION('',(0.,-1.,0.));
#44836=DIRECTION('center_axis',(-1.22464679915E-16,-1.,1.23259516441E-32));
#44837=DIRECTION('ref_axis',(1.,-1.22464679915E-16,-1.13230748611233E-48));
#44838=DIRECTION('',(0.,1.,0.));
#44839=DIRECTION('center_axis',(-1.22464679915E-16,-1.,3.08148791102E-33));
#44840=DIRECTION('ref_axis',(1.,-1.22464679915E-16,-2.83076871527624E-49));
#44841=DIRECTION('',(0.,-1.,0.));
#44842=DIRECTION('center_axis',(-0.978784588777817,0.0498161334628422,-0.198743758689054));
#44843=DIRECTION('ref_axis',(0.194346018843094,-0.0814603510708595,-0.9775448000799));
#44844=DIRECTION('center_axis',(1.22464679915E-16,1.,0.));
#44845=DIRECTION('ref_axis',(1.,-1.22464679915E-16,0.));
#44846=DIRECTION('',(1.23054276128E-16,1.,0.));
#44847=DIRECTION('center_axis',(0.382683432365114,-4.6865204053314E-17,
0.923879532511277));
#44848=DIRECTION('ref_axis',(-1.22464679914861E-16,-1.,3.33030126354153E-33));
#44849=DIRECTION('',(0.923879532511277,-1.79771717893054E-16,-0.382683432365114));
#44850=DIRECTION('',(-1.66950830771E-16,-1.,0.));
#44851=DIRECTION('center_axis',(-0.382683432285969,-1.4148764236578E-8,
-0.92387953254406));
#44852=DIRECTION('ref_axis',(0.907892103408984,-0.185229284331876,-0.376061219475649));
#44853=DIRECTION('',(-0.923879532511277,1.79771717893054E-16,0.382683432365114));
#44854=DIRECTION('',(-1.22604516347E-16,-1.,0.));
#44855=DIRECTION('center_axis',(-1.22464679915019E-16,-1.,-7.85779417309992E-30));
#44856=DIRECTION('ref_axis',(0.923879532511277,-1.13142611229034E-16,0.382683432365114));
#44857=DIRECTION('center_axis',(1.22464679915E-16,1.,0.));
#44858=DIRECTION('ref_axis',(1.,-1.22464679915E-16,0.));
#44859=DIRECTION('',(-1.16865581539E-16,-1.,0.));
#44860=DIRECTION('center_axis',(0.923879532511277,-1.13142611229034E-16,
0.382683432365114));
#44861=DIRECTION('ref_axis',(-1.31021084567677E-32,-1.,-2.95655891162504E-16));
#44862=DIRECTION('',(0.382683432365114,0.,-0.923879532511277));
#44863=DIRECTION('',(0.,-1.,0.));
#44864=DIRECTION('center_axis',(-0.923879532551608,-4.64401307323437E-9,
-0.382683432267745));
#44865=DIRECTION('ref_axis',(0.376061194482232,-0.185229675161476,-0.907892034023964));
#44866=DIRECTION('',(-0.382683432365114,0.,0.923879532511277));
#44867=DIRECTION('center_axis',(-0.923879532525146,-3.85070599698536E-9,
-0.382683432331632));
#44868=DIRECTION('ref_axis',(0.375653592878795,0.190793753652541,-0.906908000694903));
#44869=DIRECTION('center_axis',(-1.22464679915019E-16,-1.,7.85779417309992E-30));
#44870=DIRECTION('ref_axis',(0.923879532511276,-1.13142611229034E-16,-0.382683432365115));
#44871=DIRECTION('center_axis',(1.22464679915E-16,1.,6.16297582204E-33));
#44872=DIRECTION('ref_axis',(1.,-1.22464679915E-16,-7.54746861370013E-49));
#44873=DIRECTION('',(-2.33731163079E-16,-1.,0.));
#44874=DIRECTION('center_axis',(0.923879532511277,-1.13142611229034E-16,
-0.382683432365114));
#44875=DIRECTION('ref_axis',(-1.31021084567677E-32,-1.,2.95655891162504E-16));
#44876=DIRECTION('',(-0.382683432365114,0.,-0.923879532511277));
#44877=DIRECTION('',(-1.66950830771E-16,-1.,0.));
#44878=DIRECTION('',(0.382683432365114,0.,0.923879532511277));
#44879=DIRECTION('center_axis',(-0.923879531876915,-6.81101431042489E-8,
0.382683433896593));
#44880=DIRECTION('ref_axis',(0.372466611695662,-0.229527742255026,0.899213900419285));
#44881=DIRECTION('center_axis',(-1.2246467991498E-16,-1.,-4.9218209689896E-29));
#44882=DIRECTION('ref_axis',(0.382683432365114,-4.6865204053314E-17,-0.923879532511277));
#44883=DIRECTION('center_axis',(1.22464679915E-16,1.,0.));
#44884=DIRECTION('ref_axis',(1.,-1.22464679915E-16,0.));
#44885=DIRECTION('center_axis',(-1.22464679915E-16,-1.,0.));
#44886=DIRECTION('ref_axis',(1.,-1.22464679915E-16,0.));
#44887=DIRECTION('center_axis',(-0.766057840542209,-0.255399249832434,0.589853039433415));
#44888=DIRECTION('ref_axis',(0.202361789893946,-0.966835675378721,-0.155815540963958));
#44889=DIRECTION('center_axis',(-0.792335098973394,9.70330642810483E-17,
0.610086134029304));
#44890=DIRECTION('ref_axis',(0.610086134029304,5.05601228850744E-32,0.792335098973394));
#44891=DIRECTION('center_axis',(1.22464679915E-16,1.,0.));
#44892=DIRECTION('ref_axis',(1.,-1.22464679915E-16,0.));
#44893=DIRECTION('center_axis',(-7.68827025909336E-17,-1.,5.91985270603321E-17));
#44894=DIRECTION('ref_axis',(0.610086134029304,0.,0.792335098973394));
#44895=DIRECTION('center_axis',(-0.611236674075818,7.48549036428777E-17,
0.791447868317764));
#44896=DIRECTION('ref_axis',(0.791447868317764,-7.00049973634741E-32,0.611236674075818));
#44897=DIRECTION('center_axis',(1.22464679915E-16,1.,5.47382212627E-48));
#44898=DIRECTION('ref_axis',(1.,-1.22464679915E-16,5.40238148608971E-64));
#44899=DIRECTION('center_axis',(-1.22464679914914E-16,-1.,1.11943608056428E-28));
#44900=DIRECTION('ref_axis',(0.610086134029304,-7.47140031243373E-17,0.792335098973394));
#44901=DIRECTION('',(0.,-1.,0.));
#44902=DIRECTION('',(0.,-1.,0.));
#44903=DIRECTION('center_axis',(0.,1.,0.));
#44904=DIRECTION('ref_axis',(0.998985821715464,0.,0.0450258593641339));
#44905=DIRECTION('center_axis',(0.678891257295808,-8.31402005216764E-17,
-0.734238830876792));
#44906=DIRECTION('ref_axis',(4.92781901212525E-33,-1.,1.13233183843457E-16));
#44907=DIRECTION('',(0.734238830876792,0.,0.678891257295808));
#44908=DIRECTION('center_axis',(-0.678891257318237,-7.43492351073594E-12,
0.734238830856053));
#44909=DIRECTION('ref_axis',(1.46208970879984E-10,-1.,1.25062923000865E-10));
#44910=DIRECTION('',(0.,-1.,0.));
#44911=DIRECTION('',(0.734238830876792,0.,0.678891257295808));
#44912=DIRECTION('',(0.,-1.,0.));
#44913=DIRECTION('',(-0.734238830876791,0.,-0.678891257295807));
#44914=DIRECTION('center_axis',(-1.22464679914942E-16,-1.,7.54279763108459E-29));
#44915=DIRECTION('ref_axis',(-0.612227349738988,7.49762264208985E-17,-0.790681776842982));
#44916=DIRECTION('center_axis',(-1.22464679915E-16,-1.,-6.16297582204E-33));
#44917=DIRECTION('ref_axis',(1.,-1.22464679915E-16,-7.54746861370013E-49));
#44918=DIRECTION('',(0.,-1.,0.));
#44919=DIRECTION('center_axis',(1.22464679915E-16,1.,1.23259516441E-32));
#44920=DIRECTION('ref_axis',(1.,-1.22464679915E-16,-1.50949372274247E-48));
#44921=DIRECTION('center_axis',(1.22464679914998E-16,1.,-1.73663083545565E-29));
#44922=DIRECTION('ref_axis',(0.095298509688002,-1.16707014853003E-17,0.99544874004202));
#44923=DIRECTION('center_axis',(-1.22464679915E-16,-1.,0.));
#44924=DIRECTION('ref_axis',(1.,-1.22464679915E-16,0.));
#44925=DIRECTION('center_axis',(1.22464679915E-16,1.,0.));
#44926=DIRECTION('ref_axis',(1.,-1.22464679915E-16,0.));
#44927=DIRECTION('',(-1.32169407693E-16,-1.,0.));
#44928=DIRECTION('center_axis',(-1.22464679915E-16,-1.,-7.60253073092891E-48));
#44929=DIRECTION('ref_axis',(-1.,1.22464679915E-16,9.3104149250716E-64));
#44930=DIRECTION('center_axis',(-1.22464679915E-16,-1.,6.16297582204E-33));
#44931=DIRECTION('ref_axis',(1.,-1.22464679915E-16,7.54746861370013E-49));
#44932=DIRECTION('',(-1.23358113847E-16,-1.,0.));
#44933=DIRECTION('center_axis',(1.22464679915E-16,1.,3.08148791102E-33));
#44934=DIRECTION('ref_axis',(1.,-1.22464679915E-16,-3.77373430685006E-49));
#44935=DIRECTION('center_axis',(-1.,1.22464679915E-16,-6.12323399574E-17));
#44936=DIRECTION('ref_axis',(-6.12323399574E-17,0.,1.));
#44937=DIRECTION('',(-2.17106560191E-16,0.,1.));
#44938=DIRECTION('',(2.19188076492E-16,0.,-1.));
#44939=DIRECTION('',(-1.32169407693E-16,-1.,0.));
#44940=DIRECTION('center_axis',(1.22464679914917E-16,1.,-1.21085355525786E-28));
#44941=DIRECTION('ref_axis',(0.566106835688783,-6.93280924301735E-17,0.824331881335687));
#44942=DIRECTION('',(0.,-1.,0.));
#44943=DIRECTION('center_axis',(-1.22464679915E-16,-1.,-1.23259516441E-32));
#44944=DIRECTION('ref_axis',(1.,-1.22464679915E-16,-1.50949372274247E-48));
#44945=DIRECTION('center_axis',(1.22464679915E-16,1.,-1.21640491694863E-46));
#44946=DIRECTION('ref_axis',(-1.,1.22464679915E-16,-5.78241158658936E-15));
#44947=DIRECTION('center_axis',(-1.22464679915E-16,-1.,-6.16297582204E-33));
#44948=DIRECTION('ref_axis',(1.,-1.22464679915E-16,-7.54746861370013E-49));
#44949=DIRECTION('',(-1.04083408559E-16,-1.,0.));
#44950=DIRECTION('center_axis',(1.22464679915E-16,1.,7.00649232162E-46));
#44951=DIRECTION('ref_axis',(1.,-1.22464679915E-16,-8.58047839494098E-62));
#44952=DIRECTION('center_axis',(1.22464679914999E-16,1.,-1.9442368107527E-29));
#44953=DIRECTION('ref_axis',(0.0510637267514752,-6.25350295186696E-18,0.998695396910515));
#44954=DIRECTION('center_axis',(-1.22464679915E-16,-1.,1.23259516441E-32));
#44955=DIRECTION('ref_axis',(1.,-1.22464679915E-16,-1.40210791623289E-48));
#44956=DIRECTION('center_axis',(1.22464679915E-16,1.,-1.54074395551E-33));
#44957=DIRECTION('ref_axis',(1.,-1.22464679915E-16,-1.75263489528827E-49));
#44958=DIRECTION('center_axis',(2.17357452795E-16,-2.66186108837E-32,-1.));
#44959=DIRECTION('ref_axis',(1.,5.7857534586223E-48,2.17357452795E-16));
#44960=DIRECTION('',(-8.96394535471E-17,0.,1.));
#44961=DIRECTION('center_axis',(1.65006284806E-14,-2.02074418527E-30,-1.));
#44962=DIRECTION('ref_axis',(1.,-1.71077471584193E-45,1.65006284806E-14));
#44963=DIRECTION('',(-8.96394535471E-17,0.,1.));
#44964=DIRECTION('center_axis',(-1.74860126378E-14,2.14141894068E-30,-1.));
#44965=DIRECTION('ref_axis',(1.,2.97181576564967E-46,-1.74860126378E-14));
#44966=DIRECTION('center_axis',(-1.17989839311979E-16,-1.,2.29779399358865E-17));
#44967=DIRECTION('ref_axis',(0.191153986297934,0.,0.981560061087659));
#44968=DIRECTION('center_axis',(1.22464679915E-16,1.,5.47382212627E-48));
#44969=DIRECTION('ref_axis',(1.,-1.22464679915E-16,-6.703498746053E-64));
#44970=DIRECTION('center_axis',(-0.973274002238674,1.1919168915396E-16,
0.229646938943923));
#44971=DIRECTION('ref_axis',(0.229646938943923,-2.91124363913666E-32,0.973274002238674));
#44972=DIRECTION('center_axis',(1.22464679915E-16,1.,5.47382212627E-48));
#44973=DIRECTION('ref_axis',(1.,-1.22464679915E-16,-6.703498746053E-64));
#44974=DIRECTION('center_axis',(-0.981560061087659,1.20206438697958E-16,
0.191153986297933));
#44975=DIRECTION('ref_axis',(0.191153986297933,-8.55574366268044E-33,0.981560061087659));
#44976=DIRECTION('center_axis',(-1.17989839311979E-16,-1.,2.29779399358865E-17));
#44977=DIRECTION('ref_axis',(-0.191153986297933,0.,-0.981560061087659));
#44978=DIRECTION('center_axis',(-1.22464679915E-16,-1.,-5.47382212627E-48));
#44979=DIRECTION('ref_axis',(1.,-1.22464679915E-16,-6.703498746053E-64));
#44980=DIRECTION('center_axis',(-1.22464679915E-16,-1.,0.));
#44981=DIRECTION('ref_axis',(1.,-1.22464679915E-16,0.));
#44982=DIRECTION('center_axis',(-2.17357452795E-16,2.66186108837E-32,1.));
#44983=DIRECTION('ref_axis',(1.,5.7857534586223E-48,2.17357452795E-16));
#44984=DIRECTION('center_axis',(-2.17357452795E-16,2.66186108835898E-32,
1.));
#44985=DIRECTION('ref_axis',(-3.61400724161833E-16,-1.,-5.19345299584946E-32));
#44986=DIRECTION('',(5.71347413162E-17,0.,-1.));
#44987=DIRECTION('',(7.61796550883E-17,0.,-1.));
#44988=DIRECTION('center_axis',(-6.13854691746E-15,7.51755183389E-31,1.));
#44989=DIRECTION('ref_axis',(1.,2.67726580969963E-46,6.13854691746E-15));
#44990=DIRECTION('center_axis',(-4.29367103357466E-45,-1.,7.25136572506882E-31));
#44991=DIRECTION('ref_axis',(-1.,0.,-5.9211894646675E-15));
#44992=DIRECTION('center_axis',(-1.22464679915E-16,-1.,-5.47382212627E-48));
#44993=DIRECTION('ref_axis',(1.,-1.22464679915E-16,-6.703498746053E-64));
#44994=DIRECTION('center_axis',(-1.22464679915E-16,-1.,-3.08148791102E-33));
#44995=DIRECTION('ref_axis',(1.,-1.22464679915E-16,-3.77373430685006E-49));
#44996=DIRECTION('center_axis',(0.984869499718035,-1.20611728041004E-16,
-0.173297629889006));
#44997=DIRECTION('ref_axis',(0.173297629889006,5.41148511020646E-32,0.984869499718035));
#44998=DIRECTION('center_axis',(-1.18786812255882E-16,-1.,2.09017266063253E-17));
#44999=DIRECTION('ref_axis',(0.173297629889006,0.,0.984869499718035));
#45000=DIRECTION('center_axis',(-1.22464679915E-16,-1.,-5.47382212627E-48));
#45001=DIRECTION('ref_axis',(1.,-1.22464679915E-16,-6.703498746053E-64));
#45002=DIRECTION('center_axis',(-1.22464679915E-16,-1.,-5.47382212627E-48));
#45003=DIRECTION('ref_axis',(1.,-1.22464679915E-16,-6.703498746053E-64));
#45004=DIRECTION('center_axis',(0.825067330468845,-1.01041606533981E-16,
-0.565034423900893));
#45005=DIRECTION('ref_axis',(0.565034423900893,7.24547600115018E-32,0.825067330468845));
#45006=DIRECTION('center_axis',(-6.60215246509141E-17,-1.,-6.10447636300053E-17));
#45007=DIRECTION('ref_axis',(0.678891257295808,0.,-0.734238830876792));
#45008=DIRECTION('center_axis',(-1.22464679915E-16,-1.,-5.47382212627E-48));
#45009=DIRECTION('ref_axis',(1.,-1.22464679915E-16,-6.703498746053E-64));
#45010=DIRECTION('center_axis',(-0.734238830876792,8.99183234042744E-17,
-0.678891257295808));
#45011=DIRECTION('ref_axis',(0.678891257295808,-2.24691316591619E-32,-0.734238830876792));
#45012=DIRECTION('center_axis',(-1.22464679915E-16,-1.,0.));
#45013=DIRECTION('ref_axis',(1.,-1.22464679915E-16,0.));
#45014=DIRECTION('center_axis',(-8.3366128569448E-17,-1.,5.70919859380671E-17));
#45015=DIRECTION('ref_axis',(0.565034423900894,0.,0.825067330468845));
#45016=DIRECTION('center_axis',(-1.22464679915E-16,-1.,-5.47382212627E-48));
#45017=DIRECTION('ref_axis',(1.,-1.22464679915E-16,-6.703498746053E-64));
#45018=DIRECTION('center_axis',(-1.22464679915E-16,-1.,0.));
#45019=DIRECTION('ref_axis',(1.,-1.22464679915E-16,0.));
#45020=DIRECTION('center_axis',(-0.734238830876792,8.99183234042744E-17,
-0.678891257295808));
#45021=DIRECTION('ref_axis',(0.678891257295808,-2.24691316591619E-32,-0.734238830876792));
#45022=DIRECTION('center_axis',(-0.734238830876792,8.99183234039869E-17,
-0.678891257295808));
#45023=DIRECTION('ref_axis',(-6.60215246505446E-17,-1.,-6.10447636296637E-17));
#45024=DIRECTION('',(0.734238830876791,0.,0.678891257295807));
#45025=DIRECTION('',(0.734238830876791,0.,0.678891257295807));
#45026=DIRECTION('center_axis',(-5.11601622893148E-18,-1.,-2.45021972047681E-17));
#45027=DIRECTION('ref_axis',(0.978889450967439,0.,-0.204390417546091));
#45028=DIRECTION('center_axis',(1.22464679915E-16,1.,5.47382212627E-48));
#45029=DIRECTION('ref_axis',(1.,-1.22464679915E-16,-6.703498746053E-64));
#45030=DIRECTION('center_axis',(0.419584599500152,-5.13842936749187E-17,
0.90771623531933));
#45031=DIRECTION('ref_axis',(0.90771623531933,-2.72267697829008E-32,-0.419584599500152));
#45032=DIRECTION('center_axis',(1.22464679915E-16,1.,5.47382212627E-48));
#45033=DIRECTION('ref_axis',(1.,-1.22464679915E-16,-6.703498746053E-64));
#45034=DIRECTION('center_axis',(0.204390417546092,-2.50306070625112E-17,
0.978889450967439));
#45035=DIRECTION('ref_axis',(0.978889450967439,-1.05289930055147E-32,-0.204390417546092));
#45036=DIRECTION('center_axis',(0.382683432358122,-7.15701713406616E-12,
0.923879532514173));
#45037=DIRECTION('ref_axis',(0.653281512864065,-0.707106748253927,-0.270598062675614));
#45038=DIRECTION('center_axis',(0.38263696551694,0.0155798009318935,0.923767407101436));
#45039=DIRECTION('ref_axis',(0.670813976387107,-0.692209320629282,-0.266185772568081));
#45040=DIRECTION('center_axis',(-2.15600582822439E-17,-1.,-4.66423576092589E-17));
#45041=DIRECTION('ref_axis',(0.90771623531933,0.,-0.419584599500153));
#45042=DIRECTION('center_axis',(1.22464679915E-16,1.,5.47382212627E-48));
#45043=DIRECTION('ref_axis',(1.,-1.22464679915E-16,-6.703498746053E-64));
#45044=DIRECTION('center_axis',(1.22464679915E-16,1.,-6.16297582204E-33));
#45045=DIRECTION('ref_axis',(1.,-1.22464679915E-16,7.54746861370013E-49));
#45046=DIRECTION('center_axis',(-0.0335155327516907,4.10446899060886E-18,
-0.999438196720723));
#45047=DIRECTION('ref_axis',(0.999438196720723,5.21239906410075E-34,-0.0335155327516907));
#45048=DIRECTION('center_axis',(-0.382579809484663,-0.023273941363381,0.923629261678133));
#45049=DIRECTION('ref_axis',(0.67915166414103,-0.684855543423067,0.264056626005038));
#45050=DIRECTION('center_axis',(-0.854119175465141,0.0486728274083025,-0.517794737299279));
#45051=DIRECTION('ref_axis',(0.493271987057746,-0.239694157277359,-0.836199412670925));
#45052=DIRECTION('center_axis',(-0.382683355639379,3.37879318962009E-8,
0.923879564292112));
#45053=DIRECTION('ref_axis',(0.653293929364642,-0.70709332290268,0.270603168055648));
#45054=DIRECTION('center_axis',(0.382579803835696,0.0232740021763249,0.923629262485624));
#45055=DIRECTION('ref_axis',(0.679151158571202,-0.684856150498969,-0.264056351817426));
#45056=DIRECTION('center_axis',(-0.854168457972516,0.0469001823254461,0.517877030097584));
#45057=DIRECTION('ref_axis',(0.479715571846213,-0.313264897733587,0.819596287190362));
#45058=DIRECTION('center_axis',(-5.06268119967007E-18,-1.,2.43796819441885E-17));
#45059=DIRECTION('ref_axis',(0.979111878581668,0.,0.203322230019931));
#45060=DIRECTION('center_axis',(-1.22464679915E-16,-1.,-5.47382212627E-48));
#45061=DIRECTION('ref_axis',(1.,-1.22464679915E-16,-6.703498746053E-64));
#45062=DIRECTION('center_axis',(0.203322230019931,-2.48997918188915E-17,
-0.979111878581668));
#45063=DIRECTION('ref_axis',(0.979111878581668,-1.33094098597294E-33,0.203322230019931));
#45064=DIRECTION('center_axis',(-1.22464679915E-16,-1.,-5.47382212627E-48));
#45065=DIRECTION('ref_axis',(1.,-1.22464679915E-16,-6.703498746053E-64));
#45066=DIRECTION('center_axis',(-1.22464679915E-16,-1.,0.));
#45067=DIRECTION('ref_axis',(0.,0.,1.));
#45068=DIRECTION('center_axis',(1.22464679915E-16,1.,5.47382212627E-48));
#45069=DIRECTION('ref_axis',(1.,-1.22464679915E-16,-6.703498746053E-64));
#45070=DIRECTION('center_axis',(1.22464679915E-16,1.,5.47382212627E-48));
#45071=DIRECTION('ref_axis',(1.,-1.22464679915E-16,-6.703498746053E-64));
#45072=DIRECTION('center_axis',(-1.,1.22464679915E-16,-6.12323399574E-17));
#45073=DIRECTION('ref_axis',(-1.22464679915E-16,-1.,-7.49879891332945E-33));
#45074=DIRECTION('center_axis',(-5.06268119967007E-18,-1.,2.43796819441885E-17));
#45075=DIRECTION('ref_axis',(-0.979111878581668,0.,-0.203322230019931));
#45076=DIRECTION('center_axis',(1.22464679915E-16,1.,-3.08148791102E-33));
#45077=DIRECTION('ref_axis',(1.,-1.22464679915E-16,3.77373430685006E-49));
#45078=DIRECTION('center_axis',(-1.,1.22464679915E-16,-6.12323399574E-17));
#45079=DIRECTION('ref_axis',(-1.22464679915E-16,-1.,-7.49879891332945E-33));
#45080=DIRECTION('center_axis',(1.22464679915E-16,1.,5.47382212627E-48));
#45081=DIRECTION('ref_axis',(1.,-1.22464679915E-16,-6.703498746053E-64));
#45082=DIRECTION('center_axis',(-1.,1.22464679915E-16,-6.12323399574E-17));
#45083=DIRECTION('ref_axis',(6.12323399574E-17,-7.49879891332945E-33,-1.));
#45084=DIRECTION('',(1.,0.,0.));
#45085=DIRECTION('',(1.,0.,0.));
#45086=DIRECTION('center_axis',(-0.923629285580912,-0.0232739550451307,
0.382579750945933));
#45087=DIRECTION('ref_axis',(0.293516536156795,-0.684855540988734,0.666948971795853));
#45088=DIRECTION('center_axis',(-0.237817287821767,0.0486733035113049,-0.970089607788062));
#45089=DIRECTION('ref_axis',(0.940079656645484,-0.239688427719097,-0.242486487827378));
#45090=DIRECTION('center_axis',(-0.923879500687952,3.38250871562384E-8,
0.382683509193406));
#45091=DIRECTION('ref_axis',(0.27060322877475,-0.707093332552184,0.653293893769816));
#45092=DIRECTION('center_axis',(-0.382579702456672,0.0232740169688495,0.923629304105439));
#45093=DIRECTION('ref_axis',(0.666946643181329,-0.68485819132246,0.293515643412214));
#45094=DIRECTION('center_axis',(-0.382683432278913,-8.22329173318955E-13,
0.923879532546982));
#45095=DIRECTION('ref_axis',(0.653281507495611,-0.707106754092149,0.270598060380203));
#45096=DIRECTION('center_axis',(-0.970090315877611,0.0486596525433631,-0.237817192933641));
#45097=DIRECTION('ref_axis',(0.242427238271629,0.244261263603387,-0.938917179120112));
#45098=DIRECTION('center_axis',(-7.79403475186991E-17,-1.,5.89087594505755E-17));
#45099=DIRECTION('ref_axis',(0.602966636474875,0.,0.797766403966835));
#45100=DIRECTION('center_axis',(1.22464679915E-16,1.,5.47382212627E-48));
#45101=DIRECTION('ref_axis',(1.,-1.22464679915E-16,-6.703498746053E-64));
#45102=DIRECTION('center_axis',(-0.585630202615096,7.17190153117117E-17,
0.810578352650132));
#45103=DIRECTION('ref_axis',(0.810578352650132,6.4321265031143E-32,0.585630202615096));
#45104=DIRECTION('center_axis',(1.22464679915E-16,1.,5.47382212627E-48));
#45105=DIRECTION('ref_axis',(1.,-1.22464679915E-16,-6.703498746053E-64));
#45106=DIRECTION('center_axis',(-0.797766403966835,9.76982073084798E-17,
0.602966636474875));
#45107=DIRECTION('ref_axis',(0.602966636474875,6.43171104150991E-32,0.797766403966835));
#45108=DIRECTION('center_axis',(1.22464679915E-16,1.,5.47382212627E-48));
#45109=DIRECTION('ref_axis',(1.,-1.22464679915E-16,-6.703498746053E-64));
#45110=DIRECTION('center_axis',(-7.79403475186991E-17,-1.,5.89087594505755E-17));
#45111=DIRECTION('ref_axis',(-0.602966636474876,0.,-0.797766403966835));
#45112=DIRECTION('center_axis',(-1.22464679915E-16,-1.,-5.47382212627E-48));
#45113=DIRECTION('ref_axis',(1.,-1.22464679915E-16,-6.703498746053E-64));
#45114=DIRECTION('center_axis',(-1.22464679915E-16,-1.,0.));
#45115=DIRECTION('ref_axis',(1.,-1.22464679915E-16,0.));
#45116=DIRECTION('center_axis',(0.734238830876792,-8.99183234042744E-17,
0.678891257295808));
#45117=DIRECTION('ref_axis',(0.678891257295808,-2.24691316591619E-32,-0.734238830876792));
#45118=DIRECTION('center_axis',(-0.734238830876792,8.99183234042744E-17,
-0.678891257295808));
#45119=DIRECTION('ref_axis',(0.678891257295808,1.51038693775819E-31,-0.734238830876792));
#45120=DIRECTION('',(-0.734238830876791,0.,-0.678891257295807));
#45121=DIRECTION('',(-0.734238830876791,0.,-0.678891257295807));
#45122=DIRECTION('center_axis',(0.73423883087825,-8.99183234044306E-17,
0.678891257294231));
#45123=DIRECTION('ref_axis',(0.678891257294231,1.10716302178481E-31,-0.73423883087825));
#45124=DIRECTION('center_axis',(-6.60215246511763E-17,-1.,-6.10447636299848E-17));
#45125=DIRECTION('ref_axis',(-0.678891257294231,0.,0.73423883087825));
#45126=DIRECTION('center_axis',(-1.22464679915E-16,-1.,-5.47382212627E-48));
#45127=DIRECTION('ref_axis',(1.,-1.22464679915E-16,-6.703498746053E-64));
#45128=DIRECTION('center_axis',(-1.22464679915E-16,-1.,0.));
#45129=DIRECTION('ref_axis',(1.,-1.22464679915E-16,0.));
#45130=DIRECTION('center_axis',(0.581646529321033,-7.12311560368041E-17,
-0.813441648140047));
#45131=DIRECTION('ref_axis',(0.813441648140047,-2.80119922649672E-32,0.581646529321033));
#45132=DIRECTION('center_axis',(-4.14313546884292E-17,-1.,5.79423889656346E-17));
#45133=DIRECTION('ref_axis',(0.813441648140047,0.,0.581646529321034));
#45134=DIRECTION('center_axis',(-1.22464679915E-16,-1.,-5.47382212627E-48));
#45135=DIRECTION('ref_axis',(1.,-1.22464679915E-16,-6.703498746053E-64));
#45136=DIRECTION('center_axis',(-1.22464679915E-16,-1.,-5.47382212627E-48));
#45137=DIRECTION('ref_axis',(1.,-1.22464679915E-16,-6.703498746053E-64));
#45138=DIRECTION('center_axis',(0.142980079684983,-1.75100096927979E-17,
-0.98972556641388));
#45139=DIRECTION('ref_axis',(0.98972556641388,3.23015489124122E-33,0.142980079684983));
#45140=DIRECTION('center_axis',(-1.22464679915E-16,-1.,0.));
#45141=DIRECTION('ref_axis',(0.,0.,-1.));
#45142=DIRECTION('center_axis',(-1.22464679915E-16,-1.,-5.47382212627E-48));
#45143=DIRECTION('ref_axis',(1.,-1.22464679915E-16,-6.703498746053E-64));
#45144=DIRECTION('center_axis',(-1.,1.22464679915E-16,-6.12323399574E-17));
#45145=DIRECTION('ref_axis',(-1.22464679915E-16,-1.,-7.49879891332945E-33));
#45146=DIRECTION('center_axis',(-1.22464679915E-16,-1.,-5.47382212627E-48));
#45147=DIRECTION('ref_axis',(1.,-1.22464679915E-16,-6.703498746053E-64));
#45148=DIRECTION('center_axis',(-2.50358258116745E-18,-1.,1.73301042611612E-17));
#45149=DIRECTION('ref_axis',(0.98972556641388,0.,0.142980079684983));
#45150=DIRECTION('center_axis',(-1.22464679915E-16,-1.,-5.47382212627E-48));
#45151=DIRECTION('ref_axis',(1.,-1.22464679915E-16,-6.703498746053E-64));
#45152=DIRECTION('center_axis',(-1.22464679915E-16,-1.,-5.47382212627E-48));
#45153=DIRECTION('ref_axis',(1.,-1.22464679915E-16,-6.703498746053E-64));
#45154=DIRECTION('center_axis',(-1.,1.22464679915E-16,-6.12323399574E-17));
#45155=DIRECTION('ref_axis',(-1.22464679915E-16,-1.,-7.49879891332945E-33));
#45156=DIRECTION('center_axis',(-1.,1.22464679915E-16,-6.12323399574E-17));
#45157=DIRECTION('ref_axis',(-1.22464679915E-16,-1.,-7.49879891332945E-33));
#45158=DIRECTION('',(1.,0.,2.89652532403E-16));
#45159=DIRECTION('',(1.,0.,2.89652532403E-16));
#45160=DIRECTION('center_axis',(-0.734238830876792,8.99183234042744E-17,
-0.678891257295808));
#45161=DIRECTION('ref_axis',(-0.678891257295808,2.24691316591619E-32,0.734238830876792));
#45162=DIRECTION('',(0.734238830876791,0.,0.678891257295807));
#45163=DIRECTION('center_axis',(0.734238830881723,7.25497069118018E-12,
0.678891257290474));
#45164=DIRECTION('ref_axis',(-0.678891257290474,0.,0.734238830881723));
#45165=DIRECTION('',(0.734238830876791,0.,0.678891257295807));
#45166=DIRECTION('center_axis',(-0.734238830876792,8.991832340449E-17,-0.678891257295808));
#45167=DIRECTION('ref_axis',(6.6021524650914E-17,1.,6.10447636300053E-17));
#45168=DIRECTION('',(-0.734238830876791,0.,-0.678891257295807));
#45169=DIRECTION('',(-0.734238830876791,0.,-0.678891257295807));
#45170=DIRECTION('center_axis',(1.69872863391202E-17,1.,-4.23293596334453E-17));
#45171=DIRECTION('ref_axis',(-0.928056183869048,0.,-0.37244022283102));
#45172=DIRECTION('center_axis',(-1.22464679915E-16,-1.,-5.47382212627E-48));
#45173=DIRECTION('ref_axis',(1.,-1.22464679915E-16,-6.703498746053E-64));
#45174=DIRECTION('center_axis',(-1.22464679915E-16,-1.,-5.47382212627E-48));
#45175=DIRECTION('ref_axis',(1.,-1.22464679915E-16,-6.703498746053E-64));
#45176=DIRECTION('center_axis',(0.204390417555875,-1.0300808526955E-11,
0.978889450965396));
#45177=DIRECTION('ref_axis',(-1.00253139123651E-11,1.,1.26158343031571E-11));
#45178=DIRECTION('center_axis',(0.,1.,0.));
#45179=DIRECTION('ref_axis',(-0.231145326606897,0.,-0.972919235079557));
#45180=DIRECTION('center_axis',(-1.22464679915E-16,-1.,6.16297582204E-33));
#45181=DIRECTION('ref_axis',(1.,-1.22464679915E-16,7.54746861370013E-49));
#45182=DIRECTION('center_axis',(-0.0335155327516907,4.10446899060886E-18,
-0.999438196720723));
#45183=DIRECTION('ref_axis',(0.999438196720723,5.21239906410075E-34,-0.0335155327516907));
#45184=DIRECTION('center_axis',(5.9296278727138E-17,1.,-6.12017248415691E-17));
#45185=DIRECTION('ref_axis',(-0.718198537785833,0.,-0.695838242928838));
#45186=DIRECTION('center_axis',(1.22464679915E-16,1.,5.47382212627E-48));
#45187=DIRECTION('ref_axis',(1.,-1.22464679915E-16,-6.703498746053E-64));
#45188=DIRECTION('center_axis',(1.22464679915E-16,1.,5.47382212627E-48));
#45189=DIRECTION('ref_axis',(1.,-1.22464679915E-16,-6.703498746053E-64));
#45190=DIRECTION('center_axis',(0.,1.,0.));
#45191=DIRECTION('ref_axis',(0.776012376688289,0.,0.630717679494236));
#45192=DIRECTION('center_axis',(-1.22464679915E-16,-1.,-5.47382212627E-48));
#45193=DIRECTION('ref_axis',(1.,-1.22464679915E-16,-6.703498746053E-64));
#45194=DIRECTION('center_axis',(-1.,1.22464679915E-16,-6.12323399574E-17));
#45195=DIRECTION('ref_axis',(-1.22464679915E-16,-1.,-7.49879891332945E-33));
#45196=DIRECTION('center_axis',(0.,0.,1.));
#45197=DIRECTION('ref_axis',(1.,0.,0.));
#45198=DIRECTION('center_axis',(-1.22464679915E-16,-1.,3.08148791102E-33));
#45199=DIRECTION('ref_axis',(1.,-1.22464679915E-16,3.77373430685006E-49));
#45200=DIRECTION('center_axis',(-1.,1.22464679915E-16,-6.12323399574E-17));
#45201=DIRECTION('ref_axis',(-1.22464679915E-16,-1.,-7.49879891332945E-33));
#45202=DIRECTION('center_axis',(0.,1.,0.));
#45203=DIRECTION('ref_axis',(-0.998774211147154,0.,-0.0494982337804088));
#45204=DIRECTION('center_axis',(1.22464679915E-16,1.,0.));
#45205=DIRECTION('ref_axis',(1.,-1.22464679915E-16,0.));
#45206=DIRECTION('center_axis',(-0.797766403966835,9.76982073084798E-17,
0.602966636474875));
#45207=DIRECTION('ref_axis',(0.602966636474875,6.43171104150991E-32,0.797766403966835));
#45208=DIRECTION('center_axis',(-1.,1.22464679915E-16,-6.12323399574E-17));
#45209=DIRECTION('ref_axis',(-6.12323399574E-17,7.49879891332945E-33,1.));
#45210=DIRECTION('',(-1.,0.,0.));
#45211=DIRECTION('',(-1.,0.,-4.09734305096E-16));
#45212=DIRECTION('center_axis',(5.9296278727138E-17,1.,-6.12017248415691E-17));
#45213=DIRECTION('ref_axis',(0.714687205042172,0.,0.699444207173816));
#45214=DIRECTION('center_axis',(-1.22464679915E-16,-1.,-5.47382212627E-48));
#45215=DIRECTION('ref_axis',(1.,-1.22464679915E-16,-6.703498746053E-64));
#45216=DIRECTION('center_axis',(-1.22464679915E-16,-1.,-5.47382212627E-48));
#45217=DIRECTION('ref_axis',(1.,-1.22464679915E-16,-6.703498746053E-64));
#45218=DIRECTION('center_axis',(0.585630202617415,2.24275747059828E-12,
-0.810578352648456));
#45219=DIRECTION('ref_axis',(1.0249208888998E-11,1.,1.01714932772742E-11));
#45220=DIRECTION('center_axis',(-2.68354439599323E-46,-1.,-1.81284143127026E-31));
#45221=DIRECTION('ref_axis',(-1.,0.,1.97372982155583E-15));
#45222=DIRECTION('center_axis',(1.22464679915E-16,1.,5.47382212627E-48));
#45223=DIRECTION('ref_axis',(1.,-1.22464679915E-16,-6.703498746053E-64));
#45224=DIRECTION('center_axis',(-0.991694064582439,1.21447496192053E-16,
-0.128619136492057));
#45225=DIRECTION('ref_axis',(0.128619136492057,-7.10548517584315E-33,-0.991694064582438));
#45226=DIRECTION('center_axis',(1.22464679915E-16,1.,5.47382212627E-48));
#45227=DIRECTION('ref_axis',(1.,-1.22464679915E-16,-6.703498746053E-64));
#45228=DIRECTION('center_axis',(-8.38660245249135E-17,-1.,-5.68956569482564E-17));
#45229=DIRECTION('ref_axis',(0.561410669601872,0.,-0.827537346623811));
#45230=DIRECTION('center_axis',(-1.22464679915E-16,-1.,-5.47382212627E-48));
#45231=DIRECTION('ref_axis',(1.,-1.22464679915E-16,-6.703498746053E-64));
#45232=DIRECTION('center_axis',(-0.827537346623811,1.01344096271977E-16,
-0.561410669601872));
#45233=DIRECTION('ref_axis',(0.561410669601872,-5.47362952277333E-32,-0.827537346623811));
#45234=DIRECTION('center_axis',(-1.22464679915E-16,-1.,-5.47382212627E-48));
#45235=DIRECTION('ref_axis',(1.,-1.22464679915E-16,-6.703498746053E-64));
#45236=DIRECTION('center_axis',(-5.78330237622164E-17,-1.,6.11379105471829E-17));
#45237=DIRECTION('ref_axis',(0.726469216974212,0.,0.687199008140201));
#45238=DIRECTION('center_axis',(1.22464679915E-16,1.,-1.23259516441E-32));
#45239=DIRECTION('ref_axis',(1.,-1.22464679915E-16,1.50949372274247E-48));
#45240=DIRECTION('center_axis',(1.22464679915E-16,1.,5.47382212627E-48));
#45241=DIRECTION('ref_axis',(1.,-1.22464679915E-16,-6.703498746053E-64));
#45242=DIRECTION('center_axis',(-0.687199008140201,8.41576065696246E-17,
0.726469216974212));
#45243=DIRECTION('ref_axis',(0.726469216974212,1.50838013754883E-32,0.687199008140201));
#45244=DIRECTION('center_axis',(-8.38660245249135E-17,-1.,-5.68956569482564E-17));
#45245=DIRECTION('ref_axis',(-0.561410669601872,0.,0.827537346623811));
#45246=DIRECTION('center_axis',(1.22464679915E-16,1.,0.));
#45247=DIRECTION('ref_axis',(1.,-1.22464679915E-16,0.));
#45248=DIRECTION('center_axis',(-0.687199008140201,8.41576065696246E-17,
0.726469216974212));
#45249=DIRECTION('ref_axis',(0.726469216974212,1.50838013754883E-32,0.687199008140201));
#45250=DIRECTION('center_axis',(1.22464679915E-16,1.,5.47382212627E-48));
#45251=DIRECTION('ref_axis',(1.,-1.22464679915E-16,-6.703498746053E-64));
#45252=DIRECTION('center_axis',(1.,0.,0.));
#45253=DIRECTION('ref_axis',(0.,-1.,0.));
#45254=DIRECTION('center_axis',(-1.22464679915E-16,-1.,0.));
#45255=DIRECTION('ref_axis',(1.,-1.22464679915E-16,0.));
#45256=DIRECTION('center_axis',(0.973274002238674,-1.1919168915396E-16,
-0.229646938943923));
#45257=DIRECTION('ref_axis',(0.229646938943923,-2.91124363913666E-32,0.973274002238674));
#45258=DIRECTION('center_axis',(1.22464679914958E-16,1.,1.38940690218481E-28));
#45259=DIRECTION('ref_axis',(0.287097106361984,-3.51592552349981E-17,-0.957901483200948));
#45260=DIRECTION('center_axis',(-1.22464679915E-16,-1.,0.));
#45261=DIRECTION('ref_axis',(1.,-1.22464679915E-16,0.));
#45262=DIRECTION('',(-1.13288063737E-16,-1.,0.));
#45263=DIRECTION('',(-1.21155290386E-16,-1.,0.));
#45264=DIRECTION('center_axis',(0.,0.,1.));
#45265=DIRECTION('ref_axis',(1.,0.,0.));
#45266=DIRECTION('center_axis',(-1.22464679915E-16,-1.,0.));
#45267=DIRECTION('ref_axis',(1.,-1.22464679915E-16,0.));
#45268=DIRECTION('center_axis',(1.16436507708486E-16,1.,2.6493382562289E-17));
#45269=DIRECTION('ref_axis',(0.221864286407976,0.,-0.975077555077892));
#45270=DIRECTION('center_axis',(-1.22464679915E-16,-1.,-5.47382212627E-48));
#45271=DIRECTION('ref_axis',(1.,-1.22464679915E-16,-6.703498746053E-64));
#45272=DIRECTION('center_axis',(1.22464679915E-16,1.,7.60253073092891E-48));
#45273=DIRECTION('ref_axis',(1.,-1.22464679915E-16,-9.3104149250716E-64));
#45274=DIRECTION('',(0.,1.,0.));
#45275=DIRECTION('center_axis',(1.22464679915E-16,1.,0.));
#45276=DIRECTION('ref_axis',(1.,-1.22464679915E-16,0.));
#45277=DIRECTION('',(0.,1.,0.));
#45278=DIRECTION('center_axis',(-1.22464679915E-16,-1.,-8.75811540203E-47));
#45279=DIRECTION('ref_axis',(1.,-1.22464679915E-16,-1.07255979936824E-62));
#45280=DIRECTION('center_axis',(5.9296278727138E-17,1.,-6.12017248415691E-17));
#45281=DIRECTION('ref_axis',(-0.718198537785833,0.,-0.695838242928838));
#45282=DIRECTION('center_axis',(-1.22464679915E-16,-1.,-5.47382212627E-48));
#45283=DIRECTION('ref_axis',(1.,-1.22464679915E-16,-6.703498746053E-64));
#45284=DIRECTION('center_axis',(-1.22464679915E-16,-1.,-5.47382212627E-48));
#45285=DIRECTION('ref_axis',(1.,-1.22464679915E-16,-6.703498746053E-64));
#45286=DIRECTION('center_axis',(1.22464679915E-16,1.,5.47382212627E-48));
#45287=DIRECTION('ref_axis',(1.,-1.22464679915E-16,0.));
#45288=DIRECTION('center_axis',(-1.22464679915E-16,-1.,1.23259516441E-32));
#45289=DIRECTION('ref_axis',(1.,-1.22464679915E-16,-1.1821919162786E-48));
#45290=DIRECTION('center_axis',(1.22464679915E-16,1.,-1.23259516441E-32));
#45291=DIRECTION('ref_axis',(1.,-1.22464679915E-16,1.50949372274247E-48));
#45292=DIRECTION('center_axis',(-2.24037888703029E-16,-1.,-2.20413632410453E-17));
#45293=DIRECTION('ref_axis',(0.977255721664238,-2.19472257881379E-16,0.212064269679052));
#45294=DIRECTION('center_axis',(-1.22464679915E-16,-1.,-5.47382212627E-48));
#45295=DIRECTION('ref_axis',(1.,-1.22464679915E-16,5.24998673990483E-64));
#45296=DIRECTION('center_axis',(0.212064269679051,-2.59703829076063E-17,
-0.977255721664238));
#45297=DIRECTION('ref_axis',(0.977255721664238,-7.13089940857179E-32,0.212064269679051));
#45298=DIRECTION('center_axis',(-0.458332816460024,-1.74027459110009E-14,
-0.888780641866047));
#45299=DIRECTION('ref_axis',(0.888780641866047,-1.15648231731787E-14,-0.458332816460024));
#45300=DIRECTION('center_axis',(-1.17653265936146E-16,-1.,2.37924056871716E-17));
#45301=DIRECTION('ref_axis',(0.198212453337067,0.,0.980159080630334));
#45302=DIRECTION('center_axis',(-1.22464679915E-16,-1.,-5.47382212627E-48));
#45303=DIRECTION('ref_axis',(1.,-1.22464679915E-16,5.63840144221543E-64));
#45304=DIRECTION('center_axis',(0.980159080630334,-5.75630344056195E-15,
-0.198212453337067));
#45305=DIRECTION('ref_axis',(0.198212453337067,2.31296463463575E-14,0.980159080630334));
#45306=DIRECTION('center_axis',(-1.22464679915E-16,-1.,-5.47382212627E-48));
#45307=DIRECTION('ref_axis',(1.,-1.22464679915E-16,5.40238148608971E-64));
#45308=DIRECTION('center_axis',(0.611236780892201,-7.48549167240244E-17,
-0.791447785823259));
#45309=DIRECTION('ref_axis',(0.79144778582326,2.17825094235712E-31,0.611236780892201));
#45310=DIRECTION('center_axis',(-2.77602545911041E-17,-1.,-5.12739598421612E-17));
#45311=DIRECTION('ref_axis',(0.879386330848967,0.,-0.476108896278982));
#45312=DIRECTION('center_axis',(-1.22464679915E-16,-1.,-5.47382212627E-48));
#45313=DIRECTION('ref_axis',(1.,-1.22464679915E-16,5.24998673990483E-64));
#45314=DIRECTION('center_axis',(-0.559052990415089,-2.56753050562791E-11,
-0.829131927927001));
#45315=DIRECTION('ref_axis',(0.829131927927002,1.48029736616685E-14,-0.559052990415088));
#45316=DIRECTION('center_axis',(-5.0552016865731E-17,-1.,6.02936991345387E-17));
#45317=DIRECTION('ref_axis',(-0.766297237624136,0.,-0.642486220560113));
#45318=DIRECTION('center_axis',(-1.22464679915E-16,-1.,-5.47382212627E-48));
#45319=DIRECTION('ref_axis',(1.,-1.22464679915E-16,-6.703498746053E-64));
#45320=DIRECTION('center_axis',(-0.642486220560114,6.96862835096123E-15,
0.766297237624136));
#45321=DIRECTION('ref_axis',(0.766297237624136,1.15648231731787E-14,0.642486220560114));
#45322=DIRECTION('center_axis',(-1.22464679915E-16,-1.,-5.47382212627E-48));
#45323=DIRECTION('ref_axis',(1.,-1.22464679915E-16,-6.703498746053E-64));
#45324=DIRECTION('center_axis',(1.2246467991484E-16,1.,-6.47882833291866E-29));
#45325=DIRECTION('ref_axis',(0.926909189979645,-1.13513637260957E-16,0.375285695878857));
#45326=DIRECTION('center_axis',(-4.11884479880182E-8,-0.99999999999998,
-1.97187671260168E-7));
#45327=DIRECTION('ref_axis',(0.926909250500652,-1.12179643352301E-7,0.375285546399414));
#45328=DIRECTION('',(0.,1.,0.));
#45329=DIRECTION('center_axis',(-5.3135481018E-17,-1.,-1.71234534908E-16));
#45330=DIRECTION('ref_axis',(1.,-5.3135481018E-17,-9.09862937923009E-33));
#45331=DIRECTION('center_axis',(0.103350672077944,-0.961332021496742,-0.255263360132284));
#45332=DIRECTION('ref_axis',(0.843470154480493,-0.0513051793170642,0.534720372789271));
#45333=DIRECTION('center_axis',(-0.375285695878857,4.59592426223824E-17,
0.926909189979645));
#45334=DIRECTION('ref_axis',(0.926909189979645,-3.61589631838611E-32,0.375285695878857));
#45335=DIRECTION('center_axis',(-4.57540623410157E-17,-1.,5.92437539213873E-17));
#45336=DIRECTION('ref_axis',(0.791447868317764,0.,0.611236674075818));
#45337=DIRECTION('center_axis',(1.22464679915E-16,1.,0.));
#45338=DIRECTION('ref_axis',(1.,-1.22464679915E-16,0.));
#45339=DIRECTION('center_axis',(-4.57540783324772E-17,-1.,5.92437580993829E-17));
#45340=DIRECTION('ref_axis',(0.791447785823259,0.,0.611236780892201));
#45341=DIRECTION('center_axis',(-1.22464679915E-16,-1.,-5.47382212627E-48));
#45342=DIRECTION('ref_axis',(1.,-1.22464679915E-16,-6.703498746053E-64));
#45343=DIRECTION('center_axis',(-1.22464679915E-16,-1.,0.));
#45344=DIRECTION('ref_axis',(1.,-1.22464679915E-16,0.));
#45345=DIRECTION('center_axis',(-1.22464679914331E-16,-1.,1.45068233549706E-28));
#45346=DIRECTION('ref_axis',(0.977255721664238,-1.19679309148029E-16,0.212064269679051));
#45347=DIRECTION('',(0.,-1.,0.));
#45348=DIRECTION('center_axis',(-0.522520932310171,-1.21282901894159E-7,
-0.852626457071146));
#45349=DIRECTION('ref_axis',(0.602898361866691,-0.707106350234053,-0.369478246608833));
#45350=DIRECTION('center_axis',(7.05590196885209E-7,0.999999999999712,2.79920545343458E-7));
#45351=DIRECTION('ref_axis',(-0.0522188519509896,-2.42693529929814E-7,0.998635665045497));
#45352=DIRECTION('center_axis',(3.34362886570006E-17,1.,5.45598660992754E-17));
#45353=DIRECTION('ref_axis',(0.852626520482788,0.,-0.52252082883787));
#45354=DIRECTION('center_axis',(-0.496495508439081,-1.68003954310796E-11,
-0.868039290642894));
#45355=DIRECTION('ref_axis',(0.868039290642894,-1.4802973661669E-14,-0.49649550843908));
#45356=DIRECTION('center_axis',(-4.27856758992442E-7,-0.999999999999565,
-8.29299662254113E-7));
#45357=DIRECTION('ref_axis',(0.900769689431461,-7.45562834001725E-7,0.434297094856728));
#45358=DIRECTION('center_axis',(0.707141467397435,0.692946912637,-0.140625464812931));
#45359=DIRECTION('ref_axis',(-0.32401455277391,0.140799773673971,-0.935515896884752));
#45360=DIRECTION('center_axis',(-1.22464679915E-16,-1.,1.23259516441E-32));
#45361=DIRECTION('ref_axis',(1.,-1.22464679915E-16,1.50949372274247E-48));
#45362=DIRECTION('center_axis',(-1.22464679914984E-16,-1.,7.84281471797691E-29));
#45363=DIRECTION('ref_axis',(-0.195045334687923,2.38861644813906E-17,-0.980794227866618));
#45364=DIRECTION('',(0.,1.,0.));
#45365=DIRECTION('center_axis',(1.22464679914868E-16,1.,-1.10437102855485E-28));
#45366=DIRECTION('ref_axis',(0.766297237624135,-9.38443459252164E-17,0.642486220560115));
#45367=DIRECTION('',(0.,-1.,0.));
#45368=DIRECTION('center_axis',(4.21917049212E-17,1.,9.57420673393E-17));
#45369=DIRECTION('ref_axis',(1.,-4.21917049212E-17,-4.03952105372541E-33));
#45370=DIRECTION('center_axis',(-0.258465262671631,0.964605492283562,0.0522680805891321));
#45371=DIRECTION('ref_axis',(-0.945466832487627,-0.263697258719896,0.191196821127928));
#45372=DIRECTION('center_axis',(-2.17357452795E-16,2.66186108837E-32,1.));
#45373=DIRECTION('ref_axis',(1.,5.7857534586223E-48,2.17357452795E-16));
#45374=DIRECTION('center_axis',(1.22464679915E-16,1.,0.));
#45375=DIRECTION('ref_axis',(1.,-1.22464679915E-16,0.));
#45376=DIRECTION('center_axis',(-0.198212453337055,3.33211467677212E-15,
-0.980159080630336));
#45377=DIRECTION('ref_axis',(0.945466832487629,0.263697258719893,-0.191196821127922));
#45378=DIRECTION('center_axis',(2.17357452795E-16,-2.66186108837E-32,-1.));
#45379=DIRECTION('ref_axis',(-1.,-5.7857534586223E-48,-2.17357452795E-16));
#45380=DIRECTION('',(-9.00454292637E-17,0.,1.));
#45381=DIRECTION('center_axis',(2.17357452795E-16,-2.66186108837E-32,-1.));
#45382=DIRECTION('ref_axis',(1.,5.7857534586223E-48,2.17357452795E-16));
#45383=DIRECTION('',(-9.00454292637E-17,0.,1.));
#45384=DIRECTION('center_axis',(-1.22464679914984E-16,-1.,8.09446956404351E-29));
#45385=DIRECTION('ref_axis',(0.198212453337068,-2.42740246530083E-17,0.980159080630333));
#45386=DIRECTION('',(0.,-1.,0.));
#45387=DIRECTION('center_axis',(-1.86287635502571E-7,0.999999999999971,
-1.51799658010565E-7));
#45388=DIRECTION('ref_axis',(0.198212596438356,1.85712364005507E-7,0.980159051691679));
#45389=DIRECTION('',(-1.16865581539E-16,-1.,0.));
#45390=DIRECTION('center_axis',(1.,-1.22464679915E-16,6.12323399574E-17));
#45391=DIRECTION('ref_axis',(-1.22464679915E-16,-1.,-6.67366607695787E-50));
#45392=DIRECTION('',(2.17371312249E-16,0.,-1.));
#45393=DIRECTION('center_axis',(0.987243152768062,-3.98507192708808E-11,
-0.159219839569627));
#45394=DIRECTION('ref_axis',(-0.112585427377888,0.707106786546493,-0.6980863227152));
#45395=DIRECTION('center_axis',(2.17357452795E-16,-2.66186108837E-32,-1.));
#45396=DIRECTION('ref_axis',(1.,5.7857534586223E-48,2.17357452795E-16));
#45397=DIRECTION('center_axis',(-1.38777878078E-16,1.69953884181E-32,1.));
#45398=DIRECTION('ref_axis',(1.,2.35858394177534E-48,1.38777878078E-16));
#45399=DIRECTION('center_axis',(-0.941574524866389,0.336804706456248,-6.18995477252445E-5));
#45400=DIRECTION('ref_axis',(0.257425228288326,0.719541944518793,-0.644974140503957));
#45401=DIRECTION('',(1.29439338185998E-7,0.,0.999999999999992));
#45402=DIRECTION('',(0.,0.,1.));
#45403=DIRECTION('center_axis',(0.734238830876792,-8.99183234042744E-17,
0.678891257295808));
#45404=DIRECTION('ref_axis',(0.678891257295808,1.51038693775819E-31,-0.734238830876792));
#45405=DIRECTION('center_axis',(-0.734238830876792,8.99183234042744E-17,
-0.678891257295808));
#45406=DIRECTION('ref_axis',(0.678891257295808,1.51038693775819E-31,-0.734238830876792));
#45407=DIRECTION('center_axis',(-0.734238830876792,8.99183234042744E-17,
-0.678891257295808));
#45408=DIRECTION('ref_axis',(0.678891257295807,3.46311205996404E-31,-0.734238830876791));
#45409=DIRECTION('',(0.734238830876791,0.,0.678891257295807));
#45410=DIRECTION('center_axis',(1.,0.,0.));
#45411=DIRECTION('ref_axis',(0.,-1.,0.));
#45412=DIRECTION('center_axis',(-0.790681776842983,9.68305907154979E-17,
0.612227349738987));
#45413=DIRECTION('ref_axis',(0.612227349738987,1.22226555802243E-31,0.790681776842983));
#45414=DIRECTION('center_axis',(7.65621835198448E-17,1.,-5.92823359275332E-17));
#45415=DIRECTION('ref_axis',(0.612227349738987,0.,0.790681776842983));
#45416=DIRECTION('center_axis',(-0.991694064582439,1.21447496192053E-16,
0.128619136492057));
#45417=DIRECTION('ref_axis',(0.128619136492057,-4.98879909760123E-32,0.991694064582438));
#45418=DIRECTION('center_axis',(1.22464679915E-16,1.,5.47382212627E-48));
#45419=DIRECTION('ref_axis',(1.,-1.22464679915E-16,-6.703498746053E-64));
#45420=DIRECTION('center_axis',(-1.22464679915E-16,-1.,-5.47382212627E-48));
#45421=DIRECTION('ref_axis',(1.,-1.22464679915E-16,-6.703498746053E-64));
#45422=DIRECTION('center_axis',(0.,0.,1.));
#45423=DIRECTION('ref_axis',(1.,0.,0.));
#45424=DIRECTION('center_axis',(1.22464679915E-16,1.,5.47382212627E-48));
#45425=DIRECTION('ref_axis',(1.,-1.22464679915E-16,-6.703498746053E-64));
#45426=DIRECTION('center_axis',(-2.17357452795E-16,2.66186108837E-32,1.));
#45427=DIRECTION('ref_axis',(1.,5.7857534586223E-48,2.17357452795E-16));
#45428=DIRECTION('center_axis',(2.17357452795E-16,-2.66186108837E-32,-1.));
#45429=DIRECTION('ref_axis',(-1.,-5.7857534586223E-48,-2.17357452795E-16));
#45430=DIRECTION('',(-5.32230154418998E-8,0.,0.999999999999999));
#45431=DIRECTION('center_axis',(-1.20274161001E-14,1.4729336629E-30,1.));
#45432=DIRECTION('ref_axis',(1.,6.81368694281801E-46,1.20274161001E-14));
#45433=DIRECTION('center_axis',(0.,0.,1.));
#45434=DIRECTION('ref_axis',(1.,0.,0.));
#45435=DIRECTION('center_axis',(0.824331881335686,-1.00951539990962E-16,
-0.566106835688784));
#45436=DIRECTION('ref_axis',(0.566106835688784,-1.17683260639136E-31,0.824331881335686));
#45437=DIRECTION('center_axis',(1.,0.,0.));
#45438=DIRECTION('ref_axis',(0.,-1.,0.));
#45439=DIRECTION('center_axis',(1.22464679915E-16,1.,5.47382212627E-48));
#45440=DIRECTION('ref_axis',(1.,-1.22464679915E-16,-6.703498746053E-64));
#45441=DIRECTION('center_axis',(0.99733341416283,-1.22138117333977E-16,
-0.0729798670477863));
#45442=DIRECTION('ref_axis',(0.0729798670477863,2.52018738244318E-32,0.99733341416283));
#45443=DIRECTION('center_axis',(8.32175728849317E-17,1.,-5.71493568625004E-17));
#45444=DIRECTION('ref_axis',(0.566106835688784,0.,0.824331881335686));
#45445=DIRECTION('center_axis',(-1.22464679915E-16,-1.,-5.47382212627E-48));
#45446=DIRECTION('ref_axis',(1.,-1.22464679915E-16,6.49622071350503E-64));
#45447=DIRECTION('center_axis',(1.22464679915E-16,1.,5.47382212627E-48));
#45448=DIRECTION('ref_axis',(1.,-1.22464679915E-16,6.2417319857974E-64));
#45449=DIRECTION('center_axis',(1.22464679915E-16,1.,5.47382212627E-48));
#45450=DIRECTION('ref_axis',(1.,-1.22464679915E-16,0.));
#45451=DIRECTION('center_axis',(0.,0.,1.));
#45452=DIRECTION('ref_axis',(1.,0.,0.));
#45453=DIRECTION('center_axis',(-1.,1.22464679915E-16,-6.12323399574E-17));
#45454=DIRECTION('ref_axis',(1.22464679915E-16,1.,7.49879891332945E-33));
#45455=DIRECTION('center_axis',(-1.,1.22464679915E-16,-6.12323399574E-17));
#45456=DIRECTION('ref_axis',(-6.12323399574E-17,0.,1.));
#45457=DIRECTION('',(-7.55253758248E-17,-1.,0.));
#45458=DIRECTION('',(-2.28870415168E-16,0.,1.));
#45459=DIRECTION('',(1.5105075165E-16,1.,0.));
#45460=DIRECTION('center_axis',(1.22464679914868E-16,1.,-1.27704300324719E-28));
#45461=DIRECTION('ref_axis',(-0.718198537785833,8.79539540451795E-17,-0.695838242928838));
#45462=DIRECTION('',(1.5105075165E-16,1.,0.));
#45463=DIRECTION('',(1.5105075165E-16,1.,0.));
#45464=DIRECTION('center_axis',(1.22464679914988E-16,1.,-5.97423468748921E-29));
#45465=DIRECTION('ref_axis',(-0.191153986297933,2.34096117463918E-17,-0.981560061087659));
#45466=DIRECTION('center_axis',(-1.69719902425E-16,-1.,-3.8940254264E-17));
#45467=DIRECTION('ref_axis',(1.,-1.69719902425E-16,-6.60893615409077E-33));
#45468=DIRECTION('',(1.23358113847E-16,1.,0.));
#45469=DIRECTION('center_axis',(-1.,1.22464679915E-16,-6.12323399574E-17));
#45470=DIRECTION('ref_axis',(-6.12323399574E-17,0.,1.));
#45471=DIRECTION('',(-1.74378361673E-16,0.,1.));
#45472=DIRECTION('',(-1.5105075165E-16,-1.,0.));
#45473=DIRECTION('center_axis',(1.22464679915E-16,1.,3.08148791102006E-33));
#45474=DIRECTION('ref_axis',(-1.,1.22464679915E-16,-5.78241158658936E-15));
#45475=DIRECTION('center_axis',(8.30969430144E-17,1.,4.68996881439E-17));
#45476=DIRECTION('ref_axis',(1.,-8.30969430144E-17,-3.89722071308679E-33));
#45477=DIRECTION('',(-1.75298372309E-16,-1.,0.));
#45478=DIRECTION('center_axis',(1.22464679915001E-16,1.,1.11184889946404E-29));
#45479=DIRECTION('ref_axis',(0.11782622263506,-1.44295506406073E-17,0.993034229651503));
#45480=DIRECTION('center_axis',(1.22464679915E-16,1.,0.));
#45481=DIRECTION('ref_axis',(1.,-1.22464679915E-16,0.));
#45482=DIRECTION('',(0.,1.,0.));
#45483=DIRECTION('center_axis',(1.224646799149E-16,1.,1.07595286226434E-28));
#45484=DIRECTION('ref_axis',(0.678891257295807,-8.31402005216763E-17,-0.734238830876792));
#45485=DIRECTION('',(1.23358113847E-16,1.,0.));
#45486=DIRECTION('center_axis',(-1.224646799149E-16,-1.,-1.07595286226434E-28));
#45487=DIRECTION('ref_axis',(0.678891257295809,-8.31402005216765E-17,-0.73423883087679));
#45488=DIRECTION('',(2.46716227694E-16,1.,0.));
#45489=DIRECTION('center_axis',(0.678891257295808,-8.31402005216764E-17,
-0.734238830876792));
#45490=DIRECTION('ref_axis',(4.92781901212525E-33,-1.,1.13233183843457E-16));
#45491=DIRECTION('center_axis',(1.22464679915001E-16,1.,1.11184889946404E-29));
#45492=DIRECTION('ref_axis',(0.11782622263506,-1.44295506406073E-17,0.993034229651503));
#45493=DIRECTION('',(0.,1.,0.));
#45494=DIRECTION('',(0.,1.,0.));
#45495=DIRECTION('center_axis',(-1.22464679914738E-16,-1.,-8.77635576046461E-30));
#45496=DIRECTION('ref_axis',(-0.999438196720723,1.22395878855966E-16,0.0335155327516906));
#45497=DIRECTION('',(0.,1.,0.));
#45498=DIRECTION('center_axis',(1.22464679914868E-16,1.,-1.27704300324719E-28));
#45499=DIRECTION('ref_axis',(-0.718198537785833,8.79539540451795E-17,-0.695838242928838));
#45500=DIRECTION('',(0.,1.,0.));
#45501=DIRECTION('center_axis',(1.22464679915E-16,1.,1.94567767731298E-44));
#45502=DIRECTION('ref_axis',(-2.38276793969895E-60,-1.94567767731298E-44,
1.));
#45503=DIRECTION('',(0.,1.,0.));
#45504=DIRECTION('center_axis',(-1.22464679915E-16,-1.,5.12446785619646E-33));
#45505=DIRECTION('ref_axis',(-2.89120579329468E-15,3.59195059900423E-31,
1.));
#45506=DIRECTION('',(0.,1.,0.));
#45507=DIRECTION('center_axis',(-2.17357452795E-16,2.66186108837E-32,1.));
#45508=DIRECTION('ref_axis',(1.,2.56447231488414E-65,2.17357452795E-16));
#45509=DIRECTION('center_axis',(1.22464679914868E-16,1.,-1.27704300324719E-28));
#45510=DIRECTION('ref_axis',(0.714687205042302,-8.75239398046679E-17,0.699444207173684));
#45511=DIRECTION('',(0.,1.,0.));
#45512=DIRECTION('',(0.,-1.,0.));
#45513=DIRECTION('center_axis',(1.22464679914919E-16,1.,-1.07732241244701E-28));
#45514=DIRECTION('ref_axis',(-0.602966636474876,7.38421161351848E-17,-0.797766403966835));
#45515=DIRECTION('',(-2.46716227694E-16,-1.,0.));
#45516=DIRECTION('center_axis',(0.678891257295808,-8.31402005216764E-17,
-0.734238830876792));
#45517=DIRECTION('ref_axis',(4.92781901212525E-33,-1.,1.13233183843457E-16));
#45518=DIRECTION('',(0.,-1.,0.));
#45519=DIRECTION('center_axis',(-1.22464679914841E-16,-1.,1.13510031077863E-28));
#45520=DIRECTION('ref_axis',(0.813441648140047,-9.96178710688057E-17,0.581646529321034));
#45521=DIRECTION('center_axis',(1.28693262473E-16,1.,6.09147290561E-17));
#45522=DIRECTION('ref_axis',(1.,-1.28693262473E-16,-7.83931521488836E-33));
#45523=DIRECTION('',(0.,-1.,0.));
#45524=DIRECTION('center_axis',(1.22464679915001E-16,1.,1.11184889946404E-29));
#45525=DIRECTION('ref_axis',(0.11782622263506,-1.44295506406073E-17,0.993034229651503));
#45526=DIRECTION('center_axis',(1.22464679915E-16,1.,0.));
#45527=DIRECTION('ref_axis',(1.,-1.22464679915E-16,0.));
#45528=DIRECTION('',(0.,-1.,0.));
#45529=DIRECTION('center_axis',(1.22464679915E-16,1.,1.94567767731298E-44));
#45530=DIRECTION('ref_axis',(2.38276793969895E-60,1.94567767731298E-44,
-1.));
#45531=DIRECTION('',(0.,1.,0.));
#45532=DIRECTION('center_axis',(-1.50336151828E-16,-1.,-5.4521376634E-17));
#45533=DIRECTION('ref_axis',(1.,-1.50336151828E-16,-8.19653395552059E-33));
#45534=DIRECTION('center_axis',(1.22464679914423E-16,1.,-8.33007499390688E-29));
#45535=DIRECTION('ref_axis',(0.98972556641388,-1.21206424693985E-16,0.142980079684982));
#45536=DIRECTION('center_axis',(-1.64046831707E-17,1.,1.20249303974E-16));
#45537=DIRECTION('ref_axis',(1.,1.64046831707E-17,1.97265173319067E-33));
#45538=DIRECTION('',(0.,-1.,0.));
#45539=DIRECTION('center_axis',(-2.17357452795E-16,2.66186108837E-32,1.));
#45540=DIRECTION('ref_axis',(1.,2.56447231488414E-65,2.17357452795E-16));
#45541=DIRECTION('',(-1.,0.,0.));
#45542=DIRECTION('center_axis',(0.,1.,0.));
#45543=DIRECTION('ref_axis',(0.10172047258397,0.,0.994813020349701));
#45544=DIRECTION('center_axis',(0.581646529321033,-7.12311560368041E-17,
-0.813441648140047));
#45545=DIRECTION('ref_axis',(0.813441648140047,-2.80119922649672E-32,0.581646529321033));
#45546=DIRECTION('center_axis',(1.69872863391202E-17,1.,-4.23293596334453E-17));
#45547=DIRECTION('ref_axis',(0.927897590989264,0.,0.372835165503899));
#45548=DIRECTION('center_axis',(1.22464679915E-16,1.,5.47382212627E-48));
#45549=DIRECTION('ref_axis',(1.,-1.22464679915E-16,-6.703498746053E-64));
#45550=DIRECTION('center_axis',(0.,0.,1.));
#45551=DIRECTION('ref_axis',(1.,0.,0.));
#45552=DIRECTION('center_axis',(1.,-1.22464679915E-16,6.12323399574E-17));
#45553=DIRECTION('ref_axis',(-1.22464679915E-16,-1.,-7.49879891332945E-33));
#45554=DIRECTION('center_axis',(0.,0.,1.));
#45555=DIRECTION('ref_axis',(1.,0.,0.));
#45556=DIRECTION('center_axis',(-1.,1.22464679915E-16,-6.12323399574E-17));
#45557=DIRECTION('ref_axis',(-1.22464679915E-16,-1.,-7.49879891332945E-33));
#45558=DIRECTION('center_axis',(-1.,1.22464679915E-16,-6.12323399574E-17));
#45559=DIRECTION('ref_axis',(1.22464679915E-16,1.,7.49879891332945E-33));
#45560=DIRECTION('',(-1.,0.,-2.89652532403E-16));
#45561=DIRECTION('center_axis',(1.22464679915E-16,1.,5.47382212627E-48));
#45562=DIRECTION('ref_axis',(1.,-1.22464679915E-16,0.));
#45563=DIRECTION('',(-1.74378361673E-16,0.,1.));
#45564=DIRECTION('center_axis',(1.22464679915E-16,1.,0.));
#45565=DIRECTION('ref_axis',(1.,-1.22464679915E-16,0.));
#45566=DIRECTION('center_axis',(0.62218556523187,0.249390626342792,-0.742084522079155));
#45567=DIRECTION('ref_axis',(-0.160230040961959,0.968402971645766,0.191107348055953));
#45568=DIRECTION('center_axis',(0.,1.,0.));
#45569=DIRECTION('ref_axis',(-0.751205410155072,0.,0.660068505349066));
#45570=DIRECTION('center_axis',(-1.22464679915E-16,-1.,-5.47382212627E-48));
#45571=DIRECTION('ref_axis',(1.,-1.22464679915E-16,-6.703498746053E-64));
#45572=DIRECTION('center_axis',(2.17357452795E-16,-2.66186108837E-32,-1.));
#45573=DIRECTION('ref_axis',(1.,5.7857534586223E-48,2.17357452795E-16));
#45574=DIRECTION('center_axis',(-0.991694064582439,1.21447496192053E-16,
-0.128619136492057));
#45575=DIRECTION('ref_axis',(0.128619136492057,-4.98879909760123E-32,-0.991694064582438));
#45576=DIRECTION('center_axis',(1.22464679915E-16,1.,5.47382212627E-48));
#45577=DIRECTION('ref_axis',(1.,-1.22464679915E-16,0.));
#45578=DIRECTION('center_axis',(1.22464679915E-16,1.,5.47382212627E-48));
#45579=DIRECTION('ref_axis',(1.,-1.22464679915E-16,0.));
#45580=DIRECTION('center_axis',(1.22464679915E-16,1.,7.60253073092891E-48));
#45581=DIRECTION('ref_axis',(-1.,1.22464679915E-16,9.3104149250716E-64));
#45582=DIRECTION('',(1.75298372309E-16,1.,0.));
#45583=DIRECTION('center_axis',(-1.22464679915E-16,-1.,-1.94578320706031E-44));
#45584=DIRECTION('ref_axis',(-2.38289717636624E-60,-1.94578320706031E-44,
1.));
#45585=DIRECTION('center_axis',(1.22464679915E-16,1.,-1.23259516441E-32));
#45586=DIRECTION('ref_axis',(1.,-1.22464679915E-16,1.50949372274247E-48));
#45587=DIRECTION('center_axis',(0.,0.,1.));
#45588=DIRECTION('ref_axis',(1.,0.,0.));
#45589=DIRECTION('center_axis',(2.17357452795E-16,-2.66186108837E-32,-1.));
#45590=DIRECTION('ref_axis',(1.,5.7857534586223E-48,2.17357452795E-16));
#45591=DIRECTION('center_axis',(1.69872863391202E-17,1.,-4.23293596334453E-17));
#45592=DIRECTION('ref_axis',(-0.928056183869048,0.,-0.37244022283102));
#45593=DIRECTION('center_axis',(-1.22464679914985E-16,-1.,-5.43497430306078E-29));
#45594=DIRECTION('ref_axis',(0.269603455472075,-3.30169008783092E-17,-0.962971430935268));
#45595=DIRECTION('center_axis',(-4.73893099620284E-8,0.999999999999998,
3.5943940930386E-8));
#45596=DIRECTION('ref_axis',(0.604316184158962,-1.36908907673765E-14,0.796744594938398));
#45597=DIRECTION('center_axis',(-2.17357452795E-16,2.66186108836794E-32,
1.));
#45598=DIRECTION('ref_axis',(5.78575345861782E-48,1.,-2.66186108836794E-32));
#45599=DIRECTION('center_axis',(2.17357452795E-16,-2.66186108837E-32,-1.));
#45600=DIRECTION('ref_axis',(-1.,-5.7857534586223E-48,-2.17357452795E-16));
#45601=DIRECTION('',(0.,0.,1.));
#45602=DIRECTION('center_axis',(0.,1.,0.));
#45603=DIRECTION('ref_axis',(-0.642923934113106,0.,0.765930032669124));
#45604=DIRECTION('center_axis',(9.19369336238712E-17,1.,-5.29776121060009E-17));
#45605=DIRECTION('ref_axis',(0.499277443708891,0.,0.86644217014381));
#45606=DIRECTION('center_axis',(0.,-1.,5.47382212627E-48));
#45607=DIRECTION('ref_axis',(1.,0.,0.));
#45608=DIRECTION('center_axis',(-1.22464679915E-16,-1.,-5.47382212627E-48));
#45609=DIRECTION('ref_axis',(1.,-1.22464679915E-16,-6.703498746053E-64));
#45610=DIRECTION('center_axis',(-1.,1.22464679915E-16,-6.12323399574E-17));
#45611=DIRECTION('ref_axis',(1.22464679915E-16,1.,7.49879891332945E-33));
#45612=DIRECTION('center_axis',(1.,0.,0.));
#45613=DIRECTION('ref_axis',(0.,-1.,0.));
#45614=DIRECTION('center_axis',(-1.22464679915E-16,-1.,0.));
#45615=DIRECTION('ref_axis',(1.,-1.22464679915E-16,0.));
#45616=DIRECTION('center_axis',(-0.827537346623811,1.01344096271977E-16,
-0.561410669601872));
#45617=DIRECTION('ref_axis',(0.561410669601872,-1.40589310424814E-31,-0.827537346623811));
#45618=DIRECTION('center_axis',(-0.687199008140201,8.41576065696246E-17,
0.726469216974212));
#45619=DIRECTION('ref_axis',(0.726469216974212,1.50838013754883E-32,0.687199008140201));
#45620=DIRECTION('center_axis',(-1.22464679914912E-16,-1.,8.35682402091226E-29));
#45621=DIRECTION('ref_axis',(0.726469216974212,-8.89668201247259E-17,0.687199008140201));
#45622=DIRECTION('',(0.,1.,0.));
#45623=DIRECTION('',(0.,1.,0.));
#45624=DIRECTION('center_axis',(1.22464679914998E-16,1.,-1.73663083545565E-29));
#45625=DIRECTION('ref_axis',(0.095298509688002,-1.16707014853003E-17,0.99544874004202));
#45626=DIRECTION('center_axis',(-1.22464679915E-16,-1.,0.));
#45627=DIRECTION('ref_axis',(1.,-1.22464679915E-16,0.));
#45628=DIRECTION('center_axis',(1.68490994230906E-17,1.,-4.21844451941189E-17));
#45629=DIRECTION('ref_axis',(-0.928663912412966,0.,-0.370922279974987));
#45630=DIRECTION('center_axis',(-1.22464679915E-16,-1.,-5.47382212627E-48));
#45631=DIRECTION('ref_axis',(1.,-1.22464679915E-16,-6.703498746053E-64));
#45632=DIRECTION('center_axis',(2.17357452795E-16,-2.66186108837E-32,-1.));
#45633=DIRECTION('ref_axis',(-1.,-5.7857534586223E-48,-2.17357452795E-16));
#45634=DIRECTION('center_axis',(2.74323727954E-15,-3.35949675369E-31,1.));
#45635=DIRECTION('ref_axis',(1.,-4.97099741607164E-47,-2.74323727954E-15));
#45636=DIRECTION('center_axis',(-2.17357452795E-16,5.59737441582E-15,1.));
#45637=DIRECTION('ref_axis',(1.,1.21663104536254E-30,2.17357452795E-16));
#45638=DIRECTION('',(0.,0.,-1.));
#45639=DIRECTION('center_axis',(2.68354439599323E-46,1.,-1.81284143127026E-31));
#45640=DIRECTION('ref_axis',(1.,0.,1.97372982155583E-15));
#45641=DIRECTION('center_axis',(-0.904759192693671,1.1080104493296E-16,
-0.425923471102845));
#45642=DIRECTION('ref_axis',(0.425923471102845,3.65487816993661E-32,-0.904759192693671));
#45643=DIRECTION('center_axis',(1.22464679915E-16,1.,5.47382212627E-48));
#45644=DIRECTION('ref_axis',(1.,-1.22464679915E-16,-6.703498746053E-64));
#45645=DIRECTION('center_axis',(1.0293130162049E-16,1.,4.48396705262131E-17));
#45646=DIRECTION('ref_axis',(0.399377187820903,0.,-0.916786704663777));
#45647=DIRECTION('center_axis',(-0.916786704663777,1.12273990336973E-16,
-0.399377187820903));
#45648=DIRECTION('ref_axis',(0.399377187820903,3.93858763528754E-32,-0.916786704663777));
#45649=DIRECTION('center_axis',(-1.22464679915E-16,-1.,-5.47382212627E-48));
#45650=DIRECTION('ref_axis',(1.,-1.22464679915E-16,-6.703498746053E-64));
#45651=DIRECTION('center_axis',(1.0293130162049E-16,1.,4.48396705262131E-17));
#45652=DIRECTION('ref_axis',(-0.399377187820903,0.,0.916786704663777));
#45653=DIRECTION('center_axis',(2.17357452795E-16,-2.66186108837E-32,-1.));
#45654=DIRECTION('ref_axis',(1.,5.7857534586223E-48,2.17357452795E-16));
#45655=DIRECTION('center_axis',(1.22464679915E-16,1.,5.47382212627E-48));
#45656=DIRECTION('ref_axis',(1.,-1.22464679915E-16,-6.703498746053E-64));
#45657=DIRECTION('center_axis',(2.17357452795E-16,-2.66186108836821E-32,
-1.));
#45658=DIRECTION('ref_axis',(5.78575345861839E-48,1.,-2.66186108836821E-32));
#45659=DIRECTION('center_axis',(8.746404436E-17,5.79129605623E-15,-1.));
#45660=DIRECTION('ref_axis',(1.,-5.06530175163994E-31,8.746404436E-17));
#45661=DIRECTION('',(0.,0.,1.));
#45662=DIRECTION('center_axis',(0.,0.957608642877659,-0.288072364321897));
#45663=DIRECTION('ref_axis',(0.,-0.288072364321899,-0.957608642877659));
#45664=DIRECTION('center_axis',(1.22464679915E-16,1.,5.47382212627E-48));
#45665=DIRECTION('ref_axis',(1.,-1.22464679915E-16,-6.703498746053E-64));
#45666=DIRECTION('center_axis',(-0.890715300400791,1.09081164158974E-16,
-0.454561605980893));
#45667=DIRECTION('ref_axis',(0.454561605980893,-9.65132779741589E-32,-0.890715300400791));
#45668=DIRECTION('center_axis',(-1.,1.2919345348203E-16,-3.88645861503935E-17));
#45669=DIRECTION('ref_axis',(0.,0.288072364321903,0.957608642877657));
#45670=DIRECTION('center_axis',(1.178693242477E-16,1.,2.32734068666895E-17));
#45671=DIRECTION('ref_axis',(0.193710935823942,0.,-0.981058649287703));
#45672=DIRECTION('center_axis',(-1.22464679915E-16,-1.,-5.47382212627E-48));
#45673=DIRECTION('ref_axis',(1.,-1.22464679915E-16,6.22660996643423E-64));
#45674=DIRECTION('center_axis',(-1.22464679915E-16,-1.,-5.47382212627E-48));
#45675=DIRECTION('ref_axis',(1.,-1.22464679915E-16,6.49622071350503E-64));
#45676=DIRECTION('center_axis',(0.684308456885095,0.684308456885093,0.25188066950658));
#45677=DIRECTION('ref_axis',(0.178106529457909,0.178106529457906,-0.967758300573505));
#45678=DIRECTION('center_axis',(0.938446715307966,-1.14926576606996E-16,
0.345424032932987));
#45679=DIRECTION('ref_axis',(0.345424032932987,5.96953449650393E-32,-0.938446715307966));
#45680=DIRECTION('center_axis',(1.178693242477E-16,1.,2.32734068666895E-17));
#45681=DIRECTION('ref_axis',(0.193710935823942,0.,-0.981058649287703));
#45682=DIRECTION('center_axis',(-1.22464679915E-16,-1.,-5.47382212627E-48));
#45683=DIRECTION('ref_axis',(1.,-1.22464679915E-16,6.22660996643423E-64));
#45684=DIRECTION('center_axis',(-1.22464679915E-16,-1.,-5.47382212627E-48));
#45685=DIRECTION('ref_axis',(1.,-1.22464679915E-16,6.49622071350503E-64));
#45686=DIRECTION('center_axis',(-1.22464679915E-16,-1.,-7.60253073092891E-48));
#45687=DIRECTION('ref_axis',(-1.,1.22464679915E-16,9.3104149250716E-64));
#45688=DIRECTION('',(-1.38777878078E-16,-1.,0.));
#45689=DIRECTION('center_axis',(1.22464679914586E-16,1.,-1.3947821589454E-28));
#45690=DIRECTION('ref_axis',(0.947590338356885,-1.16046347476986E-16,0.319487950715961));
#45691=DIRECTION('',(0.,-1.,0.));
#45692=DIRECTION('center_axis',(1.22464679914586E-16,1.,-1.3947821589454E-28));
#45693=DIRECTION('ref_axis',(0.947590338356885,-1.16046347476986E-16,0.319487950715961));
#45694=DIRECTION('',(1.21655932081E-16,1.,0.));
#45695=DIRECTION('center_axis',(-1.22464679914899E-16,-1.,-1.21650294976139E-28));
#45696=DIRECTION('ref_axis',(0.638858327474962,-7.82375805850953E-17,-0.769324403236954));
#45697=DIRECTION('',(0.,-1.,0.));
#45698=DIRECTION('center_axis',(1.83586547022E-16,1.,-3.67652253532E-18));
#45699=DIRECTION('ref_axis',(1.,-1.83586547022E-16,6.74960077307968E-34));
#45700=DIRECTION('center_axis',(0.,1.,0.));
#45701=DIRECTION('ref_axis',(0.998195841446114,0.,-0.0600421695118078));
#45702=DIRECTION('center_axis',(0.687199008140201,-8.41576065696246E-17,
-0.726469216974212));
#45703=DIRECTION('ref_axis',(0.726469216974212,1.50838013754883E-32,0.687199008140201));
#45704=DIRECTION('center_axis',(0.687199008140201,-8.41576065697951E-17,
-0.726469216974212));
#45705=DIRECTION('ref_axis',(5.78330237622164E-17,1.,-6.11379105471828E-17));
#45706=DIRECTION('',(0.687199008140201,0.,-0.726469216974212));
#45707=DIRECTION('',(0.687199008140201,0.,-0.726469216974212));
#45708=DIRECTION('center_axis',(-0.726469216974212,8.89668201247259E-17,
-0.687199008140201));
#45709=DIRECTION('ref_axis',(-0.687199008140201,2.45619021304035E-33,0.726469216974212));
#45710=DIRECTION('',(0.687199008140201,0.,-0.726469216974212));
#45711=DIRECTION('center_axis',(0.687199008140201,-8.41576065697951E-17,
-0.726469216974212));
#45712=DIRECTION('ref_axis',(-5.78330237622164E-17,-1.,6.11379105471828E-17));
#45713=DIRECTION('',(0.687199008140201,0.,-0.726469216974212));
#45714=DIRECTION('center_axis',(0.678891827805225,7.76974089072413E-7,-0.734238303372057));
#45715=DIRECTION('ref_axis',(0.519185258240454,-0.707106778553177,0.480048613527778));
#45716=DIRECTION('center_axis',(0.734238830876792,-8.99183234042744E-17,
0.678891257295808));
#45717=DIRECTION('ref_axis',(-0.678891257295808,-1.51038693775819E-31,0.734238830876792));
#45718=DIRECTION('center_axis',(0.734238830876792,-8.99183234042744E-17,
0.678891257295808));
#45719=DIRECTION('ref_axis',(0.678891257295808,1.51038693775819E-31,-0.734238830876792));
#45720=DIRECTION('',(-0.734238830876791,0.,-0.678891257295807));
#45721=DIRECTION('center_axis',(-6.60215246509141E-17,-1.,-6.10447636300053E-17));
#45722=DIRECTION('ref_axis',(0.678891257295808,0.,-0.734238830876791));
#45723=DIRECTION('center_axis',(0.790681776842983,-9.68305907154979E-17,
-0.612227349738987));
#45724=DIRECTION('ref_axis',(0.612227349738987,1.22226555802243E-31,0.790681776842983));
#45725=DIRECTION('center_axis',(1.22464679915E-16,1.,5.47382212627E-48));
#45726=DIRECTION('ref_axis',(1.,-1.22464679915E-16,-6.703498746053E-64));
#45727=DIRECTION('center_axis',(-1.20438761132693E-16,-1.,1.56204720894266E-17));
#45728=DIRECTION('ref_axis',(0.128619136492057,0.,0.991694064582438));
#45729=DIRECTION('center_axis',(0.991694064582439,-1.21447496192053E-16,
-0.128619136492057));
#45730=DIRECTION('ref_axis',(0.128619136492057,-7.10548517584315E-33,0.991694064582438));
#45731=DIRECTION('center_axis',(-1.22464679915E-16,-1.,-5.47382212627E-48));
#45732=DIRECTION('ref_axis',(1.,-1.22464679915E-16,-6.703498746053E-64));
#45733=DIRECTION('center_axis',(-1.20438761132693E-16,-1.,1.56204720894266E-17));
#45734=DIRECTION('ref_axis',(-0.128619136492057,0.,-0.991694064582438));
#45735=DIRECTION('center_axis',(2.17357452795E-16,-2.66186108837E-32,-1.));
#45736=DIRECTION('ref_axis',(1.,5.7857534586223E-48,2.17357452795E-16));
#45737=DIRECTION('center_axis',(1.22464679915E-16,1.,5.47382212627E-48));
#45738=DIRECTION('ref_axis',(1.,-1.22464679915E-16,-6.703498746053E-64));
#45739=DIRECTION('center_axis',(2.17357452795E-16,-2.66186108837E-32,-1.));
#45740=DIRECTION('ref_axis',(1.,5.7857534586223E-48,2.17357452795E-16));
#45741=DIRECTION('center_axis',(6.13854691746E-15,-7.51755183389E-31,-1.));
#45742=DIRECTION('ref_axis',(1.,2.67726580969963E-46,6.13854691746E-15));
#45743=DIRECTION('',(-5.89048887673E-17,0.,1.));
#45744=DIRECTION('center_axis',(-0.734238830876792,8.99183234042744E-17,
-0.678891257295808));
#45745=DIRECTION('ref_axis',(0.678891257295807,3.46311205996404E-31,-0.734238830876791));
#45746=DIRECTION('center_axis',(-8.32175728849317E-17,-1.,5.71493568625004E-17));
#45747=DIRECTION('ref_axis',(0.566106835688784,0.,0.824331881335687));
#45748=DIRECTION('center_axis',(1.22464679915E-16,1.,5.47382212627E-48));
#45749=DIRECTION('ref_axis',(1.,-1.22464679915E-16,-6.703498746053E-64));
#45750=DIRECTION('center_axis',(-0.824331881335686,1.00951539990962E-16,
0.566106835688784));
#45751=DIRECTION('ref_axis',(0.566106835688784,-1.17683260639136E-31,0.824331881335686));
#45752=DIRECTION('center_axis',(-1.07341775839004E-43,-1.,-3.62568286252829E-30));
#45753=DIRECTION('ref_axis',(-1.,0.,2.96059473233375E-14));
#45754=DIRECTION('center_axis',(-0.99733341416283,1.22138117333977E-16,
0.0729798670477863));
#45755=DIRECTION('ref_axis',(0.0729798670477863,-2.55070953490458E-32,0.99733341416283));
#45756=DIRECTION('center_axis',(1.22464679915E-16,1.,5.47382212627E-48));
#45757=DIRECTION('ref_axis',(1.,-1.22464679915E-16,-6.703498746053E-64));
#45758=DIRECTION('center_axis',(-1.21812425560124E-16,-1.,8.91362356450131E-18));
#45759=DIRECTION('ref_axis',(0.0729798670477876,0.,0.99733341416283));
#45760=DIRECTION('center_axis',(1.22464679915E-16,1.,5.47382212627E-48));
#45761=DIRECTION('ref_axis',(1.,-1.22464679915E-16,5.9677926224237E-64));
#45762=DIRECTION('center_axis',(-7.91623497736024E-17,-1.,5.85483919904324E-17));
#45763=DIRECTION('ref_axis',(-0.594634643326775,0.,-0.803996045360696));
#45764=DIRECTION('center_axis',(0.803996045360697,-9.84611183477626E-17,
-0.594634643326775));
#45765=DIRECTION('ref_axis',(0.594634643326775,4.97302608069436E-32,0.803996045360697));
#45766=DIRECTION('center_axis',(1.22464679915E-16,1.,5.47382212627E-48));
#45767=DIRECTION('ref_axis',(1.,-1.22464679915E-16,-6.703498746053E-64));
#45768=DIRECTION('center_axis',(-7.91623497736024E-17,-1.,5.85483919904324E-17));
#45769=DIRECTION('ref_axis',(0.594634643326775,0.,0.803996045360696));
#45770=DIRECTION('center_axis',(0.766648875028861,7.59597220210557E-12,
-0.642066587214272));
#45771=DIRECTION('ref_axis',(0.642066587214271,0.,0.766648875028862));
#45772=DIRECTION('center_axis',(-1.22464679915E-16,-1.,-5.47382212627E-48));
#45773=DIRECTION('ref_axis',(1.,-1.22464679915E-16,-6.703498746053E-64));
#45774=DIRECTION('center_axis',(-0.988161317760145,0.0726194459501342,0.135142984103609));
#45775=DIRECTION('ref_axis',(0.140217557783907,0.0700183990770855,0.987641868431973));
#45776=DIRECTION('center_axis',(-0.198845167758325,-4.16446674120852E-11,
0.980030917501669));
#45777=DIRECTION('ref_axis',(0.692986511637353,0.707106776997594,0.1406047673899));
#45778=DIRECTION('center_axis',(-0.204326613183897,-0.267662308375891,0.941598387753339));
#45779=DIRECTION('ref_axis',(-0.591797156233802,-0.732434393923313,-0.336624396726937));
#45780=DIRECTION('center_axis',(0.734238830876792,-8.991832340449E-17,0.678891257295808));
#45781=DIRECTION('ref_axis',(6.6021524650914E-17,1.,6.10447636300053E-17));
#45782=DIRECTION('center_axis',(-0.734238830865093,1.72051620514813E-11,
-0.67889125730846));
#45783=DIRECTION('ref_axis',(-5.25579579857545E-11,1.,8.21898105129997E-11));
#45784=DIRECTION('',(0.734238830876791,0.,0.678891257295807));
#45785=DIRECTION('center_axis',(0.911344477115603,-2.366403068759E-7,0.411644560307595));
#45786=DIRECTION('ref_axis',(0.291076810513629,0.707106786078308,-0.644417786426801));
#45787=DIRECTION('center_axis',(2.17357452795E-16,-2.66186108837E-32,-1.));
#45788=DIRECTION('ref_axis',(-1.,-5.7857534586223E-48,-2.17357452795E-16));
#45789=DIRECTION('',(0.,0.,-1.));
#45790=DIRECTION('center_axis',(-0.815922385281966,-1.22989217005322E-6,
0.578161449073072));
#45791=DIRECTION('ref_axis',(-0.408798373511725,-0.707146211104366,-0.576912580842979));
#45792=DIRECTION('center_axis',(0.734238830876792,-8.99183234042744E-17,
0.678891257295808));
#45793=DIRECTION('ref_axis',(0.678891257295808,1.51038693775819E-31,-0.734238830876792));
#45794=DIRECTION('',(0.734238830876791,0.,0.678891257295807));
#45795=DIRECTION('center_axis',(-2.19931778314037E-16,-1.,-1.97757654230408E-17));
#45796=DIRECTION('ref_axis',(0.980030917502135,-2.19472257881379E-16,0.198845167756028));
#45797=DIRECTION('center_axis',(1.22464679915E-16,1.,5.47382212627E-48));
#45798=DIRECTION('ref_axis',(1.,-1.22464679915E-16,5.24998673990483E-64));
#45799=DIRECTION('center_axis',(-5.46401789901627E-17,-1.,6.08764557973899E-17));
#45800=DIRECTION('ref_axis',(0.744196935834912,0.,0.667960268798922));
#45801=DIRECTION('center_axis',(1.22464679915E-16,1.,-6.16297582204E-33));
#45802=DIRECTION('ref_axis',(1.,-1.22464679915E-16,7.54746861370013E-49));
#45803=DIRECTION('center_axis',(-1.24015983872461E-7,0.999999999999986,
1.11611400503811E-7));
#45804=DIRECTION('ref_axis',(0.721583920149089,1.6675952356328E-7,-0.692326979239033));
#45805=DIRECTION('center_axis',(-0.884316205578325,0.0178356349302338,0.466547681033985));
#45806=DIRECTION('ref_axis',(-0.0157873708942533,-0.999840932052135,0.00829876577361474));
#45807=DIRECTION('center_axis',(-1.14444500362894E-17,-1.,3.5644992269101E-17));
#45808=DIRECTION('ref_axis',(0.952128653909774,0.,0.305697606146927));
#45809=DIRECTION('center_axis',(1.22464679915E-16,1.,5.47382212627E-48));
#45810=DIRECTION('ref_axis',(1.,-1.22464679915E-16,6.22660996643423E-64));
#45811=DIRECTION('center_axis',(0.110668766458005,-1.35530150608006E-17,
0.993857345966041));
#45812=DIRECTION('ref_axis',(0.993857345966041,-5.87811925404552E-33,-0.110668766458005));
#45813=DIRECTION('center_axis',(1.22464679915E-16,1.,5.47382212627E-48));
#45814=DIRECTION('ref_axis',(1.,-1.22464679915E-16,5.9677926224237E-64));
#45815=DIRECTION('center_axis',(-1.49989545857296E-18,-1.,-1.34697635782315E-17));
#45816=DIRECTION('ref_axis',(0.993857345966041,0.,-0.110668766458005));
#45817=DIRECTION('center_axis',(1.22464679915E-16,1.,1.54074395551E-33));
#45818=DIRECTION('ref_axis',(1.,-1.22464679915E-16,-1.88686715342503E-49));
#45819=DIRECTION('center_axis',(1.,-1.22464679915E-16,6.12323399574E-17));
#45820=DIRECTION('ref_axis',(1.22464679915E-16,1.,7.49879891332945E-33));
#45821=DIRECTION('center_axis',(1.22464679915E-16,1.,5.47382212627E-48));
#45822=DIRECTION('ref_axis',(1.,-1.22464679915E-16,-6.703498746053E-64));
#45823=DIRECTION('center_axis',(1.,-1.22464679915E-16,6.12323399574E-17));
#45824=DIRECTION('ref_axis',(-6.12323399574E-17,7.49879891332945E-33,1.));
#45825=DIRECTION('',(-1.,0.,-1.32512071049E-16));
#45826=DIRECTION('center_axis',(1.,-1.22464679915E-16,6.12323399574E-17));
#45827=DIRECTION('ref_axis',(-1.22464679915E-16,-1.,-7.49879891332945E-33));
#45828=DIRECTION('',(-1.,0.,-1.32512071049E-16));
#45829=DIRECTION('center_axis',(-1.22464679915E-16,-1.,1.81284143127026E-30));
#45830=DIRECTION('ref_axis',(-1.57898385724467E-14,0.,-1.));
#45831=DIRECTION('center_axis',(1.22464679915E-16,1.,5.47382212627E-48));
#45832=DIRECTION('ref_axis',(1.,-1.22464679915E-16,-6.703498746053E-64));
#45833=DIRECTION('center_axis',(0.106117864373042,-1.29956902936052E-17,
-0.994353558278395));
#45834=DIRECTION('ref_axis',(0.994353558278395,1.45479619498441E-32,0.106117864373042));
#45835=DIRECTION('center_axis',(1.22464679915E-16,1.,5.47382212627E-48));
#45836=DIRECTION('ref_axis',(1.,-1.22464679915E-16,-6.703498746053E-64));
#45837=DIRECTION('center_axis',(-4.52327322274045E-17,-1.,5.91050929206098E-17));
#45838=DIRECTION('ref_axis',(0.794132678900969,0.,0.607744426795977));
#45839=DIRECTION('center_axis',(-1.22464679915E-16,-1.,-5.47382212627E-48));
#45840=DIRECTION('ref_axis',(1.,-1.22464679915E-16,-6.703498746053E-64));
#45841=DIRECTION('center_axis',(0.607744426795977,-7.44272266974971E-17,
-0.794132678900969));
#45842=DIRECTION('ref_axis',(0.794132678900969,-2.10244190700647E-31,0.607744426795977));
#45843=DIRECTION('center_axis',(-1.22464679915E-16,-1.,-5.47382212627E-48));
#45844=DIRECTION('ref_axis',(1.,-1.22464679915E-16,-6.703498746053E-64));
#45845=DIRECTION('center_axis',(-4.52327322274045E-17,-1.,5.91050929206098E-17));
#45846=DIRECTION('ref_axis',(-0.794132678900969,0.,-0.607744426795977));
#45847=DIRECTION('center_axis',(1.22464679915E-16,1.,1.23259516441E-32));
#45848=DIRECTION('ref_axis',(1.,-1.22464679915E-16,-1.50949372274247E-48));
#45849=DIRECTION('center_axis',(-0.734238830876792,8.99183234042744E-17,
-0.678891257295808));
#45850=DIRECTION('ref_axis',(0.678891257295808,1.51038693775819E-31,-0.734238830876792));
#45851=DIRECTION('center_axis',(1.22464679915E-16,1.,5.47382212627E-48));
#45852=DIRECTION('ref_axis',(1.,-1.22464679915E-16,-6.703498746053E-64));
#45853=DIRECTION('center_axis',(0.757497881302333,0.120607621490521,-0.641600156998793));
#45854=DIRECTION('ref_axis',(0.519185231994408,-0.707106824013922,0.480048574950346));
#45855=DIRECTION('center_axis',(-0.540714503083014,-0.0890998529400356,
-0.836474173158833));
#45856=DIRECTION('ref_axis',(0.803860483463198,-0.347724019666725,-0.482593337369186));
#45857=DIRECTION('center_axis',(0.734238830876792,-8.991832340449E-17,0.678891257295808));
#45858=DIRECTION('ref_axis',(-6.6021524650914E-17,-1.,-6.10447636300053E-17));
#45859=DIRECTION('',(0.734238830876791,0.,0.678891257295807));
#45860=DIRECTION('',(0.734238830876791,0.,0.678891257295807));
#45861=DIRECTION('center_axis',(1.2246467991486E-16,1.,-1.56475089353662E-28));
#45862=DIRECTION('ref_axis',(0.667272304480808,-8.17172891841765E-17,0.744813850349785));
#45863=DIRECTION('',(0.,1.,0.));
#45864=DIRECTION('center_axis',(1.22464679915E-16,1.,6.16297582204E-33));
#45865=DIRECTION('ref_axis',(1.,-1.22464679915E-16,7.0105395811531E-49));
#45866=DIRECTION('',(0.,-1.,0.));
#45867=DIRECTION('center_axis',(-1.22464679915011E-16,-1.,-3.67313358993533E-30));
#45868=DIRECTION('ref_axis',(0.952128653909774,-1.16602130838972E-16,0.305697606146927));
#45869=DIRECTION('center_axis',(1.22464679915E-16,1.,-6.16297582204E-33));
#45870=DIRECTION('ref_axis',(1.,-1.22464679915E-16,7.54746861370013E-49));
#45871=DIRECTION('',(0.,-1.,0.));
#45872=DIRECTION('center_axis',(1.22464679914586E-16,1.,-1.3947821589454E-28));
#45873=DIRECTION('ref_axis',(0.947590338356885,-1.16046347476986E-16,0.319487950715961));
#45874=DIRECTION('center_axis',(1.22464679915E-16,1.,0.));
#45875=DIRECTION('ref_axis',(1.,-1.22464679915E-16,0.));
#45876=DIRECTION('center_axis',(1.22464679914997E-16,1.,-3.04211334326766E-29));
#45877=DIRECTION('ref_axis',(0.111333411199055,-1.36344105663067E-17,0.993783110920478));
#45878=DIRECTION('center_axis',(-1.75622944019E-17,1.,1.50524498801E-15));
#45879=DIRECTION('ref_axis',(1.,1.75622944019E-17,2.64355556264161E-32));
#45880=DIRECTION('',(-2.77555756156E-16,-1.,0.));
#45881=DIRECTION('center_axis',(1.22464679914586E-16,1.,-1.3947821589454E-28));
#45882=DIRECTION('ref_axis',(0.947590338356885,-1.16046347476986E-16,0.319487950715961));
#45883=DIRECTION('center_axis',(1.22464679915E-16,1.,0.));
#45884=DIRECTION('ref_axis',(1.,-1.22464679915E-16,0.));
#45885=DIRECTION('',(0.,1.,0.));
#45886=DIRECTION('center_axis',(-1.22464679915E-16,-1.,-1.69953884181051E-33));
#45887=DIRECTION('ref_axis',(2.08133480265435E-49,1.69953884181051E-33,
-1.));
#45888=DIRECTION('center_axis',(-2.44959827562E-16,-1.,1.36892417294E-16));
#45889=DIRECTION('ref_axis',(1.,-2.44959827562E-16,3.35331429348836E-32));
#45890=DIRECTION('',(0.,1.,0.));
#45891=DIRECTION('center_axis',(-2.17357452795E-16,2.66186108837E-32,1.));
#45892=DIRECTION('ref_axis',(1.,2.56447231488414E-65,2.17357452795E-16));
#45893=DIRECTION('',(-1.,0.,-1.09790153833E-16));
#45894=DIRECTION('',(0.,1.,0.));
#45895=DIRECTION('center_axis',(1.22464679915E-16,1.,1.94567767731298E-44));
#45896=DIRECTION('ref_axis',(2.38276793969895E-60,1.94567767731298E-44,
-1.));
#45897=DIRECTION('center_axis',(3.43485006637E-19,-1.,1.36611674972E-16));
#45898=DIRECTION('ref_axis',(1.,3.43485006637E-19,-4.69240620844491E-35));
#45899=DIRECTION('',(0.,1.,0.));
#45900=DIRECTION('center_axis',(1.22464679914998E-16,1.,-1.73663083545565E-29));
#45901=DIRECTION('ref_axis',(0.095298509688002,-1.16707014853003E-17,0.99544874004202));
#45902=DIRECTION('center_axis',(-1.22464679915E-16,-1.,0.));
#45903=DIRECTION('ref_axis',(1.,-1.22464679915E-16,0.));
#45904=DIRECTION('',(0.,1.,0.));
#45905=DIRECTION('center_axis',(-1.224646799149E-16,-1.,-1.07603845915075E-28));
#45906=DIRECTION('ref_axis',(-0.678891257295809,8.31402005216765E-17,0.73423883087679));
#45907=DIRECTION('center_axis',(-1.83472486973E-16,-1.,5.23898221099E-18));
#45908=DIRECTION('ref_axis',(1.,-1.83472486973E-16,9.61209095457641E-34));
#45909=DIRECTION('',(0.,1.,0.));
#45910=DIRECTION('center_axis',(0.678891257295808,-8.31402005216764E-17,
-0.734238830876792));
#45911=DIRECTION('ref_axis',(4.92781901212525E-33,-1.,1.13233183843457E-16));
#45912=DIRECTION('',(0.734238830876791,0.,0.678891257295807));
#45913=DIRECTION('',(0.,1.,0.));
#45914=DIRECTION('center_axis',(1.224646799149E-16,1.,1.07603845915075E-28));
#45915=DIRECTION('ref_axis',(-0.67889125729581,8.31402005216767E-17,0.734238830876789));
#45916=DIRECTION('center_axis',(1.22564216467E-16,1.,6.12322590562E-17));
#45917=DIRECTION('ref_axis',(1.,-1.22564216467E-16,-7.50488385372752E-33));
#45918=DIRECTION('center_axis',(0.,1.,0.));
#45919=DIRECTION('ref_axis',(0.00162555525320111,0.,0.999998678784187));
#45920=DIRECTION('center_axis',(0.732027802944257,-8.96475505763315E-17,
-0.68127475787424));
#45921=DIRECTION('ref_axis',(0.68127475787424,-1.91888914560603E-31,0.732027802944257));
#45922=DIRECTION('center_axis',(0.734238830876792,-8.99183234042744E-17,
0.678891257295808));
#45923=DIRECTION('ref_axis',(0.678891257295807,3.46311205996404E-31,-0.734238830876791));
#45924=DIRECTION('center_axis',(5.46401789901627E-17,1.,-6.08764557973899E-17));
#45925=DIRECTION('ref_axis',(0.744196935834912,0.,0.667960268798922));
#45926=DIRECTION('center_axis',(1.22464679915E-16,1.,5.47382212627E-48));
#45927=DIRECTION('ref_axis',(1.,-1.22464679915E-16,6.49622071350503E-64));
#45928=DIRECTION('center_axis',(-0.667960268798921,8.18015405141904E-17,
0.744196935834913));
#45929=DIRECTION('ref_axis',(0.744196935834913,-3.15837441223295E-32,0.667960268798921));
#45930=DIRECTION('center_axis',(1.14444500362894E-17,1.,-3.5644992269101E-17));
#45931=DIRECTION('ref_axis',(0.952128653909774,0.,0.305697606146927));
#45932=DIRECTION('center_axis',(1.22464679915E-16,1.,5.47382212627E-48));
#45933=DIRECTION('ref_axis',(1.,-1.22464679915E-16,-6.703498746053E-64));
#45934=DIRECTION('center_axis',(-0.305697606146928,3.74371594874912E-17,
0.952128653909774));
#45935=DIRECTION('ref_axis',(0.952128653909774,-6.76944606262743E-33,0.305697606146928));
#45936=DIRECTION('center_axis',(0.222411493783323,0.670605060062733,-0.707687770737441));
#45937=DIRECTION('ref_axis',(0.848579081651793,0.224251763465943,0.479191703564883));
#45938=DIRECTION('center_axis',(-0.299820876204079,3.67174676361097E-17,
0.953995514765252));
#45939=DIRECTION('ref_axis',(0.953995514765252,-6.3869078326472E-32,0.299820876204079));
#45940=DIRECTION('center_axis',(0.734238830876792,-8.99183234042744E-17,
0.678891257295808));
#45941=DIRECTION('ref_axis',(0.678891257295807,3.46311205996404E-31,-0.734238830876791));
#45942=DIRECTION('center_axis',(2.41898181523141E-16,1.,1.1741867647411E-17));
#45943=DIRECTION('ref_axis',(-0.99520202856178,2.41886400693281E-16,-0.0978413120645785));
#45944=DIRECTION('center_axis',(1.22464679915E-16,1.,5.47382212627E-48));
#45945=DIRECTION('ref_axis',(1.,-1.22464679915E-16,6.49622071350503E-64));
#45946=DIRECTION('center_axis',(0.962126872935794,0.250387400346799,-0.107786966384449));
#45947=DIRECTION('ref_axis',(-0.248830769651925,0.968145727536702,0.0278764834019926));
#45948=DIRECTION('center_axis',(-0.993783110920478,1.2170333058406E-16,
0.111333411199054));
#45949=DIRECTION('ref_axis',(0.111333411199054,1.57725565511394E-32,0.993783110920478));
#45950=DIRECTION('center_axis',(0.152411459643054,-1.86650206205066E-17,
-0.988317128744349));
#45951=DIRECTION('ref_axis',(0.988317128744349,-1.89428554374595E-32,0.152411459643054));
#45952=DIRECTION('center_axis',(2.41898181523141E-16,1.,1.1741867647411E-17));
#45953=DIRECTION('ref_axis',(0.99977954662694,-2.41886400693281E-16,0.0209966222623895));
#45954=DIRECTION('center_axis',(1.22464679915E-16,1.,5.47382212627E-48));
#45955=DIRECTION('ref_axis',(1.,-1.22464679915E-16,6.49622071350503E-64));
#45956=DIRECTION('center_axis',(0.,0.,1.));
#45957=DIRECTION('ref_axis',(1.,0.,0.));
#45958=DIRECTION('center_axis',(1.,-1.22464679915E-16,6.12323399574E-17));
#45959=DIRECTION('ref_axis',(1.22464679915E-16,1.,7.49879891332945E-33));
#45960=DIRECTION('center_axis',(1.,-1.22464679915E-16,6.12323399574E-17));
#45961=DIRECTION('ref_axis',(6.12323399574E-17,-7.49879891332945E-33,-1.));
#45962=DIRECTION('',(-1.,0.,-2.65024142098E-16));
#45963=DIRECTION('center_axis',(1.,0.,0.));
#45964=DIRECTION('ref_axis',(0.,-1.,0.));
#45965=DIRECTION('center_axis',(0.106117864373042,-1.29956902936052E-17,
-0.994353558278395));
#45966=DIRECTION('ref_axis',(0.994353558278395,-3.91187297993902E-33,0.106117864373042));
#45967=DIRECTION('center_axis',(1.68490994230906E-17,1.,-4.21844451941189E-17));
#45968=DIRECTION('ref_axis',(0.928711112494875,0.,0.37080408510227));
#45969=DIRECTION('center_axis',(-1.22464679915E-16,-1.,-5.47382212627E-48));
#45970=DIRECTION('ref_axis',(1.,-1.22464679915E-16,-6.703498746053E-64));
#45971=DIRECTION('center_axis',(0.,0.,1.));
#45972=DIRECTION('ref_axis',(1.,0.,0.));
#45973=DIRECTION('center_axis',(-0.734238830876792,8.99183234042744E-17,
-0.678891257295808));
#45974=DIRECTION('ref_axis',(0.678891257295808,-2.24691316591619E-32,-0.734238830876792));
#45975=DIRECTION('center_axis',(0.734238830876792,-8.991832340449E-17,0.678891257295808));
#45976=DIRECTION('ref_axis',(6.6021524650914E-17,1.,6.10447636300053E-17));
#45977=DIRECTION('',(0.734238830876791,0.,0.678891257295807));
#45978=DIRECTION('center_axis',(0.734238830876792,-8.99183234042744E-17,
0.678891257295808));
#45979=DIRECTION('ref_axis',(0.678891257295807,3.46311205996404E-31,-0.734238830876791));
#45980=DIRECTION('',(-0.734238830876791,0.,-0.678891257295807));
#45981=DIRECTION('center_axis',(0.734238830876792,-8.99183234042744E-17,
0.678891257295808));
#45982=DIRECTION('ref_axis',(0.678891257295807,3.46311205996404E-31,-0.734238830876791));
#45983=DIRECTION('center_axis',(6.60215246509141E-17,1.,6.10447636300053E-17));
#45984=DIRECTION('ref_axis',(-0.678891257295808,0.,0.734238830876791));
#45985=DIRECTION('center_axis',(-1.22464679915E-16,-1.,-5.47382212627E-48));
#45986=DIRECTION('ref_axis',(1.,-1.22464679915E-16,-6.703498746053E-64));
#45987=DIRECTION('center_axis',(-0.613815420645987,7.51707090161983E-17,
0.789449573675983));
#45988=DIRECTION('ref_axis',(0.789449573675983,7.34020703099417E-32,0.613815420645987));
#45989=DIRECTION('center_axis',(3.85062311351295E-17,1.,-5.68588026119494E-17));
#45990=DIRECTION('ref_axis',(0.827993213361104,0.,0.560738119471071));
#45991=DIRECTION('center_axis',(1.22464679915E-16,1.,5.47382212627E-48));
#45992=DIRECTION('ref_axis',(1.,-1.22464679915E-16,-6.703498746053E-64));
#45993=DIRECTION('center_axis',(-0.560738119471071,6.86706143170087E-17,
0.827993213361104));
#45994=DIRECTION('ref_axis',(0.827993213361104,-2.38131063616686E-32,0.560738119471071));
#45995=DIRECTION('center_axis',(3.85062311351295E-17,1.,-5.68588026119494E-17));
#45996=DIRECTION('ref_axis',(-0.827993213361104,0.,-0.560738119471072));
#45997=DIRECTION('center_axis',(-1.22464679915E-16,-1.,-5.47382212627E-48));
#45998=DIRECTION('ref_axis',(1.,-1.22464679915E-16,-6.703498746053E-64));
#45999=DIRECTION('center_axis',(1.22464679915E-16,1.,5.47382212627E-48));
#46000=DIRECTION('ref_axis',(1.,-1.22464679915E-16,0.));
#46001=DIRECTION('center_axis',(1.224646799149E-16,1.,-1.07595286226434E-28));
#46002=DIRECTION('ref_axis',(0.67889125729581,-8.31402005216767E-17,0.734238830876789));
#46003=DIRECTION('',(0.,-1.,0.));
#46004=DIRECTION('center_axis',(-1.22464679915E-16,-1.,-6.16297582204E-33));
#46005=DIRECTION('ref_axis',(1.,-1.22464679915E-16,-7.54746861370013E-49));
#46006=DIRECTION('',(-2.85587916301E-16,-1.,0.));
#46007=DIRECTION('center_axis',(-1.22464679915E-16,-1.,-1.23259516441E-32));
#46008=DIRECTION('ref_axis',(1.,-1.22464679915E-16,-1.50949372274247E-48));
#46009=DIRECTION('center_axis',(-1.22464679914912E-16,-1.,-1.26181562037188E-28));
#46010=DIRECTION('ref_axis',(-0.572811155566786,7.01491348180737E-17,0.819687367267694));
#46011=DIRECTION('center_axis',(-0.641370372756966,0.046782002687993,0.765803818986358));
#46012=DIRECTION('ref_axis',(0.766534261679224,0.0816131667450425,0.636996480905298));
#46013=DIRECTION('center_axis',(1.22464679915E-16,1.,0.));
#46014=DIRECTION('ref_axis',(1.,-1.22464679915E-16,0.));
#46015=DIRECTION('center_axis',(1.22464679915E-16,1.,-1.23259516441E-32));
#46016=DIRECTION('ref_axis',(1.,-1.22464679915E-16,1.50949372274247E-48));
#46017=DIRECTION('',(0.,-1.,0.));
#46018=DIRECTION('center_axis',(1.22464679914824E-16,1.,2.07777882089137E-28));
#46019=DIRECTION('ref_axis',(0.646318112561793,-7.91511407778746E-17,-0.763068081742751));
#46020=DIRECTION('center_axis',(-1.22464679915E-16,-1.,6.16297582204E-33));
#46021=DIRECTION('ref_axis',(1.,-1.22464679915E-16,7.54746861370013E-49));
#46022=DIRECTION('',(0.,-1.,0.));
#46023=DIRECTION('center_axis',(-1.22464679914844E-16,-1.,-1.36783824494702E-28));
#46024=DIRECTION('ref_axis',(-0.751089446707,9.19819286783E-17,0.660200456713999));
#46025=DIRECTION('',(2.85587916301E-16,1.,0.));
#46026=DIRECTION('center_axis',(1.22464679915E-16,1.,0.));
#46027=DIRECTION('ref_axis',(1.,-1.22464679915E-16,0.));
#46028=DIRECTION('',(2.85587916301E-16,1.,0.));
#46029=DIRECTION('center_axis',(-1.2246467991496E-16,-1.,-1.24243880634581E-29));
#46030=DIRECTION('ref_axis',(-0.953995514765253,1.16830755356031E-16,0.299820876204076));
#46031=DIRECTION('',(0.,1.,0.));
#46032=DIRECTION('center_axis',(1.22464679915E-16,1.,0.));
#46033=DIRECTION('ref_axis',(1.,-1.22464679915E-16,0.));
#46034=DIRECTION('',(0.,1.,0.));
#46035=DIRECTION('center_axis',(-0.678891257295808,8.31402005216763E-17,
-0.734238830876792));
#46036=DIRECTION('ref_axis',(-0.734238830876792,-5.02124004685594E-34,0.678891257295808));
#46037=DIRECTION('',(0.734238830876791,0.,-0.678891257295807));
#46038=DIRECTION('',(-0.734238830876791,0.,0.678891257295807));
#46039=DIRECTION('',(0.,-1.,0.));
#46040=DIRECTION('center_axis',(1.224646799149E-16,1.,-1.07595286226434E-28));
#46041=DIRECTION('ref_axis',(0.67889125729581,-8.31402005216767E-17,0.734238830876789));
#46042=DIRECTION('center_axis',(-1.22464679915E-16,-1.,0.));
#46043=DIRECTION('ref_axis',(1.,-1.22464679915E-16,0.));
#46044=DIRECTION('',(0.,-1.,0.));
#46045=DIRECTION('center_axis',(1.22464679915E-16,1.,-1.23259516441E-32));
#46046=DIRECTION('ref_axis',(1.,-1.22464679915E-16,1.50949372274247E-48));
#46047=DIRECTION('center_axis',(-1.22464679914912E-16,-1.,-1.26181562037188E-28));
#46048=DIRECTION('ref_axis',(-0.572811155566786,7.01491348180737E-17,0.819687367267694));
#46049=DIRECTION('center_axis',(-1.22464679915E-16,-1.,0.));
#46050=DIRECTION('ref_axis',(1.,-1.22464679915E-16,0.));
#46051=DIRECTION('center_axis',(1.22464679915E-16,1.,-1.23259516441E-32));
#46052=DIRECTION('ref_axis',(1.,-1.22464679915E-16,1.50949372274247E-48));
#46053=DIRECTION('',(0.,-1.,0.));
#46054=DIRECTION('center_axis',(-1.224646799149E-16,-1.,1.07603845915075E-28));
#46055=DIRECTION('ref_axis',(-0.67889125729581,8.31402005216767E-17,-0.734238830876789));
#46056=DIRECTION('center_axis',(-1.22464679915E-16,-1.,0.));
#46057=DIRECTION('ref_axis',(1.,-1.22464679915E-16,0.));
#46058=DIRECTION('',(0.,-1.,0.));
#46059=DIRECTION('',(0.,-1.,0.));
#46060=DIRECTION('center_axis',(1.22464679915E-16,1.,-2.46519032882E-32));
#46061=DIRECTION('ref_axis',(1.,-1.22464679915E-16,3.01898744548495E-48));
#46062=DIRECTION('center_axis',(-0.678891257295808,8.31402005216763E-17,
-0.734238830876792));
#46063=DIRECTION('ref_axis',(-0.734238830876792,-5.02124004685594E-34,0.678891257295808));
#46064=DIRECTION('',(-0.734238830876791,0.,0.678891257295807));
#46065=DIRECTION('center_axis',(-0.678891258039564,8.05580512386835E-9,
-0.7342388301891));
#46066=DIRECTION('ref_axis',(-1.90502136153082E-5,-0.999999999663608,1.76032200345041E-5));
#46067=DIRECTION('',(0.734238830876791,0.,-0.678891257295807));
#46068=DIRECTION('',(0.,1.,0.));
#46069=DIRECTION('center_axis',(0.734238830876792,-8.99183234042744E-17,
-0.678891257295808));
#46070=DIRECTION('ref_axis',(0.678891257295807,3.46311205996404E-31,0.734238830876791));
#46071=DIRECTION('',(-0.734238830876791,0.,0.678891257295807));
#46072=DIRECTION('center_axis',(-0.734238830876792,8.99183234042744E-17,
0.678891257295808));
#46073=DIRECTION('ref_axis',(0.678891257295807,3.46311205996404E-31,0.734238830876791));
#46074=DIRECTION('',(-0.734238830876791,0.,0.678891257295807));
#46075=DIRECTION('center_axis',(0.734238830904136,4.02815121124967E-11,
-0.678891257266234));
#46076=DIRECTION('ref_axis',(-4.69698354284746E-11,-1.,-1.10134124042815E-10));
#46077=DIRECTION('center_axis',(0.,0.,1.));
#46078=DIRECTION('ref_axis',(1.,0.,0.));
#46079=DIRECTION('center_axis',(0.803996045360697,-9.84611183477626E-17,
0.594634643326775));
#46080=DIRECTION('ref_axis',(0.594634643326775,4.97302608069436E-32,-0.803996045360697));
#46081=DIRECTION('center_axis',(-7.91623497736024E-17,-1.,-5.85483919904324E-17));
#46082=DIRECTION('ref_axis',(-0.594634643326775,0.,0.803996045360696));
#46083=DIRECTION('center_axis',(0.763068081742753,-9.34488883837698E-17,
0.646318112561791));
#46084=DIRECTION('ref_axis',(0.646318112561791,2.50438493602067E-31,-0.763068081742753));
#46085=DIRECTION('center_axis',(1.22464679915E-16,1.,5.47382212627E-48));
#46086=DIRECTION('ref_axis',(1.,-1.22464679915E-16,-6.703498746053E-64));
#46087=DIRECTION('center_axis',(1.,0.,0.));
#46088=DIRECTION('ref_axis',(0.,-1.,0.));
#46089=DIRECTION('center_axis',(0.734238830876792,-8.99183234042744E-17,
-0.678891257295808));
#46090=DIRECTION('ref_axis',(0.678891257295807,3.46311205996404E-31,0.734238830876791));
#46091=DIRECTION('center_axis',(-0.734238830876792,8.99183234042744E-17,
0.678891257295808));
#46092=DIRECTION('ref_axis',(-0.678891257295807,-3.46311205996404E-31,-0.734238830876791));
#46093=DIRECTION('center_axis',(0.734238830876792,-8.99183234042744E-17,
-0.678891257295808));
#46094=DIRECTION('ref_axis',(0.678891257295807,3.46311205996404E-31,0.734238830876791));
#46095=DIRECTION('',(0.734238830876791,0.,-0.678891257295807));
#46096=DIRECTION('',(0.734238830876791,0.,-0.678891257295807));
#46097=DIRECTION('center_axis',(-6.60215246509141E-17,-1.,6.10447636300053E-17));
#46098=DIRECTION('ref_axis',(0.678891257295808,0.,0.734238830876791));
#46099=DIRECTION('center_axis',(0.732027802944257,-8.96475505763315E-17,
0.68127475787424));
#46100=DIRECTION('ref_axis',(0.68127475787424,-1.91888914560603E-31,-0.732027802944257));
#46101=DIRECTION('center_axis',(1.22464679915E-16,1.,-1.23259516441E-32));
#46102=DIRECTION('ref_axis',(1.,-1.22464679915E-16,1.50949372274247E-48));
#46103=DIRECTION('center_axis',(1.22464679915E-16,1.,5.47382212627E-48));
#46104=DIRECTION('ref_axis',(1.,-1.22464679915E-16,-6.703498746053E-64));
#46105=DIRECTION('center_axis',(-6.56244994878123E-17,-1.,-6.10746133129891E-17));
#46106=DIRECTION('ref_axis',(-0.681274757874239,0.,0.732027802944258));
#46107=DIRECTION('center_axis',(0.660200456714,-8.0851237611E-17,0.751089446706999));
#46108=DIRECTION('ref_axis',(0.751089446706999,6.24086217807948E-32,-0.660200456714));
#46109=DIRECTION('center_axis',(1.22464679915E-16,1.,5.47382212627E-48));
#46110=DIRECTION('ref_axis',(1.,-1.22464679915E-16,6.22660996643423E-64));
#46111=DIRECTION('center_axis',(1.22464679915E-16,1.,5.47382212627E-48));
#46112=DIRECTION('ref_axis',(1.,-1.22464679915E-16,5.9677926224237E-64));
#46113=DIRECTION('center_axis',(-5.33780239968174E-17,-1.,-6.0726511322985E-17));
#46114=DIRECTION('ref_axis',(-0.751089446706998,0.,0.660200456714001));
#46115=DIRECTION('center_axis',(0.315563048033822,-3.86453276703782E-17,
0.948904612021463));
#46116=DIRECTION('ref_axis',(0.948904612021463,7.52823903108453E-32,-0.315563048033822));
#46117=DIRECTION('center_axis',(1.22464679915E-16,1.,5.47382212627E-48));
#46118=DIRECTION('ref_axis',(1.,-1.22464679915E-16,-6.703498746053E-64));
#46119=DIRECTION('center_axis',(-1.21950373919573E-17,-1.,-3.66707296595837E-17));
#46120=DIRECTION('ref_axis',(-0.948904612021463,0.,0.315563048033822));
#46121=DIRECTION('center_axis',(0.299820876204079,-3.67174676361097E-17,
0.953995514765252));
#46122=DIRECTION('ref_axis',(0.953995514765252,-6.3869078326472E-32,-0.299820876204079));
#46123=DIRECTION('center_axis',(1.22464679915E-16,1.,5.47382212627E-48));
#46124=DIRECTION('ref_axis',(1.,-1.22464679915E-16,6.22660996643423E-64));
#46125=DIRECTION('center_axis',(1.22464679915E-16,1.,5.47382212627E-48));
#46126=DIRECTION('ref_axis',(1.,-1.22464679915E-16,5.9677926224237E-64));
#46127=DIRECTION('center_axis',(-1.10086633186706E-17,-1.,-3.5028299438442E-17));
#46128=DIRECTION('ref_axis',(-0.953995514765252,0.,0.299820876204079));
#46129=DIRECTION('center_axis',(-0.734238830876792,8.99183234042744E-17,
0.678891257295808));
#46130=DIRECTION('ref_axis',(0.678891257295807,3.46311205996404E-31,0.734238830876791));
#46131=DIRECTION('center_axis',(1.22464679915E-16,1.,5.47382212627E-48));
#46132=DIRECTION('ref_axis',(1.,-1.22464679915E-16,-6.703498746053E-64));
#46133=DIRECTION('center_axis',(0.734238830876792,-8.99183234042744E-17,
-0.678891257295808));
#46134=DIRECTION('ref_axis',(0.678891257295807,3.46311205996404E-31,0.734238830876791));
#46135=DIRECTION('center_axis',(-0.734238830876792,8.99183234042744E-17,
0.678891257295808));
#46136=DIRECTION('ref_axis',(0.678891257295807,3.46311205996404E-31,0.734238830876791));
#46137=DIRECTION('',(-0.734238830876791,0.,0.678891257295807));
#46138=DIRECTION('center_axis',(0.,0.,1.));
#46139=DIRECTION('ref_axis',(1.,0.,0.));
#46140=DIRECTION('center_axis',(0.613815420645987,-7.51707090161983E-17,
0.789449573675983));
#46141=DIRECTION('ref_axis',(0.789449573675983,7.34020703099417E-32,-0.613815420645987));
#46142=DIRECTION('center_axis',(-4.61409403750984E-17,-1.,-5.93434841858408E-17));
#46143=DIRECTION('ref_axis',(-0.789449573675983,0.,0.613815420645986));
#46144=DIRECTION('center_axis',(0.560738119471071,-6.86706143170087E-17,
0.827993213361104));
#46145=DIRECTION('ref_axis',(0.827993213361104,-2.38131063616686E-32,-0.560738119471071));
#46146=DIRECTION('center_axis',(1.22464679915E-16,1.,5.47382212627E-48));
#46147=DIRECTION('ref_axis',(1.,-1.22464679915E-16,-6.703498746053E-64));
#46148=DIRECTION('center_axis',(1.,0.,0.));
#46149=DIRECTION('ref_axis',(0.,-1.,0.));
#46150=DIRECTION('center_axis',(0.734238830876792,-8.99183234042744E-17,
-0.678891257295808));
#46151=DIRECTION('ref_axis',(0.678891257295807,3.46311205996404E-31,0.734238830876791));
#46152=DIRECTION('center_axis',(0.734238830876792,-8.99183234039869E-17,
-0.678891257295808));
#46153=DIRECTION('ref_axis',(-6.60215246505446E-17,-1.,6.10447636296637E-17));
#46154=DIRECTION('',(0.734238830876791,0.,-0.678891257295807));
#46155=DIRECTION('center_axis',(0.734238830865106,1.72097426658295E-11,
-0.678891257308446));
#46156=DIRECTION('ref_axis',(-0.678891257308445,-1.48029736616684E-14,-0.734238830865107));
#46157=DIRECTION('center_axis',(-1.22464679915E-16,-1.,-5.47382212627E-48));
#46158=DIRECTION('ref_axis',(-1.,1.22464679915E-16,0.));
#46159=DIRECTION('center_axis',(-1.22464679915E-16,-1.,0.));
#46160=DIRECTION('ref_axis',(1.,-1.22464679915E-16,0.));
#46161=DIRECTION('center_axis',(-1.22464679915E-16,-1.,1.23259516441E-32));
#46162=DIRECTION('ref_axis',(1.,-1.22464679915E-16,1.50949372274247E-48));
#46163=DIRECTION('center_axis',(1.,-1.22464679915E-16,6.12323399574E-17));
#46164=DIRECTION('ref_axis',(-1.22464679915E-16,-1.,-6.67366607695787E-50));
#46165=DIRECTION('',(2.5585870064E-16,0.,-1.));
#46166=DIRECTION('',(-1.34875042533E-16,-1.,0.));
#46167=DIRECTION('',(2.21800239814E-16,0.,-1.));
#46168=DIRECTION('',(-1.26882631386E-16,-1.,0.));
#46169=DIRECTION('',(1.75377892382E-16,0.,-1.));
#46170=DIRECTION('',(-1.26882631386E-16,-1.,0.));
#46171=DIRECTION('center_axis',(1.22464679915E-16,1.,7.60253073092891E-48));
#46172=DIRECTION('ref_axis',(-1.,1.22464679915E-16,9.3104149250716E-64));
#46173=DIRECTION('center_axis',(-1.22464679915E-16,-1.,0.));
#46174=DIRECTION('ref_axis',(1.,-1.22464679915E-16,0.));
#46175=DIRECTION('',(-1.42793958151E-16,-1.,0.));
#46176=DIRECTION('center_axis',(-1.22464679915E-16,-1.,0.));
#46177=DIRECTION('ref_axis',(1.,-1.22464679915E-16,0.));
#46178=DIRECTION('center_axis',(-1.22464679914955E-16,-1.,8.72911003161552E-29));
#46179=DIRECTION('ref_axis',(-0.457271150163836,5.59995650390798E-17,-0.889327327381681));
#46180=DIRECTION('center_axis',(1.22464679915E-16,1.,6.16297582204E-33));
#46181=DIRECTION('ref_axis',(1.,-1.22464679915E-16,-7.54746861370012E-49));
#46182=DIRECTION('center_axis',(1.22464679915E-16,1.,0.));
#46183=DIRECTION('ref_axis',(1.,-1.22464679915E-16,0.));
#46184=DIRECTION('',(-1.26882631386E-16,-1.,0.));
#46185=DIRECTION('center_axis',(-1.22464679915E-16,-1.,-6.16297582204006E-33));
#46186=DIRECTION('ref_axis',(1.,-1.22464679915E-16,-2.89120579329468E-15));
#46187=DIRECTION('center_axis',(-1.22464679915E-16,-1.,0.));
#46188=DIRECTION('ref_axis',(1.,-1.22464679915E-16,0.));
#46189=DIRECTION('',(-2.0185873175E-16,-1.,0.));
#46190=DIRECTION('center_axis',(-1.22464679915E-16,-1.,-1.23259516441E-32));
#46191=DIRECTION('ref_axis',(1.,-1.22464679915E-16,-1.50949372274247E-48));
#46192=DIRECTION('center_axis',(1.,-1.22464679915E-16,6.12323399574E-17));
#46193=DIRECTION('ref_axis',(-1.22464679915E-16,-1.,-6.67366607695787E-50));
#46194=DIRECTION('',(-1.75377892382E-16,0.,1.));
#46195=DIRECTION('',(1.26882631386E-16,1.,0.));
#46196=DIRECTION('',(-2.58629566281E-16,0.,1.));
#46197=DIRECTION('center_axis',(1.22464679914969E-16,1.,-8.28235472972929E-29));
#46198=DIRECTION('ref_axis',(-0.345424032932988,4.23022436279984E-17,-0.938446715307966));
#46199=DIRECTION('center_axis',(0.,1.,0.));
#46200=DIRECTION('ref_axis',(-1.,0.,-3.70074341541717E-15));
#46201=DIRECTION('center_axis',(1.22464679915E-16,1.,4.37905770102E-47));
#46202=DIRECTION('ref_axis',(1.,-1.22464679915E-16,-5.3627989968473E-63));
#46203=DIRECTION('',(1.42793958151E-16,1.,0.));
#46204=DIRECTION('center_axis',(-1.22464679915E-16,-1.,0.));
#46205=DIRECTION('ref_axis',(-1.,1.22464679915E-16,0.));
#46206=DIRECTION('',(0.,-1.,0.));
#46207=DIRECTION('center_axis',(-1.22464679915E-16,-1.,-6.16297582204E-33));
#46208=DIRECTION('ref_axis',(1.,-1.22464679915E-16,-7.54746861370013E-49));
#46209=DIRECTION('center_axis',(-1.53814670812197E-6,0.999999999998278,
-1.03837087347816E-6));
#46210=DIRECTION('ref_axis',(-0.999999999998817,-1.53814670630209E-6,1.76525460915653E-12));
#46211=DIRECTION('center_axis',(-2.17357452795E-16,2.66186108837E-32,1.));
#46212=DIRECTION('ref_axis',(-1.,-5.7857534586223E-48,-2.17357452795E-16));
#46213=DIRECTION('center_axis',(2.31296463464E-16,-2.83256473635E-32,-1.));
#46214=DIRECTION('ref_axis',(1.,6.55162206050593E-48,2.31296463464E-16));
#46215=DIRECTION('center_axis',(4.16333634234E-16,-5.09861652543E-32,-1.));
#46216=DIRECTION('ref_axis',(1.,2.1227255475978E-47,4.16333634234E-16));
#46217=DIRECTION('',(2.0973706922E-16,0.,-1.));
#46218=DIRECTION('center_axis',(1.,0.,0.));
#46219=DIRECTION('ref_axis',(0.,-1.,0.));
#46220=DIRECTION('center_axis',(-0.904759192693671,1.1080104493296E-16,
0.425923471102845));
#46221=DIRECTION('ref_axis',(0.425923471102845,3.65487816993661E-32,0.904759192693671));
#46222=DIRECTION('center_axis',(-1.00248263963544E-16,-1.,4.71927656598494E-17));
#46223=DIRECTION('ref_axis',(-0.425923471102846,0.,-0.904759192693671));
#46224=DIRECTION('center_axis',(-0.916786704663777,1.12273990336973E-16,
0.399377187820903));
#46225=DIRECTION('ref_axis',(0.399377187820903,3.93858763528754E-32,0.916786704663777));
#46226=DIRECTION('center_axis',(1.22464679915E-16,1.,5.47382212627E-48));
#46227=DIRECTION('ref_axis',(1.,-1.22464679915E-16,-6.703498746053E-64));
#46228=DIRECTION('center_axis',(0.,0.,1.));
#46229=DIRECTION('ref_axis',(1.,0.,0.));
#46230=DIRECTION('center_axis',(-2.17357452795E-16,2.66186108837E-32,1.));
#46231=DIRECTION('ref_axis',(1.,5.7857534586223E-48,2.17357452795E-16));
#46232=DIRECTION('center_axis',(-2.17357452795E-16,2.66186108835898E-32,
1.));
#46233=DIRECTION('ref_axis',(-5.78575345859834E-48,-1.,2.66186108835898E-32));
#46234=DIRECTION('center_axis',(-2.17357452795E-16,2.66186108837E-32,1.));
#46235=DIRECTION('ref_axis',(1.,5.7857534586223E-48,2.17357452795E-16));
#46236=DIRECTION('',(0.,0.,1.));
#46237=DIRECTION('center_axis',(-1.07341775839004E-45,-1.,-3.62568286252829E-31));
#46238=DIRECTION('ref_axis',(-1.,0.,3.94745964311167E-15));
#46239=DIRECTION('center_axis',(-0.938446715307966,1.14926576606996E-16,
0.345424032932987));
#46240=DIRECTION('ref_axis',(0.345424032932987,5.96953449650393E-32,0.938446715307966));
#46241=DIRECTION('center_axis',(1.22464679915E-16,1.,5.47382212627E-48));
#46242=DIRECTION('ref_axis',(1.,-1.22464679915E-16,-6.703498746053E-64));
#46243=DIRECTION('center_axis',(1.22464679915E-16,1.,3.08148791102E-33));
#46244=DIRECTION('ref_axis',(1.,-1.22464679915E-16,-3.77373430685006E-49));
#46245=DIRECTION('center_axis',(-1.07852468318872E-16,-1.,3.96984015829353E-17));
#46246=DIRECTION('ref_axis',(-0.345424032932988,0.,-0.938446715307966));
#46247=DIRECTION('center_axis',(1.22464679915E-16,1.,5.47382212627E-48));
#46248=DIRECTION('ref_axis',(1.,-1.22464679915E-16,6.22660996643423E-64));
#46249=DIRECTION('center_axis',(1.22464679915E-16,1.,5.47382212627E-48));
#46250=DIRECTION('ref_axis',(1.,-1.22464679915E-16,5.9677926224237E-64));
#46251=DIRECTION('center_axis',(0.,0.,1.));
#46252=DIRECTION('ref_axis',(1.,0.,0.));
#46253=DIRECTION('center_axis',(0.927477365469186,-1.13583218690023E-16,
-0.373879307454075));
#46254=DIRECTION('ref_axis',(0.373879307454075,-5.54912062383212E-32,0.927477365469186));
#46255=DIRECTION('center_axis',(1.22464679915E-16,1.,3.08148791102E-33));
#46256=DIRECTION('ref_axis',(1.,-1.22464679915E-16,-3.77373430685006E-49));
#46257=DIRECTION('center_axis',(-1.0534586443266E-16,-1.,4.2466415142443E-17));
#46258=DIRECTION('ref_axis',(-0.373879307454075,0.,-0.927477365469186));
#46259=DIRECTION('center_axis',(-1.22464679915E-16,-1.,-5.47382212627E-48));
#46260=DIRECTION('ref_axis',(1.,-1.22464679915E-16,5.24998673990483E-64));
#46261=DIRECTION('center_axis',(-1.22464679915E-16,-1.,-5.47382212627E-48));
#46262=DIRECTION('ref_axis',(1.,-1.22464679915E-16,5.02845536814161E-64));
#46263=DIRECTION('center_axis',(-1.22464679915E-16,-1.,-5.47382212627E-48));
#46264=DIRECTION('ref_axis',(-1.,1.22464679915E-16,0.));
#46265=DIRECTION('center_axis',(0.687199008140201,-8.41576065696246E-17,
0.726469216974212));
#46266=DIRECTION('ref_axis',(0.726469216974212,1.50838013754883E-32,-0.687199008140201));
#46267=DIRECTION('center_axis',(0.687199008140272,-9.99737898630458E-14,
0.726469216974145));
#46268=DIRECTION('ref_axis',(-4.37797946043856E-12,1.,4.27898457407615E-12));
#46269=DIRECTION('',(0.687199008140201,0.,0.726469216974212));
#46270=DIRECTION('',(0.687199008140201,0.,0.726469216974212));
#46271=DIRECTION('center_axis',(1.68490994230906E-17,1.,4.21844451941189E-17));
#46272=DIRECTION('ref_axis',(0.928663912412966,0.,-0.370922279974987));
#46273=DIRECTION('center_axis',(1.22464679915E-16,1.,5.47382212627E-48));
#46274=DIRECTION('ref_axis',(1.,-1.22464679915E-16,-6.703498746053E-64));
#46275=DIRECTION('center_axis',(-0.151695779270758,-1.70262634961358E-12,
0.988427230782033));
#46276=DIRECTION('ref_axis',(5.62512999143433E-12,1.,2.58589446152285E-12));
#46277=DIRECTION('center_axis',(1.22464679915E-16,1.,5.47382212627E-48));
#46278=DIRECTION('ref_axis',(1.,-1.22464679915E-16,-6.703498746053E-64));
#46279=DIRECTION('center_axis',(1.,-1.22464679915E-16,6.12323399574E-17));
#46280=DIRECTION('ref_axis',(1.22464679915E-16,1.,7.49879891332945E-33));
#46281=DIRECTION('',(-1.,0.,-2.9545627326E-16));
#46282=DIRECTION('',(-1.,0.,-2.21592204945E-16));
#46283=DIRECTION('center_axis',(2.41898181523141E-16,1.,-1.1741867647411E-17));
#46284=DIRECTION('ref_axis',(0.99520202856178,-2.41886400693281E-16,-0.0978413120645785));
#46285=DIRECTION('center_axis',(-1.22464679915E-16,-1.,-5.47382212627E-48));
#46286=DIRECTION('ref_axis',(1.,-1.22464679915E-16,6.49622071350503E-64));
#46287=DIRECTION('center_axis',(-0.256628500559793,-5.7981162678719E-12,
0.966510120330063));
#46288=DIRECTION('ref_axis',(-0.966510120330063,0.,-0.256628500559793));
#46289=DIRECTION('center_axis',(-1.22464679915E-16,-1.,-5.47382212627E-48));
#46290=DIRECTION('ref_axis',(1.,-1.22464679915E-16,6.22660996643423E-64));
#46291=DIRECTION('center_axis',(0.,1.,0.));
#46292=DIRECTION('ref_axis',(-0.0129687405446048,0.,-0.999915902348136));
#46293=DIRECTION('center_axis',(-1.22464679915E-16,-1.,1.23259516441E-32));
#46294=DIRECTION('ref_axis',(1.,-1.22464679915E-16,1.50949372274247E-48));
#46295=DIRECTION('center_axis',(-0.726469216974212,8.89668201247259E-17,
0.687199008140201));
#46296=DIRECTION('ref_axis',(1.22464679914833E-16,1.,-2.7960247294612E-34));
#46297=DIRECTION('',(0.,1.,0.));
#46298=DIRECTION('',(0.,-1.,0.));
#46299=DIRECTION('',(0.687199008140201,0.,0.726469216974212));
#46300=DIRECTION('center_axis',(0.,0.,1.));
#46301=DIRECTION('ref_axis',(1.,0.,0.));
#46302=DIRECTION('center_axis',(1.22464679915E-16,1.,-1.23259516441E-32));
#46303=DIRECTION('ref_axis',(1.,-1.22464679915E-16,1.50949372274247E-48));
#46304=DIRECTION('center_axis',(-1.22464679914998E-16,-1.,-1.73663083545565E-29));
#46305=DIRECTION('ref_axis',(-0.095298509688002,1.16707014853003E-17,0.99544874004202));
#46306=DIRECTION('',(0.,1.,0.));
#46307=DIRECTION('',(0.,1.,0.));
#46308=DIRECTION('center_axis',(1.22464679915E-16,1.,-6.16297582204E-33));
#46309=DIRECTION('ref_axis',(1.,-1.22464679915E-16,7.54746861370013E-49));
#46310=DIRECTION('center_axis',(0.,0.,1.));
#46311=DIRECTION('ref_axis',(1.,0.,0.));
#46312=DIRECTION('center_axis',(1.22464679915E-16,1.,3.08148791102E-33));
#46313=DIRECTION('ref_axis',(1.,-1.22464679915E-16,-3.77373430685006E-49));
#46314=DIRECTION('center_axis',(-2.17357452795E-16,2.66186108837E-32,1.));
#46315=DIRECTION('ref_axis',(1.,2.56447231488414E-65,2.17357452795E-16));
#46316=DIRECTION('',(-1.,0.,-4.75520106567E-17));
#46317=DIRECTION('',(0.,-1.,0.));
#46318=DIRECTION('',(0.,1.,0.));
#46319=DIRECTION('center_axis',(0.,1.,0.));
#46320=DIRECTION('ref_axis',(-0.79266275948672,0.,0.609660356036784));
#46321=DIRECTION('center_axis',(-1.22464679915E-16,-1.,0.));
#46322=DIRECTION('ref_axis',(1.,-1.22464679915E-16,0.));
#46323=DIRECTION('center_axis',(-1.22464679914586E-16,-1.,-1.3947821589454E-28));
#46324=DIRECTION('ref_axis',(-0.947590338356885,1.16046347476986E-16,0.319487950715961));
#46325=DIRECTION('center_axis',(-1.22464679915E-16,-1.,0.));
#46326=DIRECTION('ref_axis',(1.,-1.22464679915E-16,0.));
#46327=DIRECTION('',(0.,-1.,0.));
#46328=DIRECTION('',(0.,-1.,0.));
#46329=DIRECTION('center_axis',(-1.22464679914811E-16,-1.,1.69678707944837E-28));
#46330=DIRECTION('ref_axis',(-0.744047562132924,9.11195465378906E-17,-0.668126653624934));
#46331=DIRECTION('center_axis',(-1.22464679915E-16,-1.,0.));
#46332=DIRECTION('ref_axis',(1.,-1.22464679915E-16,0.));
#46333=DIRECTION('center_axis',(0.687199008140201,-8.41576065696246E-17,
0.726469216974212));
#46334=DIRECTION('ref_axis',(-0.726469216974212,-1.50838013754883E-32,0.687199008140201));
#46335=DIRECTION('center_axis',(0.687199008140201,-8.41576065696246E-17,
0.726469216974212));
#46336=DIRECTION('ref_axis',(0.726469216974212,1.50838013754883E-32,-0.687199008140201));
#46337=DIRECTION('',(0.687199008140201,0.,0.726469216974212));
#46338=DIRECTION('center_axis',(0.687199008140201,-8.41576065696246E-17,
0.726469216974212));
#46339=DIRECTION('ref_axis',(0.726469216974212,1.50838013754883E-32,-0.687199008140201));
#46340=DIRECTION('center_axis',(-1.22464679914912E-16,-1.,-8.35596805204809E-29));
#46341=DIRECTION('ref_axis',(0.726469216974212,-8.89668201247259E-17,-0.687199008140201));
#46342=DIRECTION('center_axis',(-1.22464679915E-16,-1.,0.));
#46343=DIRECTION('ref_axis',(1.,-1.22464679915E-16,0.));
#46344=DIRECTION('center_axis',(-2.81810938552877E-18,-1.,1.83623833789471E-17));
#46345=DIRECTION('ref_axis',(-0.988427230781696,0.,-0.151695779272953));
#46346=DIRECTION('center_axis',(-0.656401557320037,8.03860066128046E-17,
0.754411688369043));
#46347=DIRECTION('ref_axis',(0.754411688369043,7.40115717670054E-32,0.656401557320037));
#46348=DIRECTION('center_axis',(1.22464679915E-16,1.,5.47382212627E-48));
#46349=DIRECTION('ref_axis',(1.,-1.22464679915E-16,-6.703498746053E-64));
#46350=DIRECTION('center_axis',(-0.151695779272953,1.85773750529943E-17,
0.988427230781696));
#46351=DIRECTION('ref_axis',(0.988427230781695,3.4608594993322E-33,0.151695779272953));
#46352=DIRECTION('center_axis',(1.22464679915E-16,1.,4.31748667364107E-33));
#46353=DIRECTION('ref_axis',(-5.28739623524732E-49,-4.31748667364107E-33,
1.));
#46354=DIRECTION('center_axis',(-1.22464679915E-16,-1.,-3.08148791102E-33));
#46355=DIRECTION('ref_axis',(1.,-1.22464679915E-16,-3.77373430685006E-49));
#46356=DIRECTION('center_axis',(1.,-1.22464679915E-16,6.12323399574E-17));
#46357=DIRECTION('ref_axis',(-1.22464679915E-16,-1.,-7.49879891332945E-33));
#46358=DIRECTION('center_axis',(-1.,1.22464679915E-16,-6.16173778667E-15));
#46359=DIRECTION('ref_axis',(1.22464679915E-16,1.,7.54595245764702E-31));
#46360=DIRECTION('',(-1.,0.,-1.4772813663E-16));
#46361=DIRECTION('center_axis',(-1.,1.22464679915E-16,-5.92731269866E-14));
#46362=DIRECTION('ref_axis',(1.22464679915E-16,1.,7.25886452397512E-30));
#46363=DIRECTION('center_axis',(1.22464679914936E-16,1.,-1.70680191515918E-29));
#46364=DIRECTION('ref_axis',(-0.966510120331627,1.18363352520954E-16,-0.2566285005539));
#46365=DIRECTION('center_axis',(-1.22464679915E-16,-1.,7.00649232162E-46));
#46366=DIRECTION('ref_axis',(1.,-1.22464679915E-16,8.58047839494098E-62));
#46367=DIRECTION('center_axis',(-8.06530182705333E-18,-1.,3.03754096780024E-17));
#46368=DIRECTION('ref_axis',(-0.966510120331627,0.,-0.256628500553901));
#46369=DIRECTION('center_axis',(0.256628500553901,-3.14279271772879E-17,
-0.966510120331627));
#46370=DIRECTION('ref_axis',(0.966510120331627,1.90417037848503E-32,0.256628500553901));
#46371=DIRECTION('center_axis',(-1.22464679915E-16,-1.,-5.47382212627E-48));
#46372=DIRECTION('ref_axis',(1.,-1.22464679915E-16,5.9677926224237E-64));
#46373=DIRECTION('center_axis',(0.668126653624933,-8.18219167786918E-17,
-0.744047562132925));
#46374=DIRECTION('ref_axis',(0.744047562132925,-1.50412683502806E-31,0.668126653624933));
#46375=DIRECTION('center_axis',(-5.46674034506358E-17,-1.,6.0879397708352E-17));
#46376=DIRECTION('ref_axis',(-0.744047562132925,0.,-0.668126653624934));
#46377=DIRECTION('center_axis',(-1.22464679915E-16,-1.,-5.47382212627E-48));
#46378=DIRECTION('ref_axis',(1.,-1.22464679915E-16,-6.703498746053E-64));
#46379=DIRECTION('center_axis',(0.,1.,0.));
#46380=DIRECTION('ref_axis',(-0.997344825668515,0.,0.0728237510173635));
#46381=DIRECTION('center_axis',(0.734238830876792,-8.99183234042744E-17,
-0.678891257295808));
#46382=DIRECTION('ref_axis',(0.678891257295808,1.51038693775819E-31,0.734238830876792));
#46383=DIRECTION('center_axis',(-0.825067330468845,1.01041606533981E-16,
-0.565034423900893));
#46384=DIRECTION('ref_axis',(0.565034423900893,7.24547600115018E-32,-0.825067330468845));
#46385=DIRECTION('center_axis',(1.22464679915E-16,1.,-1.23259516441E-32));
#46386=DIRECTION('ref_axis',(1.,-1.22464679915E-16,1.50949372274247E-48));
#46387=DIRECTION('center_axis',(-5.78330237622164E-17,-1.,-6.11379105471829E-17));
#46388=DIRECTION('ref_axis',(0.726469216974212,0.,-0.687199008140201));
#46389=DIRECTION('center_axis',(-1.22464679915E-16,-1.,-5.47382212627E-48));
#46390=DIRECTION('ref_axis',(1.,-1.22464679915E-16,-6.703498746053E-64));
#46391=DIRECTION('center_axis',(-2.81810938552877E-18,-1.,1.83623833789471E-17));
#46392=DIRECTION('ref_axis',(0.988427230781696,0.,0.151695779272954));
#46393=DIRECTION('center_axis',(-1.22464679915E-16,-1.,-5.47382212627E-48));
#46394=DIRECTION('ref_axis',(1.,-1.22464679915E-16,-6.703498746053E-64));
#46395=DIRECTION('center_axis',(-1.22464679915E-16,-1.,-6.16366086630911E-30));
#46396=DIRECTION('ref_axis',(-4.93432455388959E-14,0.,1.));
#46397=DIRECTION('center_axis',(-1.22464679915E-16,-1.,-5.47382212627E-48));
#46398=DIRECTION('ref_axis',(1.,-1.22464679915E-16,-6.703498746053E-64));
#46399=DIRECTION('center_axis',(-1.22464679915E-16,-1.,0.));
#46400=DIRECTION('ref_axis',(1.,-1.22464679915E-16,0.));
#46401=DIRECTION('center_axis',(-1.13563209349214E-16,-1.,3.17943322838876E-17));
#46402=DIRECTION('ref_axis',(-0.269603455472075,0.,-0.962971430935268));
#46403=DIRECTION('center_axis',(-1.22464679915E-16,-1.,-5.47382212627E-48));
#46404=DIRECTION('ref_axis',(1.,-1.22464679915E-16,-6.703498746053E-64));
#46405=DIRECTION('center_axis',(-0.962971430935267,1.17929988057033E-16,
0.269603455472075));
#46406=DIRECTION('ref_axis',(0.269603455472075,3.05583905676118E-32,0.962971430935268));
#46407=DIRECTION('center_axis',(-1.22464679915E-16,-1.,-5.47382212627E-48));
#46408=DIRECTION('ref_axis',(1.,-1.22464679915E-16,-6.703498746053E-64));
#46409=DIRECTION('center_axis',(1.22464679915E-16,1.,5.47382212627E-48));
#46410=DIRECTION('ref_axis',(1.,-1.22464679915E-16,0.));
#46411=DIRECTION('center_axis',(0.,0.,-1.));
#46412=DIRECTION('ref_axis',(-0.707106778693304,0.707106783679791,0.));
#46413=DIRECTION('center_axis',(-7.24819500366175E-17,-1.,6.01900799944532E-17));
#46414=DIRECTION('ref_axis',(-0.638858327474962,0.,-0.769324403236954));
#46415=DIRECTION('center_axis',(-1.22464679915E-16,-1.,-5.47382212627E-48));
#46416=DIRECTION('ref_axis',(1.,-1.22464679915E-16,6.22660996643423E-64));
#46417=DIRECTION('center_axis',(0.769324403236954,-9.42150667929943E-17,
-0.638858327474961));
#46418=DIRECTION('ref_axis',(0.638858327474961,7.17307849792281E-32,0.769324403236954));
#46419=DIRECTION('center_axis',(-1.22464679915E-16,-1.,-5.47382212627E-48));
#46420=DIRECTION('ref_axis',(1.,-1.22464679915E-16,5.9677926224237E-64));
#46421=DIRECTION('center_axis',(1.2246467991498E-16,1.,4.9218209689896E-29));
#46422=DIRECTION('ref_axis',(0.382683432365114,-4.6865204053314E-17,-0.923879532511277));
#46423=DIRECTION('center_axis',(1.22464679915E-16,1.,6.16297582204E-33));
#46424=DIRECTION('ref_axis',(1.,-1.22464679915E-16,-7.54746861370013E-49));
#46425=DIRECTION('',(-1.24169680386E-16,-1.,0.));
#46426=DIRECTION('center_axis',(-1.22464679915E-16,-1.,0.));
#46427=DIRECTION('ref_axis',(1.,-1.22464679915E-16,0.));
#46428=DIRECTION('center_axis',(0.382683432365114,-4.6865204053314E-17,
0.923879532511277));
#46429=DIRECTION('ref_axis',(-1.22464679914861E-16,-1.,3.33030126354153E-33));
#46430=DIRECTION('',(-1.66950830771E-16,-1.,0.));
#46431=DIRECTION('',(0.923879532511277,-1.79771717893054E-16,-0.382683432365114));
#46432=DIRECTION('',(-0.923879532511277,1.79771717893054E-16,0.382683432365114));
#46433=DIRECTION('center_axis',(-1.22464679914969E-16,-1.,1.40937670198757E-28));
#46434=DIRECTION('ref_axis',(-0.215815367394074,2.64297598885091E-17,-0.976434189895336));
#46435=DIRECTION('',(0.,1.,0.));
#46436=DIRECTION('center_axis',(0.,1.,5.04725420579478E-11));
#46437=DIRECTION('ref_axis',(-0.215814054939841,4.92832405001852E-11,-0.976434479978264));
#46438=DIRECTION('center_axis',(1.22464679914995E-16,1.,-2.84643200354157E-29));
#46439=DIRECTION('ref_axis',(-0.175818770215043,2.15315894174053E-17,-0.984422551570244));
#46440=DIRECTION('center_axis',(-1.22464679915E-16,-1.,-3.08148791102E-33));
#46441=DIRECTION('ref_axis',(1.,-1.22464679915E-16,2.83076871527624E-49));
#46442=DIRECTION('center_axis',(-0.978784588777817,-0.0498161334628422,
0.198743758689054));
#46443=DIRECTION('ref_axis',(0.194346018843094,0.0814603510708595,0.9775448000799));
#46444=DIRECTION('',(0.,-1.,0.));
#46445=DIRECTION('center_axis',(1.22464679915E-16,1.,3.08148791102E-33));
#46446=DIRECTION('ref_axis',(1.,-1.22464679915E-16,2.83076871527624E-49));
#46447=DIRECTION('',(0.,1.,0.));
#46448=DIRECTION('center_axis',(1.22464679915E-16,1.,-1.23259516441E-32));
#46449=DIRECTION('ref_axis',(1.,-1.22464679915E-16,-1.13230748611233E-48));
#46450=DIRECTION('',(0.,-1.,0.));
#46451=DIRECTION('center_axis',(1.22464679915E-16,1.,-6.16297582204E-33));
#46452=DIRECTION('ref_axis',(1.,-1.22464679915E-16,-5.66153743055249E-49));
#46453=DIRECTION('center_axis',(1.2246467991498E-16,1.,4.9218209689896E-29));
#46454=DIRECTION('ref_axis',(-0.382683432365115,4.68652040533141E-17,0.923879532511276));
#46455=DIRECTION('center_axis',(1.22464679915E-16,1.,-6.16297582204E-33));
#46456=DIRECTION('ref_axis',(1.,-1.22464679915E-16,7.54746861370013E-49));
#46457=DIRECTION('center_axis',(-1.22464679915E-16,-1.,-6.16297582204E-33));
#46458=DIRECTION('ref_axis',(1.,-1.22464679915E-16,-7.54746861370013E-49));
#46459=DIRECTION('',(-1.24169680386E-16,-1.,0.));
#46460=DIRECTION('center_axis',(0.382683432365114,-4.68652040533141E-17,
-0.923879532511277));
#46461=DIRECTION('ref_axis',(2.5429740769239E-34,-1.,5.07265313324192E-17));
#46462=DIRECTION('',(-0.923879532511277,1.79771717893054E-16,-0.382683432365114));
#46463=DIRECTION('center_axis',(0.382683432331542,-3.85987976375918E-9,
-0.923879532525183));
#46464=DIRECTION('ref_axis',(0.906907964349175,0.19079395606161,0.375653577821903));
#46465=DIRECTION('',(-1.66950830771E-16,-1.,0.));
#46466=DIRECTION('',(0.923879532511277,-1.79771717893054E-16,0.382683432365114));
#46467=DIRECTION('center_axis',(1.22464679915019E-16,1.,-7.85779417309992E-30));
#46468=DIRECTION('ref_axis',(-0.923879532511277,1.13142611229034E-16,0.382683432365114));
#46469=DIRECTION('center_axis',(1.22464679915E-16,1.,-6.16297582204E-33));
#46470=DIRECTION('ref_axis',(1.,-1.22464679915E-16,7.54746861370013E-49));
#46471=DIRECTION('',(-1.16865581539E-16,-1.,0.));
#46472=DIRECTION('center_axis',(0.923879532511277,-1.13142611229034E-16,
-0.382683432365114));
#46473=DIRECTION('ref_axis',(-1.31021084567677E-32,-1.,2.95655891162504E-16));
#46474=DIRECTION('center_axis',(0.923879532544053,-1.41481107281946E-8,
-0.382683432285984));
#46475=DIRECTION('ref_axis',(0.376061245770244,-0.185228919800991,0.907892166889378));
#46476=DIRECTION('',(-0.382683432365114,0.,-0.923879532511277));
#46477=DIRECTION('center_axis',(0.923879532507688,-2.76759523330007E-9,
-0.382683432373779));
#46478=DIRECTION('ref_axis',(0.375653574352959,0.190794018963353,0.906907952552881));
#46479=DIRECTION('',(0.,-1.,0.));
#46480=DIRECTION('',(0.382683432365114,0.,0.923879532511277));
#46481=DIRECTION('center_axis',(1.22464679915019E-16,1.,7.86635386174164E-30));
#46482=DIRECTION('ref_axis',(-0.923879532511276,1.13142611229034E-16,-0.382683432365115));
#46483=DIRECTION('center_axis',(1.22464679915E-16,1.,6.16297582204E-33));
#46484=DIRECTION('ref_axis',(1.,-1.22464679915E-16,-7.54746861370013E-49));
#46485=DIRECTION('',(-2.33731163079E-16,-1.,0.));
#46486=DIRECTION('center_axis',(0.923879532511277,-1.13142611229034E-16,
0.382683432365114));
#46487=DIRECTION('ref_axis',(-1.31021084567677E-32,-1.,-2.95655891162504E-16));
#46488=DIRECTION('',(0.382683432365114,0.,-0.923879532511277));
#46489=DIRECTION('',(-1.66950830771E-16,-1.,0.));
#46490=DIRECTION('',(-0.382683432365114,0.,0.923879532511277));
#46491=DIRECTION('center_axis',(1.2246467991498E-16,1.,-4.9218209689896E-29));
#46492=DIRECTION('ref_axis',(-0.382683432365114,4.6865204053314E-17,-0.923879532511277));
#46493=DIRECTION('center_axis',(1.22464679915E-16,1.,6.16297582204E-33));
#46494=DIRECTION('ref_axis',(1.,-1.22464679915E-16,-7.54746861370013E-49));
#46495=DIRECTION('center_axis',(-1.22464679915E-16,-1.,0.));
#46496=DIRECTION('ref_axis',(1.,-1.22464679915E-16,0.));
#46497=DIRECTION('center_axis',(0.766057840542209,-0.255399249832434,0.589853039433415));
#46498=DIRECTION('ref_axis',(-0.202361789893946,-0.966835675378721,-0.155815540963958));
#46499=DIRECTION('center_axis',(-1.22464679915E-16,-1.,0.));
#46500=DIRECTION('ref_axis',(1.,-1.22464679915E-16,0.));
#46501=DIRECTION('center_axis',(-0.792335098973394,9.70330642810483E-17,
-0.610086134029304));
#46502=DIRECTION('ref_axis',(0.610086134029304,5.05601228850744E-32,-0.792335098973394));
#46503=DIRECTION('center_axis',(-7.68827025909336E-17,-1.,-5.91985270603321E-17));
#46504=DIRECTION('ref_axis',(-0.610086134029304,0.,0.792335098973394));
#46505=DIRECTION('center_axis',(-1.22464679915E-16,-1.,-5.47382212627E-48));
#46506=DIRECTION('ref_axis',(1.,-1.22464679915E-16,5.40238148608971E-64));
#46507=DIRECTION('center_axis',(-0.611236674075818,7.48549036428777E-17,
-0.791447868317764));
#46508=DIRECTION('ref_axis',(0.791447868317764,-7.00049973634741E-32,-0.611236674075818));
#46509=DIRECTION('center_axis',(-1.22464679914949E-16,-1.,-1.08530702891677E-28));
#46510=DIRECTION('ref_axis',(2.12313165367255E-16,-1.08554598373815E-28,
1.));
#46511=DIRECTION('center_axis',(1.22464679915E-16,1.,0.));
#46512=DIRECTION('ref_axis',(1.,-1.22464679915E-16,0.));
#46513=DIRECTION('',(0.,-1.,0.));
#46514=DIRECTION('',(0.,-1.,0.));
#46515=DIRECTION('center_axis',(1.22464679915E-16,1.,1.54074395551E-33));
#46516=DIRECTION('ref_axis',(1.,-1.22464679915E-16,1.52063520297906E-49));
#46517=DIRECTION('center_axis',(-1.22464679915E-16,-1.,0.));
#46518=DIRECTION('ref_axis',(1.,-1.22464679915E-16,0.));
#46519=DIRECTION('',(-1.03939138974E-16,-1.,0.));
#46520=DIRECTION('center_axis',(1.22464679914914E-16,1.,1.11943608056428E-28));
#46521=DIRECTION('ref_axis',(-0.610086134029304,7.47140031243373E-17,0.792335098973394));
#46522=DIRECTION('center_axis',(0.,-1.,0.));
#46523=DIRECTION('ref_axis',(-0.610086133998045,0.,0.792335098997463));
#46524=DIRECTION('',(0.,-1.,0.));
#46525=DIRECTION('center_axis',(0.678891257295808,-8.31402005216763E-17,
0.734238830876792));
#46526=DIRECTION('ref_axis',(-1.22464679914784E-16,-1.,1.83887638005312E-34));
#46527=DIRECTION('',(0.734238830876791,0.,-0.678891257295807));
#46528=DIRECTION('',(0.,-1.,0.));
#46529=DIRECTION('',(-0.734238830876792,0.,0.678891257295808));
#46530=DIRECTION('',(0.,-1.,0.));
#46531=DIRECTION('center_axis',(-0.678891257318237,7.43492351073594E-12,
-0.734238830856053));
#46532=DIRECTION('ref_axis',(-1.46208970879984E-10,-1.,1.25062923000865E-10));
#46533=DIRECTION('',(-0.734238830876792,0.,0.678891257295808));
#46534=DIRECTION('center_axis',(1.22464679914942E-16,1.,7.54279763108459E-29));
#46535=DIRECTION('ref_axis',(0.612227349738988,-7.49762264208985E-17,-0.790681776842982));
#46536=DIRECTION('center_axis',(-1.22464679915E-16,-1.,0.));
#46537=DIRECTION('ref_axis',(1.,-1.22464679915E-16,0.));
#46538=DIRECTION('',(0.,-1.,0.));
#46539=DIRECTION('center_axis',(1.22464679915E-16,1.,-6.16297582204E-33));
#46540=DIRECTION('ref_axis',(1.,-1.22464679915E-16,7.54746861370013E-49));
#46541=DIRECTION('center_axis',(-1.22464679914998E-16,-1.,-1.73663083545565E-29));
#46542=DIRECTION('ref_axis',(-0.095298509688002,1.16707014853003E-17,0.99544874004202));
#46543=DIRECTION('',(-1.32169407693E-16,-1.,0.));
#46544=DIRECTION('center_axis',(-1.22464679915E-16,-1.,6.16297582204E-33));
#46545=DIRECTION('ref_axis',(1.,-1.22464679915E-16,7.54746861370013E-49));
#46546=DIRECTION('center_axis',(1.22464679915E-16,1.,0.));
#46547=DIRECTION('ref_axis',(1.,-1.22464679915E-16,0.));
#46548=DIRECTION('center_axis',(1.22464679915E-16,1.,7.60253073092891E-48));
#46549=DIRECTION('ref_axis',(1.,-1.22464679915E-16,-9.3104149250716E-64));
#46550=DIRECTION('center_axis',(-1.22464679915E-16,-1.,3.08148791102E-33));
#46551=DIRECTION('ref_axis',(1.,-1.22464679915E-16,3.77373430685006E-49));
#46552=DIRECTION('',(-1.23358113847E-16,-1.,0.));
#46553=DIRECTION('center_axis',(1.22464679915E-16,1.,0.));
#46554=DIRECTION('ref_axis',(1.,-1.22464679915E-16,0.));
#46555=DIRECTION('center_axis',(-1.,1.22464679915E-16,-6.12323399574E-17));
#46556=DIRECTION('ref_axis',(-6.12323399574E-17,0.,1.));
#46557=DIRECTION('',(-1.32169407693E-16,-1.,0.));
#46558=DIRECTION('',(2.19188076492E-16,0.,-1.));
#46559=DIRECTION('',(-2.17106560191E-16,0.,1.));
#46560=DIRECTION('center_axis',(-1.22464679914917E-16,-1.,-1.21085355525786E-28));
#46561=DIRECTION('ref_axis',(-0.566106835688783,6.93280924301735E-17,0.824331881335687));
#46562=DIRECTION('center_axis',(1.22464679915E-16,1.,0.));
#46563=DIRECTION('ref_axis',(1.,-1.22464679915E-16,0.));
#46564=DIRECTION('',(0.,-1.,0.));
#46565=DIRECTION('center_axis',(-1.22464679915E-16,-1.,1.54074395550985E-33));
#46566=DIRECTION('ref_axis',(1.,-1.22464679915E-16,-5.78241158658936E-15));
#46567=DIRECTION('center_axis',(-1.22464679915E-16,-1.,0.));
#46568=DIRECTION('ref_axis',(1.,-1.22464679915E-16,0.));
#46569=DIRECTION('',(-1.04083408559E-16,-1.,0.));
#46570=DIRECTION('center_axis',(1.22464679915E-16,1.,0.));
#46571=DIRECTION('ref_axis',(1.,-1.22464679915E-16,0.));
#46572=DIRECTION('center_axis',(-1.22464679914999E-16,-1.,-1.9442368107527E-29));
#46573=DIRECTION('ref_axis',(-0.0510637267514752,6.25350295186696E-18,0.998695396910515));
#46574=DIRECTION('center_axis',(-1.22464679915E-16,-1.,1.54074395551E-33));
#46575=DIRECTION('ref_axis',(1.,-1.22464679915E-16,-1.75263489528827E-49));
#46576=DIRECTION('center_axis',(1.22464679915E-16,1.,-1.23259516441E-32));
#46577=DIRECTION('ref_axis',(1.,-1.22464679915E-16,-1.40210791623289E-48));
#46578=DIRECTION('center_axis',(-2.17357452795E-16,2.66186108837E-32,1.));
#46579=DIRECTION('ref_axis',(-1.,-5.7857534586223E-48,-2.17357452795E-16));
#46580=DIRECTION('center_axis',(-1.78560869794E-14,2.18673997646E-30,1.));
#46581=DIRECTION('ref_axis',(1.,1.11272749077955E-45,1.78560869794E-14));
#46582=DIRECTION('',(-8.96394535471E-17,0.,1.));
#46583=DIRECTION('center_axis',(1.6065913575E-14,-1.96750696351E-30,1.));
#46584=DIRECTION('ref_axis',(1.,-2.52100835352406E-45,-1.6065913575E-14));
#46585=DIRECTION('',(-8.96394535471E-17,0.,1.));
#46586=DIRECTION('center_axis',(-1.17989839311979E-16,-1.,-2.29779399358865E-17));
#46587=DIRECTION('ref_axis',(-0.191153986297934,0.,0.981560061087659));
#46588=DIRECTION('center_axis',(-0.981560061087659,1.20206438697958E-16,
-0.191153986297933));
#46589=DIRECTION('ref_axis',(0.191153986297933,-8.55574366268044E-33,-0.981560061087659));
#46590=DIRECTION('center_axis',(-1.22464679915E-16,-1.,-5.47382212627E-48));
#46591=DIRECTION('ref_axis',(1.,-1.22464679915E-16,-6.703498746053E-64));
#46592=DIRECTION('center_axis',(-0.973274002238674,1.1919168915396E-16,
-0.229646938943923));
#46593=DIRECTION('ref_axis',(0.229646938943923,-2.91124363913666E-32,-0.973274002238674));
#46594=DIRECTION('center_axis',(-1.22464679915E-16,-1.,-5.47382212627E-48));
#46595=DIRECTION('ref_axis',(1.,-1.22464679915E-16,-6.703498746053E-64));
#46596=DIRECTION('center_axis',(-1.17989839311979E-16,-1.,-2.29779399358865E-17));
#46597=DIRECTION('ref_axis',(0.191153986297933,0.,-0.981560061087659));
#46598=DIRECTION('center_axis',(2.17357452795E-16,-2.66186108837E-32,-1.));
#46599=DIRECTION('ref_axis',(1.,5.7857534586223E-48,2.17357452795E-16));
#46600=DIRECTION('center_axis',(1.22464679915E-16,1.,3.08148791102E-33));
#46601=DIRECTION('ref_axis',(1.,-1.22464679915E-16,-3.77373430685006E-49));
#46602=DIRECTION('center_axis',(1.22464679915E-16,1.,5.47382212627E-48));
#46603=DIRECTION('ref_axis',(1.,-1.22464679915E-16,-6.703498746053E-64));
#46604=DIRECTION('center_axis',(2.17357452795E-16,-2.66186108836821E-32,
-1.));
#46605=DIRECTION('ref_axis',(-5.78575345861839E-48,-1.,2.66186108836821E-32));
#46606=DIRECTION('center_axis',(-5.70383201187E-15,6.98517961621E-31,-1.));
#46607=DIRECTION('ref_axis',(1.,-5.48892443580096E-47,-5.70383201187E-15));
#46608=DIRECTION('',(7.61796550883E-17,0.,-1.));
#46609=DIRECTION('',(5.71347413162E-17,0.,-1.));
#46610=DIRECTION('center_axis',(-4.29367103357466E-45,-1.,-7.25136572506882E-31));
#46611=DIRECTION('ref_axis',(1.,0.,-5.9211894646675E-15));
#46612=DIRECTION('center_axis',(0.984869499718035,-1.20611728041004E-16,
0.173297629889006));
#46613=DIRECTION('ref_axis',(0.173297629889006,5.41148511020646E-32,-0.984869499718035));
#46614=DIRECTION('center_axis',(1.22464679915E-16,1.,-3.08148791102E-33));
#46615=DIRECTION('ref_axis',(1.,-1.22464679915E-16,3.77373430685006E-49));
#46616=DIRECTION('center_axis',(1.22464679915E-16,1.,5.47382212627E-48));
#46617=DIRECTION('ref_axis',(1.,-1.22464679915E-16,-6.703498746053E-64));
#46618=DIRECTION('center_axis',(-1.18786812255882E-16,-1.,-2.09017266063253E-17));
#46619=DIRECTION('ref_axis',(-0.173297629889006,0.,0.984869499718035));
#46620=DIRECTION('center_axis',(0.825067330468845,-1.01041606533981E-16,
0.565034423900893));
#46621=DIRECTION('ref_axis',(0.565034423900893,7.24547600115018E-32,-0.825067330468845));
#46622=DIRECTION('center_axis',(1.22464679915E-16,1.,5.47382212627E-48));
#46623=DIRECTION('ref_axis',(1.,-1.22464679915E-16,-6.703498746053E-64));
#46624=DIRECTION('center_axis',(1.22464679915E-16,1.,5.47382212627E-48));
#46625=DIRECTION('ref_axis',(1.,-1.22464679915E-16,-6.703498746053E-64));
#46626=DIRECTION('center_axis',(-6.60215246509141E-17,-1.,6.10447636300053E-17));
#46627=DIRECTION('ref_axis',(-0.678891257295808,0.,-0.734238830876792));
#46628=DIRECTION('center_axis',(1.22464679915E-16,1.,-1.23259516441E-32));
#46629=DIRECTION('ref_axis',(1.,-1.22464679915E-16,1.50949372274247E-48));
#46630=DIRECTION('center_axis',(-0.734238830876792,8.99183234042744E-17,
0.678891257295808));
#46631=DIRECTION('ref_axis',(0.678891257295808,-2.24691316591619E-32,0.734238830876792));
#46632=DIRECTION('center_axis',(1.22464679915E-16,1.,5.47382212627E-48));
#46633=DIRECTION('ref_axis',(1.,-1.22464679915E-16,-6.703498746053E-64));
#46634=DIRECTION('center_axis',(-8.3366128569448E-17,-1.,-5.70919859380671E-17));
#46635=DIRECTION('ref_axis',(-0.565034423900894,0.,0.825067330468845));
#46636=DIRECTION('center_axis',(-0.734238830876792,8.99183234042744E-17,
0.678891257295808));
#46637=DIRECTION('ref_axis',(0.678891257295808,-2.24691316591619E-32,0.734238830876792));
#46638=DIRECTION('center_axis',(1.22464679915E-16,1.,-1.23259516441E-32));
#46639=DIRECTION('ref_axis',(1.,-1.22464679915E-16,1.50949372274247E-48));
#46640=DIRECTION('center_axis',(1.22464679915E-16,1.,5.47382212627E-48));
#46641=DIRECTION('ref_axis',(1.,-1.22464679915E-16,-6.703498746053E-64));
#46642=DIRECTION('center_axis',(-0.734238830876792,8.99183234044499E-17,
0.678891257295808));
#46643=DIRECTION('ref_axis',(-6.60215246508846E-17,-1.,6.1044763629978E-17));
#46644=DIRECTION('',(-0.734238830876791,0.,0.678891257295807));
#46645=DIRECTION('',(-0.734238830876791,0.,0.678891257295807));
#46646=DIRECTION('center_axis',(-5.11601622893148E-18,-1.,2.45021972047681E-17));
#46647=DIRECTION('ref_axis',(-0.978889450967439,0.,-0.204390417546091));
#46648=DIRECTION('center_axis',(0.204390417546092,-2.50306070625112E-17,
-0.978889450967439));
#46649=DIRECTION('ref_axis',(0.978889450967439,-1.05289930055147E-32,0.204390417546092));
#46650=DIRECTION('center_axis',(-1.22464679915E-16,-1.,-5.47382212627E-48));
#46651=DIRECTION('ref_axis',(1.,-1.22464679915E-16,-6.703498746053E-64));
#46652=DIRECTION('center_axis',(0.419584599500152,-5.13842936749187E-17,
-0.90771623531933));
#46653=DIRECTION('ref_axis',(0.90771623531933,-2.72267697829008E-32,0.419584599500152));
#46654=DIRECTION('center_axis',(-1.22464679915E-16,-1.,-5.47382212627E-48));
#46655=DIRECTION('ref_axis',(1.,-1.22464679915E-16,-6.703498746053E-64));
#46656=DIRECTION('center_axis',(0.382636981165606,-0.0155797766458367,-0.923767401029143));
#46657=DIRECTION('ref_axis',(0.670813900451024,0.692209394753623,0.266185771175894));
#46658=DIRECTION('center_axis',(0.382683425383291,2.34479170719746E-9,-0.923879535403242));
#46659=DIRECTION('ref_axis',(0.653279884842593,0.70710851193395,0.270597384338069));
#46660=DIRECTION('center_axis',(-2.15600582822439E-17,-1.,4.66423576092589E-17));
#46661=DIRECTION('ref_axis',(-0.90771623531933,0.,-0.419584599500153));
#46662=DIRECTION('center_axis',(-0.0335155327516907,4.10446899060886E-18,
0.999438196720723));
#46663=DIRECTION('ref_axis',(0.999438196720723,5.21239906410075E-34,0.0335155327516907));
#46664=DIRECTION('center_axis',(-1.22464679915E-16,-1.,0.));
#46665=DIRECTION('ref_axis',(1.,-1.22464679915E-16,0.));
#46666=DIRECTION('center_axis',(-1.22464679915E-16,-1.,-5.47382212627E-48));
#46667=DIRECTION('ref_axis',(1.,-1.22464679915E-16,-6.703498746053E-64));
#46668=DIRECTION('center_axis',(-0.382683432388042,2.52266547895476E-11,
-0.92387953250178));
#46669=DIRECTION('ref_axis',(0.653281506872114,0.707106754739568,-0.270598060193668));
#46670=DIRECTION('center_axis',(0.854119591553195,0.0486596199953837,-0.517795292279593));
#46671=DIRECTION('ref_axis',(0.492492289235195,0.244264035758894,0.835336115511986));
#46672=DIRECTION('center_axis',(-0.382579843714528,0.0232740187023026,-0.923629245550839));
#46673=DIRECTION('ref_axis',(0.679149393449658,0.684858194219679,-0.264055591092333));
#46674=DIRECTION('center_axis',(0.382579759521302,-0.0232739793740044,-0.923629281415829));
#46675=DIRECTION('ref_axis',(0.679152682329405,0.684854387074657,0.264057006325091));
#46676=DIRECTION('center_axis',(-5.06268119967007E-18,-1.,-2.43796819441885E-17));
#46677=DIRECTION('ref_axis',(-0.979111878581668,0.,0.203322230019931));
#46678=DIRECTION('center_axis',(1.22464679915E-16,1.,5.47382212627E-48));
#46679=DIRECTION('ref_axis',(1.,-1.22464679915E-16,-6.703498746053E-64));
#46680=DIRECTION('center_axis',(0.203322230019931,-2.48997918188915E-17,
0.979111878581668));
#46681=DIRECTION('ref_axis',(0.979111878581668,-1.33094098597294E-33,-0.203322230019931));
#46682=DIRECTION('center_axis',(1.22464679915E-16,1.,5.47382212627E-48));
#46683=DIRECTION('ref_axis',(1.,-1.22464679915E-16,-6.703498746053E-64));
#46684=DIRECTION('center_axis',(-1.22464679915E-16,-1.,0.));
#46685=DIRECTION('ref_axis',(0.,0.,1.));
#46686=DIRECTION('center_axis',(-1.,1.22464679915E-16,-6.12323399574E-17));
#46687=DIRECTION('ref_axis',(-1.22464679915E-16,-1.,-7.49879891332945E-33));
#46688=DIRECTION('center_axis',(-1.22464679915E-16,-1.,-5.47382212627E-48));
#46689=DIRECTION('ref_axis',(1.,-1.22464679915E-16,-6.703498746053E-64));
#46690=DIRECTION('center_axis',(-1.22464679915E-16,-1.,-5.47382212627E-48));
#46691=DIRECTION('ref_axis',(1.,-1.22464679915E-16,-6.703498746053E-64));
#46692=DIRECTION('center_axis',(-5.06268119967007E-18,-1.,-2.43796819441885E-17));
#46693=DIRECTION('ref_axis',(0.979111878581668,0.,-0.203322230019931));
#46694=DIRECTION('center_axis',(-1.22464679915E-16,-1.,-5.47382212627E-48));
#46695=DIRECTION('ref_axis',(1.,-1.22464679915E-16,-6.703498746053E-64));
#46696=DIRECTION('center_axis',(-1.,1.22464679915E-16,-6.12323399574E-17));
#46697=DIRECTION('ref_axis',(-1.22464679915E-16,-1.,-7.49879891332945E-33));
#46698=DIRECTION('center_axis',(-1.22464679915E-16,-1.,-6.16297582204E-33));
#46699=DIRECTION('ref_axis',(1.,-1.22464679915E-16,-7.54746861370013E-49));
#46700=DIRECTION('center_axis',(-1.,1.22464679915E-16,-6.12323399574E-17));
#46701=DIRECTION('ref_axis',(6.12323399574E-17,-7.49879891332945E-33,-1.));
#46702=DIRECTION('',(-1.,0.,0.));
#46703=DIRECTION('',(-1.,0.,0.));
#46704=DIRECTION('center_axis',(-0.923879532523066,-2.50321061818283E-11,
-0.382683432336653));
#46705=DIRECTION('ref_axis',(0.270598059367657,0.707106756803419,-0.653281504980363));
#46706=DIRECTION('center_axis',(0.237817192548205,0.0486596292822717,-0.970090317138874));
#46707=DIRECTION('ref_axis',(0.938916649716559,0.244263330956247,0.242427205641592));
#46708=DIRECTION('center_axis',(-0.923629304634498,0.0232740186304629,-0.382579701078328));
#46709=DIRECTION('ref_axis',(0.293515644570473,0.684858188071701,-0.666946646009654));
#46710=DIRECTION('center_axis',(-0.38257978588401,-0.0232739793753114,-0.923629270496005));
#46711=DIRECTION('ref_axis',(0.66694996580489,0.684854388356,-0.293516966907172));
#46712=DIRECTION('center_axis',(0.970089609818427,0.0486732638221455,-0.237817287662678));
#46713=DIRECTION('ref_axis',(0.242486471652566,-0.239688973466001,0.940079521670536));
#46714=DIRECTION('center_axis',(-0.382683509132997,3.37979830178284E-8,
-0.923879500712974));
#46715=DIRECTION('ref_axis',(0.653293893777471,0.707093332555111,-0.27060322874862));
#46716=DIRECTION('center_axis',(-7.79403475186991E-17,-1.,-5.89087594505755E-17));
#46717=DIRECTION('ref_axis',(-0.602966636474875,0.,0.797766403966835));
#46718=DIRECTION('center_axis',(-1.22464679915E-16,-1.,-5.47382212627E-48));
#46719=DIRECTION('ref_axis',(1.,-1.22464679915E-16,-6.703498746053E-64));
#46720=DIRECTION('center_axis',(-0.797766403966835,9.76982073084798E-17,
-0.602966636474875));
#46721=DIRECTION('ref_axis',(0.602966636474875,6.43171104150991E-32,-0.797766403966835));
#46722=DIRECTION('center_axis',(-1.22464679915E-16,-1.,-5.47382212627E-48));
#46723=DIRECTION('ref_axis',(1.,-1.22464679915E-16,-6.703498746053E-64));
#46724=DIRECTION('center_axis',(-0.585630202615096,7.17190153117117E-17,
-0.810578352650132));
#46725=DIRECTION('ref_axis',(0.810578352650132,6.4321265031143E-32,-0.585630202615096));
#46726=DIRECTION('center_axis',(-1.22464679915E-16,-1.,-5.47382212627E-48));
#46727=DIRECTION('ref_axis',(1.,-1.22464679915E-16,-6.703498746053E-64));
#46728=DIRECTION('center_axis',(-7.79403475186991E-17,-1.,-5.89087594505755E-17));
#46729=DIRECTION('ref_axis',(0.602966636474876,0.,-0.797766403966835));
#46730=DIRECTION('center_axis',(0.734238830876792,-8.99183234042744E-17,
-0.678891257295808));
#46731=DIRECTION('ref_axis',(0.678891257295808,-2.24691316591619E-32,0.734238830876792));
#46732=DIRECTION('center_axis',(1.22464679915E-16,1.,0.));
#46733=DIRECTION('ref_axis',(1.,-1.22464679915E-16,0.));
#46734=DIRECTION('center_axis',(1.22464679915E-16,1.,5.47382212627E-48));
#46735=DIRECTION('ref_axis',(1.,-1.22464679915E-16,-6.703498746053E-64));
#46736=DIRECTION('center_axis',(-0.734238830876792,8.99183234042744E-17,
0.678891257295808));
#46737=DIRECTION('ref_axis',(-0.678891257295808,-1.51038693775819E-31,-0.734238830876792));
#46738=DIRECTION('center_axis',(0.73423883087825,-8.99183234044306E-17,
-0.678891257294231));
#46739=DIRECTION('ref_axis',(0.678891257294231,1.10716302178481E-31,0.73423883087825));
#46740=DIRECTION('',(0.734238830876791,0.,-0.678891257295807));
#46741=DIRECTION('',(0.734238830876791,0.,-0.678891257295807));
#46742=DIRECTION('center_axis',(-6.60215246511763E-17,-1.,6.10447636299848E-17));
#46743=DIRECTION('ref_axis',(0.678891257294231,0.,0.73423883087825));
#46744=DIRECTION('center_axis',(0.581646529321033,-7.12311560368041E-17,
0.813441648140047));
#46745=DIRECTION('ref_axis',(0.813441648140047,-2.80119922649672E-32,-0.581646529321033));
#46746=DIRECTION('center_axis',(1.22464679915E-16,1.,-1.23259516441E-32));
#46747=DIRECTION('ref_axis',(1.,-1.22464679915E-16,1.50949372274247E-48));
#46748=DIRECTION('center_axis',(1.22464679915E-16,1.,5.47382212627E-48));
#46749=DIRECTION('ref_axis',(1.,-1.22464679915E-16,-6.703498746053E-64));
#46750=DIRECTION('center_axis',(-4.14313546884292E-17,-1.,-5.79423889656346E-17));
#46751=DIRECTION('ref_axis',(-0.813441648140047,0.,0.581646529321034));
#46752=DIRECTION('center_axis',(0.142980079684983,-1.75100096927979E-17,
0.98972556641388));
#46753=DIRECTION('ref_axis',(0.98972556641388,3.23015489124122E-33,-0.142980079684983));
#46754=DIRECTION('center_axis',(1.22464679915E-16,1.,5.47382212627E-48));
#46755=DIRECTION('ref_axis',(1.,-1.22464679915E-16,-6.703498746053E-64));
#46756=DIRECTION('center_axis',(1.22464679915E-16,1.,5.47382212627E-48));
#46757=DIRECTION('ref_axis',(1.,-1.22464679915E-16,-6.703498746053E-64));
#46758=DIRECTION('center_axis',(-1.22464679915E-16,-1.,0.));
#46759=DIRECTION('ref_axis',(0.,0.,-1.));
#46760=DIRECTION('center_axis',(1.22464679915E-16,1.,5.47382212627E-48));
#46761=DIRECTION('ref_axis',(1.,-1.22464679915E-16,-6.703498746053E-64));
#46762=DIRECTION('center_axis',(-1.,1.22464679915E-16,-6.12323399574E-17));
#46763=DIRECTION('ref_axis',(-1.22464679915E-16,-1.,-7.49879891332945E-33));
#46764=DIRECTION('center_axis',(1.22464679915E-16,1.,5.47382212627E-48));
#46765=DIRECTION('ref_axis',(1.,-1.22464679915E-16,-6.703498746053E-64));
#46766=DIRECTION('center_axis',(-2.50358258116745E-18,-1.,-1.73301042611612E-17));
#46767=DIRECTION('ref_axis',(-0.98972556641388,0.,0.142980079684983));
#46768=DIRECTION('center_axis',(-1.,1.22464679915E-16,-6.12323399574E-17));
#46769=DIRECTION('ref_axis',(-1.22464679915E-16,-1.,-7.49879891332945E-33));
#46770=DIRECTION('center_axis',(1.22464679915E-16,1.,5.47382212627E-48));
#46771=DIRECTION('ref_axis',(1.,-1.22464679915E-16,-6.703498746053E-64));
#46772=DIRECTION('center_axis',(1.22464679915E-16,1.,5.47382212627E-48));
#46773=DIRECTION('ref_axis',(1.,-1.22464679915E-16,-6.703498746053E-64));
#46774=DIRECTION('center_axis',(-1.,1.22464679915E-16,-6.12323399574E-17));
#46775=DIRECTION('ref_axis',(-1.22464679915E-16,-1.,-7.49879891332945E-33));
#46776=DIRECTION('',(-1.,0.,-2.89652532403E-16));
#46777=DIRECTION('',(-1.,0.,-2.89652532403E-16));
#46778=DIRECTION('center_axis',(-0.734238830876792,8.99183234042744E-17,
0.678891257295808));
#46779=DIRECTION('ref_axis',(0.678891257295808,-2.24691316591619E-32,0.734238830876792));
#46780=DIRECTION('',(-0.734238830876791,0.,0.678891257295807));
#46781=DIRECTION('',(-0.734238830876791,0.,0.678891257295807));
#46782=DIRECTION('center_axis',(-0.734238830876792,8.991832340449E-17,0.678891257295808));
#46783=DIRECTION('ref_axis',(6.6021524650914E-17,1.,-6.10447636300053E-17));
#46784=DIRECTION('',(0.734238830876791,0.,-0.678891257295807));
#46785=DIRECTION('center_axis',(0.734238830881096,6.3373930704663E-12,-0.678891257291153));
#46786=DIRECTION('ref_axis',(6.40968759550252E-12,1.,1.62684680541738E-11));
#46787=DIRECTION('',(0.734238830876791,0.,-0.678891257295807));
#46788=DIRECTION('center_axis',(1.69872863391202E-17,1.,4.23293596334453E-17));
#46789=DIRECTION('ref_axis',(0.928056183869048,0.,-0.37244022283102));
#46790=DIRECTION('center_axis',(1.22464679915E-16,1.,5.47382212627E-48));
#46791=DIRECTION('ref_axis',(1.,-1.22464679915E-16,-6.703498746053E-64));
#46792=DIRECTION('center_axis',(1.22464679915E-16,1.,5.47382212627E-48));
#46793=DIRECTION('ref_axis',(1.,-1.22464679915E-16,-6.703498746053E-64));
#46794=DIRECTION('center_axis',(0.,1.,0.));
#46795=DIRECTION('ref_axis',(0.231145326606897,0.,-0.972919235079557));
#46796=DIRECTION('center_axis',(-0.0335155327516907,4.10446899060886E-18,
0.999438196720723));
#46797=DIRECTION('ref_axis',(0.999438196720723,5.21239906410075E-34,0.0335155327516907));
#46798=DIRECTION('center_axis',(1.22464679915E-16,1.,0.));
#46799=DIRECTION('ref_axis',(1.,-1.22464679915E-16,0.));
#46800=DIRECTION('center_axis',(5.9296278727138E-17,1.,6.12017248415691E-17));
#46801=DIRECTION('ref_axis',(0.718198537785833,0.,-0.695838242928838));
#46802=DIRECTION('center_axis',(-1.22464679915E-16,-1.,-5.47382212627E-48));
#46803=DIRECTION('ref_axis',(1.,-1.22464679915E-16,-6.703498746053E-64));
#46804=DIRECTION('center_axis',(-1.22464679915E-16,-1.,-5.47382212627E-48));
#46805=DIRECTION('ref_axis',(1.,-1.22464679915E-16,-6.703498746053E-64));
#46806=DIRECTION('center_axis',(0.,1.,0.));
#46807=DIRECTION('ref_axis',(-0.776012376688289,0.,0.630717679494236));
#46808=DIRECTION('center_axis',(-1.,1.22464679915E-16,-6.12323399574E-17));
#46809=DIRECTION('ref_axis',(-1.22464679915E-16,-1.,-7.49879891332945E-33));
#46810=DIRECTION('center_axis',(1.22464679915E-16,1.,5.47382212627E-48));
#46811=DIRECTION('ref_axis',(1.,-1.22464679915E-16,-6.703498746053E-64));
#46812=DIRECTION('center_axis',(0.,0.,1.));
#46813=DIRECTION('ref_axis',(1.,0.,0.));
#46814=DIRECTION('center_axis',(-1.,1.22464679915E-16,-6.12323399574E-17));
#46815=DIRECTION('ref_axis',(-1.22464679915E-16,-1.,-7.49879891332945E-33));
#46816=DIRECTION('center_axis',(1.22464679915E-16,1.,6.16297582204E-33));
#46817=DIRECTION('ref_axis',(1.,-1.22464679915E-16,-7.54746861370013E-49));
#46818=DIRECTION('center_axis',(0.,1.,0.));
#46819=DIRECTION('ref_axis',(0.998774211147154,0.,-0.0494982337804088));
#46820=DIRECTION('center_axis',(-0.797766403966835,9.76982073084798E-17,
-0.602966636474875));
#46821=DIRECTION('ref_axis',(0.602966636474875,6.43171104150991E-32,-0.797766403966835));
#46822=DIRECTION('center_axis',(-1.22464679915E-16,-1.,0.));
#46823=DIRECTION('ref_axis',(1.,-1.22464679915E-16,0.));
#46824=DIRECTION('center_axis',(-1.,1.22464679915E-16,-6.12323399574E-17));
#46825=DIRECTION('ref_axis',(-6.12323399574E-17,7.49879891332945E-33,1.));
#46826=DIRECTION('',(1.,0.,4.09734305096E-16));
#46827=DIRECTION('',(1.,0.,0.));
#46828=DIRECTION('center_axis',(5.9296278727138E-17,1.,6.12017248415691E-17));
#46829=DIRECTION('ref_axis',(-0.714690181301574,0.,0.699441166039806));
#46830=DIRECTION('center_axis',(1.22464679915E-16,1.,5.47382212627E-48));
#46831=DIRECTION('ref_axis',(1.,-1.22464679915E-16,-6.703498746053E-64));
#46832=DIRECTION('center_axis',(1.22464679915E-16,1.,5.47382212627E-48));
#46833=DIRECTION('ref_axis',(1.,-1.22464679915E-16,-6.703498746053E-64));
#46834=DIRECTION('center_axis',(-2.68354439599323E-46,-1.,1.81284143127026E-31));
#46835=DIRECTION('ref_axis',(1.,0.,1.97372982155583E-15));
#46836=DIRECTION('center_axis',(-1.22464679915E-16,-1.,-5.47382212627E-48));
#46837=DIRECTION('ref_axis',(1.,-1.22464679915E-16,-6.703498746053E-64));
#46838=DIRECTION('center_axis',(-0.991694064582439,1.21447496192053E-16,
0.128619136492057));
#46839=DIRECTION('ref_axis',(0.128619136492057,-7.10548517584315E-33,0.991694064582438));
#46840=DIRECTION('center_axis',(-1.22464679915E-16,-1.,-5.47382212627E-48));
#46841=DIRECTION('ref_axis',(1.,-1.22464679915E-16,-6.703498746053E-64));
#46842=DIRECTION('center_axis',(-8.38660245249135E-17,-1.,5.68956569482564E-17));
#46843=DIRECTION('ref_axis',(-0.561410669601872,0.,-0.827537346623811));
#46844=DIRECTION('center_axis',(1.22464679915E-16,1.,5.47382212627E-48));
#46845=DIRECTION('ref_axis',(1.,-1.22464679915E-16,-6.703498746053E-64));
#46846=DIRECTION('center_axis',(-0.827537346623811,1.01344096271977E-16,
0.561410669601872));
#46847=DIRECTION('ref_axis',(0.561410669601872,-5.47362952277333E-32,0.827537346623811));
#46848=DIRECTION('center_axis',(1.22464679915E-16,1.,5.47382212627E-48));
#46849=DIRECTION('ref_axis',(1.,-1.22464679915E-16,-6.703498746053E-64));
#46850=DIRECTION('center_axis',(-5.78330237622164E-17,-1.,-6.11379105471829E-17));
#46851=DIRECTION('ref_axis',(-0.726469216974212,0.,0.687199008140201));
#46852=DIRECTION('center_axis',(-0.687199008140201,8.41576065696246E-17,
-0.726469216974212));
#46853=DIRECTION('ref_axis',(0.726469216974212,1.50838013754883E-32,-0.687199008140201));
#46854=DIRECTION('center_axis',(-1.22464679915E-16,-1.,-5.47382212627E-48));
#46855=DIRECTION('ref_axis',(1.,-1.22464679915E-16,-6.703498746053E-64));
#46856=DIRECTION('center_axis',(-1.22464679915E-16,-1.,0.));
#46857=DIRECTION('ref_axis',(1.,-1.22464679915E-16,0.));
#46858=DIRECTION('center_axis',(-8.38660245249135E-17,-1.,5.68956569482564E-17));
#46859=DIRECTION('ref_axis',(0.561410669601872,0.,0.827537346623811));
#46860=DIRECTION('center_axis',(-1.22464679915E-16,-1.,-5.47382212627E-48));
#46861=DIRECTION('ref_axis',(1.,-1.22464679915E-16,-6.703498746053E-64));
#46862=DIRECTION('center_axis',(-0.687199008140201,8.41576065696246E-17,
-0.726469216974212));
#46863=DIRECTION('ref_axis',(0.726469216974212,1.50838013754883E-32,-0.687199008140201));
#46864=DIRECTION('center_axis',(-1.22464679915E-16,-1.,1.23259516441E-32));
#46865=DIRECTION('ref_axis',(1.,-1.22464679915E-16,1.50949372274247E-48));
#46866=DIRECTION('center_axis',(1.,0.,0.));
#46867=DIRECTION('ref_axis',(0.,-1.,0.));
#46868=DIRECTION('center_axis',(0.973274002238674,-1.1919168915396E-16,
0.229646938943923));
#46869=DIRECTION('ref_axis',(0.229646938943923,-2.91124363913666E-32,-0.973274002238674));
#46870=DIRECTION('center_axis',(1.22464679915E-16,1.,-1.23259516441E-32));
#46871=DIRECTION('ref_axis',(1.,-1.22464679915E-16,1.50949372274247E-48));
#46872=DIRECTION('center_axis',(1.22464679914982E-16,1.,7.00298942658309E-29));
#46873=DIRECTION('ref_axis',(0.246934184763054,-3.02407158970066E-17,-0.969032253537211));
#46874=DIRECTION('center_axis',(-1.81298926929756E-20,-0.999999999999994,
1.08984439787114E-7));
#46875=DIRECTION('ref_axis',(0.246934184762501,-1.0560943675131E-7,-0.969032253537346));
#46876=DIRECTION('',(-1.22066246076E-16,-1.,0.));
#46877=DIRECTION('center_axis',(-1.22464679914958E-16,-1.,1.38940690218481E-28));
#46878=DIRECTION('ref_axis',(-0.287097106361984,3.51592552349981E-17,-0.957901483200948));
#46879=DIRECTION('',(-1.13288063737E-16,-1.,0.));
#46880=DIRECTION('center_axis',(1.22464679915E-16,1.,0.));
#46881=DIRECTION('ref_axis',(1.,-1.22464679915E-16,0.));
#46882=DIRECTION('center_axis',(0.,0.,1.));
#46883=DIRECTION('ref_axis',(1.,0.,0.));
#46884=DIRECTION('center_axis',(1.22464679915E-16,1.,0.));
#46885=DIRECTION('ref_axis',(1.,-1.22464679915E-16,0.));
#46886=DIRECTION('center_axis',(1.16436507708486E-16,1.,-2.6493382562289E-17));
#46887=DIRECTION('ref_axis',(-0.221864286407976,0.,-0.975077555077892));
#46888=DIRECTION('center_axis',(1.22464679915E-16,1.,5.47382212627E-48));
#46889=DIRECTION('ref_axis',(1.,-1.22464679915E-16,-6.703498746053E-64));
#46890=DIRECTION('center_axis',(-1.22464679915E-16,-1.,-7.60253073092891E-48));
#46891=DIRECTION('ref_axis',(-1.,1.22464679915E-16,9.3104149250716E-64));
#46892=DIRECTION('center_axis',(1.22464679915E-16,1.,-4.37905770102E-47));
#46893=DIRECTION('ref_axis',(1.,-1.22464679915E-16,5.3627989968473E-63));
#46894=DIRECTION('',(0.,1.,0.));
#46895=DIRECTION('center_axis',(-1.22464679915E-16,-1.,-6.16297582204E-33));
#46896=DIRECTION('ref_axis',(1.,-1.22464679915E-16,-7.54746861370013E-49));
#46897=DIRECTION('',(0.,1.,0.));
#46898=DIRECTION('center_axis',(5.9296278727138E-17,1.,6.12017248415691E-17));
#46899=DIRECTION('ref_axis',(0.718198537785833,0.,-0.695838242928838));
#46900=DIRECTION('center_axis',(1.22464679915E-16,1.,5.47382212627E-48));
#46901=DIRECTION('ref_axis',(1.,-1.22464679915E-16,-6.703498746053E-64));
#46902=DIRECTION('center_axis',(0.981560061088029,-1.66999853996006E-12,
0.191153986296036));
#46903=DIRECTION('ref_axis',(-7.15168665029376E-13,1.,1.24085926718939E-11));
#46904=DIRECTION('center_axis',(1.22464679915E-16,1.,5.47382212627E-48));
#46905=DIRECTION('ref_axis',(1.,-1.22464679915E-16,-6.703498746053E-64));
#46906=DIRECTION('center_axis',(1.22464679915E-16,1.,5.47382212627E-48));
#46907=DIRECTION('ref_axis',(1.,-1.22464679915E-16,0.));
#46908=DIRECTION('center_axis',(-1.22464679915E-16,-1.,6.16297582204E-33));
#46909=DIRECTION('ref_axis',(1.,-1.22464679915E-16,7.54746861370013E-49));
#46910=DIRECTION('center_axis',(1.22464679915E-16,1.,-1.23259516441E-32));
#46911=DIRECTION('ref_axis',(1.,-1.22464679915E-16,-1.1821919162786E-48));
#46912=DIRECTION('center_axis',(-2.24037888703029E-16,-1.,2.20413632410453E-17));
#46913=DIRECTION('ref_axis',(-0.977255721664238,2.19472257881379E-16,0.212064269679052));
#46914=DIRECTION('center_axis',(-0.458332816460024,1.75137682135009E-14,
0.888780641866047));
#46915=DIRECTION('ref_axis',(0.888780641866047,1.15648231731787E-14,0.458332816460024));
#46916=DIRECTION('center_axis',(0.212064269679051,-2.59703829076063E-17,
0.977255721664238));
#46917=DIRECTION('ref_axis',(0.977255721664238,-7.13089940857179E-32,-0.212064269679051));
#46918=DIRECTION('center_axis',(1.22464679915E-16,1.,5.47382212627E-48));
#46919=DIRECTION('ref_axis',(1.,-1.22464679915E-16,5.24998673990483E-64));
#46920=DIRECTION('center_axis',(-1.17653265936146E-16,-1.,-2.37924056871716E-17));
#46921=DIRECTION('ref_axis',(-0.198212453337067,0.,0.980159080630334));
#46922=DIRECTION('center_axis',(0.611236780892201,-7.48549167240244E-17,
0.791447785823259));
#46923=DIRECTION('ref_axis',(0.79144778582326,2.17825094235712E-31,-0.611236780892201));
#46924=DIRECTION('center_axis',(0.980159080630334,5.57379143139189E-15,
0.198212453337067));
#46925=DIRECTION('ref_axis',(0.198212453337067,-2.31296463463575E-14,-0.980159080630334));
#46926=DIRECTION('center_axis',(1.22464679915E-16,1.,5.47382212627E-48));
#46927=DIRECTION('ref_axis',(1.,-1.22464679915E-16,5.63840144221543E-64));
#46928=DIRECTION('center_axis',(-0.923879532511277,1.13142611229034E-16,
-0.382683432365114));
#46929=DIRECTION('ref_axis',(-0.382683432365114,-7.46986778962313E-32,0.923879532511277));
#46930=DIRECTION('center_axis',(-0.923879532511277,1.13142611229034E-16,
-0.382683432365115));
#46931=DIRECTION('ref_axis',(0.382683432365115,-2.77240367868488E-33,-0.923879532511276));
#46932=DIRECTION('',(-0.923879532511277,0.,-0.382683432365114));
#46933=DIRECTION('center_axis',(-0.923879532511277,1.13142611229034E-16,
-0.382683432365115));
#46934=DIRECTION('ref_axis',(0.382683432365115,2.61659610287296E-32,-0.923879532511276));
#46935=DIRECTION('center_axis',(0.923879532511277,-1.13142611229034E-16,
-0.382683432365114));
#46936=DIRECTION('ref_axis',(-0.382683432365114,-7.46986778962313E-32,-0.923879532511277));
#46937=DIRECTION('center_axis',(0.923879532511277,-1.13142611229034E-16,
-0.382683432365115));
#46938=DIRECTION('ref_axis',(0.382683432365115,2.61659610287296E-32,0.923879532511276));
#46939=DIRECTION('',(0.923879532511277,0.,-0.382683432365114));
#46940=DIRECTION('center_axis',(0.923879532511277,-1.13142611229034E-16,
-0.382683432365115));
#46941=DIRECTION('ref_axis',(0.382683432365115,-2.77240367868488E-33,0.923879532511276));
#46942=DIRECTION('center_axis',(-1.79345371456341E-17,-1.,4.32978028118705E-17));
#46943=DIRECTION('ref_axis',(0.923879532511277,0.,0.382683432365114));
#46944=DIRECTION('center_axis',(1.22464679915E-16,1.,5.47382212627E-48));
#46945=DIRECTION('ref_axis',(1.,-1.22464679915E-16,-6.703498746053E-64));
#46946=DIRECTION('center_axis',(0.382683432365114,-4.6865204053314E-17,
-0.923879532511277));
#46947=DIRECTION('ref_axis',(0.923879532511277,-1.59663321827302E-32,0.382683432365114));
#46948=DIRECTION('center_axis',(0.382683432365114,-4.6865204053314E-17,
-0.923879532511277));
#46949=DIRECTION('ref_axis',(-0.923879532511277,1.59663321827302E-32,-0.382683432365114));
#46950=DIRECTION('',(0.382683432365114,0.,-0.923879532511277));
#46951=DIRECTION('center_axis',(0.382683432365114,-4.6865204053314E-17,
-0.923879532511277));
#46952=DIRECTION('ref_axis',(0.923879532511277,-1.59663321827302E-32,0.382683432365114));
#46953=DIRECTION('center_axis',(-1.79345371456341E-17,-1.,-4.32978028118705E-17));
#46954=DIRECTION('ref_axis',(0.923879532511276,0.,-0.382683432365115));
#46955=DIRECTION('center_axis',(1.22464679915E-16,1.,5.47382212627E-48));
#46956=DIRECTION('ref_axis',(1.,-1.22464679915E-16,-6.703498746053E-64));
#46957=DIRECTION('center_axis',(-0.382683432365114,4.6865204053314E-17,
-0.923879532511277));
#46958=DIRECTION('ref_axis',(0.923879532511277,-1.59663321827302E-32,-0.382683432365114));
#46959=DIRECTION('center_axis',(-0.382683432365114,4.6865204053314E-17,
-0.923879532511277));
#46960=DIRECTION('ref_axis',(-0.923879532511277,1.59663321827302E-32,0.382683432365114));
#46961=DIRECTION('',(-0.382683432365114,0.,-0.923879532511277));
#46962=DIRECTION('center_axis',(-0.382683432365114,4.6865204053314E-17,
-0.923879532511277));
#46963=DIRECTION('ref_axis',(0.923879532511277,-1.59663321827302E-32,-0.382683432365114));
#46964=DIRECTION('center_axis',(-1.04530142769366E-16,-1.,-4.32978028118705E-17));
#46965=DIRECTION('ref_axis',(0.382683432365114,0.,-0.923879532511277));
#46966=DIRECTION('center_axis',(1.22464679915E-16,1.,5.47382212627E-48));
#46967=DIRECTION('ref_axis',(1.,-1.22464679915E-16,-6.703498746053E-64));
#46968=DIRECTION('center_axis',(-1.04530142769366E-16,-1.,4.32978028118705E-17));
#46969=DIRECTION('ref_axis',(-0.382683432365115,0.,-0.923879532511276));
#46970=DIRECTION('center_axis',(1.22464679915E-16,1.,5.47382212627E-48));
#46971=DIRECTION('ref_axis',(1.,-1.22464679915E-16,-6.703498746053E-64));
#46972=DIRECTION('center_axis',(-0.923879532511277,1.13142611229034E-16,
0.382683432365115));
#46973=DIRECTION('ref_axis',(0.382683432365115,2.61659610287296E-32,0.923879532511276));
#46974=DIRECTION('center_axis',(0.923879532511277,-1.13142611229013E-16,
-0.382683432365114));
#46975=DIRECTION('ref_axis',(1.22464679915E-16,1.,4.82508167451141E-31));
#46976=DIRECTION('',(-0.923879532511277,0.,0.382683432365114));
#46977=DIRECTION('center_axis',(-0.923879532511277,1.13142611229034E-16,
0.382683432365115));
#46978=DIRECTION('ref_axis',(0.382683432365115,-2.77240367868488E-33,0.923879532511276));
#46979=DIRECTION('center_axis',(-1.04530142769366E-16,-1.,4.32978028118705E-17));
#46980=DIRECTION('ref_axis',(0.382683432365115,0.,0.923879532511276));
#46981=DIRECTION('center_axis',(0.923879532511277,-1.13142611229034E-16,
0.382683432365115));
#46982=DIRECTION('ref_axis',(0.382683432365115,2.61659610287296E-32,-0.923879532511276));
#46983=DIRECTION('center_axis',(1.22464679915E-16,1.,5.47382212627E-48));
#46984=DIRECTION('ref_axis',(1.,-1.22464679915E-16,-6.703498746053E-64));
#46985=DIRECTION('center_axis',(-0.923879532511277,1.13142611229013E-16,
-0.382683432365114));
#46986=DIRECTION('ref_axis',(1.22464679915E-16,1.,-4.82508167451141E-31));
#46987=DIRECTION('center_axis',(0.923879532511277,-1.13142611229034E-16,
0.382683432365115));
#46988=DIRECTION('ref_axis',(0.382683432365115,-2.77240367868488E-33,-0.923879532511276));
#46989=DIRECTION('',(0.923879532511277,0.,0.382683432365114));
#46990=DIRECTION('center_axis',(-1.04530142769366E-16,-1.,-4.32978028118705E-17));
#46991=DIRECTION('ref_axis',(-0.382683432365114,0.,0.923879532511277));
#46992=DIRECTION('center_axis',(0.382683432365114,-4.6865204053314E-17,
0.923879532511277));
#46993=DIRECTION('ref_axis',(0.923879532511277,-1.59663321827302E-32,-0.382683432365114));
#46994=DIRECTION('center_axis',(1.22464679915E-16,1.,5.47382212627E-48));
#46995=DIRECTION('ref_axis',(1.,-1.22464679915E-16,-6.703498746053E-64));
#46996=DIRECTION('center_axis',(-0.382683432365114,4.68652040533673E-17,
-0.923879532511277));
#46997=DIRECTION('ref_axis',(1.79345371456341E-17,1.,4.32978028118705E-17));
#46998=DIRECTION('center_axis',(0.382683432365114,-4.6865204053314E-17,
0.923879532511277));
#46999=DIRECTION('ref_axis',(0.923879532511277,-1.59663321827302E-32,-0.382683432365114));
#47000=DIRECTION('',(0.382683432365114,0.,0.923879532511277));
#47001=DIRECTION('center_axis',(-1.79345371456341E-17,-1.,-4.32978028118705E-17));
#47002=DIRECTION('ref_axis',(-0.923879532511276,0.,0.382683432365115));
#47003=DIRECTION('center_axis',(-0.382683432365114,4.6865204053314E-17,
0.923879532511277));
#47004=DIRECTION('ref_axis',(0.923879532511277,-1.59663321827302E-32,0.382683432365114));
#47005=DIRECTION('center_axis',(1.22464679915E-16,1.,5.47382212627E-48));
#47006=DIRECTION('ref_axis',(1.,-1.22464679915E-16,-6.703498746053E-64));
#47007=DIRECTION('center_axis',(0.382683432365114,-4.68652040533673E-17,
-0.923879532511277));
#47008=DIRECTION('ref_axis',(1.79345371456341E-17,1.,-4.32978028118705E-17));
#47009=DIRECTION('center_axis',(-0.382683432365114,4.6865204053314E-17,
0.923879532511277));
#47010=DIRECTION('ref_axis',(0.923879532511277,-1.59663321827302E-32,0.382683432365114));
#47011=DIRECTION('',(-0.382683432365114,0.,0.923879532511277));
#47012=DIRECTION('center_axis',(-1.79345371456341E-17,-1.,4.32978028118705E-17));
#47013=DIRECTION('ref_axis',(-0.923879532511277,0.,-0.382683432365114));
#47014=DIRECTION('center_axis',(1.22464679915E-16,1.,5.47382212627E-48));
#47015=DIRECTION('ref_axis',(1.,-1.22464679915E-16,-6.703498746053E-64));
#47016=DIRECTION('center_axis',(-1.22464679915E-16,-1.,-5.47382212627E-48));
#47017=DIRECTION('ref_axis',(-1.,1.22464679915E-16,0.));
#47018=DIRECTION('center_axis',(1.22464679915E-16,1.,-1.23259516441E-32));
#47019=DIRECTION('ref_axis',(1.,-1.22464679915E-16,1.50949372274247E-48));
#47020=DIRECTION('',(-2.1862358377E-16,0.,1.));
#47021=DIRECTION('center_axis',(1.22464679915E-16,1.,-4.37905770102E-47));
#47022=DIRECTION('ref_axis',(1.,-1.22464679915E-16,5.3627989968473E-63));
#47023=DIRECTION('',(1.,0.,0.));
#47024=DIRECTION('center_axis',(1.22464679915E-16,1.,-6.16297582204E-33));
#47025=DIRECTION('ref_axis',(1.,-1.22464679915E-16,-5.9109595813834E-49));
#47026=DIRECTION('center_axis',(1.22464679915E-16,1.,1.23259516441E-32));
#47027=DIRECTION('ref_axis',(1.,-1.22464679915E-16,-1.50949372274247E-48));
#47028=DIRECTION('center_axis',(-2.77602545911041E-17,-1.,5.12739598421612E-17));
#47029=DIRECTION('ref_axis',(-0.879386330848967,0.,-0.476108896278982));
#47030=DIRECTION('center_axis',(-5.0552016865731E-17,-1.,-6.02936991345387E-17));
#47031=DIRECTION('ref_axis',(0.766297237624136,0.,-0.642486220560113));
#47032=DIRECTION('center_axis',(-0.642486220560114,-6.75485423398119E-15,
-0.766297237624136));
#47033=DIRECTION('ref_axis',(0.766297237624136,1.12931390012428E-29,-0.642486220560114));
#47034=DIRECTION('center_axis',(1.22464679915E-16,1.,5.47382212627E-48));
#47035=DIRECTION('ref_axis',(1.,-1.22464679915E-16,-6.703498746053E-64));
#47036=DIRECTION('center_axis',(0.980794227872242,7.97285521065847E-12,
0.195045334659643));
#47037=DIRECTION('ref_axis',(-5.58812255727995E-12,1.,-1.27592381105046E-11));
#47038=DIRECTION('center_axis',(-1.2246467991484E-16,-1.,-6.47882833291866E-29));
#47039=DIRECTION('ref_axis',(-0.926909189979645,1.13513637260957E-16,0.375285695878857));
#47040=DIRECTION('center_axis',(1.9201908781E-16,1.,1.71790773243E-16));
#47041=DIRECTION('ref_axis',(1.,-1.9201908781E-16,-3.29871075722954E-32));
#47042=DIRECTION('',(0.,1.,0.));
#47043=DIRECTION('center_axis',(-4.39408528056178E-8,0.99999999999998,1.96572411306371E-7));
#47044=DIRECTION('ref_axis',(-0.926909250500648,-1.14499965064849E-7,0.375285546399425));
#47045=DIRECTION('center_axis',(-0.103350672077944,-0.961332021496742,-0.255263360132284));
#47046=DIRECTION('ref_axis',(-0.360774156658016,0.275391983262014,-0.891067485347048));
#47047=DIRECTION('center_axis',(-0.375285695878857,4.59592426223824E-17,
-0.926909189979645));
#47048=DIRECTION('ref_axis',(0.926909189979645,-3.61589631838611E-32,-0.375285695878857));
#47049=DIRECTION('center_axis',(-4.57540623410157E-17,-1.,-5.92437539213873E-17));
#47050=DIRECTION('ref_axis',(-0.791447868317764,0.,0.611236674075818));
#47051=DIRECTION('center_axis',(-1.22464679915E-16,-1.,0.));
#47052=DIRECTION('ref_axis',(1.,-1.22464679915E-16,0.));
#47053=DIRECTION('center_axis',(-4.57540783324772E-17,-1.,-5.92437580993829E-17));
#47054=DIRECTION('ref_axis',(-0.791447785823259,0.,0.611236780892201));
#47055=DIRECTION('center_axis',(1.22464679915E-16,1.,0.));
#47056=DIRECTION('ref_axis',(1.,-1.22464679915E-16,0.));
#47057=DIRECTION('center_axis',(1.22464679914331E-16,1.,1.45068233549706E-28));
#47058=DIRECTION('ref_axis',(-0.977255721664238,1.19679309148029E-16,0.212064269679051));
#47059=DIRECTION('center_axis',(6.05558773490554E-7,-0.999999999999779,
-2.73579685865623E-7));
#47060=DIRECTION('ref_axis',(-0.0522365709531267,2.41573864176758E-7,-0.998634738357825));
#47061=DIRECTION('center_axis',(-0.522521046689147,2.55431910633826E-7,
0.852626386975452));
#47062=DIRECTION('ref_axis',(0.602897982970372,0.707106794621592,0.36947801440713));
#47063=DIRECTION('center_axis',(3.34362886570006E-17,1.,-5.45598660992754E-17));
#47064=DIRECTION('ref_axis',(-0.852626520482788,0.,-0.52252082883787));
#47065=DIRECTION('center_axis',(-0.496495443044673,-7.53189665075629E-8,
0.868039328046759));
#47066=DIRECTION('ref_axis',(0.613796700774017,0.707106513896531,0.351075473543833));
#47067=DIRECTION('center_axis',(-4.27856751109758E-7,0.999999999999565,
8.29299678606429E-7));
#47068=DIRECTION('ref_axis',(0.900769699186529,7.45562821397678E-7,-0.434297074623873));
#47069=DIRECTION('center_axis',(-0.707141467397435,0.692946912637,-0.140625464812931));
#47070=DIRECTION('ref_axis',(0.32401455277391,0.140799773673971,-0.935515896884752));
#47071=DIRECTION('center_axis',(1.22464679915E-16,1.,-1.23259516441E-32));
#47072=DIRECTION('ref_axis',(1.,-1.22464679915E-16,1.50949372274247E-48));
#47073=DIRECTION('center_axis',(1.22464679914984E-16,1.,7.84281471797691E-29));
#47074=DIRECTION('ref_axis',(0.195045334687923,-2.38861644813906E-17,-0.980794227866618));
#47075=DIRECTION('',(0.,1.,0.));
#47076=DIRECTION('center_axis',(-1.22464679914868E-16,-1.,-1.10428543166843E-28));
#47077=DIRECTION('ref_axis',(-0.766297237624135,9.38443459252164E-17,0.642486220560115));
#47078=DIRECTION('center_axis',(-2.20517453689E-16,-1.,-1.1694814189E-16));
#47079=DIRECTION('ref_axis',(1.,-2.20517453689E-16,-2.57891064632427E-32));
#47080=DIRECTION('',(0.,-1.,0.));
#47081=DIRECTION('center_axis',(1.,-1.22464679915E-16,6.12323399574E-17));
#47082=DIRECTION('ref_axis',(1.22464679915E-16,1.,7.49879891332945E-33));
#47083=DIRECTION('center_axis',(-1.,1.22464679915E-16,5.03301104497E-15));
#47084=DIRECTION('ref_axis',(-1.22464679915E-16,-1.,6.16366086630911E-31));
#47085=DIRECTION('',(1.,0.,3.62521803959E-16));
#47086=DIRECTION('center_axis',(2.17357452795E-16,-2.66186108837E-32,-1.));
#47087=DIRECTION('ref_axis',(0.,-1.,2.66186108837E-32));
#47088=DIRECTION('',(-1.,0.,0.));
#47089=DIRECTION('center_axis',(1.,-1.22464679915E-16,6.12323399574E-17));
#47090=DIRECTION('ref_axis',(-1.22464679915E-16,-1.,-7.49879891332945E-33));
#47091=DIRECTION('center_axis',(-1.,1.22464679915E-16,-9.25185853854E-17));
#47092=DIRECTION('ref_axis',(-1.22464679915E-16,-1.,-1.13302589454116E-32));
#47093=DIRECTION('',(1.,0.,0.));
#47094=DIRECTION('center_axis',(1.1936008304232E-16,1.,1.92500633904415E-17));
#47095=DIRECTION('ref_axis',(-0.159219839565945,0.,0.987243152768655));
#47096=DIRECTION('center_axis',(1.22464679915E-16,1.,5.47382212627E-48));
#47097=DIRECTION('ref_axis',(1.,-1.22464679915E-16,5.63840144221543E-64));
#47098=DIRECTION('center_axis',(0.987243152771461,1.8496896112958E-11,0.159219839548546));
#47099=DIRECTION('ref_axis',(-0.159219839548546,1.48029736616686E-14,0.987243152771461));
#47100=DIRECTION('center_axis',(1.22464679915E-16,1.,5.47382212627E-48));
#47101=DIRECTION('ref_axis',(1.,-1.22464679915E-16,0.));
#47102=DIRECTION('center_axis',(7.52478899174175E-8,0.999999999999997,1.38031989516745E-8));
#47103=DIRECTION('ref_axis',(-0.12861910970648,-4.01023408411311E-9,0.991694068056431));
#47104=DIRECTION('center_axis',(-1.22464679915E-16,-1.,0.));
#47105=DIRECTION('ref_axis',(1.,-1.22464679915E-16,0.));
#47106=DIRECTION('',(-2.19188076492E-16,0.,1.));
#47107=DIRECTION('center_axis',(-1.22464679915E-16,-1.,0.));
#47108=DIRECTION('ref_axis',(1.,-1.22464679915E-16,0.));
#47109=DIRECTION('center_axis',(-1.0413655165592E-9,-1.,-1.26007888238395E-10));
#47110=DIRECTION('ref_axis',(-0.167003259896707,4.96731596649238E-11,0.985956343447251));
#47111=DIRECTION('',(-2.17371312249E-16,0.,1.));
#47112=DIRECTION('center_axis',(0.258465262671631,0.964605492283562,0.0522680805891321));
#47113=DIRECTION('ref_axis',(0.945466832487627,-0.263697258719896,0.191196821127928));
#47114=DIRECTION('center_axis',(-1.22464679915E-16,-1.,-6.16297582204E-33));
#47115=DIRECTION('ref_axis',(1.,-1.22464679915E-16,-7.54746861370013E-49));
#47116=DIRECTION('center_axis',(2.17357452795E-16,-2.66186108837E-32,-1.));
#47117=DIRECTION('ref_axis',(1.,5.7857534586223E-48,2.17357452795E-16));
#47118=DIRECTION('center_axis',(-0.198212453337055,-3.31043063332241E-15,
0.980159080630336));
#47119=DIRECTION('ref_axis',(-0.945466832487629,0.263697258719893,-0.191196821127922));
#47120=DIRECTION('center_axis',(-2.17357452795E-16,2.66186108837E-32,1.));
#47121=DIRECTION('ref_axis',(1.,5.7857534586223E-48,2.17357452795E-16));
#47122=DIRECTION('',(-9.00454292637E-17,0.,1.));
#47123=DIRECTION('center_axis',(-2.17357452795E-16,2.66186108837E-32,1.));
#47124=DIRECTION('ref_axis',(1.,5.7857534586223E-48,2.17357452795E-16));
#47125=DIRECTION('center_axis',(1.22464679914984E-16,1.,8.09446956404351E-29));
#47126=DIRECTION('ref_axis',(-0.198212453337068,2.42740246530083E-17,0.980159080630333));
#47127=DIRECTION('',(0.,-1.,0.));
#47128=DIRECTION('center_axis',(1.,-1.22464679915E-16,6.12323399574E-17));
#47129=DIRECTION('ref_axis',(-1.22464679915E-16,-1.,-6.67366607695787E-50));
#47130=DIRECTION('',(2.17371312249E-16,0.,-1.));
#47131=DIRECTION('center_axis',(-2.17357452795E-16,2.66186108837E-32,1.));
#47132=DIRECTION('ref_axis',(-1.,-5.7857534586223E-48,-2.17357452795E-16));
#47133=DIRECTION('',(-1.29439338185998E-7,0.,0.999999999999992));
#47134=DIRECTION('center_axis',(-0.941574524866053,-0.33680470645719,6.18995477862716E-5));
#47135=DIRECTION('ref_axis',(0.257425227315659,-0.719541941796582,0.644974143929108));
#47136=DIRECTION('center_axis',(3.23815048849E-16,-3.96559063089E-32,-1.));
#47137=DIRECTION('ref_axis',(1.,1.28411792385678E-47,3.23815048849E-16));
#47138=DIRECTION('center_axis',(0.734238830876792,-8.99183234042744E-17,
-0.678891257295808));
#47139=DIRECTION('ref_axis',(-0.678891257295808,-1.51038693775819E-31,-0.734238830876792));
#47140=DIRECTION('',(-0.734238830876791,0.,0.678891257295807));
#47141=DIRECTION('center_axis',(-0.734238830876792,8.99183234042744E-17,
0.678891257295808));
#47142=DIRECTION('ref_axis',(0.678891257295807,3.46311205996404E-31,0.734238830876791));
#47143=DIRECTION('center_axis',(-0.734238830876792,8.99183234042744E-17,
0.678891257295808));
#47144=DIRECTION('ref_axis',(0.678891257295808,1.51038693775819E-31,0.734238830876792));
#47145=DIRECTION('center_axis',(1.,0.,0.));
#47146=DIRECTION('ref_axis',(0.,-1.,0.));
#47147=DIRECTION('center_axis',(-0.790681776842983,9.68305907154979E-17,
-0.612227349738987));
#47148=DIRECTION('ref_axis',(0.612227349738987,1.22226555802243E-31,-0.790681776842983));
#47149=DIRECTION('center_axis',(7.65621835198448E-17,1.,5.92823359275332E-17));
#47150=DIRECTION('ref_axis',(-0.612227349738987,0.,0.790681776842983));
#47151=DIRECTION('center_axis',(-1.22464679915E-16,-1.,-5.47382212627E-48));
#47152=DIRECTION('ref_axis',(1.,-1.22464679915E-16,-6.703498746053E-64));
#47153=DIRECTION('center_axis',(-0.991694064582439,1.21447496192053E-16,
-0.128619136492057));
#47154=DIRECTION('ref_axis',(0.128619136492057,-4.98879909760123E-32,-0.991694064582438));
#47155=DIRECTION('center_axis',(0.,0.,1.));
#47156=DIRECTION('ref_axis',(1.,0.,0.));
#47157=DIRECTION('center_axis',(2.17357452795E-16,-2.66186108837E-32,-1.));
#47158=DIRECTION('ref_axis',(1.,5.7857534586223E-48,2.17357452795E-16));
#47159=DIRECTION('center_axis',(-2.17357452795E-16,2.66186108837E-32,1.));
#47160=DIRECTION('ref_axis',(1.,5.7857534586223E-48,2.17357452795E-16));
#47161=DIRECTION('center_axis',(-1.17036010513E-14,1.43327775659E-30,-1.));
#47162=DIRECTION('ref_axis',(1.,1.98907245817996E-46,-1.17036010513E-14));
#47163=DIRECTION('center_axis',(0.,0.,1.));
#47164=DIRECTION('ref_axis',(1.,0.,0.));
#47165=DIRECTION('center_axis',(0.824331881335686,-1.00951539990962E-16,
0.566106835688784));
#47166=DIRECTION('ref_axis',(0.566106835688784,-1.17683260639136E-31,-0.824331881335686));
#47167=DIRECTION('center_axis',(1.,0.,0.));
#47168=DIRECTION('ref_axis',(0.,-1.,0.));
#47169=DIRECTION('center_axis',(0.99733341416283,-1.22138117333977E-16,
0.0729798670477863));
#47170=DIRECTION('ref_axis',(0.0729798670477863,2.52018738244318E-32,-0.99733341416283));
#47171=DIRECTION('center_axis',(8.32175728849317E-17,1.,5.71493568625004E-17));
#47172=DIRECTION('ref_axis',(-0.566106835688784,0.,0.824331881335686));
#47173=DIRECTION('center_axis',(1.22464679915E-16,1.,5.47382212627E-48));
#47174=DIRECTION('ref_axis',(1.,-1.22464679915E-16,6.49622071350503E-64));
#47175=DIRECTION('center_axis',(1.22464679915E-16,1.,5.47382212627E-48));
#47176=DIRECTION('ref_axis',(1.,-1.22464679915E-16,0.));
#47177=DIRECTION('center_axis',(0.,0.,1.));
#47178=DIRECTION('ref_axis',(1.,0.,0.));
#47179=DIRECTION('center_axis',(-1.,1.22464679915E-16,-6.12323399574E-17));
#47180=DIRECTION('ref_axis',(-6.12323399574E-17,0.,1.));
#47181=DIRECTION('',(1.5105075165E-16,1.,0.));
#47182=DIRECTION('',(-2.28870415168E-16,0.,1.));
#47183=DIRECTION('',(-7.55253758248E-17,-1.,0.));
#47184=DIRECTION('center_axis',(-1.22464679914868E-16,-1.,-1.27704300324719E-28));
#47185=DIRECTION('ref_axis',(0.718198537785833,-8.79539540451795E-17,-0.695838242928838));
#47186=DIRECTION('',(1.5105075165E-16,1.,0.));
#47187=DIRECTION('',(1.5105075165E-16,1.,0.));
#47188=DIRECTION('center_axis',(-1.22464679914988E-16,-1.,-5.97423468748921E-29));
#47189=DIRECTION('ref_axis',(0.191153986297933,-2.34096117463918E-17,-0.981560061087659));
#47190=DIRECTION('',(1.23358113847E-16,1.,0.));
#47191=DIRECTION('center_axis',(7.52094574043E-17,1.,3.8940254264E-17));
#47192=DIRECTION('ref_axis',(1.,-7.52094574043E-17,-2.92867539438092E-33));
#47193=DIRECTION('center_axis',(-1.,1.22464679915E-16,-6.12323399574E-17));
#47194=DIRECTION('ref_axis',(-6.12323399574E-17,0.,1.));
#47195=DIRECTION('',(-1.5105075165E-16,-1.,0.));
#47196=DIRECTION('',(-1.74378361673E-16,0.,1.));
#47197=DIRECTION('center_axis',(-1.22464679915E-16,-1.,3.08148791102006E-33));
#47198=DIRECTION('ref_axis',(1.,-1.22464679915E-16,-5.78241158658936E-15));
#47199=DIRECTION('',(-1.16865581539E-16,-1.,0.));
#47200=DIRECTION('center_axis',(-1.61832416815E-16,-1.,-4.68996881439E-17));
#47201=DIRECTION('ref_axis',(1.,-1.61832416815E-16,-7.58988988019714E-33));
#47202=DIRECTION('center_axis',(-1.22464679915001E-16,-1.,1.11184889946404E-29));
#47203=DIRECTION('ref_axis',(-0.11782622263506,1.44295506406073E-17,0.993034229651503));
#47204=DIRECTION('',(0.,1.,0.));
#47205=DIRECTION('center_axis',(-1.22464679915E-16,-1.,-3.08148791102E-33));
#47206=DIRECTION('ref_axis',(1.,-1.22464679915E-16,-3.77373430685006E-49));
#47207=DIRECTION('center_axis',(-1.224646799149E-16,-1.,1.07603845915075E-28));
#47208=DIRECTION('ref_axis',(-0.678891257295807,8.31402005216763E-17,-0.734238830876792));
#47209=DIRECTION('',(1.23358113847E-16,1.,0.));
#47210=DIRECTION('center_axis',(1.224646799149E-16,1.,-1.07603845915075E-28));
#47211=DIRECTION('ref_axis',(-0.678891257295809,8.31402005216765E-17,-0.73423883087679));
#47212=DIRECTION('',(2.46716227694E-16,1.,0.));
#47213=DIRECTION('center_axis',(0.678891257295808,-8.31402005216763E-17,
0.734238830876792));
#47214=DIRECTION('ref_axis',(-1.22464679914784E-16,-1.,1.83887638005312E-34));
#47215=DIRECTION('center_axis',(-1.22464679915001E-16,-1.,1.11184889946404E-29));
#47216=DIRECTION('ref_axis',(-0.11782622263506,1.44295506406073E-17,0.993034229651503));
#47217=DIRECTION('',(0.,1.,0.));
#47218=DIRECTION('',(0.,1.,0.));
#47219=DIRECTION('center_axis',(1.22464679914738E-16,1.,-8.7827755269459E-30));
#47220=DIRECTION('ref_axis',(0.999438196720723,-1.22395878855966E-16,0.0335155327516906));
#47221=DIRECTION('',(0.,1.,0.));
#47222=DIRECTION('center_axis',(-1.22464679914868E-16,-1.,-1.27704300324719E-28));
#47223=DIRECTION('ref_axis',(0.718198537785833,-8.79539540451795E-17,-0.695838242928838));
#47224=DIRECTION('',(0.,1.,0.));
#47225=DIRECTION('center_axis',(-1.22464679915E-16,-1.,-1.94567767731298E-44));
#47226=DIRECTION('ref_axis',(-2.38276793969895E-60,-1.94567767731298E-44,
1.));
#47227=DIRECTION('',(0.,1.,0.));
#47228=DIRECTION('center_axis',(1.22464679915E-16,1.,6.39482694638668E-33));
#47229=DIRECTION('ref_axis',(2.89120579329468E-15,-3.60465418990613E-31,
1.));
#47230=DIRECTION('',(0.,1.,0.));
#47231=DIRECTION('center_axis',(-2.17357452795E-16,2.66186108837E-32,1.));
#47232=DIRECTION('ref_axis',(1.,2.56447231488414E-65,2.17357452795E-16));
#47233=DIRECTION('center_axis',(-1.22464679914868E-16,-1.,-1.27704300324719E-28));
#47234=DIRECTION('ref_axis',(-0.714687205042302,8.7523939804668E-17,0.699444207173683));
#47235=DIRECTION('',(0.,-1.,0.));
#47236=DIRECTION('',(0.,1.,0.));
#47237=DIRECTION('center_axis',(-1.22464679914919E-16,-1.,-1.07732241244701E-28));
#47238=DIRECTION('ref_axis',(0.602966636474876,-7.38421161351848E-17,-0.797766403966835));
#47239=DIRECTION('',(-2.46716227694E-16,-1.,0.));
#47240=DIRECTION('center_axis',(0.678891257295808,-8.31402005216763E-17,
0.734238830876792));
#47241=DIRECTION('ref_axis',(-1.22464679914784E-16,-1.,1.83887638005312E-34));
#47242=DIRECTION('',(0.,-1.,0.));
#47243=DIRECTION('center_axis',(1.22464679914841E-16,1.,1.13501471389221E-28));
#47244=DIRECTION('ref_axis',(-0.813441648140047,9.96178710688057E-17,0.581646529321034));
#47245=DIRECTION('',(0.,-1.,0.));
#47246=DIRECTION('center_axis',(-1.16236097357E-16,-1.,-6.09147290561E-17));
#47247=DIRECTION('ref_axis',(1.,-1.16236097357E-16,-7.08049037704012E-33));
#47248=DIRECTION('center_axis',(-1.22464679915001E-16,-1.,1.11184889946404E-29));
#47249=DIRECTION('ref_axis',(-0.11782622263506,1.44295506406073E-17,0.993034229651503));
#47250=DIRECTION('',(0.,-1.,0.));
#47251=DIRECTION('center_axis',(-1.22464679915E-16,-1.,-3.08148791102E-33));
#47252=DIRECTION('ref_axis',(1.,-1.22464679915E-16,-3.77373430685006E-49));
#47253=DIRECTION('center_axis',(-1.22464679915E-16,-1.,-1.94567767731298E-44));
#47254=DIRECTION('ref_axis',(2.38276793969895E-60,1.94567767731298E-44,
-1.));
#47255=DIRECTION('center_axis',(9.4593208002E-17,1.,5.4521376634E-17));
#47256=DIRECTION('ref_axis',(1.,-9.4593208002E-17,-5.15735192049534E-33));
#47257=DIRECTION('',(0.,1.,0.));
#47258=DIRECTION('center_axis',(-1.22464679914423E-16,-1.,-8.33007499390688E-29));
#47259=DIRECTION('ref_axis',(-0.98972556641388,1.21206424693985E-16,0.142980079684982));
#47260=DIRECTION('',(0.,-1.,0.));
#47261=DIRECTION('center_axis',(-2.61334043E-16,-1.,-1.20249303974E-16));
#47262=DIRECTION('ref_axis',(1.,-2.61334043E-16,-3.14252367754614E-32));
#47263=DIRECTION('center_axis',(-2.17357452795E-16,2.66186108837E-32,1.));
#47264=DIRECTION('ref_axis',(1.,2.56447231488414E-65,2.17357452795E-16));
#47265=DIRECTION('',(1.,0.,0.));
#47266=DIRECTION('center_axis',(0.,1.,0.));
#47267=DIRECTION('ref_axis',(-0.10172047258397,0.,0.994813020349701));
#47268=DIRECTION('center_axis',(0.581646529321033,-7.12311560368041E-17,
0.813441648140047));
#47269=DIRECTION('ref_axis',(0.813441648140047,-2.80119922649672E-32,-0.581646529321033));
#47270=DIRECTION('center_axis',(1.69872863391202E-17,1.,4.23293596334453E-17));
#47271=DIRECTION('ref_axis',(-0.927892968287493,0.,0.372846670097274));
#47272=DIRECTION('center_axis',(-1.22464679915E-16,-1.,-5.47382212627E-48));
#47273=DIRECTION('ref_axis',(1.,-1.22464679915E-16,-6.703498746053E-64));
#47274=DIRECTION('center_axis',(0.,0.,1.));
#47275=DIRECTION('ref_axis',(1.,0.,0.));
#47276=DIRECTION('center_axis',(1.,-1.22464679915E-16,6.12323399574E-17));
#47277=DIRECTION('ref_axis',(-1.22464679915E-16,-1.,-7.49879891332945E-33));
#47278=DIRECTION('center_axis',(0.,0.,1.));
#47279=DIRECTION('ref_axis',(1.,0.,0.));
#47280=DIRECTION('center_axis',(-1.,1.22464679915E-16,-6.12323399574E-17));
#47281=DIRECTION('ref_axis',(-1.22464679915E-16,-1.,-7.49879891332945E-33));
#47282=DIRECTION('center_axis',(-1.,1.22464679915E-16,-6.12323399574E-17));
#47283=DIRECTION('ref_axis',(1.22464679915E-16,1.,7.49879891332945E-33));
#47284=DIRECTION('',(1.,0.,2.89652532403E-16));
#47285=DIRECTION('center_axis',(1.22464679915E-16,1.,5.47382212627E-48));
#47286=DIRECTION('ref_axis',(1.,-1.22464679915E-16,0.));
#47287=DIRECTION('center_axis',(-1.22464679915E-16,-1.,-3.08148791102E-33));
#47288=DIRECTION('ref_axis',(1.,-1.22464679915E-16,-3.77373430685006E-49));
#47289=DIRECTION('',(-1.74378361673E-16,0.,1.));
#47290=DIRECTION('center_axis',(-0.62218556523187,0.249390626342792,-0.742084522079155));
#47291=DIRECTION('ref_axis',(0.160230040961959,0.968402971645766,0.191107348055953));
#47292=DIRECTION('center_axis',(0.,1.,0.));
#47293=DIRECTION('ref_axis',(0.751205410155072,0.,0.660068505349066));
#47294=DIRECTION('center_axis',(-0.991694064582439,1.21447496192053E-16,
0.128619136492057));
#47295=DIRECTION('ref_axis',(0.128619136492057,-4.98879909760123E-32,0.991694064582438));
#47296=DIRECTION('center_axis',(-2.17357452795E-16,2.66186108837E-32,1.));
#47297=DIRECTION('ref_axis',(1.,5.7857534586223E-48,2.17357452795E-16));
#47298=DIRECTION('center_axis',(1.22464679915E-16,1.,5.47382212627E-48));
#47299=DIRECTION('ref_axis',(1.,-1.22464679915E-16,-6.703498746053E-64));
#47300=DIRECTION('center_axis',(1.22464679915E-16,1.,5.47382212627E-48));
#47301=DIRECTION('ref_axis',(1.,-1.22464679915E-16,0.));
#47302=DIRECTION('center_axis',(1.22464679915E-16,1.,5.47382212627E-48));
#47303=DIRECTION('ref_axis',(1.,-1.22464679915E-16,0.));
#47304=DIRECTION('center_axis',(-1.22464679915E-16,-1.,-7.60253073092891E-48));
#47305=DIRECTION('ref_axis',(1.,-1.22464679915E-16,-9.3104149250716E-64));
#47306=DIRECTION('',(1.16865581539E-16,1.,0.));
#47307=DIRECTION('center_axis',(1.22464679915E-16,1.,1.94578320706031E-44));
#47308=DIRECTION('ref_axis',(-2.38289717636624E-60,-1.94578320706031E-44,
1.));
#47309=DIRECTION('center_axis',(-1.22464679915E-16,-1.,6.16297582204E-33));
#47310=DIRECTION('ref_axis',(1.,-1.22464679915E-16,7.54746861370013E-49));
#47311=DIRECTION('center_axis',(0.,0.,1.));
#47312=DIRECTION('ref_axis',(1.,0.,0.));
#47313=DIRECTION('center_axis',(-2.17357452795E-16,2.66186108837E-32,1.));
#47314=DIRECTION('ref_axis',(1.,5.7857534586223E-48,2.17357452795E-16));
#47315=DIRECTION('center_axis',(1.69872863391202E-17,1.,4.23293596334453E-17));
#47316=DIRECTION('ref_axis',(0.928056183869048,0.,-0.37244022283102));
#47317=DIRECTION('center_axis',(1.22464679914985E-16,1.,-5.43497430306078E-29));
#47318=DIRECTION('ref_axis',(-0.269603455472075,3.30169008783092E-17,-0.962971430935268));
#47319=DIRECTION('center_axis',(0.,-1.,0.));
#47320=DIRECTION('ref_axis',(-0.269603444240349,0.,-0.962971434079818));
#47321=DIRECTION('center_axis',(2.17357452795E-16,-2.66186108836794E-32,
-1.));
#47322=DIRECTION('ref_axis',(5.78575345861782E-48,1.,-2.66186108836794E-32));
#47323=DIRECTION('center_axis',(-2.17357452795E-16,2.66186108837E-32,1.));
#47324=DIRECTION('ref_axis',(1.,5.7857534586223E-48,2.17357452795E-16));
#47325=DIRECTION('',(0.,0.,1.));
#47326=DIRECTION('center_axis',(0.,1.,0.));
#47327=DIRECTION('ref_axis',(0.642923934113106,0.,0.765930032669124));
#47328=DIRECTION('center_axis',(9.19369336238712E-17,1.,5.29776121060009E-17));
#47329=DIRECTION('ref_axis',(-0.499277443708891,0.,0.86644217014381));
#47330=DIRECTION('center_axis',(-4.29367103357466E-45,-1.,7.25136572506882E-31));
#47331=DIRECTION('ref_axis',(-1.,0.,-5.9211894646675E-15));
#47332=DIRECTION('center_axis',(1.,0.,0.));
#47333=DIRECTION('ref_axis',(0.,-1.,0.));
#47334=DIRECTION('center_axis',(-0.687199008140201,8.41576065696246E-17,
-0.726469216974212));
#47335=DIRECTION('ref_axis',(0.726469216974212,1.50838013754883E-32,-0.687199008140201));
#47336=DIRECTION('center_axis',(-0.827537346623811,1.01344096271977E-16,
0.561410669601872));
#47337=DIRECTION('ref_axis',(0.561410669601872,-5.47362952277333E-32,0.827537346623811));
#47338=DIRECTION('center_axis',(1.22464679915E-16,1.,-1.23259516441E-32));
#47339=DIRECTION('ref_axis',(1.,-1.22464679915E-16,1.50949372274247E-48));
#47340=DIRECTION('center_axis',(1.22464679914912E-16,1.,8.35596805204809E-29));
#47341=DIRECTION('ref_axis',(-0.726469216974212,8.89668201247259E-17,0.687199008140201));
#47342=DIRECTION('',(0.,1.,0.));
#47343=DIRECTION('',(0.,1.,0.));
#47344=DIRECTION('center_axis',(-1.22464679914998E-16,-1.,-1.73663083545565E-29));
#47345=DIRECTION('ref_axis',(-0.095298509688002,1.16707014853003E-17,0.99544874004202));
#47346=DIRECTION('center_axis',(1.22464679915E-16,1.,0.));
#47347=DIRECTION('ref_axis',(1.,-1.22464679915E-16,0.));
#47348=DIRECTION('center_axis',(1.68490994230906E-17,1.,4.21844451941189E-17));
#47349=DIRECTION('ref_axis',(0.928663912412966,0.,-0.370922279974987));
#47350=DIRECTION('center_axis',(1.22464679915E-16,1.,5.47382212627E-48));
#47351=DIRECTION('ref_axis',(1.,-1.22464679915E-16,-6.703498746053E-64));
#47352=DIRECTION('center_axis',(-2.17357452795E-16,2.66186108837E-32,1.));
#47353=DIRECTION('ref_axis',(1.,5.7857534586223E-48,2.17357452795E-16));
#47354=DIRECTION('',(0.,0.,-1.));
#47355=DIRECTION('center_axis',(2.17357452795E-16,-5.59737441582E-15,-1.));
#47356=DIRECTION('ref_axis',(1.,1.21663104536254E-30,2.17357452795E-16));
#47357=DIRECTION('center_axis',(3.17795218513E-15,-3.89186897136E-31,-1.));
#47358=DIRECTION('ref_axis',(1.,1.11597938503332E-46,3.17795218513E-15));
#47359=DIRECTION('center_axis',(2.68354439599323E-46,1.,1.81284143127026E-31));
#47360=DIRECTION('ref_axis',(-1.,0.,1.97372982155583E-15));
#47361=DIRECTION('center_axis',(-1.22464679915E-16,-1.,-5.47382212627E-48));
#47362=DIRECTION('ref_axis',(1.,-1.22464679915E-16,-6.703498746053E-64));
#47363=DIRECTION('center_axis',(-0.904759192693671,1.1080104493296E-16,
0.425923471102845));
#47364=DIRECTION('ref_axis',(0.425923471102845,3.65487816993661E-32,0.904759192693671));
#47365=DIRECTION('center_axis',(1.0293130162049E-16,1.,-4.48396705262131E-17));
#47366=DIRECTION('ref_axis',(-0.399377187820903,0.,-0.916786704663777));
#47367=DIRECTION('center_axis',(1.22464679915E-16,1.,5.47382212627E-48));
#47368=DIRECTION('ref_axis',(1.,-1.22464679915E-16,-6.703498746053E-64));
#47369=DIRECTION('center_axis',(-0.916786704663777,1.12273990336973E-16,
0.399377187820903));
#47370=DIRECTION('ref_axis',(0.399377187820903,3.93858763528754E-32,0.916786704663777));
#47371=DIRECTION('center_axis',(1.0293130162049E-16,1.,-4.48396705262131E-17));
#47372=DIRECTION('ref_axis',(0.399377187820903,0.,0.916786704663777));
#47373=DIRECTION('center_axis',(-1.22464679915E-16,-1.,-5.47382212627E-48));
#47374=DIRECTION('ref_axis',(1.,-1.22464679915E-16,-6.703498746053E-64));
#47375=DIRECTION('center_axis',(-2.17357452795E-16,2.66186108837E-32,1.));
#47376=DIRECTION('ref_axis',(1.,5.7857534586223E-48,2.17357452795E-16));
#47377=DIRECTION('center_axis',(-2.17357452795E-16,2.66186108835898E-32,
1.));
#47378=DIRECTION('ref_axis',(5.78575345859834E-48,1.,-2.66186108835898E-32));
#47379=DIRECTION('',(0.,0.,1.));
#47380=DIRECTION('center_axis',(-3.47250861231E-16,-5.79129605623E-15,1.));
#47381=DIRECTION('ref_axis',(1.,-2.01103254316956E-30,3.47250861231E-16));
#47382=DIRECTION('center_axis',(1.22464679915E-16,1.,5.47382212627E-48));
#47383=DIRECTION('ref_axis',(1.,-1.22464679915E-16,0.));
#47384=DIRECTION('center_axis',(1.22464679915E-16,1.,0.));
#47385=DIRECTION('ref_axis',(1.,-1.22464679915E-16,0.));
#47386=DIRECTION('',(-0.687199008140201,0.,-0.726469216974212));
#47387=DIRECTION('center_axis',(1.22464679915E-16,1.,0.));
#47388=DIRECTION('ref_axis',(1.,-1.22464679915E-16,0.));
#47389=DIRECTION('center_axis',(0.,0.957608642877659,-0.288072364321897));
#47390=DIRECTION('ref_axis',(0.,-0.288072364321899,-0.957608642877659));
#47391=DIRECTION('center_axis',(-0.890715300400791,1.09081164158974E-16,
0.454561605980893));
#47392=DIRECTION('ref_axis',(0.454561605980893,-9.65132779741589E-32,0.890715300400791));
#47393=DIRECTION('center_axis',(-1.22464679915E-16,-1.,-5.47382212627E-48));
#47394=DIRECTION('ref_axis',(1.,-1.22464679915E-16,-6.703498746053E-64));
#47395=DIRECTION('center_axis',(-1.,1.2919345348203E-16,-3.88645861503935E-17));
#47396=DIRECTION('ref_axis',(0.,0.288072364321903,0.957608642877657));
#47397=DIRECTION('center_axis',(1.178693242477E-16,1.,-2.32734068666895E-17));
#47398=DIRECTION('ref_axis',(-0.193710935823942,0.,-0.981058649287703));
#47399=DIRECTION('center_axis',(1.22464679915E-16,1.,5.47382212627E-48));
#47400=DIRECTION('ref_axis',(1.,-1.22464679915E-16,6.22660996643423E-64));
#47401=DIRECTION('center_axis',(-0.684308456885095,0.684308456885093,0.25188066950658));
#47402=DIRECTION('ref_axis',(-0.178106529457909,0.178106529457906,-0.967758300573505));
#47403=DIRECTION('center_axis',(0.938446715307966,-1.14926576606996E-16,
-0.345424032932987));
#47404=DIRECTION('ref_axis',(0.345424032932987,5.96953449650393E-32,0.938446715307966));
#47405=DIRECTION('center_axis',(1.22464679915E-16,1.,3.08148791102E-33));
#47406=DIRECTION('ref_axis',(1.,-1.22464679915E-16,-3.77373430685006E-49));
#47407=DIRECTION('center_axis',(1.178693242477E-16,1.,-2.32734068666895E-17));
#47408=DIRECTION('ref_axis',(-0.193710935823942,0.,-0.981058649287703));
#47409=DIRECTION('center_axis',(1.22464679915E-16,1.,5.47382212627E-48));
#47410=DIRECTION('ref_axis',(1.,-1.22464679915E-16,6.22660996643423E-64));
#47411=DIRECTION('center_axis',(1.22464679915E-16,1.,7.60253073092891E-48));
#47412=DIRECTION('ref_axis',(1.,-1.22464679915E-16,-9.3104149250716E-64));
#47413=DIRECTION('',(-1.38777878078E-16,-1.,0.));
#47414=DIRECTION('center_axis',(-1.22464679914586E-16,-1.,-1.3947821589454E-28));
#47415=DIRECTION('ref_axis',(-0.947590338356885,1.16046347476986E-16,0.319487950715961));
#47416=DIRECTION('',(0.,-1.,0.));
#47417=DIRECTION('center_axis',(-1.22464679914973E-16,-1.,1.28029659727041E-28));
#47418=DIRECTION('ref_axis',(-0.207931718074914,2.54642912980895E-17,-0.978143343594595));
#47419=DIRECTION('',(1.42793958151E-16,1.,0.));
#47420=DIRECTION('center_axis',(-1.22464679914586E-16,-1.,-1.3947821589454E-28));
#47421=DIRECTION('ref_axis',(-0.947590338356885,1.16046347476986E-16,0.319487950715961));
#47422=DIRECTION('center_axis',(1.22464679914899E-16,1.,-1.21650294976139E-28));
#47423=DIRECTION('ref_axis',(-0.638858327474962,7.82375805850953E-17,-0.769324403236954));
#47424=DIRECTION('center_axis',(-6.13428128073E-17,-1.,3.67652253532E-18));
#47425=DIRECTION('ref_axis',(1.,-6.13428128073E-17,2.25528233665955E-34));
#47426=DIRECTION('',(0.,-1.,0.));
#47427=DIRECTION('center_axis',(0.,1.,0.));
#47428=DIRECTION('ref_axis',(-0.998195841446114,0.,-0.0600421695118078));
#47429=DIRECTION('center_axis',(0.687199008140201,-8.41576065696246E-17,
0.726469216974212));
#47430=DIRECTION('ref_axis',(0.726469216974212,1.50838013754883E-32,-0.687199008140201));
#47431=DIRECTION('center_axis',(0.687199008140201,-8.41576065697951E-17,
0.726469216974212));
#47432=DIRECTION('ref_axis',(5.78330237622164E-17,1.,6.11379105471828E-17));
#47433=DIRECTION('',(-0.687199008140201,0.,-0.726469216974212));
#47434=DIRECTION('center_axis',(-0.726469216974212,8.89668201247259E-17,
0.687199008140201));
#47435=DIRECTION('ref_axis',(1.22464679914833E-16,1.,-2.7960247294612E-34));
#47436=DIRECTION('',(-0.687199008140201,0.,-0.726469216974212));
#47437=DIRECTION('center_axis',(0.687199008140201,-8.41576065697951E-17,
0.726469216974212));
#47438=DIRECTION('ref_axis',(-5.78330237622164E-17,-1.,-6.11379105471828E-17));
#47439=DIRECTION('',(-0.687199008140201,0.,-0.726469216974212));
#47440=DIRECTION('center_axis',(0.678892491799354,-1.68130604497259E-6,
0.734237689427366));
#47441=DIRECTION('ref_axis',(0.519185258239941,0.70710677855387,-0.480048613527311));
#47442=DIRECTION('center_axis',(0.734238830876792,-8.99183234042744E-17,
-0.678891257295808));
#47443=DIRECTION('ref_axis',(0.678891257295808,1.51038693775819E-31,0.734238830876792));
#47444=DIRECTION('',(0.734238830876791,0.,-0.678891257295807));
#47445=DIRECTION('center_axis',(0.734238830876792,-8.99183234042744E-17,
-0.678891257295808));
#47446=DIRECTION('ref_axis',(0.678891257295808,1.51038693775819E-31,0.734238830876792));
#47447=DIRECTION('center_axis',(-6.60215246509141E-17,-1.,6.10447636300053E-17));
#47448=DIRECTION('ref_axis',(-0.678891257295808,0.,-0.734238830876791));
#47449=DIRECTION('center_axis',(-1.22464679915E-16,-1.,-5.47382212627E-48));
#47450=DIRECTION('ref_axis',(1.,-1.22464679915E-16,-6.703498746053E-64));
#47451=DIRECTION('center_axis',(0.790681776842983,-9.68305907154979E-17,
0.612227349738987));
#47452=DIRECTION('ref_axis',(0.612227349738987,1.22226555802243E-31,-0.790681776842983));
#47453=DIRECTION('center_axis',(-1.20438761132693E-16,-1.,-1.56204720894266E-17));
#47454=DIRECTION('ref_axis',(-0.128619136492057,0.,0.991694064582438));
#47455=DIRECTION('center_axis',(1.22464679915E-16,1.,5.47382212627E-48));
#47456=DIRECTION('ref_axis',(1.,-1.22464679915E-16,-6.703498746053E-64));
#47457=DIRECTION('center_axis',(0.991694064582439,-1.21447496192053E-16,
0.128619136492057));
#47458=DIRECTION('ref_axis',(0.128619136492057,-7.10548517584315E-33,-0.991694064582438));
#47459=DIRECTION('center_axis',(-1.20438761132693E-16,-1.,-1.56204720894266E-17));
#47460=DIRECTION('ref_axis',(0.128619136492057,0.,-0.991694064582438));
#47461=DIRECTION('center_axis',(-1.22464679915E-16,-1.,-5.47382212627E-48));
#47462=DIRECTION('ref_axis',(1.,-1.22464679915E-16,-6.703498746053E-64));
#47463=DIRECTION('center_axis',(-2.17357452795E-16,2.66186108837E-32,1.));
#47464=DIRECTION('ref_axis',(1.,5.7857534586223E-48,2.17357452795E-16));
#47465=DIRECTION('center_axis',(-2.17357452795E-16,2.66186108837E-32,1.));
#47466=DIRECTION('ref_axis',(-1.,-5.7857534586223E-48,-2.17357452795E-16));
#47467=DIRECTION('',(-5.89048887673E-17,0.,1.));
#47468=DIRECTION('center_axis',(5.70383201187E-15,-6.98517961621E-31,1.));
#47469=DIRECTION('ref_axis',(1.,-5.48892443580096E-47,-5.70383201187E-15));
#47470=DIRECTION('center_axis',(-0.734238830876792,8.99183234042744E-17,
0.678891257295808));
#47471=DIRECTION('ref_axis',(0.678891257295807,3.46311205996404E-31,0.734238830876791));
#47472=DIRECTION('center_axis',(-8.32175728849317E-17,-1.,-5.71493568625004E-17));
#47473=DIRECTION('ref_axis',(-0.566106835688784,0.,0.824331881335687));
#47474=DIRECTION('center_axis',(-0.824331881335686,1.00951539990962E-16,
-0.566106835688784));
#47475=DIRECTION('ref_axis',(0.566106835688784,-1.17683260639136E-31,-0.824331881335686));
#47476=DIRECTION('center_axis',(-1.22464679915E-16,-1.,-5.47382212627E-48));
#47477=DIRECTION('ref_axis',(1.,-1.22464679915E-16,-6.703498746053E-64));
#47478=DIRECTION('center_axis',(-1.07341775839004E-43,-1.,3.62568286252829E-30));
#47479=DIRECTION('ref_axis',(1.,0.,2.96059473233375E-14));
#47480=DIRECTION('center_axis',(-1.22464679915E-16,-1.,-5.47382212627E-48));
#47481=DIRECTION('ref_axis',(1.,-1.22464679915E-16,-6.703498746053E-64));
#47482=DIRECTION('center_axis',(-0.99733341416283,1.22138117333977E-16,
-0.0729798670477863));
#47483=DIRECTION('ref_axis',(0.0729798670477863,2.52018738244318E-32,-0.99733341416283));
#47484=DIRECTION('center_axis',(-1.21812425560124E-16,-1.,-8.91362356450131E-18));
#47485=DIRECTION('ref_axis',(-0.0729798670477876,0.,0.99733341416283));
#47486=DIRECTION('center_axis',(-1.22464679915E-16,-1.,-5.47382212627E-48));
#47487=DIRECTION('ref_axis',(1.,-1.22464679915E-16,5.9677926224237E-64));
#47488=DIRECTION('center_axis',(-7.91623497736024E-17,-1.,-5.85483919904324E-17));
#47489=DIRECTION('ref_axis',(0.594634643326775,0.,-0.803996045360696));
#47490=DIRECTION('center_axis',(-1.22464679915E-16,-1.,-5.47382212627E-48));
#47491=DIRECTION('ref_axis',(1.,-1.22464679915E-16,-6.703498746053E-64));
#47492=DIRECTION('center_axis',(0.803996045360697,-9.84611183477626E-17,
0.594634643326775));
#47493=DIRECTION('ref_axis',(0.594634643326775,4.97302608069436E-32,-0.803996045360697));
#47494=DIRECTION('center_axis',(-7.91623497736024E-17,-1.,-5.85483919904324E-17));
#47495=DIRECTION('ref_axis',(-0.594634643326775,0.,0.803996045360696));
#47496=DIRECTION('center_axis',(1.22464679915E-16,1.,5.47382212627E-48));
#47497=DIRECTION('ref_axis',(1.,-1.22464679915E-16,-6.703498746053E-64));
#47498=DIRECTION('center_axis',(0.766648861207372,2.15189723830724E-8,0.642066603717589));
#47499=DIRECTION('ref_axis',(-0.454009649462123,-0.707106763017885,0.542102632247482));
#47500=DIRECTION('center_axis',(-0.204326481649494,0.26766241396516,-0.941598386281052));
#47501=DIRECTION('ref_axis',(-0.591685618293079,0.732523927752735,0.336625644262053));
#47502=DIRECTION('center_axis',(-0.198845429179661,-2.66706420366427E-7,
-0.980030864460036));
#47503=DIRECTION('ref_axis',(0.692986505330404,-0.707106783433054,-0.140604766110239));
#47504=DIRECTION('center_axis',(-0.988161317760145,-0.0726194459501342,
-0.135142984103609));
#47505=DIRECTION('ref_axis',(0.140217557783907,-0.0700183990770855,-0.987641868431973));
#47506=DIRECTION('center_axis',(0.734238830876792,-8.991832340449E-17,-0.678891257295808));
#47507=DIRECTION('ref_axis',(6.6021524650914E-17,1.,-6.10447636300053E-17));
#47508=DIRECTION('',(-0.734238830876791,0.,0.678891257295807));
#47509=DIRECTION('center_axis',(-0.734238784116523,6.88429683969821E-8,
0.678891307868266));
#47510=DIRECTION('ref_axis',(0.480048418882853,-0.707107065263036,0.519185047726887));
#47511=DIRECTION('center_axis',(0.911344426846927,1.14523576333168E-7,-0.411644671598009));
#47512=DIRECTION('ref_axis',(0.291076971310159,-0.707106395458268,0.644418142416025));
#47513=DIRECTION('center_axis',(-2.17357452795E-16,2.66186108837E-32,1.));
#47514=DIRECTION('ref_axis',(1.,5.7857534586223E-48,2.17357452795E-16));
#47515=DIRECTION('',(0.,0.,-1.));
#47516=DIRECTION('center_axis',(-0.815922427322792,1.0845679086032E-6,-0.578161389743822));
#47517=DIRECTION('ref_axis',(0.408841377131885,-0.707071904207434,-0.576973180161242));
#47518=DIRECTION('center_axis',(0.734238830876792,-8.99183234042744E-17,
-0.678891257295808));
#47519=DIRECTION('ref_axis',(-0.678891257295808,-1.51038693775819E-31,-0.734238830876792));
#47520=DIRECTION('',(-0.734238830876791,0.,0.678891257295807));
#47521=DIRECTION('center_axis',(-2.19931778314037E-16,-1.,1.97757654230408E-17));
#47522=DIRECTION('ref_axis',(-0.980030917502135,2.19472257881379E-16,0.198845167756028));
#47523=DIRECTION('center_axis',(-1.22464679915E-16,-1.,-5.47382212627E-48));
#47524=DIRECTION('ref_axis',(1.,-1.22464679915E-16,5.24998673990483E-64));
#47525=DIRECTION('center_axis',(-1.00613328137095E-16,-1.,-4.6888561789305E-17));
#47526=DIRECTION('ref_axis',(4.11834732982896E-10,0.,1.));
#47527=DIRECTION('center_axis',(1.22464679915E-16,1.,5.47382212627E-48));
#47528=DIRECTION('ref_axis',(1.,-1.22464679915E-16,5.63840144221543E-64));
#47529=DIRECTION('center_axis',(-0.923879532511277,1.13142611229013E-16,
-0.382683432365114));
#47530=DIRECTION('ref_axis',(-1.22464679915E-16,-1.,-1.95419172973166E-31));
#47531=DIRECTION('center_axis',(0.923879532511277,-1.13142611229034E-16,
0.382683432365115));
#47532=DIRECTION('ref_axis',(0.382683432365115,2.61659610287296E-32,-0.923879532511276));
#47533=DIRECTION('',(0.923879532511277,0.,0.382683432365114));
#47534=DIRECTION('center_axis',(0.923879532511277,-1.13142611229034E-16,
0.382683432365115));
#47535=DIRECTION('ref_axis',(0.382683432365115,-2.77240367868488E-33,-0.923879532511276));
#47536=DIRECTION('center_axis',(0.923879532511277,-1.13142611229013E-16,
-0.382683432365114));
#47537=DIRECTION('ref_axis',(-1.22464679915E-16,-1.,1.95419172973166E-31));
#47538=DIRECTION('',(-0.923879532511277,0.,0.382683432365114));
#47539=DIRECTION('center_axis',(-0.923879532511277,1.13142611229034E-16,
0.382683432365115));
#47540=DIRECTION('ref_axis',(0.382683432365115,2.61659610287296E-32,0.923879532511276));
#47541=DIRECTION('center_axis',(0.382683432365114,-4.68652040533673E-17,
-0.923879532511277));
#47542=DIRECTION('ref_axis',(-1.79345371456341E-17,-1.,4.32978028118705E-17));
#47543=DIRECTION('',(-0.382683432365114,0.,0.923879532511277));
#47544=DIRECTION('center_axis',(-0.382683432365114,4.68652040533673E-17,
-0.923879532511277));
#47545=DIRECTION('ref_axis',(-1.79345371456341E-17,-1.,-4.32978028118705E-17));
#47546=DIRECTION('center_axis',(0.382683432365114,-4.6865204053314E-17,
0.923879532511277));
#47547=DIRECTION('ref_axis',(0.923879532511277,-1.59663321827302E-32,-0.382683432365114));
#47548=DIRECTION('',(0.382683432365114,0.,0.923879532511277));
#47549=DIRECTION('center_axis',(-1.04530142769366E-16,-1.,-4.32978028118705E-17));
#47550=DIRECTION('ref_axis',(0.382683432365114,0.,-0.923879532511277));
#47551=DIRECTION('center_axis',(-1.22464679915E-16,-1.,-5.47382212627E-48));
#47552=DIRECTION('ref_axis',(1.,-1.22464679915E-16,-6.703498746053E-64));
#47553=DIRECTION('center_axis',(-1.04530142769366E-16,-1.,4.32978028118705E-17));
#47554=DIRECTION('ref_axis',(-0.382683432365115,0.,-0.923879532511276));
#47555=DIRECTION('center_axis',(0.923879532511277,-1.13142611229034E-16,
-0.382683432365115));
#47556=DIRECTION('ref_axis',(0.382683432365115,2.61659610287296E-32,0.923879532511276));
#47557=DIRECTION('center_axis',(-1.22464679915E-16,-1.,-5.47382212627E-48));
#47558=DIRECTION('ref_axis',(1.,-1.22464679915E-16,-6.703498746053E-64));
#47559=DIRECTION('center_axis',(0.923879532511277,-1.13142611229034E-16,
-0.382683432365114));
#47560=DIRECTION('ref_axis',(0.382683432365114,7.46986778962313E-32,0.923879532511277));
#47561=DIRECTION('center_axis',(0.923879532511277,-1.13142611229034E-16,
-0.382683432365115));
#47562=DIRECTION('ref_axis',(0.382683432365115,-2.77240367868488E-33,0.923879532511276));
#47563=DIRECTION('',(0.923879532511277,0.,-0.382683432365114));
#47564=DIRECTION('center_axis',(-1.04530142769366E-16,-1.,4.32978028118705E-17));
#47565=DIRECTION('ref_axis',(0.382683432365115,0.,0.923879532511276));
#47566=DIRECTION('center_axis',(-1.22464679915E-16,-1.,-5.47382212627E-48));
#47567=DIRECTION('ref_axis',(1.,-1.22464679915E-16,-6.703498746053E-64));
#47568=DIRECTION('center_axis',(-0.923879532511277,1.13142611229034E-16,
-0.382683432365115));
#47569=DIRECTION('ref_axis',(0.382683432365115,2.61659610287296E-32,-0.923879532511276));
#47570=DIRECTION('center_axis',(-0.923879532511277,1.13142611229034E-16,
-0.382683432365114));
#47571=DIRECTION('ref_axis',(0.382683432365114,7.46986778962313E-32,-0.923879532511277));
#47572=DIRECTION('',(-0.923879532511277,0.,-0.382683432365114));
#47573=DIRECTION('center_axis',(-0.382683432365114,4.6865204053314E-17,
-0.923879532511277));
#47574=DIRECTION('ref_axis',(0.923879532511277,-1.59663321827302E-32,-0.382683432365114));
#47575=DIRECTION('',(-0.382683432365114,0.,-0.923879532511277));
#47576=DIRECTION('center_axis',(0.382683432365114,-4.6865204053314E-17,
-0.923879532511277));
#47577=DIRECTION('ref_axis',(0.923879532511277,-1.59663321827302E-32,0.382683432365114));
#47578=DIRECTION('',(0.382683432365114,0.,-0.923879532511277));
#47579=DIRECTION('center_axis',(0.382683432365114,-4.6865204053314E-17,
-0.923879532511277));
#47580=DIRECTION('ref_axis',(0.923879532511277,-1.59663321827302E-32,0.382683432365114));
#47581=DIRECTION('center_axis',(-1.79345371456341E-17,-1.,4.32978028118705E-17));
#47582=DIRECTION('ref_axis',(-0.923879532511277,0.,-0.382683432365114));
#47583=DIRECTION('center_axis',(-1.22464679915E-16,-1.,-5.47382212627E-48));
#47584=DIRECTION('ref_axis',(1.,-1.22464679915E-16,-6.703498746053E-64));
#47585=DIRECTION('center_axis',(-1.22464679915E-16,-1.,-5.47382212627E-48));
#47586=DIRECTION('ref_axis',(-1.,1.22464679915E-16,0.));
#47587=DIRECTION('',(-0.734238830876791,0.,0.678891257295807));
#47588=DIRECTION('center_axis',(-1.22464679915E-16,-1.,0.));
#47589=DIRECTION('ref_axis',(1.,-1.22464679915E-16,0.));
#47590=DIRECTION('center_axis',(1.22464679915E-16,1.,1.23259516441E-32));
#47591=DIRECTION('ref_axis',(1.,-1.22464679915E-16,-1.50949372274247E-48));
#47592=DIRECTION('center_axis',(-1.22464679915E-16,-1.,0.));
#47593=DIRECTION('ref_axis',(1.,-1.22464679915E-16,0.));
#47594=DIRECTION('',(1.,0.,4.75520106567E-17));
#47595=DIRECTION('center_axis',(-1.22464679915E-16,-1.,1.54074395551E-33));
#47596=DIRECTION('ref_axis',(1.,-1.22464679915E-16,1.88686715342503E-49));
#47597=DIRECTION('center_axis',(-1.22464679915E-16,-1.,0.));
#47598=DIRECTION('ref_axis',(1.,-1.22464679915E-16,0.));
#47599=DIRECTION('center_axis',(-5.46401789901627E-17,-1.,-6.08764557973899E-17));
#47600=DIRECTION('ref_axis',(-0.744196935834912,0.,0.667960268798922));
#47601=DIRECTION('center_axis',(-1.22464679915E-16,-1.,0.));
#47602=DIRECTION('ref_axis',(1.,-1.22464679915E-16,0.));
#47603=DIRECTION('center_axis',(-1.24261220950731E-7,-0.999999999999986,
-1.11355973133144E-7));
#47604=DIRECTION('ref_axis',(0.721616554826204,-1.66759910844075E-7,0.692292963853261));
#47605=DIRECTION('center_axis',(-0.884316205578325,-0.0178356349302338,
-0.466547681033985));
#47606=DIRECTION('ref_axis',(0.0157873708942533,-0.999840932052135,0.00829876577361474));
#47607=DIRECTION('center_axis',(-1.14444500362894E-17,-1.,-3.5644992269101E-17));
#47608=DIRECTION('ref_axis',(-0.952128653909774,0.,0.305697606146927));
#47609=DIRECTION('center_axis',(0.110668766458005,-1.35530150608006E-17,
-0.993857345966041));
#47610=DIRECTION('ref_axis',(0.993857345966041,-5.87811925404552E-33,0.110668766458005));
#47611=DIRECTION('center_axis',(-1.22464679915E-16,-1.,-5.47382212627E-48));
#47612=DIRECTION('ref_axis',(1.,-1.22464679915E-16,6.22660996643423E-64));
#47613=DIRECTION('center_axis',(-1.49989545857296E-18,-1.,1.34697635782315E-17));
#47614=DIRECTION('ref_axis',(-0.993857345966041,0.,-0.110668766458005));
#47615=DIRECTION('center_axis',(1.,-1.22464679915E-16,6.12323399574E-17));
#47616=DIRECTION('ref_axis',(1.22464679915E-16,1.,7.49879891332945E-33));
#47617=DIRECTION('center_axis',(-1.22464679915E-16,-1.,3.08148791102E-33));
#47618=DIRECTION('ref_axis',(1.,-1.22464679915E-16,3.77373430685006E-49));
#47619=DIRECTION('center_axis',(1.,-1.22464679915E-16,6.12323399574E-17));
#47620=DIRECTION('ref_axis',(-6.12323399574E-17,7.49879891332945E-33,1.));
#47621=DIRECTION('center_axis',(1.,-1.22464679915E-16,6.12323399574E-17));
#47622=DIRECTION('ref_axis',(-1.22464679915E-16,-1.,-7.49879891332945E-33));
#47623=DIRECTION('',(1.,0.,2.65024142098E-16));
#47624=DIRECTION('center_axis',(-1.22464679915E-16,-1.,-1.81284143127026E-30));
#47625=DIRECTION('ref_axis',(1.57898385724467E-14,0.,-1.));
#47626=DIRECTION('center_axis',(0.106117864373042,-1.29956902936052E-17,
0.994353558278395));
#47627=DIRECTION('ref_axis',(0.994353558278395,-3.91187297993902E-33,-0.106117864373042));
#47628=DIRECTION('center_axis',(-1.22464679915E-16,-1.,-5.47382212627E-48));
#47629=DIRECTION('ref_axis',(1.,-1.22464679915E-16,-6.703498746053E-64));
#47630=DIRECTION('center_axis',(-4.52327322274045E-17,-1.,-5.91050929206098E-17));
#47631=DIRECTION('ref_axis',(-0.794132678900969,0.,0.607744426795977));
#47632=DIRECTION('center_axis',(0.607744426795977,-7.44272266974971E-17,
0.794132678900969));
#47633=DIRECTION('ref_axis',(0.794132678900969,-3.80543459761737E-32,-0.607744426795977));
#47634=DIRECTION('center_axis',(1.22464679915E-16,1.,5.47382212627E-48));
#47635=DIRECTION('ref_axis',(1.,-1.22464679915E-16,-6.703498746053E-64));
#47636=DIRECTION('center_axis',(-4.52327322274045E-17,-1.,-5.91050929206098E-17));
#47637=DIRECTION('ref_axis',(0.794132678900969,0.,-0.607744426795977));
#47638=DIRECTION('center_axis',(-0.734238830876792,8.99183234042744E-17,
0.678891257295808));
#47639=DIRECTION('ref_axis',(0.678891257295808,1.51038693775819E-31,0.734238830876792));
#47640=DIRECTION('center_axis',(-1.22464679915E-16,-1.,-1.23259516441E-32));
#47641=DIRECTION('ref_axis',(1.,-1.22464679915E-16,-1.50949372274247E-48));
#47642=DIRECTION('center_axis',(-0.540714503083014,0.0890998529400356,0.836474173158833));
#47643=DIRECTION('ref_axis',(0.803860483463198,0.347724019666725,0.482593337369186));
#47644=DIRECTION('center_axis',(0.757497881302333,-0.120607621490521,0.641600156998793));
#47645=DIRECTION('ref_axis',(0.519185231994408,0.707106824013922,-0.480048574950346));
#47646=DIRECTION('center_axis',(0.734238830876792,-8.991832340449E-17,-0.678891257295808));
#47647=DIRECTION('ref_axis',(-6.6021524650914E-17,-1.,6.10447636300053E-17));
#47648=DIRECTION('',(-0.734238830876791,0.,0.678891257295807));
#47649=DIRECTION('center_axis',(-1.2246467991486E-16,-1.,-1.56475089353662E-28));
#47650=DIRECTION('ref_axis',(-0.667272304480808,8.17172891841765E-17,0.744813850349785));
#47651=DIRECTION('',(0.,-1.,0.));
#47652=DIRECTION('center_axis',(-1.22464679915E-16,-1.,0.));
#47653=DIRECTION('ref_axis',(1.,-1.22464679915E-16,0.));
#47654=DIRECTION('',(0.,1.,0.));
#47655=DIRECTION('center_axis',(1.22464679915011E-16,1.,-3.67929656575737E-30));
#47656=DIRECTION('ref_axis',(-0.952128653909774,1.16602130838972E-16,0.305697606146927));
#47657=DIRECTION('',(-2.85587916301E-16,-1.,0.));
#47658=DIRECTION('center_axis',(-1.22464679915E-16,-1.,0.));
#47659=DIRECTION('ref_axis',(1.,-1.22464679915E-16,0.));
#47660=DIRECTION('center_axis',(-1.22464679914586E-16,-1.,-1.3947821589454E-28));
#47661=DIRECTION('ref_axis',(-0.947590338356885,1.16046347476986E-16,0.319487950715961));
#47662=DIRECTION('center_axis',(-1.22464679915E-16,-1.,6.16297582204E-33));
#47663=DIRECTION('ref_axis',(1.,-1.22464679915E-16,-7.0105395811531E-49));
#47664=DIRECTION('center_axis',(-1.22464679914997E-16,-1.,-3.04211334326766E-29));
#47665=DIRECTION('ref_axis',(-0.111333411199055,1.36344105663067E-17,0.993783110920478));
#47666=DIRECTION('',(-2.77555756156E-16,-1.,0.));
#47667=DIRECTION('center_axis',(-2.96428448085E-16,-1.,-1.50904692324E-15));
#47668=DIRECTION('ref_axis',(1.,-2.96428448085E-16,-4.47324437543477E-31));
#47669=DIRECTION('center_axis',(-1.22464679914586E-16,-1.,-1.3947821589454E-28));
#47670=DIRECTION('ref_axis',(-0.947590338356885,1.16046347476986E-16,0.319487950715961));
#47671=DIRECTION('',(0.,1.,0.));
#47672=DIRECTION('center_axis',(-1.22464679915E-16,-1.,6.16297582204E-33));
#47673=DIRECTION('ref_axis',(1.,-1.22464679915E-16,-7.0105395811531E-49));
#47674=DIRECTION('center_axis',(1.22464679915E-16,1.,-5.21020650422465E-33));
#47675=DIRECTION('ref_axis',(-6.38066271830923E-49,-5.21020650422465E-33,
-1.));
#47676=DIRECTION('',(0.,1.,0.));
#47677=DIRECTION('center_axis',(-3.04677329401E-20,1.,-1.36892417294E-16));
#47678=DIRECTION('ref_axis',(1.,3.04677329401E-20,-4.17080161163832E-36));
#47679=DIRECTION('center_axis',(-2.17357452795E-16,2.66186108837E-32,1.));
#47680=DIRECTION('ref_axis',(1.,2.56447231488414E-65,2.17357452795E-16));
#47681=DIRECTION('',(0.,1.,0.));
#47682=DIRECTION('',(1.,0.,1.09790153833E-16));
#47683=DIRECTION('center_axis',(-1.22464679915E-16,-1.,-1.94567767731298E-44));
#47684=DIRECTION('ref_axis',(2.38276793969895E-60,1.94567767731298E-44,
-1.));
#47685=DIRECTION('',(0.,1.,0.));
#47686=DIRECTION('center_axis',(2.45272844836E-16,1.,-1.36611674972E-16));
#47687=DIRECTION('ref_axis',(1.,-2.45272844836E-16,3.35071341581934E-32));
#47688=DIRECTION('center_axis',(-1.22464679914998E-16,-1.,-1.73663083545565E-29));
#47689=DIRECTION('ref_axis',(-0.095298509688002,1.16707014853003E-17,0.99544874004202));
#47690=DIRECTION('',(0.,1.,0.));
#47691=DIRECTION('center_axis',(1.22464679915E-16,1.,0.));
#47692=DIRECTION('ref_axis',(1.,-1.22464679915E-16,0.));
#47693=DIRECTION('center_axis',(1.224646799149E-16,1.,-1.07586726537792E-28));
#47694=DIRECTION('ref_axis',(0.678891257295809,-8.31402005216765E-17,0.73423883087679));
#47695=DIRECTION('',(0.,1.,0.));
#47696=DIRECTION('center_axis',(6.14568728566E-17,1.,-5.23898221099E-18));
#47697=DIRECTION('ref_axis',(1.,-6.14568728566E-17,3.21971463638802E-34));
#47698=DIRECTION('center_axis',(0.678891257295808,-8.31402005216763E-17,
0.734238830876792));
#47699=DIRECTION('ref_axis',(-1.22464679914784E-16,-1.,1.83887638005312E-34));
#47700=DIRECTION('',(0.,1.,0.));
#47701=DIRECTION('',(-0.734238830876791,0.,0.678891257295807));
#47702=DIRECTION('center_axis',(-1.224646799149E-16,-1.,1.07603845915075E-28));
#47703=DIRECTION('ref_axis',(0.67889125729581,-8.31402005216767E-17,0.734238830876789));
#47704=DIRECTION('center_axis',(-1.22365143363E-16,-1.,-6.12322590562E-17));
#47705=DIRECTION('ref_axis',(1.,-1.22365143363E-16,-7.49269415785227E-33));
#47706=DIRECTION('center_axis',(0.,1.,0.));
#47707=DIRECTION('ref_axis',(-0.00162555525320111,0.,0.999998678784187));
#47708=DIRECTION('center_axis',(0.734238830876792,-8.99183234042744E-17,
-0.678891257295808));
#47709=DIRECTION('ref_axis',(0.678891257295807,3.46311205996404E-31,0.734238830876791));
#47710=DIRECTION('center_axis',(0.732027802944257,-8.96475505763315E-17,
0.68127475787424));
#47711=DIRECTION('ref_axis',(0.68127475787424,-1.91888914560603E-31,-0.732027802944257));
#47712=DIRECTION('center_axis',(5.46401789901627E-17,1.,6.08764557973899E-17));
#47713=DIRECTION('ref_axis',(-0.744196935834912,0.,0.667960268798922));
#47714=DIRECTION('center_axis',(-0.667960268798921,8.18015405141904E-17,
-0.744196935834913));
#47715=DIRECTION('ref_axis',(0.744196935834913,-3.15837441223295E-32,-0.667960268798921));
#47716=DIRECTION('center_axis',(-1.22464679915E-16,-1.,-5.47382212627E-48));
#47717=DIRECTION('ref_axis',(1.,-1.22464679915E-16,6.49622071350503E-64));
#47718=DIRECTION('center_axis',(1.14444500362894E-17,1.,3.5644992269101E-17));
#47719=DIRECTION('ref_axis',(-0.952128653909774,0.,0.305697606146927));
#47720=DIRECTION('center_axis',(-0.305697606146928,3.74371594874912E-17,
-0.952128653909774));
#47721=DIRECTION('ref_axis',(0.952128653909774,-6.76944606262743E-33,-0.305697606146928));
#47722=DIRECTION('center_axis',(-1.22464679915E-16,-1.,-5.47382212627E-48));
#47723=DIRECTION('ref_axis',(1.,-1.22464679915E-16,-6.703498746053E-64));
#47724=DIRECTION('center_axis',(-0.222411493783323,0.670605060062733,-0.707687770737441));
#47725=DIRECTION('ref_axis',(-0.848579081651793,0.224251763465943,0.479191703564883));
#47726=DIRECTION('center_axis',(0.734238830876792,-8.99183234042744E-17,
-0.678891257295808));
#47727=DIRECTION('ref_axis',(0.678891257295807,3.46311205996404E-31,0.734238830876791));
#47728=DIRECTION('center_axis',(-0.299820876204079,3.67174676361097E-17,
-0.953995514765252));
#47729=DIRECTION('ref_axis',(0.953995514765252,-6.3869078326472E-32,-0.299820876204079));
#47730=DIRECTION('center_axis',(2.41898181523141E-16,1.,-1.1741867647411E-17));
#47731=DIRECTION('ref_axis',(0.99520202856178,-2.41886400693281E-16,-0.0978413120645785));
#47732=DIRECTION('center_axis',(-1.22464679915E-16,-1.,-5.47382212627E-48));
#47733=DIRECTION('ref_axis',(1.,-1.22464679915E-16,6.49622071350503E-64));
#47734=DIRECTION('center_axis',(-0.962126872935794,0.250387400346799,-0.107786966384449));
#47735=DIRECTION('ref_axis',(0.248830769651925,0.968145727536702,0.0278764834019926));
#47736=DIRECTION('center_axis',(0.152411459643054,-1.86650206205066E-17,
0.988317128744349));
#47737=DIRECTION('ref_axis',(0.988317128744349,-1.89428554374595E-32,-0.152411459643054));
#47738=DIRECTION('center_axis',(-0.993783110920478,1.2170333058406E-16,
-0.111333411199054));
#47739=DIRECTION('ref_axis',(0.111333411199054,1.57725565511394E-32,-0.993783110920478));
#47740=DIRECTION('center_axis',(2.41898181523141E-16,1.,-1.1741867647411E-17));
#47741=DIRECTION('ref_axis',(-0.999778332126524,2.41886400693281E-16,0.0210543727122351));
#47742=DIRECTION('center_axis',(0.110668766460438,2.4072234423934E-12,-0.99385734596577));
#47743=DIRECTION('ref_axis',(2.68725782367101E-10,1.,3.2344497450746E-11));
#47744=DIRECTION('center_axis',(-1.22464679915E-16,-1.,-5.47382212627E-48));
#47745=DIRECTION('ref_axis',(1.,-1.22464679915E-16,6.49622071350503E-64));
#47746=DIRECTION('center_axis',(0.,1.,0.));
#47747=DIRECTION('ref_axis',(-0.666832525280057,0.,-0.745207610823066));
#47748=DIRECTION('center_axis',(1.,-1.22464679915E-16,6.12323399574E-17));
#47749=DIRECTION('ref_axis',(1.22464679915E-16,1.,7.49879891332945E-33));
#47750=DIRECTION('center_axis',(1.,-1.22464679915E-16,6.12323399574E-17));
#47751=DIRECTION('ref_axis',(6.12323399574E-17,-7.49879891332945E-33,-1.));
#47752=DIRECTION('center_axis',(1.,0.,0.));
#47753=DIRECTION('ref_axis',(0.,1.,3.70074341541721E-15));
#47754=DIRECTION('',(1.,0.,2.65024142098E-16));
#47755=DIRECTION('center_axis',(0.,1.,0.));
#47756=DIRECTION('ref_axis',(0.66853651195256,0.,-0.743679320800507));
#47757=DIRECTION('center_axis',(0.106117864373042,-1.29956902936052E-17,
0.994353558278395));
#47758=DIRECTION('ref_axis',(0.994353558278395,-3.91187297993902E-33,-0.106117864373042));
#47759=DIRECTION('center_axis',(1.68490994230906E-17,1.,4.21844451941189E-17));
#47760=DIRECTION('ref_axis',(-0.928750804671078,0.,0.370704657136683));
#47761=DIRECTION('center_axis',(0.607744426797546,-1.7991646764781E-12,
0.794132678899768));
#47762=DIRECTION('ref_axis',(-4.46309655899322E-12,1.,5.68064114266551E-12));
#47763=DIRECTION('center_axis',(1.22464679915E-16,1.,5.47382212627E-48));
#47764=DIRECTION('ref_axis',(1.,-1.22464679915E-16,-6.703498746053E-64));
#47765=DIRECTION('center_axis',(0.,0.,1.));
#47766=DIRECTION('ref_axis',(1.,0.,0.));
#47767=DIRECTION('center_axis',(-0.734238830876792,8.99183234042744E-17,
0.678891257295808));
#47768=DIRECTION('ref_axis',(0.678891257295808,1.51038693775819E-31,0.734238830876792));
#47769=DIRECTION('center_axis',(0.734238830876792,-8.991832340449E-17,-0.678891257295808));
#47770=DIRECTION('ref_axis',(6.6021524650914E-17,1.,-6.10447636300053E-17));
#47771=DIRECTION('',(-0.734238830876791,0.,0.678891257295807));
#47772=DIRECTION('center_axis',(0.734238830876792,-8.99183234042744E-17,
-0.678891257295808));
#47773=DIRECTION('ref_axis',(-0.678891257295807,-3.46311205996404E-31,-0.734238830876791));
#47774=DIRECTION('center_axis',(0.734238830876792,-8.99183234042744E-17,
-0.678891257295808));
#47775=DIRECTION('ref_axis',(0.678891257295807,3.46311205996404E-31,0.734238830876791));
#47776=DIRECTION('',(0.734238830876791,0.,-0.678891257295807));
#47777=DIRECTION('center_axis',(6.60215246509141E-17,1.,-6.10447636300053E-17));
#47778=DIRECTION('ref_axis',(0.678891257295808,0.,0.734238830876791));
#47779=DIRECTION('center_axis',(-0.613815420645987,7.51707090161983E-17,
-0.789449573675983));
#47780=DIRECTION('ref_axis',(0.789449573675983,7.34020703099417E-32,-0.613815420645987));
#47781=DIRECTION('center_axis',(1.22464679915E-16,1.,5.47382212627E-48));
#47782=DIRECTION('ref_axis',(1.,-1.22464679915E-16,-6.703498746053E-64));
#47783=DIRECTION('center_axis',(3.85062311351295E-17,1.,5.68588026119494E-17));
#47784=DIRECTION('ref_axis',(-0.827993213361104,0.,0.560738119471071));
#47785=DIRECTION('center_axis',(-0.560738119471071,6.86706143170087E-17,
-0.827993213361104));
#47786=DIRECTION('ref_axis',(0.827993213361104,-2.38131063616686E-32,-0.560738119471071));
#47787=DIRECTION('center_axis',(-1.22464679915E-16,-1.,-5.47382212627E-48));
#47788=DIRECTION('ref_axis',(1.,-1.22464679915E-16,-6.703498746053E-64));
#47789=DIRECTION('center_axis',(3.85062311351295E-17,1.,5.68588026119494E-17));
#47790=DIRECTION('ref_axis',(0.827993213361104,0.,-0.560738119471072));
#47791=DIRECTION('center_axis',(1.22464679915E-16,1.,5.47382212627E-48));
#47792=DIRECTION('ref_axis',(1.,-1.22464679915E-16,-6.703498746053E-64));
#47793=DIRECTION('center_axis',(1.22464679915E-16,1.,5.47382212627E-48));
#47794=DIRECTION('ref_axis',(1.,-1.22464679915E-16,0.));
#47795=DIRECTION('axis',(0.,0.,1.));
#47796=DIRECTION('refdir',(1.,0.,0.));
#47797=DIRECTION('center_axis',(-4.22828176385563E-17,-1.,5.82264120529052E-17));
#47798=DIRECTION('ref_axis',(0.809156716779487,0.,0.587592892818354));
#47799=DIRECTION('center_axis',(1.22464679915E-16,1.,3.21507022015E-32));
#47800=DIRECTION('ref_axis',(1.,-1.22464679915E-16,-3.93732545414918E-48));
#47801=DIRECTION('center_axis',(0.814436178114135,-9.97396658637165E-17,
-0.580253144566095));
#47802=DIRECTION('ref_axis',(0.580253144566095,-1.05208313255741E-31,0.814436178114135));
#47803=DIRECTION('center_axis',(1.22464679915E-16,1.,2.46519032882E-32));
#47804=DIRECTION('ref_axis',(1.,-1.22464679915E-16,-3.01898744548495E-48));
#47805=DIRECTION('center_axis',(0.54648608815598,-6.69252438638976E-17,
-0.837468181754969));
#47806=DIRECTION('ref_axis',(0.837468181754969,-2.14539310633749E-32,0.54648608815598));
#47807=DIRECTION('center_axis',(1.22464679914918E-16,1.,2.56032743355287E-29));
#47808=DIRECTION('ref_axis',(0.954110409263768,-1.16844825873972E-16,-0.299455049939928));
#47809=DIRECTION('center_axis',(-1.22464679915E-16,-1.,-3.38963670212E-32));
#47810=DIRECTION('ref_axis',(1.,-1.22464679915E-16,4.23644123317814E-49));
#47811=DIRECTION('',(8.6905911908E-17,1.,0.));
#47812=DIRECTION('center_axis',(1.22464679915E-16,1.,3.21507022015E-32));
#47813=DIRECTION('ref_axis',(1.,-1.22464679915E-16,-3.93732545414918E-48));
#47814=DIRECTION('',(0.,1.,0.));
#47815=DIRECTION('center_axis',(-1.2246467991493E-16,-1.,-2.25761787925393E-29));
#47816=DIRECTION('ref_axis',(0.952002172953202,-1.16586641389025E-16,-0.306091265299064));
#47817=DIRECTION('center_axis',(0.,1.,0.));
#47818=DIRECTION('ref_axis',(0.95200562088917,0.,-0.306080541353786));
#47819=DIRECTION('center_axis',(1.22464679915E-16,1.,3.21507022015E-32));
#47820=DIRECTION('ref_axis',(1.,-1.22464679915E-16,-3.93732545414918E-48));
#47821=DIRECTION('',(2.43336553343E-16,1.,0.));
#47822=DIRECTION('center_axis',(1.22464679915E-16,1.,-1.86877716572514E-30));
#47823=DIRECTION('ref_axis',(0.00535506551034943,-6.5580638364693E-19,0.999985661533894));
#47824=DIRECTION('center_axis',(-1.22464679915E-16,-1.,-2.46519032882E-32));
#47825=DIRECTION('ref_axis',(1.,-1.22464679915E-16,-3.01898744548495E-48));
#47826=DIRECTION('center_axis',(1.22464679915E-16,1.,3.21507022015E-32));
#47827=DIRECTION('ref_axis',(1.,-1.22464679915E-16,-3.93732545414918E-48));
#47828=DIRECTION('',(1.22211438621E-16,1.,0.));
#47829=DIRECTION('center_axis',(-1.59015019497209E-16,-1.,3.16247585529168E-17));
#47830=DIRECTION('ref_axis',(0.756223380296384,-1.38202005618507E-16,-0.654313532714333));
#47831=DIRECTION('center_axis',(-1.22464679915E-16,-1.,-3.21507022015E-32));
#47832=DIRECTION('ref_axis',(1.,-1.22464679915E-16,4.87897920646316E-49));
#47833=DIRECTION('center_axis',(0.654313532714333,-8.01302973477407E-17,
0.756223380296384));
#47834=DIRECTION('ref_axis',(0.756223380296384,1.79722796841309E-32,-0.654313532714333));
#47835=DIRECTION('center_axis',(-1.02993792068947E-16,-1.,4.47814757931693E-17));
#47836=DIRECTION('ref_axis',(0.393698211550324,0.,0.919239750131638));
#47837=DIRECTION('center_axis',(-0.999959189367103,1.22459682054048E-16,
0.00903435666143352));
#47838=DIRECTION('ref_axis',(0.00903435666143352,1.38777878078145E-14,0.999959189367103));
#47839=DIRECTION('center_axis',(-1.22464679915E-16,-1.,-3.21507022015E-32));
#47840=DIRECTION('ref_axis',(1.,-1.22464679915E-16,-3.93732545414918E-48));
#47841=DIRECTION('center_axis',(-1.22464679915E-16,-1.,-3.21507022015E-32));
#47842=DIRECTION('ref_axis',(-1.,1.22464679915E-16,0.));
#47843=DIRECTION('center_axis',(-1.22464679915E-16,-1.,-3.23556230657E-32));
#47844=DIRECTION('ref_axis',(1.,-1.22464679915E-16,4.91007664965853E-49));
#47845=DIRECTION('center_axis',(-1.22464679915E-16,-1.,-2.46519032882E-32));
#47846=DIRECTION('ref_axis',(1.,-1.22464679915E-16,-3.01898744548495E-48));
#47847=DIRECTION('center_axis',(-1.22464679915E-16,-1.,-3.21630300713E-32));
#47848=DIRECTION('ref_axis',(1.,-1.22464679915E-16,-3.93883518277827E-48));
#47849=DIRECTION('center_axis',(-1.22464679915E-16,-1.,-2.46519032882E-32));
#47850=DIRECTION('ref_axis',(1.,-1.22464679915E-16,-3.01898744548495E-48));
#47851=DIRECTION('center_axis',(-5.24303379351633E-17,-1.,6.05964043245936E-17));
#47852=DIRECTION('ref_axis',(-0.756223380296385,0.,-0.654313532714333));
#47853=DIRECTION('center_axis',(-1.22464679915E-16,-1.,-2.46519032882E-32));
#47854=DIRECTION('ref_axis',(1.,-1.22464679915E-16,-3.01898744548495E-48));
#47855=DIRECTION('center_axis',(0.654313532714333,-8.01302973477407E-17,
-0.756223380296384));
#47856=DIRECTION('ref_axis',(0.756223380296384,1.79722796841309E-32,0.654313532714333));
#47857=DIRECTION('center_axis',(-1.22464679914857E-16,-1.,1.23638169675289E-28));
#47858=DIRECTION('ref_axis',(-0.756223380296385,9.2610654212047E-17,-0.654313532714332));
#47859=DIRECTION('',(0.,1.,0.));
#47860=DIRECTION('center_axis',(1.22464679915E-16,1.,3.21507022015E-32));
#47861=DIRECTION('ref_axis',(1.,-1.22464679915E-16,-3.93732545414918E-48));
#47862=DIRECTION('center_axis',(-1.55713156083392E-16,-1.,-2.32366652287783E-17));
#47863=DIRECTION('ref_axis',(-0.871681712672678,1.38202005618507E-16,-0.490072435250165));
#47864=DIRECTION('center_axis',(-1.22464679915E-16,-1.,-3.21507022015E-32));
#47865=DIRECTION('ref_axis',(1.,-1.22464679915E-16,4.01826426994016E-49));
#47866=DIRECTION('center_axis',(-1.22464679914918E-16,-1.,2.55459749524577E-29));
#47867=DIRECTION('ref_axis',(-0.954110409263768,1.16844825873972E-16,-0.299455049939928));
#47868=DIRECTION('',(0.,1.,0.));
#47869=DIRECTION('center_axis',(-1.22464679915E-16,-1.,-3.21507022015E-32));
#47870=DIRECTION('ref_axis',(1.,-1.22464679915E-16,-3.93732545414918E-48));
#47871=DIRECTION('center_axis',(-1.22454684396776E-16,-1.,1.10634444432041E-18));
#47872=DIRECTION('ref_axis',(0.00903435666143093,0.,0.999959189367103));
#47873=DIRECTION('center_axis',(-1.22464679915E-16,-1.,-3.19704370768E-32));
#47874=DIRECTION('ref_axis',(1.,-1.22464679915E-16,-3.91524934335296E-48));
#47875=DIRECTION('center_axis',(-0.999959189367103,1.22459682054048E-16,
-0.00903435666143352));
#47876=DIRECTION('ref_axis',(0.00903435666143352,1.38777878078145E-14,-0.999959189367103));
#47877=DIRECTION('center_axis',(-1.22464679915E-16,-1.,-2.69938341005315E-32));
#47878=DIRECTION('ref_axis',(0.00903435666143093,-1.10638959678011E-18,
0.999959189367103));
#47879=DIRECTION('center_axis',(1.22464679915E-16,1.,3.21507022015E-32));
#47880=DIRECTION('ref_axis',(1.,-1.22464679915E-16,-3.93732545414918E-48));
#47881=DIRECTION('',(1.21668276671E-16,1.,0.));
#47882=DIRECTION('center_axis',(-1.22464679914807E-16,-1.,-1.87465740942333E-28));
#47883=DIRECTION('ref_axis',(-0.717530579084786,8.78721526965739E-17,0.696527004557793));
#47884=DIRECTION('center_axis',(0.,1.,0.));
#47885=DIRECTION('ref_axis',(-0.717538425134005,0.,0.696518921822094));
#47886=DIRECTION('',(0.,1.,0.));
#47887=DIRECTION('center_axis',(1.22464679915E-16,1.,3.21507022015E-32));
#47888=DIRECTION('ref_axis',(1.,-1.22464679915E-16,-3.93732545414918E-48));
#47889=DIRECTION('center_axis',(-1.22454684396776E-16,-1.,-1.10634444432041E-18));
#47890=DIRECTION('ref_axis',(-0.00903435666143093,0.,0.999959189367103));
#47891=DIRECTION('center_axis',(-1.22464679915E-16,-1.,-3.21507022015E-32));
#47892=DIRECTION('ref_axis',(1.,-1.22464679915E-16,-3.93732545414918E-48));
#47893=DIRECTION('center_axis',(-1.22464679915E-16,-1.,-1.86877716572514E-30));
#47894=DIRECTION('ref_axis',(-0.00535506551034943,6.5580638364693E-19,0.999985661533894));
#47895=DIRECTION('center_axis',(-1.22464679915E-16,-1.,-3.21507022015E-32));
#47896=DIRECTION('ref_axis',(1.,-1.22464679915E-16,-3.93732545414918E-48));
#47897=DIRECTION('center_axis',(1.22464679915E-16,1.,3.21507022015E-32));
#47898=DIRECTION('ref_axis',(1.,-1.22464679915E-16,0.));
#47899=DIRECTION('',(-0.734238830876791,0.,0.678891257295807));
#47900=DIRECTION('center_axis',(1.22464679915E-16,1.,2.46519032882E-32));
#47901=DIRECTION('ref_axis',(1.,-1.22464679915E-16,-3.01898744548495E-48));
#47902=DIRECTION('',(0.734238830876791,0.,-0.678891257295807));
#47903=DIRECTION('center_axis',(-1.22464679915E-16,-1.,-3.08148791102E-32));
#47904=DIRECTION('ref_axis',(1.,-1.22464679915E-16,-3.77373430685006E-48));
#47905=DIRECTION('center_axis',(-1.22464679915E-16,-1.,-2.46519032882E-32));
#47906=DIRECTION('ref_axis',(1.,-1.22464679915E-16,2.53931026341659E-48));
#47907=DIRECTION('center_axis',(0.734238830876792,-8.99183234039869E-17,
-0.678891257295808));
#47908=DIRECTION('ref_axis',(-6.60215246505446E-17,-1.,6.10447636296637E-17));
#47909=DIRECTION('center_axis',(0.734238830876792,-8.99183234042744E-17,
-0.678891257295808));
#47910=DIRECTION('ref_axis',(0.678891257295807,3.46311205996404E-31,0.734238830876791));
#47911=DIRECTION('',(0.734238830876791,0.,-0.678891257295807));
#47912=DIRECTION('center_axis',(-0.678891257295808,8.31402005216763E-17,
-0.734238830876792));
#47913=DIRECTION('ref_axis',(-0.734238830876792,-5.02124004685594E-34,0.678891257295808));
#47914=DIRECTION('',(0.734238830876791,-1.7529794737095E-16,-0.678891257295807));
#47915=DIRECTION('',(0.,1.,0.));
#47916=DIRECTION('',(0.,-1.,0.));
#47917=DIRECTION('center_axis',(3.65737147181347E-17,1.,5.60477622923109E-17));
#47918=DIRECTION('ref_axis',(-0.837468181754969,0.,0.54648608815598));
#47919=DIRECTION('center_axis',(0.814436178114135,-9.97396658637165E-17,
0.580253144566095));
#47920=DIRECTION('ref_axis',(0.580253144566095,-1.05208313255741E-31,-0.814436178114135));
#47921=DIRECTION('center_axis',(1.22464679915E-16,1.,3.21507022015E-32));
#47922=DIRECTION('ref_axis',(1.,-1.22464679915E-16,-3.93732545414918E-48));
#47923=DIRECTION('center_axis',(0.54648608815598,-6.69252438638976E-17,
0.837468181754969));
#47924=DIRECTION('ref_axis',(0.837468181754969,1.49530298329546E-31,-0.54648608815598));
#47925=DIRECTION('center_axis',(1.,0.,0.));
#47926=DIRECTION('ref_axis',(0.,-1.,0.));
#47927=DIRECTION('center_axis',(-1.22464679915E-16,-1.,-2.46519032882E-32));
#47928=DIRECTION('ref_axis',(1.,-1.22464679915E-16,-3.01898744548495E-48));
#47929=DIRECTION('center_axis',(-1.224646799149E-16,-1.,1.07586726537792E-28));
#47930=DIRECTION('ref_axis',(-0.678891257295809,8.31402005216766E-17,-0.73423883087679));
#47931=DIRECTION('center_axis',(-1.22464679915E-16,-1.,-2.46519032882E-32));
#47932=DIRECTION('ref_axis',(1.,-1.22464679915E-16,-3.01898744548495E-48));
#47933=DIRECTION('',(0.,-1.,0.));
#47934=DIRECTION('center_axis',(1.22464679914909E-16,1.,-6.61121943250621E-29));
#47935=DIRECTION('ref_axis',(-0.809156716779487,9.90931183213597E-17,-0.587592892818354));
#47936=DIRECTION('',(0.,-1.,0.));
#47937=DIRECTION('center_axis',(1.22464679915E-16,1.,2.46519032882E-32));
#47938=DIRECTION('ref_axis',(1.,-1.22464679915E-16,-3.01898744548495E-48));
#47939=DIRECTION('center_axis',(0.734238830876792,-8.99183234042744E-17,
-0.678891257295808));
#47940=DIRECTION('ref_axis',(0.678891257295807,3.46311205996404E-31,0.734238830876791));
#47941=DIRECTION('',(-0.734238830876791,0.,0.678891257295807));
#47942=DIRECTION('center_axis',(-0.734238830876792,8.99183234042744E-17,
0.678891257295808));
#47943=DIRECTION('ref_axis',(0.678891257295808,1.51038693775819E-31,0.734238830876792));
#47944=DIRECTION('center_axis',(0.,0.,1.));
#47945=DIRECTION('ref_axis',(1.,0.,0.));
#47946=DIRECTION('center_axis',(-1.22464679915E-16,-1.,-3.69778549322E-32));
#47947=DIRECTION('ref_axis',(1.,-1.22464679915E-16,-4.52848116821518E-48));
#47948=DIRECTION('center_axis',(1.224646799149E-16,1.,-1.07586726537792E-28));
#47949=DIRECTION('ref_axis',(0.678891257295809,-8.31402005216765E-17,0.73423883087679));
#47950=DIRECTION('center_axis',(-1.22464679915E-16,-1.,-2.46519032882E-32));
#47951=DIRECTION('ref_axis',(1.,-1.22464679915E-16,-3.01898744548495E-48));
#47952=DIRECTION('',(0.,-1.,0.));
#47953=DIRECTION('center_axis',(-0.678891257295808,8.31402005216763E-17,
-0.734238830876792));
#47954=DIRECTION('ref_axis',(-0.734238830876792,-5.02124004685594E-34,0.678891257295808));
#47955=DIRECTION('',(0.,-1.,0.));
#47956=DIRECTION('',(-0.734238830876791,1.47705801254958E-16,0.678891257295807));
#47957=DIRECTION('center_axis',(1.22464679915E-16,1.,3.21507022015E-32));
#47958=DIRECTION('ref_axis',(1.,-1.22464679915E-16,0.));
#47959=DIRECTION('',(0.734238830876791,0.,0.678891257295807));
#47960=DIRECTION('center_axis',(1.22464679915E-16,1.,2.46519032882E-32));
#47961=DIRECTION('ref_axis',(1.,-1.22464679915E-16,-3.01898744548495E-48));
#47962=DIRECTION('',(-0.734238830876791,0.,-0.678891257295807));
#47963=DIRECTION('center_axis',(-1.22464679915E-16,-1.,-2.46519032882E-32));
#47964=DIRECTION('ref_axis',(1.,-1.22464679915E-16,2.53931026341659E-48));
#47965=DIRECTION('center_axis',(-1.22464679915E-16,-1.,-2.46519032882E-32));
#47966=DIRECTION('ref_axis',(1.,-1.22464679915E-16,-3.01898744548495E-48));
#47967=DIRECTION('center_axis',(-0.734238830876792,8.99183234039869E-17,
-0.678891257295808));
#47968=DIRECTION('ref_axis',(-6.60215246505446E-17,-1.,-6.10447636296637E-17));
#47969=DIRECTION('center_axis',(-0.734238830876792,8.99183234042744E-17,
-0.678891257295808));
#47970=DIRECTION('ref_axis',(0.678891257295807,3.46311205996404E-31,-0.734238830876791));
#47971=DIRECTION('',(-0.734238830876791,0.,-0.678891257295807));
#47972=DIRECTION('center_axis',(-0.678891257295808,8.31402005216763E-17,
0.734238830876792));
#47973=DIRECTION('ref_axis',(1.22464679914784E-16,1.,1.83887638005312E-34));
#47974=DIRECTION('',(-0.734238830876791,1.47829617289958E-16,-0.678891257295807));
#47975=DIRECTION('',(0.,1.,0.));
#47976=DIRECTION('',(0.,1.,0.));
#47977=DIRECTION('center_axis',(0.,0.,1.));
#47978=DIRECTION('ref_axis',(1.,0.,0.));
#47979=DIRECTION('center_axis',(0.814436178114135,-9.97396658637165E-17,
-0.580253144566095));
#47980=DIRECTION('ref_axis',(0.580253144566095,-3.4207048899363E-31,0.814436178114135));
#47981=DIRECTION('center_axis',(-1.22464679915E-16,-1.,-3.69778549322E-32));
#47982=DIRECTION('ref_axis',(1.,-1.22464679915E-16,-4.52848116821518E-48));
#47983=DIRECTION('center_axis',(1.22464679914972E-16,1.,-3.85870763968785E-29));
#47984=DIRECTION('ref_axis',(-0.580253144566094,7.10605156189115E-17,-0.814436178114135));
#47985=DIRECTION('center_axis',(-1.22464679915E-16,-1.,-3.69778549322E-32));
#47986=DIRECTION('ref_axis',(1.,-1.22464679915E-16,-4.52848116821518E-48));
#47987=DIRECTION('',(0.,1.,0.));
#47988=DIRECTION('center_axis',(1.22464679914909E-16,1.,-6.61121943250621E-29));
#47989=DIRECTION('ref_axis',(0.721410252528561,-8.83472756631981E-17,0.692507940421391));
#47990=DIRECTION('center_axis',(1.22464679915E-16,1.,2.46519032882E-32));
#47991=DIRECTION('ref_axis',(1.,-1.22464679915E-16,-3.01898744548495E-48));
#47992=DIRECTION('',(0.,-1.,0.));
#47993=DIRECTION('center_axis',(8.12315922726109E-17,1.,-5.78742547555248E-17));
#47994=DIRECTION('ref_axis',(0.580253144566096,0.,0.814436178114134));
#47995=DIRECTION('center_axis',(0.54648608815598,-6.69252438638976E-17,
-0.837468181754969));
#47996=DIRECTION('ref_axis',(0.837468181754969,1.49530298329546E-31,0.54648608815598));
#47997=DIRECTION('center_axis',(-0.734238830876792,8.99183234042744E-17,
-0.678891257295808));
#47998=DIRECTION('ref_axis',(0.678891257295807,3.46311205996404E-31,-0.734238830876791));
#47999=DIRECTION('',(0.734238830876791,0.,0.678891257295807));
#48000=DIRECTION('center_axis',(0.734238830876792,-8.99183234042744E-17,
0.678891257295808));
#48001=DIRECTION('ref_axis',(0.678891257295808,1.72414837744489E-31,-0.734238830876792));
#48002=DIRECTION('center_axis',(1.,0.,0.));
#48003=DIRECTION('ref_axis',(0.,-1.,0.));
#48004=DIRECTION('center_axis',(-1.22464679915E-16,-1.,-2.46519032882E-32));
#48005=DIRECTION('ref_axis',(1.,-1.22464679915E-16,-3.01898744548495E-48));
#48006=DIRECTION('center_axis',(1.224646799149E-16,1.,1.07603845915075E-28));
#48007=DIRECTION('ref_axis',(0.678891257295809,-8.31402005216765E-17,-0.73423883087679));
#48008=DIRECTION('center_axis',(-1.22464679915E-16,-1.,-2.46519032882E-32));
#48009=DIRECTION('ref_axis',(1.,-1.22464679915E-16,-3.01898744548495E-48));
#48010=DIRECTION('',(0.,-1.,0.));
#48011=DIRECTION('center_axis',(-0.678891257295808,8.31402005216763E-17,
0.734238830876792));
#48012=DIRECTION('ref_axis',(1.22464679914784E-16,1.,1.83887638005312E-34));
#48013=DIRECTION('',(0.,-1.,0.));
#48014=DIRECTION('',(0.734238830876791,-1.7634971726895E-16,0.678891257295807));
#48015=DIRECTION('center_axis',(1.,-1.22464679915E-16,2.44929359829E-16));
#48016=DIRECTION('ref_axis',(-2.44929359829E-16,0.,1.));
#48017=DIRECTION('',(2.54245135096E-16,0.,-1.));
#48018=DIRECTION('',(-1.4098070154E-16,-1.,0.));
#48019=DIRECTION('',(3.06496402452E-16,0.,-1.));
#48020=DIRECTION('',(2.04649405461E-16,1.,0.));
#48021=DIRECTION('center_axis',(-2.44929359829E-16,5.34329236504435E-33,
1.));
#48022=DIRECTION('ref_axis',(-1.3087291783495E-48,-1.,5.34329236504435E-33));
#48023=DIRECTION('',(2.04893992976E-16,0.,-1.));
#48024=DIRECTION('center_axis',(3.01898744547E-48,2.46519032882E-32,-1.));
#48025=DIRECTION('ref_axis',(1.,-7.44237865340164E-80,3.01898744547E-48));
#48026=DIRECTION('center_axis',(1.22464679915E-16,1.,3.21507022015E-32));
#48027=DIRECTION('ref_axis',(1.,-1.22464679915E-16,0.));
#48028=DIRECTION('',(-3.06496402452E-16,0.,1.));
#48029=DIRECTION('center_axis',(-1.22464679915E-16,-1.,-3.08148791102E-32));
#48030=DIRECTION('ref_axis',(1.,-1.22464679915E-16,-3.77373430685006E-48));
#48031=DIRECTION('center_axis',(-1.22464679915E-16,-1.,-3.08148791102E-32));
#48032=DIRECTION('ref_axis',(1.,-1.22464679915E-16,-3.77373430685006E-48));
#48033=DIRECTION('center_axis',(-1.22464679915E-16,-1.,-2.46519032882E-32));
#48034=DIRECTION('ref_axis',(1.,-1.22464679915E-16,-3.01898744548495E-48));
#48035=DIRECTION('center_axis',(1.22464679915E-16,1.,2.46519032882E-32));
#48036=DIRECTION('ref_axis',(1.,-1.22464679915E-16,2.36438383255719E-48));
#48037=DIRECTION('center_axis',(1.22464679915E-16,1.,3.38963670212E-32));
#48038=DIRECTION('ref_axis',(1.,-1.22464679915E-16,-4.15110773753262E-48));
#48039=DIRECTION('center_axis',(1.22464679915E-16,1.,3.08148791102E-32));
#48040=DIRECTION('ref_axis',(1.,-1.22464679915E-16,2.9554797906917E-48));
#48041=DIRECTION('center_axis',(1.22464679914907E-16,1.,1.86840883671487E-28));
#48042=DIRECTION('ref_axis',(-0.446669893168924,5.47012854943908E-17,0.894698835662851));
#48043=DIRECTION('center_axis',(1.22464679915E-16,1.,3.21507022015E-32));
#48044=DIRECTION('ref_axis',(1.,-1.22464679915E-16,-3.93732545414918E-48));
#48045=DIRECTION('center_axis',(1.22464679915E-16,1.,3.08148791102E-32));
#48046=DIRECTION('ref_axis',(1.,-1.22464679915E-16,-3.77373430685006E-48));
#48047=DIRECTION('',(0.,1.,0.));
#48048=DIRECTION('center_axis',(1.,0.,0.));
#48049=DIRECTION('ref_axis',(0.,-1.,0.));
#48050=DIRECTION('center_axis',(0.894698835662851,-1.09569006529982E-16,
0.446669893168925));
#48051=DIRECTION('ref_axis',(0.446669893168925,-6.79741207737406E-32,-0.894698835662851));
#48052=DIRECTION('center_axis',(9.80312625669243E-17,1.,4.89411764412796E-17));
#48053=DIRECTION('ref_axis',(0.446669893168925,0.,-0.894698835662851));
#48054=DIRECTION('center_axis',(-1.22464679915E-16,-1.,-3.21507022015E-32));
#48055=DIRECTION('ref_axis',(1.,-1.22464679915E-16,-3.93732545414918E-48));
#48056=DIRECTION('center_axis',(0.965607221472844,-1.18252779300981E-16,
0.260005180408957));
#48057=DIRECTION('ref_axis',(0.260005180408957,3.6319060404761E-32,-0.965607221472844));
#48058=DIRECTION('center_axis',(1.22464679914936E-16,1.,1.40353954282933E-28));
#48059=DIRECTION('ref_axis',(0.35511183407264,-4.34886570935806E-17,-0.934823825809744));
#48060=DIRECTION('',(1.43023900113E-16,1.,0.));
#48061=DIRECTION('center_axis',(-1.22464679915E-16,-1.,-2.46519032882E-32));
#48062=DIRECTION('ref_axis',(1.,-1.22464679915E-16,-3.01898744548495E-48));
#48063=DIRECTION('center_axis',(1.14185737652554E-16,1.,3.07463352160911E-17));
#48064=DIRECTION('ref_axis',(0.260005180408958,0.,-0.965607221472844));
#48065=DIRECTION('center_axis',(-1.22464679915E-16,-1.,-3.08148791102E-32));
#48066=DIRECTION('ref_axis',(1.,-1.22464679915E-16,-3.77373430685006E-48));
#48067=DIRECTION('center_axis',(0.965607221472844,-1.18252779300981E-16,
-0.260005180408957));
#48068=DIRECTION('ref_axis',(0.260005180408957,3.6319060404761E-32,0.965607221472844));
#48069=DIRECTION('center_axis',(1.22464679915E-16,1.,3.03685191950031E-32));
#48070=DIRECTION('ref_axis',(-6.0392731067552E-15,7.69966167133047E-31,
-1.));
#48071=DIRECTION('',(0.,1.,0.));
#48072=DIRECTION('center_axis',(-1.22464679915E-16,-1.,-3.08148791102E-32));
#48073=DIRECTION('ref_axis',(1.,-1.22464679915E-16,-3.77373430685006E-48));
#48074=DIRECTION('center_axis',(1.14185737652555E-16,1.,-3.07463352160911E-17));
#48075=DIRECTION('ref_axis',(-0.260005180408958,0.,-0.965607221472844));
#48076=DIRECTION('center_axis',(-1.22464679915E-16,-1.,-3.21507022015E-32));
#48077=DIRECTION('ref_axis',(1.,-1.22464679915E-16,-3.93732545414918E-48));
#48078=DIRECTION('center_axis',(0.894698835662851,-1.09569006529982E-16,
-0.446669893168925));
#48079=DIRECTION('ref_axis',(0.446669893168925,-6.79741207737406E-32,0.894698835662851));
#48080=DIRECTION('center_axis',(1.22464679914936E-16,1.,-1.40336501664893E-28));
#48081=DIRECTION('ref_axis',(-0.35511183407264,4.34886570935806E-17,-0.934823825809744));
#48082=DIRECTION('',(-2.04649405461E-16,-1.,0.));
#48083=DIRECTION('center_axis',(-1.22464679915E-16,-1.,-3.08148791102E-32));
#48084=DIRECTION('ref_axis',(1.,-1.22464679915E-16,-3.77373430685006E-48));
#48085=DIRECTION('center_axis',(-2.44929359829E-16,5.34329236508E-33,1.));
#48086=DIRECTION('ref_axis',(-1.,-1.30872917835823E-48,-2.44929359829E-16));
#48087=DIRECTION('',(-2.71043176004E-16,0.,1.));
#48088=DIRECTION('center_axis',(1.15648231732E-16,-3.88147269699E-32,1.));
#48089=DIRECTION('ref_axis',(1.,4.48885453922931E-48,-1.15648231732E-16));
#48090=DIRECTION('center_axis',(1.,0.,0.));
#48091=DIRECTION('ref_axis',(0.,-1.,0.));
#48092=DIRECTION('center_axis',(1.22464679915E-16,1.,3.21507022015E-32));
#48093=DIRECTION('ref_axis',(1.,-1.22464679915E-16,-3.93732545414918E-48));
#48094=DIRECTION('center_axis',(1.22464679915E-16,1.,3.21507022015E-32));
#48095=DIRECTION('ref_axis',(-1.,1.22464679915E-16,3.93732545414918E-48));
#48096=DIRECTION('center_axis',(1.22464679915E-16,1.,3.08148791102E-32));
#48097=DIRECTION('ref_axis',(1.,-1.22464679915E-16,-3.77373430685006E-48));
#48098=DIRECTION('',(-1.43023900113E-16,-1.,0.));
#48099=DIRECTION('center_axis',(1.,-1.22464679915E-16,2.44929359829E-16));
#48100=DIRECTION('ref_axis',(-2.44929359829E-16,0.,1.));
#48101=DIRECTION('',(1.4098070154E-16,1.,0.));
#48102=DIRECTION('',(-2.54245135096E-16,0.,1.));
#48103=DIRECTION('center_axis',(-1.22464679915E-16,-1.,-3.21507022015E-32));
#48104=DIRECTION('ref_axis',(-1.,1.22464679915E-16,0.));
#48105=DIRECTION('center_axis',(-1.22464679915E-16,-1.,-3.21507022015E-32));
#48106=DIRECTION('ref_axis',(1.,-1.22464679915E-16,-3.93732545414918E-48));
#48107=DIRECTION('center_axis',(1.22464679915E-16,1.,3.38963670212E-32));
#48108=DIRECTION('ref_axis',(1.,-1.22464679915E-16,-4.15110773753262E-48));
#48109=DIRECTION('center_axis',(-1.22464679915E-16,-1.,-3.21507022015E-32));
#48110=DIRECTION('ref_axis',(1.,-1.22464679915E-16,-3.93732545414918E-48));
#48111=DIRECTION('center_axis',(1.22464679915E-16,1.,3.08148791102E-32));
#48112=DIRECTION('ref_axis',(1.,-1.22464679915E-16,-3.77373430685006E-48));
#48113=DIRECTION('center_axis',(-1.22464679915E-16,-1.,-3.21507022015E-32));
#48114=DIRECTION('ref_axis',(1.,-1.22464679915E-16,-3.93732545414918E-48));
#48115=DIRECTION('center_axis',(1.22464679915E-16,1.,3.69778549322E-32));
#48116=DIRECTION('ref_axis',(1.,-1.22464679915E-16,-4.52848116821518E-48));
#48117=DIRECTION('center_axis',(0.734238830876792,-8.99183234039869E-17,
-0.678891257295808));
#48118=DIRECTION('ref_axis',(2.09848214201023E-17,1.,-1.09753148030108E-16));
#48119=DIRECTION('center_axis',(0.734238830876792,-2.0982535965894E-15,
-0.678891257295808));
#48120=DIRECTION('ref_axis',(0.678891257295807,8.02543484770833E-30,0.734238830876791));
#48121=DIRECTION('center_axis',(0.734238830876792,-8.99183234042744E-17,
-0.678891257295808));
#48122=DIRECTION('ref_axis',(0.678891257295808,1.72414837744489E-31,0.734238830876792));
#48123=DIRECTION('',(0.734238830876791,0.,-0.678891257295807));
#48124=DIRECTION('center_axis',(-6.60215246509141E-17,-1.,6.10447636300053E-17));
#48125=DIRECTION('ref_axis',(-0.678891257295808,0.,-0.734238830876791));
#48126=DIRECTION('center_axis',(0.54648608815598,-6.69252438638976E-17,
0.837468181754969));
#48127=DIRECTION('ref_axis',(0.837468181754969,-2.14539310633749E-32,-0.54648608815598));
#48128=DIRECTION('center_axis',(-1.22464679915E-16,-1.,-3.21507022015E-32));
#48129=DIRECTION('ref_axis',(1.,-1.22464679915E-16,-3.93732545414918E-48));
#48130=DIRECTION('center_axis',(-8.12315922726109E-17,-1.,-5.78742547555248E-17));
#48131=DIRECTION('ref_axis',(-0.580253144566096,0.,0.814436178114134));
#48132=DIRECTION('center_axis',(0.814436178114135,-9.97396658637165E-17,
0.580253144566095));
#48133=DIRECTION('ref_axis',(0.580253144566095,-1.05208313255741E-31,-0.814436178114135));
#48134=DIRECTION('center_axis',(1.22464679915E-16,1.,3.21507022015E-32));
#48135=DIRECTION('ref_axis',(1.,-1.22464679915E-16,-3.93732545414918E-48));
#48136=DIRECTION('center_axis',(-8.12315922726109E-17,-1.,-5.78742547555248E-17));
#48137=DIRECTION('ref_axis',(0.580253144566096,0.,-0.814436178114134));
#48138=DIRECTION('center_axis',(-0.734238830876792,8.99183234042744E-17,
0.678891257295808));
#48139=DIRECTION('ref_axis',(0.678891257295808,1.51038693775819E-31,0.734238830876792));
#48140=DIRECTION('center_axis',(-1.22464679915E-16,-1.,-3.21507022015E-32));
#48141=DIRECTION('ref_axis',(1.,-1.22464679915E-16,-3.93732545414918E-48));
#48142=DIRECTION('center_axis',(0.734238830876792,-8.99183234042744E-17,
-0.678891257295808));
#48143=DIRECTION('ref_axis',(-0.678891257295808,1.09298769049165E-33,-0.734238830876792));
#48144=DIRECTION('center_axis',(-0.734238830876792,-3.99271497926887E-15,
0.678891257295808));
#48145=DIRECTION('ref_axis',(0.678891257295807,-1.5084889012382E-29,0.734238830876791));
#48146=DIRECTION('',(-0.734238830876791,0.,0.678891257295807));
#48147=DIRECTION('center_axis',(-0.734238830876792,8.99183234039869E-17,
-0.678891257295808));
#48148=DIRECTION('ref_axis',(6.60215246505446E-17,1.,6.10447636296637E-17));
#48149=DIRECTION('center_axis',(-0.734238830876792,2.56033960610927E-18,
-0.678891257295808));
#48150=DIRECTION('ref_axis',(0.678891257295807,9.76887763626404E-33,-0.734238830876791));
#48151=DIRECTION('center_axis',(-0.734238830876792,8.99183234042744E-17,
-0.678891257295808));
#48152=DIRECTION('ref_axis',(0.678891257295808,1.51038693775819E-31,-0.734238830876792));
#48153=DIRECTION('',(-0.734238830876791,0.,-0.678891257295807));
#48154=DIRECTION('center_axis',(-6.60215246509141E-17,-1.,-6.10447636300053E-17));
#48155=DIRECTION('ref_axis',(-0.678891257295808,0.,0.734238830876791));
#48156=DIRECTION('center_axis',(-1.22464679915E-16,-1.,-3.21507022015E-32));
#48157=DIRECTION('ref_axis',(1.,-1.22464679915E-16,-3.93732545414918E-48));
#48158=DIRECTION('center_axis',(-3.65737147181347E-17,-1.,5.60477622923109E-17));
#48159=DIRECTION('ref_axis',(-0.83746818175497,0.,-0.54648608815598));
#48160=DIRECTION('center_axis',(0.734238830876792,-8.99183234042744E-17,
0.678891257295808));
#48161=DIRECTION('ref_axis',(0.678891257295808,1.72414837744489E-31,-0.734238830876792));
#48162=DIRECTION('center_axis',(-1.22464679915E-16,-1.,-3.21507022015E-32));
#48163=DIRECTION('ref_axis',(1.,-1.22464679915E-16,-3.93732545414918E-48));
#48164=DIRECTION('center_axis',(-0.734238830876792,8.99183234042744E-17,
-0.678891257295808));
#48165=DIRECTION('ref_axis',(-0.678891257295808,1.01431800150836E-32,0.734238830876792));
#48166=DIRECTION('center_axis',(0.734238830876792,1.02275665268971E-14,
0.678891257295808));
#48167=DIRECTION('ref_axis',(0.678891257295807,-1.15648231731787E-14,-0.734238830876791));
#48168=DIRECTION('',(0.734238830876791,0.,0.678891257295807));
#48169=DIRECTION('center_axis',(-2.44929359829E-16,5.34329236504435E-33,
1.));
#48170=DIRECTION('ref_axis',(1.3087291783495E-48,1.,-5.34329236504435E-33));
#48171=DIRECTION('center_axis',(3.20552409216E-15,-3.67911578618E-31,-1.));
#48172=DIRECTION('ref_axis',(1.,1.15641341524065E-46,3.20552409216E-15));
#48173=DIRECTION('',(4.25315706605E-16,0.,-1.));
#48174=DIRECTION('center_axis',(2.44929359829E-16,-9.25185853854E-17,-1.));
#48175=DIRECTION('ref_axis',(1.,2.26605178907307E-32,2.44929359829E-16));
#48176=DIRECTION('center_axis',(-1.00043346337309E-45,-1.,3.37916382964629E-31));
#48177=DIRECTION('ref_axis',(1.,0.,2.96059473233375E-15));
#48178=DIRECTION('center_axis',(0.894698835662851,-1.09569006529982E-16,
0.446669893168925));
#48179=DIRECTION('ref_axis',(0.446669893168925,7.79859429427442E-32,-0.894698835662851));
#48180=DIRECTION('center_axis',(1.22464679915E-16,1.,3.21507022015E-32));
#48181=DIRECTION('ref_axis',(1.,-1.22464679915E-16,-3.93732545414918E-48));
#48182=DIRECTION('center_axis',(-1.14185737652555E-16,-1.,-3.07463352160911E-17));
#48183=DIRECTION('ref_axis',(0.260005180408958,0.,-0.965607221472844));
#48184=DIRECTION('center_axis',(0.965607221472844,-1.18252779300981E-16,
0.260005180408957));
#48185=DIRECTION('ref_axis',(0.260005180408957,3.6319060404761E-32,-0.965607221472844));
#48186=DIRECTION('center_axis',(-1.22464679915E-16,-1.,-3.21507022015E-32));
#48187=DIRECTION('ref_axis',(1.,-1.22464679915E-16,-3.93732545414918E-48));
#48188=DIRECTION('center_axis',(-1.14185737652555E-16,-1.,3.07463352160911E-17));
#48189=DIRECTION('ref_axis',(-0.260005180408958,0.,-0.965607221472844));
#48190=DIRECTION('center_axis',(0.965607221472844,-1.18252779300981E-16,
-0.260005180408957));
#48191=DIRECTION('ref_axis',(0.260005180408957,3.6319060404761E-32,0.965607221472844));
#48192=DIRECTION('center_axis',(-1.22464679915E-16,-1.,-3.21507022015E-32));
#48193=DIRECTION('ref_axis',(1.,-1.22464679915E-16,-3.93732545414918E-48));
#48194=DIRECTION('center_axis',(-9.80312625669243E-17,-1.,4.89411764412795E-17));
#48195=DIRECTION('ref_axis',(-0.446669893168925,0.,-0.894698835662851));
#48196=DIRECTION('center_axis',(0.894698835662851,-1.09569006529982E-16,
-0.446669893168925));
#48197=DIRECTION('ref_axis',(0.446669893168925,7.79859429427442E-32,0.894698835662851));
#48198=DIRECTION('center_axis',(-1.22464679915E-16,-1.,-3.21507022015E-32));
#48199=DIRECTION('ref_axis',(1.,-1.22464679915E-16,-3.93732545414918E-48));
#48200=DIRECTION('center_axis',(-9.80312625669243E-17,-1.,4.89411764412795E-17));
#48201=DIRECTION('ref_axis',(0.446669893168926,0.,0.894698835662851));
#48202=DIRECTION('center_axis',(-2.44929359829E-16,5.34329236508E-33,1.));
#48203=DIRECTION('ref_axis',(1.,1.30872917835823E-48,2.44929359829E-16));
#48204=DIRECTION('center_axis',(1.22464679915E-16,1.,3.21507022015E-32));
#48205=DIRECTION('ref_axis',(1.,-1.22464679915E-16,-3.93732545414918E-48));
#48206=DIRECTION('center_axis',(-2.44929359829E-16,5.34329236508E-33,1.));
#48207=DIRECTION('ref_axis',(1.,1.30872917835823E-48,2.44929359829E-16));
#48208=DIRECTION('center_axis',(5.67626010484E-15,-1.38777878078E-16,1.));
#48209=DIRECTION('ref_axis',(1.,-1.47314773920115E-32,-5.67626010484E-15));
#48210=DIRECTION('',(-4.25315706605E-16,0.,1.));
#48211=DIRECTION('center_axis',(-1.22464679915E-16,-1.,-3.21507022015E-32));
#48212=DIRECTION('ref_axis',(-1.,1.22464679915E-16,0.));
#48213=DIRECTION('center_axis',(-1.22464679915E-16,-1.,-3.08148791102E-32));
#48214=DIRECTION('ref_axis',(1.,-1.22464679915E-16,2.9554797906917E-48));
#48215=DIRECTION('center_axis',(-1.22464679915E-16,-1.,-3.08148791102E-32));
#48216=DIRECTION('ref_axis',(1.,-1.22464679915E-16,2.9554797906917E-48));
#48217=DIRECTION('center_axis',(-1.22464679915E-16,-1.,-2.46519032882E-32));
#48218=DIRECTION('ref_axis',(1.,-1.22464679915E-16,2.53931026341659E-48));
#48219=DIRECTION('center_axis',(0.221508968488806,0.953407602538901,0.204811426195051));
#48220=DIRECTION('ref_axis',(0.700028883437118,-0.301685172690054,0.647260086003111));
#48221=DIRECTION('center_axis',(-1.22464679915E-16,-1.,-2.46519032882E-32));
#48222=DIRECTION('ref_axis',(1.,-1.22464679915E-16,-3.01898744548495E-48));
#48223=DIRECTION('center_axis',(0.184321578630023,-2.25728831283027E-17,
-0.982865990688118));
#48224=DIRECTION('ref_axis',(0.982865990688118,3.73386811100911E-32,0.184321578630023));
#48225=DIRECTION('center_axis',(-0.678891257295897,3.86265093984168E-14,
0.734238830876709));
#48226=DIRECTION('ref_axis',(-0.70002888343712,0.301685172690054,-0.647260086003109));
#48227=DIRECTION('center_axis',(0.,0.235800057020902,-0.971801591431574));
#48228=DIRECTION('ref_axis',(0.,0.971801591431575,0.235800057020898));
#48229=DIRECTION('center_axis',(-0.905552945157821,1.10898251574978E-16,
-0.424233265451916));
#48230=DIRECTION('ref_axis',(0.424233265451916,2.2812757295719E-31,-0.905552945157821));
#48231=DIRECTION('center_axis',(-1.22464679915E-16,-1.,-3.08148791102E-32));
#48232=DIRECTION('ref_axis',(1.,-1.22464679915E-16,-3.77373430685006E-48));
#48233=DIRECTION('center_axis',(-1.,6.29350163966441E-17,-2.59373767181107E-16));
#48234=DIRECTION('ref_axis',(0.,-0.971801591431574,-0.235800057020901));
#48235=DIRECTION('center_axis',(-1.22464679915E-16,-1.,-3.08148791102E-32));
#48236=DIRECTION('ref_axis',(1.,-1.22464679915E-16,-3.77373430685006E-48));
#48237=DIRECTION('center_axis',(-1.16760731574493E-16,-1.,-2.58069211860055E-17));
#48238=DIRECTION('ref_axis',(0.215815367394074,0.,-0.976434189895336));
#48239=DIRECTION('center_axis',(-1.22464679915E-16,-1.,-3.21507022015E-32));
#48240=DIRECTION('ref_axis',(1.,-1.22464679915E-16,2.95348236287722E-48));
#48241=DIRECTION('center_axis',(-1.22464679915E-16,-1.,-2.46519032882E-32));
#48242=DIRECTION('ref_axis',(1.,-1.22464679915E-16,-3.01898744548495E-48));
#48243=DIRECTION('center_axis',(-0.201250650785258,-0.315250304640726,0.927424078284816));
#48244=DIRECTION('ref_axis',(-0.244245415585181,0.93304050163127,0.264158284521404));
#48245=DIRECTION('center_axis',(1.224646799149E-16,1.,1.07603845915075E-28));
#48246=DIRECTION('ref_axis',(-0.67889125729581,8.31402005216767E-17,0.734238830876789));
#48247=DIRECTION('',(0.,-1.,0.));
#48248=DIRECTION('center_axis',(-1.22464679915E-16,-1.,-3.08148791102001E-32));
#48249=DIRECTION('ref_axis',(-1.,1.22464679915E-16,5.78241158658936E-15));
#48250=DIRECTION('',(-9.55030558817E-17,-1.,0.));
#48251=DIRECTION('center_axis',(-0.922303035444809,-6.8218782867173E-7,
-0.386467477038916));
#48252=DIRECTION('ref_axis',(-0.273271953394989,0.707112642513919,0.652161138281536));
#48253=DIRECTION('center_axis',(1.04173678864568E-16,1.,4.36513558728617E-17));
#48254=DIRECTION('ref_axis',(0.386467796953067,0.,-0.922302901393161));
#48255=DIRECTION('center_axis',(1.22464679915E-16,1.,3.21507022015E-32));
#48256=DIRECTION('ref_axis',(1.,-1.22464679915E-16,2.95348236287722E-48));
#48257=DIRECTION('center_axis',(-0.976434189895336,1.19578700523041E-16,
-0.215815367394074));
#48258=DIRECTION('ref_axis',(0.215815367394074,2.78959734683971E-32,-0.976434189895336));
#48259=DIRECTION('center_axis',(-1.22464679914995E-16,-1.,-2.84643200354157E-29));
#48260=DIRECTION('ref_axis',(0.175818770215043,-2.15315894174053E-17,-0.984422551570244));
#48261=DIRECTION('',(0.,-1.,0.));
#48262=DIRECTION('',(-1.27905878413E-16,-1.,0.));
#48263=DIRECTION('center_axis',(1.16760731574493E-16,1.,2.58069211860055E-17));
#48264=DIRECTION('ref_axis',(0.215815367394074,0.,-0.976434189895336));
#48265=DIRECTION('center_axis',(1.22464679915E-16,1.,3.08148791102E-32));
#48266=DIRECTION('ref_axis',(1.,-1.22464679915E-16,-3.77373430685006E-48));
#48267=DIRECTION('center_axis',(-0.976434189895336,1.19578700523041E-16,
0.215815367394074));
#48268=DIRECTION('ref_axis',(0.215815367394074,2.78959734683971E-32,0.976434189895336));
#48269=DIRECTION('center_axis',(1.22464679914969E-16,1.,1.40937670198757E-28));
#48270=DIRECTION('ref_axis',(0.215815367394074,-2.64297598885091E-17,-0.976434189895336));
#48271=DIRECTION('',(-9.55030558817E-17,-1.,0.));
#48272=DIRECTION('center_axis',(-0.716038439225428,0.221273058165028,0.662062827292024));
#48273=DIRECTION('ref_axis',(0.162467271531971,0.97521189170882,-0.150220344662972));
#48274=DIRECTION('center_axis',(1.22464679915E-16,1.,2.46519032882E-32));
#48275=DIRECTION('ref_axis',(1.,-1.22464679915E-16,-3.01898744548495E-48));
#48276=DIRECTION('center_axis',(0.678891257295725,-4.93644477147132E-13,
0.734238830876867));
#48277=DIRECTION('ref_axis',(-0.162467271531966,-0.97521189170882,0.150220344662973));
#48278=DIRECTION('center_axis',(1.22464679915E-16,1.,2.46519032882E-32));
#48279=DIRECTION('ref_axis',(1.,-1.22464679915E-16,-3.01898744548495E-48));
#48280=DIRECTION('center_axis',(-0.184321578630023,2.25728831283027E-17,
-0.982865990688118));
#48281=DIRECTION('ref_axis',(0.982865990688118,3.73386811100911E-32,-0.184321578630023));
#48282=DIRECTION('center_axis',(-1.48029736616688E-15,0.958902687765847,
-0.283735150087956));
#48283=DIRECTION('ref_axis',(-7.4014868308344E-15,-0.28373515008795,-0.958902687765849));
#48284=DIRECTION('center_axis',(1.22464679915E-16,1.,2.46519032882E-32));
#48285=DIRECTION('ref_axis',(1.,-1.22464679915E-16,-3.01898744548495E-48));
#48286=DIRECTION('center_axis',(0.905552945157821,-1.10898251574978E-16,
-0.424233265451916));
#48287=DIRECTION('ref_axis',(0.424233265451916,8.51126007998586E-32,0.905552945157821));
#48288=DIRECTION('center_axis',(1.,-8.38443144529068E-16,-7.47061316104109E-15));
#48289=DIRECTION('ref_axis',(7.40148683083439E-15,0.28373515008795,0.958902687765849));
#48290=DIRECTION('center_axis',(-2.24037888703029E-16,-1.,2.20413632410453E-17));
#48291=DIRECTION('ref_axis',(-0.977255721664238,2.19472257881379E-16,0.212064269679052));
#48292=DIRECTION('center_axis',(-1.22464679915E-16,-1.,-3.21507022015E-32));
#48293=DIRECTION('ref_axis',(1.,-1.22464679915E-16,2.95348236287722E-48));
#48294=DIRECTION('center_axis',(-0.201250866957998,0.315250529579522,-0.927423954914086));
#48295=DIRECTION('ref_axis',(0.244245793120094,0.933040379819622,0.264158365699804));
#48296=DIRECTION('center_axis',(1.22464679915E-16,1.,2.46519032882E-32));
#48297=DIRECTION('ref_axis',(1.,-1.22464679915E-16,-3.01898744548495E-48));
#48298=DIRECTION('center_axis',(1.22464679915054E-16,1.,-1.00619139983431E-29));
#48299=DIRECTION('ref_axis',(-0.982865990688119,1.20366368949015E-16,0.184321578630021));
#48300=DIRECTION('',(1.91006111763E-16,1.,0.));
#48301=DIRECTION('center_axis',(1.16760731574493E-16,1.,-2.58069211860055E-17));
#48302=DIRECTION('ref_axis',(-0.215815367394074,0.,-0.976434189895336));
#48303=DIRECTION('center_axis',(1.22464679915E-16,1.,3.21507022015E-32));
#48304=DIRECTION('ref_axis',(1.,-1.22464679915E-16,2.95348236287722E-48));
#48305=DIRECTION('center_axis',(-0.922302870765176,-7.9241150460774E-8,
0.386467870046539));
#48306=DIRECTION('ref_axis',(-0.273273899979641,-0.707107039843237,-0.652166397320539));
#48307=DIRECTION('center_axis',(-1.22464679914968E-16,-1.,6.73818689876281E-29));
#48308=DIRECTION('ref_axis',(-0.424233265451918,5.19535910627899E-17,-0.905552945157821));
#48309=DIRECTION('',(9.55030558817E-17,1.,0.));
#48310=DIRECTION('center_axis',(-1.22464679914914E-16,-1.,-3.06469357969891E-29));
#48311=DIRECTION('ref_axis',(-0.941567095721782,1.15308712995973E-16,0.336825480410922));
#48312=DIRECTION('',(0.,-1.,0.));
#48313=DIRECTION('center_axis',(4.57540783324772E-17,1.,-5.92437580993829E-17));
#48314=DIRECTION('ref_axis',(0.791447785823259,0.,0.611236780892201));
#48315=DIRECTION('center_axis',(-0.299529302547155,-6.98450310923572E-8,
0.954087101325456));
#48316=DIRECTION('ref_axis',(-8.54331494437577E-8,0.999999999999995,4.63849662383584E-8));
#48317=DIRECTION('center_axis',(-0.611236780892201,7.48549167240244E-17,
0.791447785823259));
#48318=DIRECTION('ref_axis',(0.79144778582326,2.17825094235712E-31,0.611236780892201));
#48319=DIRECTION('center_axis',(-1.22464679915E-16,-1.,-3.69778549322E-32));
#48320=DIRECTION('ref_axis',(1.,-1.22464679915E-16,-4.52848116821518E-48));
#48321=DIRECTION('center_axis',(1.22464679914882E-16,1.,-9.11791729617953E-29));
#48322=DIRECTION('ref_axis',(0.79144778582326,-9.69243997601319E-17,0.611236780892201));
#48323=DIRECTION('',(-1.91006111763E-16,-1.,0.));
#48324=DIRECTION('center_axis',(1.09872665289959E-17,1.,3.49976006725472E-17));
#48325=DIRECTION('ref_axis',(-0.954087082104669,0.,0.299529363770896));
#48326=DIRECTION('center_axis',(-0.611236780892201,7.48549167240244E-17,
-0.791447785823259));
#48327=DIRECTION('ref_axis',(0.79144778582326,2.17825094235712E-31,-0.611236780892201));
#48328=DIRECTION('center_axis',(-0.299529300208521,-6.66484614947436E-8,
-0.954087102059654));
#48329=DIRECTION('ref_axis',(0.67464125064528,0.707106985515452,-0.211799183102824));
#48330=DIRECTION('center_axis',(-1.22464679915E-16,-1.,-3.38963670212E-32));
#48331=DIRECTION('ref_axis',(1.,-1.22464679915E-16,-4.15110773753262E-48));
#48332=DIRECTION('center_axis',(1.22464679914331E-16,1.,1.45106580954821E-28));
#48333=DIRECTION('ref_axis',(-0.977255721664238,1.19679309148029E-16,0.212064269679051));
#48334=DIRECTION('',(-1.91006111763E-16,-1.,0.));
#48335=DIRECTION('center_axis',(-0.194458884741274,0.964291220370907,0.17980040172582));
#48336=DIRECTION('ref_axis',(-0.708020058269897,-0.264844184975968,0.654648878996907));
#48337=DIRECTION('center_axis',(-1.22464679915E-16,-1.,-3.69778549322E-32));
#48338=DIRECTION('ref_axis',(1.,-1.22464679915E-16,-4.52848116821518E-48));
#48339=DIRECTION('center_axis',(0.823541624224482,-1.00854761407059E-16,
0.567255844544332));
#48340=DIRECTION('ref_axis',(0.567255844544332,2.21497266631789E-31,-0.823541624224482));
#48341=DIRECTION('center_axis',(-0.678891257295798,3.62846327058483E-15,
-0.7342388308768));
#48342=DIRECTION('ref_axis',(0.7080200582699,0.264844184975966,-0.654648878996905));
#48343=DIRECTION('center_axis',(0.710368265197812,0.252911675402861,0.656820076006183));
#48344=DIRECTION('ref_axis',(-0.185697572862959,0.967489371747782,-0.171699525298959));
#48345=DIRECTION('center_axis',(1.22464679915E-16,1.,3.69778549322E-32));
#48346=DIRECTION('ref_axis',(1.,-1.22464679915E-16,-4.52848116821518E-48));
#48347=DIRECTION('center_axis',(0.678891257295789,9.85612054934161E-14,
-0.734238830876809));
#48348=DIRECTION('ref_axis',(0.185697572862958,-0.967489371747782,0.171699525298964));
#48349=DIRECTION('center_axis',(1.22464679915E-16,1.,3.69778549322E-32));
#48350=DIRECTION('ref_axis',(1.,-1.22464679915E-16,-4.52848116821518E-48));
#48351=DIRECTION('center_axis',(-0.823541624224482,1.00854761407059E-16,
0.567255844544332));
#48352=DIRECTION('ref_axis',(0.567255844544332,2.21497266631789E-31,0.823541624224482));
#48353=DIRECTION('center_axis',(-4.57540783324772E-17,-1.,5.92437580993829E-17));
#48354=DIRECTION('ref_axis',(0.791447785823259,0.,0.611236780892201));
#48355=DIRECTION('center_axis',(-1.22464679915E-16,-1.,-3.21507022015E-32));
#48356=DIRECTION('ref_axis',(1.,-1.22464679915E-16,3.1731092887471E-48));
#48357=DIRECTION('center_axis',(4.57540783324772E-17,1.,5.92437580993829E-17));
#48358=DIRECTION('ref_axis',(-0.791447785823259,0.,0.611236780892201));
#48359=DIRECTION('center_axis',(-0.800318648295141,-2.90491584479981E-7,
-0.599574900401071));
#48360=DIRECTION('ref_axis',(-1.43841294430989E-7,0.999999999999947,-2.92495087409794E-7));
#48361=DIRECTION('center_axis',(-1.22464679915E-16,-1.,-3.21507022015E-32));
#48362=DIRECTION('ref_axis',(1.,-1.22464679915E-16,3.1731092887471E-48));
#48363=DIRECTION('center_axis',(1.224646799149E-16,1.,-1.07586726537792E-28));
#48364=DIRECTION('ref_axis',(-0.67889125729581,8.31402005216767E-17,-0.734238830876789));
#48365=DIRECTION('',(0.,-1.,0.));
#48366=DIRECTION('center_axis',(7.84398113463332E-17,1.,-5.8764805666941E-17));
#48367=DIRECTION('ref_axis',(0.599575127105149,0.,0.800318478455199));
#48368=DIRECTION('center_axis',(-0.80031675586116,2.87294455355871E-6,0.599577426425991));
#48369=DIRECTION('ref_axis',(0.424001176459416,-0.707044168099605,0.565960728953316));
#48370=DIRECTION('center_axis',(-1.22464679915E-16,-1.,-3.21507022015E-32));
#48371=DIRECTION('ref_axis',(1.,-1.22464679915E-16,3.1731092887471E-48));
#48372=DIRECTION('center_axis',(1.22464679914947E-16,1.,-7.73624659438748E-29));
#48373=DIRECTION('ref_axis',(0.567255844544333,-6.94688054319408E-17,0.82354162422448));
#48374=DIRECTION('',(0.,1.,0.));
#48375=DIRECTION('center_axis',(-1.22464679915E-16,-1.,-3.21507022014744E-32));
#48376=DIRECTION('ref_axis',(7.6571373978586E-16,-1.25923590250867E-31,
1.));
#48377=DIRECTION('axis',(0.,0.,1.));
#48378=DIRECTION('refdir',(1.,0.,0.));
#48379=DIRECTION('center_axis',(0.,-1.,0.));
#48380=DIRECTION('ref_axis',(-0.864870204545057,0.,-0.501995547082034));
#48381=DIRECTION('center_axis',(0.,-1.,0.));
#48382=DIRECTION('ref_axis',(1.,0.,0.));
#48383=DIRECTION('center_axis',(0.,-1.,0.));
#48384=DIRECTION('ref_axis',(1.,0.,0.));
#48385=DIRECTION('center_axis',(0.,-1.,0.));
#48386=DIRECTION('ref_axis',(1.,0.,0.));
#48387=DIRECTION('center_axis',(0.362576028100137,-1.34614541736051E-15,
0.931954196217351));
#48388=DIRECTION('ref_axis',(0.931954196217351,6.44102416595859E-31,-0.362576028100137));
#48389=DIRECTION('center_axis',(0.,-1.,0.));
#48390=DIRECTION('ref_axis',(1.,0.,0.));
#48391=DIRECTION('center_axis',(0.362576028100137,-9.99200722163376E-16,
-0.931954196217351));
#48392=DIRECTION('ref_axis',(0.931954196217351,4.30399528931578E-31,0.362576028100137));
#48393=DIRECTION('center_axis',(0.,1.,0.));
#48394=DIRECTION('ref_axis',(1.,0.,0.));
#48395=DIRECTION('center_axis',(0.,1.,0.));
#48396=DIRECTION('ref_axis',(1.,0.,0.));
#48397=DIRECTION('',(-0.838443593764828,0.,-0.544988385265888));
#48398=DIRECTION('center_axis',(0.,-1.,0.));
#48399=DIRECTION('ref_axis',(1.,0.,0.));
#48400=DIRECTION('',(0.,0.,1.));
#48401=DIRECTION('',(0.612862105001227,0.,0.790189876076292));
#48402=DIRECTION('center_axis',(0.790189876076292,0.,-0.612862105001227));
#48403=DIRECTION('ref_axis',(0.,-1.,0.));
#48404=DIRECTION('',(0.,1.,0.));
#48405=DIRECTION('',(0.612862105001227,0.,0.790189876076292));
#48406=DIRECTION('',(0.,1.,0.));
#48407=DIRECTION('center_axis',(1.,0.,0.));
#48408=DIRECTION('ref_axis',(0.,1.,0.));
#48409=DIRECTION('',(0.,1.,0.));
#48410=DIRECTION('',(0.,0.,1.));
#48411=DIRECTION('center_axis',(0.,1.,0.));
#48412=DIRECTION('ref_axis',(0.617975203688407,0.,0.786197588158519));
#48413=DIRECTION('',(0.,1.,0.));
#48414=DIRECTION('center_axis',(0.,-1.,0.));
#48415=DIRECTION('ref_axis',(1.,0.,0.));
#48416=DIRECTION('center_axis',(-0.544988385265888,0.,0.838443593764828));
#48417=DIRECTION('ref_axis',(0.,1.,0.));
#48418=DIRECTION('',(0.,1.,0.));
#48419=DIRECTION('',(-0.838443593764828,0.,-0.544988385265888));
#48420=DIRECTION('center_axis',(0.,1.,0.));
#48421=DIRECTION('ref_axis',(1.,0.,0.));
#48422=DIRECTION('',(-0.492017200046991,0.,0.870585478202984));
#48423=DIRECTION('',(0.61395827519323,0.,0.789338480198295));
#48424=DIRECTION('center_axis',(0.,1.,0.));
#48425=DIRECTION('ref_axis',(1.,0.,0.));
#48426=DIRECTION('',(-0.977071912385473,0.,-0.212909553631103));
#48427=DIRECTION('center_axis',(-0.789338480198295,0.,0.61395827519323));
#48428=DIRECTION('ref_axis',(0.,1.,0.));
#48429=DIRECTION('',(-0.61395827519323,0.,-0.789338480198295));
#48430=DIRECTION('',(0.,1.,0.));
#48431=DIRECTION('',(0.,1.,0.));
#48432=DIRECTION('center_axis',(-0.870585478202985,0.,-0.492017200046991));
#48433=DIRECTION('ref_axis',(-0.492017200046991,0.,0.870585478202985));
#48434=DIRECTION('',(0.,1.,0.));
#48435=DIRECTION('',(0.492017200046991,0.,-0.870585478202984));
#48436=DIRECTION('center_axis',(0.212909553631103,0.,-0.977071912385473));
#48437=DIRECTION('ref_axis',(0.,-1.,0.));
#48438=DIRECTION('',(0.,1.,0.));
#48439=DIRECTION('',(0.977071912385473,0.,0.212909553631103));
#48440=DIRECTION('center_axis',(0.,-1.,0.));
#48441=DIRECTION('ref_axis',(0.,0.,-1.));
#48442=DIRECTION('center_axis',(0.,-1.,0.));
#48443=DIRECTION('ref_axis',(1.,0.,0.));
#48444=DIRECTION('center_axis',(0.,-1.,0.));
#48445=DIRECTION('ref_axis',(1.,0.,0.));
#48446=DIRECTION('',(0.,-1.,0.));
#48447=DIRECTION('center_axis',(0.,-1.,0.));
#48448=DIRECTION('ref_axis',(1.,0.,-1.8432640466762E-15));
#48449=DIRECTION('center_axis',(0.,-1.,0.));
#48450=DIRECTION('ref_axis',(0.,0.,-1.));
#48451=DIRECTION('',(-1.,0.,0.));
#48452=DIRECTION('center_axis',(0.,-1.,0.));
#48453=DIRECTION('ref_axis',(1.,0.,0.));
#48454=DIRECTION('',(0.,0.,-1.));
#48455=DIRECTION('center_axis',(0.,1.,0.));
#48456=DIRECTION('ref_axis',(1.,0.,0.));
#48457=DIRECTION('',(0.,0.,-1.));
#48458=DIRECTION('center_axis',(0.,-1.,0.));
#48459=DIRECTION('ref_axis',(1.,0.,0.));
#48460=DIRECTION('center_axis',(0.,1.,0.));
#48461=DIRECTION('ref_axis',(1.,0.,0.));
#48462=DIRECTION('',(-1.,0.,0.));
#48463=DIRECTION('center_axis',(0.,-1.,0.));
#48464=DIRECTION('ref_axis',(1.,0.,0.));
#48465=DIRECTION('center_axis',(0.,-1.,0.));
#48466=DIRECTION('ref_axis',(1.,0.,0.));
#48467=DIRECTION('',(0.,0.,-1.));
#48468=DIRECTION('center_axis',(0.,1.,0.));
#48469=DIRECTION('ref_axis',(1.,0.,0.));
#48470=DIRECTION('center_axis',(0.,1.,0.));
#48471=DIRECTION('ref_axis',(1.,0.,0.));
#48472=DIRECTION('center_axis',(0.,-1.,0.));
#48473=DIRECTION('ref_axis',(1.,0.,0.));
#48474=DIRECTION('center_axis',(0.,-1.,0.));
#48475=DIRECTION('ref_axis',(1.,0.,0.));
#48476=DIRECTION('center_axis',(0.,1.,0.));
#48477=DIRECTION('ref_axis',(1.,0.,0.));
#48478=DIRECTION('center_axis',(0.,1.,0.));
#48479=DIRECTION('ref_axis',(1.,0.,0.));
#48480=DIRECTION('center_axis',(0.,1.,0.));
#48481=DIRECTION('ref_axis',(1.,0.,0.));
#48482=DIRECTION('',(0.,0.,-1.));
#48483=DIRECTION('center_axis',(0.,1.,0.));
#48484=DIRECTION('ref_axis',(1.,0.,0.));
#48485=DIRECTION('center_axis',(0.,-1.,0.));
#48486=DIRECTION('ref_axis',(1.,0.,0.));
#48487=DIRECTION('',(-1.,0.,0.));
#48488=DIRECTION('center_axis',(0.,1.,0.));
#48489=DIRECTION('ref_axis',(1.,0.,0.));
#48490=DIRECTION('center_axis',(0.,-1.,0.));
#48491=DIRECTION('ref_axis',(1.,0.,0.));
#48492=DIRECTION('',(0.,0.,-1.));
#48493=DIRECTION('center_axis',(0.,1.,0.));
#48494=DIRECTION('ref_axis',(1.,0.,0.));
#48495=DIRECTION('',(0.,0.,-1.));
#48496=DIRECTION('center_axis',(0.,-1.,0.));
#48497=DIRECTION('ref_axis',(1.,0.,0.));
#48498=DIRECTION('',(-1.,0.,0.));
#48499=DIRECTION('center_axis',(6.12323399573677E-17,1.,0.));
#48500=DIRECTION('ref_axis',(1.,0.,0.));
#48501=DIRECTION('center_axis',(0.,0.,1.));
#48502=DIRECTION('ref_axis',(1.,0.,0.));
#48503=DIRECTION('center_axis',(0.,1.,0.));
#48504=DIRECTION('ref_axis',(1.,0.,0.));
#48505=DIRECTION('center_axis',(0.,1.,0.));
#48506=DIRECTION('ref_axis',(1.,0.,0.));
#48507=DIRECTION('',(-1.,0.,0.));
#48508=DIRECTION('center_axis',(0.,1.,0.));
#48509=DIRECTION('ref_axis',(1.,0.,0.));
#48510=DIRECTION('',(0.,0.,-1.));
#48511=DIRECTION('',(-1.,0.,0.));
#48512=DIRECTION('',(0.,0.,-1.));
#48513=DIRECTION('',(-1.,0.,0.));
#48514=DIRECTION('',(0.,0.,-1.));
#48515=DIRECTION('center_axis',(0.,1.,0.));
#48516=DIRECTION('ref_axis',(1.,0.,0.));
#48517=DIRECTION('',(-1.,0.,0.));
#48518=DIRECTION('center_axis',(0.,1.,0.));
#48519=DIRECTION('ref_axis',(1.,0.,0.));
#48520=DIRECTION('',(0.,0.,-1.));
#48521=DIRECTION('center_axis',(0.,1.,0.));
#48522=DIRECTION('ref_axis',(1.,0.,0.));
#48523=DIRECTION('center_axis',(0.,1.,0.));
#48524=DIRECTION('ref_axis',(1.,0.,0.));
#48525=DIRECTION('center_axis',(0.,1.,0.));
#48526=DIRECTION('ref_axis',(1.,0.,0.));
#48527=DIRECTION('center_axis',(-1.,0.,0.));
#48528=DIRECTION('ref_axis',(0.,0.,1.));
#48529=DIRECTION('',(0.,0.,1.));
#48530=DIRECTION('',(0.,-1.,0.));
#48531=DIRECTION('',(0.,-1.,0.));
#48532=DIRECTION('',(0.,0.,-1.));
#48533=DIRECTION('',(0.,-1.,0.));
#48534=DIRECTION('',(0.,-1.,0.));
#48535=DIRECTION('center_axis',(1.,0.,0.));
#48536=DIRECTION('ref_axis',(0.,0.707106781186548,-0.707106781186547));
#48537=DIRECTION('',(1.,0.,0.));
#48538=DIRECTION('center_axis',(1.,0.,0.));
#48539=DIRECTION('ref_axis',(0.,0.707106781186548,-0.707106781186547));
#48540=DIRECTION('center_axis',(1.,0.,0.));
#48541=DIRECTION('ref_axis',(0.,1.,0.));
#48542=DIRECTION('',(0.,1.,0.));
#48543=DIRECTION('',(0.,0.,1.));
#48544=DIRECTION('',(0.,1.,0.));
#48545=DIRECTION('center_axis',(1.,0.,0.));
#48546=DIRECTION('ref_axis',(0.,1.,0.));
#48547=DIRECTION('',(0.,-1.,0.));
#48548=DIRECTION('',(0.,0.,-1.));
#48549=DIRECTION('center_axis',(0.,-1.,0.));
#48550=DIRECTION('ref_axis',(0.,0.,-1.));
#48551=DIRECTION('',(-1.,0.,0.));
#48552=DIRECTION('center_axis',(0.,1.,0.));
#48553=DIRECTION('ref_axis',(1.,0.,0.));
#48554=DIRECTION('center_axis',(0.,0.,-1.));
#48555=DIRECTION('ref_axis',(0.,-1.,0.));
#48556=DIRECTION('',(0.,-1.,0.));
#48557=DIRECTION('',(1.,0.,0.));
#48558=DIRECTION('center_axis',(1.,0.,0.));
#48559=DIRECTION('ref_axis',(0.,0.,1.));
#48560=DIRECTION('',(-1.,0.,0.));
#48561=DIRECTION('center_axis',(0.,0.,1.));
#48562=DIRECTION('ref_axis',(1.,0.,0.));
#48563=DIRECTION('',(0.,-1.,0.));
#48564=DIRECTION('',(-1.,0.,0.));
#48565=DIRECTION('center_axis',(0.,1.,0.));
#48566=DIRECTION('ref_axis',(1.,0.,0.));
#48567=DIRECTION('center_axis',(0.,1.,0.));
#48568=DIRECTION('ref_axis',(1.,0.,0.));
#48569=DIRECTION('center_axis',(0.,-1.,0.));
#48570=DIRECTION('ref_axis',(0.,0.,-1.));
#48571=DIRECTION('center_axis',(0.,-1.,0.));
#48572=DIRECTION('ref_axis',(1.,0.,0.));
#48573=DIRECTION('',(0.,0.,1.));
#48574=DIRECTION('',(-1.,0.,0.));
#48575=DIRECTION('center_axis',(1.,0.,0.));
#48576=DIRECTION('ref_axis',(0.,1.,0.));
#48577=DIRECTION('',(0.,1.,0.));
#48578=DIRECTION('',(0.,0.,-1.));
#48579=DIRECTION('center_axis',(1.,0.,0.));
#48580=DIRECTION('ref_axis',(0.,1.,0.));
#48581=DIRECTION('',(0.,1.,0.));
#48582=DIRECTION('center_axis',(0.,0.,1.));
#48583=DIRECTION('ref_axis',(1.,0.,0.));
#48584=DIRECTION('',(0.,-1.,0.));
#48585=DIRECTION('',(1.,0.,0.));
#48586=DIRECTION('center_axis',(1.,0.,0.));
#48587=DIRECTION('ref_axis',(0.,0.707106781186548,0.707106781186547));
#48588=DIRECTION('',(-1.,0.,0.));
#48589=DIRECTION('center_axis',(0.,-1.,0.));
#48590=DIRECTION('ref_axis',(0.,0.,-1.));
#48591=DIRECTION('center_axis',(0.,1.,0.));
#48592=DIRECTION('ref_axis',(1.,0.,0.));
#48593=DIRECTION('center_axis',(1.,0.,0.));
#48594=DIRECTION('ref_axis',(0.,1.,0.));
#48595=DIRECTION('',(0.,1.,0.));
#48596=DIRECTION('',(0.,0.,1.));
#48597=DIRECTION('',(0.,1.,0.));
#48598=DIRECTION('center_axis',(1.,0.,0.));
#48599=DIRECTION('ref_axis',(0.,1.,0.));
#48600=DIRECTION('',(0.,0.,-1.));
#48601=DIRECTION('center_axis',(0.,-1.,0.));
#48602=DIRECTION('ref_axis',(0.,0.,-1.));
#48603=DIRECTION('center_axis',(0.,1.,0.));
#48604=DIRECTION('ref_axis',(1.,0.,0.));
#48605=DIRECTION('',(-1.,0.,0.));
#48606=DIRECTION('center_axis',(1.,0.,0.));
#48607=DIRECTION('ref_axis',(0.,0.707106781187215,0.70710678118588));
#48608=DIRECTION('',(1.,0.,0.));
#48609=DIRECTION('center_axis',(0.,0.,1.));
#48610=DIRECTION('ref_axis',(1.,0.,0.));
#48611=DIRECTION('',(-1.,0.,0.));
#48612=DIRECTION('',(0.,-1.,0.));
#48613=DIRECTION('center_axis',(0.,-1.,0.));
#48614=DIRECTION('ref_axis',(0.,0.,-1.));
#48615=DIRECTION('center_axis',(0.,-1.,0.));
#48616=DIRECTION('ref_axis',(1.,0.,0.));
#48617=DIRECTION('center_axis',(0.,1.,0.));
#48618=DIRECTION('ref_axis',(1.,0.,0.));
#48619=DIRECTION('center_axis',(0.,1.,0.));
#48620=DIRECTION('ref_axis',(1.,0.,0.));
#48621=DIRECTION('',(0.,0.,1.));
#48622=DIRECTION('',(-1.,0.,0.));
#48623=DIRECTION('center_axis',(1.,0.,0.));
#48624=DIRECTION('ref_axis',(0.,1.,0.));
#48625=DIRECTION('',(0.,1.,0.));
#48626=DIRECTION('',(0.,0.,-1.));
#48627=DIRECTION('',(0.,-1.,0.));
#48628=DIRECTION('center_axis',(1.,0.,0.));
#48629=DIRECTION('ref_axis',(0.,1.,0.));
#48630=DIRECTION('',(0.,1.,0.));
#48631=DIRECTION('center_axis',(0.,0.,1.));
#48632=DIRECTION('ref_axis',(1.,0.,0.));
#48633=DIRECTION('',(-1.,0.,0.));
#48634=DIRECTION('',(0.,-1.,0.));
#48635=DIRECTION('center_axis',(1.,0.,0.));
#48636=DIRECTION('ref_axis',(0.,0.,1.));
#48637=DIRECTION('',(1.,0.,0.));
#48638=DIRECTION('center_axis',(0.,0.,-1.));
#48639=DIRECTION('ref_axis',(0.,-1.,0.));
#48640=DIRECTION('',(0.,-1.,0.));
#48641=DIRECTION('',(-1.,0.,0.));
#48642=DIRECTION('center_axis',(0.,-1.,0.));
#48643=DIRECTION('ref_axis',(0.,0.,-1.));
#48644=DIRECTION('center_axis',(0.,1.,0.));
#48645=DIRECTION('ref_axis',(1.,0.,0.));
#48646=DIRECTION('center_axis',(0.,1.,0.));
#48647=DIRECTION('ref_axis',(1.,0.,0.));
#48648=DIRECTION('center_axis',(0.,-1.,0.));
#48649=DIRECTION('ref_axis',(1.,0.,0.));
#48650=DIRECTION('',(0.,0.,-1.));
#48651=DIRECTION('center_axis',(0.,1.,0.));
#48652=DIRECTION('ref_axis',(1.,0.,0.));
#48653=DIRECTION('center_axis',(0.,-1.,0.));
#48654=DIRECTION('ref_axis',(1.,0.,0.));
#48655=DIRECTION('',(0.,0.,-1.));
#48656=DIRECTION('center_axis',(0.,1.,0.));
#48657=DIRECTION('ref_axis',(0.,0.,1.));
#48658=DIRECTION('',(0.,-1.,0.));
#48659=DIRECTION('',(0.,1.,0.));
#48660=DIRECTION('center_axis',(0.,1.,0.));
#48661=DIRECTION('ref_axis',(0.,0.,1.));
#48662=DIRECTION('',(0.,-1.,0.));
#48663=DIRECTION('',(0.,1.,0.));
#48664=DIRECTION('center_axis',(0.,-1.,0.));
#48665=DIRECTION('ref_axis',(0.,0.,-1.));
#48666=DIRECTION('center_axis',(0.,1.,0.));
#48667=DIRECTION('ref_axis',(1.,0.,0.));
#48668=DIRECTION('center_axis',(0.,-1.,0.));
#48669=DIRECTION('ref_axis',(1.,0.,0.));
#48670=DIRECTION('',(-1.,0.,0.));
#48671=DIRECTION('center_axis',(0.,-1.,0.));
#48672=DIRECTION('ref_axis',(1.,0.,0.));
#48673=DIRECTION('center_axis',(-1.,0.,0.));
#48674=DIRECTION('ref_axis',(0.,0.,1.));
#48675=DIRECTION('',(0.,0.,-1.));
#48676=DIRECTION('center_axis',(-1.,0.,0.));
#48677=DIRECTION('ref_axis',(0.,0.,1.));
#48678=DIRECTION('',(0.,0.,-1.));
#48679=DIRECTION('center_axis',(0.,-1.,0.));
#48680=DIRECTION('ref_axis',(3.06161699786735E-16,0.,1.));
#48681=DIRECTION('center_axis',(0.,1.,0.));
#48682=DIRECTION('ref_axis',(1.,0.,0.));
#48683=DIRECTION('',(0.,1.,0.));
#48684=DIRECTION('',(0.,-1.,0.));
#48685=DIRECTION('center_axis',(0.,-1.,0.));
#48686=DIRECTION('ref_axis',(-0.707106781186548,0.,-0.707106781186548));
#48687=DIRECTION('center_axis',(0.,-1.,0.));
#48688=DIRECTION('ref_axis',(1.,0.,0.));
#48689=DIRECTION('',(0.,-1.,0.));
#48690=DIRECTION('center_axis',(0.,0.,1.));
#48691=DIRECTION('ref_axis',(1.,0.,0.));
#48692=DIRECTION('',(0.,-1.,0.));
#48693=DIRECTION('',(-1.,0.,0.));
#48694=DIRECTION('center_axis',(0.,-1.,0.));
#48695=DIRECTION('ref_axis',(0.707106781186548,0.,-0.707106781186548));
#48696=DIRECTION('center_axis',(0.,-1.,0.));
#48697=DIRECTION('ref_axis',(1.,0.,0.));
#48698=DIRECTION('center_axis',(1.,0.,0.));
#48699=DIRECTION('ref_axis',(0.,0.707106781186548,-0.707106781186547));
#48700=DIRECTION('center_axis',(-1.,0.,0.));
#48701=DIRECTION('ref_axis',(0.,0.707106781186548,-0.707106781186547));
#48702=DIRECTION('',(1.,0.,0.));
#48703=DIRECTION('center_axis',(0.,-1.,0.));
#48704=DIRECTION('ref_axis',(0.,0.,-1.));
#48705=DIRECTION('center_axis',(0.,-1.,0.));
#48706=DIRECTION('ref_axis',(1.,0.,0.));
#48707=DIRECTION('',(1.,0.,0.));
#48708=DIRECTION('',(0.,0.,-1.));
#48709=DIRECTION('center_axis',(0.,0.,-1.));
#48710=DIRECTION('ref_axis',(0.,-1.,0.));
#48711=DIRECTION('',(0.,-1.,0.));
#48712=DIRECTION('',(-1.,0.,0.));
#48713=DIRECTION('',(0.,-1.,0.));
#48714=DIRECTION('center_axis',(1.,0.,0.));
#48715=DIRECTION('ref_axis',(0.,0.,1.));
#48716=DIRECTION('',(1.,0.,0.));
#48717=DIRECTION('center_axis',(1.,0.,0.));
#48718=DIRECTION('ref_axis',(0.,1.,0.));
#48719=DIRECTION('center_axis',(0.,0.,1.));
#48720=DIRECTION('ref_axis',(1.,0.,0.));
#48721=DIRECTION('',(-1.,0.,0.));
#48722=DIRECTION('',(0.,1.,0.));
#48723=DIRECTION('',(0.,-1.,0.));
#48724=DIRECTION('center_axis',(0.,0.,1.));
#48725=DIRECTION('ref_axis',(1.,0.,0.));
#48726=DIRECTION('',(0.,-1.,0.));
#48727=DIRECTION('',(1.,0.,0.));
#48728=DIRECTION('',(0.,1.,0.));
#48729=DIRECTION('',(-1.,0.,0.));
#48730=DIRECTION('center_axis',(1.,0.,0.));
#48731=DIRECTION('ref_axis',(0.,0.,1.));
#48732=DIRECTION('',(-1.,0.,0.));
#48733=DIRECTION('center_axis',(1.,0.,0.));
#48734=DIRECTION('ref_axis',(0.,1.,0.));
#48735=DIRECTION('center_axis',(0.,0.,-1.));
#48736=DIRECTION('ref_axis',(0.,-1.,0.));
#48737=DIRECTION('',(0.,-1.,0.));
#48738=DIRECTION('',(0.,-1.,0.));
#48739=DIRECTION('',(1.,0.,0.));
#48740=DIRECTION('center_axis',(0.,-1.,0.));
#48741=DIRECTION('ref_axis',(0.,0.,-1.));
#48742=DIRECTION('center_axis',(0.,-1.,0.));
#48743=DIRECTION('ref_axis',(1.,0.,0.));
#48744=DIRECTION('',(0.,0.,-1.));
#48745=DIRECTION('center_axis',(0.,-1.,0.));
#48746=DIRECTION('ref_axis',(0.,0.,-1.));
#48747=DIRECTION('',(0.,0.,-1.));
#48748=DIRECTION('center_axis',(0.,-1.,0.));
#48749=DIRECTION('ref_axis',(1.,0.,0.));
#48750=DIRECTION('',(1.,0.,0.));
#48751=DIRECTION('center_axis',(1.,0.,0.));
#48752=DIRECTION('ref_axis',(0.,0.707106781187215,0.70710678118588));
#48753=DIRECTION('',(-1.,0.,0.));
#48754=DIRECTION('center_axis',(1.,0.,0.));
#48755=DIRECTION('ref_axis',(0.,1.,0.));
#48756=DIRECTION('center_axis',(0.,0.,1.));
#48757=DIRECTION('ref_axis',(1.,0.,0.));
#48758=DIRECTION('',(0.,-1.,0.));
#48759=DIRECTION('',(-1.,0.,0.));
#48760=DIRECTION('',(0.,1.,0.));
#48761=DIRECTION('center_axis',(0.,-1.,0.));
#48762=DIRECTION('ref_axis',(0.,0.,-1.));
#48763=DIRECTION('',(0.,0.,-1.));
#48764=DIRECTION('',(1.,0.,0.));
#48765=DIRECTION('center_axis',(0.,-1.,0.));
#48766=DIRECTION('ref_axis',(1.,0.,0.));
#48767=DIRECTION('center_axis',(1.,0.,0.));
#48768=DIRECTION('ref_axis',(0.,0.707106781186548,0.707106781186547));
#48769=DIRECTION('',(-1.,0.,0.));
#48770=DIRECTION('center_axis',(1.,0.,0.));
#48771=DIRECTION('ref_axis',(0.,1.,0.));
#48772=DIRECTION('center_axis',(0.,0.,1.));
#48773=DIRECTION('ref_axis',(1.,0.,0.));
#48774=DIRECTION('',(0.,1.,0.));
#48775=DIRECTION('',(-1.,0.,0.));
#48776=DIRECTION('',(0.,-1.,0.));
#48777=DIRECTION('center_axis',(0.,0.,-1.));
#48778=DIRECTION('ref_axis',(1.,0.,0.));
#48779=DIRECTION('center_axis',(-6.12323399574E-17,0.,1.));
#48780=DIRECTION('ref_axis',(1.,0.,6.12323399574E-17));
#48781=DIRECTION('center_axis',(2.96059473233E-15,0.,1.));
#48782=DIRECTION('ref_axis',(1.,0.,-2.96059473233E-15));
#48783=DIRECTION('',(0.,0.,1.));
#48784=DIRECTION('center_axis',(0.,1.,0.));
#48785=DIRECTION('ref_axis',(1.,0.,0.));
#48786=DIRECTION('',(-1.,0.,0.));
#48787=DIRECTION('center_axis',(0.,-1.,0.));
#48788=DIRECTION('ref_axis',(1.,0.,0.));
#48789=DIRECTION('center_axis',(0.,1.,0.));
#48790=DIRECTION('ref_axis',(1.,0.,0.));
#48791=DIRECTION('',(0.,0.,-1.));
#48792=DIRECTION('center_axis',(0.,1.,0.));
#48793=DIRECTION('ref_axis',(1.,0.,0.));
#48794=DIRECTION('center_axis',(0.,-1.,0.));
#48795=DIRECTION('ref_axis',(1.,0.,0.));
#48796=DIRECTION('center_axis',(0.,1.,0.));
#48797=DIRECTION('ref_axis',(1.,0.,0.));
#48798=DIRECTION('center_axis',(0.,1.,0.));
#48799=DIRECTION('ref_axis',(1.,0.,0.));
#48800=DIRECTION('center_axis',(0.,-1.,0.));
#48801=DIRECTION('ref_axis',(1.,0.,0.));
#48802=DIRECTION('center_axis',(0.,1.,0.));
#48803=DIRECTION('ref_axis',(1.,0.,0.));
#48804=DIRECTION('',(0.,0.,-1.));
#48805=DIRECTION('center_axis',(0.,1.,0.));
#48806=DIRECTION('ref_axis',(1.,0.,0.));
#48807=DIRECTION('center_axis',(0.,-1.,0.));
#48808=DIRECTION('ref_axis',(1.,0.,0.));
#48809=DIRECTION('center_axis',(0.,1.,0.));
#48810=DIRECTION('ref_axis',(1.,0.,0.));
#48811=DIRECTION('',(0.,0.,1.));
#48812=DIRECTION('center_axis',(0.,1.,0.));
#48813=DIRECTION('ref_axis',(1.,0.,0.));
#48814=DIRECTION('center_axis',(0.,-1.,0.));
#48815=DIRECTION('ref_axis',(1.,0.,0.));
#48816=DIRECTION('center_axis',(0.,1.,0.));
#48817=DIRECTION('ref_axis',(1.,0.,0.));
#48818=DIRECTION('center_axis',(0.,1.,0.));
#48819=DIRECTION('ref_axis',(1.,0.,0.));
#48820=DIRECTION('center_axis',(0.,-1.,0.));
#48821=DIRECTION('ref_axis',(1.,0.,0.));
#48822=DIRECTION('center_axis',(0.,1.,0.));
#48823=DIRECTION('ref_axis',(1.,0.,0.));
#48824=DIRECTION('',(0.,0.,-1.));
#48825=DIRECTION('center_axis',(0.,1.,0.));
#48826=DIRECTION('ref_axis',(1.,0.,0.));
#48827=DIRECTION('center_axis',(0.,-1.,0.));
#48828=DIRECTION('ref_axis',(1.,0.,0.));
#48829=DIRECTION('',(-1.,0.,0.));
#48830=DIRECTION('center_axis',(0.,-1.,0.));
#48831=DIRECTION('ref_axis',(1.,0.,0.));
#48832=DIRECTION('center_axis',(0.,1.,0.));
#48833=DIRECTION('ref_axis',(1.,0.,0.));
#48834=DIRECTION('center_axis',(0.,1.,0.));
#48835=DIRECTION('ref_axis',(1.,0.,0.));
#48836=DIRECTION('',(1.,0.,0.));
#48837=DIRECTION('center_axis',(0.,1.,0.));
#48838=DIRECTION('ref_axis',(1.,0.,0.));
#48839=DIRECTION('',(0.,0.,-1.));
#48840=DIRECTION('center_axis',(0.,1.,0.));
#48841=DIRECTION('ref_axis',(1.,0.,0.));
#48842=DIRECTION('center_axis',(0.,-1.,0.));
#48843=DIRECTION('ref_axis',(-0.873189157202533,0.,0.487381468404298));
#48844=DIRECTION('',(0.,-1.,0.));
#48845=DIRECTION('',(0.,1.,0.));
#48846=DIRECTION('center_axis',(0.,-1.,0.));
#48847=DIRECTION('ref_axis',(1.,0.,0.));
#48848=DIRECTION('center_axis',(0.,0.,-1.));
#48849=DIRECTION('ref_axis',(0.,-1.,0.));
#48850=DIRECTION('',(0.,-1.,0.));
#48851=DIRECTION('',(-1.,0.,0.));
#48852=DIRECTION('center_axis',(0.,-1.,0.));
#48853=DIRECTION('ref_axis',(3.06161699786735E-16,0.,1.));
#48854=DIRECTION('center_axis',(0.,-1.,0.));
#48855=DIRECTION('ref_axis',(1.,0.,0.));
#48856=DIRECTION('',(0.,-1.,0.));
#48857=DIRECTION('center_axis',(0.,0.,-1.));
#48858=DIRECTION('ref_axis',(0.,-1.,0.));
#48859=DIRECTION('',(0.,1.,0.));
#48860=DIRECTION('',(-1.,0.,0.));
#48861=DIRECTION('center_axis',(0.,-1.,0.));
#48862=DIRECTION('ref_axis',(0.543088776464994,0.,-0.839675282997991));
#48863=DIRECTION('',(0.,-1.,0.));
#48864=DIRECTION('center_axis',(0.,-1.,0.));
#48865=DIRECTION('ref_axis',(1.,0.,0.));
#48866=DIRECTION('center_axis',(0.,1.,0.));
#48867=DIRECTION('ref_axis',(-1.,0.,0.));
#48868=DIRECTION('',(0.,-1.,0.));
#48869=DIRECTION('center_axis',(0.,-1.,0.));
#48870=DIRECTION('ref_axis',(1.,0.,0.));
#48871=DIRECTION('center_axis',(1.,0.,0.));
#48872=DIRECTION('ref_axis',(0.,1.,0.));
#48873=DIRECTION('',(0.,1.,0.));
#48874=DIRECTION('',(0.,0.,1.));
#48875=DIRECTION('center_axis',(0.,-1.,0.));
#48876=DIRECTION('ref_axis',(0.418360127903027,0.,-0.90828123584106));
#48877=DIRECTION('center_axis',(0.,-1.,0.));
#48878=DIRECTION('ref_axis',(1.,0.,0.));
#48879=DIRECTION('',(0.,1.,0.));
#48880=DIRECTION('center_axis',(0.,-1.,0.));
#48881=DIRECTION('ref_axis',(-0.429581475917968,0.,-0.903028103409933));
#48882=DIRECTION('center_axis',(0.,-1.,0.));
#48883=DIRECTION('ref_axis',(1.,0.,0.));
#48884=DIRECTION('',(0.,1.,0.));
#48885=DIRECTION('center_axis',(0.,1.,0.));
#48886=DIRECTION('ref_axis',(0.344636603387807,0.,-0.938736177850473));
#48887=DIRECTION('center_axis',(0.,-1.,0.));
#48888=DIRECTION('ref_axis',(1.,0.,0.));
#48889=DIRECTION('',(0.,-1.,0.));
#48890=DIRECTION('center_axis',(0.,1.,0.));
#48891=DIRECTION('ref_axis',(-0.307788100148132,0.,0.951454930833407));
#48892=DIRECTION('',(0.,-1.,0.));
#48893=DIRECTION('center_axis',(0.,-1.,0.));
#48894=DIRECTION('ref_axis',(1.,0.,0.));
#48895=DIRECTION('center_axis',(0.,-1.,0.));
#48896=DIRECTION('ref_axis',(-0.329929783129,0.,-0.944005475728002));
#48897=DIRECTION('',(0.,-1.,0.));
#48898=DIRECTION('center_axis',(0.,-1.,0.));
#48899=DIRECTION('ref_axis',(1.,0.,0.));
#48900=DIRECTION('center_axis',(0.,1.,0.));
#48901=DIRECTION('ref_axis',(-1.,0.,0.));
#48902=DIRECTION('',(0.,-1.,0.));
#48903=DIRECTION('center_axis',(0.,-1.,0.));
#48904=DIRECTION('ref_axis',(1.,0.,0.));
#48905=DIRECTION('center_axis',(1.,0.,0.));
#48906=DIRECTION('ref_axis',(0.,1.,0.));
#48907=DIRECTION('',(0.,0.,1.));
#48908=DIRECTION('',(0.,1.,0.));
#48909=DIRECTION('center_axis',(0.,-1.,0.));
#48910=DIRECTION('ref_axis',(0.186470178118022,0.,-0.982460621436113));
#48911=DIRECTION('center_axis',(0.,-1.,0.));
#48912=DIRECTION('ref_axis',(1.,0.,0.));
#48913=DIRECTION('',(0.,1.,0.));
#48914=DIRECTION('center_axis',(0.,-1.,0.));
#48915=DIRECTION('ref_axis',(-0.429581475917968,0.,-0.903028103409933));
#48916=DIRECTION('',(0.,1.,0.));
#48917=DIRECTION('center_axis',(0.,-1.,0.));
#48918=DIRECTION('ref_axis',(1.,0.,0.));
#48919=DIRECTION('center_axis',(0.,1.,0.));
#48920=DIRECTION('ref_axis',(-0.186470178118022,0.,-0.982460621436113));
#48921=DIRECTION('center_axis',(0.,-1.,0.));
#48922=DIRECTION('ref_axis',(1.,0.,0.));
#48923=DIRECTION('',(0.,1.,0.));
#48924=DIRECTION('center_axis',(1.,0.,0.));
#48925=DIRECTION('ref_axis',(0.,1.,0.));
#48926=DIRECTION('',(0.,-1.,0.));
#48927=DIRECTION('',(0.,0.,-1.));
#48928=DIRECTION('center_axis',(0.,-1.,0.));
#48929=DIRECTION('ref_axis',(1.,0.,1.15648231731787E-14));
#48930=DIRECTION('',(0.,-1.,0.));
#48931=DIRECTION('center_axis',(0.,-1.,0.));
#48932=DIRECTION('ref_axis',(1.,0.,0.));
#48933=DIRECTION('center_axis',(0.,-1.,0.));
#48934=DIRECTION('ref_axis',(-0.329929783129,0.,-0.944005475728002));
#48935=DIRECTION('',(0.,-1.,0.));
#48936=DIRECTION('center_axis',(0.,-1.,0.));
#48937=DIRECTION('ref_axis',(1.,0.,0.));
#48938=DIRECTION('center_axis',(0.,1.,0.));
#48939=DIRECTION('ref_axis',(-1.,0.,0.));
#48940=DIRECTION('',(0.,1.,0.));
#48941=DIRECTION('center_axis',(0.,-1.,0.));
#48942=DIRECTION('ref_axis',(1.,0.,0.));
#48943=DIRECTION('center_axis',(0.,1.,0.));
#48944=DIRECTION('ref_axis',(0.902179063668487,0.,-0.43136172416923));
#48945=DIRECTION('center_axis',(0.,-1.,0.));
#48946=DIRECTION('ref_axis',(1.,0.,0.));
#48947=DIRECTION('',(0.,1.,0.));
#48948=DIRECTION('center_axis',(0.,-1.,0.));
#48949=DIRECTION('ref_axis',(-0.429581475917968,0.,-0.903028103409933));
#48950=DIRECTION('',(0.,1.,0.));
#48951=DIRECTION('center_axis',(0.,-1.,0.));
#48952=DIRECTION('ref_axis',(1.,0.,0.));
#48953=DIRECTION('center_axis',(0.,1.,0.));
#48954=DIRECTION('ref_axis',(-0.418360127903027,0.,-0.90828123584106));
#48955=DIRECTION('center_axis',(0.,-1.,0.));
#48956=DIRECTION('ref_axis',(1.,0.,0.));
#48957=DIRECTION('',(0.,1.,0.));
#48958=DIRECTION('center_axis',(1.,0.,0.));
#48959=DIRECTION('ref_axis',(0.,1.,0.));
#48960=DIRECTION('',(0.,-1.,0.));
#48961=DIRECTION('',(0.,0.,-1.));
#48962=DIRECTION('center_axis',(0.,-1.,0.));
#48963=DIRECTION('ref_axis',(1.,0.,5.78241158658936E-15));
#48964=DIRECTION('center_axis',(0.,-1.,0.));
#48965=DIRECTION('ref_axis',(1.,0.,0.));
#48966=DIRECTION('center_axis',(0.,-1.,0.));
#48967=DIRECTION('ref_axis',(0.,0.,-1.));
#48968=DIRECTION('center_axis',(0.,-1.,0.));
#48969=DIRECTION('ref_axis',(1.,0.,0.));
#48970=DIRECTION('',(0.,0.,1.));
#48971=DIRECTION('center_axis',(1.,0.,0.));
#48972=DIRECTION('ref_axis',(0.,1.,0.));
#48973=DIRECTION('',(0.,1.,0.));
#48974=DIRECTION('center_axis',(1.,0.,0.));
#48975=DIRECTION('ref_axis',(0.,1.,0.));
#48976=DIRECTION('',(0.,1.,0.));
#48977=DIRECTION('',(0.,0.,1.));
#48978=DIRECTION('center_axis',(0.,1.,0.));
#48979=DIRECTION('ref_axis',(1.,0.,0.));
#48980=DIRECTION('center_axis',(0.,1.,0.));
#48981=DIRECTION('ref_axis',(1.,0.,0.));
#48982=DIRECTION('center_axis',(0.,1.,0.));
#48983=DIRECTION('ref_axis',(1.,0.,0.));
#48984=DIRECTION('center_axis',(0.,1.,0.));
#48985=DIRECTION('ref_axis',(1.,0.,0.));
#48986=DIRECTION('',(0.,0.,1.));
#48987=DIRECTION('center_axis',(1.,0.,0.));
#48988=DIRECTION('ref_axis',(0.,1.,0.));
#48989=DIRECTION('',(0.,1.,0.));
#48990=DIRECTION('center_axis',(0.,1.,0.));
#48991=DIRECTION('ref_axis',(1.07187543957E-15,0.,-1.));
#48992=DIRECTION('',(0.,-1.,0.));
#48993=DIRECTION('center_axis',(0.,-1.,0.));
#48994=DIRECTION('ref_axis',(1.,0.,0.));
#48995=DIRECTION('center_axis',(0.,-1.,0.));
#48996=DIRECTION('ref_axis',(1.,0.,0.));
#48997=DIRECTION('',(0.,1.,0.));
#48998=DIRECTION('center_axis',(1.,0.,0.));
#48999=DIRECTION('ref_axis',(0.,1.,0.));
#49000=DIRECTION('',(0.,0.,1.));
#49001=DIRECTION('center_axis',(0.,-1.,0.));
#49002=DIRECTION('ref_axis',(0.,0.,-1.));
#49003=DIRECTION('center_axis',(0.,1.,0.));
#49004=DIRECTION('ref_axis',(-1.,0.,0.));
#49005=DIRECTION('center_axis',(0.,1.,0.));
#49006=DIRECTION('ref_axis',(1.,0.,0.));
#49007=DIRECTION('center_axis',(1.,0.,0.));
#49008=DIRECTION('ref_axis',(0.,-1.,0.));
#49009=DIRECTION('center_axis',(0.,-1.,0.));
#49010=DIRECTION('ref_axis',(0.,0.,1.));
#49011=DIRECTION('',(0.,-1.,0.));
#49012=DIRECTION('center_axis',(-1.,0.,0.));
#49013=DIRECTION('ref_axis',(0.,0.,-1.));
#49014=DIRECTION('',(1.,0.,0.));
#49015=DIRECTION('center_axis',(1.,0.,0.));
#49016=DIRECTION('ref_axis',(0.,-1.,0.));
#49017=DIRECTION('center_axis',(0.,0.,1.));
#49018=DIRECTION('ref_axis',(1.,0.,0.));
#49019=DIRECTION('',(0.,-1.,0.));
#49020=DIRECTION('center_axis',(0.,1.,0.));
#49021=DIRECTION('ref_axis',(0.,0.,1.));
#49022=DIRECTION('center_axis',(0.,1.,0.));
#49023=DIRECTION('ref_axis',(1.,0.,0.));
#49024=DIRECTION('center_axis',(0.,0.,-1.));
#49025=DIRECTION('ref_axis',(1.,0.,0.));
#49026=DIRECTION('center_axis',(0.,-1.,0.));
#49027=DIRECTION('ref_axis',(1.,0.,0.));
#49028=DIRECTION('',(0.,-1.,0.));
#49029=DIRECTION('center_axis',(0.,0.,-1.));
#49030=DIRECTION('ref_axis',(0.,-1.,0.));
#49031=DIRECTION('',(0.,0.,-1.));
#49032=DIRECTION('center_axis',(-2.96059473233E-15,0.,-1.));
#49033=DIRECTION('ref_axis',(1.,0.,-2.96059473233E-15));
#49034=DIRECTION('center_axis',(-1.,0.,0.));
#49035=DIRECTION('ref_axis',(0.,0.,1.));
#49036=DIRECTION('',(0.,-1.,0.));
#49037=DIRECTION('center_axis',(-0.281178364446097,0.957593555167328,-0.0628753566146216));
#49038=DIRECTION('ref_axis',(0.959655525367003,0.280574208691291,-0.0184224333310672));
#49039=DIRECTION('center_axis',(-0.347084583568743,0.937833829550263,-7.75916811511616E-9));
#49040=DIRECTION('ref_axis',(-0.000199174768141593,-7.37046693238533E-5,
0.999999977448517));
#49041=DIRECTION('center_axis',(0.402792847081471,-0.209438030836135,0.891007089522572));
#49042=DIRECTION('ref_axis',(0.142300775827966,-0.947302276471775,-0.286999801724934));
#49043=DIRECTION('center_axis',(-0.975898622063701,0.,-0.218224378688931));
#49044=DIRECTION('ref_axis',(0.218224378688931,0.,-0.975898622063701));
#49045=DIRECTION('center_axis',(0.,1.,0.));
#49046=DIRECTION('ref_axis',(1.,0.,0.));
#49047=DIRECTION('center_axis',(0.,1.,0.));
#49048=DIRECTION('ref_axis',(1.,0.,0.));
#49049=DIRECTION('center_axis',(0.,-1.,0.));
#49050=DIRECTION('ref_axis',(0.,0.,-1.));
#49051=DIRECTION('',(0.,-1.,0.));
#49052=DIRECTION('center_axis',(0.,0.,1.));
#49053=DIRECTION('ref_axis',(1.,1.04089100950122E-14,0.));
#49054=DIRECTION('center_axis',(0.,0.,1.));
#49055=DIRECTION('ref_axis',(1.,0.,0.));
#49056=DIRECTION('center_axis',(-0.347083730899991,-0.937834145110104,3.18494860620805E-6));
#49057=DIRECTION('ref_axis',(0.000200278976134303,-7.07253260845549E-5,
0.99999997744313));
#49058=DIRECTION('center_axis',(0.,0.,1.));
#49059=DIRECTION('ref_axis',(1.,0.,0.));
#49060=DIRECTION('',(0.,-1.,0.));
#49061=DIRECTION('center_axis',(-0.281178364446097,-0.957593555167328,0.0628753566146216));
#49062=DIRECTION('ref_axis',(0.959655525367003,-0.280574208691291,0.0184224333310672));
#49063=DIRECTION('center_axis',(-0.359750052411863,-0.876095983477336,0.320991787316344));
#49064=DIRECTION('ref_axis',(-0.230372498903045,0.416775382555072,0.879333152022167));
#49065=DIRECTION('center_axis',(0.975898622063701,0.,-0.218224378688931));
#49066=DIRECTION('ref_axis',(0.218224378688931,0.,0.975898622063701));
#49067=DIRECTION('center_axis',(0.,1.,0.));
#49068=DIRECTION('ref_axis',(0.,0.,-1.));
#49069=DIRECTION('center_axis',(0.,1.,0.));
#49070=DIRECTION('ref_axis',(1.,0.,0.));
#49071=DIRECTION('center_axis',(0.,-1.,0.));
#49072=DIRECTION('ref_axis',(-1.,0.,0.));
#49073=DIRECTION('center_axis',(0.,-1.,0.));
#49074=DIRECTION('ref_axis',(0.,0.,-1.));
#49075=DIRECTION('center_axis',(0.,0.,-1.));
#49076=DIRECTION('ref_axis',(0.,-1.,0.));
#49077=DIRECTION('',(1.,0.,0.));
#49078=DIRECTION('',(0.,-1.,0.));
#49079=DIRECTION('center_axis',(1.,0.,0.));
#49080=DIRECTION('ref_axis',(0.,1.,0.));
#49081=DIRECTION('',(0.,0.,-1.));
#49082=DIRECTION('',(0.,-1.,0.));
#49083=DIRECTION('center_axis',(0.,1.,0.));
#49084=DIRECTION('ref_axis',(1.,0.,0.));
#49085=DIRECTION('',(1.,0.,0.));
#49086=DIRECTION('center_axis',(0.,0.,-1.));
#49087=DIRECTION('ref_axis',(0.,-1.,0.));
#49088=DIRECTION('',(0.,0.,1.));
#49089=DIRECTION('',(1.,0.,0.));
#49090=DIRECTION('',(0.,0.,1.));
#49091=DIRECTION('',(1.,0.,0.));
#49092=DIRECTION('',(0.,0.,1.));
#49093=DIRECTION('',(1.,0.,0.));
#49094=DIRECTION('',(0.,0.,1.));
#49095=DIRECTION('',(1.,0.,0.));
#49096=DIRECTION('',(0.,0.,1.));
#49097=DIRECTION('',(1.,0.,0.));
#49098=DIRECTION('',(0.,0.,1.));
#49099=DIRECTION('',(1.,0.,0.));
#49100=DIRECTION('',(0.,0.,1.));
#49101=DIRECTION('',(1.,0.,0.));
#49102=DIRECTION('',(0.,0.,1.));
#49103=DIRECTION('',(1.,0.,0.));
#49104=DIRECTION('',(0.,0.,1.));
#49105=DIRECTION('',(1.,0.,0.));
#49106=DIRECTION('',(0.,0.,1.));
#49107=DIRECTION('',(1.,0.,0.));
#49108=CARTESIAN_POINT('',(0.,0.,0.));
#49109=CARTESIAN_POINT('',(0.,0.,0.));
#49110=CARTESIAN_POINT('Origin',(-8.8,-9.17423561284002,0.473661560390005));
#49111=CARTESIAN_POINT('',(-8.39999999999935,-8.47423561284007,-0.738774004907511));
#49112=CARTESIAN_POINT('',(-8.4,-10.57423561284,0.47366156039));
#49113=CARTESIAN_POINT('Origin',(-8.4,-9.17423561284,0.47366156039));
#49114=CARTESIAN_POINT('',(-8.4999999999994,-8.52423561284007,-0.652171464529114));
#49115=CARTESIAN_POINT('',(-8.79999999999999,-8.67423561284028,-0.392363843393547));
#49116=CARTESIAN_POINT('Origin',(-8.5,-9.17423561284,0.47366156039));
#49117=CARTESIAN_POINT('Origin',(-8.4,-9.17423561284,0.47366156039));
#49118=CARTESIAN_POINT('Origin',(0.,-9.17423561284,0.47366156039));
#49119=CARTESIAN_POINT('',(8.4,-10.5742356128,0.47366156039));
#49120=CARTESIAN_POINT('',(8.39999999999934,-8.47423561284007,-0.73877400490752));
#49121=CARTESIAN_POINT('Origin',(8.4,-9.17423561284,0.47366156039));
#49122=CARTESIAN_POINT('',(0.,-10.57423561284,0.47366156039));
#49123=CARTESIAN_POINT('Origin',(8.4,-9.17423561284,0.47366156039));
#49124=CARTESIAN_POINT('Origin',(-8.5,0.,0.));
#49125=CARTESIAN_POINT('Origin',(8.8,-9.17423561284002,0.473661560390005));
#49126=CARTESIAN_POINT('',(8.4999999999994,-8.52423561284007,-0.652171464529115));
#49127=CARTESIAN_POINT('',(8.79999999999999,-8.67423561284028,-0.392363843393547));
#49128=CARTESIAN_POINT('Origin',(8.5,-9.17423561284,0.47366156039));
#49129=CARTESIAN_POINT('Origin',(8.5,0.,0.));
#49130=CARTESIAN_POINT('',(0.,0.,0.));
#49131=CARTESIAN_POINT('Origin',(-3.46627170195,-36.1242356128,2.26279399804));
#49132=CARTESIAN_POINT('',(-3.16691857253,-35.4710616262,2.28248419619));
#49133=CARTESIAN_POINT('',(-3.16691857253,-36.3742356128,2.28248419619));
#49134=CARTESIAN_POINT('',(-3.16691857253,-35.9226486195,2.28248419619));
#49135=CARTESIAN_POINT('',(-3.25430421882,-35.4710616254,2.47509045608));
#49136=CARTESIAN_POINT('Origin',(-3.46627170195,-35.4710616258,2.26279399804));
#49137=CARTESIAN_POINT('',(-3.25430421882,-36.3742356128,2.47509045608));
#49138=CARTESIAN_POINT('',(-3.25430421882,-36.1242356128,2.47509045608));
#49139=CARTESIAN_POINT('Origin',(-3.46627170195,-36.3742356128,2.26279399804));
#49140=CARTESIAN_POINT('Origin',(-1.57756236842E-15,-36.3742356128,4.77612251667E-16));
#49141=CARTESIAN_POINT('',(-14.1514385284,-36.3742356128,6.93238331308));
#49142=CARTESIAN_POINT('',(-14.1514385284,-36.3742356128,-6.93238331308));
#49143=CARTESIAN_POINT('',(-14.1514385284,-36.3742356128,-3.5527136788E-15));
#49144=CARTESIAN_POINT('',(-14.1086187499,-36.3742356128,-7.11244521731));
#49145=CARTESIAN_POINT('Origin',(-13.7514385284,-36.3742356128,-6.93238331308));
#49146=CARTESIAN_POINT('',(-13.1408443824,-36.3742356128,-8.77258279628));
#49147=CARTESIAN_POINT('Origin',(5.52786498918E-15,-36.3742356128,2.25396909107E-15));
#49148=CARTESIAN_POINT('',(-12.8348977878,-36.3742356128,-8.80475037519));
#49149=CARTESIAN_POINT('Origin',(-12.9745045801,-36.3742356128,-8.66153744443));
#49150=CARTESIAN_POINT('',(-11.686904291,-36.3742356128,-7.68566365004));
#49151=CARTESIAN_POINT('',(-0.45986885604,-36.3742356128,3.25867214427));
#49152=CARTESIAN_POINT('',(-11.1212648448,-36.3742356128,-7.69287592692));
#49153=CARTESIAN_POINT('Origin',(-11.4076907064,-36.3742356128,-7.97208951156));
#49154=CARTESIAN_POINT('',(-8.11331856237,-36.3742356128,-10.7785195086));
#49155=CARTESIAN_POINT('',(-8.43647932171,-36.3742356128,-10.447011287));
#49156=CARTESIAN_POINT('',(-8.12053083925,-36.3742356128,-11.3441589548));
#49157=CARTESIAN_POINT('Origin',(-8.39974442389,-36.3742356128,-11.0577330933));
#49158=CARTESIAN_POINT('',(-9.29417531907,-36.3742356128,-12.4882507647));
#49159=CARTESIAN_POINT('',(0.316839226711,-36.3742356128,-3.11924403781));
#49160=CARTESIAN_POINT('',(-9.27193478991,-36.3742356128,-12.7934055377));
#49161=CARTESIAN_POINT('Origin',(-9.15456852675,-36.3742356128,-12.6314636954));
#49162=CARTESIAN_POINT('',(9.27193478991,-36.3742356128,-12.7934055377));
#49163=CARTESIAN_POINT('Origin',(1.97515131038E-15,-36.3742356128,2.25396909107E-15));
#49164=CARTESIAN_POINT('',(9.29417531907,-36.3742356128,-12.4882507647));
#49165=CARTESIAN_POINT('Origin',(9.15456852675,-36.3742356128,-12.6314636954));
#49166=CARTESIAN_POINT('',(8.12053083925,-36.3742356128,-11.3441589548));
#49167=CARTESIAN_POINT('',(-0.316839226711,-36.3742356128,-3.11924403781));
#49168=CARTESIAN_POINT('',(8.11331856237,-36.3742356128,-10.7785195086));
#49169=CARTESIAN_POINT('Origin',(8.39974442389,-36.3742356128,-11.0577330933));
#49170=CARTESIAN_POINT('',(11.1212648448,-36.3742356128,-7.69287592692));
#49171=CARTESIAN_POINT('',(8.43647932171,-36.3742356128,-10.447011287));
#49172=CARTESIAN_POINT('',(11.686904291,-36.3742356128,-7.68566365004));
#49173=CARTESIAN_POINT('Origin',(11.4076907064,-36.3742356128,-7.97208951156));
#49174=CARTESIAN_POINT('',(12.8348977878,-36.3742356128,-8.80475037519));
#49175=CARTESIAN_POINT('',(0.45986885604,-36.3742356128,3.25867214427));
#49176=CARTESIAN_POINT('',(13.1408443824,-36.3742356128,-8.77258279628));
#49177=CARTESIAN_POINT('Origin',(12.9745045801,-36.3742356128,-8.66153744443));
#49178=CARTESIAN_POINT('',(14.1086187499,-36.3742356128,-7.11244521731));
#49179=CARTESIAN_POINT('Origin',(1.98794470979E-16,-36.3742356128,4.77612251667E-16));
#49180=CARTESIAN_POINT('',(14.1514385284,-36.3742356128,-6.93238331308));
#49181=CARTESIAN_POINT('Origin',(13.7514385284,-36.3742356128,-6.93238331308));
#49182=CARTESIAN_POINT('',(14.1514385284,-36.3742356128,6.93238331308));
#49183=CARTESIAN_POINT('',(14.1514385284,-36.3742356128,7.1054273576E-15));
#49184=CARTESIAN_POINT('',(14.1086187499,-36.3742356128,7.11244521731));
#49185=CARTESIAN_POINT('Origin',(13.7514385284,-36.3742356128,6.93238331308));
#49186=CARTESIAN_POINT('',(13.1408443824,-36.3742356128,8.77258279628));
#49187=CARTESIAN_POINT('Origin',(5.04684136861E-13,-36.3742356128,3.05122810209E-13));
#49188=CARTESIAN_POINT('',(12.8348977878,-36.3742356128,8.80475037519));
#49189=CARTESIAN_POINT('Origin',(12.9745045801,-36.3742356128,8.66153744443));
#49190=CARTESIAN_POINT('',(11.686904291,-36.3742356128,7.68566365004));
#49191=CARTESIAN_POINT('',(0.45986885604,-36.3742356128,-3.25867214427));
#49192=CARTESIAN_POINT('',(11.1212648448,-36.3742356128,7.69287592692));
#49193=CARTESIAN_POINT('Origin',(11.4076907064,-36.3742356128,7.97208951156));
#49194=CARTESIAN_POINT('',(8.11331856237,-36.3742356128,10.7785195086));
#49195=CARTESIAN_POINT('',(8.43647932171,-36.3742356128,10.447011287));
#49196=CARTESIAN_POINT('',(8.12053083925,-36.3742356128,11.3441589548));
#49197=CARTESIAN_POINT('Origin',(8.39974442389,-36.3742356128,11.0577330933));
#49198=CARTESIAN_POINT('',(9.29417531907,-36.3742356128,12.4882507647));
#49199=CARTESIAN_POINT('',(-0.316839226711,-36.3742356128,3.11924403781));
#49200=CARTESIAN_POINT('',(9.27193478991,-36.3742356128,12.7934055377));
#49201=CARTESIAN_POINT('Origin',(9.15456852675,-36.3742356128,12.6314636954));
#49202=CARTESIAN_POINT('',(-8.84971102033,-36.3742356128,13.0890265053));
#49203=CARTESIAN_POINT('Origin',(-5.13027604722E-15,-36.3742356128,-1.29874458773E-15));
#49204=CARTESIAN_POINT('',(-8.87729615416,-36.3742356128,12.7801296947));
#49205=CARTESIAN_POINT('Origin',(-8.73768936184,-36.3742356128,12.9233426255));
#49206=CARTESIAN_POINT('',(-7.77151385845,-36.3742356128,11.7021912817));
#49207=CARTESIAN_POINT('',(0.67498798988,-36.3742356128,3.46837452298));
#49208=CARTESIAN_POINT('',(-7.76430158156,-36.3742356128,11.1365518355));
#49209=CARTESIAN_POINT('Origin',(-8.05072744309,-36.3742356128,11.4157654202));
#49210=CARTESIAN_POINT('',(-11.4702818256,-36.3742356128,7.33484360001));
#49211=CARTESIAN_POINT('',(-8.43647932171,-36.3742356128,10.447011287));
#49212=CARTESIAN_POINT('',(-12.0359212718,-36.3742356128,7.32763132313));
#49213=CARTESIAN_POINT('Origin',(-11.7567076872,-36.3742356128,7.61405718465));
#49214=CARTESIAN_POINT('',(-13.1112015384,-36.3742356128,8.37583575597));
#49215=CARTESIAN_POINT('',(-0.818017619209,-36.3742356128,-3.60780262944));
#49216=CARTESIAN_POINT('',(-13.4206904888,-36.3742356128,8.33816927169));
#49217=CARTESIAN_POINT('Origin',(-13.2508083307,-36.3742356128,8.23262282521));
#49218=CARTESIAN_POINT('',(-14.1086187499,-36.3742356128,7.11244521731));
#49219=CARTESIAN_POINT('Origin',(5.79112209092E-12,-36.3742356128,-3.26979532908E-12));
#49220=CARTESIAN_POINT('Origin',(-13.7514385284,-36.3742356128,6.93238331308));
#49221=CARTESIAN_POINT('',(3.51985615629,-36.3742356128,-3.20601908088));
#49222=CARTESIAN_POINT('',(3.67755401867,-36.3742356128,-3.05915055738));
#49223=CARTESIAN_POINT('Origin',(3.78952269078,-36.3742356128,-3.33747234321));
#49224=CARTESIAN_POINT('',(7.07911993306,-36.3742356128,1.41233341424));
#49225=CARTESIAN_POINT('Ctrl Pts',(7.07911993306,-36.3742356128,1.41233341424));
#49226=CARTESIAN_POINT('Ctrl Pts',(7.02062825816,-36.3742356128,0.811131443794));
#49227=CARTESIAN_POINT('Ctrl Pts',(6.765884240706,-36.3742356128,-0.388148698646161));
#49228=CARTESIAN_POINT('Ctrl Pts',(6.23382280728197,-36.3742356128,-1.38868983255432));
#49229=CARTESIAN_POINT('Ctrl Pts',(5.42444395807881,-36.3742356128,-2.19049195793964));
#49230=CARTESIAN_POINT('Ctrl Pts',(4.33774769283,-36.3742356128,-2.79355507478));
#49231=CARTESIAN_POINT('Ctrl Pts',(3.67755401867,-36.3742356128,-3.05915055738));
#49232=CARTESIAN_POINT('',(7.21384189758,-36.3742356128,2.18958432614));
#49233=CARTESIAN_POINT('Ctrl Pts',(7.21384189758,-36.3742356128,2.18958432614));
#49234=CARTESIAN_POINT('Ctrl Pts',(7.13908599018,-36.3742356128,2.05065155888));
#49235=CARTESIAN_POINT('Ctrl Pts',(7.08904524264,-36.3742356128,1.89842024269));
#49236=CARTESIAN_POINT('Ctrl Pts',(7.10533215541,-36.3742356128,1.72680915639));
#49237=CARTESIAN_POINT('Ctrl Pts',(7.09439724612,-36.3742356128,1.56936004643));
#49238=CARTESIAN_POINT('Ctrl Pts',(7.07911993306,-36.3742356128,1.41233341424));
#49239=CARTESIAN_POINT('',(8.75956299023,-36.3742356128,2.0634404101));
#49240=CARTESIAN_POINT('Ctrl Pts',(8.75956299023,-36.3742356128,2.0634404101));
#49241=CARTESIAN_POINT('Ctrl Pts',(8.72637376563,-36.3742356128,2.11781888978));
#49242=CARTESIAN_POINT('Ctrl Pts',(8.6915484,-36.3742356128,2.17268982337));
#49243=CARTESIAN_POINT('Ctrl Pts',(8.65506636668,-36.3742356128,2.22762960985));
#49244=CARTESIAN_POINT('Ctrl Pts',(8.53055023262,-36.3742356128,2.40503324452));
#49245=CARTESIAN_POINT('Ctrl Pts',(8.26494430118178,-36.3742356128,2.70523539119787));
#49246=CARTESIAN_POINT('Ctrl Pts',(7.96786455664539,-36.3742356128,2.8806545502764));
#49247=CARTESIAN_POINT('Ctrl Pts',(7.60100727895793,-36.3742356128,2.68829057805622));
#49248=CARTESIAN_POINT('Ctrl Pts',(7.33749157791351,-36.3742356128,2.40256623079952));
#49249=CARTESIAN_POINT('Ctrl Pts',(7.2297761181,-36.3742356128,2.21919784335));
#49250=CARTESIAN_POINT('Ctrl Pts',(7.21384189758,-36.3742356128,2.18958432614));
#49251=CARTESIAN_POINT('',(9.23698117862,-36.3742356128,0.509886547139));
#49252=CARTESIAN_POINT('Ctrl Pts',(8.75956299023,-36.3742356128,2.0634404101));
#49253=CARTESIAN_POINT('Ctrl Pts',(8.92890465395,-36.3742356128,1.78598462948));
#49254=CARTESIAN_POINT('Ctrl Pts',(9.07291332076,-36.3742356128,1.49306717121));
#49255=CARTESIAN_POINT('Ctrl Pts',(9.12674872803,-36.3742356128,1.15064845916));
#49256=CARTESIAN_POINT('Ctrl Pts',(9.18664865847,-36.3742356128,0.831017278590001));
#49257=CARTESIAN_POINT('Ctrl Pts',(9.23698117862,-36.3742356128,0.509886547135));
#49258=CARTESIAN_POINT('',(1.87043161103,-36.3742356128,-8.24476960824));
#49259=CARTESIAN_POINT('Ctrl Pts',(1.87043161103,-36.3742356128,-8.24476960824));
#49260=CARTESIAN_POINT('Ctrl Pts',(2.47265813357,-36.3742356128,-8.13634296351));
#49261=CARTESIAN_POINT('Ctrl Pts',(3.05192283465,-36.3742356128,-7.98771609515));
#49262=CARTESIAN_POINT('Ctrl Pts',(4.33873711989964,-36.3742356128,-7.55106216307255));
#49263=CARTESIAN_POINT('Ctrl Pts',(5.96679547826005,-36.3742356128,-6.64390177065611));
#49264=CARTESIAN_POINT('Ctrl Pts',(7.82299194608668,-36.3742356128,-5.03608217876813));
#49265=CARTESIAN_POINT('Ctrl Pts',(9.32974836502124,-36.3742356128,-3.47204744400302));
#49266=CARTESIAN_POINT('Ctrl Pts',(9.44907784606298,-36.3742356128,-1.45170212295927));
#49267=CARTESIAN_POINT('Ctrl Pts',(9.34900416387435,-36.3742356128,-0.255886314382252));
#49268=CARTESIAN_POINT('Ctrl Pts',(9.25795835827,-36.3742356128,0.376048284641));
#49269=CARTESIAN_POINT('Ctrl Pts',(9.23698117862,-36.3742356128,0.509886547139));
#49270=CARTESIAN_POINT('',(1.51727342606,-36.3742356128,-7.9495168227));
#49271=CARTESIAN_POINT('Origin',(1.81727342606,-36.3742356128,-7.9495168227));
#49272=CARTESIAN_POINT('',(1.51727342606,-36.3742356128,-5.3088808072));
#49273=CARTESIAN_POINT('',(1.51727342606,-36.3742356128,-6.62919881495));
#49274=CARTESIAN_POINT('',(1.68475792039,-36.3742356128,-5.03973467448));
#49275=CARTESIAN_POINT('Origin',(1.81727342606,-36.3742356128,-5.3088808072));
#49276=CARTESIAN_POINT('Ctrl Pts',(3.51985615629,-36.3742356128,-3.20601908088));
#49277=CARTESIAN_POINT('Ctrl Pts',(3.41903503516,-36.3742356128,-3.4128460691));
#49278=CARTESIAN_POINT('Ctrl Pts',(3.30675917974,-36.3742356128,-3.60871163219));
#49279=CARTESIAN_POINT('Ctrl Pts',(3.01387620630693,-36.3742356128,-4.04639865742235));
#49280=CARTESIAN_POINT('Ctrl Pts',(2.65681036718069,-36.3742356128,-4.42266691385755));
#49281=CARTESIAN_POINT('Ctrl Pts',(2.23556166242,-36.3742356128,-4.73751640159));
#49282=CARTESIAN_POINT('Ctrl Pts',(1.97086406258,-36.3742356128,-4.89886881947));
#49283=CARTESIAN_POINT('Ctrl Pts',(1.68475792039,-36.3742356128,-5.03973467448));
#49284=CARTESIAN_POINT('',(3.0462613877,-36.3742356128,0.448114344193));
#49285=CARTESIAN_POINT('',(2.97642257165,-36.3742356128,0.274612461872));
#49286=CARTESIAN_POINT('Origin',(2.74690825827,-36.3742356128,0.467804542343));
#49287=CARTESIAN_POINT('',(-2.97642257165,-36.3742356128,0.274612461872));
#49288=CARTESIAN_POINT('Origin',(-1.14807003446E-14,-36.3742356128,2.77999550541));
#49289=CARTESIAN_POINT('',(-3.0462613877,-36.3742356128,0.448114344193));
#49290=CARTESIAN_POINT('Origin',(-2.74690825827,-36.3742356128,0.467804542343));
#49291=CARTESIAN_POINT('',(-3.10658998011,-36.3742356128,1.36529927019));
#49292=CARTESIAN_POINT('',(8.77076189454E-15,-36.3742356128,9.2896999221));
#49293=CARTESIAN_POINT('Origin',(-0.425321894002,-36.3742356128,5.30846337982));
#49294=CARTESIAN_POINT('',(3.25430421882,-36.3742356128,2.47509045608));
#49295=CARTESIAN_POINT('Origin',(0.425321894002,-36.3742356128,5.30846337982));
#49296=CARTESIAN_POINT('',(3.16691857253,-36.3742356128,2.28248419619));
#49297=CARTESIAN_POINT('Origin',(3.46627170195,-36.3742356128,2.26279399804));
#49298=CARTESIAN_POINT('',(3.10658998011,-36.3742356128,1.36529927019));
#49299=CARTESIAN_POINT('',(-1.51727342606,-36.3742356128,-5.3088808072));
#49300=CARTESIAN_POINT('',(-1.51727342606,-36.3742356128,-7.9495168227));
#49301=CARTESIAN_POINT('',(-1.51727342606,-36.3742356128,-6.62919881495));
#49302=CARTESIAN_POINT('',(-1.87043161103,-36.3742356128,-8.24476960824));
#49303=CARTESIAN_POINT('Origin',(-1.81727342606,-36.3742356128,-7.9495168227));
#49304=CARTESIAN_POINT('',(-9.23698117862,-36.3742356128,0.509886547139));
#49305=CARTESIAN_POINT('Ctrl Pts',(-1.87043161103,-36.3742356128,-8.24476960824));
#49306=CARTESIAN_POINT('Ctrl Pts',(-2.47265813357,-36.3742356128,-8.13634296351));
#49307=CARTESIAN_POINT('Ctrl Pts',(-3.05192283465,-36.3742356128,-7.98771609515));
#49308=CARTESIAN_POINT('Ctrl Pts',(-3.608285111,-36.3742356128,-7.79892601222));
#49309=CARTESIAN_POINT('Ctrl Pts',(-4.84313848674,-36.3742356128,-7.27000777732));
#49310=CARTESIAN_POINT('Ctrl Pts',(-5.97499470659,-36.3742356128,-6.53839758248));
#49311=CARTESIAN_POINT('Ctrl Pts',(-6.59156749188,-36.3742356128,-6.06232184959));
#49312=CARTESIAN_POINT('Ctrl Pts',(-7.62010012329,-36.3742356128,-5.1678005996));
#49313=CARTESIAN_POINT('Ctrl Pts',(-8.47746400168,-36.3742356128,-4.11735171219));
#49314=CARTESIAN_POINT('Ctrl Pts',(-8.78407978672,-36.3742356128,-3.65866522624));
#49315=CARTESIAN_POINT('Ctrl Pts',(-9.22504359392,-36.3742356128,-2.71647636201));
#49316=CARTESIAN_POINT('Ctrl Pts',(-9.38605456704,-36.3742356128,-1.68617604095));
#49317=CARTESIAN_POINT('Ctrl Pts',(-9.40005841918,-36.3742356128,-1.17735235373));
#49318=CARTESIAN_POINT('Ctrl Pts',(-9.36972184244,-36.3742356128,-0.530817230024));
#49319=CARTESIAN_POINT('Ctrl Pts',(-9.2950327654,-36.3742356128,0.106470788818));
#49320=CARTESIAN_POINT('Ctrl Pts',(-9.27733443288,-36.3742356128,0.241562002067001));
#49321=CARTESIAN_POINT('Ctrl Pts',(-9.25795835827,-36.3742356128,0.376048284641));
#49322=CARTESIAN_POINT('Ctrl Pts',(-9.23698117862397,-36.3742356128,0.509886547139624));
#49323=CARTESIAN_POINT('',(-8.75956299023,-36.3742356128,2.0634404101));
#49324=CARTESIAN_POINT('Ctrl Pts',(-8.75956299023,-36.3742356128,2.0634404101));
#49325=CARTESIAN_POINT('Ctrl Pts',(-8.92890465395,-36.3742356128,1.78598462948));
#49326=CARTESIAN_POINT('Ctrl Pts',(-9.07291332076,-36.3742356128,1.49306717121));
#49327=CARTESIAN_POINT('Ctrl Pts',(-9.12674872803,-36.3742356128,1.15064845916));
#49328=CARTESIAN_POINT('Ctrl Pts',(-9.18664865847,-36.3742356128,0.831017278590001));
#49329=CARTESIAN_POINT('Ctrl Pts',(-9.23698117862,-36.3742356128,0.509886547135));
#49330=CARTESIAN_POINT('',(-7.21384189759,-36.3742356128,2.18958432614));
#49331=CARTESIAN_POINT('Ctrl Pts',(-8.75956299024,-36.3742356128,2.0634404101));
#49332=CARTESIAN_POINT('Ctrl Pts',(-8.72637376563,-36.3742356128,2.11781888978));
#49333=CARTESIAN_POINT('Ctrl Pts',(-8.6915484,-36.3742356128,2.17268982337));
#49334=CARTESIAN_POINT('Ctrl Pts',(-8.65506636668,-36.3742356128,2.22762960985));
#49335=CARTESIAN_POINT('Ctrl Pts',(-8.53055023262,-36.3742356128,2.40503324452));
#49336=CARTESIAN_POINT('Ctrl Pts',(-8.3876008666,-36.3742356128,2.56660232663));
#49337=CARTESIAN_POINT('Ctrl Pts',(-8.27908544119,-36.3742356128,2.66027026629));
#49338=CARTESIAN_POINT('Ctrl Pts',(-8.01327762974,-36.3742356128,2.78696551824));
#49339=CARTESIAN_POINT('Ctrl Pts',(-7.71906576509,-36.3742356128,2.71717075777));
#49340=CARTESIAN_POINT('Ctrl Pts',(-7.55641153588,-36.3742356128,2.61428156978));
#49341=CARTESIAN_POINT('Ctrl Pts',(-7.38865661676,-36.3742356128,2.45617777771));
#49342=CARTESIAN_POINT('Ctrl Pts',(-7.26550535688,-36.3742356128,2.27753774962));
#49343=CARTESIAN_POINT('Ctrl Pts',(-7.24701042964,-36.3742356128,2.24853650952));
#49344=CARTESIAN_POINT('Ctrl Pts',(-7.2297761181,-36.3742356128,2.21919784335));
#49345=CARTESIAN_POINT('Ctrl Pts',(-7.21384189758642,-36.3742356128,2.18958432614193));
#49346=CARTESIAN_POINT('',(-7.07911993306,-36.3742356128,1.41233341424));
#49347=CARTESIAN_POINT('Ctrl Pts',(-7.21384189759,-36.3742356128,2.18958432614));
#49348=CARTESIAN_POINT('Ctrl Pts',(-7.13908599018,-36.3742356128,2.05065155888));
#49349=CARTESIAN_POINT('Ctrl Pts',(-7.08904524264,-36.3742356128,1.89842024269));
#49350=CARTESIAN_POINT('Ctrl Pts',(-7.10533215541,-36.3742356128,1.72680915639));
#49351=CARTESIAN_POINT('Ctrl Pts',(-7.09439724612,-36.3742356128,1.56936004643));
#49352=CARTESIAN_POINT('Ctrl Pts',(-7.07911993306,-36.3742356128,1.41233341424));
#49353=CARTESIAN_POINT('',(-3.67755401867,-36.3742356128,-3.05915055738));
#49354=CARTESIAN_POINT('Ctrl Pts',(-7.07911993306,-36.3742356128,1.41233341424));
#49355=CARTESIAN_POINT('Ctrl Pts',(-6.86965601460853,-36.3742356128,-0.740624604739125));
#49356=CARTESIAN_POINT('Ctrl Pts',(-5.73580070981187,-36.3742356128,-2.23111926194579));
#49357=CARTESIAN_POINT('Ctrl Pts',(-3.67755401867,-36.3742356128,-3.05915055738));
#49358=CARTESIAN_POINT('',(-3.51985615629,-36.3742356128,-3.20601908088));
#49359=CARTESIAN_POINT('Origin',(-3.78952269078,-36.3742356128,-3.33747234321));
#49360=CARTESIAN_POINT('',(-1.68475792039,-36.3742356128,-5.03973467448));
#49361=CARTESIAN_POINT('Ctrl Pts',(-3.51985615629,-36.3742356128,-3.20601908088));
#49362=CARTESIAN_POINT('Ctrl Pts',(-3.12209962985425,-36.3742356128,-4.0219868412465));
#49363=CARTESIAN_POINT('Ctrl Pts',(-2.51040021788758,-36.3742356128,-4.6332253724465));
#49364=CARTESIAN_POINT('Ctrl Pts',(-1.68475792039,-36.3742356128,-5.03973467448));
#49365=CARTESIAN_POINT('Origin',(-1.81727342606,-36.3742356128,-5.3088808072));
#49366=CARTESIAN_POINT('Ctrl Pts',(-9.23698117862,-35.3742356128,0.509886547138));
#49367=CARTESIAN_POINT('Ctrl Pts',(-9.85462053301,-32.4742356128,2.00920484002));
#49368=CARTESIAN_POINT('Ctrl Pts',(-9.29448486778,-35.3742356128,0.14300248283));
#49369=CARTESIAN_POINT('Ctrl Pts',(-9.89942675021,-32.4742356128,1.54440936128));
#49370=CARTESIAN_POINT('Ctrl Pts',(-9.33952412131,-35.3742356128,-0.225988266205));
#49371=CARTESIAN_POINT('Ctrl Pts',(-9.93347655148,-32.4742356128,1.07876884298));
#49372=CARTESIAN_POINT('Ctrl Pts',(-9.37147906182,-35.3742356128,-0.598052135313));
#49373=CARTESIAN_POINT('Ctrl Pts',(-9.95684539874,-32.4742356128,0.6105872463));
#49374=CARTESIAN_POINT('Ctrl Pts',(-9.39776085185,-35.3742356128,-1.34354990637));
#49375=CARTESIAN_POINT('Ctrl Pts',(-9.98182966629,-32.4742356128,-0.323612218818));
#49376=CARTESIAN_POINT('Ctrl Pts',(-9.31944120585,-35.3742356128,-2.08553948714));
#49377=CARTESIAN_POINT('Ctrl Pts',(-9.96363436978,-32.4742356128,-1.25779968708));
#49378=CARTESIAN_POINT('Ctrl Pts',(-9.24709061054,-35.3742356128,-2.45151005123));
#49379=CARTESIAN_POINT('Ctrl Pts',(-9.943864011,-32.4742356128,-1.72215443881));
#49380=CARTESIAN_POINT('Ctrl Pts',(-9.13406983882,-35.3742356128,-2.80846571914));
#49381=CARTESIAN_POINT('Ctrl Pts',(-9.91319925962,-32.4742356128,-2.18875096266));
#49382=CARTESIAN_POINT('Ctrl Pts',(-8.98669828191,-35.3742356128,-3.15062625521));
#49383=CARTESIAN_POINT('Ctrl Pts',(-9.87176476169,-32.4742356128,-2.65438916225));
#49384=CARTESIAN_POINT('',(-9.01911881647387,-35.2680071588898,-3.13244858247421));
#49385=CARTESIAN_POINT('',(-9.87176476169,-32.4742356128,-2.65438916225));
#49386=CARTESIAN_POINT('',(-9.01911869317,-35.2680072167,-3.13244885159));
#49387=CARTESIAN_POINT('',(-9.85462053301,-32.4742356128,2.00920484002));
#49388=CARTESIAN_POINT('Ctrl Pts',(-9.87176476169,-32.4742356128,-2.65438916225));
#49389=CARTESIAN_POINT('Ctrl Pts',(-9.91319925961983,-32.4742356128006,
-2.18875096266014));
#49390=CARTESIAN_POINT('Ctrl Pts',(-9.94386401099985,-32.4742356128006,
-1.72215443881016));
#49391=CARTESIAN_POINT('Ctrl Pts',(-9.96363436977986,-32.4742356128006,
-1.25779968708018));
#49392=CARTESIAN_POINT('Ctrl Pts',(-9.98182966628987,-32.4742356128006,
-0.323612218818225));
#49393=CARTESIAN_POINT('Ctrl Pts',(-9.95684539873987,-32.4742356128006,
0.610587246299733));
#49394=CARTESIAN_POINT('Ctrl Pts',(-9.93347655147987,-32.4742356128006,
1.07876884297971));
#49395=CARTESIAN_POINT('Ctrl Pts',(-9.89942675020987,-32.4742356128006,
1.54440936127969));
#49396=CARTESIAN_POINT('Ctrl Pts',(-9.85462053301,-32.4742356128,2.00920484002));
#49397=CARTESIAN_POINT('',(-9.26569106343796,-35.2394341085959,0.579579885999344));
#49398=CARTESIAN_POINT('',(-9.26569107792,-35.2394341184,0.579579770069));
#49399=CARTESIAN_POINT('',(-9.27386188271847,-35.2408046524422,0.522899877211487));
#49400=CARTESIAN_POINT('Ctrl Pts',(-9.27386188241726,-35.2408046523711,
0.522899878102206));
#49401=CARTESIAN_POINT('Ctrl Pts',(-9.272854956216,-35.2406369805721,0.529976427463772));
#49402=CARTESIAN_POINT('Ctrl Pts',(-9.27184238659432,-35.240469340988,0.537055008970363));
#49403=CARTESIAN_POINT('Ctrl Pts',(-9.27082740815912,-35.2403006245684,
0.544116409517216));
#49404=CARTESIAN_POINT('Ctrl Pts',(-9.26952133291424,-35.2400835201144,
0.553203026659481));
#49405=CARTESIAN_POINT('Ctrl Pts',(-9.26821080810748,-35.2398633916849,
0.562266670796889));
#49406=CARTESIAN_POINT('Ctrl Pts',(-9.26689225647901,-35.2396388881584,
0.571334399836343));
#49407=CARTESIAN_POINT('Ctrl Pts',(-9.26649252516074,-35.2395708278044,
0.574083367115571));
#49408=CARTESIAN_POINT('Ctrl Pts',(-9.26609219211384,-35.2395024442855,
0.576831669736027));
#49409=CARTESIAN_POINT('Ctrl Pts',(-9.26569107942698,-35.2394341188372,
0.579579770121116));
#49410=CARTESIAN_POINT('Ctrl Pts',(-9.01911901239593,-35.2680072483449,
-3.13244806238356));
#49411=CARTESIAN_POINT('Ctrl Pts',(-9.04725342339902,-35.2707959773529,
-3.06289434530028));
#49412=CARTESIAN_POINT('Ctrl Pts',(-9.0738646799152,-35.2732630041589,-2.99276671560158));
#49413=CARTESIAN_POINT('Ctrl Pts',(-9.09886532753374,-35.2754096171468,
-2.9220854676137));
#49414=CARTESIAN_POINT('Ctrl Pts',(-9.12517964497291,-35.2776690248407,
-2.84769024294082));
#49415=CARTESIAN_POINT('Ctrl Pts',(-9.14970966431518,-35.2795734922357,
-2.77268175024793));
#49416=CARTESIAN_POINT('Ctrl Pts',(-9.17240841720282,-35.2811368888824,
-2.69710071226188));
#49417=CARTESIAN_POINT('Ctrl Pts',(-9.19600438692266,-35.2827620821306,
-2.61853217184287));
#49418=CARTESIAN_POINT('Ctrl Pts',(-9.21762169379382,-35.2840187974798,
-2.5393450744354));
#49419=CARTESIAN_POINT('Ctrl Pts',(-9.23726341419725,-35.2849346746476,
-2.45960149213306));
#49420=CARTESIAN_POINT('Ctrl Pts',(-9.25786492376434,-35.2858953059899,
-2.37596125390682));
#49421=CARTESIAN_POINT('Ctrl Pts',(-9.27629335665372,-35.2864810937416,
-2.29170901187452));
#49422=CARTESIAN_POINT('Ctrl Pts',(-9.29260846387214,-35.2867353478736,
-2.2069313808944));
#49423=CARTESIAN_POINT('Ctrl Pts',(-9.31079942565656,-35.2870188352658,
-2.11240631129561));
#49424=CARTESIAN_POINT('Ctrl Pts',(-9.32636317658767,-35.2868902870952,
-2.01722832593922));
#49425=CARTESIAN_POINT('Ctrl Pts',(-9.33944913890977,-35.2864218830791,
-1.92153248339109));
#49426=CARTESIAN_POINT('Ctrl Pts',(-9.35381931851821,-35.2859075112908,
-1.81644533646613));
#49427=CARTESIAN_POINT('Ctrl Pts',(-9.36520238713606,-35.2849836925435,
-1.71073435590058));
#49428=CARTESIAN_POINT('Ctrl Pts',(-9.37386541799886,-35.2837558348772,
-1.60458838444502));
#49429=CARTESIAN_POINT('Ctrl Pts',(-9.38474687491737,-35.2822135478291,
-1.47126058800049));
#49430=CARTESIAN_POINT('Ctrl Pts',(-9.39133885899346,-35.2801929029209,
-1.3372488789615));
#49431=CARTESIAN_POINT('Ctrl Pts',(-9.39425596414206,-35.2779042511112,
-1.20291850223005));
#49432=CARTESIAN_POINT('Ctrl Pts',(-9.39511004211027,-35.2772341734184,
-1.16358888969212));
#49433=CARTESIAN_POINT('Ctrl Pts',(-9.39564939677077,-35.2765410404658,
-1.12423175686172));
#49434=CARTESIAN_POINT('Ctrl Pts',(-9.39588979120016,-35.2758298198528,
-1.08485559963608));
#49435=CARTESIAN_POINT('Ctrl Pts',(-9.396596184031,-35.2737399164243,-0.969149777163249));
#49436=CARTESIAN_POINT('Ctrl Pts',(-9.39472508784569,-35.2714936022906,
-0.853280252617673));
#49437=CARTESIAN_POINT('Ctrl Pts',(-9.39066660958969,-35.2691363044524,
-0.737398533363237));
#49438=CARTESIAN_POINT('Ctrl Pts',(-9.38695087508032,-35.2669780834706,
-0.631303175429051));
#49439=CARTESIAN_POINT('Ctrl Pts',(-9.38140163564093,-35.2647271155357,
-0.525197961588922));
#49440=CARTESIAN_POINT('Ctrl Pts',(-9.37427716929374,-35.2624161741734,
-0.41918685381147));
#49441=CARTESIAN_POINT('Ctrl Pts',(-9.36741419186441,-35.2601900511717,
-0.317066666210076));
#49442=CARTESIAN_POINT('Ctrl Pts',(-9.3590897311375,-35.2579084833464,-0.215034122490352));
#49443=CARTESIAN_POINT('Ctrl Pts',(-9.34949252196957,-35.2555953326665,
-0.113165335408674));
#49444=CARTESIAN_POINT('Ctrl Pts',(-9.34019666058181,-35.2533548138122,
-0.0144951795455671));
#49445=CARTESIAN_POINT('Ctrl Pts',(-9.32970691361629,-35.2510848261654,
0.0840210909909912));
#49446=CARTESIAN_POINT('Ctrl Pts',(-9.31815142540981,-35.2487992164153,
0.182334480492819));
#49447=CARTESIAN_POINT('Ctrl Pts',(-9.30702365779603,-35.2465982073623,
0.277008849255942));
#49448=CARTESIAN_POINT('Ctrl Pts',(-9.29490766568224,-35.2443828222107,
0.371494917639165));
#49449=CARTESIAN_POINT('Ctrl Pts',(-9.28187516958525,-35.2421561121088,
0.465770832179655));
#49450=CARTESIAN_POINT('Ctrl Pts',(-9.27924152669378,-35.2417061323668,
0.484822369990843));
#49451=CARTESIAN_POINT('Ctrl Pts',(-9.27657030962703,-35.2412556556506,
0.503865404015155));
#49452=CARTESIAN_POINT('Ctrl Pts',(-9.27386188313803,-35.2408046525553,
0.522899876806236));
#49453=CARTESIAN_POINT('Origin',(-3.46627170195,-35.4710616254,2.26279399804));
#49454=CARTESIAN_POINT('',(-3.24268782378383,-35.295907687595,2.35939289985189));
#49455=CARTESIAN_POINT('Origin',(-3.46628339291417,-35.4710655417899,2.26279140790743));
#49456=CARTESIAN_POINT('Origin',(-3.46628278031483,-35.4710655875802,2.26278688734025));
#49457=CARTESIAN_POINT('Origin',(12.7514385284,-32.4742356128,7.05028367309));
#49458=CARTESIAN_POINT('',(12.7514385284,-32.4742356128,6.7682619245));
#49459=CARTESIAN_POINT('',(12.7514385284,-32.4742356128,-6.7682619245));
#49460=CARTESIAN_POINT('',(12.7514385284,-32.4742356128,3.5527136788E-15));
#49461=CARTESIAN_POINT('',(12.7514385284,-32.8742356128,-6.7682619245));
#49462=CARTESIAN_POINT('',(12.7514385284,-33.6742356128,-6.7682619245));
#49463=CARTESIAN_POINT('',(12.7514385284,-32.8742356128,6.7682619245));
#49464=CARTESIAN_POINT('',(12.7514385284,-32.8742356128,5.3290705182E-15));
#49465=CARTESIAN_POINT('',(12.7514385284,-33.6742356128,6.7682619245));
#49466=CARTESIAN_POINT('Ctrl Pts',(3.51985615629,-36.3742356128,-3.20601908088));
#49467=CARTESIAN_POINT('Ctrl Pts',(3.51985615629,-35.2912304609806,-3.20601908088));
#49468=CARTESIAN_POINT('Ctrl Pts',(3.41903503516,-36.3742356128,-3.4128460691));
#49469=CARTESIAN_POINT('Ctrl Pts',(3.41903503516,-35.2912304609806,-3.4128460691));
#49470=CARTESIAN_POINT('Ctrl Pts',(3.30675917974,-36.3742356128,-3.60871163219));
#49471=CARTESIAN_POINT('Ctrl Pts',(3.30675917974,-35.2912304609806,-3.60871163219));
#49472=CARTESIAN_POINT('Ctrl Pts',(3.18302859005,-36.3742356128,-3.79361577017));
#49473=CARTESIAN_POINT('Ctrl Pts',(3.18302859005,-35.2912304609806,-3.79361577017));
#49474=CARTESIAN_POINT('Ctrl Pts',(2.86303108781,-36.3742356128,-4.20535597988));
#49475=CARTESIAN_POINT('Ctrl Pts',(2.86303108781,-35.2912304609806,-4.20535597988));
#49476=CARTESIAN_POINT('Ctrl Pts',(2.47885071991,-36.3742356128,-4.55567742084));
#49477=CARTESIAN_POINT('Ctrl Pts',(2.47885071991,-35.2912304609806,-4.55567742084));
#49478=CARTESIAN_POINT('Ctrl Pts',(2.23556166242,-36.3742356128,-4.73751640159));
#49479=CARTESIAN_POINT('Ctrl Pts',(2.23556166242,-35.2912304609806,-4.73751640159));
#49480=CARTESIAN_POINT('Ctrl Pts',(1.97086406258,-36.3742356128,-4.89886881947));
#49481=CARTESIAN_POINT('Ctrl Pts',(1.97086406258,-35.2912304609806,-4.89886881947));
#49482=CARTESIAN_POINT('Ctrl Pts',(1.68475792038,-36.3742356128,-5.03973467448));
#49483=CARTESIAN_POINT('Ctrl Pts',(1.68475792038,-35.2912304609806,-5.03973467448));
#49484=CARTESIAN_POINT('',(1.68475791952077,-35.4771141863372,-5.03973467240991));
#49485=CARTESIAN_POINT('',(1.68475792039,-36.1242356128,-5.03973467448));
#49486=CARTESIAN_POINT('',(3.51985615455486,-35.4822398766,-3.20601908003418));
#49487=CARTESIAN_POINT('Ctrl Pts',(3.51985615629,-35.4822398766,-3.20601908088));
#49488=CARTESIAN_POINT('Ctrl Pts',(3.48180288665517,-35.4888161519969,-3.28408251701604));
#49489=CARTESIAN_POINT('Ctrl Pts',(3.44134140954082,-35.4947135960524,-3.36118600277347));
#49490=CARTESIAN_POINT('Ctrl Pts',(3.39844886475906,-35.4999359868531,-3.4370172166045));
#49491=CARTESIAN_POINT('Ctrl Pts',(3.35616498680118,-35.5050842692967,-3.51177234730016));
#49492=CARTESIAN_POINT('Ctrl Pts',(3.31151851954779,-35.5095765212415,-3.58529103121342));
#49493=CARTESIAN_POINT('Ctrl Pts',(3.26452422693521,-35.5134163622067,-3.65730914068904));
#49494=CARTESIAN_POINT('Ctrl Pts',(3.21779936995671,-35.5172341879456,-3.72891434374746));
#49495=CARTESIAN_POINT('Ctrl Pts',(3.16875348688733,-35.5204070622853,-3.79903608623969));
#49496=CARTESIAN_POINT('Ctrl Pts',(3.11743821539015,-35.5229385428452,-3.86745028487632));
#49497=CARTESIAN_POINT('Ctrl Pts',(3.06637753705852,-35.525457463837,-3.93552505653747));
#49498=CARTESIAN_POINT('Ctrl Pts',(3.01306991419488,-35.5273413396226,-4.00190916785641));
#49499=CARTESIAN_POINT('Ctrl Pts',(2.95760356691231,-35.528593675132,-4.06641759311961));
#49500=CARTESIAN_POINT('Ctrl Pts',(2.93904343249216,-35.5290127313081,-4.08800338527602));
#49501=CARTESIAN_POINT('Ctrl Pts',(2.92024189659838,-35.5293610736877,-4.10937945444489));
#49502=CARTESIAN_POINT('Ctrl Pts',(2.90120320780892,-35.5296388335917,-4.13053977074822));
#49503=CARTESIAN_POINT('Ctrl Pts',(2.84438099451083,-35.5304678262125,-4.19369412028033));
#49504=CARTESIAN_POINT('Ctrl Pts',(2.78544352061609,-35.5306680961798,-4.25492395294756));
#49505=CARTESIAN_POINT('Ctrl Pts',(2.72452890068556,-35.5302431347145,-4.31409304263514));
#49506=CARTESIAN_POINT('Ctrl Pts',(2.66349205332807,-35.5298173205484,-4.373380857279));
#49507=CARTESIAN_POINT('Ctrl Pts',(2.60047012309514,-35.5287637633326,-4.43059965604713));
#49508=CARTESIAN_POINT('Ctrl Pts',(2.53563992629681,-35.5270859753459,-4.48564862898242));
#49509=CARTESIAN_POINT('Ctrl Pts',(2.47028724896019,-35.525394665704,-4.54114125346331));
#49510=CARTESIAN_POINT('Ctrl Pts',(2.40309703862138,-35.523069023126,-4.59442893453327));
#49511=CARTESIAN_POINT('Ctrl Pts',(2.33428890096677,-35.5201126454955,-4.64544522784908));
#49512=CARTESIAN_POINT('Ctrl Pts',(2.26501486437094,-35.5171362502732,-4.69680695177601));
#49513=CARTESIAN_POINT('Ctrl Pts',(2.19410095479911,-35.5135205496852,-4.74586646153125));
#49514=CARTESIAN_POINT('Ctrl Pts',(2.12180983582931,-35.5092692151946,-4.79259285979375));
#49515=CARTESIAN_POINT('Ctrl Pts',(2.04834448774971,-35.5049488260153,-4.84007823782884));
#49516=CARTESIAN_POINT('Ctrl Pts',(1.97345684281429,-35.4999719859482,-4.88515411046425));
#49517=CARTESIAN_POINT('Ctrl Pts',(1.89746194913474,-35.4943425482858,-4.92782573054381));
#49518=CARTESIAN_POINT('Ctrl Pts',(1.82740924757862,-35.4891532875684,-4.9671607716448));
#49519=CARTESIAN_POINT('Ctrl Pts',(1.75641620304805,-35.483409495094,-5.00445334434491));
#49520=CARTESIAN_POINT('Ctrl Pts',(1.68475792038805,-35.4771141891,-5.03973467447604));
#49521=CARTESIAN_POINT('',(3.51985615629,-36.1242356128,-3.20601908088));
#49522=CARTESIAN_POINT('Origin',(1.81727342606,-36.1242356128,-5.3088808072));
#49523=CARTESIAN_POINT('',(1.51727374257837,-35.5445459414522,-5.30854202326636));
#49524=CARTESIAN_POINT('',(1.51727342606,-35.9593880834,-5.3088808072));
#49525=CARTESIAN_POINT('',(1.67696448374633,-35.4768981244436,-5.04371406601353));
#49526=CARTESIAN_POINT('Ctrl Pts',(1.67696448325,-35.4768981249,-5.04371406613));
#49527=CARTESIAN_POINT('Ctrl Pts',(1.64455688984,-35.4917317677,-5.06086202998));
#49528=CARTESIAN_POINT('Ctrl Pts',(1.61513825447,-35.505058041,-5.08277314744));
#49529=CARTESIAN_POINT('Ctrl Pts',(1.58873141496,-35.5179848719,-5.10914094848));
#49530=CARTESIAN_POINT('Ctrl Pts',(1.54998925981,-35.5347051565,-5.16293840519));
#49531=CARTESIAN_POINT('Ctrl Pts',(1.52721834654,-35.5426195859,-5.22486268019));
#49532=CARTESIAN_POINT('Ctrl Pts',(1.52071813077,-35.5443146003,-5.25227472437));
#49533=CARTESIAN_POINT('Ctrl Pts',(1.51732687674,-35.5452006575,-5.27999548691));
#49534=CARTESIAN_POINT('Ctrl Pts',(1.51727394979,-35.5445470238,-5.30832023528));
#49535=CARTESIAN_POINT('Origin',(1.6862492552706,-35.5734099629681,-5.04271729832598));
#49536=CARTESIAN_POINT('Origin',(1.51727342606,-32.4742356128,-5.11808633804));
#49537=CARTESIAN_POINT('',(1.51727342288,-35.544540501139,-7.94951682269995));
#49538=CARTESIAN_POINT('',(1.51727342606,-36.1242356128,-7.9495168227));
#49539=CARTESIAN_POINT('',(1.51727342606,-35.544540554,-5.3083202352798));
#49540=CARTESIAN_POINT('Origin',(1.81727342606,-36.1242356128,-7.9495168227));
#49541=CARTESIAN_POINT('',(1.8704316154347,-35.4944687624331,-8.24476961257036));
#49542=CARTESIAN_POINT('',(1.87043161103,-36.1242356128,-8.24476960824));
#49543=CARTESIAN_POINT('',(1.85568221013649,-35.4970690565643,-8.24704793966574));
#49544=CARTESIAN_POINT('Origin',(1.86844266437558,-35.7037699017498,-8.22958286354931));
#49545=CARTESIAN_POINT('',(1.51739959473689,-35.5460990323408,-7.95821664298045));
#49546=CARTESIAN_POINT('Ctrl Pts',(1.51739959739202,-35.5460990330595,-7.95821664354419));
#49547=CARTESIAN_POINT('Ctrl Pts',(1.51784040157713,-35.551544433581,-7.9734107080064));
#49548=CARTESIAN_POINT('Ctrl Pts',(1.51944015474546,-35.5564624662645,-7.98865298821528));
#49549=CARTESIAN_POINT('Ctrl Pts',(1.52221396870495,-35.5607753418337,-8.00374326615405));
#49550=CARTESIAN_POINT('Ctrl Pts',(1.52508034792987,-35.5652321428706,-8.01933712349758));
#49551=CARTESIAN_POINT('Ctrl Pts',(1.52920035542674,-35.5690427768125,-8.03476806671595));
#49552=CARTESIAN_POINT('Ctrl Pts',(1.53454083399218,-35.5721488750417,-8.04981508926192));
#49553=CARTESIAN_POINT('Ctrl Pts',(1.53985832132163,-35.5752416012412,-8.06479733303534));
#49554=CARTESIAN_POINT('Ctrl Pts',(1.54638538066407,-35.577636071276,-8.07939834280623));
#49555=CARTESIAN_POINT('Ctrl Pts',(1.55404503872652,-35.579299076886,-8.09340906153831));
#49556=CARTESIAN_POINT('Ctrl Pts',(1.56199623962116,-35.5810253800168,-8.10795305794244));
#49557=CARTESIAN_POINT('Ctrl Pts',(1.57116678649342,-35.581963465072,-8.12185869749068));
#49558=CARTESIAN_POINT('Ctrl Pts',(1.58142798632441,-35.5821006264457,-8.13491533384685));
#49559=CARTESIAN_POINT('Ctrl Pts',(1.59149584448517,-35.5822352034228,-8.14772595687882));
#49560=CARTESIAN_POINT('Ctrl Pts',(1.602613595017,-35.5815989923742,-8.15971912255805));
#49561=CARTESIAN_POINT('Ctrl Pts',(1.61462398371853,-35.5801988565566,-8.17072375022459));
#49562=CARTESIAN_POINT('Ctrl Pts',(1.62401123170297,-35.5791045187746,-8.17932490139875));
#49563=CARTESIAN_POINT('Ctrl Pts',(1.63394272185038,-35.5775439293429,-8.18732229002714));
#49564=CARTESIAN_POINT('Ctrl Pts',(1.64432960286547,-35.5755276116623,-8.19465032514282));
#49565=CARTESIAN_POINT('Ctrl Pts',(1.65751223624117,-35.5729685781358,-8.20395078792408));
#49566=CARTESIAN_POINT('Ctrl Pts',(1.67143040403805,-35.5696742607946,-8.21217315079081));
#49567=CARTESIAN_POINT('Ctrl Pts',(1.68587374540741,-35.565686430912,-8.2192114954254));
#49568=CARTESIAN_POINT('Ctrl Pts',(1.70041483395494,-35.5616716128756,-8.22629747296635));
#49569=CARTESIAN_POINT('Ctrl Pts',(1.7154879825108,-35.5569536553932,-8.23218342574401));
#49570=CARTESIAN_POINT('Ctrl Pts',(1.7308718665687,-35.5515942287824,-8.23681029394356));
#49571=CARTESIAN_POINT('Ctrl Pts',(1.74453974665183,-35.5468326224185,-8.24092105553498));
#49572=CARTESIAN_POINT('Ctrl Pts',(1.75845269437942,-35.5415648512774,-8.24403870478297));
#49573=CARTESIAN_POINT('Ctrl Pts',(1.77245352352828,-35.5358486074623,-8.24615310101329));
#49574=CARTESIAN_POINT('Ctrl Pts',(1.78937968978829,-35.5289380100849,-8.24870927977624));
#49575=CARTESIAN_POINT('Ctrl Pts',(1.8064255637685,-35.521374841914,-8.24979779098238));
#49576=CARTESIAN_POINT('Ctrl Pts',(1.82333732775558,-35.5132798883306,-8.24945548954978));
#49577=CARTESIAN_POINT('Ctrl Pts',(1.83055847689705,-35.5098234264757,-8.24930933036154));
#49578=CARTESIAN_POINT('Ctrl Pts',(1.83775521093275,-35.5062703565462,-8.2489028379445));
#49579=CARTESIAN_POINT('Ctrl Pts',(1.84490789334748,-35.5026317912376,-8.24824123808703));
#49580=CARTESIAN_POINT('Ctrl Pts',(1.84751151403415,-35.5013073309362,-8.24800041164245));
#49581=CARTESIAN_POINT('Ctrl Pts',(1.85010944922896,-35.499971478242,-8.24772578323896));
#49582=CARTESIAN_POINT('Ctrl Pts',(1.85270080612586,-35.4986247745774,-8.24741763123874));
#49583=CARTESIAN_POINT('Ctrl Pts',(1.8536955086597,-35.4981078370806,-8.24729934588183));
#49584=CARTESIAN_POINT('Ctrl Pts',(1.85468986954109,-35.4975889712202,-8.24717603800027));
#49585=CARTESIAN_POINT('Ctrl Pts',(1.85568130399,-35.4970695389,-8.24704805785));
#49586=CARTESIAN_POINT('Origin',(1.88128360390313,-40.0416488169456,-7.95002524253046));
#49587=CARTESIAN_POINT('Ctrl Pts',(1.87043161103,-36.3742356128,-8.24476960824));
#49588=CARTESIAN_POINT('Ctrl Pts',(1.87043161103,-35.2215351205278,-8.24476960824));
#49589=CARTESIAN_POINT('Ctrl Pts',(2.47265813357,-36.3742356128,-8.13634296351));
#49590=CARTESIAN_POINT('Ctrl Pts',(2.47265813357,-35.2215351205278,-8.13634296351));
#49591=CARTESIAN_POINT('Ctrl Pts',(3.05192283465,-36.3742356128,-7.98771609515));
#49592=CARTESIAN_POINT('Ctrl Pts',(3.05192283465,-35.2215351205278,-7.98771609515));
#49593=CARTESIAN_POINT('Ctrl Pts',(3.608285111,-36.3742356128,-7.79892601222));
#49594=CARTESIAN_POINT('Ctrl Pts',(3.608285111,-35.2215351205278,-7.79892601222));
#49595=CARTESIAN_POINT('Ctrl Pts',(4.84313848674,-36.3742356128,-7.27000777732));
#49596=CARTESIAN_POINT('Ctrl Pts',(4.84313848674,-35.2215351205278,-7.27000777732));
#49597=CARTESIAN_POINT('Ctrl Pts',(5.97499470659,-36.3742356128,-6.53839758248));
#49598=CARTESIAN_POINT('Ctrl Pts',(5.97499470659,-35.2215351205278,-6.53839758248));
#49599=CARTESIAN_POINT('Ctrl Pts',(6.59156749188,-36.3742356128,-6.06232184959));
#49600=CARTESIAN_POINT('Ctrl Pts',(6.59156749188,-35.2215351205278,-6.06232184959));
#49601=CARTESIAN_POINT('Ctrl Pts',(7.62010012329,-36.3742356128,-5.1678005996));
#49602=CARTESIAN_POINT('Ctrl Pts',(7.62010012329,-35.2215351205278,-5.1678005996));
#49603=CARTESIAN_POINT('Ctrl Pts',(8.47746400168,-36.3742356128,-4.11735171219));
#49604=CARTESIAN_POINT('Ctrl Pts',(8.47746400168,-35.2215351205278,-4.11735171219));
#49605=CARTESIAN_POINT('Ctrl Pts',(8.78407978672,-36.3742356128,-3.65866522624));
#49606=CARTESIAN_POINT('Ctrl Pts',(8.78407978672,-35.2215351205278,-3.65866522624));
#49607=CARTESIAN_POINT('Ctrl Pts',(9.22504359392,-36.3742356128,-2.71647636201));
#49608=CARTESIAN_POINT('Ctrl Pts',(9.22504359392,-35.2215351205278,-2.71647636201));
#49609=CARTESIAN_POINT('Ctrl Pts',(9.38605456704,-36.3742356128,-1.68617604095));
#49610=CARTESIAN_POINT('Ctrl Pts',(9.38605456704,-35.2215351205278,-1.68617604095));
#49611=CARTESIAN_POINT('Ctrl Pts',(9.40005841918,-36.3742356128,-1.17735235373));
#49612=CARTESIAN_POINT('Ctrl Pts',(9.40005841918,-35.2215351205278,-1.17735235373));
#49613=CARTESIAN_POINT('Ctrl Pts',(9.36972184244,-36.3742356128,-0.530817230024));
#49614=CARTESIAN_POINT('Ctrl Pts',(9.36972184244,-35.2215351205278,-0.530817230024));
#49615=CARTESIAN_POINT('Ctrl Pts',(9.2950327654,-36.3742356128,0.106470788818));
#49616=CARTESIAN_POINT('Ctrl Pts',(9.2950327654,-35.2215351205278,0.106470788818));
#49617=CARTESIAN_POINT('Ctrl Pts',(9.27733443288,-36.3742356128,0.241562002067001));
#49618=CARTESIAN_POINT('Ctrl Pts',(9.27733443288,-35.2215351205278,0.241562002067001));
#49619=CARTESIAN_POINT('Ctrl Pts',(9.25795835827,-36.3742356128,0.376048284641));
#49620=CARTESIAN_POINT('Ctrl Pts',(9.25795835827,-35.2215351205278,0.376048284641));
#49621=CARTESIAN_POINT('Ctrl Pts',(9.23698117862,-36.3742356128,0.509886547165));
#49622=CARTESIAN_POINT('Ctrl Pts',(9.23698117862,-35.2215351205278,0.509886547165));
#49623=CARTESIAN_POINT('',(9.23698117854899,-35.5153448503988,0.509886547089956));
#49624=CARTESIAN_POINT('',(9.23698117862,-36.1242356128,0.509886547139));
#49625=CARTESIAN_POINT('',(9.00070981177086,-35.4796534480026,-3.11774626039934));
#49626=CARTESIAN_POINT('Ctrl Pts',(9.00070981177086,-35.4796534480026,-3.11774626039934));
#49627=CARTESIAN_POINT('Ctrl Pts',(9.02957171740057,-35.4769219470675,-3.04928528637033));
#49628=CARTESIAN_POINT('Ctrl Pts',(9.05680199238443,-35.4745170641086,-2.98008474679654));
#49629=CARTESIAN_POINT('Ctrl Pts',(9.08232187979775,-35.4724444037653,-2.910198820275));
#49630=CARTESIAN_POINT('Ctrl Pts',(9.10927225564361,-35.4702555627901,-2.83639551716526));
#49631=CARTESIAN_POINT('Ctrl Pts',(9.13431510786021,-35.4684371095379,-2.76182792423961));
#49632=CARTESIAN_POINT('Ctrl Pts',(9.15741235945346,-35.4669762581242,-2.68657232100095));
#49633=CARTESIAN_POINT('Ctrl Pts',(9.18148566903293,-35.4654536731453,-2.60813651979576));
#49634=CARTESIAN_POINT('Ctrl Pts',(9.20344567588574,-35.4643193005489,-2.52895350431998));
#49635=CARTESIAN_POINT('Ctrl Pts',(9.22330541366417,-35.4635411664201,-2.44912073619115));
#49636=CARTESIAN_POINT('Ctrl Pts',(9.24419465191341,-35.4627226949283,-2.36514955126694));
#49637=CARTESIAN_POINT('Ctrl Pts',(9.26276050520176,-35.4622980003227,-2.28045974660158));
#49638=CARTESIAN_POINT('Ctrl Pts',(9.27907531337767,-35.4622156178015,-2.19517351658305));
#49639=CARTESIAN_POINT('Ctrl Pts',(9.29723571129714,-35.4621239158735,-2.10023940166805));
#49640=CARTESIAN_POINT('Ctrl Pts',(9.31260699943646,-35.4624557836193,-2.00456669258708));
#49641=CARTESIAN_POINT('Ctrl Pts',(9.32535642051477,-35.4631302190584,-1.90832945811796));
#49642=CARTESIAN_POINT('Ctrl Pts',(9.33904599640173,-35.463854388028,-1.80499559563723));
#49643=CARTESIAN_POINT('Ctrl Pts',(9.34971379577462,-35.4649723642263,-1.70101166885288));
#49644=CARTESIAN_POINT('Ctrl Pts',(9.35763181221748,-35.4663868382239,-1.59658955684038));
#49645=CARTESIAN_POINT('Ctrl Pts',(9.36576400690357,-35.4678395730105,-1.48934288078885));
#49646=CARTESIAN_POINT('Ctrl Pts',(9.37099761991728,-35.4696036037748,-1.38163498160731));
#49647=CARTESIAN_POINT('Ctrl Pts',(9.37366922576191,-35.471596964129,-1.27367781011332));
#49648=CARTESIAN_POINT('Ctrl Pts',(9.37519483192013,-35.4727352618453,-1.21202944758001));
#49649=CARTESIAN_POINT('Ctrl Pts',(9.37588558818129,-35.4739488889969,-1.15029939791678));
#49650=CARTESIAN_POINT('Ctrl Pts',(9.37580612763427,-35.4752287322034,-1.08852272605951));
#49651=CARTESIAN_POINT('Ctrl Pts',(9.3756771929251,-35.4773054384155,-0.988282323516714));
#49652=CARTESIAN_POINT('Ctrl Pts',(9.37352221687252,-35.4795545444975,-0.887915672555842));
#49653=CARTESIAN_POINT('Ctrl Pts',(9.36960764020662,-35.4818966426587,-0.787510754476126));
#49654=CARTESIAN_POINT('Ctrl Pts',(9.3656030093745,-35.4842926203873,-0.684796038440355));
#49655=CARTESIAN_POINT('Ctrl Pts',(9.35975775607616,-35.486786172115,-0.582042878943941));
#49656=CARTESIAN_POINT('Ctrl Pts',(9.3523252340311,-35.4893296612911,-0.479365968570074));
#49657=CARTESIAN_POINT('Ctrl Pts',(9.34529365064581,-35.4917359449351,-0.382227843360345));
#49658=CARTESIAN_POINT('Ctrl Pts',(9.33684172327988,-35.4941875092004,-0.28515935974196));
#49659=CARTESIAN_POINT('Ctrl Pts',(9.32714804515724,-35.4966702396909,-0.18825370987044));
#49660=CARTESIAN_POINT('Ctrl Pts',(9.31792029758086,-35.4990336367396,-0.0960058691202795));
#49661=CARTESIAN_POINT('Ctrl Pts',(9.30756748520679,-35.5014256840601,-0.00390652794974493));
#49662=CARTESIAN_POINT('Ctrl Pts',(9.29620682473956,-35.5038517559769,0.0879838265690647));
#49663=CARTESIAN_POINT('Ctrl Pts',(9.28558220327457,-35.5061206465787,0.173920752143267));
#49664=CARTESIAN_POINT('Ctrl Pts',(9.27407606940699,-35.5084196106949,0.259674395231827));
#49665=CARTESIAN_POINT('Ctrl Pts',(9.26175043835322,-35.5107637359109,0.345222825128153));
#49666=CARTESIAN_POINT('Ctrl Pts',(9.25383028777107,-35.5122700137326,0.400194164436453));
#49667=CARTESIAN_POINT('Ctrl Pts',(9.24557108699713,-35.5137951391701,0.455081343764294));
#49668=CARTESIAN_POINT('Ctrl Pts',(9.23698117833998,-35.5153448508951,0.509886546917127));
#49669=CARTESIAN_POINT('',(8.91162791630276,-35.4775418018592,-3.31601642789431));
#49670=CARTESIAN_POINT('Origin',(8.92974789374037,-35.4242646256046,-3.20847971418429));
#49671=CARTESIAN_POINT('',(2.02993009745,-35.4952697797,-8.21479904026));
#49672=CARTESIAN_POINT('Ctrl Pts',(2.02993009745,-35.4952697797,-8.21479904026));
#49673=CARTESIAN_POINT('Ctrl Pts',(2.1975178934536,-35.4899768112507,-8.1819801957285));
#49674=CARTESIAN_POINT('Ctrl Pts',(2.36364233174554,-35.4848180347522,-8.14522817489977));
#49675=CARTESIAN_POINT('Ctrl Pts',(2.52813765848659,-35.4798773000524,-8.10448244801098));
#49676=CARTESIAN_POINT('Ctrl Pts',(2.68928215337265,-35.4750372099821,-8.06456672694862));
#49677=CARTESIAN_POINT('Ctrl Pts',(2.84886323116559,-35.4704064674222,-8.02081818934416));
#49678=CARTESIAN_POINT('Ctrl Pts',(3.00675547641862,-35.4660483132631,-7.97321492935763));
#49679=CARTESIAN_POINT('Ctrl Pts',(3.16170539309467,-35.4617713734886,-7.92649875810679));
#49680=CARTESIAN_POINT('Ctrl Pts',(3.3150288310632,-35.4577570434877,-7.8760700511927));
#49681=CARTESIAN_POINT('Ctrl Pts',(3.46663688737487,-35.4540485714109,-7.82194436965912));
#49682=CARTESIAN_POINT('Ctrl Pts',(3.61564458295988,-35.4504037065419,-7.76874704444108));
#49683=CARTESIAN_POINT('Ctrl Pts',(3.76299523221431,-35.4470543738175,-7.71197835196257));
#49684=CARTESIAN_POINT('Ctrl Pts',(3.90863338135848,-35.4440243272187,-7.65169038609799));
#49685=CARTESIAN_POINT('Ctrl Pts',(4.05084484294492,-35.4410655739112,-7.5928209223479));
#49686=CARTESIAN_POINT('Ctrl Pts',(4.19142347414132,-35.438411301993,-7.53059578517629));
#49687=CARTESIAN_POINT('Ctrl Pts',(4.33034523746524,-35.4360661416366,-7.46510065395307));
#49688=CARTESIAN_POINT('Ctrl Pts',(4.46756230134255,-35.4337497585825,-7.40040920900103));
#49689=CARTESIAN_POINT('Ctrl Pts',(4.60316289372039,-35.4317350148565,-7.33252741469367));
#49690=CARTESIAN_POINT('Ctrl Pts',(4.73715106390426,-35.4300082452412,-7.26157592932336));
#49691=CARTESIAN_POINT('Ctrl Pts',(4.86874877422086,-35.4283122826252,-7.19189027718346));
#49692=CARTESIAN_POINT('Ctrl Pts',(4.99879109554046,-35.4268941515193,-7.11924342586109));
#49693=CARTESIAN_POINT('Ctrl Pts',(5.12730826788093,-35.4257225409936,-7.04378791082896));
#49694=CARTESIAN_POINT('Ctrl Pts',(5.21963571122407,-35.4248808495491,-6.98958025388953));
#49695=CARTESIAN_POINT('Ctrl Pts',(5.311176557266,-35.4241660139734,-6.93392380881406));
#49696=CARTESIAN_POINT('Ctrl Pts',(5.40195064262958,-35.423560213071,-6.87688796232893));
#49697=CARTESIAN_POINT('Ctrl Pts',(5.57266510194519,-35.4224209124316,-6.76962338725426));
#49698=CARTESIAN_POINT('Ctrl Pts',(5.74066892757427,-35.4216668875503,-6.65748707456149));
#49699=CARTESIAN_POINT('Ctrl Pts',(5.90607489885303,-35.4211448538569,-6.54086756734377));
#49700=CARTESIAN_POINT('Ctrl Pts',(6.02322228246083,-35.4207751278979,-6.45827278528984));
#49701=CARTESIAN_POINT('Ctrl Pts',(6.13906856601719,-35.4205205600216,-6.3734289106523));
#49702=CARTESIAN_POINT('Ctrl Pts',(6.25362891329586,-35.4203360786063,-6.28645115877483));
#49703=CARTESIAN_POINT('Ctrl Pts',(6.35123185698643,-35.4201789044216,-6.21234799113884));
#49704=CARTESIAN_POINT('Ctrl Pts',(6.44790169045711,-35.4200724071828,-6.13669582147483));
#49705=CARTESIAN_POINT('Ctrl Pts',(6.54361636231053,-35.4200029704147,-6.05954834485368));
#49706=CARTESIAN_POINT('Ctrl Pts',(6.63435282649732,-35.4199371451165,-5.98641337908524));
#49707=CARTESIAN_POINT('Ctrl Pts',(6.72423135978761,-35.4199043868614,-5.91193471524081));
#49708=CARTESIAN_POINT('Ctrl Pts',(6.81319693299893,-35.4199101028679,-5.83614049502093));
#49709=CARTESIAN_POINT('Ctrl Pts',(6.90000716025135,-35.4199156803943,-5.76218252179369));
#49710=CARTESIAN_POINT('Ctrl Pts',(6.98594861911178,-35.4199576407568,-5.68697211269862));
#49711=CARTESIAN_POINT('Ctrl Pts',(7.07092770952919,-35.4200612492516,-5.61051622553605));
#49712=CARTESIAN_POINT('Ctrl Pts',(7.15069751739736,-35.4201585064673,-5.53874714211339));
#49713=CARTESIAN_POINT('Ctrl Pts',(7.22961939495362,-35.4203100434311,-5.46588058088319));
#49714=CARTESIAN_POINT('Ctrl Pts',(7.30757463585883,-35.4205566121551,-5.39190447875861));
#49715=CARTESIAN_POINT('Ctrl Pts',(7.31266542004049,-35.4205727140637,-5.38707354800728));
#49716=CARTESIAN_POINT('Ctrl Pts',(7.31775206621492,-35.4205892288169,-5.38223787887034));
#49717=CARTESIAN_POINT('Ctrl Pts',(7.32283453462144,-35.4206061710013,-5.37739746516443));
#49718=CARTESIAN_POINT('Ctrl Pts',(7.38569118267643,-35.4208157008674,-5.31753439147313));
#49719=CARTESIAN_POINT('Ctrl Pts',(7.44791297110117,-35.4210888089051,-5.25694587282929));
#49720=CARTESIAN_POINT('Ctrl Pts',(7.50945481532502,-35.4214338225053,-5.19559372525316));
#49721=CARTESIAN_POINT('Ctrl Pts',(7.57397402407752,-35.4217955276959,-5.13127339058004));
#49722=CARTESIAN_POINT('Ctrl Pts',(7.63774567323264,-35.4222365134176,-5.06611357288604));
#49723=CARTESIAN_POINT('Ctrl Pts',(7.70066498678859,-35.4227880797105,-5.00006853898814));
#49724=CARTESIAN_POINT('Ctrl Pts',(7.76988847984058,-35.4233949100029,-4.92740614509402));
#49725=CARTESIAN_POINT('Ctrl Pts',(7.8380802462688,-35.4241358884641,-4.8536719426947));
#49726=CARTESIAN_POINT('Ctrl Pts',(7.90503975752188,-35.4250742536816,-4.77880693738246));
#49727=CARTESIAN_POINT('Ctrl Pts',(7.97788603307253,-35.4260951155417,-4.69736015403509));
#49728=CARTESIAN_POINT('Ctrl Pts',(8.04927322937182,-35.4273503513893,-4.61457442442277));
#49729=CARTESIAN_POINT('Ctrl Pts',(8.11887950897483,-35.4289372554664,-4.53038316516456));
#49730=CARTESIAN_POINT('Ctrl Pts',(8.19656257649718,-35.4307082964886,-4.43642274499775));
#49731=CARTESIAN_POINT('Ctrl Pts',(8.27202600384564,-35.4328940611376,-4.34071049739949));
#49732=CARTESIAN_POINT('Ctrl Pts',(8.34476245153336,-35.4356296730107,-4.24317952523622));
#49733=CARTESIAN_POINT('Ctrl Pts',(8.4121335395811,-35.4381634941448,-4.15284286566765));
#49734=CARTESIAN_POINT('Ctrl Pts',(8.47716266034837,-35.4411702157103,-4.06094562941393));
#49735=CARTESIAN_POINT('Ctrl Pts',(8.53942996026822,-35.4447364851622,-3.96746489499558));
#49736=CARTESIAN_POINT('Ctrl Pts',(8.59656003661319,-35.4480085275715,-3.88169657838349));
#49737=CARTESIAN_POINT('Ctrl Pts',(8.65136388597018,-35.4517521215922,-3.79459524998933));
#49738=CARTESIAN_POINT('Ctrl Pts',(8.70352740691122,-35.4560050698587,-3.70617136906099));
#49739=CARTESIAN_POINT('Ctrl Pts',(8.75100223690881,-35.4598757440827,-3.62569542267033));
#49740=CARTESIAN_POINT('Ctrl Pts',(8.79628946802519,-35.4641684489054,-3.54412410061856));
#49741=CARTESIAN_POINT('Ctrl Pts',(8.83917328519815,-35.4688825330422,-3.46148888657376));
#49742=CARTESIAN_POINT('Ctrl Pts',(8.86415243523348,-35.4716284130196,-3.41335517213549));
#49743=CARTESIAN_POINT('Ctrl Pts',(8.88831657813022,-35.4745166981789,-3.36486093276358));
#49744=CARTESIAN_POINT('Ctrl Pts',(8.91162790031208,-35.4775418017954,-3.31601642164564));
#49745=CARTESIAN_POINT('Origin',(1.87573872781907,-33.3311293309267,-7.7757813654712));
#49746=CARTESIAN_POINT('Ctrl Pts',(8.75956299023,-36.3742356128,2.0634404101));
#49747=CARTESIAN_POINT('Ctrl Pts',(8.75956299023,-35.3373826802055,2.0634404101));
#49748=CARTESIAN_POINT('Ctrl Pts',(8.92890465395,-36.3742356128,1.78598462948));
#49749=CARTESIAN_POINT('Ctrl Pts',(8.92890465395,-35.3373826802055,1.78598462948));
#49750=CARTESIAN_POINT('Ctrl Pts',(9.07291332076,-36.3742356128,1.49306717121));
#49751=CARTESIAN_POINT('Ctrl Pts',(9.07291332076,-35.3373826802055,1.49306717121));
#49752=CARTESIAN_POINT('Ctrl Pts',(9.12674872803,-36.3742356128,1.15064845916));
#49753=CARTESIAN_POINT('Ctrl Pts',(9.12674872803,-35.3373826802055,1.15064845916));
#49754=CARTESIAN_POINT('Ctrl Pts',(9.18664865847,-36.3742356128,0.831017278590001));
#49755=CARTESIAN_POINT('Ctrl Pts',(9.18664865847,-35.3373826802055,0.831017278590001));
#49756=CARTESIAN_POINT('Ctrl Pts',(9.23698117862,-36.3742356128,0.509886547135));
#49757=CARTESIAN_POINT('Ctrl Pts',(9.23698117862,-35.3373826802055,0.509886547135));
#49758=CARTESIAN_POINT('',(8.75956299007003,-35.6438772168027,2.06344041036242));
#49759=CARTESIAN_POINT('',(8.75956299023,-36.1242356128,2.0634404101));
#49760=CARTESIAN_POINT('',(9.22799880548,-35.5169181946,0.566467047115));
#49761=CARTESIAN_POINT('Ctrl Pts',(9.22799880548,-35.5169181946,0.566467047115));
#49762=CARTESIAN_POINT('Ctrl Pts',(9.22709573015,-35.5170698741,0.572088224967));
#49763=CARTESIAN_POINT('Ctrl Pts',(9.22618896279,-35.5172202096,0.57771674331));
#49764=CARTESIAN_POINT('Ctrl Pts',(9.22528372099,-35.5173684625,0.58332051525));
#49765=CARTESIAN_POINT('Ctrl Pts',(9.21064489493,-35.5197392711,0.67370187071));
#49766=CARTESIAN_POINT('Ctrl Pts',(9.19547141468,-35.5218042907,0.763606652472));
#49767=CARTESIAN_POINT('Ctrl Pts',(9.18087022532,-35.5239641094,0.847743194451));
#49768=CARTESIAN_POINT('Ctrl Pts',(9.1488371776,-35.5298747429,1.02282666839));
#49769=CARTESIAN_POINT('Ctrl Pts',(9.1112963015,-35.5399157471,1.19686722852));
#49770=CARTESIAN_POINT('Ctrl Pts',(9.08965016934,-35.5466085932,1.28690888429));
#49771=CARTESIAN_POINT('Ctrl Pts',(9.04054093324,-35.5631550729,1.46510383868));
#49772=CARTESIAN_POINT('Ctrl Pts',(8.97813093642,-35.5847442368,1.63735111856));
#49773=CARTESIAN_POINT('Ctrl Pts',(8.94306195143,-35.596524942,1.72177132487));
#49774=CARTESIAN_POINT('Ctrl Pts',(8.89434925659,-35.6115263375,1.82461373716));
#49775=CARTESIAN_POINT('Ctrl Pts',(8.84001654494,-35.6256966309,1.92519756404));
#49776=CARTESIAN_POINT('Ctrl Pts',(8.82896553279,-35.6284769797,1.94517168962));
#49777=CARTESIAN_POINT('Ctrl Pts',(8.80877742677,-35.6333588617,1.98085549694));
#49778=CARTESIAN_POINT('Ctrl Pts',(8.78793522997,-35.6380188734,2.01638522454));
#49779=CARTESIAN_POINT('Ctrl Pts',(8.77859596185,-35.6400309319,2.03207294823));
#49780=CARTESIAN_POINT('Ctrl Pts',(8.76913081737,-35.641984033,2.04776380401));
#49781=CARTESIAN_POINT('Ctrl Pts',(8.75956299023,-35.6438772164,2.0634404101));
#49782=CARTESIAN_POINT('Ctrl Pts',(9.23698117862,-35.5153448509,0.509886547139));
#49783=CARTESIAN_POINT('Ctrl Pts',(9.23547079661,-35.5156173384,0.519523062039));
#49784=CARTESIAN_POINT('Ctrl Pts',(9.23395444171,-35.5158907435,0.529141367463));
#49785=CARTESIAN_POINT('Ctrl Pts',(9.2324173579,-35.5161611506,0.538838588998));
#49786=CARTESIAN_POINT('Ctrl Pts',(9.2306125394,-35.5164751965,0.550165758707));
#49787=CARTESIAN_POINT('Ctrl Pts',(9.22879492211,-35.5167839497,0.561507557195));
#49788=CARTESIAN_POINT('Ctrl Pts',(9.22852978607,-35.5168288241,0.563160610681));
#49789=CARTESIAN_POINT('Ctrl Pts',(9.22826440991,-35.5168735732,0.564813796021));
#49790=CARTESIAN_POINT('Ctrl Pts',(9.22799880548,-35.5169181946,0.566467047115));
#49791=CARTESIAN_POINT('Ctrl Pts',(8.75956299024,-36.3742356128,2.0634404101));
#49792=CARTESIAN_POINT('Ctrl Pts',(8.75956299024,-35.2767450158758,2.0634404101));
#49793=CARTESIAN_POINT('Ctrl Pts',(8.72637376563,-36.3742356128,2.11781888978));
#49794=CARTESIAN_POINT('Ctrl Pts',(8.72637376563,-35.2767450158758,2.11781888978));
#49795=CARTESIAN_POINT('Ctrl Pts',(8.6915484,-36.3742356128,2.17268982337));
#49796=CARTESIAN_POINT('Ctrl Pts',(8.6915484,-35.2767450158758,2.17268982337));
#49797=CARTESIAN_POINT('Ctrl Pts',(8.65506636668,-36.3742356128,2.22762960985));
#49798=CARTESIAN_POINT('Ctrl Pts',(8.65506636668,-35.2767450158758,2.22762960985));
#49799=CARTESIAN_POINT('Ctrl Pts',(8.53055023262,-36.3742356128,2.40503324452));
#49800=CARTESIAN_POINT('Ctrl Pts',(8.53055023262,-35.2767450158758,2.40503324452));
#49801=CARTESIAN_POINT('Ctrl Pts',(8.3876008666,-36.3742356128,2.56660232663));
#49802=CARTESIAN_POINT('Ctrl Pts',(8.3876008666,-35.2767450158758,2.56660232663));
#49803=CARTESIAN_POINT('Ctrl Pts',(8.27908544119,-36.3742356128,2.66027026629));
#49804=CARTESIAN_POINT('Ctrl Pts',(8.27908544119,-35.2767450158758,2.66027026629));
#49805=CARTESIAN_POINT('Ctrl Pts',(8.01327762974,-36.3742356128,2.78696551824));
#49806=CARTESIAN_POINT('Ctrl Pts',(8.01327762974,-35.2767450158758,2.78696551824));
#49807=CARTESIAN_POINT('Ctrl Pts',(7.71906576509,-36.3742356128,2.71717075777));
#49808=CARTESIAN_POINT('Ctrl Pts',(7.71906576509,-35.2767450158758,2.71717075777));
#49809=CARTESIAN_POINT('Ctrl Pts',(7.55641153588,-36.3742356128,2.61428156978));
#49810=CARTESIAN_POINT('Ctrl Pts',(7.55641153588,-35.2767450158758,2.61428156978));
#49811=CARTESIAN_POINT('Ctrl Pts',(7.38865661676,-36.3742356128,2.45617777771));
#49812=CARTESIAN_POINT('Ctrl Pts',(7.38865661676,-35.2767450158758,2.45617777771));
#49813=CARTESIAN_POINT('Ctrl Pts',(7.26550535688,-36.3742356128,2.27753774962));
#49814=CARTESIAN_POINT('Ctrl Pts',(7.26550535688,-35.2767450158758,2.27753774962));
#49815=CARTESIAN_POINT('Ctrl Pts',(7.24701042964,-36.3742356128,2.24853650952));
#49816=CARTESIAN_POINT('Ctrl Pts',(7.24701042964,-35.2767450158758,2.24853650952));
#49817=CARTESIAN_POINT('Ctrl Pts',(7.2297761181,-36.3742356128,2.21919784335));
#49818=CARTESIAN_POINT('Ctrl Pts',(7.2297761181,-35.2767450158758,2.21919784335));
#49819=CARTESIAN_POINT('Ctrl Pts',(7.21384189758,-36.3742356128,2.18958432613));
#49820=CARTESIAN_POINT('Ctrl Pts',(7.21384189758,-35.2767450158758,2.18958432613));
#49821=CARTESIAN_POINT('',(7.21384189757838,-35.4651148398171,2.18958432618296));
#49822=CARTESIAN_POINT('',(7.21384189758,-36.1242356128,2.18958432614));
#49823=CARTESIAN_POINT('',(7.23334333080301,-35.4800020975,2.22433302562685));
#49824=CARTESIAN_POINT('Ctrl Pts',(7.23334333044,-35.4800020975,2.22433302572));
#49825=CARTESIAN_POINT('Ctrl Pts',(7.22937402512,-35.477126751,2.21754286118));
#49826=CARTESIAN_POINT('Ctrl Pts',(7.22542564343,-35.4742071929,2.21065452768));
#49827=CARTESIAN_POINT('Ctrl Pts',(7.22151371785,-35.4712377752,2.20368850558));
#49828=CARTESIAN_POINT('Ctrl Pts',(7.21764954964,-35.4682109676,2.19666066586));
#49829=CARTESIAN_POINT('Ctrl Pts',(7.21384189758,-35.46511484,2.18958432614));
#49830=CARTESIAN_POINT('',(8.49626470339955,-35.699502272635,2.43550539329785));
#49831=CARTESIAN_POINT('Ctrl Pts',(8.49626470706,-35.699502273,2.43550539877));
#49832=CARTESIAN_POINT('Ctrl Pts',(8.45240512852,-35.7099399342,2.48655698047));
#49833=CARTESIAN_POINT('Ctrl Pts',(8.40764108873,-35.7197613468,2.53363446576));
#49834=CARTESIAN_POINT('Ctrl Pts',(8.36047222003,-35.7299082045,2.5777319381));
#49835=CARTESIAN_POINT('Ctrl Pts',(8.24494252704,-35.7503872354,2.66806485365));
#49836=CARTESIAN_POINT('Ctrl Pts',(8.12018530542,-35.7590565367,2.723855906));
#49837=CARTESIAN_POINT('Ctrl Pts',(8.0441099093,-35.7553391142,2.74240669266));
#49838=CARTESIAN_POINT('Ctrl Pts',(7.81966214074,-35.7098598702,2.74888110871));
#49839=CARTESIAN_POINT('Ctrl Pts',(7.59696106493,-35.6321549665,2.64143245401));
#49840=CARTESIAN_POINT('Ctrl Pts',(7.45050807009,-35.5975831903,2.52611015512));
#49841=CARTESIAN_POINT('Ctrl Pts',(7.3239386903,-35.5456357901,2.37931366962));
#49842=CARTESIAN_POINT('Ctrl Pts',(7.23334333044,-35.4800020975,2.22433302572));
#49843=CARTESIAN_POINT('',(8.73000675245248,-35.6496340209958,2.1111701504857));
#49844=CARTESIAN_POINT('Ctrl Pts',(8.73000528472,-35.6496341999,2.11117245845));
#49845=CARTESIAN_POINT('Ctrl Pts',(8.71278579373065,-35.6529734545507,2.13857243132976));
#49846=CARTESIAN_POINT('Ctrl Pts',(8.69523611065439,-35.656418433528,2.16578280028398));
#49847=CARTESIAN_POINT('Ctrl Pts',(8.67736328843596,-35.6599993397373,2.19267530487441));
#49848=CARTESIAN_POINT('Ctrl Pts',(8.65990881423403,-35.6634964279019,2.21893833831492));
#49849=CARTESIAN_POINT('Ctrl Pts',(8.64214969971165,-35.6671228124049,2.24489443760551));
#49850=CARTESIAN_POINT('Ctrl Pts',(8.6240892075043,-35.6709094567015,2.27040574861869));
#49851=CARTESIAN_POINT('Ctrl Pts',(8.60885152877019,-35.6741042571869,2.29192970028301));
#49852=CARTESIAN_POINT('Ctrl Pts',(8.59340033381773,-35.6774130775882,2.31313561363373));
#49853=CARTESIAN_POINT('Ctrl Pts',(8.57770836660362,-35.6808587827496,2.33395912375569));
#49854=CARTESIAN_POINT('Ctrl Pts',(8.57480139519109,-35.6814971072033,2.33781672476946));
#49855=CARTESIAN_POINT('Ctrl Pts',(8.57188604813872,-35.6821401439685,2.3416612893117));
#49856=CARTESIAN_POINT('Ctrl Pts',(8.56896198405368,-35.6827880598152,2.34549254173609));
#49857=CARTESIAN_POINT('Ctrl Pts',(8.56143090936174,-35.6844567997929,2.35536012580152));
#49858=CARTESIAN_POINT('Ctrl Pts',(8.55384786331649,-35.6861566070827,2.36513232166256));
#49859=CARTESIAN_POINT('Ctrl Pts',(8.54621303383084,-35.6878884842043,2.37479733602594));
#49860=CARTESIAN_POINT('Ctrl Pts',(8.53873858847129,-35.6895839799504,2.38425931836546));
#49861=CARTESIAN_POINT('Ctrl Pts',(8.53121142039016,-35.6913109462438,2.39362216719067));
#49862=CARTESIAN_POINT('Ctrl Pts',(8.52362054975123,-35.6930722906216,2.40288673572145));
#49863=CARTESIAN_POINT('Ctrl Pts',(8.51695920442706,-35.6946179529959,2.41101682951418));
#49864=CARTESIAN_POINT('Ctrl Pts',(8.51024738112154,-35.6961904182621,2.41907287662946));
#49865=CARTESIAN_POINT('Ctrl Pts',(8.50349797791776,-35.6977863767698,2.42703115952841));
#49866=CARTESIAN_POINT('Ctrl Pts',(8.50255616499077,-35.6980090771046,2.42814165974369));
#49867=CARTESIAN_POINT('Ctrl Pts',(8.50161367399323,-35.6982322214535,2.42925019294274));
#49868=CARTESIAN_POINT('Ctrl Pts',(8.50067059768458,-35.6984557864418,2.43035662659535));
#49869=CARTESIAN_POINT('Ctrl Pts',(8.49920411912565,-35.6988034287893,2.43207712494054));
#49870=CARTESIAN_POINT('Ctrl Pts',(8.49773226797996,-35.6991530223845,2.43379716100814));
#49871=CARTESIAN_POINT('Ctrl Pts',(8.49626469608749,-35.6995022721787,2.43550538236112));
#49872=CARTESIAN_POINT('Origin',(8.8025233360182,-35.5994617475288,1.55277754717549));
#49873=CARTESIAN_POINT('Ctrl Pts',(7.21384189758,-36.3742356128,2.18958432614));
#49874=CARTESIAN_POINT('Ctrl Pts',(7.21384189758,-35.1742356128,2.18958432614));
#49875=CARTESIAN_POINT('Ctrl Pts',(7.13908599018,-36.3742356128,2.05065155888));
#49876=CARTESIAN_POINT('Ctrl Pts',(7.13908599018,-35.1742356128,2.05065155888));
#49877=CARTESIAN_POINT('Ctrl Pts',(7.08904524264,-36.3742356128,1.89842024269));
#49878=CARTESIAN_POINT('Ctrl Pts',(7.08904524264,-35.1742356128,1.89842024269));
#49879=CARTESIAN_POINT('Ctrl Pts',(7.10533215541,-36.3742356128,1.72680915639));
#49880=CARTESIAN_POINT('Ctrl Pts',(7.10533215541,-35.1742356128,1.72680915639));
#49881=CARTESIAN_POINT('Ctrl Pts',(7.09439724612,-36.3742356128,1.56936004643));
#49882=CARTESIAN_POINT('Ctrl Pts',(7.09439724612,-35.1742356128,1.56936004643));
#49883=CARTESIAN_POINT('Ctrl Pts',(7.07911993306,-36.3742356128,1.41233341424));
#49884=CARTESIAN_POINT('Ctrl Pts',(7.07911993306,-35.1742356128,1.41233341424));
#49885=CARTESIAN_POINT('',(7.07911993306,-35.3742356128,1.41233341424));
#49886=CARTESIAN_POINT('',(7.07911993306,-36.1242356128,1.41233341424));
#49887=CARTESIAN_POINT('',(7.1397347564578,-35.374237430427,2.0065547463937));
#49888=CARTESIAN_POINT('Ctrl Pts',(7.07911993306,-35.3742356128,1.41233341424));
#49889=CARTESIAN_POINT('Ctrl Pts',(7.08088379359945,-35.3742356128,1.43046208289637));
#49890=CARTESIAN_POINT('Ctrl Pts',(7.08257391393288,-35.3742355920726,1.44859911701881));
#49891=CARTESIAN_POINT('Ctrl Pts',(7.08413990039285,-35.3742355563688,1.46677978317043));
#49892=CARTESIAN_POINT('Ctrl Pts',(7.0857719589442,-35.3742355191587,1.48572752787993));
#49893=CARTESIAN_POINT('Ctrl Pts',(7.08726945163805,-35.3742354656818,1.50472259826732));
#49894=CARTESIAN_POINT('Ctrl Pts',(7.08862788994042,-35.3742354024484,1.52378297170932));
#49895=CARTESIAN_POINT('Ctrl Pts',(7.09010880652105,-35.3742353335137,1.54456184919967));
#49896=CARTESIAN_POINT('Ctrl Pts',(7.09142454145998,-35.3742352529839,1.56541838105122));
#49897=CARTESIAN_POINT('Ctrl Pts',(7.0926283564623,-35.3742351692935,1.58635022088257));
#49898=CARTESIAN_POINT('Ctrl Pts',(7.09392979130781,-35.3742350788164,1.60897946680883));
#49899=CARTESIAN_POINT('Ctrl Pts',(7.09510098835278,-35.3742349846454,1.63169662189142));
#49900=CARTESIAN_POINT('Ctrl Pts',(7.09627031081491,-35.374234897438,1.65447046219548));
#49901=CARTESIAN_POINT('Ctrl Pts',(7.09759721920307,-35.3742347984778,1.68031346163214));
#49902=CARTESIAN_POINT('Ctrl Pts',(7.09892280102895,-35.3742347084845,1.70622930734304));
#49903=CARTESIAN_POINT('Ctrl Pts',(7.10049797330183,-35.3742346430312,1.73213889512637));
#49904=CARTESIAN_POINT('Ctrl Pts',(7.10268355309499,-35.3742345522134,1.76808891309181));
#49905=CARTESIAN_POINT('Ctrl Pts',(7.10535563162098,-35.3742345086401,1.80402663896773));
#49906=CARTESIAN_POINT('Ctrl Pts',(7.10925382044881,-35.3742345539108,1.83967755757583));
#49907=CARTESIAN_POINT('Ctrl Pts',(7.11201818443795,-35.3742345860141,1.86495907161537));
#49908=CARTESIAN_POINT('Ctrl Pts',(7.11540160752117,-35.3742346627953,1.89009455114752));
#49909=CARTESIAN_POINT('Ctrl Pts',(7.11963758304748,-35.3742347990894,1.91498267217133));
#49910=CARTESIAN_POINT('Ctrl Pts',(7.12328042918059,-35.3742349162993,1.93638591089839));
#49911=CARTESIAN_POINT('Ctrl Pts',(7.12755425624601,-35.3742350775227,1.95760586664661));
#49912=CARTESIAN_POINT('Ctrl Pts',(7.13256782595141,-35.3742352921947,1.97858502102889));
#49913=CARTESIAN_POINT('Ctrl Pts',(7.13480768313481,-35.3742353881014,1.98795764620536));
#49914=CARTESIAN_POINT('Ctrl Pts',(7.13719457595005,-35.374235494676,1.99728233675496));
#49915=CARTESIAN_POINT('Ctrl Pts',(7.13973478937165,-35.37423561276,2.00655473739996));
#49916=CARTESIAN_POINT('Ctrl Pts',(7.21384189752768,-35.4651148399886,2.18958432613476));
#49917=CARTESIAN_POINT('Ctrl Pts',(7.20248970608986,-35.4558376974459,2.16852385244726));
#49918=CARTESIAN_POINT('Ctrl Pts',(7.19216154685804,-35.4455454559162,2.14764262477417));
#49919=CARTESIAN_POINT('Ctrl Pts',(7.18277070542258,-35.4348282931029,2.12663643219701));
#49920=CARTESIAN_POINT('Ctrl Pts',(7.17770336693684,-35.4290452658892,2.11530140020689));
#49921=CARTESIAN_POINT('Ctrl Pts',(7.17290922441346,-35.4231375971107,2.10393011818054));
#49922=CARTESIAN_POINT('Ctrl Pts',(7.16837646591349,-35.4171920851989,2.09247569166495));
#49923=CARTESIAN_POINT('Ctrl Pts',(7.1586926057656,-35.404489995321,2.06800426561125));
#49924=CARTESIAN_POINT('Ctrl Pts',(7.15020429789434,-35.3915941161304,2.04315346963811));
#49925=CARTESIAN_POINT('Ctrl Pts',(7.14282824899172,-35.3794131715241,2.01756660856244));
#49926=CARTESIAN_POINT('Ctrl Pts',(7.14201563347066,-35.37807120311,2.01474771721293));
#49927=CARTESIAN_POINT('Ctrl Pts',(7.14121690146011,-35.376735446728,2.01192135159036));
#49928=CARTESIAN_POINT('Ctrl Pts',(7.1404309617392,-35.3754137600701,2.0090835975648));
#49929=CARTESIAN_POINT('Ctrl Pts',(7.1401977511474,-35.375021578177,2.00824155551238));
#49930=CARTESIAN_POINT('Ctrl Pts',(7.13996568730528,-35.3746302925694,2.00739857926709));
#49931=CARTESIAN_POINT('Ctrl Pts',(7.13973478936,-35.3742392475,2.00655473738));
#49932=CARTESIAN_POINT('Ctrl Pts',(7.07911993306,-36.3742356128,1.41233341424));
#49933=CARTESIAN_POINT('Ctrl Pts',(7.07911993306,-35.17422421556,1.41233341424));
#49934=CARTESIAN_POINT('Ctrl Pts',(7.02062825816,-36.3742356128,0.811131443794));
#49935=CARTESIAN_POINT('Ctrl Pts',(7.02062825816,-35.17422421556,0.811131443794));
#49936=CARTESIAN_POINT('Ctrl Pts',(6.90206842567,-36.3742356128,0.252977206386));
#49937=CARTESIAN_POINT('Ctrl Pts',(6.90206842567,-35.17422421556,0.252977206386));
#49938=CARTESIAN_POINT('Ctrl Pts',(6.72344043556,-36.3742356128,-0.262129297982999));
#49939=CARTESIAN_POINT('Ctrl Pts',(6.72344043556,-35.17422421556,-0.262129297983));
#49940=CARTESIAN_POINT('Ctrl Pts',(6.21056508527,-36.3742356128,-1.27642010253));
#49941=CARTESIAN_POINT('Ctrl Pts',(6.21056508527,-35.17422421556,-1.27642010253));
#49942=CARTESIAN_POINT('Ctrl Pts',(5.42037231907,-36.3742356128,-2.09197189854));
#49943=CARTESIAN_POINT('Ctrl Pts',(5.42037231907,-35.17422421556,-2.09197189854));
#49944=CARTESIAN_POINT('Ctrl Pts',(4.91868712629,-36.3742356128,-2.4711621885));
#49945=CARTESIAN_POINT('Ctrl Pts',(4.91868712629,-35.17422421556,-2.4711621885));
#49946=CARTESIAN_POINT('Ctrl Pts',(4.33774769283,-36.3742356128,-2.79355507478));
#49947=CARTESIAN_POINT('Ctrl Pts',(4.33774769283,-35.17422421556,-2.79355507478));
#49948=CARTESIAN_POINT('Ctrl Pts',(3.67755401866,-36.3742356128,-3.05915055738));
#49949=CARTESIAN_POINT('Ctrl Pts',(3.67755401866,-35.17422421556,-3.05915055738));
#49950=CARTESIAN_POINT('',(3.67755401867,-35.5065774118,-3.05915055738));
#49951=CARTESIAN_POINT('',(3.67755401867,-36.1242356128,-3.05915055738));
#49952=CARTESIAN_POINT('',(7.05021190275089,-35.3742261150874,1.16209541224075));
#49953=CARTESIAN_POINT('Ctrl Pts',(7.05021190275,-35.3742261151,1.16209541223));
#49954=CARTESIAN_POINT('Ctrl Pts',(7.01549246939,-35.4131252568,0.903392902078));
#49955=CARTESIAN_POINT('Ctrl Pts',(6.96767646618,-35.4506441608,0.642127552041));
#49956=CARTESIAN_POINT('Ctrl Pts',(6.90349674466,-35.485563689,0.372787607728));
#49957=CARTESIAN_POINT('Ctrl Pts',(6.71982081074,-35.5526247648,-0.221149174844));
#49958=CARTESIAN_POINT('Ctrl Pts',(6.43798249823,-35.5965248091,-0.799107100072));
#49959=CARTESIAN_POINT('Ctrl Pts',(6.25293978467,-35.6126874115,-1.1016283265));
#49960=CARTESIAN_POINT('Ctrl Pts',(5.73382235555,-35.6343159234,-1.78819570677));
#49961=CARTESIAN_POINT('Ctrl Pts',(5.06131871348,-35.6148773502,-2.35107992573));
#49962=CARTESIAN_POINT('Ctrl Pts',(4.62352979415,-35.5904307331,-2.63143094545));
#49963=CARTESIAN_POINT('Ctrl Pts',(4.15886281142,-35.5534449291,-2.86552034537));
#49964=CARTESIAN_POINT('Ctrl Pts',(3.67755401867,-35.5065774118,-3.05915055738));
#49965=CARTESIAN_POINT('Ctrl Pts',(7.05021164825251,-35.3742261150622,1.16209544641769));
#49966=CARTESIAN_POINT('Ctrl Pts',(7.05298995234347,-35.3742266401801,1.18279723134882));
#49967=CARTESIAN_POINT('Ctrl Pts',(7.05571064340935,-35.3742477797274,1.20381716459059));
#49968=CARTESIAN_POINT('Ctrl Pts',(7.0582960532776,-35.3742431701946,1.22454392284646));
#49969=CARTESIAN_POINT('Ctrl Pts',(7.06089275591971,-35.3742385405279,1.24536121320582));
#49970=CARTESIAN_POINT('Ctrl Pts',(7.06339480482353,-35.3742375427219,1.26620204691362));
#49971=CARTESIAN_POINT('Ctrl Pts',(7.06580506972233,-35.3742369799114,1.28708281574342));
#49972=CARTESIAN_POINT('Ctrl Pts',(7.07061980686755,-35.3742358556428,1.32879417010786));
#49973=CARTESIAN_POINT('Ctrl Pts',(7.07505478224174,-35.3742356535495,1.37055008889877));
#49974=CARTESIAN_POINT('Ctrl Pts',(7.07911993306,-35.3742356128,1.41233341424));
#49975=CARTESIAN_POINT('Origin',(3.78952269078,-36.1242356128,-3.33747234321));
#49976=CARTESIAN_POINT('',(3.52268743213354,-35.4813642832762,-3.20036310945193));
#49977=CARTESIAN_POINT('Origin',(3.61904102711591,-42.5155158381654,-3.57476675253502));
#49978=CARTESIAN_POINT('',(3.67199242350841,-35.5050278513059,-3.06145306063948));
#49979=CARTESIAN_POINT('Ctrl Pts',(3.67199241167966,-35.5050281562424,-3.06145308005705));
#49980=CARTESIAN_POINT('Ctrl Pts',(3.6709074577687,-35.5049566525245,-3.06191505565046));
#49981=CARTESIAN_POINT('Ctrl Pts',(3.66982199759305,-35.5048835280257,-3.06238484334962));
#49982=CARTESIAN_POINT('Ctrl Pts',(3.66873907853604,-35.50480884055,-3.06286118186356));
#49983=CARTESIAN_POINT('Ctrl Pts',(3.66289150728548,-35.5044055413997,-3.06543332553541));
#49984=CARTESIAN_POINT('Ctrl Pts',(3.65709238413361,-35.5039531995699,-3.06820792066641));
#49985=CARTESIAN_POINT('Ctrl Pts',(3.65138326543097,-35.5034460774675,-3.07116933797591));
#49986=CARTESIAN_POINT('Ctrl Pts',(3.64385317118268,-35.5027772041395,-3.07507532637981));
#49987=CARTESIAN_POINT('Ctrl Pts',(3.63648014365973,-35.502013095345,-3.07930633742901));
#49988=CARTESIAN_POINT('Ctrl Pts',(3.62931742279077,-35.501179385654,-3.08383070640602));
#49989=CARTESIAN_POINT('Ctrl Pts',(3.62044924431927,-35.5001471680835,-3.08943233633033));
#49990=CARTESIAN_POINT('Ctrl Pts',(3.61190059299212,-35.4990131921254,-3.09548294507778));
#49991=CARTESIAN_POINT('Ctrl Pts',(3.60370943709272,-35.4978391465399,-3.10194452884521));
#49992=CARTESIAN_POINT('Ctrl Pts',(3.60239376448108,-35.4976505700263,-3.10298239564875));
#49993=CARTESIAN_POINT('Ctrl Pts',(3.60108727881218,-35.4974608692547,-3.10403091641481));
#49994=CARTESIAN_POINT('Ctrl Pts',(3.59979013424323,-35.4972701540212,-3.10508999234876));
#49995=CARTESIAN_POINT('Ctrl Pts',(3.59307320703001,-35.4962825845759,-3.11057414279112));
#49996=CARTESIAN_POINT('Ctrl Pts',(3.58660464543982,-35.4952699607466,-3.11634152422183));
#49997=CARTESIAN_POINT('Ctrl Pts',(3.58038951136343,-35.4942505186859,-3.12238406331074));
#49998=CARTESIAN_POINT('Ctrl Pts',(3.57282468603545,-35.4930096924983,-3.12973881257009));
#49999=CARTESIAN_POINT('Ctrl Pts',(3.56563464692084,-35.4917567679128,-3.13750357265183));
#50000=CARTESIAN_POINT('Ctrl Pts',(3.5588517837043,-35.490452932207,-3.14566041031418));
#50001=CARTESIAN_POINT('Ctrl Pts',(3.55802545675573,-35.4902940915308,-3.14665412263896));
#50002=CARTESIAN_POINT('Ctrl Pts',(3.55720520361751,-35.4901344532814,-3.14765361987113));
#50003=CARTESIAN_POINT('Ctrl Pts',(3.55639110831416,-35.4899739242682,-3.14865883467));
#50004=CARTESIAN_POINT('Ctrl Pts',(3.55057178146724,-35.4888264286467,-3.15584432443014));
#50005=CARTESIAN_POINT('Ctrl Pts',(3.54506529823488,-35.4876301819156,-3.1633259113768));
#50006=CARTESIAN_POINT('Ctrl Pts',(3.53991036414267,-35.4863565833647,-3.17105947667676));
#50007=CARTESIAN_POINT('Ctrl Pts',(3.53549626013491,-35.4852660172455,-3.17768162954511));
#50008=CARTESIAN_POINT('Ctrl Pts',(3.53134016454137,-35.4841178588891,-3.18448858769416));
#50009=CARTESIAN_POINT('Ctrl Pts',(3.52747469739242,-35.4829203077151,-3.19142278851816));
#50010=CARTESIAN_POINT('Ctrl Pts',(3.5261396778866,-35.4825067085007,-3.19381765904754));
#50011=CARTESIAN_POINT('Ctrl Pts',(3.52483939140283,-35.4820875246346,-3.19622741344477));
#50012=CARTESIAN_POINT('Ctrl Pts',(3.5235753914424,-35.481664210634,-3.1986486709718));
#50013=CARTESIAN_POINT('Ctrl Pts',(3.52327750749173,-35.4815644492014,-3.19921928313977));
#50014=CARTESIAN_POINT('Ctrl Pts',(3.52298214216414,-35.4814641936595,-3.19978955303356));
#50015=CARTESIAN_POINT('Ctrl Pts',(3.5226878028,-35.4813642944,-3.200362378));
#50016=CARTESIAN_POINT('Ctrl Pts',(3.67755401867,-35.5065774118,-3.05915055738));
#50017=CARTESIAN_POINT('Ctrl Pts',(3.67567292389694,-35.5056650882282,-3.05990732050017));
#50018=CARTESIAN_POINT('Ctrl Pts',(3.67381662092036,-35.5051480133643,-3.06067630953423));
#50019=CARTESIAN_POINT('Ctrl Pts',(3.67199243004608,-35.5050275473134,-3.06145302884574));
#50020=CARTESIAN_POINT('Origin',(-1.81727342606,-36.1242356128,-5.3088808072));
#50021=CARTESIAN_POINT('',(-1.68475791584498,-35.4771141120081,-5.0397346703217));
#50022=CARTESIAN_POINT('',(-1.68475792039,-36.1242356128,-5.03973467448));
#50023=CARTESIAN_POINT('',(-1.67696448377282,-35.4768981244436,-5.04371406606362));
#50024=CARTESIAN_POINT('Origin',(-1.6862492552706,-35.5734099629681,-5.04271729832598));
#50025=CARTESIAN_POINT('',(-1.51727373422622,-35.5445458978274,-5.30855096294675));
#50026=CARTESIAN_POINT('Ctrl Pts',(-1.67696448332951,-35.4768981249,-5.04371406628026));
#50027=CARTESIAN_POINT('Ctrl Pts',(-1.66756289682901,-35.4812014304152,
-5.04868876654869));
#50028=CARTESIAN_POINT('Ctrl Pts',(-1.65865341395941,-35.4852624079317,
-5.05404323411107));
#50029=CARTESIAN_POINT('Ctrl Pts',(-1.65022740097744,-35.4891142229921,
-5.05969253075887));
#50030=CARTESIAN_POINT('Ctrl Pts',(-1.63878500787594,-35.4943449272611,
-5.06736418675197));
#50031=CARTESIAN_POINT('Ctrl Pts',(-1.62823550640092,-35.4991871312493,
-5.07558040378508));
#50032=CARTESIAN_POINT('Ctrl Pts',(-1.61857496186333,-35.503616112498,-5.08412107360671));
#50033=CARTESIAN_POINT('Ctrl Pts',(-1.61461412195328,-35.5054320024432,
-5.08762276295316));
#50034=CARTESIAN_POINT('Ctrl Pts',(-1.61080272967728,-35.5071777837279,
-5.09117884037656));
#50035=CARTESIAN_POINT('Ctrl Pts',(-1.60714002108678,-35.5088508710531,
-5.09477352063633));
#50036=CARTESIAN_POINT('Ctrl Pts',(-1.59755275514454,-35.5132302347767,
-5.10418272007882));
#50037=CARTESIAN_POINT('Ctrl Pts',(-1.58896916888366,-35.5171365517006,
-5.11387017935044));
#50038=CARTESIAN_POINT('Ctrl Pts',(-1.58131204543875,-35.520569821731,-5.12362230218826));
#50039=CARTESIAN_POINT('Ctrl Pts',(-1.5784190059488,-35.5218669910727,-5.12730688121897));
#50040=CARTESIAN_POINT('Ctrl Pts',(-1.57579805519001,-35.523034690164,-5.13081589216099));
#50041=CARTESIAN_POINT('Ctrl Pts',(-1.57327569865429,-35.5241485245477,
-5.13434172428996));
#50042=CARTESIAN_POINT('Ctrl Pts',(-1.57079104913356,-35.5252457080857,
-5.1378148483251));
#50043=CARTESIAN_POINT('Ctrl Pts',(-1.5684020132668,-35.526290690752,-5.14130475228606));
#50044=CARTESIAN_POINT('Ctrl Pts',(-1.56597703365574,-35.5273357042058,
-5.14502335170683));
#50045=CARTESIAN_POINT('Ctrl Pts',(-1.56434809980794,-35.5280376720816,
-5.147521250013));
#50046=CARTESIAN_POINT('Ctrl Pts',(-1.56270356513962,-35.5287392753758,
-5.15012286969908));
#50047=CARTESIAN_POINT('Ctrl Pts',(-1.56101368681577,-35.5294504909325,
-5.15289878983892));
#50048=CARTESIAN_POINT('Ctrl Pts',(-1.557010778241,-35.5311351866944,-5.15947426593909));
#50049=CARTESIAN_POINT('Ctrl Pts',(-1.55321985384439,-35.5326854602331,
-5.16627227889667));
#50050=CARTESIAN_POINT('Ctrl Pts',(-1.54967548527541,-35.5340943103496,
-5.17326610846632));
#50051=CARTESIAN_POINT('Ctrl Pts',(-1.54469252990046,-35.5360749839517,
-5.18309859060448));
#50052=CARTESIAN_POINT('Ctrl Pts',(-1.54019901641157,-35.5377746196872,
-5.1933165367817));
#50053=CARTESIAN_POINT('Ctrl Pts',(-1.53626707299023,-35.5391855953774,
-5.20383985939881));
#50054=CARTESIAN_POINT('Ctrl Pts',(-1.53153200391583,-35.5408847722575,
-5.21651264080603));
#50055=CARTESIAN_POINT('Ctrl Pts',(-1.52761121680424,-35.5421688202375,
-5.22962559950965));
#50056=CARTESIAN_POINT('Ctrl Pts',(-1.52459023053592,-35.5430760811842,
-5.24305374223109));
#50057=CARTESIAN_POINT('Ctrl Pts',(-1.52222092663657,-35.5437876292376,
-5.25358518729078));
#50058=CARTESIAN_POINT('Ctrl Pts',(-1.52040370135698,-35.544270262472,-5.26431017256738));
#50059=CARTESIAN_POINT('Ctrl Pts',(-1.5191724082318,-35.5445240117425,-5.27519362838246));
#50060=CARTESIAN_POINT('Ctrl Pts',(-1.51811496284579,-35.544741933852,-5.28454043614104));
#50061=CARTESIAN_POINT('Ctrl Pts',(-1.517489253763,-35.5447918131442,-5.29400411313174));
#50062=CARTESIAN_POINT('Ctrl Pts',(-1.51732015056857,-35.5446392551355,
-5.30358506151032));
#50063=CARTESIAN_POINT('Ctrl Pts',(-1.51729234940888,-35.5446141740625,
-5.30516020310793));
#50064=CARTESIAN_POINT('Ctrl Pts',(-1.51727690525093,-35.5445835229505,
-5.30673857060276));
#50065=CARTESIAN_POINT('Ctrl Pts',(-1.51727394979,-35.5445470238,-5.30832023528));
#50066=CARTESIAN_POINT('',(-1.51727342606,-35.9593880834,-5.3088808072));
#50067=CARTESIAN_POINT('Ctrl Pts',(-3.51985615629,-36.3742356128,-3.20601908088));
#50068=CARTESIAN_POINT('Ctrl Pts',(-3.51985615629,-35.2912304609806,-3.20601908088));
#50069=CARTESIAN_POINT('Ctrl Pts',(-3.41903503516,-36.3742356128,-3.4128460691));
#50070=CARTESIAN_POINT('Ctrl Pts',(-3.41903503516,-35.2912304609806,-3.4128460691));
#50071=CARTESIAN_POINT('Ctrl Pts',(-3.30675917974,-36.3742356128,-3.60871163219));
#50072=CARTESIAN_POINT('Ctrl Pts',(-3.30675917974,-35.2912304609806,-3.60871163219));
#50073=CARTESIAN_POINT('Ctrl Pts',(-3.18302859005,-36.3742356128,-3.79361577017));
#50074=CARTESIAN_POINT('Ctrl Pts',(-3.18302859005,-35.2912304609806,-3.79361577017));
#50075=CARTESIAN_POINT('Ctrl Pts',(-2.86303108781,-36.3742356128,-4.20535597988));
#50076=CARTESIAN_POINT('Ctrl Pts',(-2.86303108781,-35.2912304609806,-4.20535597988));
#50077=CARTESIAN_POINT('Ctrl Pts',(-2.47885071991,-36.3742356128,-4.55567742084));
#50078=CARTESIAN_POINT('Ctrl Pts',(-2.47885071991,-35.2912304609806,-4.55567742084));
#50079=CARTESIAN_POINT('Ctrl Pts',(-2.23556166242,-36.3742356128,-4.73751640159));
#50080=CARTESIAN_POINT('Ctrl Pts',(-2.23556166242,-35.2912304609806,-4.73751640159));
#50081=CARTESIAN_POINT('Ctrl Pts',(-1.97086406258,-36.3742356128,-4.89886881947));
#50082=CARTESIAN_POINT('Ctrl Pts',(-1.97086406258,-35.2912304609806,-4.89886881947));
#50083=CARTESIAN_POINT('Ctrl Pts',(-1.68475792038,-36.3742356128,-5.03973467448));
#50084=CARTESIAN_POINT('Ctrl Pts',(-1.68475792038,-35.2912304609806,-5.03973467448));
#50085=CARTESIAN_POINT('',(-3.51985615281972,-35.4822398766,-3.20601907918835));
#50086=CARTESIAN_POINT('',(-3.51985615629,-36.1242356128,-3.20601908088));
#50087=CARTESIAN_POINT('Ctrl Pts',(-3.51985614934943,-35.4822398766,-3.2060190774967));
#50088=CARTESIAN_POINT('Ctrl Pts',(-3.47358259555133,-35.4902367502796,
-3.30094564082806));
#50089=CARTESIAN_POINT('Ctrl Pts',(-3.4242629704013,-35.4972659530676,-3.39340146700136));
#50090=CARTESIAN_POINT('Ctrl Pts',(-3.3718427520045,-35.503328318492,-3.48331166418977));
#50091=CARTESIAN_POINT('Ctrl Pts',(-3.31249447844996,-35.510191909156,-3.58510473452171));
#50092=CARTESIAN_POINT('Ctrl Pts',(-3.24917345130392,-35.5158169873826,
-3.68363701688898));
#50093=CARTESIAN_POINT('Ctrl Pts',(-3.18180390147332,-35.5202068551407,
-3.77885381081047));
#50094=CARTESIAN_POINT('Ctrl Pts',(-3.13358539867495,-35.5233488213748,
-3.84700346084822));
#50095=CARTESIAN_POINT('Ctrl Pts',(-3.08318941873635,-35.5258600003757,
-3.91359418324414));
#50096=CARTESIAN_POINT('Ctrl Pts',(-3.03070303605501,-35.527733093042,-3.97843169083073));
#50097=CARTESIAN_POINT('Ctrl Pts',(-2.97800189477388,-35.5296138498439,
-4.04353449413085));
#50098=CARTESIAN_POINT('Ctrl Pts',(-2.92319335516364,-35.530851377402,-4.10686950873771));
#50099=CARTESIAN_POINT('Ctrl Pts',(-2.86640625775876,-35.5314483764335,
-4.16827188132273));
#50100=CARTESIAN_POINT('Ctrl Pts',(-2.83093719259086,-35.5318212603899,
-4.20662363469999));
#50101=CARTESIAN_POINT('Ctrl Pts',(-2.7946970489135,-35.5319444556458,-4.24422206648277));
#50102=CARTESIAN_POINT('Ctrl Pts',(-2.75772481668771,-35.5318203627783,
-4.28103375340558));
#50103=CARTESIAN_POINT('Ctrl Pts',(-2.67048928304337,-35.531527567162,-4.36789048235417));
#50104=CARTESIAN_POINT('Ctrl Pts',(-2.57940688791399,-35.5298512045927,
-4.45014995560896));
#50105=CARTESIAN_POINT('Ctrl Pts',(-2.48455366341829,-35.5268238896998,
-4.52797607796499));
#50106=CARTESIAN_POINT('Ctrl Pts',(-2.39693745208812,-35.5240275497458,
-4.59986430337437));
#50107=CARTESIAN_POINT('Ctrl Pts',(-2.30610083339999,-35.5200781360858,
-4.66796989091402));
#50108=CARTESIAN_POINT('Ctrl Pts',(-2.21210582445137,-35.5149804585593,
-4.7323874423026));
#50109=CARTESIAN_POINT('Ctrl Pts',(-2.12903950494902,-35.5104754820199,
-4.78931524054483));
#50110=CARTESIAN_POINT('Ctrl Pts',(-2.04350466714415,-35.5050732914157,
-4.84336174171714));
#50111=CARTESIAN_POINT('Ctrl Pts',(-1.95557759183873,-35.4987661218997,
-4.89457253052966));
#50112=CARTESIAN_POINT('Ctrl Pts',(-1.87970413987643,-35.4933235807754,
-4.93876300668755));
#50113=CARTESIAN_POINT('Ctrl Pts',(-1.80204873908433,-35.487206903096,-4.98084109124512));
#50114=CARTESIAN_POINT('Ctrl Pts',(-1.72270160875273,-35.4804067652161,
-5.02083270682539));
#50115=CARTESIAN_POINT('Ctrl Pts',(-1.71009614007247,-35.4793264624413,
-5.02718596819179));
#50116=CARTESIAN_POINT('Ctrl Pts',(-1.69744808216162,-35.4782289048639,
-5.03348657861682));
#50117=CARTESIAN_POINT('Ctrl Pts',(-1.68475792683372,-35.4771140496188,
-5.03973465570198));
#50118=CARTESIAN_POINT('Origin',(-3.78952269078,-36.1242356128,-3.33747234321));
#50119=CARTESIAN_POINT('',(-3.67755401867,-35.5065774118,-3.05915055738));
#50120=CARTESIAN_POINT('',(-3.67755401867,-36.1242356128,-3.05915055738));
#50121=CARTESIAN_POINT('',(-3.67199242351697,-35.5050278513065,-3.06145306063582));
#50122=CARTESIAN_POINT('Ctrl Pts',(-3.67755401867,-35.5065774118,-3.05915055738));
#50123=CARTESIAN_POINT('Ctrl Pts',(-3.67567292389988,-35.5056650882297,
-3.05990732049898));
#50124=CARTESIAN_POINT('Ctrl Pts',(-3.67381662092617,-35.5051480133659,
-3.06067630953182));
#50125=CARTESIAN_POINT('Ctrl Pts',(-3.67199243005465,-35.505027547314,-3.06145302884209));
#50126=CARTESIAN_POINT('',(-3.52268743213354,-35.4813642832762,-3.20036310945193));
#50127=CARTESIAN_POINT('Ctrl Pts',(-3.67199241168822,-35.5050281562429,
-3.0614530800534));
#50128=CARTESIAN_POINT('Ctrl Pts',(-3.67090745777441,-35.5049566525248,
-3.06191505564798));
#50129=CARTESIAN_POINT('Ctrl Pts',(-3.6698219975959,-35.5048835280259,-3.06238484334836));
#50130=CARTESIAN_POINT('Ctrl Pts',(-3.66873907853603,-35.50480884055,-3.06286118186355));
#50131=CARTESIAN_POINT('Ctrl Pts',(-3.66289150728548,-35.5044055413997,
-3.06543332553541));
#50132=CARTESIAN_POINT('Ctrl Pts',(-3.65709238413361,-35.5039531995698,
-3.06820792066641));
#50133=CARTESIAN_POINT('Ctrl Pts',(-3.65138326543097,-35.5034460774675,
-3.0711693379759));
#50134=CARTESIAN_POINT('Ctrl Pts',(-3.64385317118269,-35.5027772041395,
-3.0750753263798));
#50135=CARTESIAN_POINT('Ctrl Pts',(-3.63648014365975,-35.502013095345,-3.079306337429));
#50136=CARTESIAN_POINT('Ctrl Pts',(-3.6293174227908,-35.501179385654,-3.083830706406));
#50137=CARTESIAN_POINT('Ctrl Pts',(-3.62044924431911,-35.5001471680835,
-3.08943233633042));
#50138=CARTESIAN_POINT('Ctrl Pts',(-3.6119005929918,-35.4990131921253,-3.09548294507801));
#50139=CARTESIAN_POINT('Ctrl Pts',(-3.60370943709224,-35.4978391465398,
-3.10194452884559));
#50140=CARTESIAN_POINT('Ctrl Pts',(-3.60239376448076,-35.4976505700263,
-3.10298239564901));
#50141=CARTESIAN_POINT('Ctrl Pts',(-3.60108727881202,-35.4974608692547,
-3.10403091641494));
#50142=CARTESIAN_POINT('Ctrl Pts',(-3.59979013424323,-35.4972701540212,
-3.10508999234876));
#50143=CARTESIAN_POINT('Ctrl Pts',(-3.59307320703006,-35.4962825845759,
-3.11057414279108));
#50144=CARTESIAN_POINT('Ctrl Pts',(-3.58660464543991,-35.4952699607466,
-3.11634152422175));
#50145=CARTESIAN_POINT('Ctrl Pts',(-3.58038951136356,-35.4942505186859,
-3.12238406331061));
#50146=CARTESIAN_POINT('Ctrl Pts',(-3.57282468603562,-35.4930096924983,
-3.12973881256992));
#50147=CARTESIAN_POINT('Ctrl Pts',(-3.56563464692104,-35.4917567679128,
-3.13750357265161));
#50148=CARTESIAN_POINT('Ctrl Pts',(-3.55885178370453,-35.4904529322071,
-3.14566041031391));
#50149=CARTESIAN_POINT('Ctrl Pts',(-3.55802545675588,-35.4902940915308,
-3.14665412263877));
#50150=CARTESIAN_POINT('Ctrl Pts',(-3.55720520361759,-35.4901344532814,
-3.14765361987103));
#50151=CARTESIAN_POINT('Ctrl Pts',(-3.55639110831416,-35.4899739242682,
-3.14865883467));
#50152=CARTESIAN_POINT('Ctrl Pts',(-3.55057178146725,-35.4888264286467,
-3.15584432443014));
#50153=CARTESIAN_POINT('Ctrl Pts',(-3.54506529823488,-35.4876301819156,
-3.16332591137679));
#50154=CARTESIAN_POINT('Ctrl Pts',(-3.53991036414268,-35.4863565833647,
-3.17105947667675));
#50155=CARTESIAN_POINT('Ctrl Pts',(-3.53549626013493,-35.4852660172455,
-3.17768162954508));
#50156=CARTESIAN_POINT('Ctrl Pts',(-3.53134016454139,-35.4841178588891,
-3.18448858769411));
#50157=CARTESIAN_POINT('Ctrl Pts',(-3.52747469739246,-35.4829203077152,
-3.1914227885181));
#50158=CARTESIAN_POINT('Ctrl Pts',(-3.52613967788663,-35.4825067085007,
-3.1938176590475));
#50159=CARTESIAN_POINT('Ctrl Pts',(-3.52483939140284,-35.4820875246346,
-3.19622741344476));
#50160=CARTESIAN_POINT('Ctrl Pts',(-3.5235753914424,-35.481664210634,-3.1986486709718));
#50161=CARTESIAN_POINT('Ctrl Pts',(-3.52327750749173,-35.4815644492014,
-3.19921928313977));
#50162=CARTESIAN_POINT('Ctrl Pts',(-3.52298214216414,-35.4814641936595,
-3.19978955303356));
#50163=CARTESIAN_POINT('Ctrl Pts',(-3.5226878028,-35.4813642944,-3.200362378));
#50164=CARTESIAN_POINT('Origin',(-3.61904102711591,-42.5155158381654,-3.57476675253502));
#50165=CARTESIAN_POINT('Ctrl Pts',(-7.07911993306,-36.3742356128,1.41233341424));
#50166=CARTESIAN_POINT('Ctrl Pts',(-7.07911993306,-35.17422421556,1.41233341424));
#50167=CARTESIAN_POINT('Ctrl Pts',(-7.02062825816,-36.3742356128,0.811131443794));
#50168=CARTESIAN_POINT('Ctrl Pts',(-7.02062825816,-35.17422421556,0.811131443794));
#50169=CARTESIAN_POINT('Ctrl Pts',(-6.90206842567,-36.3742356128,0.252977206386));
#50170=CARTESIAN_POINT('Ctrl Pts',(-6.90206842567,-35.17422421556,0.252977206386));
#50171=CARTESIAN_POINT('Ctrl Pts',(-6.72344043556,-36.3742356128,-0.262129297982999));
#50172=CARTESIAN_POINT('Ctrl Pts',(-6.72344043556,-35.17422421556,-0.262129297983));
#50173=CARTESIAN_POINT('Ctrl Pts',(-6.21056508527,-36.3742356128,-1.27642010253));
#50174=CARTESIAN_POINT('Ctrl Pts',(-6.21056508527,-35.17422421556,-1.27642010253));
#50175=CARTESIAN_POINT('Ctrl Pts',(-5.42037231907,-36.3742356128,-2.09197189854));
#50176=CARTESIAN_POINT('Ctrl Pts',(-5.42037231907,-35.17422421556,-2.09197189854));
#50177=CARTESIAN_POINT('Ctrl Pts',(-4.91868712629,-36.3742356128,-2.4711621885));
#50178=CARTESIAN_POINT('Ctrl Pts',(-4.91868712629,-35.17422421556,-2.4711621885));
#50179=CARTESIAN_POINT('Ctrl Pts',(-4.33774769283,-36.3742356128,-2.79355507478));
#50180=CARTESIAN_POINT('Ctrl Pts',(-4.33774769283,-35.17422421556,-2.79355507478));
#50181=CARTESIAN_POINT('Ctrl Pts',(-3.67755401866,-36.3742356128,-3.05915055738));
#50182=CARTESIAN_POINT('Ctrl Pts',(-3.67755401866,-35.17422421556,-3.05915055738));
#50183=CARTESIAN_POINT('',(-7.07911993306,-35.3742356128,1.41233341424));
#50184=CARTESIAN_POINT('',(-7.07911993306,-36.1242356128,1.41233341424));
#50185=CARTESIAN_POINT('',(-7.05021189233511,-35.3742261184909,1.16209533463037));
#50186=CARTESIAN_POINT('Ctrl Pts',(-7.05021164825251,-35.3742261150622,
1.16209544641768));
#50187=CARTESIAN_POINT('Ctrl Pts',(-7.05298995234368,-35.3742266401801,
1.18279723135034));
#50188=CARTESIAN_POINT('Ctrl Pts',(-7.05571064340917,-35.3742477797272,
1.20381716458915));
#50189=CARTESIAN_POINT('Ctrl Pts',(-7.05829605327761,-35.3742431701945,
1.22454392284656));
#50190=CARTESIAN_POINT('Ctrl Pts',(-7.0608927559198,-35.3742385405278,1.24536121320659));
#50191=CARTESIAN_POINT('Ctrl Pts',(-7.06339480482366,-35.3742375427218,
1.26620204691466));
#50192=CARTESIAN_POINT('Ctrl Pts',(-7.06580506972233,-35.3742369799112,
1.28708281574342));
#50193=CARTESIAN_POINT('Ctrl Pts',(-7.07061980686756,-35.3742358556427,
1.32879417010789));
#50194=CARTESIAN_POINT('Ctrl Pts',(-7.07505478224174,-35.3742356535494,
1.37055008889881));
#50195=CARTESIAN_POINT('Ctrl Pts',(-7.07911993306,-35.3742356128,1.41233341424));
#50196=CARTESIAN_POINT('Ctrl Pts',(-7.05021188141398,-35.3742261390046,
1.1620952532504));
#50197=CARTESIAN_POINT('Ctrl Pts',(-7.04352707146932,-35.381715700076,1.11228520069688));
#50198=CARTESIAN_POINT('Ctrl Pts',(-7.03635023271754,-35.3890407899385,
1.06303551389404));
#50199=CARTESIAN_POINT('Ctrl Pts',(-7.02867908891517,-35.3961811568166,
1.01427777377839));
#50200=CARTESIAN_POINT('Ctrl Pts',(-7.01997402407047,-35.404283906327,0.958948438242224));
#50201=CARTESIAN_POINT('Ctrl Pts',(-7.01063229140259,-35.4121485106884,
0.904253034225137));
#50202=CARTESIAN_POINT('Ctrl Pts',(-7.00066015753755,-35.4197633417748,
0.850158125696098));
#50203=CARTESIAN_POINT('Ctrl Pts',(-6.98968258670088,-35.4281459355899,
0.790609116595527));
#50204=CARTESIAN_POINT('Ctrl Pts',(-6.97794100473584,-35.4362257116211,
0.731789102718959));
#50205=CARTESIAN_POINT('Ctrl Pts',(-6.96545655070105,-35.4440111016219,
0.673714193997119));
#50206=CARTESIAN_POINT('Ctrl Pts',(-6.95155204539388,-35.4526820452036,
0.609033521996102));
#50207=CARTESIAN_POINT('Ctrl Pts',(-6.93672600539964,-35.4609877333797,
0.545278981739372));
#50208=CARTESIAN_POINT('Ctrl Pts',(-6.92102403957521,-35.4689702606657,
0.482517887121766));
#50209=CARTESIAN_POINT('Ctrl Pts',(-6.89588675441965,-35.4817494926992,
0.382043618503607));
#50210=CARTESIAN_POINT('Ctrl Pts',(-6.86846319411156,-35.4936186298441,
0.283938115251837));
#50211=CARTESIAN_POINT('Ctrl Pts',(-6.83883729901714,-35.5045777234444,
0.188140683587292));
#50212=CARTESIAN_POINT('Ctrl Pts',(-6.83670483057942,-35.5053665577103,
0.181245195745052));
#50213=CARTESIAN_POINT('Ctrl Pts',(-6.83456094047648,-35.5061506762736,
0.174361641847689));
#50214=CARTESIAN_POINT('Ctrl Pts',(-6.83240565405016,-35.5069300791112,
0.167489984676289));
#50215=CARTESIAN_POINT('Ctrl Pts',(-6.81635656074776,-35.5127338129942,
0.116320977281485));
#50216=CARTESIAN_POINT('Ctrl Pts',(-6.7996760330039,-35.518276096045,0.0658134591906613));
#50217=CARTESIAN_POINT('Ctrl Pts',(-6.78237703513777,-35.5235569279985,
0.0159579638384577));
#50218=CARTESIAN_POINT('Ctrl Pts',(-6.7737275362047,-35.5261973439752,-0.00896978383764373));
#50219=CARTESIAN_POINT('Ctrl Pts',(-6.76492343663421,-35.5287723971648,
-0.0337345291900959));
#50220=CARTESIAN_POINT('Ctrl Pts',(-6.75596652857811,-35.5312820875257,
-0.0583375110691009));
#50221=CARTESIAN_POINT('Ctrl Pts',(-6.75148807455006,-35.5325369327061,
-0.0706390020086038));
#50222=CARTESIAN_POINT('Ctrl Pts',(-6.74697142075146,-35.5337754371799,
-0.0829000529775413));
#50223=CARTESIAN_POINT('Ctrl Pts',(-6.74241680762996,-35.5349976009461,
-0.0951208255204967));
#50224=CARTESIAN_POINT('Ctrl Pts',(-6.73891429679059,-35.5359374484643,
-0.104518635423402));
#50225=CARTESIAN_POINT('Ctrl Pts',(-6.73570406504125,-35.5367853631935,
-0.113059445497894));
#50226=CARTESIAN_POINT('Ctrl Pts',(-6.73206100729518,-35.537731318041,-0.122665614285448));
#50227=CARTESIAN_POINT('Ctrl Pts',(-6.73096668680786,-35.5380154688401,
-0.125551164842593));
#50228=CARTESIAN_POINT('Ctrl Pts',(-6.72983298604664,-35.538308389363,-0.128532797850881));
#50229=CARTESIAN_POINT('Ctrl Pts',(-6.72863934124971,-35.538615014252,-0.131662481145629));
#50230=CARTESIAN_POINT('Ctrl Pts',(-6.7245761357129,-35.539658775302,-0.14231602441441));
#50231=CARTESIAN_POINT('Ctrl Pts',(-6.72047624723707,-35.5406929458301,
-0.152958731118445));
#50232=CARTESIAN_POINT('Ctrl Pts',(-6.71633948303299,-35.5417175400764,
-0.163590489490864));
#50233=CARTESIAN_POINT('Ctrl Pts',(-6.67755929772736,-35.5513226209492,
-0.263258137794542));
#50234=CARTESIAN_POINT('Ctrl Pts',(-6.63553882391724,-35.5600852051321,
-0.361959218829963));
#50235=CARTESIAN_POINT('Ctrl Pts',(-6.59009883490075,-35.5680052181569,
-0.459541970726329));
#50236=CARTESIAN_POINT('Ctrl Pts',(-6.54175602567053,-35.5764311814338,
-0.563358553018467));
#50237=CARTESIAN_POINT('Ctrl Pts',(-6.48954401475643,-35.5839042846034,
-0.665911252177743));
#50238=CARTESIAN_POINT('Ctrl Pts',(-6.43323009460924,-35.5904302877287,
-0.767062608930708));
#50239=CARTESIAN_POINT('Ctrl Pts',(-6.35567379192739,-35.5994179886802,
-0.906369643861105));
#50240=CARTESIAN_POINT('Ctrl Pts',(-6.2703500558032,-35.6066100934343,-1.04299798700632));
#50241=CARTESIAN_POINT('Ctrl Pts',(-6.17666402058228,-35.6119997299894,
-1.17652254193963));
#50242=CARTESIAN_POINT('Ctrl Pts',(-6.16625937752191,-35.6125982956609,
-1.19135159656446));
#50243=CARTESIAN_POINT('Ctrl Pts',(-6.15575156510111,-35.6131745884083,
-1.20614235116042));
#50244=CARTESIAN_POINT('Ctrl Pts',(-6.14513974492393,-35.6137285633824,
-1.22089421231661));
#50245=CARTESIAN_POINT('Ctrl Pts',(-6.12744585650583,-35.6146522476527,
-1.24549110341529));
#50246=CARTESIAN_POINT('Ctrl Pts',(-6.10918547518569,-35.6155271446915,
-1.27035748958776));
#50247=CARTESIAN_POINT('Ctrl Pts',(-6.09076485774616,-35.6163316064952,
-1.29492033009841));
#50248=CARTESIAN_POINT('Ctrl Pts',(-6.07234424030663,-35.6171360682989,
-1.31948317060907));
#50249=CARTESIAN_POINT('Ctrl Pts',(-6.05376357297037,-35.6178701284919,
-1.34374234998056));
#50250=CARTESIAN_POINT('Ctrl Pts',(-6.03547539301575,-35.6185238313854,
-1.3671556564777));
#50251=CARTESIAN_POINT('Ctrl Pts',(-5.96003196187137,-35.6212205234211,
-1.46374154862018));
#50252=CARTESIAN_POINT('Ctrl Pts',(-5.8806430282633,-35.6228887681904,-1.55747864373515));
#50253=CARTESIAN_POINT('Ctrl Pts',(-5.79732811347347,-35.6235530383653,
-1.64835399093985));
#50254=CARTESIAN_POINT('Ctrl Pts',(-5.71907262973099,-35.6241769696747,
-1.7337107877836));
#50255=CARTESIAN_POINT('Ctrl Pts',(-5.63735326506376,-35.6239144984006,
-1.81654508341693));
#50256=CARTESIAN_POINT('Ctrl Pts',(-5.55216217707629,-35.6227748437847,
-1.89687171823991));
#50257=CARTESIAN_POINT('Ctrl Pts',(-5.43288206744175,-35.6211791589456,
-2.00934087475155));
#50258=CARTESIAN_POINT('Ctrl Pts',(-5.30680750719591,-35.6178655165706,
-2.11688217438336));
#50259=CARTESIAN_POINT('Ctrl Pts',(-5.17395137625618,-35.6128041649775,
-2.21950506889937));
#50260=CARTESIAN_POINT('Ctrl Pts',(-5.13538698860863,-35.6113349973638,
-2.24929360073177));
#50261=CARTESIAN_POINT('Ctrl Pts',(-5.09625123076711,-35.609718224167,-2.27866769919633));
#50262=CARTESIAN_POINT('Ctrl Pts',(-5.05654447604708,-35.6079523441408,
-2.30762755684394));
#50263=CARTESIAN_POINT('Ctrl Pts',(-5.04054291620784,-35.6072407061561,
-2.31929818815974));
#50264=CARTESIAN_POINT('Ctrl Pts',(-5.02394560548748,-35.6064813720674,
-2.33126302911098));
#50265=CARTESIAN_POINT('Ctrl Pts',(-5.00770854202776,-35.6057181156694,
-2.34283175821588));
#50266=CARTESIAN_POINT('Ctrl Pts',(-4.9983604602823,-35.6052786899556,-2.34949216362922));
#50267=CARTESIAN_POINT('Ctrl Pts',(-4.98913243268586,-35.6048381769909,
-2.35602204061313));
#50268=CARTESIAN_POINT('Ctrl Pts',(-4.98021172600241,-35.6044065601333,
-2.36229557116517));
#50269=CARTESIAN_POINT('Ctrl Pts',(-4.83811928258686,-35.5975316009961,
-2.46222277610684));
#50270=CARTESIAN_POINT('Ctrl Pts',(-4.6899512138041,-35.5888504066531,-2.55634922532136));
#50271=CARTESIAN_POINT('Ctrl Pts',(-4.53605954555446,-35.5783538872027,
-2.64486936122386));
#50272=CARTESIAN_POINT('Ctrl Pts',(-4.40146233214111,-35.5691733884491,
-2.72229112004266));
#50273=CARTESIAN_POINT('Ctrl Pts',(-4.2624871398174,-35.558602765964,-2.79542528542047));
#50274=CARTESIAN_POINT('Ctrl Pts',(-4.11934100470481,-35.5466380561341,
-2.86442049917059));
#50275=CARTESIAN_POINT('Ctrl Pts',(-3.99031460571353,-35.5358535286782,
-2.92661012078217));
#50276=CARTESIAN_POINT('Ctrl Pts',(-3.85790038353982,-35.5239354720522,
-2.98543736793842));
#50277=CARTESIAN_POINT('Ctrl Pts',(-3.7222163946605,-35.5108977782426,-3.04101944174927));
#50278=CARTESIAN_POINT('Ctrl Pts',(-3.70736809901062,-35.5094710252861,
-3.04710195061117));
#50279=CARTESIAN_POINT('Ctrl Pts',(-3.6924806009018,-35.5080308900275,-3.0531456031268));
#50280=CARTESIAN_POINT('Ctrl Pts',(-3.67755401867,-35.5065774118,-3.05915055738));
#50281=CARTESIAN_POINT('Ctrl Pts',(-7.21384189759,-36.3742356128,2.18958432614));
#50282=CARTESIAN_POINT('Ctrl Pts',(-7.21384189759,-35.1742356128,2.18958432614));
#50283=CARTESIAN_POINT('Ctrl Pts',(-7.13908599018,-36.3742356128,2.05065155888));
#50284=CARTESIAN_POINT('Ctrl Pts',(-7.13908599018,-35.1742356128,2.05065155888));
#50285=CARTESIAN_POINT('Ctrl Pts',(-7.08904524264,-36.3742356128,1.89842024269));
#50286=CARTESIAN_POINT('Ctrl Pts',(-7.08904524264,-35.1742356128,1.89842024269));
#50287=CARTESIAN_POINT('Ctrl Pts',(-7.10533215541,-36.3742356128,1.72680915639));
#50288=CARTESIAN_POINT('Ctrl Pts',(-7.10533215541,-35.1742356128,1.72680915639));
#50289=CARTESIAN_POINT('Ctrl Pts',(-7.09439724612,-36.3742356128,1.56936004643));
#50290=CARTESIAN_POINT('Ctrl Pts',(-7.09439724612,-35.1742356128,1.56936004643));
#50291=CARTESIAN_POINT('Ctrl Pts',(-7.07911993306,-36.3742356128,1.41233341424));
#50292=CARTESIAN_POINT('Ctrl Pts',(-7.07911993306,-35.1742356128,1.41233341424));
#50293=CARTESIAN_POINT('',(-7.21384189758587,-35.4651148398172,2.18958432618295));
#50294=CARTESIAN_POINT('',(-7.21384189758,-36.1242356128,2.18958432614));
#50295=CARTESIAN_POINT('',(-7.13973478936,-35.3742392475,2.00655473738));
#50296=CARTESIAN_POINT('Ctrl Pts',(-7.21384189753719,-35.4651148399882,
2.18958432613386));
#50297=CARTESIAN_POINT('Ctrl Pts',(-7.20248970613278,-35.4558376974756,
2.16852385251479));
#50298=CARTESIAN_POINT('Ctrl Pts',(-7.19216154693066,-35.4455454559845,
2.14764262491228));
#50299=CARTESIAN_POINT('Ctrl Pts',(-7.18277070551959,-35.4348282932108,
2.12663643240788));
#50300=CARTESIAN_POINT('Ctrl Pts',(-7.17770336699823,-35.4290452659627,
2.11530140034788));
#50301=CARTESIAN_POINT('Ctrl Pts',(-7.17290922444295,-35.4231375971478,
2.10393011825159));
#50302=CARTESIAN_POINT('Ctrl Pts',(-7.16837646591434,-35.4171920851989,
2.09247569166461));
#50303=CARTESIAN_POINT('Ctrl Pts',(-7.15869260576572,-35.404489995321,2.06800426561123));
#50304=CARTESIAN_POINT('Ctrl Pts',(-7.15020429789435,-35.3915941161304,
2.04315346963811));
#50305=CARTESIAN_POINT('Ctrl Pts',(-7.14282824899172,-35.3794131715241,
2.01756660856243));
#50306=CARTESIAN_POINT('Ctrl Pts',(-7.14201563347066,-35.37807120311,2.01474771721293));
#50307=CARTESIAN_POINT('Ctrl Pts',(-7.14121690146011,-35.376735446728,2.01192135159036));
#50308=CARTESIAN_POINT('Ctrl Pts',(-7.1404309617392,-35.3754137600701,2.0090835975648));
#50309=CARTESIAN_POINT('Ctrl Pts',(-7.1401977511474,-35.375021578177,2.00824155551238));
#50310=CARTESIAN_POINT('Ctrl Pts',(-7.13996568730528,-35.3746302925694,
2.00739857926709));
#50311=CARTESIAN_POINT('Ctrl Pts',(-7.13973478936,-35.3742392475,2.00655473738));
#50312=CARTESIAN_POINT('Ctrl Pts',(-7.07911993306,-35.3742356128,1.41233341424));
#50313=CARTESIAN_POINT('Ctrl Pts',(-7.08088379359945,-35.3742356128,1.43046208289635));
#50314=CARTESIAN_POINT('Ctrl Pts',(-7.08257391393288,-35.3742355920726,
1.44859911701878));
#50315=CARTESIAN_POINT('Ctrl Pts',(-7.08413990039285,-35.3742355563689,
1.46677978317039));
#50316=CARTESIAN_POINT('Ctrl Pts',(-7.08577195894419,-35.3742355191587,
1.4857275278798));
#50317=CARTESIAN_POINT('Ctrl Pts',(-7.08726945163803,-35.3742354656818,
1.5047225982671));
#50318=CARTESIAN_POINT('Ctrl Pts',(-7.0886278899404,-35.3742354024484,1.52378297170902));
#50319=CARTESIAN_POINT('Ctrl Pts',(-7.09010880652101,-35.3742353335138,
1.54456184919918));
#50320=CARTESIAN_POINT('Ctrl Pts',(-7.09142454145993,-35.3742352529839,
1.56541838105054));
#50321=CARTESIAN_POINT('Ctrl Pts',(-7.09262835646224,-35.3742351692935,
1.58635022088169));
#50322=CARTESIAN_POINT('Ctrl Pts',(-7.09392979130774,-35.3742350788165,
1.60897946680765));
#50323=CARTESIAN_POINT('Ctrl Pts',(-7.0951009883527,-35.3742349846456,1.63169662188994));
#50324=CARTESIAN_POINT('Ctrl Pts',(-7.09627031081483,-35.3742348974381,
1.6544704621937));
#50325=CARTESIAN_POINT('Ctrl Pts',(-7.09759721920297,-35.3742347984779,
1.68031346162976));
#50326=CARTESIAN_POINT('Ctrl Pts',(-7.09892280102883,-35.3742347084847,
1.70622930734005));
#50327=CARTESIAN_POINT('Ctrl Pts',(-7.10049797330169,-35.3742346430313,
1.73213889512276));
#50328=CARTESIAN_POINT('Ctrl Pts',(-7.10268355309506,-35.3742345522136,
1.76808891309122));
#50329=CARTESIAN_POINT('Ctrl Pts',(-7.10535563162135,-35.3742345086403,
1.80402663897013));
#50330=CARTESIAN_POINT('Ctrl Pts',(-7.10925382044981,-35.374234553911,1.8396775575811));
#50331=CARTESIAN_POINT('Ctrl Pts',(-7.11201818443917,-35.3742345860143,
1.86495907162076));
#50332=CARTESIAN_POINT('Ctrl Pts',(-7.1154016075227,-35.3742346627955,1.890094551153));
#50333=CARTESIAN_POINT('Ctrl Pts',(-7.11963758304941,-35.3742347990895,
1.91498267217685));
#50334=CARTESIAN_POINT('Ctrl Pts',(-7.12328042918288,-35.3742349162994,
1.93638591090411));
#50335=CARTESIAN_POINT('Ctrl Pts',(-7.12755425624875,-35.3742350775228,
1.95760586665248));
#50336=CARTESIAN_POINT('Ctrl Pts',(-7.13256782595468,-35.3742352921948,
1.97858502103487));
#50337=CARTESIAN_POINT('Ctrl Pts',(-7.13480768313778,-35.3742353881014,
1.98795764620913));
#50338=CARTESIAN_POINT('Ctrl Pts',(-7.13719457595265,-35.3742354946761,
1.99728233675654));
#50339=CARTESIAN_POINT('Ctrl Pts',(-7.13973478937384,-35.37423561276,2.00655473739936));
#50340=CARTESIAN_POINT('Ctrl Pts',(-8.75956299024,-36.3742356128,2.0634404101));
#50341=CARTESIAN_POINT('Ctrl Pts',(-8.75956299024,-35.2767450158758,2.0634404101));
#50342=CARTESIAN_POINT('Ctrl Pts',(-8.72637376563,-36.3742356128,2.11781888978));
#50343=CARTESIAN_POINT('Ctrl Pts',(-8.72637376563,-35.2767450158758,2.11781888978));
#50344=CARTESIAN_POINT('Ctrl Pts',(-8.6915484,-36.3742356128,2.17268982337));
#50345=CARTESIAN_POINT('Ctrl Pts',(-8.6915484,-35.2767450158758,2.17268982337));
#50346=CARTESIAN_POINT('Ctrl Pts',(-8.65506636668,-36.3742356128,2.22762960985));
#50347=CARTESIAN_POINT('Ctrl Pts',(-8.65506636668,-35.2767450158758,2.22762960985));
#50348=CARTESIAN_POINT('Ctrl Pts',(-8.53055023262,-36.3742356128,2.40503324452));
#50349=CARTESIAN_POINT('Ctrl Pts',(-8.53055023262,-35.2767450158758,2.40503324452));
#50350=CARTESIAN_POINT('Ctrl Pts',(-8.3876008666,-36.3742356128,2.56660232663));
#50351=CARTESIAN_POINT('Ctrl Pts',(-8.3876008666,-35.2767450158758,2.56660232663));
#50352=CARTESIAN_POINT('Ctrl Pts',(-8.27908544119,-36.3742356128,2.66027026629));
#50353=CARTESIAN_POINT('Ctrl Pts',(-8.27908544119,-35.2767450158758,2.66027026629));
#50354=CARTESIAN_POINT('Ctrl Pts',(-8.01327762974,-36.3742356128,2.78696551824));
#50355=CARTESIAN_POINT('Ctrl Pts',(-8.01327762974,-35.2767450158758,2.78696551824));
#50356=CARTESIAN_POINT('Ctrl Pts',(-7.71906576509,-36.3742356128,2.71717075777));
#50357=CARTESIAN_POINT('Ctrl Pts',(-7.71906576509,-35.2767450158758,2.71717075777));
#50358=CARTESIAN_POINT('Ctrl Pts',(-7.55641153588,-36.3742356128,2.61428156978));
#50359=CARTESIAN_POINT('Ctrl Pts',(-7.55641153588,-35.2767450158758,2.61428156978));
#50360=CARTESIAN_POINT('Ctrl Pts',(-7.38865661676,-36.3742356128,2.45617777771));
#50361=CARTESIAN_POINT('Ctrl Pts',(-7.38865661676,-35.2767450158758,2.45617777771));
#50362=CARTESIAN_POINT('Ctrl Pts',(-7.26550535688,-36.3742356128,2.27753774962));
#50363=CARTESIAN_POINT('Ctrl Pts',(-7.26550535688,-35.2767450158758,2.27753774962));
#50364=CARTESIAN_POINT('Ctrl Pts',(-7.24701042964,-36.3742356128,2.24853650952));
#50365=CARTESIAN_POINT('Ctrl Pts',(-7.24701042964,-35.2767450158758,2.24853650952));
#50366=CARTESIAN_POINT('Ctrl Pts',(-7.2297761181,-36.3742356128,2.21919784335));
#50367=CARTESIAN_POINT('Ctrl Pts',(-7.2297761181,-35.2767450158758,2.21919784335));
#50368=CARTESIAN_POINT('Ctrl Pts',(-7.21384189758,-36.3742356128,2.18958432613));
#50369=CARTESIAN_POINT('Ctrl Pts',(-7.21384189758,-35.2767450158758,2.18958432613));
#50370=CARTESIAN_POINT('',(-8.75956299007003,-35.6438772168026,2.06344041036242));
#50371=CARTESIAN_POINT('',(-8.75956299023,-36.1242356128,2.0634404101));
#50372=CARTESIAN_POINT('',(-8.73000675245248,-35.6496340209958,2.1111701504857));
#50373=CARTESIAN_POINT('Origin',(-8.8025233360182,-35.5994617475288,1.55277754717549));
#50374=CARTESIAN_POINT('',(-8.49626470339955,-35.699502272635,2.43550539329785));
#50375=CARTESIAN_POINT('Ctrl Pts',(-8.73000528472,-35.6496341999,2.11117245845));
#50376=CARTESIAN_POINT('Ctrl Pts',(-8.71278579373065,-35.6529734545507,
2.13857243132976));
#50377=CARTESIAN_POINT('Ctrl Pts',(-8.69523611065439,-35.656418433528,2.16578280028398));
#50378=CARTESIAN_POINT('Ctrl Pts',(-8.67736328843596,-35.6599993397373,
2.19267530487441));
#50379=CARTESIAN_POINT('Ctrl Pts',(-8.65990881423403,-35.6634964279019,
2.21893833831492));
#50380=CARTESIAN_POINT('Ctrl Pts',(-8.64214969971165,-35.6671228124049,
2.24489443760551));
#50381=CARTESIAN_POINT('Ctrl Pts',(-8.6240892075043,-35.6709094567015,2.27040574861869));
#50382=CARTESIAN_POINT('Ctrl Pts',(-8.60885152877019,-35.6741042571869,
2.29192970028301));
#50383=CARTESIAN_POINT('Ctrl Pts',(-8.59340033381773,-35.6774130775882,
2.31313561363373));
#50384=CARTESIAN_POINT('Ctrl Pts',(-8.57770836660362,-35.6808587827496,
2.33395912375569));
#50385=CARTESIAN_POINT('Ctrl Pts',(-8.57480139519109,-35.6814971072033,
2.33781672476946));
#50386=CARTESIAN_POINT('Ctrl Pts',(-8.57188604813872,-35.6821401439685,
2.3416612893117));
#50387=CARTESIAN_POINT('Ctrl Pts',(-8.56896198405368,-35.6827880598152,
2.34549254173609));
#50388=CARTESIAN_POINT('Ctrl Pts',(-8.56143090936174,-35.6844567997929,
2.35536012580152));
#50389=CARTESIAN_POINT('Ctrl Pts',(-8.55384786331649,-35.6861566070827,
2.36513232166256));
#50390=CARTESIAN_POINT('Ctrl Pts',(-8.54621303383084,-35.6878884842043,
2.37479733602594));
#50391=CARTESIAN_POINT('Ctrl Pts',(-8.53873858847129,-35.6895839799504,
2.38425931836546));
#50392=CARTESIAN_POINT('Ctrl Pts',(-8.53121142039016,-35.6913109462438,
2.39362216719067));
#50393=CARTESIAN_POINT('Ctrl Pts',(-8.52362054975123,-35.6930722906216,
2.40288673572145));
#50394=CARTESIAN_POINT('Ctrl Pts',(-8.51695920442706,-35.6946179529959,
2.41101682951418));
#50395=CARTESIAN_POINT('Ctrl Pts',(-8.51024738112154,-35.6961904182621,
2.41907287662946));
#50396=CARTESIAN_POINT('Ctrl Pts',(-8.50349797791776,-35.6977863767698,
2.42703115952841));
#50397=CARTESIAN_POINT('Ctrl Pts',(-8.50255616499077,-35.6980090771046,
2.42814165974369));
#50398=CARTESIAN_POINT('Ctrl Pts',(-8.50161367399323,-35.6982322214535,
2.42925019294274));
#50399=CARTESIAN_POINT('Ctrl Pts',(-8.50067059768458,-35.6984557864418,
2.43035662659535));
#50400=CARTESIAN_POINT('Ctrl Pts',(-8.49920411912565,-35.6988034287893,
2.43207712494054));
#50401=CARTESIAN_POINT('Ctrl Pts',(-8.49773226797996,-35.6991530223845,
2.43379716100814));
#50402=CARTESIAN_POINT('Ctrl Pts',(-8.49626469608749,-35.6995022721787,
2.43550538236112));
#50403=CARTESIAN_POINT('',(-7.23334333080301,-35.4800020975,2.22433302562685));
#50404=CARTESIAN_POINT('Ctrl Pts',(-8.49626470705517,-35.699502273,2.43550539876585));
#50405=CARTESIAN_POINT('Ctrl Pts',(-8.48478738974076,-35.7022336299315,
2.44886473885747));
#50406=CARTESIAN_POINT('Ctrl Pts',(-8.47349630523902,-35.7048385205551,
2.46159463232704));
#50407=CARTESIAN_POINT('Ctrl Pts',(-8.46237222531038,-35.707344358481,2.4737420925269));
#50408=CARTESIAN_POINT('Ctrl Pts',(-8.44944563624108,-35.7102562341012,
2.48785788702376));
#50409=CARTESIAN_POINT('Ctrl Pts',(-8.43674458927482,-35.7130334581298,
2.50118599352194));
#50410=CARTESIAN_POINT('Ctrl Pts',(-8.42428045772585,-35.7156815003471,
2.51375562733581));
#50411=CARTESIAN_POINT('Ctrl Pts',(-8.40827473989147,-35.7190819632174,
2.52989682508521));
#50412=CARTESIAN_POINT('Ctrl Pts',(-8.39265963522996,-35.7222671863208,
2.54478430272951));
#50413=CARTESIAN_POINT('Ctrl Pts',(-8.37752566693042,-35.7252176514594,
2.55844769532221));
#50414=CARTESIAN_POINT('Ctrl Pts',(-8.36221547823891,-35.7282024719047,
2.57227018487816));
#50415=CARTESIAN_POINT('Ctrl Pts',(-8.34740012240277,-35.7309447120799,
2.58483721748327));
#50416=CARTESIAN_POINT('Ctrl Pts',(-8.33320903630987,-35.7334376491566,
2.59620216330057));
#50417=CARTESIAN_POINT('Ctrl Pts',(-8.33095938864949,-35.7338328430147,
2.59800379593114));
#50418=CARTESIAN_POINT('Ctrl Pts',(-8.32872546097848,-35.7342218324706,
2.59977530309741));
#50419=CARTESIAN_POINT('Ctrl Pts',(-8.32650779509264,-35.7346046636448,
2.60151699533483));
#50420=CARTESIAN_POINT('Ctrl Pts',(-8.31036047399732,-35.7373921430097,
2.61419864588754));
#50421=CARTESIAN_POINT('Ctrl Pts',(-8.29499932423798,-35.7398659334796,
2.62535730899568));
#50422=CARTESIAN_POINT('Ctrl Pts',(-8.28052173447358,-35.742015932203,2.63519468961952));
#50423=CARTESIAN_POINT('Ctrl Pts',(-8.27333546216802,-35.7430831316841,
2.64007769135439));
#50424=CARTESIAN_POINT('Ctrl Pts',(-8.26636661759111,-35.7440712201303,
2.64463574972307));
#50425=CARTESIAN_POINT('Ctrl Pts',(-8.25962499438878,-35.7449822598253,
2.64889600990654));
#50426=CARTESIAN_POINT('Ctrl Pts',(-8.25889069886849,-35.745081489988,2.64936003613199));
#50427=CARTESIAN_POINT('Ctrl Pts',(-8.25815909729571,-35.7451798077242,
2.64982053030333));
#50428=CARTESIAN_POINT('Ctrl Pts',(-8.25743019202015,-35.7452772092317,
2.65027752888441));
#50429=CARTESIAN_POINT('Ctrl Pts',(-8.24697862589458,-35.7466738218366,
2.65683030199446));
#50430=CARTESIAN_POINT('Ctrl Pts',(-8.23708400295828,-35.747879361664,2.66266250084632));
#50431=CARTESIAN_POINT('Ctrl Pts',(-8.22777710389026,-35.74889382729,2.66786953541919));
#50432=CARTESIAN_POINT('Ctrl Pts',(-8.22312365435624,-35.7494010601031,
2.67047305270562));
#50433=CARTESIAN_POINT('Ctrl Pts',(-8.21861717004876,-35.7498605244786,
2.67292030448637));
#50434=CARTESIAN_POINT('Ctrl Pts',(-8.21426118604618,-35.750272220593,2.67522322539416));
#50435=CARTESIAN_POINT('Ctrl Pts',(-8.21208319404489,-35.7504780686502,
2.67637468584805));
#50436=CARTESIAN_POINT('Ctrl Pts',(-8.20994282504322,-35.7506719746426,
2.67749005947097));
#50437=CARTESIAN_POINT('Ctrl Pts',(-8.20784050698368,-35.7508539385916,
2.67857080521581));
#50438=CARTESIAN_POINT('Ctrl Pts',(-8.20650579572473,-35.7509694631337,
2.6792569447403));
#50439=CARTESIAN_POINT('Ctrl Pts',(-8.20582892443352,-35.7510274346216,
2.67960206025779));
#50440=CARTESIAN_POINT('Ctrl Pts',(-8.20458681491374,-35.7511290070974,
2.6802314134196));
#50441=CARTESIAN_POINT('Ctrl Pts',(-8.20387246436933,-35.7511874225207,
2.680593361192));
#50442=CARTESIAN_POINT('Ctrl Pts',(-8.20297109329813,-35.7512601548331,
2.68104909082734));
#50443=CARTESIAN_POINT('Ctrl Pts',(-8.20164809435695,-35.7513630392347,
2.68171060399119));
#50444=CARTESIAN_POINT('Ctrl Pts',(-8.18485787866432,-35.7526687479855,
2.69010588561904));
#50445=CARTESIAN_POINT('Ctrl Pts',(-8.16817698260155,-35.7535209183249,
2.69748506803798));
#50446=CARTESIAN_POINT('Ctrl Pts',(-8.15163776364548,-35.7538884883522,
2.70389891515113));
#50447=CARTESIAN_POINT('Ctrl Pts',(-8.13962292624303,-35.7541555078605,
2.70855822405763));
#50448=CARTESIAN_POINT('Ctrl Pts',(-8.12768358697008,-35.7541679447663,
2.71270833239839));
#50449=CARTESIAN_POINT('Ctrl Pts',(-8.11583718940693,-35.7539295817332,
2.71637303718402));
#50450=CARTESIAN_POINT('Ctrl Pts',(-8.1017603154413,-35.7536463389703,2.7207277439304));
#50451=CARTESIAN_POINT('Ctrl Pts',(-8.08781260069513,-35.7529999537971,
2.72439784378331));
#50452=CARTESIAN_POINT('Ctrl Pts',(-8.07401645344997,-35.7520148983668,
2.72743067381259));
#50453=CARTESIAN_POINT('Ctrl Pts',(-8.06812797876998,-35.7515944567857,
2.72872514700998));
#50454=CARTESIAN_POINT('Ctrl Pts',(-8.06203309974918,-35.7510936806319,
2.72995126932923));
#50455=CARTESIAN_POINT('Ctrl Pts',(-8.05603177437216,-35.7505342564226,
2.73104354710272));
#50456=CARTESIAN_POINT('Ctrl Pts',(-8.04981368520668,-35.7499546261916,
2.73217527720604));
#50457=CARTESIAN_POINT('Ctrl Pts',(-8.04369619708462,-35.7493120766649,
2.73316328375298));
#50458=CARTESIAN_POINT('Ctrl Pts',(-8.03801937794833,-35.7486606699676,
2.73398364682132));
#50459=CARTESIAN_POINT('Ctrl Pts',(-8.03633851273534,-35.7484677931415,
2.73422655041055));
#50460=CARTESIAN_POINT('Ctrl Pts',(-8.03469631248028,-35.7482743247953,
2.73445506571509));
#50461=CARTESIAN_POINT('Ctrl Pts',(-8.03310166808097,-35.7480820929171,
2.73466929183492));
#50462=CARTESIAN_POINT('Ctrl Pts',(-8.01904331881673,-35.7463873809903,
2.73655790450332));
#50463=CARTESIAN_POINT('Ctrl Pts',(-8.00417431429791,-35.7442048206208,
2.73794428304994));
#50464=CARTESIAN_POINT('Ctrl Pts',(-7.98849033151252,-35.7414881426324,
2.73862510052901));
#50465=CARTESIAN_POINT('Ctrl Pts',(-7.97700158377802,-35.7394981361073,
2.73912380933132));
#50466=CARTESIAN_POINT('Ctrl Pts',(-7.96507585493778,-35.7372214968454,
2.739243343789));
#50467=CARTESIAN_POINT('Ctrl Pts',(-7.95271576416055,-35.73465776535,2.73890188665224));
#50468=CARTESIAN_POINT('Ctrl Pts',(-7.93982887381466,-35.7319847650257,
2.738545876267));
#50469=CARTESIAN_POINT('Ctrl Pts',(-7.92646901975442,-35.7290141149945,
2.73768804175695));
#50470=CARTESIAN_POINT('Ctrl Pts',(-7.91264398168322,-35.7257422917824,
2.7362414335458));
#50471=CARTESIAN_POINT('Ctrl Pts',(-7.91078813887005,-35.7253030894046,
2.73604724402977));
#50472=CARTESIAN_POINT('Ctrl Pts',(-7.90892391692481,-35.7248585353482,
2.73584246338455));
#50473=CARTESIAN_POINT('Ctrl Pts',(-7.90705133663703,-35.7244086969031,
2.73562690117746));
#50474=CARTESIAN_POINT('Ctrl Pts',(-7.90169678951765,-35.723122406982,2.73501051212189));
#50475=CARTESIAN_POINT('Ctrl Pts',(-7.89627373543874,-35.7217919098803,
2.73430590796455));
#50476=CARTESIAN_POINT('Ctrl Pts',(-7.89078303968402,-35.7204175849161,
2.73350900493847));
#50477=CARTESIAN_POINT('Ctrl Pts',(-7.8881614288968,-35.7197613939136,2.73312851225359));
#50478=CARTESIAN_POINT('Ctrl Pts',(-7.88552439629046,-35.7190952432039,
2.7327269889564));
#50479=CARTESIAN_POINT('Ctrl Pts',(-7.88287195037857,-35.7184189512514,
2.73230381816035));
#50480=CARTESIAN_POINT('Ctrl Pts',(-7.87876808903727,-35.7173725931006,
2.7316490887791));
#50481=CARTESIAN_POINT('Ctrl Pts',(-7.87462744214398,-35.7163022013537,
2.73094255475833));
#50482=CARTESIAN_POINT('Ctrl Pts',(-7.87045039924609,-35.715207775882,2.73018200139144));
#50483=CARTESIAN_POINT('Ctrl Pts',(-7.86836187779715,-35.7146605631461,
2.72980172470799));
#50484=CARTESIAN_POINT('Ctrl Pts',(-7.86626425749866,-35.7141073419777,
2.7294079434931));
#50485=CARTESIAN_POINT('Ctrl Pts',(-7.86415759379027,-35.7135481123587,
2.72900038410796));
#50486=CARTESIAN_POINT('Ctrl Pts',(-7.86263403344017,-35.7131436718821,
2.7287056330677));
#50487=CARTESIAN_POINT('Ctrl Pts',(-7.86043402929441,-35.7125561966667,
2.72826931136775));
#50488=CARTESIAN_POINT('Ctrl Pts',(-7.85901499360382,-35.7121757253659,
2.72798160782829));
#50489=CARTESIAN_POINT('Ctrl Pts',(-7.85847189435825,-35.7120301098062,
2.72787149673223));
#50490=CARTESIAN_POINT('Ctrl Pts',(-7.85804317970972,-35.7119149484461,
2.72778377381318));
#50491=CARTESIAN_POINT('Ctrl Pts',(-7.85781053033946,-35.7118523981339,
2.72773609981549));
#50492=CARTESIAN_POINT('Ctrl Pts',(-7.84994145632762,-35.7097367120469,
2.72612358646172));
#50493=CARTESIAN_POINT('Ctrl Pts',(-7.84068239994918,-35.7072048188565,
2.72406334905565));
#50494=CARTESIAN_POINT('Ctrl Pts',(-7.83005001361465,-35.7042419520675,
2.72135502913469));
#50495=CARTESIAN_POINT('Ctrl Pts',(-7.81915993834101,-35.7012072765635,
2.7185810697547));
#50496=CARTESIAN_POINT('Ctrl Pts',(-7.80682873097179,-35.6977199958601,
2.71512684077666));
#50497=CARTESIAN_POINT('Ctrl Pts',(-7.79308077972864,-35.6937771023739,
2.71072322623729));
#50498=CARTESIAN_POINT('Ctrl Pts',(-7.77861281360236,-35.6896277096106,
2.70608898329724));
#50499=CARTESIAN_POINT('Ctrl Pts',(-7.76257469854674,-35.6849738906446,
2.70040264847822));
#50500=CARTESIAN_POINT('Ctrl Pts',(-7.74501367358198,-35.6798298211235,
2.6932991938513));
#50501=CARTESIAN_POINT('Ctrl Pts',(-7.73986644545326,-35.6783220674823,
2.69121713420272));
#50502=CARTESIAN_POINT('Ctrl Pts',(-7.73458856949642,-35.6767722872443,
2.68901304949919));
#50503=CARTESIAN_POINT('Ctrl Pts',(-7.72918178710914,-35.675180990914,2.68667714192434));
#50504=CARTESIAN_POINT('Ctrl Pts',(-7.71231260111563,-35.6702161390217,
2.67938909951367));
#50505=CARTESIAN_POINT('Ctrl Pts',(-7.69419464788743,-35.6648336045937,
2.67082125009322));
#50506=CARTESIAN_POINT('Ctrl Pts',(-7.67493810743223,-35.6590387042651,
2.66069067140836));
#50507=CARTESIAN_POINT('Ctrl Pts',(-7.66080762111701,-35.6547863952909,
2.65325683334151));
#50508=CARTESIAN_POINT('Ctrl Pts',(-7.64606456718289,-35.6503122888981,
2.64498127475074));
#50509=CARTESIAN_POINT('Ctrl Pts',(-7.63076909921078,-35.6456126593791,
2.63575755957871));
#50510=CARTESIAN_POINT('Ctrl Pts',(-7.61363620758056,-35.6403484697904,
2.62542581211217));
#50511=CARTESIAN_POINT('Ctrl Pts',(-7.59581096096198,-35.6348035164443,
2.61390435324381));
#50512=CARTESIAN_POINT('Ctrl Pts',(-7.5774141102286,-35.6289786177062,2.60106619052009));
#50513=CARTESIAN_POINT('Ctrl Pts',(-7.57640807967092,-35.6286600835065,
2.60036413644617));
#50514=CARTESIAN_POINT('Ctrl Pts',(-7.57540034858448,-35.6283407047128,
2.59965815139513));
#50515=CARTESIAN_POINT('Ctrl Pts',(-7.57439093986371,-35.6280204787728,
2.59894821699336));
#50516=CARTESIAN_POINT('Ctrl Pts',(-7.56465692262456,-35.6249324483681,
2.59210211633733));
#50517=CARTESIAN_POINT('Ctrl Pts',(-7.55476669689201,-35.6217664170923,
2.58488857366488));
#50518=CARTESIAN_POINT('Ctrl Pts',(-7.54474277191305,-35.6185223831134,
2.57729276601061));
#50519=CARTESIAN_POINT('Ctrl Pts',(-7.53973080942357,-35.6169003661239,
2.57349486218347));
#50520=CARTESIAN_POINT('Ctrl Pts',(-7.53468542030573,-35.6152588484409,
2.56960139494148));
#50521=CARTESIAN_POINT('Ctrl Pts',(-7.52960981050698,-35.6135978298282,
2.56561085056718));
#50522=CARTESIAN_POINT('Ctrl Pts',(-7.52618192995733,-35.6124760388276,
2.56291578337612));
#50523=CARTESIAN_POINT('Ctrl Pts',(-7.52233273639884,-35.6112115631965,
2.55985046954054));
#50524=CARTESIAN_POINT('Ctrl Pts',(-7.51888963042791,-35.6100752410138,
2.55707291744137));
#50525=CARTESIAN_POINT('Ctrl Pts',(-7.51723458255391,-35.6095290284869,
2.55573779103647));
#50526=CARTESIAN_POINT('Ctrl Pts',(-7.51567307453838,-35.6090125180102,
2.55446999111925));
#50527=CARTESIAN_POINT('Ctrl Pts',(-7.51429555183542,-35.6085562709412,
2.55334652921959));
#50528=CARTESIAN_POINT('Ctrl Pts',(-7.49347539579041,-35.6016604606929,
2.53636629941192));
#50529=CARTESIAN_POINT('Ctrl Pts',(-7.47369655728357,-35.5948224054086,
2.51897852016351));
#50530=CARTESIAN_POINT('Ctrl Pts',(-7.45495956403958,-35.5880314450045,
2.50143384534816));
#50531=CARTESIAN_POINT('Ctrl Pts',(-7.43600847283916,-35.581162887799,2.48368869658401));
#50532=CARTESIAN_POINT('Ctrl Pts',(-7.41812311910607,-35.5743420635078,
2.46578288578056));
#50533=CARTESIAN_POINT('Ctrl Pts',(-7.40128135426698,-35.5675671484218,
2.44792790971538));
#50534=CARTESIAN_POINT('Ctrl Pts',(-7.38389671326328,-35.560573851239,2.42949739771213));
#50535=CARTESIAN_POINT('Ctrl Pts',(-7.36762388066498,-35.5536294822877,
2.41112096378186));
#50536=CARTESIAN_POINT('Ctrl Pts',(-7.35241586795669,-35.5467450555932,
2.39298218315277));
#50537=CARTESIAN_POINT('Ctrl Pts',(-7.3494232602091,-35.5453903494222,2.3894128637102));
#50538=CARTESIAN_POINT('Ctrl Pts',(-7.34647182064179,-35.5440380011469,
2.38585260191175));
#50539=CARTESIAN_POINT('Ctrl Pts',(-7.34356110202383,-35.5426881450861,
2.38230258867009));
#50540=CARTESIAN_POINT('Ctrl Pts',(-7.32870011786219,-35.5357963110845,
2.36417761766375));
#50541=CARTESIAN_POINT('Ctrl Pts',(-7.31489650839871,-35.5289775157615,
2.34631671551307));
#50542=CARTESIAN_POINT('Ctrl Pts',(-7.30207897807166,-35.5222043598003,
2.32884768056689));
#50543=CARTESIAN_POINT('Ctrl Pts',(-7.28834454310235,-35.514946684748,2.31012899464824));
#50544=CARTESIAN_POINT('Ctrl Pts',(-7.27574201356474,-35.5077416746932,
2.29186029304521));
#50545=CARTESIAN_POINT('Ctrl Pts',(-7.26416802488409,-35.5005907838209,
2.27414872095136));
#50546=CARTESIAN_POINT('Ctrl Pts',(-7.25296364227466,-35.4936682509291,
2.25700275374595));
#50547=CARTESIAN_POINT('Ctrl Pts',(-7.24272271209379,-35.4867971847728,
2.24037824521197));
#50548=CARTESIAN_POINT('Ctrl Pts',(-7.23334333153,-35.4800020975,2.22433302544));
#50549=CARTESIAN_POINT('Ctrl Pts',(-7.23334333044,-35.4800020975,2.22433302572));
#50550=CARTESIAN_POINT('Ctrl Pts',(-7.22937402512,-35.477126751,2.21754286118));
#50551=CARTESIAN_POINT('Ctrl Pts',(-7.22542564343,-35.4742071929,2.21065452768));
#50552=CARTESIAN_POINT('Ctrl Pts',(-7.22151371785,-35.4712377752,2.20368850558));
#50553=CARTESIAN_POINT('Ctrl Pts',(-7.21764954964,-35.4682109676,2.19666066586));
#50554=CARTESIAN_POINT('Ctrl Pts',(-7.21384189759,-35.46511484,2.18958432614));
#50555=CARTESIAN_POINT('Ctrl Pts',(-8.75956299023,-36.3742356128,2.0634404101));
#50556=CARTESIAN_POINT('Ctrl Pts',(-8.75956299023,-35.3373826802055,2.0634404101));
#50557=CARTESIAN_POINT('Ctrl Pts',(-8.92890465395,-36.3742356128,1.78598462948));
#50558=CARTESIAN_POINT('Ctrl Pts',(-8.92890465395,-35.3373826802055,1.78598462948));
#50559=CARTESIAN_POINT('Ctrl Pts',(-9.07291332076,-36.3742356128,1.49306717121));
#50560=CARTESIAN_POINT('Ctrl Pts',(-9.07291332076,-35.3373826802055,1.49306717121));
#50561=CARTESIAN_POINT('Ctrl Pts',(-9.12674872803,-36.3742356128,1.15064845916));
#50562=CARTESIAN_POINT('Ctrl Pts',(-9.12674872803,-35.3373826802055,1.15064845916));
#50563=CARTESIAN_POINT('Ctrl Pts',(-9.18664865847,-36.3742356128,0.831017278590001));
#50564=CARTESIAN_POINT('Ctrl Pts',(-9.18664865847,-35.3373826802055,0.831017278590001));
#50565=CARTESIAN_POINT('Ctrl Pts',(-9.23698117862,-36.3742356128,0.509886547135));
#50566=CARTESIAN_POINT('Ctrl Pts',(-9.23698117862,-35.3373826802055,0.509886547135));
#50567=CARTESIAN_POINT('',(-9.23698117854899,-35.5153448503988,0.509886547089706));
#50568=CARTESIAN_POINT('',(-9.23698117862,-36.1242356128,0.509886547138));
#50569=CARTESIAN_POINT('',(-9.22799880548,-35.5169181946,0.566467047115));
#50570=CARTESIAN_POINT('Ctrl Pts',(-9.23698117862,-35.5153448509,0.509886547139));
#50571=CARTESIAN_POINT('Ctrl Pts',(-9.23547079661,-35.5156173384,0.519523062039));
#50572=CARTESIAN_POINT('Ctrl Pts',(-9.23395444171,-35.5158907435,0.529141367463));
#50573=CARTESIAN_POINT('Ctrl Pts',(-9.2324173579,-35.5161611506,0.538838588998));
#50574=CARTESIAN_POINT('Ctrl Pts',(-9.2306125394,-35.5164751965,0.550165758707));
#50575=CARTESIAN_POINT('Ctrl Pts',(-9.22879492211,-35.5167839497,0.561507557195));
#50576=CARTESIAN_POINT('Ctrl Pts',(-9.22852978607,-35.5168288241,0.563160610681));
#50577=CARTESIAN_POINT('Ctrl Pts',(-9.22826440991,-35.5168735732,0.564813796021));
#50578=CARTESIAN_POINT('Ctrl Pts',(-9.22799880548,-35.5169181946,0.566467047115));
#50579=CARTESIAN_POINT('Ctrl Pts',(-9.22799880548,-35.5169181946,0.566467047115));
#50580=CARTESIAN_POINT('Ctrl Pts',(-9.22709573015,-35.5170698741,0.572088224967));
#50581=CARTESIAN_POINT('Ctrl Pts',(-9.22618896279,-35.5172202096,0.57771674331));
#50582=CARTESIAN_POINT('Ctrl Pts',(-9.22528372099,-35.5173684625,0.58332051525));
#50583=CARTESIAN_POINT('Ctrl Pts',(-9.21064489493,-35.5197392711,0.67370187071));
#50584=CARTESIAN_POINT('Ctrl Pts',(-9.19547141468,-35.5218042907,0.763606652472));
#50585=CARTESIAN_POINT('Ctrl Pts',(-9.18087022532,-35.5239641094,0.847743194451));
#50586=CARTESIAN_POINT('Ctrl Pts',(-9.1488371776,-35.5298747429,1.02282666839));
#50587=CARTESIAN_POINT('Ctrl Pts',(-9.1112963015,-35.5399157471,1.19686722852));
#50588=CARTESIAN_POINT('Ctrl Pts',(-9.08965016934,-35.5466085932,1.28690888429));
#50589=CARTESIAN_POINT('Ctrl Pts',(-9.04054093324,-35.5631550729,1.46510383868));
#50590=CARTESIAN_POINT('Ctrl Pts',(-8.97813093642,-35.5847442368,1.63735111856));
#50591=CARTESIAN_POINT('Ctrl Pts',(-8.94306195143,-35.596524942,1.72177132487));
#50592=CARTESIAN_POINT('Ctrl Pts',(-8.89434925659,-35.6115263375,1.82461373716));
#50593=CARTESIAN_POINT('Ctrl Pts',(-8.84001654494,-35.6256966309,1.92519756404));
#50594=CARTESIAN_POINT('Ctrl Pts',(-8.82896553279,-35.6284769797,1.94517168962));
#50595=CARTESIAN_POINT('Ctrl Pts',(-8.80877742677,-35.6333588617,1.98085549694));
#50596=CARTESIAN_POINT('Ctrl Pts',(-8.78793522997,-35.6380188734,2.01638522454));
#50597=CARTESIAN_POINT('Ctrl Pts',(-8.77859596185,-35.6400309319,2.03207294823));
#50598=CARTESIAN_POINT('Ctrl Pts',(-8.76913081737,-35.641984033,2.04776380401));
#50599=CARTESIAN_POINT('Ctrl Pts',(-8.75956299023,-35.6438772164,2.0634404101));
#50600=CARTESIAN_POINT('Ctrl Pts',(-1.87043161103,-36.3742356128,-8.24476960824));
#50601=CARTESIAN_POINT('Ctrl Pts',(-1.87043161103,-35.2215350722322,-8.24476960824));
#50602=CARTESIAN_POINT('Ctrl Pts',(-2.47265813357,-36.3742356128,-8.13634296351));
#50603=CARTESIAN_POINT('Ctrl Pts',(-2.47265813357,-35.2215350722322,-8.13634296351));
#50604=CARTESIAN_POINT('Ctrl Pts',(-3.05192283465,-36.3742356128,-7.98771609515));
#50605=CARTESIAN_POINT('Ctrl Pts',(-3.05192283465,-35.2215350722322,-7.98771609515));
#50606=CARTESIAN_POINT('Ctrl Pts',(-3.608285111,-36.3742356128,-7.79892601222));
#50607=CARTESIAN_POINT('Ctrl Pts',(-3.608285111,-35.2215350722322,-7.79892601222));
#50608=CARTESIAN_POINT('Ctrl Pts',(-4.84313848674,-36.3742356128,-7.27000777732));
#50609=CARTESIAN_POINT('Ctrl Pts',(-4.84313848674,-35.2215350722322,-7.27000777732));
#50610=CARTESIAN_POINT('Ctrl Pts',(-5.97499470659,-36.3742356128,-6.53839758248));
#50611=CARTESIAN_POINT('Ctrl Pts',(-5.97499470659,-35.2215350722322,-6.53839758248));
#50612=CARTESIAN_POINT('Ctrl Pts',(-6.59156749188,-36.3742356128,-6.06232184959));
#50613=CARTESIAN_POINT('Ctrl Pts',(-6.59156749188,-35.2215350722322,-6.06232184959));
#50614=CARTESIAN_POINT('Ctrl Pts',(-7.62010012329,-36.3742356128,-5.1678005996));
#50615=CARTESIAN_POINT('Ctrl Pts',(-7.62010012329,-35.2215350722322,-5.1678005996));
#50616=CARTESIAN_POINT('Ctrl Pts',(-8.47746400168,-36.3742356128,-4.11735171219));
#50617=CARTESIAN_POINT('Ctrl Pts',(-8.47746400168,-35.2215350722322,-4.11735171219));
#50618=CARTESIAN_POINT('Ctrl Pts',(-8.78407978672,-36.3742356128,-3.65866522624));
#50619=CARTESIAN_POINT('Ctrl Pts',(-8.78407978672,-35.2215350722322,-3.65866522624));
#50620=CARTESIAN_POINT('Ctrl Pts',(-9.22504359392,-36.3742356128,-2.71647636201));
#50621=CARTESIAN_POINT('Ctrl Pts',(-9.22504359392,-35.2215350722322,-2.71647636201));
#50622=CARTESIAN_POINT('Ctrl Pts',(-9.38605456704,-36.3742356128,-1.68617604095));
#50623=CARTESIAN_POINT('Ctrl Pts',(-9.38605456704,-35.2215350722322,-1.68617604095));
#50624=CARTESIAN_POINT('Ctrl Pts',(-9.40005841918,-36.3742356128,-1.17735235373));
#50625=CARTESIAN_POINT('Ctrl Pts',(-9.40005841918,-35.2215350722322,-1.17735235373));
#50626=CARTESIAN_POINT('Ctrl Pts',(-9.36972184244,-36.3742356128,-0.530817230024));
#50627=CARTESIAN_POINT('Ctrl Pts',(-9.36972184244,-35.2215350722322,-0.530817230024));
#50628=CARTESIAN_POINT('Ctrl Pts',(-9.2950327654,-36.3742356128,0.106470788818));
#50629=CARTESIAN_POINT('Ctrl Pts',(-9.2950327654,-35.2215350722322,0.106470788818));
#50630=CARTESIAN_POINT('Ctrl Pts',(-9.27733443288,-36.3742356128,0.241562002067001));
#50631=CARTESIAN_POINT('Ctrl Pts',(-9.27733443288,-35.2215350722322,0.241562002067001));
#50632=CARTESIAN_POINT('Ctrl Pts',(-9.25795835827,-36.3742356128,0.376048284641));
#50633=CARTESIAN_POINT('Ctrl Pts',(-9.25795835827,-35.2215350722322,0.376048284641));
#50634=CARTESIAN_POINT('Ctrl Pts',(-9.23698117862,-36.3742356128,0.509886547165));
#50635=CARTESIAN_POINT('Ctrl Pts',(-9.23698117862,-35.2215350722322,0.509886547165));
#50636=CARTESIAN_POINT('',(-1.8704316154347,-35.4944687624331,-8.24476961257036));
#50637=CARTESIAN_POINT('',(-1.87043161103,-36.1242356128,-8.24476960824));
#50638=CARTESIAN_POINT('',(-2.0299262428936,-35.4952698980321,-8.21479979569791));
#50639=CARTESIAN_POINT('Origin',(-1.87573872781909,-33.331129330927,-7.77578136547059));
#50640=CARTESIAN_POINT('',(-8.91162791630276,-35.4775418018593,-3.31601642789431));
#50641=CARTESIAN_POINT('Ctrl Pts',(-2.02993009745,-35.4952697797,-8.21479904026));
#50642=CARTESIAN_POINT('Ctrl Pts',(-2.18929689584727,-35.4902364571318,
-8.18359011989225));
#50643=CARTESIAN_POINT('Ctrl Pts',(-2.34325066281365,-35.4854550094663,
-8.14962872511168));
#50644=CARTESIAN_POINT('Ctrl Pts',(-2.49201818344239,-35.4809648403771,
-8.11335881534916));
#50645=CARTESIAN_POINT('Ctrl Pts',(-2.65136293418602,-35.4761554245094,
-8.0745101492816));
#50646=CARTESIAN_POINT('Ctrl Pts',(-2.80475858050197,-35.4716799045491,
-8.03301402245608));
#50647=CARTESIAN_POINT('Ctrl Pts',(-2.95252830755803,-35.4675538289942,
-7.98939303684412));
#50648=CARTESIAN_POINT('Ctrl Pts',(-3.02398660722482,-35.4655585465414,
-7.96829885521626));
#50649=CARTESIAN_POINT('Ctrl Pts',(-3.09412984908824,-35.463644537325,-7.94670735028006));
#50650=CARTESIAN_POINT('Ctrl Pts',(-3.16299705647906,-35.4618113955355,
-7.92467486461585));
#50651=CARTESIAN_POINT('Ctrl Pts',(-3.29831147262683,-35.4582095286912,
-7.88138411642247));
#50652=CARTESIAN_POINT('Ctrl Pts',(-3.42893430185573,-35.454884995394,-7.83631198095569));
#50653=CARTESIAN_POINT('Ctrl Pts',(-3.55481517329765,-35.4518612230206,
-7.7899762595127));
#50654=CARTESIAN_POINT('Ctrl Pts',(-3.69766906756152,-35.4484297432893,
-7.73739290688861));
#50655=CARTESIAN_POINT('Ctrl Pts',(-3.83441616439784,-35.4453853684485,
-7.68318308540026));
#50656=CARTESIAN_POINT('Ctrl Pts',(-3.96503125082369,-35.4427217611445,
-7.62813243602623));
#50657=CARTESIAN_POINT('Ctrl Pts',(-4.01212236679739,-35.4417614414456,
-7.60828483200867));
#50658=CARTESIAN_POINT('Ctrl Pts',(-4.05841681338306,-35.4408502938001,
-7.58832810721544));
#50659=CARTESIAN_POINT('Ctrl Pts',(-4.10391457658464,-35.4399870947724,
-7.56829943995679));
#50660=CARTESIAN_POINT('Ctrl Pts',(-4.25389323618712,-35.4371416486662,
-7.50227701472747));
#50661=CARTESIAN_POINT('Ctrl Pts',(-4.40819154727007,-35.4345650870246,
-7.42976069922605));
#50662=CARTESIAN_POINT('Ctrl Pts',(-4.56648104744728,-35.432294211752,-7.3498427515548));
#50663=CARTESIAN_POINT('Ctrl Pts',(-4.70676304345842,-35.4302816782892,
-7.27901651732014));
#50664=CARTESIAN_POINT('Ctrl Pts',(-4.85017801583353,-35.4285109316766,
-7.20237417174943));
#50665=CARTESIAN_POINT('Ctrl Pts',(-4.99649524902321,-35.4269957372856,
-7.11931649038508));
#50666=CARTESIAN_POINT('Ctrl Pts',(-5.11556507709157,-35.4257627045682,
-7.05172592962735));
#50667=CARTESIAN_POINT('Ctrl Pts',(-5.23656919882029,-35.4247157623198,
-6.97987983296062));
#50668=CARTESIAN_POINT('Ctrl Pts',(-5.35943588605315,-35.4238515670765,
-6.90346517638933));
#50669=CARTESIAN_POINT('Ctrl Pts',(-5.37358279482046,-35.4237520633661,
-6.89466676894996));
#50670=CARTESIAN_POINT('Ctrl Pts',(-5.3877544121134,-35.42365495475,-6.88580784316436));
#50671=CARTESIAN_POINT('Ctrl Pts',(-5.40195064262958,-35.423560213071,-6.87688796232893));
#50672=CARTESIAN_POINT('Ctrl Pts',(-5.5317365229437,-35.4226940583409,-6.7953399355338));
#50673=CARTESIAN_POINT('Ctrl Pts',(-5.66358167884288,-35.4220280565828,
-6.70869588257285));
#50674=CARTESIAN_POINT('Ctrl Pts',(-5.79738679233785,-35.4215214553207,
-6.61659013521258));
#50675=CARTESIAN_POINT('Ctrl Pts',(-5.83350781056089,-35.4213846970688,
-6.59172596304496));
#50676=CARTESIAN_POINT('Ctrl Pts',(-5.86977143199235,-35.4212594104568,
-6.56646389334973));
#50677=CARTESIAN_POINT('Ctrl Pts',(-5.90617504013701,-35.4211445378308,
-6.54079696194274));
#50678=CARTESIAN_POINT('Ctrl Pts',(-5.92159327159422,-35.4210958851608,
-6.52992609750379));
#50679=CARTESIAN_POINT('Ctrl Pts',(-5.93605165098445,-35.4210520297038,
-6.51968217529532));
#50680=CARTESIAN_POINT('Ctrl Pts',(-5.95172616209454,-35.4210060263787,
-6.5085204996939));
#50681=CARTESIAN_POINT('Ctrl Pts',(-5.95734063671402,-35.4209895483847,
-6.50452248381098));
#50682=CARTESIAN_POINT('Ctrl Pts',(-5.96311091048011,-35.4209728148743,
-6.50040632012766));
#50683=CARTESIAN_POINT('Ctrl Pts',(-5.9691361516031,-35.420955575595,-6.49609959272189));
#50684=CARTESIAN_POINT('Ctrl Pts',(-6.06908640339718,-35.4206696002674,
-6.42465705958041));
#50685=CARTESIAN_POINT('Ctrl Pts',(-6.16548414027397,-35.4204459918632,
-6.35344243759832));
#50686=CARTESIAN_POINT('Ctrl Pts',(-6.25844568390168,-35.4202640009878,
-6.28279230429464));
#50687=CARTESIAN_POINT('Ctrl Pts',(-6.35363024262543,-35.4200776581143,
-6.21045269481897));
#50688=CARTESIAN_POINT('Ctrl Pts',(-6.44521227760241,-35.4199348833781,
-6.1387046910448));
#50689=CARTESIAN_POINT('Ctrl Pts',(-6.53328629732009,-35.4198314487939,
-6.06786581553125));
#50690=CARTESIAN_POINT('Ctrl Pts',(-6.62786612394948,-35.4197203737565,
-5.99179424997572));
#50691=CARTESIAN_POINT('Ctrl Pts',(-6.71840025583166,-35.4196547552607,
-5.91677103106586));
#50692=CARTESIAN_POINT('Ctrl Pts',(-6.80497303596595,-35.419649997424,-5.84314099276948));
#50693=CARTESIAN_POINT('Ctrl Pts',(-6.84700206399384,-35.4196476876073,
-5.80739535842053));
#50694=CARTESIAN_POINT('Ctrl Pts',(-6.8880970092318,-35.4196600097299,-5.77197738755347));
#50695=CARTESIAN_POINT('Ctrl Pts',(-6.92826553348727,-35.419690092492,-5.73692300258239));
#50696=CARTESIAN_POINT('Ctrl Pts',(-7.02473825161427,-35.4197623422418,
-5.65273290939095));
#50697=CARTESIAN_POINT('Ctrl Pts',(-7.11586309787553,-35.4199125655208,
-5.5706480730014));
#50698=CARTESIAN_POINT('Ctrl Pts',(-7.20173998727502,-35.4201398128318,
-5.49111566364252));
#50699=CARTESIAN_POINT('Ctrl Pts',(-7.23835353620077,-35.4202366995565,
-5.45720707913734));
#50700=CARTESIAN_POINT('Ctrl Pts',(-7.27401300829813,-35.4203477035167,
-5.42376176294008));
#50701=CARTESIAN_POINT('Ctrl Pts',(-7.3087261154237,-35.4204728900179,-5.39081163268007));
#50702=CARTESIAN_POINT('Ctrl Pts',(-7.31344645414271,-35.4204899130601,
-5.38633102611551));
#50703=CARTESIAN_POINT('Ctrl Pts',(-7.31814930121898,-35.4205071935359,
-5.3818595672839));
#50704=CARTESIAN_POINT('Ctrl Pts',(-7.32283466808666,-35.4205247406587,
-5.37739734263404));
#50705=CARTESIAN_POINT('Ctrl Pts',(-7.37578536236207,-35.4207230457994,
-5.32696844348988));
#50706=CARTESIAN_POINT('Ctrl Pts',(-7.4265050614639,-35.4209546111681,-5.27771872821795));
#50707=CARTESIAN_POINT('Ctrl Pts',(-7.47503381051047,-35.4212195168391,
-5.22975918031341));
#50708=CARTESIAN_POINT('Ctrl Pts',(-7.50144522952509,-35.4213636898255,
-5.20365754488402));
#50709=CARTESIAN_POINT('Ctrl Pts',(-7.52720756230863,-35.4215177304207,
-5.1779379121768));
#50710=CARTESIAN_POINT('Ctrl Pts',(-7.55232793900539,-35.4216816385961,
-5.15261626108499));
#50711=CARTESIAN_POINT('Ctrl Pts',(-7.56488812735376,-35.4217635926838,
-5.13995543553908));
#50712=CARTESIAN_POINT('Ctrl Pts',(-7.57728782906225,-35.4218455841287,
-5.12739409426947));
#50713=CARTESIAN_POINT('Ctrl Pts',(-7.58952795253593,-35.4219285831362,
-5.11493418074097));
#50714=CARTESIAN_POINT('Ctrl Pts',(-7.59603051813133,-35.4219726763589,
-5.10831485167896));
#50715=CARTESIAN_POINT('Ctrl Pts',(-7.60248804511812,-35.422017468346,-5.10172414935278));
#50716=CARTESIAN_POINT('Ctrl Pts',(-7.60890067435508,-35.4220629582103,
-5.09516235913147));
#50717=CARTESIAN_POINT('Ctrl Pts',(-7.61200679164173,-35.4220849923633,
-5.09198399199302));
#50718=CARTESIAN_POINT('Ctrl Pts',(-7.61510237508418,-35.4221071902546,
-5.08881240815013));
#50719=CARTESIAN_POINT('Ctrl Pts',(-7.61818744096429,-35.4221295517926,
-5.08564763970962));
#50720=CARTESIAN_POINT('Ctrl Pts',(-7.61894665639572,-35.4221350548274,
-5.08486880997621));
#50721=CARTESIAN_POINT('Ctrl Pts',(-7.61970523486104,-35.4221405677729,
-5.08409039299812));
#50722=CARTESIAN_POINT('Ctrl Pts',(-7.62046317660273,-35.4221460906279,
-5.08331238925388));
#50723=CARTESIAN_POINT('Ctrl Pts',(-7.6206575511755,-35.422147506967,-5.08311286976962));
#50724=CARTESIAN_POINT('Ctrl Pts',(-7.62085188387294,-35.4221489239579,
-5.08291337746247));
#50725=CARTESIAN_POINT('Ctrl Pts',(-7.62104617469914,-35.4221503416005,
-5.08271391234048));
#50726=CARTESIAN_POINT('Ctrl Pts',(-7.62121633244005,-35.422151583156,-5.08253922300898));
#50727=CARTESIAN_POINT('Ctrl Pts',(-7.62138859966819,-35.4221528408801,
-5.08236235519101));
#50728=CARTESIAN_POINT('Ctrl Pts',(-7.62154789780562,-35.4221540045504,
-5.08219879236452));
#50729=CARTESIAN_POINT('Ctrl Pts',(-7.62225305804759,-35.4221591557344,
-5.08147475375261));
#50730=CARTESIAN_POINT('Ctrl Pts',(-7.6227731152015,-35.4221629636036,-5.08094062756502));
#50731=CARTESIAN_POINT('Ctrl Pts',(-7.62344669187689,-35.4221679057579,
-5.08024866069744));
#50732=CARTESIAN_POINT('Ctrl Pts',(-7.62378216463514,-35.4221703671823,
-5.07990402876144));
#50733=CARTESIAN_POINT('Ctrl Pts',(-7.62415571356334,-35.4221731105011,
-5.0795202395543));
#50734=CARTESIAN_POINT('Ctrl Pts',(-7.62460913497078,-35.422176446303,-5.07905429122528));
#50735=CARTESIAN_POINT('Ctrl Pts',(-7.62480121816504,-35.4221778594508,
-5.0788569012434));
#50736=CARTESIAN_POINT('Ctrl Pts',(-7.62500763509778,-35.4221793789766,
-5.07864476630863));
#50737=CARTESIAN_POINT('Ctrl Pts',(-7.62523156111189,-35.4221810287663,
-5.07841461473952));
#50738=CARTESIAN_POINT('Ctrl Pts',(-7.62538775764981,-35.4221821795546,
-5.07825407565059));
#50739=CARTESIAN_POINT('Ctrl Pts',(-7.62555247332383,-35.4221833937273,
-5.07808477041067));
#50740=CARTESIAN_POINT('Ctrl Pts',(-7.62572678528594,-35.4221846794553,
-5.07790558807117));
#50741=CARTESIAN_POINT('Ctrl Pts',(-7.62588995094337,-35.422185882968,-5.07773786347056));
#50742=CARTESIAN_POINT('Ctrl Pts',(-7.62605590764984,-35.4221871077609,
-5.07756725845795));
#50743=CARTESIAN_POINT('Ctrl Pts',(-7.62622054005713,-35.422188323481,-5.07739800334206));
#50744=CARTESIAN_POINT('Ctrl Pts',(-7.70695216467482,-35.422784482276,-4.99439951777019));
#50745=CARTESIAN_POINT('Ctrl Pts',(-7.78297578327702,-35.4235131623992,
-4.91349867411078));
#50746=CARTESIAN_POINT('Ctrl Pts',(-7.85437558442288,-35.424403953379,-4.83498231891968));
#50747=CARTESIAN_POINT('Ctrl Pts',(-7.9134915281878,-35.4251414897393,-4.76997417654936));
#50748=CARTESIAN_POINT('Ctrl Pts',(-7.96943659929543,-35.4259906431666,
-4.70660119463088));
#50749=CARTESIAN_POINT('Ctrl Pts',(-8.02227857318465,-35.4269587081494,
-4.6450340975051));
#50750=CARTESIAN_POINT('Ctrl Pts',(-8.08393265604328,-35.4280882109721,
-4.57319985990611));
#50751=CARTESIAN_POINT('Ctrl Pts',(-8.14136523220772,-35.4293803500542,
-4.50381970168519));
#50752=CARTESIAN_POINT('Ctrl Pts',(-8.19476584495109,-35.4308233199233,
-4.43713267964401));
#50753=CARTESIAN_POINT('Ctrl Pts',(-8.22146615132277,-35.4315448048578,
-4.40378916862343));
#50754=CARTESIAN_POINT('Ctrl Pts',(-8.24715933772014,-35.4323035759929,
-4.37111898073678));
#50755=CARTESIAN_POINT('Ctrl Pts',(-8.27187486588063,-35.4330958492025,
-4.33915071527316));
#50756=CARTESIAN_POINT('Ctrl Pts',(-8.28423262996087,-35.4334919858072,
-4.32316658254135));
#50757=CARTESIAN_POINT('Ctrl Pts',(-8.29634600764459,-35.4338964747233,
-4.30735795075904));
#50758=CARTESIAN_POINT('Ctrl Pts',(-8.30821901697159,-35.4343087198482,
-4.29172826253413));
#50759=CARTESIAN_POINT('Ctrl Pts',(-8.31415552163508,-35.4345148424107,
-4.28391341842168));
#50760=CARTESIAN_POINT('Ctrl Pts',(-8.32003193672778,-35.4347229028061,
-4.27614330971437));
#50761=CARTESIAN_POINT('Ctrl Pts',(-8.32584877735325,-35.4349328194777,
-4.2684183656988));
#50762=CARTESIAN_POINT('Ctrl Pts',(-8.32875719766598,-35.4350377778135,
-4.26455589369101));
#50763=CARTESIAN_POINT('Ctrl Pts',(-8.33165072448736,-35.4351432001474,
-4.26070471284826));
#50764=CARTESIAN_POINT('Ctrl Pts',(-8.33452942331843,-35.4352490758846,
-4.25686487626074));
#50765=CARTESIAN_POINT('Ctrl Pts',(-8.33477470837254,-35.4352580972298,
-4.25653769562102));
#50766=CARTESIAN_POINT('Ctrl Pts',(-8.33501937674538,-35.4352671032692,
-4.25621127527631));
#50767=CARTESIAN_POINT('Ctrl Pts',(-8.33525702577003,-35.4352758576722,
-4.25589416277902));
#50768=CARTESIAN_POINT('Ctrl Pts',(-8.33780845809389,-35.4353698461356,
-4.25248959978085));
#50769=CARTESIAN_POINT('Ctrl Pts',(-8.33979079821542,-35.4354432477629,
-4.24984122829577));
#50770=CARTESIAN_POINT('Ctrl Pts',(-8.34312110187758,-35.4355680524468,
-4.24537945221164));
#50771=CARTESIAN_POINT('Ctrl Pts',(-8.40612657614725,-35.4379292119982,
-4.16096783489886));
#50772=CARTESIAN_POINT('Ctrl Pts',(-8.46644700936824,-35.4406790565229,
-4.07605040377369));
#50773=CARTESIAN_POINT('Ctrl Pts',(-8.52390193196485,-35.4438618010421,
-3.99065934753446));
#50774=CARTESIAN_POINT('Ctrl Pts',(-8.57900386837241,-35.4469142007004,
-3.90876536285878));
#50775=CARTESIAN_POINT('Ctrl Pts',(-8.63146962841867,-35.4503649522411,
-3.82643584977495));
#50776=CARTESIAN_POINT('Ctrl Pts',(-8.68117225080198,-35.4542258470509,
-3.74371800949252));
#50777=CARTESIAN_POINT('Ctrl Pts',(-8.72917890183889,-35.4579549989736,
-3.66382269808739));
#50778=CARTESIAN_POINT('Ctrl Pts',(-8.7746075349702,-35.4620668174179,-3.58356521086298));
#50779=CARTESIAN_POINT('Ctrl Pts',(-8.81737998421833,-35.4665445123863,
-3.50300456770493));
#50780=CARTESIAN_POINT('Ctrl Pts',(-8.85038312017606,-35.4699994928333,
-3.44084413720063));
#50781=CARTESIAN_POINT('Ctrl Pts',(-8.88180556085801,-35.4736717653558,
-3.37850355041783));
#50782=CARTESIAN_POINT('Ctrl Pts',(-8.91162790031208,-35.4775418017954,
-3.31601642164564));
#50783=CARTESIAN_POINT('',(-9.00070817952036,-35.4796536185211,-3.11775012994394));
#50784=CARTESIAN_POINT('Origin',(-8.92974789374037,-35.4242646256046,-3.20847971418429));
#50785=CARTESIAN_POINT('Ctrl Pts',(-9.00070981177086,-35.4796534480026,
-3.11774626039934));
#50786=CARTESIAN_POINT('Ctrl Pts',(-9.03140777082974,-35.4767481961118,
-3.0449301336738));
#50787=CARTESIAN_POINT('Ctrl Pts',(-9.0605225219848,-35.4741877030414,-2.9706562389485));
#50788=CARTESIAN_POINT('Ctrl Pts',(-9.08787309691769,-35.4719966235732,
-2.89491150963051));
#50789=CARTESIAN_POINT('Ctrl Pts',(-9.11100123829071,-35.4701438071033,
-2.83086039508443));
#50790=CARTESIAN_POINT('Ctrl Pts',(-9.1328685889702,-35.4685547439761,-2.76575784469073));
#50791=CARTESIAN_POINT('Ctrl Pts',(-9.1533905300849,-35.4672329840956,-2.69960607538102));
#50792=CARTESIAN_POINT('Ctrl Pts',(-9.17578578500115,-35.4657905693992,
-2.62741574364917));
#50793=CARTESIAN_POINT('Ctrl Pts',(-9.19657795467695,-35.4646666084973,
-2.55397669769755));
#50794=CARTESIAN_POINT('Ctrl Pts',(-9.21568765704498,-35.4638527593822,
-2.4793089047899));
#50795=CARTESIAN_POINT('Ctrl Pts',(-9.230019933821,-35.4632423725458,-2.42330806010916));
#50796=CARTESIAN_POINT('Ctrl Pts',(-9.24340649218174,-35.4628061254186,
-2.36661637379091));
#50797=CARTESIAN_POINT('Ctrl Pts',(-9.25582614175848,-35.4625360683822,
-2.30924802224927));
#50798=CARTESIAN_POINT('Ctrl Pts',(-9.2569904839063,-35.462510750535,-2.30386973929224));
#50799=CARTESIAN_POINT('Ctrl Pts',(-9.25814633549059,-35.4624868908549,
-2.29848551281977));
#50800=CARTESIAN_POINT('Ctrl Pts',(-9.25929368381884,-35.4624644812833,
-2.29309535677824));
#50801=CARTESIAN_POINT('Ctrl Pts',(-9.25984943066533,-35.4624536266471,
-2.29048449994562));
#50802=CARTESIAN_POINT('Ctrl Pts',(-9.26040318249775,-35.4624431122304,
-2.28787225192695));
#50803=CARTESIAN_POINT('Ctrl Pts',(-9.26095493794436,-35.4624329370971,
-2.28525861433154));
#50804=CARTESIAN_POINT('Ctrl Pts',(-9.26119582484673,-35.4624284948096,
-2.28411754527979));
#50805=CARTESIAN_POINT('Ctrl Pts',(-9.26143633122959,-35.4624241171909,
-2.28297621136869));
#50806=CARTESIAN_POINT('Ctrl Pts',(-9.26167645698157,-35.4624198041622,
-2.28183461273309));
#50807=CARTESIAN_POINT('Ctrl Pts',(-9.26188214302222,-35.4624161097238,
-2.28085674633838));
#50808=CARTESIAN_POINT('Ctrl Pts',(-9.26208707226724,-35.4624124706879,
-2.27988097625192));
#50809=CARTESIAN_POINT('Ctrl Pts',(-9.2622953257845,-35.4624088164943,-2.27888779972648));
#50810=CARTESIAN_POINT('Ctrl Pts',(-9.26337757293257,-35.4623898264642,
-2.27372648251888));
#50811=CARTESIAN_POINT('Ctrl Pts',(-9.26452141238414,-35.4623710358368,
-2.26822537986269));
#50812=CARTESIAN_POINT('Ctrl Pts',(-9.26559401474242,-35.4623546396656,
-2.26302253304785));
#50813=CARTESIAN_POINT('Ctrl Pts',(-9.26611355650972,-35.4623466977701,
-2.26050240412191));
#50814=CARTESIAN_POINT('Ctrl Pts',(-9.26661651646356,-35.4623392968953,
-2.25805228847085));
#50815=CARTESIAN_POINT('Ctrl Pts',(-9.26708848510517,-35.4623325791954,
-2.25574488479086));
#50816=CARTESIAN_POINT('Ctrl Pts',(-9.26737027271032,-35.4623285684108,
-2.25436725564401));
#50817=CARTESIAN_POINT('Ctrl Pts',(-9.2676410212449,-35.4623247998691,-2.25304050065197));
#50818=CARTESIAN_POINT('Ctrl Pts',(-9.26789772426574,-35.4623212944959,
-2.25178010843329));
#50819=CARTESIAN_POINT('Ctrl Pts',(-9.26800536503634,-35.462319824622,-2.25125160047402));
#50820=CARTESIAN_POINT('Ctrl Pts',(-9.26811222752299,-35.4623183777677,
-2.25072646251089));
#50821=CARTESIAN_POINT('Ctrl Pts',(-9.26821936925621,-35.462316939489,-2.25019950193244));
#50822=CARTESIAN_POINT('Ctrl Pts',(-9.28299197902751,-35.4621186308583,
-2.17754263185134));
#50823=CARTESIAN_POINT('Ctrl Pts',(-9.2966570505828,-35.4621723300256,-2.10172353063556));
#50824=CARTESIAN_POINT('Ctrl Pts',(-9.30891553715524,-35.4624937676329,
-2.0227156018701));
#50825=CARTESIAN_POINT('Ctrl Pts',(-9.31872911874655,-35.4627510958248,
-1.95946548117058));
#50826=CARTESIAN_POINT('Ctrl Pts',(-9.32764138299525,-35.4631796938351,
-1.89417219253685));
#50827=CARTESIAN_POINT('Ctrl Pts',(-9.33551605715918,-35.4637801263595,
-1.82683775045262));
#50828=CARTESIAN_POINT('Ctrl Pts',(-9.3444045078848,-35.4644578578816,-1.75083474916722));
#50829=CARTESIAN_POINT('Ctrl Pts',(-9.35196984152661,-35.4653545131821,
-1.67223055084684));
#50830=CARTESIAN_POINT('Ctrl Pts',(-9.35804899336456,-35.4664615511483,
-1.59105350025987));
#50831=CARTESIAN_POINT('Ctrl Pts',(-9.36108856928353,-35.4670150701314,
-1.55046497496639));
#50832=CARTESIAN_POINT('Ctrl Pts',(-9.36375720753474,-35.4676162058835,
-1.50923361836706));
#50833=CARTESIAN_POINT('Ctrl Pts',(-9.36603846791738,-35.4682703204645,
-1.4673658482447));
#50834=CARTESIAN_POINT('Ctrl Pts',(-9.36717909810869,-35.468597377755,-1.44643196318352));
#50835=CARTESIAN_POINT('Ctrl Pts',(-9.36822292905917,-35.4689376875689,
-1.42533897812757));
#50836=CARTESIAN_POINT('Ctrl Pts',(-9.36916817438962,-35.4692912499044,
-1.40408790438279));
#50837=CARTESIAN_POINT('Ctrl Pts',(-9.36964079705484,-35.4694680310722,
-1.39346236751041));
#50838=CARTESIAN_POINT('Ctrl Pts',(-9.37008877629055,-35.4696481253704,
-1.38279730865109));
#50839=CARTESIAN_POINT('Ctrl Pts',(-9.37051190644291,-35.4698315327986,
-1.37209286098262));
#50840=CARTESIAN_POINT('Ctrl Pts',(-9.37072347151909,-35.4699232365127,
-1.36674063714838));
#50841=CARTESIAN_POINT('Ctrl Pts',(-9.370928824511,-35.4700157685094,-1.36137856611917));
#50842=CARTESIAN_POINT('Ctrl Pts',(-9.37112794080608,-35.4701091287885,
-1.35600666531908));
#50843=CARTESIAN_POINT('Ctrl Pts',(-9.37132705710116,-35.4702024890677,
-1.35063476451899));
#50844=CARTESIAN_POINT('Ctrl Pts',(-9.37159114630659,-35.4703329339099,
-1.34319574304992));
#50845=CARTESIAN_POINT('Ctrl Pts',(-9.37170655573111,-35.4703916944733,
-1.33986149128067));
#50846=CARTESIAN_POINT('Ctrl Pts',(-9.37411723708609,-35.471619089855,-1.27021537177055));
#50847=CARTESIAN_POINT('Ctrl Pts',(-9.37560542972272,-35.4730255082264,
-1.19532765056696));
#50848=CARTESIAN_POINT('Ctrl Pts',(-9.37579224143258,-35.4746404878121,
-1.11525292933757));
#50849=CARTESIAN_POINT('Ctrl Pts',(-9.3758128814272,-35.4748189197208,-1.10640582967405));
#50850=CARTESIAN_POINT('Ctrl Pts',(-9.37581767076311,-35.4749999006119,
-1.0974954518827));
#50851=CARTESIAN_POINT('Ctrl Pts',(-9.3758061275957,-35.4751834744026,-1.08852189959094));
#50852=CARTESIAN_POINT('Ctrl Pts',(-9.37571122871392,-35.4766926743333,
-1.01474838079893));
#50853=CARTESIAN_POINT('Ctrl Pts',(-9.37450956737563,-35.4783778620492,
-0.936702130807714));
#50854=CARTESIAN_POINT('Ctrl Pts',(-9.37195325945033,-35.4802306516693,
-0.854430817470772));
#50855=CARTESIAN_POINT('Ctrl Pts',(-9.36950548980399,-35.4820047736944,
-0.775652661851114));
#50856=CARTESIAN_POINT('Ctrl Pts',(-9.3658155900203,-35.4839320220494,-0.693000293466503));
#50857=CARTESIAN_POINT('Ctrl Pts',(-9.3606998335278,-35.486001697316,-0.606551309684227));
#50858=CARTESIAN_POINT('Ctrl Pts',(-9.35966829322684,-35.4864190262976,
-0.589119750758425));
#50859=CARTESIAN_POINT('Ctrl Pts',(-9.35857889303645,-35.4868421507618,
-0.571533953458252));
#50860=CARTESIAN_POINT('Ctrl Pts',(-9.35743029683677,-35.487270998256,-0.553794748002522));
#50861=CARTESIAN_POINT('Ctrl Pts',(-9.35152045370082,-35.4894775364817,
-0.462521660359738));
#50862=CARTESIAN_POINT('Ctrl Pts',(-9.34404045872566,-35.4918646701929,
-0.367181055595434));
#50863=CARTESIAN_POINT('Ctrl Pts',(-9.33483171081312,-35.4944086119262,
-0.267935924614849));
#50864=CARTESIAN_POINT('Ctrl Pts',(-9.32380215519322,-35.497455556756,-0.149067463608977));
#50865=CARTESIAN_POINT('Ctrl Pts',(-9.3102957030867,-35.5007250422298,-0.0246007203337422));
#50866=CARTESIAN_POINT('Ctrl Pts',(-9.2940739809111,-35.5042080159972,0.105138041622589));
#50867=CARTESIAN_POINT('Ctrl Pts',(-9.28332216793239,-35.506516542931,0.191129337093173));
#50868=CARTESIAN_POINT('Ctrl Pts',(-9.27137885445243,-35.5089196203523,
0.27943477778053));
#50869=CARTESIAN_POINT('Ctrl Pts',(-9.25816061636275,-35.5114289434686,
0.369973937452619));
#50870=CARTESIAN_POINT('Ctrl Pts',(-9.25143593074586,-35.512705543947,0.416035097849456));
#50871=CARTESIAN_POINT('Ctrl Pts',(-9.24438092873596,-35.5140098564956,
0.46267477320469));
#50872=CARTESIAN_POINT('Ctrl Pts',(-9.23698117833998,-35.5153448508951,
0.509886546917126));
#50873=CARTESIAN_POINT('Origin',(-1.81727342606,-36.1242356128,-7.9495168227));
#50874=CARTESIAN_POINT('',(-1.51727342288,-35.544540501139,-7.94951682269995));
#50875=CARTESIAN_POINT('',(-1.51727342606,-35.9593880834,-7.9495168227));
#50876=CARTESIAN_POINT('',(-1.51739959473689,-35.5460990323408,-7.95821664298045));
#50877=CARTESIAN_POINT('Origin',(-1.88128360390313,-40.0416488169456,-7.95002524253046));
#50878=CARTESIAN_POINT('',(-1.85568130399,-35.4970695389,-8.24704805785));
#50879=CARTESIAN_POINT('Ctrl Pts',(-1.51739959739202,-35.5460990330595,
-7.95821664354419));
#50880=CARTESIAN_POINT('Ctrl Pts',(-1.51784040157713,-35.551544433581,-7.9734107080064));
#50881=CARTESIAN_POINT('Ctrl Pts',(-1.51944015474546,-35.5564624662645,
-7.98865298821528));
#50882=CARTESIAN_POINT('Ctrl Pts',(-1.52221396870495,-35.5607753418337,
-8.00374326615405));
#50883=CARTESIAN_POINT('Ctrl Pts',(-1.52508034792987,-35.5652321428706,
-8.01933712349758));
#50884=CARTESIAN_POINT('Ctrl Pts',(-1.52920035542674,-35.5690427768125,
-8.03476806671595));
#50885=CARTESIAN_POINT('Ctrl Pts',(-1.53454083399218,-35.5721488750417,
-8.04981508926192));
#50886=CARTESIAN_POINT('Ctrl Pts',(-1.53985832132163,-35.5752416012412,
-8.06479733303534));
#50887=CARTESIAN_POINT('Ctrl Pts',(-1.54638538066407,-35.577636071276,-8.07939834280623));
#50888=CARTESIAN_POINT('Ctrl Pts',(-1.55404503872652,-35.579299076886,-8.09340906153831));
#50889=CARTESIAN_POINT('Ctrl Pts',(-1.56199623962116,-35.5810253800168,
-8.10795305794244));
#50890=CARTESIAN_POINT('Ctrl Pts',(-1.57116678649342,-35.581963465072,-8.12185869749068));
#50891=CARTESIAN_POINT('Ctrl Pts',(-1.58142798632441,-35.5821006264457,
-8.13491533384685));
#50892=CARTESIAN_POINT('Ctrl Pts',(-1.59149584448517,-35.5822352034228,
-8.14772595687882));
#50893=CARTESIAN_POINT('Ctrl Pts',(-1.602613595017,-35.5815989923742,-8.15971912255805));
#50894=CARTESIAN_POINT('Ctrl Pts',(-1.61462398371853,-35.5801988565566,
-8.17072375022459));
#50895=CARTESIAN_POINT('Ctrl Pts',(-1.62401123170297,-35.5791045187746,
-8.17932490139875));
#50896=CARTESIAN_POINT('Ctrl Pts',(-1.63394272185038,-35.5775439293429,
-8.18732229002714));
#50897=CARTESIAN_POINT('Ctrl Pts',(-1.64432960286547,-35.5755276116623,
-8.19465032514282));
#50898=CARTESIAN_POINT('Ctrl Pts',(-1.65751223624117,-35.5729685781358,
-8.20395078792408));
#50899=CARTESIAN_POINT('Ctrl Pts',(-1.67143040403805,-35.5696742607946,
-8.21217315079081));
#50900=CARTESIAN_POINT('Ctrl Pts',(-1.68587374540741,-35.565686430912,-8.2192114954254));
#50901=CARTESIAN_POINT('Ctrl Pts',(-1.70041483395494,-35.5616716128756,
-8.22629747296635));
#50902=CARTESIAN_POINT('Ctrl Pts',(-1.7154879825108,-35.5569536553932,-8.23218342574401));
#50903=CARTESIAN_POINT('Ctrl Pts',(-1.7308718665687,-35.5515942287824,-8.23681029394356));
#50904=CARTESIAN_POINT('Ctrl Pts',(-1.74453974665183,-35.5468326224185,
-8.24092105553498));
#50905=CARTESIAN_POINT('Ctrl Pts',(-1.75845269437942,-35.5415648512774,
-8.24403870478297));
#50906=CARTESIAN_POINT('Ctrl Pts',(-1.77245352352828,-35.5358486074623,
-8.24615310101329));
#50907=CARTESIAN_POINT('Ctrl Pts',(-1.78937968978829,-35.5289380100849,
-8.24870927977624));
#50908=CARTESIAN_POINT('Ctrl Pts',(-1.8064255637685,-35.521374841914,-8.24979779098238));
#50909=CARTESIAN_POINT('Ctrl Pts',(-1.82333732775558,-35.5132798883306,
-8.24945548954978));
#50910=CARTESIAN_POINT('Ctrl Pts',(-1.83055847689705,-35.5098234264757,
-8.24930933036154));
#50911=CARTESIAN_POINT('Ctrl Pts',(-1.83775521093275,-35.5062703565462,
-8.2489028379445));
#50912=CARTESIAN_POINT('Ctrl Pts',(-1.84490789334748,-35.5026317912376,
-8.24824123808703));
#50913=CARTESIAN_POINT('Ctrl Pts',(-1.84751151403415,-35.5013073309362,
-8.24800041164245));
#50914=CARTESIAN_POINT('Ctrl Pts',(-1.85010944922896,-35.499971478242,-8.24772578323896));
#50915=CARTESIAN_POINT('Ctrl Pts',(-1.85270080612586,-35.4986247745774,
-8.24741763123874));
#50916=CARTESIAN_POINT('Ctrl Pts',(-1.8536955086597,-35.4981078370806,-8.24729934588183));
#50917=CARTESIAN_POINT('Ctrl Pts',(-1.85468986954109,-35.4975889712202,
-8.24717603800027));
#50918=CARTESIAN_POINT('Ctrl Pts',(-1.85568130399,-35.4970695389,-8.24704805785));
#50919=CARTESIAN_POINT('Origin',(-1.86844266437558,-35.7037699017498,-8.22958286354931));
#50920=CARTESIAN_POINT('Origin',(-1.51727342606,-32.4742356128,-5.11808633804));
#50921=CARTESIAN_POINT('',(-1.51727342606,-35.544540554,-5.3083202352798));
#50922=CARTESIAN_POINT('Origin',(-1.09995011675E-15,-34.4242356128,2.38806125834E-16));
#50923=CARTESIAN_POINT('',(9.33061792149,-32.5742356128,12.8743764588));
#50924=CARTESIAN_POINT('',(-8.90572184957,-32.5742356128,13.1718684452));
#50925=CARTESIAN_POINT('Origin',(-4.19954447987E-15,-32.5742356128,1.22464679915E-17));
#50926=CARTESIAN_POINT('',(-8.90572184957,-36.2742356128,13.1718684452));
#50927=CARTESIAN_POINT('',(-8.90572184957,-34.4242356128,13.1718684452));
#50928=CARTESIAN_POINT('',(9.33061792149,-36.2742356128,12.8743764588));
#50929=CARTESIAN_POINT('Origin',(-1.55306943244E-15,-36.2742356128,4.65365783676E-16));
#50930=CARTESIAN_POINT('',(9.33061792149,-34.4242356128,12.8743764588));
#50931=CARTESIAN_POINT('Origin',(-5.10578311124E-15,-36.2742356128,-1.31099105572E-15));
#50932=CARTESIAN_POINT('Origin',(9.27193478991,-36.2742356128,12.7934055377));
#50933=CARTESIAN_POINT('Origin',(-8.84971102033,-36.2742356128,13.0890265053));
#50934=CARTESIAN_POINT('Origin',(9.15456852675,-36.2742356128,12.6314636954));
#50935=CARTESIAN_POINT('',(9.36397871523,-36.2742356128,12.4166442993));
#50936=CARTESIAN_POINT('Origin',(9.29417531907,-36.2742356128,12.4882507647));
#50937=CARTESIAN_POINT('Origin',(9.15456852675,-36.2742356128,12.6314636954));
#50938=CARTESIAN_POINT('Origin',(9.15456852675,-34.4242356128,12.6314636954));
#50939=CARTESIAN_POINT('',(9.36397871523,-32.5742356128,12.4166442993));
#50940=CARTESIAN_POINT('',(9.36397871523,-34.4242356128,12.4166442993));
#50941=CARTESIAN_POINT('Origin',(9.15456852675,-32.5742356128,12.6314636954));
#50942=CARTESIAN_POINT('Origin',(-0.316839226711,-36.2742356128,3.11924403781));
#50943=CARTESIAN_POINT('',(8.19033423541,-36.2742356128,11.2725524894));
#50944=CARTESIAN_POINT('Origin',(8.12053083925,-36.2742356128,11.3441589548));
#50945=CARTESIAN_POINT('',(8.77715647532,-36.2742356128,11.8445983944));
#50946=CARTESIAN_POINT('Origin',(7.97551483927,-32.4742356128,11.0631423009));
#50947=CARTESIAN_POINT('',(8.19033423541,-32.5742356128,11.2725524894));
#50948=CARTESIAN_POINT('',(8.19033423541,-34.4242356128,11.2725524894));
#50949=CARTESIAN_POINT('',(-0.24703583055,-32.5742356128,3.04763757243));
#50950=CARTESIAN_POINT('Origin',(8.39974442389,-36.2742356128,11.0577330933));
#50951=CARTESIAN_POINT('',(8.18492502775,-36.2742356128,10.8483229048));
#50952=CARTESIAN_POINT('Origin',(8.11331856237,-36.2742356128,10.7785195086));
#50953=CARTESIAN_POINT('Origin',(8.39974442389,-36.2742356128,11.0577330933));
#50954=CARTESIAN_POINT('Origin',(8.39974442389,-34.4242356128,11.0577330933));
#50955=CARTESIAN_POINT('',(8.18492502775,-32.5742356128,10.8483229048));
#50956=CARTESIAN_POINT('',(8.18492502775,-34.4242356128,10.8483229048));
#50957=CARTESIAN_POINT('Origin',(8.39974442389,-32.5742356128,11.0577330933));
#50958=CARTESIAN_POINT('Origin',(8.43647932171,-36.2742356128,10.447011287));
#50959=CARTESIAN_POINT('',(11.1928713102,-36.2742356128,7.76267932308));
#50960=CARTESIAN_POINT('Origin',(11.1212648448,-36.2742356128,7.69287592692));
#50961=CARTESIAN_POINT('',(9.68889816899,-36.2742356128,9.30550111394));
#50962=CARTESIAN_POINT('Origin',(11.4022814987,-32.4742356128,7.54785992694));
#50963=CARTESIAN_POINT('',(11.1928713102,-32.5742356128,7.76267932308));
#50964=CARTESIAN_POINT('',(11.1928713102,-34.4242356128,7.76267932308));
#50965=CARTESIAN_POINT('',(8.50808578709,-32.5742356128,10.5168146831));
#50966=CARTESIAN_POINT('Origin',(11.4076907064,-36.2742356128,7.97208951156));
#50967=CARTESIAN_POINT('',(11.6171008949,-36.2742356128,7.75727011542));
#50968=CARTESIAN_POINT('Origin',(11.686904291,-36.2742356128,7.68566365004));
#50969=CARTESIAN_POINT('Origin',(11.4076907064,-36.2742356128,7.97208951156));
#50970=CARTESIAN_POINT('Origin',(11.4076907064,-34.4242356128,7.97208951156));
#50971=CARTESIAN_POINT('',(11.6171008949,-32.5742356128,7.75727011542));
#50972=CARTESIAN_POINT('',(11.6171008949,-34.4242356128,7.75727011542));
#50973=CARTESIAN_POINT('Origin',(11.4076907064,-32.5742356128,7.97208951156));
#50974=CARTESIAN_POINT('Origin',(0.45986885604,-36.2742356128,-3.25867214427));
#50975=CARTESIAN_POINT('',(12.7650943916,-36.2742356128,8.87635684058));
#50976=CARTESIAN_POINT('Origin',(12.8348977878,-36.2742356128,8.80475037519));
#50977=CARTESIAN_POINT('',(12.1910976432,-36.2742356128,8.316813478));
#50978=CARTESIAN_POINT('Origin',(11.4022814987,-32.4742356128,7.54785992694));
#50979=CARTESIAN_POINT('',(12.7650943916,-32.5742356128,8.87635684058));
#50980=CARTESIAN_POINT('',(12.7650943916,-34.4242356128,8.87635684058));
#50981=CARTESIAN_POINT('',(0.390065459879,-32.5742356128,-3.18706567889));
#50982=CARTESIAN_POINT('Origin',(12.9745045801,-36.2742356128,8.66153744443));
#50983=CARTESIAN_POINT('',(13.2240142836,-36.2742356128,8.82810547221));
#50984=CARTESIAN_POINT('Origin',(13.1408443824,-36.2742356128,8.77258279628));
#50985=CARTESIAN_POINT('Origin',(12.9745045801,-36.2742356128,8.66153744443));
#50986=CARTESIAN_POINT('Origin',(12.9745045801,-34.4242356128,8.66153744443));
#50987=CARTESIAN_POINT('',(13.2240142836,-32.5742356128,8.82810547221));
#50988=CARTESIAN_POINT('',(13.2240142836,-34.4242356128,8.82810547221));
#50989=CARTESIAN_POINT('Origin',(12.9745045801,-32.5742356128,8.66153744443));
#50990=CARTESIAN_POINT('Origin',(5.04708629797E-13,-36.2742356128,3.05110563741E-13));
#50991=CARTESIAN_POINT('',(14.1979138053,-36.2742356128,7.15746069337));
#50992=CARTESIAN_POINT('Origin',(14.1086187499,-36.2742356128,7.11244521731));
#50993=CARTESIAN_POINT('Origin',(-1.55306943244E-15,-36.2742356128,4.65365783676E-16));
#50994=CARTESIAN_POINT('Origin',(-1.09995011675E-15,-34.4242356128,2.38806125834E-16));
#50995=CARTESIAN_POINT('',(14.1979138053,-32.5742356128,7.15746069337));
#50996=CARTESIAN_POINT('',(14.1979138053,-34.4242356128,7.15746069337));
#50997=CARTESIAN_POINT('Origin',(6.68547290961E-14,-32.5742356128,3.37630264166E-14));
#50998=CARTESIAN_POINT('Origin',(13.7514385284,-36.2742356128,6.93238331308));
#50999=CARTESIAN_POINT('',(14.2514385284,-36.2742356128,6.93238331308));
#51000=CARTESIAN_POINT('Origin',(14.1514385284,-36.2742356128,6.93238331308));
#51001=CARTESIAN_POINT('Origin',(13.7514385284,-36.2742356128,6.93238331308));
#51002=CARTESIAN_POINT('Origin',(13.7514385284,-34.4242356128,6.93238331308));
#51003=CARTESIAN_POINT('',(14.2514385284,-32.5742356128,6.93238331308));
#51004=CARTESIAN_POINT('',(14.2514385284,-34.4242356128,6.93238331308));
#51005=CARTESIAN_POINT('Origin',(13.7514385284,-32.5742356128,6.93238331308));
#51006=CARTESIAN_POINT('Origin',(14.1514385284,-36.2742356128,5.66451995282E-15));
#51007=CARTESIAN_POINT('',(14.2514385284,-36.2742356128,-6.93238331308));
#51008=CARTESIAN_POINT('Origin',(14.1514385284,-36.2742356128,-6.93238331308));
#51009=CARTESIAN_POINT('',(14.2514385284,-36.2742356128,7.1054273576E-15));
#51010=CARTESIAN_POINT('Origin',(14.2514385284,-32.4742356128,7.05028367309));
#51011=CARTESIAN_POINT('',(14.2514385284,-32.5742356128,-6.93238331308));
#51012=CARTESIAN_POINT('',(14.2514385284,-34.4242356128,-6.93238331308));
#51013=CARTESIAN_POINT('',(14.2514385284,-32.5742356128,3.5527136788E-15));
#51014=CARTESIAN_POINT('Origin',(13.7514385284,-36.2742356128,-6.93238331308));
#51015=CARTESIAN_POINT('',(14.1979138053,-36.2742356128,-7.15746069337));
#51016=CARTESIAN_POINT('Origin',(14.1086187499,-36.2742356128,-7.11244521731));
#51017=CARTESIAN_POINT('Origin',(13.7514385284,-36.2742356128,-6.93238331308));
#51018=CARTESIAN_POINT('Origin',(13.7514385284,-34.4242356128,-6.93238331308));
#51019=CARTESIAN_POINT('',(14.1979138053,-32.5742356128,-7.15746069337));
#51020=CARTESIAN_POINT('',(14.1979138053,-34.4242356128,-7.15746069337));
#51021=CARTESIAN_POINT('Origin',(13.7514385284,-32.5742356128,-6.93238331308));
#51022=CARTESIAN_POINT('Origin',(2.23287406962E-16,-36.2742356128,4.65365783676E-16));
#51023=CARTESIAN_POINT('',(13.2240142836,-36.2742356128,-8.82810547221));
#51024=CARTESIAN_POINT('Origin',(13.1408443824,-36.2742356128,-8.77258279628));
#51025=CARTESIAN_POINT('Origin',(-1.55306943244E-15,-36.2742356128,4.65365783676E-16));
#51026=CARTESIAN_POINT('Origin',(-1.09995011675E-15,-34.4242356128,2.38806125834E-16));
#51027=CARTESIAN_POINT('',(13.2240142836,-32.5742356128,-8.82810547221));
#51028=CARTESIAN_POINT('',(13.2240142836,-34.4242356128,-8.82810547221));
#51029=CARTESIAN_POINT('Origin',(1.12952603833E-15,-32.5742356128,1.22464679915E-17));
#51030=CARTESIAN_POINT('Origin',(12.9745045801,-36.2742356128,-8.66153744443));
#51031=CARTESIAN_POINT('',(12.7650943916,-36.2742356128,-8.87635684058));
#51032=CARTESIAN_POINT('Origin',(12.8348977878,-36.2742356128,-8.80475037519));
#51033=CARTESIAN_POINT('Origin',(12.9745045801,-36.2742356128,-8.66153744443));
#51034=CARTESIAN_POINT('Origin',(12.9745045801,-34.4242356128,-8.66153744443));
#51035=CARTESIAN_POINT('',(12.7650943916,-32.5742356128,-8.87635684058));
#51036=CARTESIAN_POINT('',(12.7650943916,-34.4242356128,-8.87635684058));
#51037=CARTESIAN_POINT('Origin',(12.9745045801,-32.5742356128,-8.66153744443));
#51038=CARTESIAN_POINT('Origin',(0.45986885604,-36.2742356128,3.25867214427));
#51039=CARTESIAN_POINT('',(11.6171008949,-36.2742356128,-7.75727011542));
#51040=CARTESIAN_POINT('Origin',(11.686904291,-36.2742356128,-7.68566365004));
#51041=CARTESIAN_POINT('',(12.1910976432,-36.2742356128,-8.316813478));
#51042=CARTESIAN_POINT('Origin',(11.4022814987,-32.4742356128,-7.54785992694));
#51043=CARTESIAN_POINT('',(11.6171008949,-32.5742356128,-7.75727011542));
#51044=CARTESIAN_POINT('',(11.6171008949,-34.4242356128,-7.75727011542));
#51045=CARTESIAN_POINT('',(0.390065459879,-32.5742356128,3.18706567889));
#51046=CARTESIAN_POINT('Origin',(11.4076907064,-36.2742356128,-7.97208951156));
#51047=CARTESIAN_POINT('',(11.1928713102,-36.2742356128,-7.76267932308));
#51048=CARTESIAN_POINT('Origin',(11.1212648448,-36.2742356128,-7.69287592692));
#51049=CARTESIAN_POINT('Origin',(11.4076907064,-36.2742356128,-7.97208951156));
#51050=CARTESIAN_POINT('Origin',(11.4076907064,-34.4242356128,-7.97208951156));
#51051=CARTESIAN_POINT('',(11.1928713102,-32.5742356128,-7.76267932308));
#51052=CARTESIAN_POINT('',(11.1928713102,-34.4242356128,-7.76267932308));
#51053=CARTESIAN_POINT('Origin',(11.4076907064,-32.5742356128,-7.97208951156));
#51054=CARTESIAN_POINT('Origin',(8.43647932171,-36.2742356128,-10.447011287));
#51055=CARTESIAN_POINT('',(8.18492502775,-36.2742356128,-10.8483229048));
#51056=CARTESIAN_POINT('Origin',(8.11331856237,-36.2742356128,-10.7785195086));
#51057=CARTESIAN_POINT('',(9.68889816899,-36.2742356128,-9.30550111394));
#51058=CARTESIAN_POINT('Origin',(11.4022814987,-32.4742356128,-7.54785992694));
#51059=CARTESIAN_POINT('',(8.18492502775,-32.5742356128,-10.8483229048));
#51060=CARTESIAN_POINT('',(8.18492502775,-34.4242356128,-10.8483229048));
#51061=CARTESIAN_POINT('',(8.50808578709,-32.5742356128,-10.5168146831));
#51062=CARTESIAN_POINT('Origin',(8.39974442389,-36.2742356128,-11.0577330933));
#51063=CARTESIAN_POINT('',(8.19033423541,-36.2742356128,-11.2725524894));
#51064=CARTESIAN_POINT('Origin',(8.12053083925,-36.2742356128,-11.3441589548));
#51065=CARTESIAN_POINT('Origin',(8.39974442389,-36.2742356128,-11.0577330933));
#51066=CARTESIAN_POINT('Origin',(8.39974442389,-34.4242356128,-11.0577330933));
#51067=CARTESIAN_POINT('',(8.19033423541,-32.5742356128,-11.2725524894));
#51068=CARTESIAN_POINT('',(8.19033423541,-34.4242356128,-11.2725524894));
#51069=CARTESIAN_POINT('Origin',(8.39974442389,-32.5742356128,-11.0577330933));
#51070=CARTESIAN_POINT('Origin',(-0.316839226711,-36.2742356128,-3.11924403781));
#51071=CARTESIAN_POINT('',(9.36397871523,-36.2742356128,-12.4166442993));
#51072=CARTESIAN_POINT('Origin',(9.29417531907,-36.2742356128,-12.4882507647));
#51073=CARTESIAN_POINT('',(8.77715647532,-36.2742356128,-11.8445983944));
#51074=CARTESIAN_POINT('Origin',(7.97551483927,-32.4742356128,-11.0631423009));
#51075=CARTESIAN_POINT('',(9.36397871523,-32.5742356128,-12.4166442993));
#51076=CARTESIAN_POINT('',(9.36397871523,-34.4242356128,-12.4166442993));
#51077=CARTESIAN_POINT('',(-0.24703583055,-32.5742356128,-3.04763757243));
#51078=CARTESIAN_POINT('Origin',(9.15456852675,-36.2742356128,-12.6314636954));
#51079=CARTESIAN_POINT('',(9.33061792149,-36.2742356128,-12.8743764588));
#51080=CARTESIAN_POINT('Origin',(9.27193478991,-36.2742356128,-12.7934055377));
#51081=CARTESIAN_POINT('Origin',(9.15456852675,-36.2742356128,-12.6314636954));
#51082=CARTESIAN_POINT('Origin',(9.15456852675,-34.4242356128,-12.6314636954));
#51083=CARTESIAN_POINT('',(9.33061792149,-32.5742356128,-12.8743764588));
#51084=CARTESIAN_POINT('',(9.33061792149,-34.4242356128,-12.8743764588));
#51085=CARTESIAN_POINT('Origin',(9.15456852675,-32.5742356128,-12.6314636954));
#51086=CARTESIAN_POINT('Origin',(-1.09995011675E-15,-34.4242356128,2.38806125834E-16));
#51087=CARTESIAN_POINT('',(-9.33061792149,-32.5742356128,-12.8743764588));
#51088=CARTESIAN_POINT('Origin',(1.12952603833E-15,-32.5742356128,-1.76411037141E-15));
#51089=CARTESIAN_POINT('',(-9.33061792149,-36.2742356128,-12.8743764588));
#51090=CARTESIAN_POINT('Origin',(-1.55306943244E-15,-36.2742356128,4.65365783676E-16));
#51091=CARTESIAN_POINT('',(-9.33061792149,-34.4242356128,-12.8743764588));
#51092=CARTESIAN_POINT('Origin',(1.99964424636E-15,-36.2742356128,2.24172262308E-15));
#51093=CARTESIAN_POINT('Origin',(-9.27193478991,-36.2742356128,-12.7934055377));
#51094=CARTESIAN_POINT('Origin',(-9.15456852675,-36.2742356128,-12.6314636954));
#51095=CARTESIAN_POINT('',(-9.36397871523,-36.2742356128,-12.4166442993));
#51096=CARTESIAN_POINT('Origin',(-9.29417531907,-36.2742356128,-12.4882507647));
#51097=CARTESIAN_POINT('Origin',(-9.15456852675,-36.2742356128,-12.6314636954));
#51098=CARTESIAN_POINT('Origin',(-9.15456852675,-34.4242356128,-12.6314636954));
#51099=CARTESIAN_POINT('',(-9.36397871523,-32.5742356128,-12.4166442993));
#51100=CARTESIAN_POINT('',(-9.36397871523,-34.4242356128,-12.4166442993));
#51101=CARTESIAN_POINT('Origin',(-9.15456852675,-32.5742356128,-12.6314636954));
#51102=CARTESIAN_POINT('Origin',(0.316839226711,-36.2742356128,-3.11924403781));
#51103=CARTESIAN_POINT('',(-8.19033423541,-36.2742356128,-11.2725524894));
#51104=CARTESIAN_POINT('Origin',(-8.12053083925,-36.2742356128,-11.3441589548));
#51105=CARTESIAN_POINT('',(-8.77715647532,-36.2742356128,-11.8445983944));
#51106=CARTESIAN_POINT('Origin',(-7.97551483927,-32.4742356128,-11.0631423009));
#51107=CARTESIAN_POINT('',(-8.19033423541,-32.5742356128,-11.2725524894));
#51108=CARTESIAN_POINT('',(-8.19033423541,-34.4242356128,-11.2725524894));
#51109=CARTESIAN_POINT('',(0.24703583055,-32.5742356128,-3.04763757243));
#51110=CARTESIAN_POINT('Origin',(-8.39974442389,-36.2742356128,-11.0577330933));
#51111=CARTESIAN_POINT('',(-8.18492502775,-36.2742356128,-10.8483229048));
#51112=CARTESIAN_POINT('Origin',(-8.11331856237,-36.2742356128,-10.7785195086));
#51113=CARTESIAN_POINT('Origin',(-8.39974442389,-36.2742356128,-11.0577330933));
#51114=CARTESIAN_POINT('Origin',(-8.39974442389,-34.4242356128,-11.0577330933));
#51115=CARTESIAN_POINT('',(-8.18492502775,-32.5742356128,-10.8483229048));
#51116=CARTESIAN_POINT('',(-8.18492502775,-34.4242356128,-10.8483229048));
#51117=CARTESIAN_POINT('Origin',(-8.39974442389,-32.5742356128,-11.0577330933));
#51118=CARTESIAN_POINT('Origin',(-8.43647932171,-36.2742356128,-10.447011287));
#51119=CARTESIAN_POINT('',(-11.1928713102,-36.2742356128,-7.76267932308));
#51120=CARTESIAN_POINT('Origin',(-11.1212648448,-36.2742356128,-7.69287592692));
#51121=CARTESIAN_POINT('',(-9.68889816899,-36.2742356128,-9.30550111394));
#51122=CARTESIAN_POINT('Origin',(-11.4022814987,-32.4742356128,-7.54785992694));
#51123=CARTESIAN_POINT('',(-11.1928713102,-32.5742356128,-7.76267932308));
#51124=CARTESIAN_POINT('',(-11.1928713102,-34.4242356128,-7.76267932308));
#51125=CARTESIAN_POINT('',(-8.50808578709,-32.5742356128,-10.5168146831));
#51126=CARTESIAN_POINT('Origin',(-11.4076907064,-36.2742356128,-7.97208951156));
#51127=CARTESIAN_POINT('',(-11.6171008949,-36.2742356128,-7.75727011542));
#51128=CARTESIAN_POINT('Origin',(-11.686904291,-36.2742356128,-7.68566365004));
#51129=CARTESIAN_POINT('Origin',(-11.4076907064,-36.2742356128,-7.97208951156));
#51130=CARTESIAN_POINT('Origin',(-11.4076907064,-34.4242356128,-7.97208951156));
#51131=CARTESIAN_POINT('',(-11.6171008949,-32.5742356128,-7.75727011542));
#51132=CARTESIAN_POINT('',(-11.6171008949,-34.4242356128,-7.75727011542));
#51133=CARTESIAN_POINT('Origin',(-11.4076907064,-32.5742356128,-7.97208951156));
#51134=CARTESIAN_POINT('Origin',(-0.45986885604,-36.2742356128,3.25867214427));
#51135=CARTESIAN_POINT('',(-12.7650943916,-36.2742356128,-8.87635684058));
#51136=CARTESIAN_POINT('Origin',(-12.8348977878,-36.2742356128,-8.80475037519));
#51137=CARTESIAN_POINT('',(-12.1910976432,-36.2742356128,-8.316813478));
#51138=CARTESIAN_POINT('Origin',(-11.4022814987,-32.4742356128,-7.54785992694));
#51139=CARTESIAN_POINT('',(-12.7650943916,-32.5742356128,-8.87635684058));
#51140=CARTESIAN_POINT('',(-12.7650943916,-34.4242356128,-8.87635684058));
#51141=CARTESIAN_POINT('',(-0.390065459879,-32.5742356128,3.18706567889));
#51142=CARTESIAN_POINT('Origin',(-12.9745045801,-36.2742356128,-8.66153744443));
#51143=CARTESIAN_POINT('',(-13.2240142836,-36.2742356128,-8.82810547221));
#51144=CARTESIAN_POINT('Origin',(-13.1408443824,-36.2742356128,-8.77258279628));
#51145=CARTESIAN_POINT('Origin',(-12.9745045801,-36.2742356128,-8.66153744443));
#51146=CARTESIAN_POINT('Origin',(-12.9745045801,-34.4242356128,-8.66153744443));
#51147=CARTESIAN_POINT('',(-13.2240142836,-32.5742356128,-8.82810547221));
#51148=CARTESIAN_POINT('',(-13.2240142836,-34.4242356128,-8.82810547221));
#51149=CARTESIAN_POINT('Origin',(-12.9745045801,-32.5742356128,-8.66153744443));
#51150=CARTESIAN_POINT('Origin',(5.55235792516E-15,-36.2742356128,2.24172262308E-15));
#51151=CARTESIAN_POINT('',(-14.1979138053,-36.2742356128,-7.15746069337));
#51152=CARTESIAN_POINT('Origin',(-14.1086187499,-36.2742356128,-7.11244521731));
#51153=CARTESIAN_POINT('Origin',(-1.55306943244E-15,-36.2742356128,4.65365783676E-16));
#51154=CARTESIAN_POINT('Origin',(-1.09995011675E-15,-34.4242356128,2.38806125834E-16));
#51155=CARTESIAN_POINT('',(-14.1979138053,-32.5742356128,-7.15746069337));
#51156=CARTESIAN_POINT('',(-14.1979138053,-34.4242356128,-7.15746069337));
#51157=CARTESIAN_POINT('Origin',(1.12952603833E-15,-32.5742356128,1.22464679915E-17));
#51158=CARTESIAN_POINT('Origin',(-13.7514385284,-36.2742356128,-6.93238331308));
#51159=CARTESIAN_POINT('',(-14.2514385284,-36.2742356128,-6.93238331308));
#51160=CARTESIAN_POINT('Origin',(-14.1514385284,-36.2742356128,-6.93238331308));
#51161=CARTESIAN_POINT('Origin',(-13.7514385284,-36.2742356128,-6.93238331308));
#51162=CARTESIAN_POINT('Origin',(-13.7514385284,-34.4242356128,-6.93238331308));
#51163=CARTESIAN_POINT('',(-14.2514385284,-32.5742356128,-6.93238331308));
#51164=CARTESIAN_POINT('',(-14.2514385284,-34.4242356128,-6.93238331308));
#51165=CARTESIAN_POINT('Origin',(-13.7514385284,-32.5742356128,-6.93238331308));
#51166=CARTESIAN_POINT('Origin',(-14.1514385284,-36.2742356128,-4.73378838547E-15));
#51167=CARTESIAN_POINT('',(-14.2514385284,-36.2742356128,6.93238331308));
#51168=CARTESIAN_POINT('Origin',(-14.1514385284,-36.2742356128,6.93238331308));
#51169=CARTESIAN_POINT('',(-14.2514385284,-36.2742356128,-1.7763568394E-15));
#51170=CARTESIAN_POINT('Origin',(-14.2514385284,-32.4742356128,7.05028367309));
#51171=CARTESIAN_POINT('',(-14.2514385284,-32.5742356128,6.93238331308));
#51172=CARTESIAN_POINT('',(-14.2514385284,-34.4242356128,6.93238331308));
#51173=CARTESIAN_POINT('',(-14.2514385284,-32.5742356128,-3.5527136788E-15));
#51174=CARTESIAN_POINT('Origin',(-13.7514385284,-36.2742356128,6.93238331308));
#51175=CARTESIAN_POINT('',(-14.1979138053,-36.2742356128,7.15746069337));
#51176=CARTESIAN_POINT('Origin',(-14.1086187499,-36.2742356128,7.11244521731));
#51177=CARTESIAN_POINT('Origin',(-13.7514385284,-36.2742356128,6.93238331308));
#51178=CARTESIAN_POINT('Origin',(-13.7514385284,-34.4242356128,6.93238331308));
#51179=CARTESIAN_POINT('',(-14.1979138053,-32.5742356128,7.15746069337));
#51180=CARTESIAN_POINT('',(-14.1979138053,-34.4242356128,7.15746069337));
#51181=CARTESIAN_POINT('Origin',(-13.7514385284,-32.5742356128,6.93238331308));
#51182=CARTESIAN_POINT('Origin',(5.79114658385E-12,-36.2742356128,-3.26980757555E-12));
#51183=CARTESIAN_POINT('',(-13.5056315679,-36.2742356128,8.39094249493));
#51184=CARTESIAN_POINT('Origin',(-13.4206904888,-36.2742356128,8.33816927169));
#51185=CARTESIAN_POINT('Origin',(-1.55306943244E-15,-36.2742356128,4.65365783676E-16));
#51186=CARTESIAN_POINT('Origin',(-1.09995011675E-15,-34.4242356128,2.38806125834E-16));
#51187=CARTESIAN_POINT('',(-13.5056315679,-32.5742356128,8.39094249493));
#51188=CARTESIAN_POINT('',(-13.5056315679,-34.4242356128,8.39094249493));
#51189=CARTESIAN_POINT('Origin',(6.95023748177E-12,-32.5742356128,-3.88843287498E-12));
#51190=CARTESIAN_POINT('Origin',(-13.2508083307,-36.2742356128,8.23262282521));
#51191=CARTESIAN_POINT('',(-13.0413981423,-36.2742356128,8.44744222135));
#51192=CARTESIAN_POINT('Origin',(-13.1112015384,-36.2742356128,8.37583575597));
#51193=CARTESIAN_POINT('Origin',(-13.2508083307,-36.2742356128,8.23262282521));
#51194=CARTESIAN_POINT('Origin',(-13.2508083307,-34.4242356128,8.23262282521));
#51195=CARTESIAN_POINT('',(-13.0413981423,-32.5742356128,8.44744222135));
#51196=CARTESIAN_POINT('',(-13.0413981423,-34.4242356128,8.44744222135));
#51197=CARTESIAN_POINT('Origin',(-13.2508083307,-32.5742356128,8.23262282521));
#51198=CARTESIAN_POINT('Origin',(-0.818017619209,-36.2742356128,-3.60780262944));
#51199=CARTESIAN_POINT('',(-11.9661178757,-36.2742356128,7.39923778851));
#51200=CARTESIAN_POINT('Origin',(-12.0359212718,-36.2742356128,7.32763132313));
#51201=CARTESIAN_POINT('',(-12.5283819332,-36.2742356128,7.94734389244));
#51202=CARTESIAN_POINT('Origin',(-11.7512984795,-32.4742356128,7.18982760003));
#51203=CARTESIAN_POINT('',(-11.9661178757,-32.5742356128,7.39923778851));
#51204=CARTESIAN_POINT('',(-11.9661178757,-34.4242356128,7.39923778851));
#51205=CARTESIAN_POINT('',(-0.748214223049,-32.5742356128,-3.53619616406));
#51206=CARTESIAN_POINT('Origin',(-11.7567076872,-36.2742356128,7.61405718465));
#51207=CARTESIAN_POINT('',(-11.541888291,-36.2742356128,7.40464699617));
#51208=CARTESIAN_POINT('Origin',(-11.4702818256,-36.2742356128,7.33484360001));
#51209=CARTESIAN_POINT('Origin',(-11.7567076872,-36.2742356128,7.61405718465));
#51210=CARTESIAN_POINT('Origin',(-11.7567076872,-34.4242356128,7.61405718465));
#51211=CARTESIAN_POINT('',(-11.541888291,-32.5742356128,7.40464699617));
#51212=CARTESIAN_POINT('',(-11.541888291,-34.4242356128,7.40464699617));
#51213=CARTESIAN_POINT('Origin',(-11.7567076872,-32.5742356128,7.61405718465));
#51214=CARTESIAN_POINT('Origin',(-8.43647932171,-36.2742356128,10.447011287));
#51215=CARTESIAN_POINT('',(-7.83590804694,-36.2742356128,11.2063552317));
#51216=CARTESIAN_POINT('Origin',(-7.76430158156,-36.2742356128,11.1365518355));
#51217=CARTESIAN_POINT('',(-9.68889816899,-36.2742356128,9.30550111394));
#51218=CARTESIAN_POINT('Origin',(-11.4022814987,-32.4742356128,7.54785992694));
#51219=CARTESIAN_POINT('',(-7.83590804694,-32.5742356128,11.2063552317));
#51220=CARTESIAN_POINT('',(-7.83590804694,-34.4242356128,11.2063552317));
#51221=CARTESIAN_POINT('',(-8.50808578709,-32.5742356128,10.5168146831));
#51222=CARTESIAN_POINT('Origin',(-8.73768936184,-36.2742356128,12.9233426255));
#51223=CARTESIAN_POINT('',(-8.94709955032,-36.2742356128,12.7085232294));
#51224=CARTESIAN_POINT('Origin',(-8.73768936184,-36.2742356128,12.9233426255));
#51225=CARTESIAN_POINT('Origin',(-8.87729615416,-36.2742356128,12.7801296947));
#51226=CARTESIAN_POINT('Origin',(-8.73768936184,-34.4242356128,12.9233426255));
#51227=CARTESIAN_POINT('',(-8.94709955032,-32.5742356128,12.7085232294));
#51228=CARTESIAN_POINT('Origin',(-8.73768936184,-32.5742356128,12.9233426255));
#51229=CARTESIAN_POINT('',(-8.94709955032,-34.4242356128,12.7085232294));
#51230=CARTESIAN_POINT('Origin',(-8.05072744309,-36.2742356128,11.4157654202));
#51231=CARTESIAN_POINT('',(-7.84131725461,-36.2742356128,11.6305848163));
#51232=CARTESIAN_POINT('Origin',(-7.77151385845,-36.2742356128,11.7021912817));
#51233=CARTESIAN_POINT('Origin',(-8.05072744309,-36.2742356128,11.4157654202));
#51234=CARTESIAN_POINT('Origin',(-8.05072744309,-34.4242356128,11.4157654202));
#51235=CARTESIAN_POINT('',(-7.84131725461,-32.5742356128,11.6305848163));
#51236=CARTESIAN_POINT('',(-7.84131725461,-34.4242356128,11.6305848163));
#51237=CARTESIAN_POINT('Origin',(-8.05072744309,-32.5742356128,11.4157654202));
#51238=CARTESIAN_POINT('Origin',(0.67498798988,-36.2742356128,3.46837452298));
#51239=CARTESIAN_POINT('',(-8.41710184852,-36.2742356128,12.191871006));
#51240=CARTESIAN_POINT('Origin',(-7.62649785846,-32.4742356128,11.4211746278));
#51241=CARTESIAN_POINT('',(0.60518459372,-32.5742356128,3.3967680576));
#51242=CARTESIAN_POINT('Origin',(-12.7514385284,-32.4742356128,7.05028367309));
#51243=CARTESIAN_POINT('',(-12.7514385284,-32.4742356128,6.07000095416));
#51244=CARTESIAN_POINT('',(-12.7514385284,-32.8742356128,6.07000095416));
#51245=CARTESIAN_POINT('',(-12.7514385284,-32.6742356128,6.07000095416));
#51246=CARTESIAN_POINT('',(-12.7514385284,-32.8742356128,-6.7682619245));
#51247=CARTESIAN_POINT('',(-12.7514385284,-32.8742356128,-5.3290705182E-15));
#51248=CARTESIAN_POINT('',(-12.7514385284,-32.4742356128,-6.7682619245));
#51249=CARTESIAN_POINT('',(-12.7514385284,-33.6742356128,-6.7682619245));
#51250=CARTESIAN_POINT('',(-12.7514385284,-32.4742356128,-0.349130485171));
#51251=CARTESIAN_POINT('Ctrl Pts',(-1.87043161103,-35.3742356128,-8.24476960824));
#51252=CARTESIAN_POINT('Ctrl Pts',(-0.881024471639,-32.4742356128,-9.12211895883));
#51253=CARTESIAN_POINT('Ctrl Pts',(-1.76698369017,-35.3742356128,-8.26339468616));
#51254=CARTESIAN_POINT('Ctrl Pts',(-0.751586859387,-32.4742356128,-9.0904082994));
#51255=CARTESIAN_POINT('Ctrl Pts',(-1.65525765665,-35.3742356128,-8.23673498884));
#51256=CARTESIAN_POINT('Ctrl Pts',(-0.632864708596,-32.4742356128,-9.01561057704));
#51257=CARTESIAN_POINT('Ctrl Pts',(-1.56310817921,-35.3742356128,-8.15928174403));
#51258=CARTESIAN_POINT('Ctrl Pts',(-0.544519454171,-32.4742356128,-8.90337130527));
#51259=CARTESIAN_POINT('Ctrl Pts',(-1.51727343488,-35.3742356128,-8.05439924541));
#51260=CARTESIAN_POINT('Ctrl Pts',(-0.500000005883,-32.4742356128,-8.76992589769));
#51261=CARTESIAN_POINT('Ctrl Pts',(-1.51727342606,-35.3742356128,-7.9495168227));
#51262=CARTESIAN_POINT('Ctrl Pts',(-0.5,-32.4742356128,-8.63648038577));
#51263=CARTESIAN_POINT('',(-1.46144760572984,-35.2150897285804,-7.9872159489329));
#51264=CARTESIAN_POINT('',(-0.5,-32.4742356128,-8.63648038577));
#51265=CARTESIAN_POINT('',(-1.461447583,-35.2150896638,-7.98721594967));
#51266=CARTESIAN_POINT('',(-0.881024471639,-32.4742356128,-9.12211895883));
#51267=CARTESIAN_POINT('Ctrl Pts',(-0.881024471639,-32.4742356128,-9.12211895883));
#51268=CARTESIAN_POINT('Ctrl Pts',(-0.827016089126107,-32.4742356128,-9.10888755418313));
#51269=CARTESIAN_POINT('Ctrl Pts',(-0.775540637915395,-32.4742356128,-9.08673032516009));
#51270=CARTESIAN_POINT('Ctrl Pts',(-0.682134270020785,-32.4742356128,-9.02649837726588));
#51271=CARTESIAN_POINT('Ctrl Pts',(-0.640813901103346,-32.4742356141908,
-8.98885840070038));
#51272=CARTESIAN_POINT('Ctrl Pts',(-0.57228055336198,-32.4742356141908,
-8.901510263898));
#51273=CARTESIAN_POINT('Ctrl Pts',(-0.545563385694432,-32.4742356128,-8.85244719394298));
#51274=CARTESIAN_POINT('Ctrl Pts',(-0.509276617611063,-32.4742356128,-8.74739553291418));
#51275=CARTESIAN_POINT('Ctrl Pts',(-0.500000002452142,-32.4742356128,-8.69210290609089));
#51276=CARTESIAN_POINT('Ctrl Pts',(-0.5,-32.4742356128,-8.63648038577));
#51277=CARTESIAN_POINT('',(-1.83110023521525,-35.2589537682581,-8.27964633186293));
#51278=CARTESIAN_POINT('',(-1.83110005118,-35.2589529157,-8.27964657357));
#51279=CARTESIAN_POINT('Ctrl Pts',(-1.46144762641058,-35.2150897875193,
-7.98721596760513));
#51280=CARTESIAN_POINT('Ctrl Pts',(-1.45999274413531,-35.2109422616504,
-8.00191902509857));
#51281=CARTESIAN_POINT('Ctrl Pts',(-1.45957341091662,-35.2071571950236,
-8.01670884221526));
#51282=CARTESIAN_POINT('Ctrl Pts',(-1.46026191644033,-35.203764095227,-8.03143220521763));
#51283=CARTESIAN_POINT('Ctrl Pts',(-1.46096768768079,-35.2002859063528,
-8.04652478735688));
#51284=CARTESIAN_POINT('Ctrl Pts',(-1.46283764504754,-35.1972195789501,
-8.06154670605974));
#51285=CARTESIAN_POINT('Ctrl Pts',(-1.46590012256396,-35.1945898968725,
-8.07630792772827));
#51286=CARTESIAN_POINT('Ctrl Pts',(-1.46903420709223,-35.1918987274289,
-8.0914142970654));
#51287=CARTESIAN_POINT('Ctrl Pts',(-1.47341730681797,-35.1896648446532,
-8.10624662772912));
#51288=CARTESIAN_POINT('Ctrl Pts',(-1.47902730659165,-35.1879077839919,
-8.1205895819562));
#51289=CARTESIAN_POINT('Ctrl Pts',(-1.48166047777195,-35.1870830706796,
-8.1273217486647));
#51290=CARTESIAN_POINT('Ctrl Pts',(-1.48456319805496,-35.1863633079977,
-8.13394603229644));
#51291=CARTESIAN_POINT('Ctrl Pts',(-1.48772926757142,-35.1857500185123,
-8.14044030456528));
#51292=CARTESIAN_POINT('Ctrl Pts',(-1.49433115834809,-35.1844711867696,
-8.15398216647638));
#51293=CARTESIAN_POINT('Ctrl Pts',(-1.5020813773099,-35.1836556215759,-8.16695799089605));
#51294=CARTESIAN_POINT('Ctrl Pts',(-1.51088863668741,-35.1833130708024,
-8.17917555169671));
#51295=CARTESIAN_POINT('Ctrl Pts',(-1.51677966584951,-35.1830839442933,
-8.18734767470132));
#51296=CARTESIAN_POINT('Ctrl Pts',(-1.52314264543556,-35.1830663220979,
-8.19518080428534));
#51297=CARTESIAN_POINT('Ctrl Pts',(-1.52993884840686,-35.18326173225,-8.20262371909327));
#51298=CARTESIAN_POINT('Ctrl Pts',(-1.5396630145576,-35.1835413296656,-8.21327321566418));
#51299=CARTESIAN_POINT('Ctrl Pts',(-1.55027411075703,-35.1842571031188,
-8.22312066676176));
#51300=CARTESIAN_POINT('Ctrl Pts',(-1.56163020662216,-35.1854101081919,
-8.23204589669893));
#51301=CARTESIAN_POINT('Ctrl Pts',(-1.56997721952966,-35.1862575955979,
-8.23860616268935));
#51302=CARTESIAN_POINT('Ctrl Pts',(-1.57872600240808,-35.1873412311022,
-8.24466874427926));
#51303=CARTESIAN_POINT('Ctrl Pts',(-1.58780845871722,-35.1886604340494,
-8.25019966634848));
#51304=CARTESIAN_POINT('Ctrl Pts',(-1.6005630488647,-35.1905130048013,-8.25796679912947));
#51305=CARTESIAN_POINT('Ctrl Pts',(-1.6139737807599,-35.1928321347006,-8.26468081127607));
#51306=CARTESIAN_POINT('Ctrl Pts',(-1.6278554617678,-35.1955968415854,-8.27028675557324));
#51307=CARTESIAN_POINT('Ctrl Pts',(-1.64227743897151,-35.1984691550787,
-8.27611089177209));
#51308=CARTESIAN_POINT('Ctrl Pts',(-1.65720660407866,-35.2018228868763,
-8.28073943848053));
#51309=CARTESIAN_POINT('Ctrl Pts',(-1.67243049904531,-35.2056328375554,
-8.28416822709316));
#51310=CARTESIAN_POINT('Ctrl Pts',(-1.68794439477149,-35.2095153641812,
-8.28766233087671));
#51311=CARTESIAN_POINT('Ctrl Pts',(-1.70376300691381,-35.2138722198964,
-8.28991123800377));
#51312=CARTESIAN_POINT('Ctrl Pts',(-1.71967583215399,-35.2186669738979,
-8.29096015927791));
#51313=CARTESIAN_POINT('Ctrl Pts',(-1.72516869832638,-35.2203220503323,
-8.29132223100918));
#51314=CARTESIAN_POINT('Ctrl Pts',(-1.73067300845718,-35.2220291797313,
-8.29154169905675));
#51315=CARTESIAN_POINT('Ctrl Pts',(-1.73618094824065,-35.2237864091028,
-8.29162151774592));
#51316=CARTESIAN_POINT('Ctrl Pts',(-1.75076469988551,-35.2284391463775,
-8.2918328591885));
#51317=CARTESIAN_POINT('Ctrl Pts',(-1.76537892989469,-35.2334500139743,
-8.29106239128857));
#51318=CARTESIAN_POINT('Ctrl Pts',(-1.77988835203768,-35.2387691032084,
-8.28937964173054));
#51319=CARTESIAN_POINT('Ctrl Pts',(-1.79299811300231,-35.2435750829173,
-8.28785921974187));
#51320=CARTESIAN_POINT('Ctrl Pts',(-1.8060221558571,-35.2486326175861,-8.28559474347183));
#51321=CARTESIAN_POINT('Ctrl Pts',(-1.81889037024243,-35.2538888283575,
-8.28265208359663));
#51322=CARTESIAN_POINT('Ctrl Pts',(-1.82241578493209,-35.2553288356585,
-8.28184590365277));
#51323=CARTESIAN_POINT('Ctrl Pts',(-1.82592932282104,-35.2567834218319,
-8.28098898477275));
#51324=CARTESIAN_POINT('Ctrl Pts',(-1.82942950902499,-35.2582510471779,
-8.28008297427468));
#51325=CARTESIAN_POINT('Ctrl Pts',(-1.82998637759462,-35.258484541735,-8.27993883086609));
#51326=CARTESIAN_POINT('Ctrl Pts',(-1.83054294259533,-35.2587183799279,
-8.27979343760619));
#51327=CARTESIAN_POINT('Ctrl Pts',(-1.83110005096932,-35.2589529154682,
-8.27964657215517));
#51328=CARTESIAN_POINT('Origin',(-1.51727342606,-35.3742356128,-6.62635333853281));
#51329=CARTESIAN_POINT('',(-1.46090316329,-35.2135376551,-5.30645216923));
#51330=CARTESIAN_POINT('',(-0.5,-32.4742356128,-5.26505293156));
#51331=CARTESIAN_POINT('',(-1.46090316329,-35.2135376551,-5.30645216923));
#51332=CARTESIAN_POINT('',(-0.5,-32.4742356128,-5.26505293156));
#51333=CARTESIAN_POINT('',(-1.46090089616294,-35.2135311920909,-7.94951678979554));
#51334=CARTESIAN_POINT('Origin',(-2.99786357884902,-39.5950398533888,-7.94865516340226));
#51335=CARTESIAN_POINT('',(-1.46090316329,-35.2135376551,-5.30645216923));
#51336=CARTESIAN_POINT('Ctrl Pts',(-2.06618662358,-35.3742356128,-8.20763292551));
#51337=CARTESIAN_POINT('Ctrl Pts',(-1.13092983125,-32.4742356128,-9.11903336658));
#51338=CARTESIAN_POINT('Ctrl Pts',(-2.02728693019,-35.3742356128,-8.21539237438));
#51339=CARTESIAN_POINT('Ctrl Pts',(-1.08254865919,-32.4742356128,-9.13216050293));
#51340=CARTESIAN_POINT('Ctrl Pts',(-1.98835267261,-35.3742356128,-8.22296816028));
#51341=CARTESIAN_POINT('Ctrl Pts',(-1.03251986746,-32.4742356128,-9.13922496193));
#51342=CARTESIAN_POINT('Ctrl Pts',(-1.94830447917,-35.3742356128,-8.23056358523));
#51343=CARTESIAN_POINT('Ctrl Pts',(-0.980045978296,-32.4742356128,-9.13989363405));
#51344=CARTESIAN_POINT('Ctrl Pts',(-1.90939289225,-35.3742356128,-8.23775490438));
#51345=CARTESIAN_POINT('Ctrl Pts',(-0.929775106566,-32.4742356128,-9.13406227499));
#51346=CARTESIAN_POINT('Ctrl Pts',(-1.87043161103,-35.3742356128,-8.24476960824));
#51347=CARTESIAN_POINT('Ctrl Pts',(-0.881024471639,-32.4742356128,-9.12211895883));
#51348=CARTESIAN_POINT('',(-1.13092983125,-32.4742356128,-9.11903336658));
#51349=CARTESIAN_POINT('Ctrl Pts',(-0.881024471639,-32.4742356128,-9.12211895883));
#51350=CARTESIAN_POINT('Ctrl Pts',(-0.92220301191105,-32.4742356128,-9.13220720334646));
#51351=CARTESIAN_POINT('Ctrl Pts',(-0.964264740457436,-32.474235612914,
-9.13687601377793));
#51352=CARTESIAN_POINT('Ctrl Pts',(-1.04807641455819,-32.474235612914,-9.13584112130989));
#51353=CARTESIAN_POINT('Ctrl Pts',(-1.09001172345298,-32.4742356128,-9.13013556930401));
#51354=CARTESIAN_POINT('Ctrl Pts',(-1.13092983125,-32.4742356128,-9.11903336658));
#51355=CARTESIAN_POINT('',(-2.02882224805641,-35.258377357075,-8.24404435912867));
#51356=CARTESIAN_POINT('',(-2.02882173043,-35.2583763205,-8.24404472212));
#51357=CARTESIAN_POINT('',(-1.88461534275654,-35.2526204926692,-8.27242221793694));
#51358=CARTESIAN_POINT('Ctrl Pts',(-1.88461534316216,-35.2526204924197,
-8.27242222025263));
#51359=CARTESIAN_POINT('Ctrl Pts',(-1.91265386025649,-35.2529892698862,
-8.26755066673147));
#51360=CARTESIAN_POINT('Ctrl Pts',(-1.94082131994964,-35.2537157453151,
-8.26234408725425));
#51361=CARTESIAN_POINT('Ctrl Pts',(-1.96909946479954,-35.2548039079099,
-8.25679923395567));
#51362=CARTESIAN_POINT('Ctrl Pts',(-1.99780133897712,-35.2563733143722,
-8.2508227750941));
#51363=CARTESIAN_POINT('Ctrl Pts',(-2.02658489036,-35.258233098,-8.24453400819));
#51364=CARTESIAN_POINT('Ctrl Pts',(-2.02732982489,-35.2582811474,-8.24437112291));
#51365=CARTESIAN_POINT('Ctrl Pts',(-2.02807537275,-35.2583289394,-8.24420802987));
#51366=CARTESIAN_POINT('Ctrl Pts',(-2.02882173043,-35.2583763205,-8.24404472212));
#51367=CARTESIAN_POINT('Origin',(-1.87243909403022,-35.4444729230294,-8.21860710030529));
#51368=CARTESIAN_POINT('Ctrl Pts',(-8.90408048591,-35.3742356128,-3.33175685019));
#51369=CARTESIAN_POINT('Ctrl Pts',(-9.78972512979,-32.4742356128,-2.88747118331));
#51370=CARTESIAN_POINT('Ctrl Pts',(-8.6873937464,-35.3742356128,-3.78156218415));
#51371=CARTESIAN_POINT('Ctrl Pts',(-9.44154892618,-32.4742356128,-3.40960230403));
#51372=CARTESIAN_POINT('Ctrl Pts',(-8.41228804471,-35.3742356128,-4.20311089247));
#51373=CARTESIAN_POINT('Ctrl Pts',(-9.06633060557,-32.4742356128,-3.9138589137));
#51374=CARTESIAN_POINT('Ctrl Pts',(-8.09063109224,-35.3742356128,-4.59678365893));
#51375=CARTESIAN_POINT('Ctrl Pts',(-8.6592141531,-32.4742356128,-4.40538764451));
#51376=CARTESIAN_POINT('Ctrl Pts',(-7.360622472,-35.3742356128,-5.38465519647));
#51377=CARTESIAN_POINT('Ctrl Pts',(-7.74414150515,-32.4742356128,-5.40001779324));
#51378=CARTESIAN_POINT('Ctrl Pts',(-6.54392160985,-35.3742356128,-6.08248533528));
#51379=CARTESIAN_POINT('Ctrl Pts',(-6.72376489891,-32.4742356128,-6.28784412471));
#51380=CARTESIAN_POINT('Ctrl Pts',(-6.08996440487,-35.3742356128,-6.43395446983));
#51381=CARTESIAN_POINT('Ctrl Pts',(-6.15045388192,-32.4742356128,-6.72961730824));
#51382=CARTESIAN_POINT('Ctrl Pts',(-5.07098217764,-35.3742356128,-7.12903795521));
#51383=CARTESIAN_POINT('Ctrl Pts',(-4.8659622122,-32.4742356128,-7.60280558321));
#51384=CARTESIAN_POINT('Ctrl Pts',(-3.96068628695,-35.3742356128,-7.66774624913));
#51385=CARTESIAN_POINT('Ctrl Pts',(-3.47975995949,-32.4742356128,-8.30623076748));
#51386=CARTESIAN_POINT('Ctrl Pts',(-3.34362139801,-35.3742356128,-7.90067576649));
#51387=CARTESIAN_POINT('Ctrl Pts',(-2.71614717835,-32.4742356128,-8.63027694049));
#51388=CARTESIAN_POINT('Ctrl Pts',(-2.70966555084,-35.3742356128,-8.07927608136));
#51389=CARTESIAN_POINT('Ctrl Pts',(-1.93124535238,-32.4742356128,-8.90188586102));
#51390=CARTESIAN_POINT('Ctrl Pts',(-2.06618662358,-35.3742356128,-8.20763292551));
#51391=CARTESIAN_POINT('Ctrl Pts',(-1.13092983125,-32.4742356128,-9.11903336658));
#51392=CARTESIAN_POINT('',(-9.78972512979,-32.4742356128,-2.88747118331));
#51393=CARTESIAN_POINT('Ctrl Pts',(-1.13092983125,-32.4742356128,-9.11903336658));
#51394=CARTESIAN_POINT('Ctrl Pts',(-1.35748096440087,-32.4742356128002,
-9.05756384343984));
#51395=CARTESIAN_POINT('Ctrl Pts',(-1.58257164660585,-32.4742356128003,
-8.99085150410091));
#51396=CARTESIAN_POINT('Ctrl Pts',(-1.80593829563056,-32.4742356128004,
-8.91898444731663));
#51397=CARTESIAN_POINT('Ctrl Pts',(-2.06358605409587,-32.4742356128005,
-8.83608762199012));
#51398=CARTESIAN_POINT('Ctrl Pts',(-2.31894092044636,-32.4742356128005,
-8.74633156326516));
#51399=CARTESIAN_POINT('Ctrl Pts',(-2.57167018297851,-32.4742356128005,
-8.6498360378973));
#51400=CARTESIAN_POINT('Ctrl Pts',(-2.87961762633398,-32.4742356128005,
-8.53225744792893));
#51401=CARTESIAN_POINT('Ctrl Pts',(-3.18367140744747,-32.4742356128005,
-8.40466930268279));
#51402=CARTESIAN_POINT('Ctrl Pts',(-3.48328763307677,-32.4742356128004,
-8.26730091093105));
#51403=CARTESIAN_POINT('Ctrl Pts',(-3.71568832582298,-32.4742356128003,
-8.16074957400834));
#51404=CARTESIAN_POINT('Ctrl Pts',(-3.94542176433015,-32.4742356128003,
-8.0483135945673));
#51405=CARTESIAN_POINT('Ctrl Pts',(-4.17221459820387,-32.4742356128002,
-7.93012756314153));
#51406=CARTESIAN_POINT('Ctrl Pts',(-4.3691051862723,-32.4742356128002,-7.82752415706631));
#51407=CARTESIAN_POINT('Ctrl Pts',(-4.56378009094538,-32.4742356128001,
-7.72058696590365));
#51408=CARTESIAN_POINT('Ctrl Pts',(-4.75602733655703,-32.4742356128001,
-7.60942955096299));
#51409=CARTESIAN_POINT('Ctrl Pts',(-4.81482808842437,-32.4742356128001,
-7.57543093863777));
#51410=CARTESIAN_POINT('Ctrl Pts',(-4.87340144129883,-32.4742356128001,
-7.54103772494405));
#51411=CARTESIAN_POINT('Ctrl Pts',(-4.93174048144869,-32.4742356128001,
-7.50625373162201));
#51412=CARTESIAN_POINT('Ctrl Pts',(-5.17371609272893,-32.4742356128,-7.36197850828535));
#51413=CARTESIAN_POINT('Ctrl Pts',(-5.41165903155182,-32.4742356128,-7.21097959772054));
#51414=CARTESIAN_POINT('Ctrl Pts',(-5.64521361977431,-32.4742356128,-7.0534854983882));
#51415=CARTESIAN_POINT('Ctrl Pts',(-5.92854786582719,-32.4742356128,-6.86242321940786));
#51416=CARTESIAN_POINT('Ctrl Pts',(-6.20541886627958,-32.4742356128,-6.66180293529635));
#51417=CARTESIAN_POINT('Ctrl Pts',(-6.47520523011177,-32.4742356128,-6.45207607376425));
#51418=CARTESIAN_POINT('Ctrl Pts',(-6.7042174903774,-32.4742356128001,-6.27404623594872));
#51419=CARTESIAN_POINT('Ctrl Pts',(-6.92812568553406,-32.4742356128001,
-6.08945471655604));
#51420=CARTESIAN_POINT('Ctrl Pts',(-7.14656401932481,-32.4742356128001,
-5.89860434351618));
#51421=CARTESIAN_POINT('Ctrl Pts',(-7.30145174556248,-32.4742356128002,
-5.76327836927544));
#51422=CARTESIAN_POINT('Ctrl Pts',(-7.4535896236381,-32.4742356128002,-5.62480608682023));
#51423=CARTESIAN_POINT('Ctrl Pts',(-7.60284952378423,-32.4742356128003,
-5.48330473081067));
#51424=CARTESIAN_POINT('Ctrl Pts',(-7.66409102798865,-32.4742356128003,
-5.42524656595522));
#51425=CARTESIAN_POINT('Ctrl Pts',(-7.72484844931582,-32.4742356128003,
-5.36667817449847));
#51426=CARTESIAN_POINT('Ctrl Pts',(-7.78511221664714,-32.4742356128003,
-5.30760881482714));
#51427=CARTESIAN_POINT('Ctrl Pts',(-7.86083082414573,-32.4742356128003,
-5.23339092473813));
#51428=CARTESIAN_POINT('Ctrl Pts',(-7.9357705171939,-32.4742356128004,-5.1583808441567));
#51429=CARTESIAN_POINT('Ctrl Pts',(-8.00994285087825,-32.4742356128004,
-5.08255688170474));
#51430=CARTESIAN_POINT('Ctrl Pts',(-8.09229096248547,-32.4742356128004,
-4.99837508759984));
#51431=CARTESIAN_POINT('Ctrl Pts',(-8.17369314495629,-32.4742356128004,
-4.91319009037416));
#51432=CARTESIAN_POINT('Ctrl Pts',(-8.25412492760548,-32.4742356128004,
-4.82702704996663));
#51433=CARTESIAN_POINT('Ctrl Pts',(-8.31333790947206,-32.4742356128004,
-4.76359478002089));
#51434=CARTESIAN_POINT('Ctrl Pts',(-8.37202401218054,-32.4742356128004,
-4.69963371548019));
#51435=CARTESIAN_POINT('Ctrl Pts',(-8.43016285000587,-32.4742356128004,
-4.63516899165583));
#51436=CARTESIAN_POINT('Ctrl Pts',(-8.45791646133128,-32.4742356128004,
-4.60439560580666));
#51437=CARTESIAN_POINT('Ctrl Pts',(-8.48554521988306,-32.4742356128004,
-4.57350770746612));
#51438=CARTESIAN_POINT('Ctrl Pts',(-8.51305689825755,-32.4742356128004,
-4.54249677272974));
#51439=CARTESIAN_POINT('Ctrl Pts',(-8.62342507636421,-32.4742356128004,
-4.41809068155457));
#51440=CARTESIAN_POINT('Ctrl Pts',(-8.7318733436495,-32.4742356128004,-4.29174315144362));
#51441=CARTESIAN_POINT('Ctrl Pts',(-8.8382486463566,-32.4742356128004,-4.16363335145393));
#51442=CARTESIAN_POINT('Ctrl Pts',(-8.93277342320662,-32.4742356128004,
-4.04979536511541));
#51443=CARTESIAN_POINT('Ctrl Pts',(-9.02565819435723,-32.4742356128005,
-3.93456977982075));
#51444=CARTESIAN_POINT('Ctrl Pts',(-9.11679326953606,-32.4742356128005,
-3.81808802140576));
#51445=CARTESIAN_POINT('Ctrl Pts',(-9.19450142462868,-32.4742356128005,
-3.7187675069868));
#51446=CARTESIAN_POINT('Ctrl Pts',(-9.2709365589139,-32.4742356128005,-3.61853483930442));
#51447=CARTESIAN_POINT('Ctrl Pts',(-9.34605185297795,-32.4742356128005,
-3.51744756155323));
#51448=CARTESIAN_POINT('Ctrl Pts',(-9.41503263776077,-32.4742356128005,
-3.42461587078078));
#51449=CARTESIAN_POINT('Ctrl Pts',(-9.48289988060696,-32.4742356128004,
-3.33106404763001));
#51450=CARTESIAN_POINT('Ctrl Pts',(-9.54964545463381,-32.4742356128004,
-3.23680385237855));
#51451=CARTESIAN_POINT('Ctrl Pts',(-9.6112390224299,-32.4742356128003,-3.14981948208372));
#51452=CARTESIAN_POINT('Ctrl Pts',(-9.67187720579196,-32.4742356128002,
-3.0622321188807));
#51453=CARTESIAN_POINT('Ctrl Pts',(-9.73158294374893,-32.4742356128001,
-2.97401646795334));
#51454=CARTESIAN_POINT('Ctrl Pts',(-9.75106213192314,-32.4742356128001,
-2.94523582938955));
#51455=CARTESIAN_POINT('Ctrl Pts',(-9.77044232827666,-32.4742356128,-2.91638800950429));
#51456=CARTESIAN_POINT('Ctrl Pts',(-9.78972512979,-32.4742356128,-2.88747118331));
#51457=CARTESIAN_POINT('',(-8.93444612284907,-35.274804900368,-3.31652382194753));
#51458=CARTESIAN_POINT('',(-8.93444623808,-35.2748044449,-3.31652380097));
#51459=CARTESIAN_POINT('Ctrl Pts',(-2.02882232648753,-35.2583763371521,
-8.24404459697176));
#51460=CARTESIAN_POINT('Ctrl Pts',(-2.76037088316413,-35.278813606438,-8.09044863214831));
#51461=CARTESIAN_POINT('Ctrl Pts',(-3.46770779566994,-35.2977417662847,
-7.87807502189995));
#51462=CARTESIAN_POINT('Ctrl Pts',(-4.14485661336304,-35.3130519325903,
-7.60417976937799));
#51463=CARTESIAN_POINT('Ctrl Pts',(-5.21843933075938,-35.3262967397835,
-7.04499008624918));
#51464=CARTESIAN_POINT('Ctrl Pts',(-6.21090480851,-35.3291957718,-6.34191684905));
#51465=CARTESIAN_POINT('Ctrl Pts',(-6.59524089295,-35.3292320711,-6.04038307893));
#51466=CARTESIAN_POINT('Ctrl Pts',(-7.36674621113887,-35.3292429117998,
-5.37908304420829));
#51467=CARTESIAN_POINT('Ctrl Pts',(-8.06644389763777,-35.3242511580814,
-4.63577834525724));
#51468=CARTESIAN_POINT('Ctrl Pts',(-8.40676936045737,-35.3182542216342,
-4.22563367825667));
#51469=CARTESIAN_POINT('Ctrl Pts',(-8.69862023264536,-35.3007569336673,
-3.78649459696414));
#51470=CARTESIAN_POINT('Ctrl Pts',(-8.93444619651196,-35.2748044494745,
-3.31652388380974));
#51471=CARTESIAN_POINT('Ctrl Pts',(-8.98669828191,-35.3742356128,-3.15062625521));
#51472=CARTESIAN_POINT('Ctrl Pts',(-9.87176476169,-32.4742356128,-2.65438916225));
#51473=CARTESIAN_POINT('Ctrl Pts',(-8.97105229548,-35.3742356128,-3.18695239061));
#51474=CARTESIAN_POINT('Ctrl Pts',(-9.86736571705,-32.4742356128,-2.70382530588));
#51475=CARTESIAN_POINT('Ctrl Pts',(-8.95501903475,-35.3742356128,-3.22311199053));
#51476=CARTESIAN_POINT('Ctrl Pts',(-9.85683264819,-32.4742356128,-2.75271530399));
#51477=CARTESIAN_POINT('Ctrl Pts',(-8.93801024352,-35.3742356128,-3.26038797601));
#51478=CARTESIAN_POINT('Ctrl Pts',(-9.83970156009,-32.4742356128,-2.80141079064));
#51479=CARTESIAN_POINT('Ctrl Pts',(-8.92122822926,-35.3742356128,-3.29616101079));
#51480=CARTESIAN_POINT('Ctrl Pts',(-9.81727888481,-32.4742356128,-2.84615108413));
#51481=CARTESIAN_POINT('Ctrl Pts',(-8.90408048591,-35.3742356128,-3.33175685019));
#51482=CARTESIAN_POINT('Ctrl Pts',(-9.78972512979,-32.4742356128,-2.88747118331));
#51483=CARTESIAN_POINT('Ctrl Pts',(-9.78972512979,-32.4742356128,-2.88747118331));
#51484=CARTESIAN_POINT('Ctrl Pts',(-9.81295258958151,-32.4742356128,-2.85263887310081));
#51485=CARTESIAN_POINT('Ctrl Pts',(-9.83153874678994,-32.4742356128027,
-2.81516874991383));
#51486=CARTESIAN_POINT('Ctrl Pts',(-9.85907250391396,-32.4742356128027,
-2.7369427829564));
#51487=CARTESIAN_POINT('Ctrl Pts',(-9.86805391767536,-32.4742356128,-2.69609135731934));
#51488=CARTESIAN_POINT('Ctrl Pts',(-9.87176476169,-32.4742356128,-2.65438916225));
#51489=CARTESIAN_POINT('Ctrl Pts',(-8.93444605304206,-35.2748053537063,
-3.31652375104877));
#51490=CARTESIAN_POINT('Ctrl Pts',(-8.93943078683952,-35.2740356286657,
-3.30669402651363));
#51491=CARTESIAN_POINT('Ctrl Pts',(-8.94434451549187,-35.2733172975681,
-3.29686734543151));
#51492=CARTESIAN_POINT('Ctrl Pts',(-8.94920331673012,-35.272662843585,-3.28699914163946));
#51493=CARTESIAN_POINT('Ctrl Pts',(-8.95476993132043,-35.2719130510102,
-3.27569337206476));
#51494=CARTESIAN_POINT('Ctrl Pts',(-8.96026410692822,-35.2712477134621,
-3.26433342692446));
#51495=CARTESIAN_POINT('Ctrl Pts',(-8.96568233550565,-35.2706790956147,
-3.25291618430066));
#51496=CARTESIAN_POINT('Ctrl Pts',(-8.97215912488461,-35.2699993867427,
-3.23926835185764));
#51497=CARTESIAN_POINT('Ctrl Pts',(-8.97852587883437,-35.2694597776266,
-3.22554062845691));
#51498=CARTESIAN_POINT('Ctrl Pts',(-8.98475365565657,-35.2690516336245,
-3.21179689045617));
#51499=CARTESIAN_POINT('Ctrl Pts',(-8.98837874704945,-35.2688140593904,
-3.203796875723));
#51500=CARTESIAN_POINT('Ctrl Pts',(-8.99195645868942,-35.2686203376525,
-3.19579252489701));
#51501=CARTESIAN_POINT('Ctrl Pts',(-8.99548252093106,-35.2684610193862,
-3.18779854474187));
#51502=CARTESIAN_POINT('Ctrl Pts',(-8.99854073311971,-35.2683228400148,
-3.18086523333927));
#51503=CARTESIAN_POINT('Ctrl Pts',(-9.00156177291394,-35.2682167859986,
-3.17393229744647));
#51504=CARTESIAN_POINT('Ctrl Pts',(-9.00454520265064,-35.2681414577284,
-3.1670013767672));
#51505=CARTESIAN_POINT('Ctrl Pts',(-9.00705208603224,-35.2680781617218,
-3.16117753930374));
#51506=CARTESIAN_POINT('Ctrl Pts',(-9.00953172445309,-35.2680334238437,
-3.15535857579231));
#51507=CARTESIAN_POINT('Ctrl Pts',(-9.01198468982812,-35.2680064936339,
-3.14954401027304));
#51508=CARTESIAN_POINT('Ctrl Pts',(-9.01387857125029,-35.2679857014023,
-3.14505471020912));
#51509=CARTESIAN_POINT('Ctrl Pts',(-9.01575650600665,-35.2679752542737,
-3.14056830801862));
#51510=CARTESIAN_POINT('Ctrl Pts',(-9.01762235287468,-35.2679892318977,
-3.1360680066287));
#51511=CARTESIAN_POINT('Ctrl Pts',(-9.01812186455268,-35.267992973891,-3.13486321692313));
#51512=CARTESIAN_POINT('Ctrl Pts',(-9.01862041750448,-35.2679978846909,
-3.13365798589397));
#51513=CARTESIAN_POINT('Ctrl Pts',(-9.01911868766448,-35.2680072166355,
-3.13244884927113));
#51514=CARTESIAN_POINT('Ctrl Pts',(-3.51985615629,-35.3742356128,-3.20601908088));
#51515=CARTESIAN_POINT('Ctrl Pts',(-3.1350457731,-32.4742356128,-2.57376246377));
#51516=CARTESIAN_POINT('Ctrl Pts',(-3.5389561844,-35.3742356128,-3.1668368061));
#51517=CARTESIAN_POINT('Ctrl Pts',(-3.17276903042,-32.4742356128,-2.53334077836));
#51518=CARTESIAN_POINT('Ctrl Pts',(-3.56517269185,-35.3742356128,-3.13112318899));
#51519=CARTESIAN_POINT('Ctrl Pts',(-3.21038331308,-32.4742356128,-2.49281798697));
#51520=CARTESIAN_POINT('Ctrl Pts',(-3.59940527056,-35.3742356128,-3.09917422736));
#51521=CARTESIAN_POINT('Ctrl Pts',(-3.24932685202,-32.4742356128,-2.45063230102));
#51522=CARTESIAN_POINT('Ctrl Pts',(-3.63699355357,-35.3742356128,-3.07546800882));
#51523=CARTESIAN_POINT('Ctrl Pts',(-3.28665002885,-32.4742356128,-2.40998048911));
#51524=CARTESIAN_POINT('Ctrl Pts',(-3.67755401867,-35.3742356128,-3.05915055738));
#51525=CARTESIAN_POINT('Ctrl Pts',(-3.32386409198,-32.4742356128,-2.36922853848));
#51526=CARTESIAN_POINT('',(-3.66207294828794,-35.2473021021,-3.02895254909137));
#51527=CARTESIAN_POINT('',(-3.32386409198,-32.4742356128,-2.36922853848));
#51528=CARTESIAN_POINT('',(-3.66207294829203,-35.247302102094,-3.02895254911367));
#51529=CARTESIAN_POINT('',(-3.1350457731,-32.4742356128,-2.57376246377));
#51530=CARTESIAN_POINT('Origin',(15.769898679409,-32.4742355606854,15.0680202722476));
#51531=CARTESIAN_POINT('',(-3.50597898793362,-35.2696545343368,-3.18321829788018));
#51532=CARTESIAN_POINT('',(-3.50597895501,-35.2696545374,-3.18321836469));
#51533=CARTESIAN_POINT('Ctrl Pts',(-3.66207294827955,-35.2473021021057,
-3.02895254907185));
#51534=CARTESIAN_POINT('Ctrl Pts',(-3.66091495179321,-35.2473795704993,
-3.02947323796857));
#51535=CARTESIAN_POINT('Ctrl Pts',(-3.65976226369913,-35.2474575947881,
-3.0300000109274));
#51536=CARTESIAN_POINT('Ctrl Pts',(-3.65861281967912,-35.2475362729335,
-3.03053380228582));
#51537=CARTESIAN_POINT('Ctrl Pts',(-3.65240605310862,-35.2479611190979,
-3.03341616828313));
#51538=CARTESIAN_POINT('Ctrl Pts',(-3.6463111786709,-35.2484032769964,-3.03649530323666));
#51539=CARTESIAN_POINT('Ctrl Pts',(-3.64031422873348,-35.248862763431,-3.03977928431773));
#51540=CARTESIAN_POINT('Ctrl Pts',(-3.6322888734286,-35.2494776663289,-3.04417403752813));
#51541=CARTESIAN_POINT('Ctrl Pts',(-3.62443677559274,-35.2501213489573,
-3.04893623763928));
#51542=CARTESIAN_POINT('Ctrl Pts',(-3.61676784831451,-35.2508052779905,
-3.05406683233371));
#51543=CARTESIAN_POINT('Ctrl Pts',(-3.60730204981363,-35.2516494553026,
-3.06039955317002));
#51544=CARTESIAN_POINT('Ctrl Pts',(-3.59811807272275,-35.2525562450447,
-3.06729452529451));
#51545=CARTESIAN_POINT('Ctrl Pts',(-3.58929693635001,-35.2535534756824,
-3.0747059316244));
#51546=CARTESIAN_POINT('Ctrl Pts',(-3.58809950408998,-35.2536888455583,
-3.0757119989446));
#51547=CARTESIAN_POINT('Ctrl Pts',(-3.58690878465367,-35.2538258680597,
-3.07672751152805));
#51548=CARTESIAN_POINT('Ctrl Pts',(-3.58572498566927,-35.253964593268,-3.07775228998077));
#51549=CARTESIAN_POINT('Ctrl Pts',(-3.57769765100733,-35.2549052881722,
-3.08470130725703));
#51550=CARTESIAN_POINT('Ctrl Pts',(-3.56999072711075,-35.2559268700649,
-3.09207839837468));
#51551=CARTESIAN_POINT('Ctrl Pts',(-3.56268644817232,-35.2570395958347,
-3.09981180666564));
#51552=CARTESIAN_POINT('Ctrl Pts',(-3.55508194090727,-35.2581980580555,
-3.10786308181927));
#51553=CARTESIAN_POINT('Ctrl Pts',(-3.54791482463172,-35.2594544673558,
-3.11629765460186));
#51554=CARTESIAN_POINT('Ctrl Pts',(-3.54124405919227,-35.2607842073526,
-3.12502681208725));
#51555=CARTESIAN_POINT('Ctrl Pts',(-3.54078309233966,-35.2608760957674,
-3.12563001906379));
#51556=CARTESIAN_POINT('Ctrl Pts',(-3.54032447922608,-35.2609683237252,
-3.1262346405582));
#51557=CARTESIAN_POINT('Ctrl Pts',(-3.53986823173921,-35.2610608787453,
-3.12684065180599));
#51558=CARTESIAN_POINT('Ctrl Pts',(-3.53401616594948,-35.262248037212,-3.13461366490414));
#51559=CARTESIAN_POINT('Ctrl Pts',(-3.5285556873506,-35.263490013451,-3.1426127338717));
#51560=CARTESIAN_POINT('Ctrl Pts',(-3.52349535751664,-35.2647552260756,
-3.15080332732354));
#51561=CARTESIAN_POINT('Ctrl Pts',(-3.51892135499415,-35.2658988443625,
-3.15820675681106));
#51562=CARTESIAN_POINT('Ctrl Pts',(-3.51467414707485,-35.2670609744409,
-3.16576608898576));
#51563=CARTESIAN_POINT('Ctrl Pts',(-3.51073522720237,-35.2682166399343,
-3.1734916718749));
#51564=CARTESIAN_POINT('Ctrl Pts',(-3.50940929552838,-35.2686056637103,
-3.1760922820382));
#51565=CARTESIAN_POINT('Ctrl Pts',(-3.50811808179657,-35.2689939686856,
-3.17871208941865));
#51566=CARTESIAN_POINT('Ctrl Pts',(-3.50686019645209,-35.2693806830338,
-3.18135268706089));
#51567=CARTESIAN_POINT('Ctrl Pts',(-3.50656455234841,-35.269471573525,-3.18197331367565));
#51568=CARTESIAN_POINT('Ctrl Pts',(-3.50627078919946,-35.2695623867448,
-3.1825950147686));
#51569=CARTESIAN_POINT('Ctrl Pts',(-3.50597901251073,-35.2696545195266,
-3.18321824197148));
#51570=CARTESIAN_POINT('Ctrl Pts',(-7.21384189758,-35.3742356128,2.18958432614));
#51571=CARTESIAN_POINT('Ctrl Pts',(-7.92659403983,-32.4742356128,4.74000601033));
#51572=CARTESIAN_POINT('Ctrl Pts',(-7.26623945249,-35.3742356128,2.28696407666));
#51573=CARTESIAN_POINT('Ctrl Pts',(-7.98210778857,-32.4742356128,4.86805404157));
#51574=CARTESIAN_POINT('Ctrl Pts',(-7.33077888815,-35.3742356128,2.37781046265));
#51575=CARTESIAN_POINT('Ctrl Pts',(-8.06503365985,-32.4742356128,4.98421786182));
#51576=CARTESIAN_POINT('Ctrl Pts',(-7.40436869293,-35.3742356128,2.46126398331));
#51577=CARTESIAN_POINT('Ctrl Pts',(-8.17216612273,-32.4742356128,5.0807589417));
#51578=CARTESIAN_POINT('Ctrl Pts',(-7.56704033307,-35.3742356128,2.61160417272));
#51579=CARTESIAN_POINT('Ctrl Pts',(-8.41851793763,-32.4742356128,5.22052728604));
#51580=CARTESIAN_POINT('Ctrl Pts',(-7.76385631892,-35.3742356128,2.71310420624));
#51581=CARTESIAN_POINT('Ctrl Pts',(-8.70021558456,-32.4742356128,5.24806936162));
#51582=CARTESIAN_POINT('Ctrl Pts',(-7.87246551919,-35.3742356128,2.74929666995));
#51583=CARTESIAN_POINT('Ctrl Pts',(-8.84211900681,-32.4742356128,5.23137961658));
#51584=CARTESIAN_POINT('Ctrl Pts',(-8.09632446877,-35.3742356128,2.75144961057));
#51585=CARTESIAN_POINT('Ctrl Pts',(-9.10596900702,-32.4742356128,5.14052628192));
#51586=CARTESIAN_POINT('Ctrl Pts',(-8.29201770973,-35.3742356128,2.64306639111));
#51587=CARTESIAN_POINT('Ctrl Pts',(-9.31107389815,-32.4742356128,4.95155477014));
#51588=CARTESIAN_POINT('Ctrl Pts',(-8.37411601908,-35.3742356128,2.57138954697));
#51589=CARTESIAN_POINT('Ctrl Pts',(-9.39185739171,-32.4742356128,4.83723274541));
#51590=CARTESIAN_POINT('Ctrl Pts',(-8.4486251678,-35.3742356128,2.49348119172));
#51591=CARTESIAN_POINT('Ctrl Pts',(-9.44632201614,-32.4742356128,4.7098382487));
#51592=CARTESIAN_POINT('Ctrl Pts',(-8.51721509197,-35.3742356128,2.41066261776));
#51593=CARTESIAN_POINT('Ctrl Pts',(-9.47312185748,-32.4742356128,4.57687569684));
#51594=CARTESIAN_POINT('',(-8.6009108248196,-35.120322107747,2.60032839187079));
#51595=CARTESIAN_POINT('',(-9.47312185748,-32.4742356128,4.57687569684));
#51596=CARTESIAN_POINT('',(-8.60091083126,-35.1203221009,2.60032840073));
#51597=CARTESIAN_POINT('',(-7.92659403983,-32.4742356128,4.74000601033));
#51598=CARTESIAN_POINT('Ctrl Pts',(-9.47312185748,-32.4742356128,4.57687569684));
#51599=CARTESIAN_POINT('Ctrl Pts',(-9.46576357172862,-32.4742356128,4.61338249695149));
#51600=CARTESIAN_POINT('Ctrl Pts',(-9.45589852782759,-32.4742356128,4.64938312384879));
#51601=CARTESIAN_POINT('Ctrl Pts',(-9.4436151767327,-32.4742356128001,4.68454468695718));
#51602=CARTESIAN_POINT('Ctrl Pts',(-9.43116790267184,-32.4742356128001,
4.72017548583586));
#51603=CARTESIAN_POINT('Ctrl Pts',(-9.41623764589746,-32.4742356128001,
4.75494407050594));
#51604=CARTESIAN_POINT('Ctrl Pts',(-9.39896958249035,-32.4742356128001,
4.78851518953424));
#51605=CARTESIAN_POINT('Ctrl Pts',(-9.38152489595556,-32.4742356128002,
4.82242968441788));
#51606=CARTESIAN_POINT('Ctrl Pts',(-9.36169469208315,-32.4742356128002,
4.85512144315062));
#51607=CARTESIAN_POINT('Ctrl Pts',(-9.33967747672362,-32.4742356128002,
4.88626565542905));
#51608=CARTESIAN_POINT('Ctrl Pts',(-9.32473727646168,-32.4742356128002,
4.90739915305088));
#51609=CARTESIAN_POINT('Ctrl Pts',(-9.30879106644691,-32.4742356128002,
4.92782051201125));
#51610=CARTESIAN_POINT('Ctrl Pts',(-9.29191215925214,-32.4742356128002,
4.94743594307661));
#51611=CARTESIAN_POINT('Ctrl Pts',(-9.26807208685844,-32.4742356128001,
4.97514113105093));
#51612=CARTESIAN_POINT('Ctrl Pts',(-9.2423551960503,-32.4742356128002,5.00125358349318));
#51613=CARTESIAN_POINT('Ctrl Pts',(-9.21499925935546,-32.4742356128004,
5.02552229400269));
#51614=CARTESIAN_POINT('Ctrl Pts',(-9.18812489694226,-32.4742356128005,
5.04936377780233));
#51615=CARTESIAN_POINT('Ctrl Pts',(-9.15966921110771,-32.4742356128007,
5.07142540239296));
#51616=CARTESIAN_POINT('Ctrl Pts',(-9.12988757458161,-32.4742356128009,
5.09150932334396));
#51617=CARTESIAN_POINT('Ctrl Pts',(-9.1177306388397,-32.474235612801,5.09970762823674));
#51618=CARTESIAN_POINT('Ctrl Pts',(-9.10535306806464,-32.474235612801,5.1075768984626));
#51619=CARTESIAN_POINT('Ctrl Pts',(-9.09277339742187,-32.4742356128011,
5.11510591129192));
#51620=CARTESIAN_POINT('Ctrl Pts',(-9.06401134948185,-32.4742356128012,
5.13232017978011));
#51621=CARTESIAN_POINT('Ctrl Pts',(-9.03418916029184,-32.4742356128013,
5.1477537113724));
#51622=CARTESIAN_POINT('Ctrl Pts',(-9.00352034950314,-32.4742356128012,
5.1612883287322));
#51623=CARTESIAN_POINT('Ctrl Pts',(-8.98613398992056,-32.4742356128012,
5.16896119631913));
#51624=CARTESIAN_POINT('Ctrl Pts',(-8.9684764199063,-32.4742356128011,5.17602435236192));
#51625=CARTESIAN_POINT('Ctrl Pts',(-8.95059220546224,-32.474235612801,5.1824608849134));
#51626=CARTESIAN_POINT('Ctrl Pts',(-8.91460611802292,-32.4742356128007,
5.19541228537485));
#51627=CARTESIAN_POINT('Ctrl Pts',(-8.8776867278997,-32.4742356128005,5.20582893332123));
#51628=CARTESIAN_POINT('Ctrl Pts',(-8.84020622755982,-32.4742356128004,
5.21361149973278));
#51629=CARTESIAN_POINT('Ctrl Pts',(-8.80212100914067,-32.4742356128002,
5.22151963166691));
#51630=CARTESIAN_POINT('Ctrl Pts',(-8.76345811848754,-32.4742356128002,
5.22670768415973));
#51631=CARTESIAN_POINT('Ctrl Pts',(-8.72463030839696,-32.4742356128002,
5.22912100680538));
#51632=CARTESIAN_POINT('Ctrl Pts',(-8.68739236868495,-32.4742356128002,
5.23143551187209));
#51633=CARTESIAN_POINT('Ctrl Pts',(-8.65000425691521,-32.4742356128002,
5.23119800092422));
#51634=CARTESIAN_POINT('Ctrl Pts',(-8.6128267026259,-32.4742356128003,5.22840604118267));
#51635=CARTESIAN_POINT('Ctrl Pts',(-8.58737790569537,-32.4742356128003,
5.22649488758855));
#51636=CARTESIAN_POINT('Ctrl Pts',(-8.56202769486349,-32.4742356128004,
5.22338772754605));
#51637=CARTESIAN_POINT('Ctrl Pts',(-8.53688547477249,-32.4742356128005,
5.21909660544825));
#51638=CARTESIAN_POINT('Ctrl Pts',(-8.50390469579943,-32.4742356128006,
5.21346764551782));
#51639=CARTESIAN_POINT('Ctrl Pts',(-8.47128746528097,-32.4742356128007,
5.20580045842078));
#51640=CARTESIAN_POINT('Ctrl Pts',(-8.4392653732531,-32.4742356128007,5.19615646079357));
#51641=CARTESIAN_POINT('Ctrl Pts',(-8.43597511948344,-32.4742356128007,
5.19516554491213));
#51642=CARTESIAN_POINT('Ctrl Pts',(-8.43269111740371,-32.4742356128007,
5.19415379222059));
#51643=CARTESIAN_POINT('Ctrl Pts',(-8.42941359545578,-32.4742356128007,
5.19312129233961));
#51644=CARTESIAN_POINT('Ctrl Pts',(-8.3944144019285,-32.4742356128007,5.18209568710319));
#51645=CARTESIAN_POINT('Ctrl Pts',(-8.36015521648491,-32.4742356128006,
5.16869999519598));
#51646=CARTESIAN_POINT('Ctrl Pts',(-8.32695087107122,-32.4742356128006,
5.15305321371686));
#51647=CARTESIAN_POINT('Ctrl Pts',(-8.29319095413242,-32.4742356128005,
5.13714463197815));
#51648=CARTESIAN_POINT('Ctrl Pts',(-8.26052202447813,-32.4742356128004,
5.11890928463567));
#51649=CARTESIAN_POINT('Ctrl Pts',(-8.22925624736326,-32.4742356128004,
5.09852305936231));
#51650=CARTESIAN_POINT('Ctrl Pts',(-8.20513847568554,-32.4742356128003,
5.08279754821614));
#51651=CARTESIAN_POINT('Ctrl Pts',(-8.18185530346072,-32.4742356128002,
5.06579330067018));
#51652=CARTESIAN_POINT('Ctrl Pts',(-8.15953944897647,-32.4742356128002,
5.04760937719499));
#51653=CARTESIAN_POINT('Ctrl Pts',(-8.13000306159537,-32.4742356128001,
5.02354185120129));
#51654=CARTESIAN_POINT('Ctrl Pts',(-8.1021534308539,-32.4742356128001,4.99739923287759));
#51655=CARTESIAN_POINT('Ctrl Pts',(-8.07626720330521,-32.4742356128001,
4.96943994770265));
#51656=CARTESIAN_POINT('Ctrl Pts',(-8.0505351356036,-32.4742356128,4.94164716802253));
#51657=CARTESIAN_POINT('Ctrl Pts',(-8.0267436078806,-32.4742356128,4.91205976688404));
#51658=CARTESIAN_POINT('Ctrl Pts',(-8.00512575620472,-32.4742356128,4.88096523499291));
#51659=CARTESIAN_POINT('Ctrl Pts',(-7.98386071885989,-32.4742356128,4.85037818167243));
#51660=CARTESIAN_POINT('Ctrl Pts',(-7.96469932551459,-32.4742356128,4.81833327235114));
#51661=CARTESIAN_POINT('Ctrl Pts',(-7.94782028391973,-32.4742356128,4.78512968374919));
#51662=CARTESIAN_POINT('Ctrl Pts',(-7.94028653932774,-32.4742356128,4.77030968614097));
#51663=CARTESIAN_POINT('Ctrl Pts',(-7.93320686704621,-32.4742356128,4.75525915977829));
#51664=CARTESIAN_POINT('Ctrl Pts',(-7.92659403983,-32.4742356128,4.74000601033));
#51665=CARTESIAN_POINT('',(-7.23545016824,-35.2863172732,2.26690461571));
#51666=CARTESIAN_POINT('',(-7.23545016824,-35.2863172732,2.26690461571));
#51667=CARTESIAN_POINT('Ctrl Pts',(-8.60091083126,-35.1203221009,2.60032840073));
#51668=CARTESIAN_POINT('Ctrl Pts',(-8.56160117875,-35.1140346808,2.66060541831));
#51669=CARTESIAN_POINT('Ctrl Pts',(-8.51829161967,-35.1086508497,2.71924356476));
#51670=CARTESIAN_POINT('Ctrl Pts',(-8.47165311425,-35.1035435988,2.77475885702));
#51671=CARTESIAN_POINT('Ctrl Pts',(-8.35159188251,-35.0922845623,2.89275323394));
#51672=CARTESIAN_POINT('Ctrl Pts',(-8.20219946581,-35.0869079403,2.96964215712));
#51673=CARTESIAN_POINT('Ctrl Pts',(-8.10597427981,-35.0887550559,2.98941073315));
#51674=CARTESIAN_POINT('Ctrl Pts',(-7.82075728158,-35.1140008873,2.95981413055));
#51675=CARTESIAN_POINT('Ctrl Pts',(-7.56538653659,-35.1573736159,2.76989788484));
#51676=CARTESIAN_POINT('Ctrl Pts',(-7.43180190579,-35.1865123729,2.62065670169));
#51677=CARTESIAN_POINT('Ctrl Pts',(-7.32065041948,-35.231204862,2.4495725015));
#51678=CARTESIAN_POINT('Ctrl Pts',(-7.23545016824,-35.2863172732,2.26690461571));
#51679=CARTESIAN_POINT('Ctrl Pts',(-8.51721509197,-35.3742356128,2.41066261776));
#51680=CARTESIAN_POINT('Ctrl Pts',(-9.47312185748,-32.4742356128,4.57687569684));
#51681=CARTESIAN_POINT('Ctrl Pts',(-8.57124548357,-35.3742356128,2.34542388422));
#51682=CARTESIAN_POINT('Ctrl Pts',(-9.49423281845,-32.4742356128,4.47213748961));
#51683=CARTESIAN_POINT('Ctrl Pts',(-8.62160287869,-35.3742356128,2.27713826199));
#51684=CARTESIAN_POINT('Ctrl Pts',(-9.51478914505,-32.4742356128,4.367292468));
#51685=CARTESIAN_POINT('Ctrl Pts',(-8.66952448488,-35.3742356128,2.20708948255));
#51686=CARTESIAN_POINT('Ctrl Pts',(-9.53482564259,-32.4742356128,4.26215510362));
#51687=CARTESIAN_POINT('Ctrl Pts',(-8.71540499967,-35.3742356128,2.13579061508));
#51688=CARTESIAN_POINT('Ctrl Pts',(-9.55426490812,-32.4742356128,4.15713558997));
#51689=CARTESIAN_POINT('Ctrl Pts',(-8.75956299023,-35.3742356128,2.0634404101));
#51690=CARTESIAN_POINT('Ctrl Pts',(-9.5731487029,-32.4742356128,4.05201631342));
#51691=CARTESIAN_POINT('',(-8.82321718811955,-35.1473420531381,2.21902512680689));
#51692=CARTESIAN_POINT('',(-9.5731487029,-32.4742356128,4.05201631342));
#51693=CARTESIAN_POINT('',(-8.82321723512,-35.1473421125,2.21902487472));
#51694=CARTESIAN_POINT('Origin',(15.3007564523972,-32.4742356010378,-0.416450801703818));
#51695=CARTESIAN_POINT('Ctrl Pts',(-8.8232168869647,-35.1473420700646,2.219025543263));
#51696=CARTESIAN_POINT('Ctrl Pts',(-8.80526362682125,-35.145153271855,2.25350258409433));
#51697=CARTESIAN_POINT('Ctrl Pts',(-8.78684682703311,-35.1429249882693,
2.28803306323546));
#51698=CARTESIAN_POINT('Ctrl Pts',(-8.76791345287321,-35.1406440769323,
2.32254344633434));
#51699=CARTESIAN_POINT('Ctrl Pts',(-8.75132900856273,-35.138646142136,2.35277237023366));
#51700=CARTESIAN_POINT('Ctrl Pts',(-8.73434636716193,-35.1366097977285,
2.38298586372834));
#51701=CARTESIAN_POINT('Ctrl Pts',(-8.71692245297776,-35.1345191813108,
2.41310198813675));
#51702=CARTESIAN_POINT('Ctrl Pts',(-8.70215559144233,-35.1327473725865,
2.43862556650279));
#51703=CARTESIAN_POINT('Ctrl Pts',(-8.68707123431251,-35.1309370177603,
2.46407888932811));
#51704=CARTESIAN_POINT('Ctrl Pts',(-8.67165070386463,-35.1290601449782,
2.489389823811));
#51705=CARTESIAN_POINT('Ctrl Pts',(-8.66337872647115,-35.1280533411412,
2.50296727359835));
#51706=CARTESIAN_POINT('Ctrl Pts',(-8.65500395568259,-35.1270312044469,
2.51650713409901));
#51707=CARTESIAN_POINT('Ctrl Pts',(-8.64651908034742,-35.1259916049772,
2.52999652004439));
#51708=CARTESIAN_POINT('Ctrl Pts',(-8.63865177225743,-35.125027672215,2.54250408803862));
#51709=CARTESIAN_POINT('Ctrl Pts',(-8.63069362675025,-35.1240461475895,
2.55496615938241));
#51710=CARTESIAN_POINT('Ctrl Pts',(-8.62264312140985,-35.123042269789,2.56736795085125));
#51711=CARTESIAN_POINT('Ctrl Pts',(-8.61689703694199,-35.1223257474848,
2.57621978540321));
#51712=CARTESIAN_POINT('Ctrl Pts',(-8.61110407596,-35.1215977157902,2.58504077148982));
#51713=CARTESIAN_POINT('Ctrl Pts',(-8.60525029211926,-35.1208654219131,
2.59383214904833));
#51714=CARTESIAN_POINT('Ctrl Pts',(-8.60380709913618,-35.1206848820411,
2.59599957694612));
#51715=CARTESIAN_POINT('Ctrl Pts',(-8.60236297383733,-35.1205021342156,
2.59816380216256));
#51716=CARTESIAN_POINT('Ctrl Pts',(-8.60091081515229,-35.1203221010069,
2.60032838482467));
#51717=CARTESIAN_POINT('Ctrl Pts',(-8.75956299023,-35.3742356128,2.0634404101));
#51718=CARTESIAN_POINT('Ctrl Pts',(-9.5731487029,-32.4742356128,4.05201631342));
#51719=CARTESIAN_POINT('Ctrl Pts',(-8.92885481093,-35.3742356128,1.78606749512));
#51720=CARTESIAN_POINT('Ctrl Pts',(-9.64554465255,-32.4742356128,3.6490141658));
#51721=CARTESIAN_POINT('Ctrl Pts',(-9.07282740405,-35.3742356128,1.49324081294));
#51722=CARTESIAN_POINT('Ctrl Pts',(-9.70977650917,-32.4742356128,3.24454541193));
#51723=CARTESIAN_POINT('Ctrl Pts',(-9.12664920772,-35.3742356128,1.15116500779));
#51724=CARTESIAN_POINT('Ctrl Pts',(-9.76784884218,-32.4742356128,2.82302310552));
#51725=CARTESIAN_POINT('Ctrl Pts',(-9.18659879637,-35.3742356128,0.831334347991));
#51726=CARTESIAN_POINT('Ctrl Pts',(-9.8153632788,-32.4742356128,2.41643837733));
#51727=CARTESIAN_POINT('Ctrl Pts',(-9.23698117862,-35.3742356128,0.509886547138));
#51728=CARTESIAN_POINT('Ctrl Pts',(-9.85462053301,-32.4742356128,2.00920484002));
#51729=CARTESIAN_POINT('Ctrl Pts',(-9.5731487029,-32.4742356128,4.05201631342));
#51730=CARTESIAN_POINT('Ctrl Pts',(-9.58385803994689,-32.4742356128002,
3.99240129558575));
#51731=CARTESIAN_POINT('Ctrl Pts',(-9.5943536855861,-32.4742356128003,3.93274277792962));
#51732=CARTESIAN_POINT('Ctrl Pts',(-9.60464591256779,-32.4742356128005,
3.87295958919005));
#51733=CARTESIAN_POINT('Ctrl Pts',(-9.61549552175361,-32.4742356128006,
3.80993880322598));
#51734=CARTESIAN_POINT('Ctrl Pts',(-9.62611903415597,-32.4742356128007,
3.74677981964133));
#51735=CARTESIAN_POINT('Ctrl Pts',(-9.63652068269621,-32.4742356128008,
3.6834457777419));
#51736=CARTESIAN_POINT('Ctrl Pts',(-9.64770872862421,-32.4742356128009,
3.61532348281569));
#51737=CARTESIAN_POINT('Ctrl Pts',(-9.65864002597334,-32.4742356128009,
3.54699913843106));
#51738=CARTESIAN_POINT('Ctrl Pts',(-9.66931194496843,-32.4742356128009,
3.47848631183152));
#51739=CARTESIAN_POINT('Ctrl Pts',(-9.68148004640578,-32.474235612801,3.40036811919844));
#51740=CARTESIAN_POINT('Ctrl Pts',(-9.69331083177811,-32.474235612801,3.32200562453741));
#51741=CARTESIAN_POINT('Ctrl Pts',(-9.70479179824442,-32.4742356128009,
3.24348485468347));
#51742=CARTESIAN_POINT('Ctrl Pts',(-9.7201856722383,-32.4742356128009,3.13820287859019));
#51743=CARTESIAN_POINT('Ctrl Pts',(-9.73495007583227,-32.4742356128008,
3.03264005645671));
#51744=CARTESIAN_POINT('Ctrl Pts',(-9.74904466851698,-32.4742356128007,
2.92708814611483));
#51745=CARTESIAN_POINT('Ctrl Pts',(-9.75943548222614,-32.4742356128006,
2.84927318107526));
#51746=CARTESIAN_POINT('Ctrl Pts',(-9.7694618745955,-32.4742356128006,2.77146717702854));
#51747=CARTESIAN_POINT('Ctrl Pts',(-9.77911025980369,-32.4742356128005,
2.6937724200985));
#51748=CARTESIAN_POINT('Ctrl Pts',(-9.78779970867891,-32.4742356128004,
2.62379961079945));
#51749=CARTESIAN_POINT('Ctrl Pts',(-9.79618242234148,-32.4742356128003,
2.55391804485843));
#51750=CARTESIAN_POINT('Ctrl Pts',(-9.80425367824051,-32.4742356128003,
2.48416708378499));
#51751=CARTESIAN_POINT('Ctrl Pts',(-9.81180034779321,-32.4742356128002,
2.41894954381487));
#51752=CARTESIAN_POINT('Ctrl Pts',(-9.81907464790267,-32.4742356128002,
2.3538467998227));
#51753=CARTESIAN_POINT('Ctrl Pts',(-9.8260789591149,-32.4742356128001,2.28884751742815));
#51754=CARTESIAN_POINT('Ctrl Pts',(-9.83260578437975,-32.4742356128001,
2.22827925515725));
#51755=CARTESIAN_POINT('Ctrl Pts',(-9.83889814477805,-32.4742356128,2.16780107633691));
#51756=CARTESIAN_POINT('Ctrl Pts',(-9.84496431448896,-32.4742356128,2.10735907911607));
#51757=CARTESIAN_POINT('Ctrl Pts',(-9.84824849657925,-32.4742356128,2.07463620220455));
#51758=CARTESIAN_POINT('Ctrl Pts',(-9.85146649575577,-32.4742356128,2.041923117793));
#51759=CARTESIAN_POINT('Ctrl Pts',(-9.85462053301,-32.4742356128,2.00920484002));
#51760=CARTESIAN_POINT('',(-8.84972910932056,-35.1509197094744,2.16703888406964));
#51761=CARTESIAN_POINT('Ctrl Pts',(-8.84972757036633,-35.1509188455761,
2.16704273318452));
#51762=CARTESIAN_POINT('Ctrl Pts',(-8.84263701355718,-35.1498854734004,
2.18123269435607));
#51763=CARTESIAN_POINT('Ctrl Pts',(-8.83539046048538,-35.1488785397256,
2.19550438840577));
#51764=CARTESIAN_POINT('Ctrl Pts',(-8.82797601093741,-35.1479357210167,
2.20985097691311));
#51765=CARTESIAN_POINT('Ctrl Pts',(-8.82639727975385,-35.1477349701333,
2.2129057426793));
#51766=CARTESIAN_POINT('Ctrl Pts',(-8.82481106154748,-35.1475370463719,
2.21596377869292));
#51767=CARTESIAN_POINT('Ctrl Pts',(-8.82321740410989,-35.1473422016281,
2.21902486252055));
#51768=CARTESIAN_POINT('Ctrl Pts',(-9.26569102913818,-35.2394341100243,
0.579580104582361));
#51769=CARTESIAN_POINT('Ctrl Pts',(-9.26432897936841,-35.2391993937044,
0.588916840903954));
#51770=CARTESIAN_POINT('Ctrl Pts',(-9.26295526781442,-35.2389720582188,
0.598255150960743));
#51771=CARTESIAN_POINT('Ctrl Pts',(-9.26157088200535,-35.2387502154634,
0.607597401941648));
#51772=CARTESIAN_POINT('Ctrl Pts',(-9.25606802654771,-35.2378684030313,
0.644732322322909));
#51773=CARTESIAN_POINT('Ctrl Pts',(-9.25039903101778,-35.2370737660972,
0.681935582958867));
#51774=CARTESIAN_POINT('Ctrl Pts',(-9.24459515278581,-35.2362958421616,
0.719269900919489));
#51775=CARTESIAN_POINT('Ctrl Pts',(-9.23860144043817,-35.2354924737738,
0.757825355325635));
#51776=CARTESIAN_POINT('Ctrl Pts',(-9.23246358621943,-35.2347066278465,
0.796520371533143));
#51777=CARTESIAN_POINT('Ctrl Pts',(-9.22617547021298,-35.2338649909902,
0.835383081090787));
#51778=CARTESIAN_POINT('Ctrl Pts',(-9.21950775230034,-35.2329725460771,
0.876591860379445));
#51779=CARTESIAN_POINT('Ctrl Pts',(-9.21267081123946,-35.2320169111237,
0.917989042641703));
#51780=CARTESIAN_POINT('Ctrl Pts',(-9.20561664949873,-35.2309214566663,
0.959565403305954));
#51781=CARTESIAN_POINT('Ctrl Pts',(-9.20129161992591,-35.2302498144361,
0.985056595032471));
#51782=CARTESIAN_POINT('Ctrl Pts',(-9.19688415582833,-35.2295258515741,
1.0106143158295));
#51783=CARTESIAN_POINT('Ctrl Pts',(-9.19237714642468,-35.2287349082349,
1.0362297220611));
#51784=CARTESIAN_POINT('Ctrl Pts',(-9.18433806879567,-35.2273241157706,
1.08191949564519));
#51785=CARTESIAN_POINT('Ctrl Pts',(-9.17598329873894,-35.2256969838539,
1.12779875063943));
#51786=CARTESIAN_POINT('Ctrl Pts',(-9.16718884329799,-35.2237950554676,
1.17378828861314));
#51787=CARTESIAN_POINT('Ctrl Pts',(-9.15824445275229,-35.2218607014429,
1.22056189403028));
#51788=CARTESIAN_POINT('Ctrl Pts',(-9.14884412978376,-35.2196413404115,
1.26744866220585));
#51789=CARTESIAN_POINT('Ctrl Pts',(-9.13883756774077,-35.2171160563015,
1.31433550967857));
#51790=CARTESIAN_POINT('Ctrl Pts',(-9.12913301134297,-35.2146669871847,
1.35980727647108));
#51791=CARTESIAN_POINT('Ctrl Pts',(-9.11885715887533,-35.2119298210439,
1.40527813132619));
#51792=CARTESIAN_POINT('Ctrl Pts',(-9.10787101160138,-35.2089310791387,
1.4506315207492));
#51793=CARTESIAN_POINT('Ctrl Pts',(-9.10306272832524,-35.2076186262657,
1.47048124044086));
#51794=CARTESIAN_POINT('Ctrl Pts',(-9.09811845693115,-35.2062566994767,
1.49030836911984));
#51795=CARTESIAN_POINT('Ctrl Pts',(-9.09302722159328,-35.2048506613808,
1.51010300502406));
#51796=CARTESIAN_POINT('Ctrl Pts',(-9.08137976609742,-35.201634002739,1.55538811275342));
#51797=CARTESIAN_POINT('Ctrl Pts',(-9.0689621044373,-35.1981822931679,1.60050286270257));
#51798=CARTESIAN_POINT('Ctrl Pts',(-9.05566818026723,-35.1945757132466,
1.64531873653687));
#51799=CARTESIAN_POINT('Ctrl Pts',(-9.04311114502703,-35.1911690478716,
1.68765044385356));
#51800=CARTESIAN_POINT('Ctrl Pts',(-9.02977099290996,-35.1876254879663,
1.72971514826849));
#51801=CARTESIAN_POINT('Ctrl Pts',(-9.01559361637142,-35.1840385572175,
1.77140429309896));
#51802=CARTESIAN_POINT('Ctrl Pts',(-9.00271099223959,-35.1807792038035,
1.80928616650255));
#51803=CARTESIAN_POINT('Ctrl Pts',(-8.98913667424359,-35.1774848505479,
1.84685777318515));
#51804=CARTESIAN_POINT('Ctrl Pts',(-8.97487070089677,-35.1742336894979,
1.88404080636593));
#51805=CARTESIAN_POINT('Ctrl Pts',(-8.96340477304722,-35.1716206481638,
1.91392576165875));
#51806=CARTESIAN_POINT('Ctrl Pts',(-8.95149260611499,-35.1690357681137,
1.94355972733414));
#51807=CARTESIAN_POINT('Ctrl Pts',(-8.93915874000816,-35.1665192378142,
1.97290476540593));
#51808=CARTESIAN_POINT('Ctrl Pts',(-8.92511135651658,-35.1636530913943,
2.00632664625004));
#51809=CARTESIAN_POINT('Ctrl Pts',(-8.9105144674308,-35.1608758193711,2.03937607228335));
#51810=CARTESIAN_POINT('Ctrl Pts',(-8.89544878975767,-35.1582413753976,
2.07199872308543));
#51811=CARTESIAN_POINT('Ctrl Pts',(-8.8938366780672,-35.1579594751725,2.07548952900025));
#51812=CARTESIAN_POINT('Ctrl Pts',(-8.8922192469323,-35.15767920151,2.07897545514641));
#51813=CARTESIAN_POINT('Ctrl Pts',(-8.89059663078593,-35.1574006136199,
2.08245644010738));
#51814=CARTESIAN_POINT('Ctrl Pts',(-8.87729309257504,-35.155116521569,2.11099641029262));
#51815=CARTESIAN_POINT('Ctrl Pts',(-8.8636443139379,-35.1529474030868,2.13919120126784));
#51816=CARTESIAN_POINT('Ctrl Pts',(-8.84973117353,-35.1509193731,2.1670354781));
#51817=CARTESIAN_POINT('Origin',(12.4493324411,-32.4742356128,-6.47376294621));
#51818=CARTESIAN_POINT('',(12.4493324411,-32.4742356128,-6.47376294621));
#51819=CARTESIAN_POINT('',(12.4493324411,-32.8742356128,-6.47376294621));
#51820=CARTESIAN_POINT('',(12.4493324411,-32.6742356128,-6.47376294621));
#51821=CARTESIAN_POINT('',(12.4493324411,-32.8742356128,-6.47376294621));
#51822=CARTESIAN_POINT('',(12.6003854848,-32.4742356128,-6.62101243536));
#51823=CARTESIAN_POINT('Origin',(-12.4493324411,-32.4742356128,-6.47376294621));
#51824=CARTESIAN_POINT('',(-12.4493324411,-32.4742356128,-6.47376294621));
#51825=CARTESIAN_POINT('',(-12.6003854848,-32.4742356128,-6.62101243536));
#51826=CARTESIAN_POINT('',(-12.4493324411,-32.8742356128,-6.47376294621));
#51827=CARTESIAN_POINT('',(-12.7514385284,-32.8742356128,-6.7682619245));
#51828=CARTESIAN_POINT('',(-12.4493324411,-32.6742356128,-6.47376294621));
#51829=CARTESIAN_POINT('Ctrl Pts',(3.48890306473,-35.2652540838,-3.21461371005));
#51830=CARTESIAN_POINT('Ctrl Pts',(3.49935367494,-35.3079501575,-3.21504790568));
#51831=CARTESIAN_POINT('Ctrl Pts',(3.50770783242,-35.351170349,-3.21440294636));
#51832=CARTESIAN_POINT('Ctrl Pts',(3.51392345177,-35.3947427768,-3.21267707712));
#51833=CARTESIAN_POINT('Ctrl Pts',(3.51797541026,-35.4384913267,-3.20987727374));
#51834=CARTESIAN_POINT('Ctrl Pts',(3.51985615043,-35.4822398766,-3.20601907528));
#51835=CARTESIAN_POINT('Ctrl Pts',(3.24150677815,-35.2297273503,-3.67797056337));
#51836=CARTESIAN_POINT('Ctrl Pts',(3.25788366108,-35.2867834422,-3.68259788135));
#51837=CARTESIAN_POINT('Ctrl Pts',(3.2708619246,-35.3449131549,-3.6851550674));
#51838=CARTESIAN_POINT('Ctrl Pts',(3.28034612237,-35.4037663878,-3.68562224436));
#51839=CARTESIAN_POINT('Ctrl Pts',(3.28628025023,-35.4629813934,-3.68400243047));
#51840=CARTESIAN_POINT('Ctrl Pts',(3.28864951001,-35.5221963991,-3.68032135));
#51841=CARTESIAN_POINT('Ctrl Pts',(2.93020007641,-35.2159821642,-4.09471223066));
#51842=CARTESIAN_POINT('Ctrl Pts',(2.94976329618,-35.2791022779,-4.10741039029));
#51843=CARTESIAN_POINT('Ctrl Pts',(2.96507838407,-35.3440365738,-4.11671739461));
#51844=CARTESIAN_POINT('Ctrl Pts',(2.97596822887,-35.4101991223,-4.12255014873));
#51845=CARTESIAN_POINT('Ctrl Pts',(2.98233164479,-35.4769758456,-4.12487890497));
#51846=CARTESIAN_POINT('Ctrl Pts',(2.984147828,-35.543752569,-4.12372796686));
#51847=CARTESIAN_POINT('Ctrl Pts',(2.57349039398,-35.21650702,-4.45141980073));
#51848=CARTESIAN_POINT('Ctrl Pts',(2.58535390407,-35.2792535748,-4.47101557567));
#51849=CARTESIAN_POINT('Ctrl Pts',(2.59391358392,-35.3437511414,-4.48640413798));
#51850=CARTESIAN_POINT('Ctrl Pts',(2.59909669845,-35.4094332325,-4.49741590343));
#51851=CARTESIAN_POINT('Ctrl Pts',(2.60088024578,-35.4757076219,-4.50395318786));
#51852=CARTESIAN_POINT('Ctrl Pts',(2.59929137485,-35.5419820113,-4.50599426346));
#51853=CARTESIAN_POINT('Ctrl Pts',(2.15330460094,-35.2313461468,-4.76288665231));
#51854=CARTESIAN_POINT('Ctrl Pts',(2.15740174514,-35.2874140925,-4.77869293776));
#51855=CARTESIAN_POINT('Ctrl Pts',(2.15952364918,-35.3444755753,-4.7912469843));
#51856=CARTESIAN_POINT('Ctrl Pts',(2.15965446887,-35.4022061334,-4.8004623347));
#51857=CARTESIAN_POINT('Ctrl Pts',(2.15779886139,-35.4602712393,-4.80628788231));
#51858=CARTESIAN_POINT('Ctrl Pts',(2.15398176798,-35.5183363452,-4.80870937341));
#51859=CARTESIAN_POINT('Ctrl Pts',(1.69382497102,-35.2682575054,-5.0104353994));
#51860=CARTESIAN_POINT('Ctrl Pts',(1.69402180198,-35.3094041642,-5.02023545326));
#51861=CARTESIAN_POINT('Ctrl Pts',(1.69321049227,-35.3510179116,-5.02809462923));
#51862=CARTESIAN_POINT('Ctrl Pts',(1.69139030263,-35.3929453813,-5.0339763881));
#51863=CARTESIAN_POINT('Ctrl Pts',(1.68856804274,-35.4350297152,-5.03785872515));
#51864=CARTESIAN_POINT('Ctrl Pts',(1.68475791979,-35.477114049,-5.03973465917));
#51865=CARTESIAN_POINT('',(1.69382496789361,-35.2682576613344,-5.0104354398608));
#51866=CARTESIAN_POINT('Origin',(1.24303943910855,-35.4771140870975,-4.14258062935315));
#51867=CARTESIAN_POINT('',(3.48890306745266,-35.2652540841568,-3.21461371228527));
#51868=CARTESIAN_POINT('Ctrl Pts',(3.48890306460208,-35.2652540848695,-3.21461371081793));
#51869=CARTESIAN_POINT('Ctrl Pts',(3.44775130357986,-35.2593445965621,-3.29168823695534));
#51870=CARTESIAN_POINT('Ctrl Pts',(3.40380709382689,-35.2540719037323,-3.36847562230748));
#51871=CARTESIAN_POINT('Ctrl Pts',(3.35708951743242,-35.2494371435468,-3.44461007506016));
#51872=CARTESIAN_POINT('Ctrl Pts',(3.30985454838516,-35.2447510538393,-3.52158770953414));
#51873=CARTESIAN_POINT('Ctrl Pts',(3.2597844948942,-35.2407166455098,-3.59789767427568));
#51874=CARTESIAN_POINT('Ctrl Pts',(3.20687172401791,-35.2373316218687,-3.67320954173569));
#51875=CARTESIAN_POINT('Ctrl Pts',(3.15192353050766,-35.233816384791,-3.75141846934008));
#51876=CARTESIAN_POINT('Ctrl Pts',(3.09390910438811,-35.2310008789339,-3.82855109054718));
#51877=CARTESIAN_POINT('Ctrl Pts',(3.03279428228795,-35.2288868032877,-3.90429009496304));
#51878=CARTESIAN_POINT('Ctrl Pts',(2.96685035092806,-35.2266056797482,-3.98601376749996));
#51879=CARTESIAN_POINT('Ctrl Pts',(2.89729472225231,-35.2251402672288,-4.06611544111579));
#51880=CARTESIAN_POINT('Ctrl Pts',(2.82407449292744,-35.224509773473,-4.14425308595335));
#51881=CARTESIAN_POINT('Ctrl Pts',(2.79172464830231,-35.2242312114523,-4.17877552180443));
#51882=CARTESIAN_POINT('Ctrl Pts',(2.75865953861759,-35.224115929813,-4.21291522461585));
#51883=CARTESIAN_POINT('Ctrl Pts',(2.72487604324634,-35.2241673001316,-4.24664506250073));
#51884=CARTESIAN_POINT('Ctrl Pts',(2.65472562468747,-35.2242739690629,-4.31668406289263));
#51885=CARTESIAN_POINT('Ctrl Pts',(2.58276783092832,-35.2250970726848,-4.38366465920977));
#51886=CARTESIAN_POINT('Ctrl Pts',(2.50928836705134,-35.2266146759269,-4.44761232797486));
#51887=CARTESIAN_POINT('Ctrl Pts',(2.44121046007607,-35.2280207184712,-4.50685913267071));
#51888=CARTESIAN_POINT('Ctrl Pts',(2.37182601344067,-35.2300234573763,-4.56350349989407));
#51889=CARTESIAN_POINT('Ctrl Pts',(2.3014054178217,-35.2326174005493,-4.61756403780509));
#51890=CARTESIAN_POINT('Ctrl Pts',(2.23212377102363,-35.2351693905339,-4.67075022659467));
#51891=CARTESIAN_POINT('Ctrl Pts',(2.16183899809641,-35.2382939828071,-4.7214359382488));
#51892=CARTESIAN_POINT('Ctrl Pts',(2.09085658743666,-35.2419915887232,-4.76962725403854));
#51893=CARTESIAN_POINT('Ctrl Pts',(2.01848437800597,-35.2457615918445,-4.81876213078701));
#51894=CARTESIAN_POINT('Ctrl Pts',(1.94538686340585,-35.25012764269,-4.86530413139964));
#51895=CARTESIAN_POINT('Ctrl Pts',(1.87194092409075,-35.2550905119588,-4.90924276159168));
#51896=CARTESIAN_POINT('Ctrl Pts',(1.81272063931411,-35.2590921291231,-4.94467097201329));
#51897=CARTESIAN_POINT('Ctrl Pts',(1.75327501706489,-35.2634818477057,-4.97840619304004));
#51898=CARTESIAN_POINT('Ctrl Pts',(1.69382497176268,-35.2682576606557,-5.01043543637783));
#51899=CARTESIAN_POINT('Origin',(2.62096730277507,-35.4822399141373,-2.76784133732473));
#51900=CARTESIAN_POINT('Ctrl Pts',(1.65073607085,-35.2758272825,-5.03428274092));
#51901=CARTESIAN_POINT('Ctrl Pts',(1.65784980534,-35.3154856499,-5.03981034314));
#51902=CARTESIAN_POINT('Ctrl Pts',(1.66405083454,-35.3555597177,-5.04353006314));
#51903=CARTESIAN_POINT('Ctrl Pts',(1.66931464207,-35.3959128353,-5.04542284568));
#51904=CARTESIAN_POINT('Ctrl Pts',(1.67362302807,-35.4364054801,-5.0454821464));
#51905=CARTESIAN_POINT('Ctrl Pts',(1.67696448333,-35.4768981249,-5.04371406628));
#51906=CARTESIAN_POINT('Ctrl Pts',(1.61326364266,-35.2619218696,-5.05000316771));
#51907=CARTESIAN_POINT('Ctrl Pts',(1.62236549352,-35.3070877788,-5.05662956819));
#51908=CARTESIAN_POINT('Ctrl Pts',(1.63007921825,-35.3528484277,-5.0610482607));
#51909=CARTESIAN_POINT('Ctrl Pts',(1.63636464034,-35.3990097556,-5.06322951683));
#51910=CARTESIAN_POINT('Ctrl Pts',(1.64119504878,-35.4453707616,-5.06316361876));
#51911=CARTESIAN_POINT('Ctrl Pts',(1.64455688984,-35.4917317677,-5.06086202998));
#51912=CARTESIAN_POINT('Ctrl Pts',(1.57763814761,-35.2502524393,-5.07162003768));
#51913=CARTESIAN_POINT('Ctrl Pts',(1.58925529962,-35.3001212511,-5.07894359568));
#51914=CARTESIAN_POINT('Ctrl Pts',(1.59886212553,-35.350806501,-5.08374537669));
#51915=CARTESIAN_POINT('Ctrl Pts',(1.60640164997,-35.4020401921,-5.08598819927));
#51916=CARTESIAN_POINT('Ctrl Pts',(1.6118338475,-35.4535491166,-5.08566006898));
#51917=CARTESIAN_POINT('Ctrl Pts',(1.61513825447,-35.505058041,-5.08277314744));
#51918=CARTESIAN_POINT('Ctrl Pts',(1.5467652741,-35.2408307961,-5.09796224817));
#51919=CARTESIAN_POINT('Ctrl Pts',(1.56082810828,-35.2948250485,-5.10559533807));
#51920=CARTESIAN_POINT('Ctrl Pts',(1.5721279205,-35.3498911181,-5.11056679276));
#51921=CARTESIAN_POINT('Ctrl Pts',(1.58057518036,-35.4056813318,-5.11281573481));
#51922=CARTESIAN_POINT('Ctrl Pts',(1.58611547612,-35.4618331019,-5.11233170678));
#51923=CARTESIAN_POINT('Ctrl Pts',(1.58873141496,-35.5179848719,-5.10914094848));
#51924=CARTESIAN_POINT('Ctrl Pts',(1.50094788409,-35.2255784603,-5.15114151002));
#51925=CARTESIAN_POINT('Ctrl Pts',(1.51919307915,-35.2853745424,-5.15844241592));
#51926=CARTESIAN_POINT('Ctrl Pts',(1.53333303669,-35.34668297,-5.16330955045));
#51927=CARTESIAN_POINT('Ctrl Pts',(1.54322139667,-35.4090153954,-5.16568966994));
#51928=CARTESIAN_POINT('Ctrl Pts',(1.54877729981,-35.471860276,-5.16555970229));
#51929=CARTESIAN_POINT('Ctrl Pts',(1.54998925981,-35.5347051565,-5.16293840519));
#51930=CARTESIAN_POINT('Ctrl Pts',(1.47301395752,-35.2164048258,-5.21579034781));
#51931=CARTESIAN_POINT('Ctrl Pts',(1.49420720065,-35.2792319381,-5.22072059065));
#51932=CARTESIAN_POINT('Ctrl Pts',(1.51037196702,-35.3438574448,-5.22412710654));
#51933=CARTESIAN_POINT('Ctrl Pts',(1.52131309724,-35.4097044807,-5.22595779822));
#51934=CARTESIAN_POINT('Ctrl Pts',(1.52692924844,-35.4761620333,-5.22619785569));
#51935=CARTESIAN_POINT('Ctrl Pts',(1.52721834654,-35.5426195859,-5.22486268019));
#51936=CARTESIAN_POINT('Ctrl Pts',(1.46470315626,-35.213766631,-5.24531814123));
#51937=CARTESIAN_POINT('Ctrl Pts',(1.48680690707,-35.277355512,-5.24884399471));
#51938=CARTESIAN_POINT('Ctrl Pts',(1.50361778858,-35.3428209065,-5.25131648121));
#51939=CARTESIAN_POINT('Ctrl Pts',(1.51492750077,-35.4095603027,-5.25272449316));
#51940=CARTESIAN_POINT('Ctrl Pts',(1.52062825527,-35.4769374515,-5.25304460068));
#51941=CARTESIAN_POINT('Ctrl Pts',(1.52071813077,-35.5443146003,-5.25227472437));
#51942=CARTESIAN_POINT('Ctrl Pts',(1.46069629729,-35.2129478838,-5.27610920663));
#51943=CARTESIAN_POINT('Ctrl Pts',(1.48316494179,-35.2768382352,-5.27796326442));
#51944=CARTESIAN_POINT('Ctrl Pts',(1.50022470946,-35.3426337834,-5.2792979259));
#51945=CARTESIAN_POINT('Ctrl Pts',(1.51165995618,-35.4097245745,-5.28008044471));
#51946=CARTESIAN_POINT('Ctrl Pts',(1.51736021529,-35.4774626159,-5.28030986048));
#51947=CARTESIAN_POINT('Ctrl Pts',(1.51732687674,-35.5452006575,-5.27999548691));
#51948=CARTESIAN_POINT('Ctrl Pts',(1.46090316329,-35.2135376551,-5.30645216923));
#51949=CARTESIAN_POINT('Ctrl Pts',(1.48323786433,-35.277208474,-5.30683297122));
#51950=CARTESIAN_POINT('Ctrl Pts',(1.50020219619,-35.3427631323,-5.30721377032));
#51951=CARTESIAN_POINT('Ctrl Pts',(1.51158410625,-35.4095977304,-5.30759095434));
#51952=CARTESIAN_POINT('Ctrl Pts',(1.51727462121,-35.4770723771,-5.30796091202));
#51953=CARTESIAN_POINT('Ctrl Pts',(1.51727394979,-35.5445470238,-5.30832023528));
#51954=CARTESIAN_POINT('',(1.46090316329,-35.2135376551,-5.30645216923));
#51955=CARTESIAN_POINT('Origin',(0.517242653608352,-35.5445510518349,-5.30645466752134));
#51956=CARTESIAN_POINT('',(1.65073615060969,-35.2758275456144,-5.03428276116372));
#51957=CARTESIAN_POINT('Ctrl Pts',(1.65073607085,-35.2758272825,-5.03428274092));
#51958=CARTESIAN_POINT('Ctrl Pts',(1.63917641294469,-35.2715376801465,-5.03913224666584));
#51959=CARTESIAN_POINT('Ctrl Pts',(1.62778335848467,-35.2674875132726,-5.04467326186675));
#51960=CARTESIAN_POINT('Ctrl Pts',(1.61668444443609,-35.2636573158247,-5.05087657242354));
#51961=CARTESIAN_POINT('Ctrl Pts',(1.60383194679254,-35.2592219626488,-5.05805998099526));
#51962=CARTESIAN_POINT('Ctrl Pts',(1.59137279284757,-35.2550802614962,-5.06613093554639));
#51963=CARTESIAN_POINT('Ctrl Pts',(1.57945190627886,-35.2511801020351,-5.07508134045879));
#51964=CARTESIAN_POINT('Ctrl Pts',(1.57822278811962,-35.2507779711374,-5.07600418333185));
#51965=CARTESIAN_POINT('Ctrl Pts',(1.57699936255477,-35.2503784044852,-5.0769364083727));
#51966=CARTESIAN_POINT('Ctrl Pts',(1.5757817713614,-35.249981345754,-5.0778780290884));
#51967=CARTESIAN_POINT('Ctrl Pts',(1.56892018406347,-35.2477437694955,-5.08318441827502));
#51968=CARTESIAN_POINT('Ctrl Pts',(1.56238122240745,-35.2456299610748,-5.08867791263399));
#51969=CARTESIAN_POINT('Ctrl Pts',(1.55606420538616,-35.2435937838966,-5.09443615432473));
#51970=CARTESIAN_POINT('Ctrl Pts',(1.54987411671174,-35.2415985197954,-5.10007869518765));
#51971=CARTESIAN_POINT('Ctrl Pts',(1.54389660825347,-35.2396777876347,-5.10597582340282));
#51972=CARTESIAN_POINT('Ctrl Pts',(1.53806898844261,-35.2378043314629,-5.1122340347836));
#51973=CARTESIAN_POINT('Ctrl Pts',(1.53262204854038,-35.236053255808,-5.1180834385527));
#51974=CARTESIAN_POINT('Ctrl Pts',(1.52730576708068,-35.2343432891189,-5.12424859598885));
#51975=CARTESIAN_POINT('Ctrl Pts',(1.52210243099411,-35.2326677069358,-5.13084104408167));
#51976=CARTESIAN_POINT('Ctrl Pts',(1.51932482645314,-35.2317732606415,-5.13436017362742));
#51977=CARTESIAN_POINT('Ctrl Pts',(1.51658000405007,-35.2308888851264,-5.13800146111875));
#51978=CARTESIAN_POINT('Ctrl Pts',(1.51387019301489,-35.2300161278903,-5.14178470318121));
#51979=CARTESIAN_POINT('Ctrl Pts',(1.50899186094646,-35.2284449483662,-5.14859547737775));
#51980=CARTESIAN_POINT('Ctrl Pts',(1.50447971014778,-35.226974435639,-5.15550406977863));
#51981=CARTESIAN_POINT('Ctrl Pts',(1.50032158273591,-35.2256142603436,-5.16249261721141));
#51982=CARTESIAN_POINT('Ctrl Pts',(1.49062427650963,-35.2224421506284,-5.17879083942049));
#51983=CARTESIAN_POINT('Ctrl Pts',(1.48284972550606,-35.2198703197455,-5.19552723132818));
#51984=CARTESIAN_POINT('Ctrl Pts',(1.47685246235576,-35.2179251530912,-5.21241218505702));
#51985=CARTESIAN_POINT('Ctrl Pts',(1.47188719805485,-35.2163147074086,-5.22639160464748));
#51986=CARTESIAN_POINT('Ctrl Pts',(1.46814309341427,-35.2151376620024,-5.24047372826221));
#51987=CARTESIAN_POINT('Ctrl Pts',(1.46553748721243,-35.214392780468,-5.25447234610973));
#51988=CARTESIAN_POINT('Ctrl Pts',(1.46316296846251,-35.2137139614014,-5.26722944675239));
#51989=CARTESIAN_POINT('Ctrl Pts',(1.46173426076785,-35.2133943776133,-5.27991727358435));
#51990=CARTESIAN_POINT('Ctrl Pts',(1.461172945671,-35.2133981106173,-5.29237060577687));
#51991=CARTESIAN_POINT('Ctrl Pts',(1.46095968732751,-35.2133995288835,-5.29710195365816));
#51992=CARTESIAN_POINT('Ctrl Pts',(1.46087144111853,-35.2134472157513,-5.3017991828776));
#51993=CARTESIAN_POINT('Ctrl Pts',(1.46090316329,-35.2135376551,-5.30645216923));
#51994=CARTESIAN_POINT('Origin',(1.209267879813,-35.4768981557443,-4.15982468249633));
#51995=CARTESIAN_POINT('Ctrl Pts',(1.69382496103,-35.2682576589,-5.01043544546));
#51996=CARTESIAN_POINT('Ctrl Pts',(1.69402179658,-35.3094043143,-5.02023549828));
#51997=CARTESIAN_POINT('Ctrl Pts',(1.69321049045,-35.351018059,-5.02809467113));
#51998=CARTESIAN_POINT('Ctrl Pts',(1.69139030338,-35.3929455262,-5.03397642476));
#51999=CARTESIAN_POINT('Ctrl Pts',(1.68856804502,-35.4350298576,-5.03785875444));
#52000=CARTESIAN_POINT('Ctrl Pts',(1.6847579226,-35.4771141891,-5.03973467901));
#52001=CARTESIAN_POINT('Ctrl Pts',(1.68490151218,-35.268974041,-5.01524294734));
#52002=CARTESIAN_POINT('Ctrl Pts',(1.68651188124,-35.3098358784,-5.02415397172));
#52003=CARTESIAN_POINT('Ctrl Pts',(1.68714086448,-35.3511508863,-5.03116493545));
#52004=CARTESIAN_POINT('Ctrl Pts',(1.68678246934,-35.3927702163,-5.03624343644));
#52005=CARTESIAN_POINT('Ctrl Pts',(1.68543788474,-35.4345417096,-5.03937097175));
#52006=CARTESIAN_POINT('Ctrl Pts',(1.68311545107,-35.4763132029,-5.04054334111));
#52007=CARTESIAN_POINT('Ctrl Pts',(1.67612908012,-35.2701100859,-5.02003914153));
#52008=CARTESIAN_POINT('Ctrl Pts',(1.67913856906,-35.3106802184,-5.02807779826));
#52009=CARTESIAN_POINT('Ctrl Pts',(1.68118935788,-35.3516915586,-5.03424982493));
#52010=CARTESIAN_POINT('Ctrl Pts',(1.6822703811,-35.3929991785,-5.03852665843));
#52011=CARTESIAN_POINT('Ctrl Pts',(1.68237796302,-35.4344548915,-5.04089285688));
#52012=CARTESIAN_POINT('Ctrl Pts',(1.68151488066,-35.4759106045,-5.04134696784));
#52013=CARTESIAN_POINT('Ctrl Pts',(1.66745641736,-35.2716459733,-5.02484351574));
#52014=CARTESIAN_POINT('Ctrl Pts',(1.67185679176,-35.3119189644,-5.03202383893));
#52015=CARTESIAN_POINT('Ctrl Pts',(1.67531720482,-35.3526230495,-5.03736380107));
#52016=CARTESIAN_POINT('Ctrl Pts',(1.67782194293,-35.3936164734,-5.04083824001));
#52017=CARTESIAN_POINT('Ctrl Pts',(1.67936231019,-35.4347546994,-5.04243484007));
#52018=CARTESIAN_POINT('Ctrl Pts',(1.67993607839,-35.4758929253,-5.04215470289));
#52019=CARTESIAN_POINT('Ctrl Pts',(1.65900707813,-35.2735686701,-5.02958783575));
#52020=CARTESIAN_POINT('Ctrl Pts',(1.66477502429,-35.3135351172,-5.03593051298));
#52021=CARTESIAN_POINT('Ctrl Pts',(1.6696184323,-35.3539241381,-5.04045242297));
#52022=CARTESIAN_POINT('Ctrl Pts',(1.67351721006,-35.3945968399,-5.04313153636));
#52023=CARTESIAN_POINT('Ctrl Pts',(1.67645771737,-35.4354113842,-5.0439585342));
#52024=CARTESIAN_POINT('Ctrl Pts',(1.67843305643,-35.4762259285,-5.04293699751));
#52025=CARTESIAN_POINT('Ctrl Pts',(1.65073625045,-35.2758278019,-5.0342827697));
#52026=CARTESIAN_POINT('Ctrl Pts',(1.65785005217,-35.3154860139,-5.03981027692));
#52027=CARTESIAN_POINT('Ctrl Pts',(1.66405116082,-35.3555599215,-5.04352991245));
#52028=CARTESIAN_POINT('Ctrl Pts',(1.66931505993,-35.3959128757,-5.04542262153));
#52029=CARTESIAN_POINT('Ctrl Pts',(1.67362354949,-35.4364053554,-5.04548186008));
#52030=CARTESIAN_POINT('Ctrl Pts',(1.67696511998,-35.4768978351,-5.04371372921));
#52031=CARTESIAN_POINT('Ctrl Pts',(1.69382496014738,-35.268257661,-5.01043544642385));
#52032=CARTESIAN_POINT('Ctrl Pts',(1.68803312612198,-35.2687226336122,-5.01355579279809));
#52033=CARTESIAN_POINT('Ctrl Pts',(1.68231297816127,-35.2693997637279,-5.01667279399805));
#52034=CARTESIAN_POINT('Ctrl Pts',(1.67666523914987,-35.2702777195431,-5.0197822570377));
#52035=CARTESIAN_POINT('Ctrl Pts',(1.67037182346692,-35.2712560474872,-5.02324720883873));
#52036=CARTESIAN_POINT('Ctrl Pts',(1.66417391129964,-35.2724846442873,-5.02670011798684));
#52037=CARTESIAN_POINT('Ctrl Pts',(1.65809711371162,-35.2739404345783,-5.03012131671218));
#52038=CARTESIAN_POINT('Ctrl Pts',(1.65562402628534,-35.2745329006942,-5.03151364933934));
#52039=CARTESIAN_POINT('Ctrl Pts',(1.65317074085282,-35.2751628346991,-5.03290083178419));
#52040=CARTESIAN_POINT('Ctrl Pts',(1.65073625045,-35.2758278019,-5.0342827697));
#52041=CARTESIAN_POINT('Origin',(0.517276095271889,-35.5445396177181,-6.5565839998119));
#52042=CARTESIAN_POINT('',(1.46090089616294,-35.2135311920909,-7.94951678979554));
#52043=CARTESIAN_POINT('Origin',(0.51727190487542,-35.5445407938518,-7.94950134108497));
#52044=CARTESIAN_POINT('',(1.46090316329,-35.2135376551,-5.30645216923));
#52045=CARTESIAN_POINT('Ctrl Pts',(1.8311006173,-35.2589545751,-8.27964607156));
#52046=CARTESIAN_POINT('Ctrl Pts',(1.83516599722,-35.30564267,-8.26740892391));
#52047=CARTESIAN_POINT('Ctrl Pts',(1.83967892993,-35.3530290502,-8.25798461135));
#52048=CARTESIAN_POINT('Ctrl Pts',(1.84461954945,-35.4008855262,-8.25143297176));
#52049=CARTESIAN_POINT('Ctrl Pts',(1.84996359063,-35.4489770577,-8.24778618257));
#52050=CARTESIAN_POINT('Ctrl Pts',(1.85568309486,-35.4970685893,-8.24704782502));
#52051=CARTESIAN_POINT('Ctrl Pts',(1.8411549102,-35.2563947443,-8.27868180069));
#52052=CARTESIAN_POINT('Ctrl Pts',(1.84372513023,-35.3033039498,-8.26655797443));
#52053=CARTESIAN_POINT('Ctrl Pts',(1.84674896075,-35.3509164835,-8.25725221826));
#52054=CARTESIAN_POINT('Ctrl Pts',(1.85021379554,-35.3990025183,-8.25082395949));
#52055=CARTESIAN_POINT('Ctrl Pts',(1.85410255764,-35.447325312,-8.24730484866));
#52056=CARTESIAN_POINT('Ctrl Pts',(1.85839419939,-35.4956481058,-8.24669783586));
#52057=CARTESIAN_POINT('Ctrl Pts',(1.8515433823,-35.25441601,-8.27750101411));
#52058=CARTESIAN_POINT('Ctrl Pts',(1.85257607592,-35.3015060532,-8.26552228872));
#52059=CARTESIAN_POINT('Ctrl Pts',(1.85406935318,-35.3493041477,-8.25636790881));
#52060=CARTESIAN_POINT('Ctrl Pts',(1.85601808078,-35.3975789365,-8.25009675826));
#52061=CARTESIAN_POINT('Ctrl Pts',(1.8584126658,-35.4460920799,-8.24673979731));
#52062=CARTESIAN_POINT('Ctrl Pts',(1.86123915467,-35.4946052233,-8.24629917315));
#52063=CARTESIAN_POINT('Ctrl Pts',(1.86227923956,-35.2530824801,-8.2760758565));
#52064=CARTESIAN_POINT('Ctrl Pts',(1.86172760863,-35.3003142451,-8.26427721621));
#52065=CARTESIAN_POINT('Ctrl Pts',(1.86164442165,-35.3482586468,-8.25531090742));
#52066=CARTESIAN_POINT('Ctrl Pts',(1.86203232275,-35.3966828431,-8.24923515298));
#52067=CARTESIAN_POINT('Ctrl Pts',(1.86288941138,-35.4453469517,-8.24608002563));
#52068=CARTESIAN_POINT('Ctrl Pts',(1.86420909862,-35.4940110603,-8.24584666363));
#52069=CARTESIAN_POINT('Ctrl Pts',(1.8733302454,-35.2524719557,-8.27438297071));
#52070=CARTESIAN_POINT('Ctrl Pts',(1.87114978057,-35.2998071163,-8.26280107324));
#52071=CARTESIAN_POINT('Ctrl Pts',(1.86944655662,-35.34785966,-8.25406232754));
#52072=CARTESIAN_POINT('Ctrl Pts',(1.8682313281,-35.3963952193,-8.24822411924));
#52073=CARTESIAN_POINT('Ctrl Pts',(1.8675100956,-35.4451722935,-8.24531550566));
#52074=CARTESIAN_POINT('Ctrl Pts',(1.86728392959,-35.4939493677,-8.24533636007));
#52075=CARTESIAN_POINT('Ctrl Pts',(1.88461561635,-35.2526204897,-8.27242216736));
#52076=CARTESIAN_POINT('Ctrl Pts',(1.88077145213,-35.3000228694,-8.26109202298));
#52077=CARTESIAN_POINT('Ctrl Pts',(1.87741430691,-35.3481478104,-8.25261964893));
#52078=CARTESIAN_POINT('Ctrl Pts',(1.87456332753,-35.3967592797,-8.24706149184));
#52079=CARTESIAN_POINT('Ctrl Pts',(1.87223278053,-35.4456140212,-8.24444536521));
#52080=CARTESIAN_POINT('Ctrl Pts',(1.87043162953,-35.4944687629,-8.2447696254));
#52081=CARTESIAN_POINT('',(1.8846153427573,-35.2526204926719,-8.27242221793613));
#52082=CARTESIAN_POINT('Origin',(2.04762529146993,-35.4944692033061,-9.22894623475615));
#52083=CARTESIAN_POINT('',(1.83110037507866,-35.258953748698,-8.2796463148645));
#52084=CARTESIAN_POINT('Origin',(1.87243576229956,-35.4444265283287,-8.21862309905423));
#52085=CARTESIAN_POINT('Origin',(1.98368693863888,-35.4970721031414,-9.2388220939813));
#52086=CARTESIAN_POINT('Ctrl Pts',(1.46144763142,-35.2150898018,-7.98721591698));
#52087=CARTESIAN_POINT('Ctrl Pts',(1.48377600029,-35.278742568,-7.9813037531));
#52088=CARTESIAN_POINT('Ctrl Pts',(1.50069598676,-35.344292508,-7.97539158967));
#52089=CARTESIAN_POINT('Ctrl Pts',(1.51199409489,-35.4111316208,-7.96953590506));
#52090=CARTESIAN_POINT('Ctrl Pts',(1.51756138096,-35.4786154003,-7.96379316359));
#52091=CARTESIAN_POINT('Ctrl Pts',(1.51739959704,-35.5460991799,-7.95821663141));
#52092=CARTESIAN_POINT('Ctrl Pts',(1.45535023282,-35.1977075828,-8.04883580535));
#52093=CARTESIAN_POINT('Ctrl Pts',(1.48166949688,-35.2678829449,-8.03945279279));
#52094=CARTESIAN_POINT('Ctrl Pts',(1.50141667723,-35.3406016986,-8.03107453153));
#52095=CARTESIAN_POINT('Ctrl Pts',(1.51429114701,-35.4150544061,-8.02380364128));
#52096=CARTESIAN_POINT('Ctrl Pts',(1.52014358616,-35.4903742161,-8.01772327965));
#52097=CARTESIAN_POINT('Ctrl Pts',(1.51898580713,-35.5656940262,-8.01289172937));
#52098=CARTESIAN_POINT('Ctrl Pts',(1.46435245205,-35.1856198088,-8.11169781125));
#52099=CARTESIAN_POINT('Ctrl Pts',(1.49329848629,-35.2601192136,-8.09750578865));
#52100=CARTESIAN_POINT('Ctrl Pts',(1.51493019199,-35.3378102208,-8.08590190484));
#52101=CARTESIAN_POINT('Ctrl Pts',(1.52885470957,-35.4176855473,-8.07706315905));
#52102=CARTESIAN_POINT('Ctrl Pts',(1.53488112404,-35.4986532993,-8.07110658123));
#52103=CARTESIAN_POINT('Ctrl Pts',(1.53303520019,-35.5796210507,-8.06808053282));
#52104=CARTESIAN_POINT('Ctrl Pts',(1.49172176542,-35.1799552596,-8.17111299923));
#52105=CARTESIAN_POINT('Ctrl Pts',(1.51992397896,-35.2563325377,-8.15127801209));
#52106=CARTESIAN_POINT('Ctrl Pts',(1.54120100093,-35.3362785459,-8.13597848758));
#52107=CARTESIAN_POINT('Ctrl Pts',(1.5551380035,-35.4186751656,-8.12550808337));
#52108=CARTESIAN_POINT('Ctrl Pts',(1.56152781403,-35.5022972201,-8.12002297191));
#52109=CARTESIAN_POINT('Ctrl Pts',(1.5603885908,-35.5859192753,-8.11952822853));
#52110=CARTESIAN_POINT('Ctrl Pts',(1.57027832078,-35.1818573291,-8.25620202557));
#52111=CARTESIAN_POINT('Ctrl Pts',(1.59174100272,-35.2575761439,-8.2305972979));
#52112=CARTESIAN_POINT('Ctrl Pts',(1.60864769834,-35.3366611931,-8.21163579835));
#52113=CARTESIAN_POINT('Ctrl Pts',(1.62070812016,-35.4180526309,-8.19967893383));
#52114=CARTESIAN_POINT('Ctrl Pts',(1.62775389781,-35.5005977196,-8.19489712008));
#52115=CARTESIAN_POINT('Ctrl Pts',(1.62975211946,-35.5831428078,-8.19725603749));
#52116=CARTESIAN_POINT('Ctrl Pts',(1.67937525828,-35.2054111593,-8.29244102122));
#52117=CARTESIAN_POINT('Ctrl Pts',(1.69139601914,-35.2726177891,-8.26960761361));
#52118=CARTESIAN_POINT('Ctrl Pts',(1.70188615133,-35.3420423454,-8.25274940255));
#52119=CARTESIAN_POINT('Ctrl Pts',(1.7107273602,-35.4129758871,-8.24210785095));
#52120=CARTESIAN_POINT('Ctrl Pts',(1.71782785643,-35.4846639068,-8.23779633493));
#52121=CARTESIAN_POINT('Ctrl Pts',(1.72312748813,-35.5563519268,-8.23979333534));
#52122=CARTESIAN_POINT('Ctrl Pts',(1.73126212215,-35.2199435259,-8.29740056817));
#52123=CARTESIAN_POINT('Ctrl Pts',(1.73944999004,-35.2817848557,-8.27769690404));
#52124=CARTESIAN_POINT('Ctrl Pts',(1.74724337723,-35.3452273068,-8.26303381776));
#52125=CARTESIAN_POINT('Ctrl Pts',(1.75458028421,-35.4097526752,-8.25356881995));
#52126=CARTESIAN_POINT('Ctrl Pts',(1.76140026731,-35.4748200605,-8.24938018459));
#52127=CARTESIAN_POINT('Ctrl Pts',(1.7676477796,-35.5398874456,-8.25046377193));
#52128=CARTESIAN_POINT('Ctrl Pts',(1.78213085799,-35.2383375006,-8.29255588031));
#52129=CARTESIAN_POINT('Ctrl Pts',(1.7878752107,-35.2931533399,-8.27665796781));
#52130=CARTESIAN_POINT('Ctrl Pts',(1.79382722081,-35.3490506456,-8.26463904937));
#52131=CARTESIAN_POINT('Ctrl Pts',(1.79995135062,-35.4056781551,-8.25659979182));
#52132=CARTESIAN_POINT('Ctrl Pts',(1.80620870196,-35.4626704426,-8.2525916122));
#52133=CARTESIAN_POINT('Ctrl Pts',(1.81255794182,-35.5196627301,-8.25261467335));
#52134=CARTESIAN_POINT('Ctrl Pts',(1.83110005152,-35.2589529157,-8.27964657201));
#52135=CARTESIAN_POINT('Ctrl Pts',(1.83516520879,-35.3056415029,-8.26740924886));
#52136=CARTESIAN_POINT('Ctrl Pts',(1.83967790698,-35.3530283973,-8.25798482029));
#52137=CARTESIAN_POINT('Ctrl Pts',(1.84461828078,-35.4008854025,-8.25143312625));
#52138=CARTESIAN_POINT('Ctrl Pts',(1.84996206575,-35.4489774707,-8.24778634512));
#52139=CARTESIAN_POINT('Ctrl Pts',(1.85568130399,-35.4970695389,-8.24704805785));
#52140=CARTESIAN_POINT('',(1.46144760573678,-35.2150897285778,-7.98721594892785));
#52141=CARTESIAN_POINT('Ctrl Pts',(1.461447626411,-35.2150897875206,-7.98721596760062));
#52142=CARTESIAN_POINT('Ctrl Pts',(1.45975611672774,-35.2102676927798,-8.00431028529611));
#52143=CARTESIAN_POINT('Ctrl Pts',(1.45949088883459,-35.2060112736049,-8.0212499105763));
#52144=CARTESIAN_POINT('Ctrl Pts',(1.46063290708311,-35.2023078195083,-8.03785564020924));
#52145=CARTESIAN_POINT('Ctrl Pts',(1.4619849592698,-35.1979232457801,-8.0575154075472));
#52146=CARTESIAN_POINT('Ctrl Pts',(1.46530862871115,-35.1943131533458,-8.07670545288678));
#52147=CARTESIAN_POINT('Ctrl Pts',(1.47049421230562,-35.1914533514575,-8.09512876016919));
#52148=CARTESIAN_POINT('Ctrl Pts',(1.47590344828213,-35.1884702073275,-8.1143466581633));
#52149=CARTESIAN_POINT('Ctrl Pts',(1.48333705879276,-35.1863028020104,-8.13272925288172));
#52150=CARTESIAN_POINT('Ctrl Pts',(1.49261651363463,-35.1849311628113,-8.14996266488784));
#52151=CARTESIAN_POINT('Ctrl Pts',(1.50139934296483,-35.1836329321292,-8.16627376494771));
#52152=CARTESIAN_POINT('Ctrl Pts',(1.51183526909898,-35.1830473682593,-8.18155534070476));
#52153=CARTESIAN_POINT('Ctrl Pts',(1.52374090219576,-35.1831700187017,-8.19556753354493));
#52154=CARTESIAN_POINT('Ctrl Pts',(1.53476411711598,-35.183283578575,-8.20854117483937));
#52155=CARTESIAN_POINT('Ctrl Pts',(1.54704765661419,-35.1840042929883,-8.22042644252083));
#52156=CARTESIAN_POINT('Ctrl Pts',(1.56041708072795,-35.1853404899314,-8.23105732045887));
#52157=CARTESIAN_POINT('Ctrl Pts',(1.56910154768583,-35.1862084523884,-8.23796289151418));
#52158=CARTESIAN_POINT('Ctrl Pts',(1.57825731769038,-35.1873345507109,-8.24435196287183));
#52159=CARTESIAN_POINT('Ctrl Pts',(1.58782634821685,-35.1887261822664,-8.25017848425026));
#52160=CARTESIAN_POINT('Ctrl Pts',(1.60172467941707,-35.1907474273878,-8.25864108907095));
#52161=CARTESIAN_POINT('Ctrl Pts',(1.6164949308172,-35.1933280702808,-8.26591472259457));
#52162=CARTESIAN_POINT('Ctrl Pts',(1.63196242905032,-35.1964777725275,-8.27188457667519));
#52163=CARTESIAN_POINT('Ctrl Pts',(1.64849069024609,-35.1998434817482,-8.27826384409504));
#52164=CARTESIAN_POINT('Ctrl Pts',(1.66581448192413,-35.2038599872894,-8.28315426383548));
#52165=CARTESIAN_POINT('Ctrl Pts',(1.68369377872932,-35.208545021433,-8.28646866080559));
#52166=CARTESIAN_POINT('Ctrl Pts',(1.70103107100662,-35.2130880304318,-8.28968258300957));
#52167=CARTESIAN_POINT('Ctrl Pts',(1.71888903761226,-35.2182610669448,-8.29141505338385));
#52168=CARTESIAN_POINT('Ctrl Pts',(1.73704188098263,-35.2240674952026,-8.29163087046771));
#52169=CARTESIAN_POINT('Ctrl Pts',(1.75245675447925,-35.2289981474005,-8.2918141361401));
#52170=CARTESIAN_POINT('Ctrl Pts',(1.76808309114067,-35.2343860832447,-8.29090457051527));
#52171=CARTESIAN_POINT('Ctrl Pts',(1.78379592237618,-35.2402121797429,-8.28890352851202));
#52172=CARTESIAN_POINT('Ctrl Pts',(1.79823012727575,-35.2455641796059,-8.28706532062609));
#52173=CARTESIAN_POINT('Ctrl Pts',(1.81273625305411,-35.2512865057029,-8.28430641503284));
#52174=CARTESIAN_POINT('Ctrl Pts',(1.82724442381139,-35.2573372993209,-8.28064174154456));
#52175=CARTESIAN_POINT('Ctrl Pts',(1.82852960227087,-35.2578732972596,-8.28031711347759));
#52176=CARTESIAN_POINT('Ctrl Pts',(1.82981482215612,-35.2584118502895,-8.27998538547209));
#52177=CARTESIAN_POINT('Ctrl Pts',(1.83110005096932,-35.2589529154682,-8.27964657215517));
#52178=CARTESIAN_POINT('Origin',(0.51781791838867,-35.5460995682007,-7.98721608782858));
#52179=CARTESIAN_POINT('Ctrl Pts',(1.46090085849,-35.2135310847,-7.94951679032));
#52180=CARTESIAN_POINT('Ctrl Pts',(1.48323559961,-35.2772019758,-7.94951679554));
#52181=CARTESIAN_POINT('Ctrl Pts',(1.50020012625,-35.3427566518,-7.94951680076));
#52182=CARTESIAN_POINT('Ctrl Pts',(1.51158239151,-35.4095912303,-7.94951680594));
#52183=CARTESIAN_POINT('Ctrl Pts',(1.51727342189,-35.4770658384,-7.94951681101));
#52184=CARTESIAN_POINT('Ctrl Pts',(1.5172734197,-35.5445404466,-7.94951681593));
#52185=CARTESIAN_POINT('Ctrl Pts',(1.46090084734,-35.2135310529,-7.95714134841));
#52186=CARTESIAN_POINT('Ctrl Pts',(1.48323559207,-35.2772019436,-7.95594579353));
#52187=CARTESIAN_POINT('Ctrl Pts',(1.50020012179,-35.3427566195,-7.95475023866));
#52188=CARTESIAN_POINT('Ctrl Pts',(1.51158238894,-35.4095911981,-7.95356602458));
#52189=CARTESIAN_POINT('Ctrl Pts',(1.51727341997,-35.4770658064,-7.95240448782));
#52190=CARTESIAN_POINT('Ctrl Pts',(1.51727341782,-35.5445404148,-7.95127632944));
#52191=CARTESIAN_POINT('Ctrl Pts',(1.46095673562,-35.2136903768,-7.96472994159));
#52192=CARTESIAN_POINT('Ctrl Pts',(1.48329083274,-35.277359414,-7.96234446573));
#52193=CARTESIAN_POINT('Ctrl Pts',(1.50025081243,-35.3429136053,-7.95995898987));
#52194=CARTESIAN_POINT('Ctrl Pts',(1.51162447777,-35.4097486473,-7.95759614371));
#52195=CARTESIAN_POINT('Ctrl Pts',(1.51730285882,-35.477224193,-7.95527854376));
#52196=CARTESIAN_POINT('Ctrl Pts',(1.51728631578,-35.5446997387,-7.9530275433));
#52197=CARTESIAN_POINT('Ctrl Pts',(1.46106747229,-35.2140060602,-7.97227569366));
#52198=CARTESIAN_POINT('Ctrl Pts',(1.48340028139,-35.277671426,-7.9687069317));
#52199=CARTESIAN_POINT('Ctrl Pts',(1.50035124089,-35.3432246581,-7.96513816975));
#52200=CARTESIAN_POINT('Ctrl Pts',(1.51170786352,-35.4100606172,-7.96160330128));
#52201=CARTESIAN_POINT('Ctrl Pts',(1.51736118389,-35.4775380197,-7.95813620969));
#52202=CARTESIAN_POINT('Ctrl Pts',(1.51731187088,-35.5450154221,-7.95476887067));
#52203=CARTESIAN_POINT('Ctrl Pts',(1.4612316362,-35.2144740518,-7.97977268509));
#52204=CARTESIAN_POINT('Ctrl Pts',(1.48356253349,-35.2781339746,-7.97502812195));
#52205=CARTESIAN_POINT('Ctrl Pts',(1.50050012169,-35.3436857837,-7.9702835588));
#52206=CARTESIAN_POINT('Ctrl Pts',(1.51183147778,-35.4105231034,-7.96558416229));
#52207=CARTESIAN_POINT('Ctrl Pts',(1.51744764399,-35.4780032585,-7.96097508922));
#52208=CARTESIAN_POINT('Ctrl Pts',(1.51734975497,-35.5454834136,-7.95649894554));
#52209=CARTESIAN_POINT('Ctrl Pts',(1.461447583,-35.2150896638,-7.9872159128));
#52210=CARTESIAN_POINT('Ctrl Pts',(1.48377596485,-35.2787424258,-7.98130374694));
#52211=CARTESIAN_POINT('Ctrl Pts',(1.50069596198,-35.3442923623,-7.97539158107));
#52212=CARTESIAN_POINT('Ctrl Pts',(1.51199407822,-35.4111314721,-7.96953589364));
#52213=CARTESIAN_POINT('Ctrl Pts',(1.51756136975,-35.4786152489,-7.963793149));
#52214=CARTESIAN_POINT('Ctrl Pts',(1.5173995886,-35.5460990256,-7.95821661336));
#52215=CARTESIAN_POINT('Origin',(2.95627559618279,-39.4764825794548,-7.94254325147619));
#52216=CARTESIAN_POINT('Ctrl Pts',(2.02882252548,-35.2583787857,-8.24404394735));
#52217=CARTESIAN_POINT('Ctrl Pts',(2.02793435434,-35.304849438,-8.23266211897));
#52218=CARTESIAN_POINT('Ctrl Pts',(2.0275994353,-35.3519981482,-8.22400554803));
#52219=CARTESIAN_POINT('Ctrl Pts',(2.02782201048,-35.3996032301,-8.21812855721));
#52220=CARTESIAN_POINT('Ctrl Pts',(2.02860101303,-35.4474365049,-8.21505931587));
#52221=CARTESIAN_POINT('Ctrl Pts',(2.02993009745,-35.4952697797,-8.21479904026));
#52222=CARTESIAN_POINT('Ctrl Pts',(2.7603704221,-35.2788135941,-8.09044877058));
#52223=CARTESIAN_POINT('Ctrl Pts',(2.75916038902,-35.3170950643,-8.08332087145));
#52224=CARTESIAN_POINT('Ctrl Pts',(2.75848926909,-35.3556762451,-8.07788965412));
#52225=CARTESIAN_POINT('Ctrl Pts',(2.75836124945,-35.3944575182,-8.07416878882));
#52226=CARTESIAN_POINT('Ctrl Pts',(2.75877734505,-35.4333388354,-8.07216551353));
#52227=CARTESIAN_POINT('Ctrl Pts',(2.75973535856,-35.4722201525,-8.07188072536));
#52228=CARTESIAN_POINT('Ctrl Pts',(3.46770746463,-35.2977417588,-7.8780751558));
#52229=CARTESIAN_POINT('Ctrl Pts',(3.46660967304,-35.3282659767,-7.87385395784));
#52230=CARTESIAN_POINT('Ctrl Pts',(3.46593509074,-35.3589261674,-7.87061653092));
#52231=CARTESIAN_POINT('Ctrl Pts',(3.4656850911,-35.3896774143,-7.8683685806));
#52232=CARTESIAN_POINT('Ctrl Pts',(3.46586006339,-35.420474191,-7.86711317222));
#52233=CARTESIAN_POINT('Ctrl Pts',(3.46645942733,-35.4512709677,-7.86685062308));
#52234=CARTESIAN_POINT('Ctrl Pts',(4.1448564034,-35.31305193,-7.60417987874));
#52235=CARTESIAN_POINT('Ctrl Pts',(4.14387911843,-35.3375078051,-7.60136146782));
#52236=CARTESIAN_POINT('Ctrl Pts',(4.14322007764,-35.3620512903,-7.59920530757));
#52237=CARTESIAN_POINT('Ctrl Pts',(4.14288053918,-35.3866532884,-7.59771461525));
#52238=CARTESIAN_POINT('Ctrl Pts',(4.14286096901,-35.4112845426,-7.59689108063));
#52239=CARTESIAN_POINT('Ctrl Pts',(4.14316103429,-35.4359157968,-7.59673486922));
#52240=CARTESIAN_POINT('Ctrl Pts',(5.21843923371,-35.3262967395,-7.044990155));
#52241=CARTESIAN_POINT('Ctrl Pts',(5.21754878579,-35.3454147425,-7.04339100369));
#52242=CARTESIAN_POINT('Ctrl Pts',(5.21690210383,-35.3645740899,-7.04217483695));
#52243=CARTESIAN_POINT('Ctrl Pts',(5.21649981226,-35.3837610519,-7.04134271025));
#52244=CARTESIAN_POINT('Ctrl Pts',(5.21634220772,-35.4029618215,-7.04089517538));
#52245=CARTESIAN_POINT('Ctrl Pts',(5.21642926006,-35.422162591,-7.04083226933));
#52246=CARTESIAN_POINT('Ctrl Pts',(6.21090480851,-35.3291957718,-6.34191684905));
#52247=CARTESIAN_POINT('Ctrl Pts',(6.20990218356,-35.347292328,-6.34059495831));
#52248=CARTESIAN_POINT('Ctrl Pts',(6.20914711064,-35.3654273382,-6.33960321184));
#52249=CARTESIAN_POINT('Ctrl Pts',(6.20864031997,-35.3835880114,-6.33894257829));
#52250=CARTESIAN_POINT('Ctrl Pts',(6.20838217516,-35.401761516,-6.33861353938));
#52251=CARTESIAN_POINT('Ctrl Pts',(6.20837267016,-35.4199350207,-6.33861609384));
#52252=CARTESIAN_POINT('Ctrl Pts',(6.59524089295,-35.3292320711,-6.04038307893));
#52253=CARTESIAN_POINT('Ctrl Pts',(6.59420777333,-35.3473355691,-6.03905690773));
#52254=CARTESIAN_POINT('Ctrl Pts',(6.59343802139,-35.3654739877,-6.03805312954));
#52255=CARTESIAN_POINT('Ctrl Pts',(6.59293154067,-35.3836356047,-6.03737283826));
#52256=CARTESIAN_POINT('Ctrl Pts',(6.59268825297,-35.4018088233,-6.03701670404));
#52257=CARTESIAN_POINT('Ctrl Pts',(6.59270812441,-35.4199820418,-6.03698498184));
#52258=CARTESIAN_POINT('Ctrl Pts',(7.36674622516,-35.3292429118,-5.37908303219));
#52259=CARTESIAN_POINT('Ctrl Pts',(7.36563384979,-35.3471062503,-5.37795639383));
#52260=CARTESIAN_POINT('Ctrl Pts',(7.36479211144,-35.3650081661,-5.37711871787));
#52261=CARTESIAN_POINT('Ctrl Pts',(7.36422260417,-35.3829359555,-5.37657056503));
#52262=CARTESIAN_POINT('Ctrl Pts',(7.36392615799,-35.4008766793,-5.37631208835));
#52263=CARTESIAN_POINT('Ctrl Pts',(7.36390280813,-35.4188174032,-5.37634302053));
#52264=CARTESIAN_POINT('Ctrl Pts',(8.06644392307,-35.3242511579,-4.63577831824));
#52265=CARTESIAN_POINT('Ctrl Pts',(8.06481498329,-35.3443613723,-4.63450682037));
#52266=CARTESIAN_POINT('Ctrl Pts',(8.06356784153,-35.3645192368,-4.63357464248));
#52267=CARTESIAN_POINT('Ctrl Pts',(8.06270291188,-35.3847087915,-4.63298305339));
#52268=CARTESIAN_POINT('Ctrl Pts',(8.06222041463,-35.4049141939,-4.63273277941));
#52269=CARTESIAN_POINT('Ctrl Pts',(8.06212040397,-35.4251195963,-4.63282401372));
#52270=CARTESIAN_POINT('Ctrl Pts',(8.40676939645,-35.318254221,-4.22563363488));
#52271=CARTESIAN_POINT('Ctrl Pts',(8.40459143683,-35.3405015468,-4.22453866256));
#52272=CARTESIAN_POINT('Ctrl Pts',(8.40288571682,-35.3628356427,-4.22380563891));
#52273=CARTESIAN_POINT('Ctrl Pts',(8.40165936546,-35.3852283571,-4.22343491308));
#52274=CARTESIAN_POINT('Ctrl Pts',(8.40091620766,-35.4076503711,-4.22342586623));
#52275=CARTESIAN_POINT('Ctrl Pts',(8.40065659496,-35.4300723851,-4.22377686476));
#52276=CARTESIAN_POINT('Ctrl Pts',(8.6986202738,-35.3007569312,-3.78649453504));
#52277=CARTESIAN_POINT('Ctrl Pts',(8.69512018043,-35.3302263046,-3.78463499808));
#52278=CARTESIAN_POINT('Ctrl Pts',(8.69237513121,-35.3597713122,-3.78337739168));
#52279=CARTESIAN_POINT('Ctrl Pts',(8.69038139929,-35.3893659949,-3.78272454109));
#52280=CARTESIAN_POINT('Ctrl Pts',(8.68913711634,-35.4189855209,-3.78267851397));
#52281=CARTESIAN_POINT('Ctrl Pts',(8.68864247336,-35.4486050468,-3.78324063488));
#52282=CARTESIAN_POINT('Ctrl Pts',(8.93444618031,-35.2748044449,-3.31652377072));
#52283=CARTESIAN_POINT('Ctrl Pts',(8.92616350743,-35.3147858017,-3.31461838858));
#52284=CARTESIAN_POINT('Ctrl Pts',(8.91971795914,-35.3551905608,-3.31361146728));
#52285=CARTESIAN_POINT('Ctrl Pts',(8.91513837409,-35.3958795596,-3.31350964329));
#52286=CARTESIAN_POINT('Ctrl Pts',(8.91244074774,-35.4367106808,-3.31431327227));
#52287=CARTESIAN_POINT('Ctrl Pts',(8.91162790031,-35.4775418019,-3.31601642165));
#52288=CARTESIAN_POINT('',(8.93444610724292,-35.2748049035046,-3.31652381528626));
#52289=CARTESIAN_POINT('Origin',(9.81418541109622,-35.4775497621699,-3.74658646986247));
#52290=CARTESIAN_POINT('',(2.0288222656268,-35.2583777618445,-8.24404425484976));
#52291=CARTESIAN_POINT('Ctrl Pts',(2.02882252548,-35.2583787857,-8.24404394735));
#52292=CARTESIAN_POINT('Ctrl Pts',(2.18677753481697,-35.2627910468336,-8.21087984737389));
#52293=CARTESIAN_POINT('Ctrl Pts',(2.33861437522826,-35.2669852055805,-8.17542519196724));
#52294=CARTESIAN_POINT('Ctrl Pts',(2.48435108055497,-35.2709319401419,-8.13825000100819));
#52295=CARTESIAN_POINT('Ctrl Pts',(2.64525208832679,-35.2752893432196,-8.0972066298409));
#52296=CARTESIAN_POINT('Ctrl Pts',(2.79871785488418,-35.2793444717014,-8.05406686887132));
#52297=CARTESIAN_POINT('Ctrl Pts',(2.94483454315409,-35.2830773158073,-8.00961262753664));
#52298=CARTESIAN_POINT('Ctrl Pts',(3.03413015126555,-35.2853585513621,-7.98244551500408));
#52299=CARTESIAN_POINT('Ctrl Pts',(3.12068223968935,-35.2875198737809,-7.9547877183841));
#52300=CARTESIAN_POINT('Ctrl Pts',(3.20451874330892,-35.2895609699308,-7.9268175468804));
#52301=CARTESIAN_POINT('Ctrl Pts',(3.3572398925257,-35.2932791420423,-7.8758655563821));
#52302=CARTESIAN_POINT('Ctrl Pts',(3.50096252004891,-35.2965988835363,-7.82387548219649));
#52303=CARTESIAN_POINT('Ctrl Pts',(3.63595726353252,-35.2995836082428,-7.77186522336913));
#52304=CARTESIAN_POINT('Ctrl Pts',(3.65356195398893,-35.2999728467658,-7.76508255551418));
#52305=CARTESIAN_POINT('Ctrl Pts',(3.67101823732379,-35.3003564000405,-7.75829947690513));
#52306=CARTESIAN_POINT('Ctrl Pts',(3.68832673200562,-35.3007344202451,-7.75151817837785));
#52307=CARTESIAN_POINT('Ctrl Pts',(3.76334271985672,-35.3023727810382,-7.72212764977972));
#52308=CARTESIAN_POINT('Ctrl Pts',(3.83558426198059,-35.3038950886041,-7.69277255023342));
#52309=CARTESIAN_POINT('Ctrl Pts',(3.90510884594964,-35.3052987785019,-7.66362553964167));
#52310=CARTESIAN_POINT('Ctrl Pts',(3.93987113793416,-35.3060006234508,-7.64905203434579));
#52311=CARTESIAN_POINT('Ctrl Pts',(3.97395414544796,-35.3066728111262,-7.63453043970357));
#52312=CARTESIAN_POINT('Ctrl Pts',(4.00736544039963,-35.3073153616589,-7.62008124899256));
#52313=CARTESIAN_POINT('Ctrl Pts',(4.02407108787547,-35.3076366369253,-7.61285665363705));
#52314=CARTESIAN_POINT('Ctrl Pts',(4.04060880379702,-35.3079505016349,-7.60565015095042));
#52315=CARTESIAN_POINT('Ctrl Pts',(4.05697952642894,-35.3082569556414,-7.59846424465178));
#52316=CARTESIAN_POINT('Ctrl Pts',(4.06516488774489,-35.3084101826446,-7.59487129150247));
#52317=CARTESIAN_POINT('Ctrl Pts',(4.07330850050044,-35.3085615568926,-7.59128348690469));
#52318=CARTESIAN_POINT('Ctrl Pts',(4.08141048278529,-35.308711078371,-7.58770113942753));
#52319=CARTESIAN_POINT('Ctrl Pts',(4.08951246507013,-35.3088605998495,-7.58411879195037));
#52320=CARTESIAN_POINT('Ctrl Pts',(4.09652997069631,-35.3089893052348,-7.58100632499581));
#52321=CARTESIAN_POINT('Ctrl Pts',(4.10559165594891,-35.3091540843135,-7.5769707743543));
#52322=CARTESIAN_POINT('Ctrl Pts',(4.23911785829849,-35.311582145319,-7.517505924657));
#52323=CARTESIAN_POINT('Ctrl Pts',(4.37541831829351,-35.3138080692197,-7.45326567496979));
#52324=CARTESIAN_POINT('Ctrl Pts',(4.51410564517436,-35.3158091474134,-7.38380419075587));
#52325=CARTESIAN_POINT('Ctrl Pts',(4.63203743674429,-35.3175107501608,-7.32473810690604));
#52326=CARTESIAN_POINT('Ctrl Pts',(4.75169471236088,-35.319048903818,-7.26189640866632));
#52327=CARTESIAN_POINT('Ctrl Pts',(4.87285226581732,-35.3204169420525,-7.19504100971907));
#52328=CARTESIAN_POINT('Ctrl Pts',(4.91863422188269,-35.320933884369,-7.1697782766082));
#52329=CARTESIAN_POINT('Ctrl Pts',(4.96463057429613,-35.321426680412,-7.14394286693305));
#52330=CARTESIAN_POINT('Ctrl Pts',(5.01082994297537,-35.3218956802795,-7.11752369939173));
#52331=CARTESIAN_POINT('Ctrl Pts',(5.11691531470315,-35.3229726219502,-7.05685864509589));
#52332=CARTESIAN_POINT('Ctrl Pts',(5.22405614828952,-35.3239068291055,-6.99312243979726));
#52333=CARTESIAN_POINT('Ctrl Pts',(5.3321129332859,-35.3247083121071,-6.92621787562441));
#52334=CARTESIAN_POINT('Ctrl Pts',(5.35606344132569,-35.3248859587498,-6.91138865132189));
#52335=CARTESIAN_POINT('Ctrl Pts',(5.38005902814711,-35.3250571708672,-6.89640393554172));
#52336=CARTESIAN_POINT('Ctrl Pts',(5.40409832085966,-35.325222215338,-6.88126296256034));
#52337=CARTESIAN_POINT('Ctrl Pts',(5.43121311996124,-35.3254083750442,-6.864184904337));
#52338=CARTESIAN_POINT('Ctrl Pts',(5.45838352251183,-35.3255866912149,-6.84690805936453));
#52339=CARTESIAN_POINT('Ctrl Pts',(5.48560720457396,-35.3257572756508,-6.82943126754002));
#52340=CARTESIAN_POINT('Ctrl Pts',(5.56573339667789,-35.3262593488549,-6.77799264230574));
#52341=CARTESIAN_POINT('Ctrl Pts',(5.64632318459152,-35.3266943011098,-6.7248203623343));
#52342=CARTESIAN_POINT('Ctrl Pts',(5.72732506573132,-35.3270730527021,-6.66988195870045));
#52343=CARTESIAN_POINT('Ctrl Pts',(5.77469456688971,-35.327294544768,-6.63775425082558));
#52344=CARTESIAN_POINT('Ctrl Pts',(5.82179076014501,-35.3274946126195,-6.60530886215643));
#52345=CARTESIAN_POINT('Ctrl Pts',(5.86933240137305,-35.3276745273873,-6.5720410809232));
#52346=CARTESIAN_POINT('Ctrl Pts',(5.90308700092806,-35.3278022670022,-6.54842093225764));
#52347=CARTESIAN_POINT('Ctrl Pts',(5.93706562713996,-35.3279197935568,-6.52438529273794));
#52348=CARTESIAN_POINT('Ctrl Pts',(5.97151741326441,-35.3280268927031,-6.49973981824754));
#52349=CARTESIAN_POINT('Ctrl Pts',(6.07625212176294,-35.3283524780829,-6.42481666107839));
#52350=CARTESIAN_POINT('Ctrl Pts',(6.17799261229962,-35.3286064804706,-6.34951475089196));
#52351=CARTESIAN_POINT('Ctrl Pts',(6.27687958650818,-35.3288007027633,-6.27407844529289));
#52352=CARTESIAN_POINT('Ctrl Pts',(6.37620699077342,-35.3289957900975,-6.19830615594454));
#52353=CARTESIAN_POINT('Ctrl Pts',(6.47265578885625,-35.3291307886013,-6.12239783657176));
#52354=CARTESIAN_POINT('Ctrl Pts',(6.56633397049423,-35.3292071010504,-6.04656264049156));
#52355=CARTESIAN_POINT('Ctrl Pts',(6.66238066294141,-35.329285342944,-5.96881006644252));
#52356=CARTESIAN_POINT('Ctrl Pts',(6.75551494837276,-35.3293019838777,-5.89113406093224));
#52357=CARTESIAN_POINT('Ctrl Pts',(6.84581317853924,-35.3292450759539,-5.81372510819961));
#52358=CARTESIAN_POINT('Ctrl Pts',(6.85762114423611,-35.3292376343151,-5.8036026256569));
#52359=CARTESIAN_POINT('Ctrl Pts',(6.8693805591948,-35.3292289157708,-5.79348466563219));
#52360=CARTESIAN_POINT('Ctrl Pts',(6.88109154574958,-35.3292188763152,-5.78337161550293));
#52361=CARTESIAN_POINT('Ctrl Pts',(6.97439721443612,-35.3291388883386,-5.70279728469339));
#52362=CARTESIAN_POINT('Ctrl Pts',(7.06464238906416,-35.328985179861,-5.62252753578287));
#52363=CARTESIAN_POINT('Ctrl Pts',(7.15189748092528,-35.3287608286773,-5.54270464046465));
#52364=CARTESIAN_POINT('Ctrl Pts',(7.19349553981168,-35.3286538713233,-5.50464981261326));
#52365=CARTESIAN_POINT('Ctrl Pts',(7.23441338506565,-35.3285306520656,-5.46669605227421));
#52366=CARTESIAN_POINT('Ctrl Pts',(7.27465557605091,-35.3283904889136,-5.42885630951328));
#52367=CARTESIAN_POINT('Ctrl Pts',(7.29187189551032,-35.3283305246437,-5.41266779980036));
#52368=CARTESIAN_POINT('Ctrl Pts',(7.30896477210815,-35.3282674437883,-5.39649991143824));
#52369=CARTESIAN_POINT('Ctrl Pts',(7.32593406851701,-35.3282013929398,-5.38035392747592));
#52370=CARTESIAN_POINT('Ctrl Pts',(7.37039712118064,-35.3280283261088,-5.33804812304389));
#52371=CARTESIAN_POINT('Ctrl Pts',(7.41401265050169,-35.3278349578144,-5.29589242088803));
#52372=CARTESIAN_POINT('Ctrl Pts',(7.45679370714464,-35.3276206689168,-5.25389496570991));
#52373=CARTESIAN_POINT('Ctrl Pts',(7.48634791730271,-35.3274726328556,-5.22488208679023));
#52374=CARTESIAN_POINT('Ctrl Pts',(7.51550525137304,-35.3273147314449,-5.19594320056072));
#52375=CARTESIAN_POINT('Ctrl Pts',(7.54427073978588,-35.3271469506249,-5.16707824386914));
#52376=CARTESIAN_POINT('Ctrl Pts',(7.55865348399229,-35.3270630602149,-5.15264576552336));
#52377=CARTESIAN_POINT('Ctrl Pts',(7.57293825488062,-35.3269766983596,-5.1382317579152));
#52378=CARTESIAN_POINT('Ctrl Pts',(7.58712538578354,-35.3268878654927,-5.12383639135977));
#52379=CARTESIAN_POINT('Ctrl Pts',(7.59421895123501,-35.3268434490592,-5.11663870808206));
#52380=CARTESIAN_POINT('Ctrl Pts',(7.60128810618754,-35.3267984148055,-5.10944568456635));
#52381=CARTESIAN_POINT('Ctrl Pts',(7.60833288566123,-35.3267527624904,-5.10225734327071));
#52382=CARTESIAN_POINT('Ctrl Pts',(7.61185527539808,-35.3267299363328,-5.09866317262288));
#52383=CARTESIAN_POINT('Ctrl Pts',(7.61537157123757,-35.3267069556562,-5.09507017250368));
#52384=CARTESIAN_POINT('Ctrl Pts',(7.61888177667662,-35.3266838204384,-5.09147834630862));
#52385=CARTESIAN_POINT('Ctrl Pts',(7.62239198211567,-35.3266606852206,-5.08788652011355));
#52386=CARTESIAN_POINT('Ctrl Pts',(7.62478543468777,-35.3266448392919,-5.08543556574044));
#52387=CARTESIAN_POINT('Ctrl Pts',(7.62939412499817,-35.3266139511337,-5.08070639299966));
#52388=CARTESIAN_POINT('Ctrl Pts',(7.71724388637304,-35.3260251683897,-4.99056002411896));
#52389=CARTESIAN_POINT('Ctrl Pts',(7.80012523544823,-35.3252426647832,-4.90232735910713));
#52390=CARTESIAN_POINT('Ctrl Pts',(7.8781402873884,-35.3242422108242,-4.81627017606473));
#52391=CARTESIAN_POINT('Ctrl Pts',(7.93109327299415,-35.3235631492486,-4.7578585662332));
#52392=CARTESIAN_POINT('Ctrl Pts',(7.98180352905179,-35.3227842492524,-4.70045011363536));
#52393=CARTESIAN_POINT('Ctrl Pts',(8.0303108006439,-35.3219088916018,-4.64413249332142));
#52394=CARTESIAN_POINT('Ctrl Pts',(8.09029705160267,-35.3208263853717,-4.57448761751889));
#52395=CARTESIAN_POINT('Ctrl Pts',(8.14690751976985,-35.3195837043465,-4.50651864413491));
#52396=CARTESIAN_POINT('Ctrl Pts',(8.20023454467272,-35.3181885095926,-4.44041955605619));
#52397=CARTESIAN_POINT('Ctrl Pts',(8.22689805712416,-35.3174909122157,-4.40737001201683));
#52398=CARTESIAN_POINT('Ctrl Pts',(8.25274132262907,-35.3167554667997,-4.37478808215928));
#52399=CARTESIAN_POINT('Ctrl Pts',(8.27777958112633,-35.3159868446467,-4.34269824029458));
#52400=CARTESIAN_POINT('Ctrl Pts',(8.29029871037496,-35.3156025335702,-4.32665331936224));
#52401=CARTESIAN_POINT('Ctrl Pts',(8.30261653001456,-35.315210720873,-4.31073139713076));
#52402=CARTESIAN_POINT('Ctrl Pts',(8.31473547083024,-35.3148096730619,-4.29493563233504));
#52403=CARTESIAN_POINT('Ctrl Pts',(8.32079494123809,-35.3146091491563,-4.28703774993718));
#52404=CARTESIAN_POINT('Ctrl Pts',(8.32680469431384,-35.3144063137906,-4.2791714082933));
#52405=CARTESIAN_POINT('Ctrl Pts',(8.33276502615426,-35.3142011670248,-4.27133699140478));
#52406=CARTESIAN_POINT('Ctrl Pts',(8.33781611184359,-35.3140273153132,-4.26469771156446));
#52407=CARTESIAN_POINT('Ctrl Pts',(8.34198825082389,-35.3138816669016,-4.25919659070227));
#52408=CARTESIAN_POINT('Ctrl Pts',(8.34742624935289,-35.3136885395028,-4.25199874874118));
#52409=CARTESIAN_POINT('Ctrl Pts',(8.34840514370081,-35.3136537746315,-4.25070306490172));
#52410=CARTESIAN_POINT('Ctrl Pts',(8.34942495171374,-35.3136174507336,-4.24935232555719));
#52411=CARTESIAN_POINT('Ctrl Pts',(8.35049802910589,-35.3135790959847,-4.24792988360141));
#52412=CARTESIAN_POINT('Ctrl Pts',(8.41512795258716,-35.3112690440657,-4.16225822987801));
#52413=CARTESIAN_POINT('Ctrl Pts',(8.47750701667447,-35.30858490516,-4.07557038676447));
#52414=CARTESIAN_POINT('Ctrl Pts',(8.53739064535456,-35.3054895764863,-3.98787969849236));
#52415=CARTESIAN_POINT('Ctrl Pts',(8.5933670495396,-35.3025962085868,-3.9059105607134));
#52416=CARTESIAN_POINT('Ctrl Pts',(8.64716225878082,-35.2993434776791,-3.82306535457545));
#52417=CARTESIAN_POINT('Ctrl Pts',(8.69861273070644,-35.2957235257303,-3.73936182375594));
#52418=CARTESIAN_POINT('Ctrl Pts',(8.74688779638733,-35.2923269889922,-3.66082428470525));
#52419=CARTESIAN_POINT('Ctrl Pts',(8.7930983233281,-35.2886071906419,-3.58153121200422));
#52420=CARTESIAN_POINT('Ctrl Pts',(8.83714924844075,-35.2845783406043,-3.50150150967928));
#52421=CARTESIAN_POINT('Ctrl Pts',(8.87085295372428,-35.2814958361177,-3.44027016222879));
#52422=CARTESIAN_POINT('Ctrl Pts',(8.90329318573489,-35.2782328112362,-3.37860768781965));
#52423=CARTESIAN_POINT('Ctrl Pts',(8.93444613770044,-35.2748044495892,-3.31652385563538));
#52424=CARTESIAN_POINT('Origin',(2.2221106022258,-35.495269847715,-9.19615921132892));
#52425=CARTESIAN_POINT('Ctrl Pts',(8.93444595596,-35.2748053687,-3.31652394249));
#52426=CARTESIAN_POINT('Ctrl Pts',(8.92616317166,-35.3147866052,-3.31461891577));
#52427=CARTESIAN_POINT('Ctrl Pts',(8.91971750036,-35.3551912403,-3.31361234962));
#52428=CARTESIAN_POINT('Ctrl Pts',(8.91513778092,-35.3958801128,-3.31351087925));
#52429=CARTESIAN_POINT('Ctrl Pts',(8.91244000919,-35.4367111064,-3.31431485906));
#52430=CARTESIAN_POINT('Ctrl Pts',(8.91162700591,-35.4775421,-3.31601835533));
#52431=CARTESIAN_POINT('Ctrl Pts',(8.94734368663,-35.2728133782,-3.29109023634));
#52432=CARTESIAN_POINT('Ctrl Pts',(8.93895107582,-35.3135017401,-3.28875572575));
#52433=CARTESIAN_POINT('Ctrl Pts',(8.93246763725,-35.3546364096,-3.28733586636));
#52434=CARTESIAN_POINT('Ctrl Pts',(8.9279236303,-35.3960707679,-3.28683902656));
#52435=CARTESIAN_POINT('Ctrl Pts',(8.92533550226,-35.4376549725,-3.28726695529));
#52436=CARTESIAN_POINT('Ctrl Pts',(8.92470553582,-35.4792391771,-3.28861474271));
#52437=CARTESIAN_POINT('Ctrl Pts',(8.95983458954,-35.2711079221,-3.26569669172));
#52438=CARTESIAN_POINT('Ctrl Pts',(8.95141175919,-35.3123562177,-3.2628807422));
#52439=CARTESIAN_POINT('Ctrl Pts',(8.94495906105,-35.354070024,-3.26098724776));
#52440=CARTESIAN_POINT('Ctrl Pts',(8.94050773142,-35.3960964758,-3.260026589));
#52441=CARTESIAN_POINT('Ctrl Pts',(8.93807435022,-35.4382792543,-3.26000227455));
#52442=CARTESIAN_POINT('Ctrl Pts',(8.93766047318,-35.4804620328,-3.26091086944));
#52443=CARTESIAN_POINT('Ctrl Pts',(8.97214212604,-35.2697920542,-3.23978066277));
#52444=CARTESIAN_POINT('Ctrl Pts',(8.9637190734,-35.311417995,-3.23656869462));
#52445=CARTESIAN_POINT('Ctrl Pts',(8.95731138416,-35.3535230656,-3.23427864864));
#52446=CARTESIAN_POINT('Ctrl Pts',(8.95295080025,-35.3959499382,-3.2329226531));
#52447=CARTESIAN_POINT('Ctrl Pts',(8.95065387904,-35.4385377451,-3.23250578662));
#52448=CARTESIAN_POINT('Ctrl Pts',(8.95042158697,-35.481125552,-3.23302610121));
#52449=CARTESIAN_POINT('Ctrl Pts',(8.98911618271,-35.268630653,-3.20263013659));
#52450=CARTESIAN_POINT('Ctrl Pts',(8.98077765617,-35.3105436223,-3.19892614932));
#52451=CARTESIAN_POINT('Ctrl Pts',(8.97449392264,-35.3529460311,-3.19613159274));
#52452=CARTESIAN_POINT('Ctrl Pts',(8.97029699893,-35.3956772608,-3.19426066196));
#52453=CARTESIAN_POINT('Ctrl Pts',(8.96820302947,-35.4385728912,-3.19332056844));
#52454=CARTESIAN_POINT('Ctrl Pts',(8.96821193143,-35.4814685217,-3.19331131722));
#52455=CARTESIAN_POINT('Ctrl Pts',(9.00517206358,-35.2680735988,-3.16566118546));
#52456=CARTESIAN_POINT('Ctrl Pts',(8.99706509175,-35.3099657558,-3.16142494219));
#52457=CARTESIAN_POINT('Ctrl Pts',(8.99102314624,-35.3523468191,-3.15807110791));
#52458=CARTESIAN_POINT('Ctrl Pts',(8.98707727301,-35.395056319,-3.15561591639));
#52459=CARTESIAN_POINT('Ctrl Pts',(8.9852426452,-35.4379300459,-3.15406880151));
#52460=CARTESIAN_POINT('Ctrl Pts',(8.98551821082,-35.4808037728,-3.15343220651));
#52461=CARTESIAN_POINT('Ctrl Pts',(9.00990494748,-35.2680166859,-3.15455724964));
#52462=CARTESIAN_POINT('Ctrl Pts',(9.00187362208,-35.3098646744,-3.1501873274));
#52463=CARTESIAN_POINT('Ctrl Pts',(8.99590638677,-35.3522000159,-3.14669037035));
#52464=CARTESIAN_POINT('Ctrl Pts',(8.99203402793,-35.3948627823,-3.14408308561));
#52465=CARTESIAN_POINT('Ctrl Pts',(8.9902713955,-35.4376892422,-3.1423755103));
#52466=CARTESIAN_POINT('Ctrl Pts',(8.9906170886,-35.480515702,-3.141570683));
#52467=CARTESIAN_POINT('Ctrl Pts',(9.01453522232,-35.2679213672,-3.1435714055));
#52468=CARTESIAN_POINT('Ctrl Pts',(9.00660223792,-35.3097130029,-3.13902110731));
#52469=CARTESIAN_POINT('Ctrl Pts',(9.00073178209,-35.3519900952,-3.13533334259));
#52470=CARTESIAN_POINT('Ctrl Pts',(8.99695406159,-35.3945932824,-3.13252547117));
#52471=CARTESIAN_POINT('Ctrl Pts',(8.99528353801,-35.4373595352,-3.13060822223));
#52472=CARTESIAN_POINT('Ctrl Pts',(8.99571858313,-35.480125788,-3.12958551692));
#52473=CARTESIAN_POINT('Ctrl Pts',(9.01911869111,-35.2680072167,-3.13244884091));
#52474=CARTESIAN_POINT('Ctrl Pts',(9.01128168784,-35.3096922673,-3.12777947274));
#52475=CARTESIAN_POINT('Ctrl Pts',(9.00550009533,-35.3518590427,-3.12396085378));
#52476=CARTESIAN_POINT('Ctrl Pts',(9.00180365501,-35.3943494134,-3.12101070215));
#52477=CARTESIAN_POINT('Ctrl Pts',(9.00020644216,-35.4370015851,-3.1189402514));
#52478=CARTESIAN_POINT('Ctrl Pts',(9.0007065476,-35.4796537567,-3.11775399652));
#52479=CARTESIAN_POINT('',(9.01911881647387,-35.2680071588897,-3.13244858247421));
#52480=CARTESIAN_POINT('Origin',(9.92280365052534,-35.4797729820442,-3.5071455175773));
#52481=CARTESIAN_POINT('Ctrl Pts',(8.93444605244327,-35.2748053537986,-3.3165237522296));
#52482=CARTESIAN_POINT('Ctrl Pts',(8.93943079272288,-35.2740354916699,-3.30669407905226));
#52483=CARTESIAN_POINT('Ctrl Pts',(8.94434450694004,-35.2733170876845,-3.29686746416126));
#52484=CARTESIAN_POINT('Ctrl Pts',(8.94920327991744,-35.2726626041066,-3.28699933631088));
#52485=CARTESIAN_POINT('Ctrl Pts',(8.95476984379752,-35.2719127800951,-3.27569369097379));
#52486=CARTESIAN_POINT('Ctrl Pts',(8.96026395103588,-35.2712474673185,-3.26433388324753));
#52487=CARTESIAN_POINT('Ctrl Pts',(8.96568210534835,-35.2706788951834,-3.25291678406206));
#52488=CARTESIAN_POINT('Ctrl Pts',(8.97215885291872,-35.269999236026,-3.23926902411549));
#52489=CARTESIAN_POINT('Ctrl Pts',(8.97852555524635,-35.2694597083162,-3.22554138045548));
#52490=CARTESIAN_POINT('Ctrl Pts',(8.98475329027834,-35.2690516149317,-3.21179771950845));
#52491=CARTESIAN_POINT('Ctrl Pts',(8.98837850251731,-35.2688140606484,-3.20379742925564));
#52492=CARTESIAN_POINT('Ctrl Pts',(8.99195633450091,-35.2686203519649,-3.19579280171345));
#52493=CARTESIAN_POINT('Ctrl Pts',(8.99548251952631,-35.2684610265365,-3.18779854407026));
#52494=CARTESIAN_POINT('Ctrl Pts',(8.9985837231518,-35.2683209032609,-3.18076776701017));
#52495=CARTESIAN_POINT('Ctrl Pts',(9.00164600869916,-35.2682110262086,-3.17374049995815));
#52496=CARTESIAN_POINT('Ctrl Pts',(9.00466972421821,-35.2681329993825,-3.16671499647348));
#52497=CARTESIAN_POINT('Ctrl Pts',(9.00712768751884,-35.2680695717637,-3.16100399964687));
#52498=CARTESIAN_POINT('Ctrl Pts',(9.00955950605995,-35.2680241990286,-3.15529745602052));
#52499=CARTESIAN_POINT('Ctrl Pts',(9.0119661489852,-35.2679980780999,-3.14959278684721));
#52500=CARTESIAN_POINT('Ctrl Pts',(9.01413745424937,-35.2679745114506,-3.14444595842639));
#52501=CARTESIAN_POINT('Ctrl Pts',(9.0162880259156,-35.2679655281606,-3.13930185415533));
#52502=CARTESIAN_POINT('Ctrl Pts',(9.01842446912663,-35.267995823019,-3.13413122667487));
#52503=CARTESIAN_POINT('Ctrl Pts',(9.01865602825218,-35.2679991065376,-3.13357080645318));
#52504=CARTESIAN_POINT('Ctrl Pts',(9.01888742951289,-35.2680028851188,-3.13301003640059));
#52505=CARTESIAN_POINT('Ctrl Pts',(9.01911868766448,-35.2680072166355,-3.13244884927113));
#52506=CARTESIAN_POINT('Ctrl Pts',(9.01911953995,-35.2680044421,-3.13244837682));
#52507=CARTESIAN_POINT('Ctrl Pts',(9.01128290018,-35.3096899679,-3.12777753845));
#52508=CARTESIAN_POINT('Ctrl Pts',(9.00550173203,-35.3518572367,-3.12395745117));
#52509=CARTESIAN_POINT('Ctrl Pts',(9.00180577632,-35.3943481132,-3.12100583911));
#52510=CARTESIAN_POINT('Ctrl Pts',(9.00020910686,-35.4370007968,-3.11893394172));
#52511=CARTESIAN_POINT('Ctrl Pts',(9.00070981215,-35.4796534803,-3.1177462595));
#52512=CARTESIAN_POINT('Ctrl Pts',(9.17544595344,-35.2835018925,-2.74597776201));
#52513=CARTESIAN_POINT('Ctrl Pts',(9.16933554333,-35.3193494556,-2.74372235315));
#52514=CARTESIAN_POINT('Ctrl Pts',(9.16476148349,-35.3554672008,-2.74189804713));
#52515=CARTESIAN_POINT('Ctrl Pts',(9.1617381998,-35.3917657165,-2.74050818076));
#52516=CARTESIAN_POINT('Ctrl Pts',(9.1602730438,-35.428154617,-2.73955472374));
#52517=CARTESIAN_POINT('Ctrl Pts',(9.16036621938,-35.4645435174,-2.73903830807));
#52518=CARTESIAN_POINT('Ctrl Pts',(9.29269126807,-35.2907452551,-2.34477529883));
#52519=CARTESIAN_POINT('Ctrl Pts',(9.28707239127,-35.3238061129,-2.34352966982));
#52520=CARTESIAN_POINT('Ctrl Pts',(9.282834933,-35.3571174391,-2.34257541991));
#52521=CARTESIAN_POINT('Ctrl Pts',(9.27999356004,-35.3905967652,-2.34191674071));
#52522=CARTESIAN_POINT('Ctrl Pts',(9.27855558309,-35.424160093,-2.3415559411));
#52523=CARTESIAN_POINT('Ctrl Pts',(9.27852082014,-35.4577234207,-2.34149337034));
#52524=CARTESIAN_POINT('Ctrl Pts',(9.36191429928,-35.2893802972,-1.92981468559));
#52525=CARTESIAN_POINT('Ctrl Pts',(9.3560452611,-35.3232454878,-1.92921642136));
#52526=CARTESIAN_POINT('Ctrl Pts',(9.35161541947,-35.3573586818,-1.92882344418));
#52527=CARTESIAN_POINT('Ctrl Pts',(9.34863880943,-35.3916379824,-1.92863719423));
#52528=CARTESIAN_POINT('Ctrl Pts',(9.3471225791,-35.4260003368,-1.92865812789));
#52529=CARTESIAN_POINT('Ctrl Pts',(9.3470668903,-35.4603626911,-1.92888572013));
#52530=CARTESIAN_POINT('Ctrl Pts',(9.4171903904,-35.2789856765,-1.18748239275));
#52531=CARTESIAN_POINT('Ctrl Pts',(9.40981639515,-35.3169659165,-1.18801696878));
#52532=CARTESIAN_POINT('Ctrl Pts',(9.40425718706,-35.3552891517,-1.18859518921));
#52533=CARTESIAN_POINT('Ctrl Pts',(9.40053397643,-35.3938423214,-1.18921641071));
#52534=CARTESIAN_POINT('Ctrl Pts',(9.39865750897,-35.4325104595,-1.18987939995));
#52535=CARTESIAN_POINT('Ctrl Pts',(9.39862789646,-35.4711785976,-1.19058233503));
#52536=CARTESIAN_POINT('Ctrl Pts',(9.38314539193,-35.2631816303,-0.439456405049));
#52537=CARTESIAN_POINT('Ctrl Pts',(9.37293597078,-35.3077684071,-0.441248963721));
#52538=CARTESIAN_POINT('Ctrl Pts',(9.36525594777,-35.3529358557,-0.442871125473));
#52539=CARTESIAN_POINT('Ctrl Pts',(9.36014835673,-35.3984936385,-0.444315444411));
#52540=CARTESIAN_POINT('Ctrl Pts',(9.35763482817,-35.4442465927,-0.44557584201));
#52541=CARTESIAN_POINT('Ctrl Pts',(9.3577150604,-35.489999547,-0.446647757649));
#52542=CARTESIAN_POINT('Ctrl Pts',(9.3558891039,-35.2557890156,-0.116721794816));
#52543=CARTESIAN_POINT('Ctrl Pts',(9.34426128655,-35.3033050214,-0.118995176137));
#52544=CARTESIAN_POINT('Ctrl Pts',(9.33551278911,-35.3515333802,-0.120988679218));
#52545=CARTESIAN_POINT('Ctrl Pts',(9.3296998933,-35.4002411909,-0.122691582222));
#52546=CARTESIAN_POINT('Ctrl Pts',(9.32685085926,-35.4491887348,-0.124095735733));
#52547=CARTESIAN_POINT('Ctrl Pts',(9.32696513263,-35.4981362787,-0.12519578818));
#52548=CARTESIAN_POINT('Ctrl Pts',(9.3192256268,-35.2483585547,0.204089324846));
#52549=CARTESIAN_POINT('Ctrl Pts',(9.30607279618,-35.2988047548,0.201137625763));
#52550=CARTESIAN_POINT('Ctrl Pts',(9.29617649939,-35.3501183672,0.198586534665));
#52551=CARTESIAN_POINT('Ctrl Pts',(9.28960975953,-35.4020166188,0.196452114669));
#52552=CARTESIAN_POINT('Ctrl Pts',(9.28640921473,-35.4542072015,0.194746107875));
#52553=CARTESIAN_POINT('Ctrl Pts',(9.28657394094,-35.5063977842,0.193475565417));
#52554=CARTESIAN_POINT('Ctrl Pts',(9.27386188307,-35.2408046524,0.522899877563));
#52555=CARTESIAN_POINT('Ctrl Pts',(9.25898070398,-35.2942887044,0.519158422332));
#52556=CARTESIAN_POINT('Ctrl Pts',(9.24778010992,-35.3488352241,0.515965853737));
#52557=CARTESIAN_POINT('Ctrl Pts',(9.24035614705,-35.4040992505,0.513346313675));
#52558=CARTESIAN_POINT('Ctrl Pts',(9.2367570062,-35.4597220507,0.511316806249));
#52559=CARTESIAN_POINT('Ctrl Pts',(9.23698117834,-35.5153448509,0.509886546917));
#52560=CARTESIAN_POINT('',(9.27386188271851,-35.2408046524422,0.522899877211493));
#52561=CARTESIAN_POINT('Origin',(10.2249210130936,-35.5153449925992,0.664731557103899));
#52562=CARTESIAN_POINT('Ctrl Pts',(9.01911901239593,-35.2680072483449,-3.13244806238356));
#52563=CARTESIAN_POINT('Ctrl Pts',(9.04723758683849,-35.2707933216705,-3.06293411125694));
#52564=CARTESIAN_POINT('Ctrl Pts',(9.07420491323081,-35.2732952866302,-2.99193253005062));
#52565=CARTESIAN_POINT('Ctrl Pts',(9.09979229073556,-35.2754876019786,-2.91946334446916));
#52566=CARTESIAN_POINT('Ctrl Pts',(9.12398764134561,-35.2775606490697,-2.85093669091733));
#52567=CARTESIAN_POINT('Ctrl Pts',(9.1469491132796,-35.2793568774923,-2.78109788353282));
#52568=CARTESIAN_POINT('Ctrl Pts',(9.16852081216598,-35.2808658327816,-2.7099817552574));
#52569=CARTESIAN_POINT('Ctrl Pts',(9.19071305145076,-35.2824181953018,-2.63681987106791));
#52570=CARTESIAN_POINT('Ctrl Pts',(9.21143546536842,-35.2836665588565,-2.56230237824364));
#52571=CARTESIAN_POINT('Ctrl Pts',(9.2305669901781,-35.2846122497235,-2.48646441291759));
#52572=CARTESIAN_POINT('Ctrl Pts',(9.24491563378535,-35.2853215178737,-2.42958593892305));
#52573=CARTESIAN_POINT('Ctrl Pts',(9.25837039520488,-35.285860794621,-2.37196477580435));
#52574=CARTESIAN_POINT('Ctrl Pts',(9.27089709582343,-35.2862350344547,-2.31361779737502));
#52575=CARTESIAN_POINT('Ctrl Pts',(9.27207147400642,-35.2862701194391,-2.30814776814727));
#52576=CARTESIAN_POINT('Ctrl Pts',(9.27323770564116,-35.2863037565467,-2.30267136109724));
#52577=CARTESIAN_POINT('Ctrl Pts',(9.27439576888682,-35.2863359514877,-2.29718859098508));
#52578=CARTESIAN_POINT('Ctrl Pts',(9.27495670577144,-35.2863515459122,-2.294532874212));
#52579=CARTESIAN_POINT('Ctrl Pts',(9.27551572621074,-35.286366801981,-2.29187566454904));
#52580=CARTESIAN_POINT('Ctrl Pts',(9.2760728278078,-35.2863817203657,-2.28921696370895));
#52581=CARTESIAN_POINT('Ctrl Pts',(9.27630406080572,-35.286387912455,-2.28811343184139));
#52582=CARTESIAN_POINT('Ctrl Pts',(9.27653496322923,-35.2863940463689,-2.28700964307651));
#52583=CARTESIAN_POINT('Ctrl Pts',(9.27676553490977,-35.286400122156,-2.28590559753794));
#52584=CARTESIAN_POINT('Ctrl Pts',(9.27697890363755,-35.2864057446287,-2.28488392483543));
#52585=CARTESIAN_POINT('Ctrl Pts',(9.27719124975535,-35.2864112984818,-2.28386559649145));
#52586=CARTESIAN_POINT('Ctrl Pts',(9.27740737627875,-35.2864169073712,-2.28282750369869));
#52587=CARTESIAN_POINT('Ctrl Pts',(9.27850111635318,-35.2864452919815,-2.27757408236655));
#52588=CARTESIAN_POINT('Ctrl Pts',(9.27966393451027,-35.2864742483586,-2.27194332303056));
#52589=CARTESIAN_POINT('Ctrl Pts',(9.28075079770566,-35.2865001446825,-2.26663647342955));
#52590=CARTESIAN_POINT('Ctrl Pts',(9.28127724706593,-35.2865126882144,-2.26406596815406));
#52591=CARTESIAN_POINT('Ctrl Pts',(9.2817860161204,-35.2865245364181,-2.26157149447093));
#52592=CARTESIAN_POINT('Ctrl Pts',(9.28226134927632,-35.2865353930508,-2.25923293064942));
#52593=CARTESIAN_POINT('Ctrl Pts',(9.28253429611568,-35.28654162717,-2.25789007544194));
#52594=CARTESIAN_POINT('Ctrl Pts',(9.28279622640398,-35.2865475356617,-2.25659863067582));
#52595=CARTESIAN_POINT('Ctrl Pts',(9.28304421219757,-35.2865530711993,-2.25537373436067));
#52596=CARTESIAN_POINT('Ctrl Pts',(9.28313947183165,-35.2865551975844,-2.25490321073473));
#52597=CARTESIAN_POINT('Ctrl Pts',(9.28323306243032,-35.2865572778078,-2.25444059493792));
#52598=CARTESIAN_POINT('Ctrl Pts',(9.28332724213507,-35.2865593623391,-2.25397473534079));
#52599=CARTESIAN_POINT('Ctrl Pts',(9.29788837172528,-35.2868816518457,-2.18194815613067));
#52600=CARTESIAN_POINT('Ctrl Pts',(9.31146872667869,-35.2869688785728,-2.10674755967947));
#52601=CARTESIAN_POINT('Ctrl Pts',(9.32376997890423,-35.2868002832768,-2.02836049238632));
#52602=CARTESIAN_POINT('Ctrl Pts',(9.33390631642818,-35.2866613593043,-1.9637688754494));
#52603=CARTESIAN_POINT('Ctrl Pts',(9.34317423335416,-35.2863489237478,-1.89701404272316));
#52604=CARTESIAN_POINT('Ctrl Pts',(9.35142640756365,-35.2858605440817,-1.82810511544412));
#52605=CARTESIAN_POINT('Ctrl Pts',(9.36058428003333,-35.2853185634369,-1.75163324851255));
#52606=CARTESIAN_POINT('Ctrl Pts',(9.36849034355677,-35.2845592448402,-1.67250678259968));
#52607=CARTESIAN_POINT('Ctrl Pts',(9.37497292578257,-35.283623339191,-1.59076151627657));
#52608=CARTESIAN_POINT('Ctrl Pts',(9.37821421689547,-35.2831553863665,-1.54988888311502));
#52609=CARTESIAN_POINT('Ctrl Pts',(9.38110084025768,-35.282640335853,-1.50836204477103));
#52610=CARTESIAN_POINT('Ctrl Pts',(9.38361747795923,-35.2820739559404,-1.4661885577414));
#52611=CARTESIAN_POINT('Ctrl Pts',(9.38487579681,-35.2817907659841,-1.44510181422658));
#52612=CARTESIAN_POINT('Ctrl Pts',(9.38604167032792,-35.2814947469656,-1.42385340943051));
#52613=CARTESIAN_POINT('Ctrl Pts',(9.38711338690994,-35.2811858908628,-1.40244454238854));
#52614=CARTESIAN_POINT('Ctrl Pts',(9.38764924520095,-35.2810314628114,-1.39174010886756));
#52615=CARTESIAN_POINT('Ctrl Pts',(9.38816156747465,-35.2808738260956,-1.38099555997792));
#52616=CARTESIAN_POINT('Ctrl Pts',(9.38865015904411,-35.2807129817596,-1.37021105531062));
#52617=CARTESIAN_POINT('Ctrl Pts',(9.38889445482884,-35.2806325595916,-1.36481880297698));
#52618=CARTESIAN_POINT('Ctrl Pts',(9.38913281813932,-35.2805513355577,-1.35941656170578));
#52619=CARTESIAN_POINT('Ctrl Pts',(9.38936522585477,-35.2804693098204,-1.35400435240585));
#52620=CARTESIAN_POINT('Ctrl Pts',(9.38948142971249,-35.2804282969518,-1.35129824775589));
#52621=CARTESIAN_POINT('Ctrl Pts',(9.38959614468414,-35.2803870836597,-1.34858965109911));
#52622=CARTESIAN_POINT('Ctrl Pts',(9.38970936795586,-35.2803456699662,-1.34587856511458));
#52623=CARTESIAN_POINT('Ctrl Pts',(9.38982259122758,-35.2803042562727,-1.34316747913004));
#52624=CARTESIAN_POINT('Ctrl Pts',(9.38998713981212,-35.280242607951,-1.33915257906503));
#52625=CARTESIAN_POINT('Ctrl Pts',(9.39004455990828,-35.2802208277092,-1.33773784187776));
#52626=CARTESIAN_POINT('Ctrl Pts',(9.39247225065664,-35.2792999708152,-1.27792351535704));
#52627=CARTESIAN_POINT('Ctrl Pts',(9.39441622714332,-35.2781841374586,-1.21105163812287));
#52628=CARTESIAN_POINT('Ctrl Pts',(9.39537367391675,-35.2768634271352,-1.13709139363227));
#52629=CARTESIAN_POINT('Ctrl Pts',(9.39559420549972,-35.2765592239707,-1.12005590900016));
#52630=CARTESIAN_POINT('Ctrl Pts',(9.39576230582339,-35.2762442449781,-1.10264453707456));
#52631=CARTESIAN_POINT('Ctrl Pts',(9.39587173465696,-35.2759185569207,-1.08485724332022));
#52632=CARTESIAN_POINT('Ctrl Pts',(9.39630799718663,-35.2746201286072,-1.0139442168714));
#52633=CARTESIAN_POINT('Ctrl Pts',(9.39581034995002,-35.2731508427485,-0.937053566237884));
#52634=CARTESIAN_POINT('Ctrl Pts',(9.39399461730175,-35.2715038208048,-0.85419236772634));
#52635=CARTESIAN_POINT('Ctrl Pts',(9.39225680407881,-35.2699274783212,-0.774887032450933));
#52636=CARTESIAN_POINT('Ctrl Pts',(9.38931064280304,-35.2681881426592,-0.690112287146941));
#52637=CARTESIAN_POINT('Ctrl Pts',(9.38484507129186,-35.2662900810482,-0.599909998384288));
#52638=CARTESIAN_POINT('Ctrl Pts',(9.38024844937121,-35.2643363173282,-0.50706055754988));
#52639=CARTESIAN_POINT('Ctrl Pts',(9.37404580640433,-35.2622003616864,-0.408474248060987));
#52640=CARTESIAN_POINT('Ctrl Pts',(9.36593741539263,-35.2598862246104,-0.304192156387564));
#52641=CARTESIAN_POINT('Ctrl Pts',(9.3564241061767,-35.2571711234836,-0.181841398716708));
#52642=CARTESIAN_POINT('Ctrl Pts',(9.34428932059871,-35.2542113363005,-0.0516501610174696));
#52643=CARTESIAN_POINT('Ctrl Pts',(9.32909395555769,-35.2510260462912,0.0862479119727824));
#52644=CARTESIAN_POINT('Ctrl Pts',(9.31796381762815,-35.2486929192453,0.187254012744678));
#52645=CARTESIAN_POINT('Ctrl Pts',(9.3051945285179,-35.2462396541912,0.292392266742369));
#52646=CARTESIAN_POINT('Ctrl Pts',(9.29059844484657,-35.2436690517339,0.401604163680389));
#52647=CARTESIAN_POINT('Ctrl Pts',(9.28526729841894,-35.2427301520663,0.441493261833483));
#52648=CARTESIAN_POINT('Ctrl Pts',(9.2796920959383,-35.2417754911663,0.481925890883731));
#52649=CARTESIAN_POINT('Ctrl Pts',(9.27386188313803,-35.2408046525553,0.522899876806236));
#52650=CARTESIAN_POINT('Ctrl Pts',(1.88364028582742,-35.2522336654635,-8.27268614758859));
#52651=CARTESIAN_POINT('Ctrl Pts',(1.87976663689926,-35.2997052295165,-8.26132512102646));
#52652=CARTESIAN_POINT('Ctrl Pts',(1.87638081507785,-35.3479026421397,-8.25283069221518));
#52653=CARTESIAN_POINT('Ctrl Pts',(1.87350217466588,-35.3965887842191,-8.24725963970389));
#52654=CARTESIAN_POINT('Ctrl Pts',(1.87114516584333,-35.4455192584089,-8.24463992898022));
#52655=CARTESIAN_POINT('Ctrl Pts',(1.86931890580546,-35.4944496516172,-8.24496988273828));
#52656=CARTESIAN_POINT('Ctrl Pts',(1.91281732676632,-35.2526046602642,-8.26762695724934));
#52657=CARTESIAN_POINT('Ctrl Pts',(1.90952279963636,-35.3002628262793,-8.25608047625197));
#52658=CARTESIAN_POINT('Ctrl Pts',(1.90673790621558,-35.348655083091,-8.24741759078021));
#52659=CARTESIAN_POINT('Ctrl Pts',(1.90447924341404,-35.3975416565539,-8.24169641976602));
#52660=CARTESIAN_POINT('Ctrl Pts',(1.90275826638143,-35.4466753525817,-8.23894588545803));
#52661=CARTESIAN_POINT('Ctrl Pts',(1.90158091110236,-35.4958089664898,-8.23916485303755));
#52662=CARTESIAN_POINT('Ctrl Pts',(1.94211315375089,-35.2533826883717,-8.26220387826513));
#52663=CARTESIAN_POINT('Ctrl Pts',(1.93941688088205,-35.3010369730568,-8.25055875462903));
#52664=CARTESIAN_POINT('Ctrl Pts',(1.9372487324096,-35.3494248319395,-8.24179185740762));
#52665=CARTESIAN_POINT('Ctrl Pts',(1.93562271894448,-35.3983065050355,-8.23596172652887));
#52666=CARTESIAN_POINT('Ctrl Pts',(1.9345461395142,-35.4474352783484,-8.23309792984346));
#52667=CARTESIAN_POINT('Ctrl Pts',(1.93402206538774,-35.4965639696529,-8.23319987074611));
#52668=CARTESIAN_POINT('Ctrl Pts',(1.97257776832187,-35.2536956114026,-8.25641928888991));
#52669=CARTESIAN_POINT('Ctrl Pts',(1.96997955469349,-35.3013407205115,-8.24478001979218));
#52670=CARTESIAN_POINT('Ctrl Pts',(1.96792030384476,-35.3497176962493,-8.23601266253125));
#52671=CARTESIAN_POINT('Ctrl Pts',(1.96638937419042,-35.3985953585765,-8.23017817576157));
#52672=CARTESIAN_POINT('Ctrl Pts',(1.96544075319438,-35.447711491921,-8.22730061263402));
#52673=CARTESIAN_POINT('Ctrl Pts',(1.9650528772274,-35.4968275462247,-8.22738250085497));
#52674=CARTESIAN_POINT('Ctrl Pts',(2.00055083481923,-35.2562298992234,-8.25032497229716));
#52675=CARTESIAN_POINT('Ctrl Pts',(1.99912539370006,-35.3032976000604,-8.238749237339));
#52676=CARTESIAN_POINT('Ctrl Pts',(1.99825185783193,-35.3510704148417,-8.22997224725792));
#52677=CARTESIAN_POINT('Ctrl Pts',(1.99793777759489,-35.399317719028,-8.22405070694943));
#52678=CARTESIAN_POINT('Ctrl Pts',(1.99818337980841,-35.4478025374972,-8.22101390379241));
#52679=CARTESIAN_POINT('Ctrl Pts',(1.99898528943331,-35.496287277138,-8.2208624116822));
#52680=CARTESIAN_POINT('Ctrl Pts',(2.02983724854675,-35.2580732139914,-8.24391392449866));
#52681=CARTESIAN_POINT('Ctrl Pts',(2.02896194525648,-35.3045999801645,-8.23250120504607));
#52682=CARTESIAN_POINT('Ctrl Pts',(2.02864185425062,-35.3518073286936,-8.22382046327515));
#52683=CARTESIAN_POINT('Ctrl Pts',(2.0288811566285,-35.3994727360757,-8.21792630872739));
#52684=CARTESIAN_POINT('Ctrl Pts',(2.02967872348038,-35.4473671370956,-8.21484706320934));
#52685=CARTESIAN_POINT('Ctrl Pts',(2.03102808564287,-35.4952614620131,-8.21458396353363));
#52686=CARTESIAN_POINT('Ctrl Pts',(1.88461534316315,-35.2526204924184,-8.2724222202528));
#52687=CARTESIAN_POINT('Ctrl Pts',(1.93258700263877,-35.2532511304555,-8.26408746050993));
#52688=CARTESIAN_POINT('Ctrl Pts',(1.98073381621476,-35.2553235421864,-8.25456655856178));
#52689=CARTESIAN_POINT('Ctrl Pts',(2.02882173043,-35.2583763205,-8.24404472212));
#52690=CARTESIAN_POINT('Ctrl Pts',(9.26569107955,-35.2394341184,0.579579770152));
#52691=CARTESIAN_POINT('Ctrl Pts',(9.25048970237,-35.2934597015,0.575763550708));
#52692=CARTESIAN_POINT('Ctrl Pts',(9.23904466522,-35.3485828761,0.57252289393));
#52693=CARTESIAN_POINT('Ctrl Pts',(9.23145625045,-35.4044474883,0.569882968796));
#52694=CARTESIAN_POINT('Ctrl Pts',(9.22777481195,-35.4606828414,0.567861292872));
#52695=CARTESIAN_POINT('Ctrl Pts',(9.22799880569,-35.5169181946,0.566467047136));
#52696=CARTESIAN_POINT('Ctrl Pts',(9.26734254057,-35.2397154298,0.568265288566));
#52697=CARTESIAN_POINT('Ctrl Pts',(9.25220700276,-35.2936330337,0.564453943744));
#52698=CARTESIAN_POINT('Ctrl Pts',(9.24081265384,-35.3486411511,0.561212799914));
#52699=CARTESIAN_POINT('Ctrl Pts',(9.23325890658,-35.4043858824,0.558566884261));
#52700=CARTESIAN_POINT('Ctrl Pts',(9.22959566517,-35.4604989426,0.556533678149));
#52701=CARTESIAN_POINT('Ctrl Pts',(9.22982138229,-35.5166120028,0.55512243494));
#52702=CARTESIAN_POINT('Ctrl Pts',(9.26898307793,-35.2399973473,0.556947742073));
#52703=CARTESIAN_POINT('Ctrl Pts',(9.25391368938,-35.2938057049,0.55314265644));
#52704=CARTESIAN_POINT('Ctrl Pts',(9.24257020144,-35.3486974567,0.549902346095));
#52705=CARTESIAN_POINT('Ctrl Pts',(9.23505116442,-35.4043209585,0.547251660046));
#52706=CARTESIAN_POINT('Ctrl Pts',(9.23140601814,-35.4603103757,0.54520808798));
#52707=CARTESIAN_POINT('Ctrl Pts',(9.23163322063,-35.516299793,0.543780919912));
#52708=CARTESIAN_POINT('Ctrl Pts',(9.2706134925,-35.2402652369,0.545649357377));
#52709=CARTESIAN_POINT('Ctrl Pts',(9.25560999309,-35.2939662109,0.541842800001));
#52710=CARTESIAN_POINT('Ctrl Pts',(9.24431742891,-35.3487436319,0.53859575027));
#52711=CARTESIAN_POINT('Ctrl Pts',(9.23683343793,-35.4042480754,0.535933346844));
#52712=CARTESIAN_POINT('Ctrl Pts',(9.23320713925,-35.460116063,0.533872309581));
#52713=CARTESIAN_POINT('Ctrl Pts',(9.23343691736,-35.5159840505,0.532422414623));
#52714=CARTESIAN_POINT('Ctrl Pts',(9.2722446143,-35.2405353461,0.534265835364));
#52715=CARTESIAN_POINT('Ctrl Pts',(9.25730181761,-35.294127701,0.530496224362));
#52716=CARTESIAN_POINT('Ctrl Pts',(9.24605472348,-35.3487894773,0.527280786202));
#52717=CARTESIAN_POINT('Ctrl Pts',(9.2386001998,-35.4041734976,0.524643949807));
#52718=CARTESIAN_POINT('Ctrl Pts',(9.23498684878,-35.4599186602,0.522602910424));
#52719=CARTESIAN_POINT('Ctrl Pts',(9.23521314025,-35.5156638228,0.521166956934));
#52720=CARTESIAN_POINT('Ctrl Pts',(9.27386188355,-35.2408046483,0.522899878387));
#52721=CARTESIAN_POINT('Ctrl Pts',(9.25898070438,-35.2942887003,0.519158423034));
#52722=CARTESIAN_POINT('Ctrl Pts',(9.24778011027,-35.34883522,0.515965854318));
#52723=CARTESIAN_POINT('Ctrl Pts',(9.24035614735,-35.4040992464,0.513346314134));
#52724=CARTESIAN_POINT('Ctrl Pts',(9.23675700648,-35.4597220466,0.511316806589));
#52725=CARTESIAN_POINT('Ctrl Pts',(9.23698117862,-35.5153448469,0.509886547139));
#52726=CARTESIAN_POINT('',(9.26569106343796,-35.239434108596,0.579579885999606));
#52727=CARTESIAN_POINT('Origin',(10.2153393707933,-35.5169183517482,0.725089002244375));
#52728=CARTESIAN_POINT('Ctrl Pts',(9.27386188241726,-35.2408046523711,0.522899878102206));
#52729=CARTESIAN_POINT('Ctrl Pts',(9.27283706818152,-35.2406340032975,0.530102139560715));
#52730=CARTESIAN_POINT('Ctrl Pts',(9.27180627580663,-35.2404633709726,0.537307422065));
#52731=CARTESIAN_POINT('Ctrl Pts',(9.27077304606167,-35.2402915867397,0.544494586134051));
#52732=CARTESIAN_POINT('Ctrl Pts',(9.26926926806017,-35.2400415694016,0.554954892056214));
#52733=CARTESIAN_POINT('Ctrl Pts',(9.26775968832857,-35.2397868315245,0.565385481138434));
#52734=CARTESIAN_POINT('Ctrl Pts',(9.26623927281631,-35.2395275672319,0.575820625922912));
#52735=CARTESIAN_POINT('Ctrl Pts',(9.26605669997065,-35.2394964345453,0.577073687380689));
#52736=CARTESIAN_POINT('Ctrl Pts',(9.26587397022987,-35.2394652727112,0.578326749393097));
#52737=CARTESIAN_POINT('Ctrl Pts',(9.26569107942698,-35.2394341188372,0.579579770121116));
#52738=CARTESIAN_POINT('Ctrl Pts',(8.84973117353,-35.1509193731,2.1670354781));
#52739=CARTESIAN_POINT('Ctrl Pts',(8.80995437067,-35.2405490067,2.13392896451));
#52740=CARTESIAN_POINT('Ctrl Pts',(8.78039938016,-35.3367791654,2.10641082417));
#52741=CARTESIAN_POINT('Ctrl Pts',(8.76195606614,-35.4376104406,2.08522113231));
#52742=CARTESIAN_POINT('Ctrl Pts',(8.75504494547,-35.5407438285,2.07084302459));
#52743=CARTESIAN_POINT('Ctrl Pts',(8.75956295656,-35.6438772164,2.06344039042));
#52744=CARTESIAN_POINT('Ctrl Pts',(8.91091202313,-35.1598372898,2.04459467569));
#52745=CARTESIAN_POINT('Ctrl Pts',(8.87455647002,-35.246237181,2.01484191076));
#52746=CARTESIAN_POINT('Ctrl Pts',(8.84773035639,-35.3382711138,1.98987130618));
#52747=CARTESIAN_POINT('Ctrl Pts',(8.83115765576,-35.4342118768,1.97027362582));
#52748=CARTESIAN_POINT('Ctrl Pts',(8.82517322934,-35.532107067,1.95644630565));
#52749=CARTESIAN_POINT('Ctrl Pts',(8.82968488575,-35.6300022572,1.94854820039));
#52750=CARTESIAN_POINT('Ctrl Pts',(8.96795816735,-35.1710296589,1.91634945111));
#52751=CARTESIAN_POINT('Ctrl Pts',(8.93494048323,-35.2532459987,1.89161496085));
#52752=CARTESIAN_POINT('Ctrl Pts',(8.91060835461,-35.3400086156,1.87063336475));
#52753=CARTESIAN_POINT('Ctrl Pts',(8.89552405555,-35.4299031373,1.85381398232));
#52754=CARTESIAN_POINT('Ctrl Pts',(8.88994864311,-35.5213641494,1.84144178963));
#52755=CARTESIAN_POINT('Ctrl Pts',(8.89381707546,-35.6128251616,1.83365112687));
#52756=CARTESIAN_POINT('Ctrl Pts',(9.01653709076,-35.1835781664,1.78332507658));
#52757=CARTESIAN_POINT('Ctrl Pts',(8.98711360766,-35.260897748,1.76325201128));
#52758=CARTESIAN_POINT('Ctrl Pts',(8.96538998881,-35.341846639,1.74604152846));
#52759=CARTESIAN_POINT('Ctrl Pts',(8.95179602076,-35.4252853121,1.73198094156));
#52760=CARTESIAN_POINT('Ctrl Pts',(8.94653331601,-35.5099692034,1.72127486801));
#52761=CARTESIAN_POINT('Ctrl Pts',(8.9495584777,-35.5946530947,1.71402843838));
#52762=CARTESIAN_POINT('Ctrl Pts',(9.1140028877,-35.2108461818,1.46157810716));
#52763=CARTESIAN_POINT('Ctrl Pts',(9.09197113076,-35.2771127336,1.45066936239));
#52764=CARTESIAN_POINT('Ctrl Pts',(9.07556758896,-35.3453927996,1.44108450365));
#52765=CARTESIAN_POINT('Ctrl Pts',(9.06500040952,-35.4150382685,1.43291495679));
#52766=CARTESIAN_POINT('Ctrl Pts',(9.06037122564,-35.4853665076,1.42623124853));
#52767=CARTESIAN_POINT('Ctrl Pts',(9.06167021042,-35.5556947466,1.4210802448));
#52768=CARTESIAN_POINT('Ctrl Pts',(9.17852891179,-35.2281865303,1.13254165139));
#52769=CARTESIAN_POINT('Ctrl Pts',(9.16069403398,-35.2869558429,1.12639249526));
#52770=CARTESIAN_POINT('Ctrl Pts',(9.14729128577,-35.3471459486,1.12104732689));
#52771=CARTESIAN_POINT('Ctrl Pts',(9.13845933491,-35.4082985485,1.1165532711));
#52772=CARTESIAN_POINT('Ctrl Pts',(9.13426752236,-35.4699324162,1.11294417189));
#52773=CARTESIAN_POINT('Ctrl Pts',(9.13471251897,-35.531566284,1.1102388653));
#52774=CARTESIAN_POINT('Ctrl Pts',(9.20897519651,-35.2324135956,0.943972367435));
#52775=CARTESIAN_POINT('Ctrl Pts',(9.19209813045,-35.2892087111,0.939475719579));
#52776=CARTESIAN_POINT('Ctrl Pts',(9.17938477515,-35.3472963111,0.935686471687));
#52777=CARTESIAN_POINT('Ctrl Pts',(9.17095916069,-35.4062580486,0.93263706468));
#52778=CARTESIAN_POINT('Ctrl Pts',(9.16688368582,-35.4656570006,0.930349922162));
#52779=CARTESIAN_POINT('Ctrl Pts',(9.1671566108,-35.5250559527,0.928836133483));
#52780=CARTESIAN_POINT('Ctrl Pts',(9.23916608575,-35.2348774759,0.761379139513));
#52781=CARTESIAN_POINT('Ctrl Pts',(9.22290027765,-35.2906450094,0.757499573794));
#52782=CARTESIAN_POINT('Ctrl Pts',(9.21063507987,-35.3476242625,0.754282164424));
#52783=CARTESIAN_POINT('Ctrl Pts',(9.20248495391,-35.4054228352,0.75175437252));
#52784=CARTESIAN_POINT('Ctrl Pts',(9.19850755669,-35.4636310173,0.749934120027));
#52785=CARTESIAN_POINT('Ctrl Pts',(9.19870123297,-35.5218391995,0.748829315604));
#52786=CARTESIAN_POINT('Ctrl Pts',(9.26569123725,-35.2394333704,0.579580156823));
#52787=CARTESIAN_POINT('Ctrl Pts',(9.25048972376,-35.2934591001,0.575764245003));
#52788=CARTESIAN_POINT('Ctrl Pts',(9.23904456924,-35.3485824305,0.57252390595));
#52789=CARTESIAN_POINT('Ctrl Pts',(9.2314560575,-35.4044472049,0.569884306758));
#52790=CARTESIAN_POINT('Ctrl Pts',(9.22777454338,-35.4606827234,0.567862962924));
#52791=CARTESIAN_POINT('Ctrl Pts',(9.22799848318,-35.5169182418,0.566469053265));
#52792=CARTESIAN_POINT('',(8.84973118842306,-35.1509193774195,2.16703548709451));
#52793=CARTESIAN_POINT('Origin',(9.6131533587965,-35.6438801033176,2.58440681741808));
#52794=CARTESIAN_POINT('Ctrl Pts',(9.26569102913818,-35.2394341100243,0.579580104582361));
#52795=CARTESIAN_POINT('Ctrl Pts',(9.26403312974663,-35.239148763037,0.590944194137194));
#52796=CARTESIAN_POINT('Ctrl Pts',(9.26158621847309,-35.2387686053236,0.607559540293847));
#52797=CARTESIAN_POINT('Ctrl Pts',(9.25830217899466,-35.2382951410448,0.629427757030632));
#52798=CARTESIAN_POINT('Ctrl Pts',(9.25728445574588,-35.2381484145492,0.636204713498013));
#52799=CARTESIAN_POINT('Ctrl Pts',(9.25618617187326,-35.2379926909596,0.643486454517567));
#52800=CARTESIAN_POINT('Ctrl Pts',(9.25500551801042,-35.2378276994222,0.651274021297969));
#52801=CARTESIAN_POINT('Ctrl Pts',(9.25251029507681,-35.2374790022462,0.667732456610143));
#52802=CARTESIAN_POINT('Ctrl Pts',(9.24964752807473,-35.2370897742068,0.686448362167339));
#52803=CARTESIAN_POINT('Ctrl Pts',(9.24639629512545,-35.2366600504234,0.707433024476164));
#52804=CARTESIAN_POINT('Ctrl Pts',(9.24477067865081,-35.2364451885317,0.717925355630576));
#52805=CARTESIAN_POINT('Ctrl Pts',(9.24304788749146,-35.2362201852664,0.728984866587668));
#52806=CARTESIAN_POINT('Ctrl Pts',(9.24122449748462,-35.2359850638432,0.740613678664237));
#52807=CARTESIAN_POINT('Ctrl Pts',(9.2403128024812,-35.2358675031317,0.746428084702522));
#52808=CARTESIAN_POINT('Ctrl Pts',(9.23937594908501,-35.2357474102751,0.75238481461629));
#52809=CARTESIAN_POINT('Ctrl Pts',(9.23841343596212,-35.2356247874065,0.758484137541625));
#52810=CARTESIAN_POINT('Ctrl Pts',(9.23745092283922,-35.2355021645378,0.764583460466961));
#52811=CARTESIAN_POINT('Ctrl Pts',(9.23624270504607,-35.23534931158,0.772210386989164));
#52812=CARTESIAN_POINT('Ctrl Pts',(9.23544835714733,-35.2352493232179,0.777210152233157));
#52813=CARTESIAN_POINT('Ctrl Pts',(9.2296892981416,-35.2345244029677,0.813458681499608));
#52814=CARTESIAN_POINT('Ctrl Pts',(9.2242637536647,-35.2338115087621,0.84699597042143));
#52815=CARTESIAN_POINT('Ctrl Pts',(9.21920351523641,-35.2331082401535,0.87779962226023));
#52816=CARTESIAN_POINT('Ctrl Pts',(9.21868007791685,-35.2330354931791,0.880985990092489));
#52817=CARTESIAN_POINT('Ctrl Pts',(9.2181605375375,-35.2329628898038,0.884143095226426));
#52818=CARTESIAN_POINT('Ctrl Pts',(9.21764492303421,-35.2328904534041,0.887270906919236));
#52819=CARTESIAN_POINT('Ctrl Pts',(9.2148948094202,-35.2325041021135,0.903953598084017));
#52820=CARTESIAN_POINT('Ctrl Pts',(9.21225671553722,-35.2321211437485,0.919803009731216));
#52821=CARTESIAN_POINT('Ctrl Pts',(9.20973657646034,-35.23174158003,0.934814873904563));
#52822=CARTESIAN_POINT('Ctrl Pts',(9.20847650692191,-35.2315517981708,0.942320805991237));
#52823=CARTESIAN_POINT('Ctrl Pts',(9.20724593921839,-35.2313628690998,0.949617353531283));
#52824=CARTESIAN_POINT('Ctrl Pts',(9.2060456977663,-35.2311747873243,0.956704051708735));
#52825=CARTESIAN_POINT('Ctrl Pts',(9.20492302971948,-35.230998861556,0.963332725953723));
#52826=CARTESIAN_POINT('Ctrl Pts',(9.20413921238186,-35.2308745790399,0.967947012534467));
#52827=CARTESIAN_POINT('Ctrl Pts',(9.20281860737665,-35.230659138175,0.975683911631795));
#52828=CARTESIAN_POINT('Ctrl Pts',(9.20272735704886,-35.2306442517786,0.976218510982836));
#52829=CARTESIAN_POINT('Ctrl Pts',(9.20263352908835,-35.2306289206566,0.976768030388192));
#52830=CARTESIAN_POINT('Ctrl Pts',(9.20253682703764,-35.2306130927847,0.977334170225671));
#52831=CARTESIAN_POINT('Ctrl Pts',(9.19494660137613,-35.2293707497539,1.02177096438316));
#52832=CARTESIAN_POINT('Ctrl Pts',(9.18720958723024,-35.227937253375,1.06580927001366));
#52833=CARTESIAN_POINT('Ctrl Pts',(9.17923290862162,-35.2263185653215,1.1093899606357));
#52834=CARTESIAN_POINT('Ctrl Pts',(9.17463050828737,-35.2253846113785,1.13453523662425));
#52835=CARTESIAN_POINT('Ctrl Pts',(9.16994791914426,-35.2243897599338,1.15952755468674));
#52836=CARTESIAN_POINT('Ctrl Pts',(9.1651653249338,-35.2233416856826,1.18435181583264));
#52837=CARTESIAN_POINT('Ctrl Pts',(9.15590037782223,-35.2213113331001,1.23244192268248));
#52838=CARTESIAN_POINT('Ctrl Pts',(9.14628071238575,-35.2190081024355,1.27991064809126));
#52839=CARTESIAN_POINT('Ctrl Pts',(9.13619487560413,-35.216439543141,1.32666161021856));
#52840=CARTESIAN_POINT('Ctrl Pts',(9.1344163009029,-35.2159865936556,1.33490585214889));
#52841=CARTESIAN_POINT('Ctrl Pts',(9.13262326977988,-35.2155255178236,1.34312777745214));
#52842=CARTESIAN_POINT('Ctrl Pts',(9.1308152324794,-35.2150565146126,1.3513268688895));
#52843=CARTESIAN_POINT('Ctrl Pts',(9.13034074638857,-35.2149334333576,1.35347856943432));
#52844=CARTESIAN_POINT('Ctrl Pts',(9.1298652269346,-35.2148098063821,1.35562869749501));
#52845=CARTESIAN_POINT('Ctrl Pts',(9.12938866444621,-35.2146856377966,1.35777724388487));
#52846=CARTESIAN_POINT('Ctrl Pts',(9.12915808535601,-35.2146255603037,1.35881679249367));
#52847=CARTESIAN_POINT('Ctrl Pts',(9.12892834647673,-35.2145656396722,1.35985110818999));
#52848=CARTESIAN_POINT('Ctrl Pts',(9.12869331410367,-35.2145042736238,1.36090772293837));
#52849=CARTESIAN_POINT('Ctrl Pts',(9.12716376995017,-35.2141049155298,1.36778396253803));
#52850=CARTESIAN_POINT('Ctrl Pts',(9.12545911347254,-35.2136565503212,1.37536892283862));
#52851=CARTESIAN_POINT('Ctrl Pts',(9.12407478426825,-35.2132904462239,1.38147563434889));
#52852=CARTESIAN_POINT('Ctrl Pts',(9.12389028593192,-35.213241653208,1.38228951453764));
#52853=CARTESIAN_POINT('Ctrl Pts',(9.12371152874733,-35.2131943436618,1.38307714187556));
#52854=CARTESIAN_POINT('Ctrl Pts',(9.12353972887807,-35.2131488468471,1.38383334339462));
#52855=CARTESIAN_POINT('Ctrl Pts',(9.12344070744131,-35.2131226235444,1.38426920030895));
#52856=CARTESIAN_POINT('Ctrl Pts',(9.12334213194895,-35.2130965085466,1.3847028303091));
#52857=CARTESIAN_POINT('Ctrl Pts',(9.12324311753217,-35.2130702675231,1.38513812626634));
#52858=CARTESIAN_POINT('Ctrl Pts',(9.11672349360445,-35.2113424221221,1.41380027497812));
#52859=CARTESIAN_POINT('Ctrl Pts',(9.10953876734521,-35.2093940202451,1.44425287213694));
#52860=CARTESIAN_POINT('Ctrl Pts',(9.10153909374284,-35.207196182716,1.47643777477174));
#52861=CARTESIAN_POINT('Ctrl Pts',(9.09880004859498,-35.2064436549856,1.48745771205645));
#52862=CARTESIAN_POINT('Ctrl Pts',(9.09596512280942,-35.2056620167299,1.49868049535259));
#52863=CARTESIAN_POINT('Ctrl Pts',(9.09302722159292,-35.2048506613793,1.51010300502745));
#52864=CARTESIAN_POINT('Ctrl Pts',(9.08824275573008,-35.203529343305,1.52870492646046));
#52865=CARTESIAN_POINT('Ctrl Pts',(9.08318537894781,-35.2021290648566,1.54783677119873));
#52866=CARTESIAN_POINT('Ctrl Pts',(9.0778220040167,-35.2006482493061,1.56748158480479));
#52867=CARTESIAN_POINT('Ctrl Pts',(9.06907659420416,-35.1982336616607,1.59951401734633));
#52868=CARTESIAN_POINT('Ctrl Pts',(9.05951839809739,-35.1956030107588,1.63291380893745));
#52869=CARTESIAN_POINT('Ctrl Pts',(9.04897509399545,-35.1927822459941,1.66759275186022));
#52870=CARTESIAN_POINT('Ctrl Pts',(9.04841969275742,-35.192633653463,1.669419572717));
#52871=CARTESIAN_POINT('Ctrl Pts',(9.04786155274224,-35.1924845407158,1.67124993504131));
#52872=CARTESIAN_POINT('Ctrl Pts',(9.04730064717397,-35.1923349140887,1.67308382316031));
#52873=CARTESIAN_POINT('Ctrl Pts',(9.04169629738177,-35.1908399031566,1.69140731837926));
#52874=CARTESIAN_POINT('Ctrl Pts',(9.03580768079979,-35.1893154100858,1.71007792331351));
#52875=CARTESIAN_POINT('Ctrl Pts',(9.02961873353496,-35.1877372787726,1.72908730537306));
#52876=CARTESIAN_POINT('Ctrl Pts',(9.02652425990255,-35.1869482131159,1.73859199640283));
#52877=CARTESIAN_POINT('Ctrl Pts',(9.02335473459722,-35.1861456853932,1.74818142355523));
#52878=CARTESIAN_POINT('Ctrl Pts',(9.02010710682159,-35.1853296928105,1.75785384236612));
#52879=CARTESIAN_POINT('Ctrl Pts',(9.01848329293377,-35.1849216965191,1.76269005177156));
#52880=CARTESIAN_POINT('Ctrl Pts',(9.01683995395626,-35.1845103342624,1.76754700928818));
#52881=CARTESIAN_POINT('Ctrl Pts',(9.01517671455472,-35.1840956050493,1.77242449837224));
#52882=CARTESIAN_POINT('Ctrl Pts',(9.01369720400855,-35.183726688678,1.77676319822028));
#52883=CARTESIAN_POINT('Ctrl Pts',(9.01254229787951,-35.1834395465047,1.78013185822244));
#52884=CARTESIAN_POINT('Ctrl Pts',(9.01080363646111,-35.1830088514207,1.78516241231019));
#52885=CARTESIAN_POINT('Ctrl Pts',(9.01058772568367,-35.1829553667633,1.7857871175188));
#52886=CARTESIAN_POINT('Ctrl Pts',(9.01036275395945,-35.1828996662518,1.78643742390526));
#52887=CARTESIAN_POINT('Ctrl Pts',(9.01012692462632,-35.1828413166113,1.78711834497098));
#52888=CARTESIAN_POINT('Ctrl Pts',(8.99742837262227,-35.1796994006595,1.82378346821384));
#52889=CARTESIAN_POINT('Ctrl Pts',(8.98486577871898,-35.1767195613466,1.85788716927598));
#52890=CARTESIAN_POINT('Ctrl Pts',(8.9726706290217,-35.1739608658519,1.88948106381597));
#52891=CARTESIAN_POINT('Ctrl Pts',(8.96009192469607,-35.1711154054997,1.92206863082239));
#52892=CARTESIAN_POINT('Ctrl Pts',(8.94790633959043,-35.1685046108467,1.9519871584884));
#52893=CARTESIAN_POINT('Ctrl Pts',(8.93635103932819,-35.1661507431013,1.97932121069418));
#52894=CARTESIAN_POINT('Ctrl Pts',(8.92494704640639,-35.1638276973562,2.00629734552448));
#52895=CARTESIAN_POINT('Ctrl Pts',(8.91415801263107,-35.1617538398625,2.03075731440233));
#52896=CARTESIAN_POINT('Ctrl Pts',(8.90417118313868,-35.1599231615189,2.05279228655344));
#52897=CARTESIAN_POINT('Ctrl Pts',(8.89418444606352,-35.1580925001162,2.07482705479488));
#52898=CARTESIAN_POINT('Ctrl Pts',(8.88500010790469,-35.15650417239,2.09443764578029));
#52899=CARTESIAN_POINT('Ctrl Pts',(8.8767549321914,-35.1551387966204,2.11171147529049));
#52900=CARTESIAN_POINT('Ctrl Pts',(8.8682619698602,-35.1537323881481,2.1295044233667));
#52901=CARTESIAN_POINT('Ctrl Pts',(8.8607651973453,-35.1525618856043,2.14481872320988));
#52902=CARTESIAN_POINT('Ctrl Pts',(8.8543606995376,-35.1516033707736,2.15773475299162));
#52903=CARTESIAN_POINT('Ctrl Pts',(8.85274816285252,-35.1513620340796,2.16098677562852));
#52904=CARTESIAN_POINT('Ctrl Pts',(8.85120462911029,-35.1511341487073,2.16408666184874));
#52905=CARTESIAN_POINT('Ctrl Pts',(8.84973117353,-35.1509193731,2.1670354781));
#52906=CARTESIAN_POINT('Ctrl Pts',(8.84972761074,-35.1509187546,2.16704276679));
#52907=CARTESIAN_POINT('Ctrl Pts',(8.80995141052,-35.2405485577,2.13393459289));
#52908=CARTESIAN_POINT('Ctrl Pts',(8.78039709025,-35.3367789605,2.10641485522));
#52909=CARTESIAN_POINT('Ctrl Pts',(8.7619545083,-35.4376105338,2.08522367244));
#52910=CARTESIAN_POINT('Ctrl Pts',(8.75504416849,-35.5407442468,2.0708442184));
#52911=CARTESIAN_POINT('Ctrl Pts',(8.75956299023,-35.6438779598,2.0634404101));
#52912=CARTESIAN_POINT('Ctrl Pts',(8.84456885861,-35.1501669799,2.17736664036));
#52913=CARTESIAN_POINT('Ctrl Pts',(8.80450316343,-35.2400691335,2.14397755154));
#52914=CARTESIAN_POINT('Ctrl Pts',(8.77471769299,-35.3366533562,2.11624485706));
#52915=CARTESIAN_POINT('Ctrl Pts',(8.75611631291,-35.437897274,2.0949212219));
#52916=CARTESIAN_POINT('Ctrl Pts',(8.74912677261,-35.5414726393,2.08049700356));
#52917=CARTESIAN_POINT('Ctrl Pts',(8.75364509765,-35.6450480046,2.07313650893));
#52918=CARTESIAN_POINT('Ctrl Pts',(8.83934134903,-35.1494257084,2.1877279664));
#52919=CARTESIAN_POINT('Ctrl Pts',(8.79900028815,-35.2395949404,2.15403728116));
#52920=CARTESIAN_POINT('Ctrl Pts',(8.76899769743,-35.3365278505,2.12607022447));
#52921=CARTESIAN_POINT('Ctrl Pts',(8.75025126803,-35.4381791278,2.10459258862));
#52922=CARTESIAN_POINT('Ctrl Pts',(8.74319574656,-35.5421912387,2.09010248095));
#52923=CARTESIAN_POINT('Ctrl Pts',(8.74772599292,-35.6462033496,2.08276502103));
#52924=CARTESIAN_POINT('Ctrl Pts',(8.83403961773,-35.1487041475,2.19812825065));
#52925=CARTESIAN_POINT('Ctrl Pts',(8.79343976066,-35.2391345884,2.16411346789));
#52926=CARTESIAN_POINT('Ctrl Pts',(8.76323651939,-35.3364102747,2.1358885387));
#52927=CARTESIAN_POINT('Ctrl Pts',(8.74436113276,-35.4384630225,2.11423302609));
#52928=CARTESIAN_POINT('Ctrl Pts',(8.73725504684,-35.5429059973,2.0996533862));
#52929=CARTESIAN_POINT('Ctrl Pts',(8.74181161845,-35.6473489721,2.09231606717));
#52930=CARTESIAN_POINT('Ctrl Pts',(8.82866432718,-35.1480081194,2.20856250217));
#52931=CARTESIAN_POINT('Ctrl Pts',(8.78782272692,-35.2386939519,2.17420118315));
#52932=CARTESIAN_POINT('Ctrl Pts',(8.75743582295,-35.3363065177,2.14569487681));
#52933=CARTESIAN_POINT('Ctrl Pts',(8.73844810187,-35.4387548314,2.12383756828));
#52934=CARTESIAN_POINT('Ctrl Pts',(8.73130736324,-35.5436227636,2.10914471028));
#52935=CARTESIAN_POINT('Ctrl Pts',(8.73590510583,-35.6484906957,2.1017846051));
#52936=CARTESIAN_POINT('Ctrl Pts',(8.82321744436,-35.1473421125,2.21902489656));
#52937=CARTESIAN_POINT('Ctrl Pts',(8.78215104537,-35.2382777414,2.18429511356));
#52938=CARTESIAN_POINT('Ctrl Pts',(8.75159740651,-35.3362215383,2.15548447298));
#52939=CARTESIAN_POINT('Ctrl Pts',(8.73251395256,-35.4390597803,2.13340204369));
#52940=CARTESIAN_POINT('Ctrl Pts',(8.72535447592,-35.5443470397,2.11857293178));
#52941=CARTESIAN_POINT('Ctrl Pts',(8.73000824887,-35.6496342991,2.1111678244));
#52942=CARTESIAN_POINT('',(8.82321718811955,-35.1473420531381,2.21902512680689));
#52943=CARTESIAN_POINT('Origin',(9.57670448652795,-35.6496380550362,2.64327392285592));
#52944=CARTESIAN_POINT('Ctrl Pts',(8.84972757036633,-35.1509188455761,2.16704273318452));
#52945=CARTESIAN_POINT('Ctrl Pts',(8.84266601721309,-35.1498897248256,2.18117462196919));
#52946=CARTESIAN_POINT('Ctrl Pts',(8.83544640067731,-35.148886344665,2.19539418957044));
#52947=CARTESIAN_POINT('Ctrl Pts',(8.82806096535708,-35.1479465542617,2.20968655179896));
#52948=CARTESIAN_POINT('Ctrl Pts',(8.82645413028913,-35.1477420858572,2.21279611377288));
#52949=CARTESIAN_POINT('Ctrl Pts',(8.82483957760491,-35.1475405449177,2.21590899096587));
#52950=CARTESIAN_POINT('Ctrl Pts',(8.82321740410989,-35.1473422016281,2.21902486252055));
#52951=CARTESIAN_POINT('Ctrl Pts',(8.82321783753,-35.1473399652,2.21902634713));
#52952=CARTESIAN_POINT('Ctrl Pts',(8.78215068074,-35.2382758927,2.18429700681));
#52953=CARTESIAN_POINT('Ctrl Pts',(8.75159630524,-35.3362200688,2.15548691366));
#52954=CARTESIAN_POINT('Ctrl Pts',(8.73251216058,-35.4390587483,2.13340513227));
#52955=CARTESIAN_POINT('Ctrl Pts',(8.72535205902,-35.5443464741,2.11857675734));
#52956=CARTESIAN_POINT('Ctrl Pts',(8.73000528472,-35.6496341999,2.11117245845));
#52957=CARTESIAN_POINT('Ctrl Pts',(8.7950132494,-35.1439026605,2.27318832802));
#52958=CARTESIAN_POINT('Ctrl Pts',(8.75278762749,-35.2361296908,2.23654747651));
#52959=CARTESIAN_POINT('Ctrl Pts',(8.72137526051,-35.3357860213,2.20615712169));
#52960=CARTESIAN_POINT('Ctrl Pts',(8.70180041036,-35.4406403454,2.18290446914));
#52961=CARTESIAN_POINT('Ctrl Pts',(8.69454777529,-35.548095721,2.16736469093));
#52962=CARTESIAN_POINT('Ctrl Pts',(8.69949502688,-35.6555510966,2.15972094562));
#52963=CARTESIAN_POINT('Ctrl Pts',(8.76584958693,-35.140386513,2.32745356943));
#52964=CARTESIAN_POINT('Ctrl Pts',(8.72246681666,-35.2339199765,2.28869203429));
#52965=CARTESIAN_POINT('Ctrl Pts',(8.69020329348,-35.3353435452,2.25654623894));
#52966=CARTESIAN_POINT('Ctrl Pts',(8.67015581074,-35.4422984936,2.23199348318));
#52967=CARTESIAN_POINT('Ctrl Pts',(8.66284221447,-35.5520214947,2.21566670729));
#52968=CARTESIAN_POINT('Ctrl Pts',(8.66812648429,-35.6617444959,2.20776307897));
#52969=CARTESIAN_POINT('Ctrl Pts',(8.7356657971,-35.1367480171,2.38172554964));
#52970=CARTESIAN_POINT('Ctrl Pts',(8.69113780582,-35.2316121539,2.34057114953));
#52971=CARTESIAN_POINT('Ctrl Pts',(8.65803763705,-35.3348781572,2.30644499517));
#52972=CARTESIAN_POINT('Ctrl Pts',(8.63754180367,-35.4440469154,2.28042962134));
#52973=CARTESIAN_POINT('Ctrl Pts',(8.63020353714,-35.5561701517,2.26322602866));
#52974=CARTESIAN_POINT('Ctrl Pts',(8.63587110442,-35.668293388,2.25504712403));
#52975=CARTESIAN_POINT('Ctrl Pts',(8.69114735744,-35.1314764865,2.45847308227));
#52976=CARTESIAN_POINT('Ctrl Pts',(8.64510845073,-35.2282535188,2.41340322951));
#52977=CARTESIAN_POINT('Ctrl Pts',(8.61094346222,-35.3342411346,2.37601936382));
#52978=CARTESIAN_POINT('Ctrl Pts',(8.58994905716,-35.4467225347,2.34758564448));
#52979=CARTESIAN_POINT('Ctrl Pts',(8.58273119234,-35.5624541016,2.32891916373));
#52980=CARTESIAN_POINT('Ctrl Pts',(8.58910725848,-35.6781856686,2.32025995821));
#52981=CARTESIAN_POINT('Ctrl Pts',(8.64411242258,-35.1256902423,2.53413655954));
#52982=CARTESIAN_POINT('Ctrl Pts',(8.59671994041,-35.2244531785,2.48429647903));
#52983=CARTESIAN_POINT('Ctrl Pts',(8.56161211733,-35.333412859,2.44298795985));
#52984=CARTESIAN_POINT('Ctrl Pts',(8.54022333506,-35.4495924912,2.41171677405));
#52985=CARTESIAN_POINT('Ctrl Pts',(8.53321738738,-35.5693865938,2.39145291764));
#52986=CARTESIAN_POINT('Ctrl Pts',(8.54037362589,-35.6891806965,2.38246370607));
#52987=CARTESIAN_POINT('Ctrl Pts',(8.62993676763,-35.1239763388,2.55637951988));
#52988=CARTESIAN_POINT('Ctrl Pts',(8.58219189761,-35.2233231665,2.50503392418));
#52989=CARTESIAN_POINT('Ctrl Pts',(8.54685013234,-35.3331714269,2.46248222847));
#52990=CARTESIAN_POINT('Ctrl Pts',(8.52538633662,-35.4504650834,2.43030855578));
#52991=CARTESIAN_POINT('Ctrl Pts',(8.51848133158,-35.5714859455,2.4095318701));
#52992=CARTESIAN_POINT('Ctrl Pts',(8.52590127043,-35.6925068075,2.40042817508));
#52993=CARTESIAN_POINT('Ctrl Pts',(8.61560772534,-35.1221440943,2.57842131078));
#52994=CARTESIAN_POINT('Ctrl Pts',(8.56749228928,-35.2220926432,2.52550930797));
#52995=CARTESIAN_POINT('Ctrl Pts',(8.53188890827,-35.3328708509,2.48168265536));
#52996=CARTESIAN_POINT('Ctrl Pts',(8.5103168202,-35.4513369446,2.44860878814));
#52997=CARTESIAN_POINT('Ctrl Pts',(8.50347493534,-35.5736522798,2.42735915225));
#52998=CARTESIAN_POINT('Ctrl Pts',(8.51111753906,-35.695967615,2.41821700034));
#52999=CARTESIAN_POINT('Ctrl Pts',(8.60091081429,-35.1203221009,2.60032838611));
#53000=CARTESIAN_POINT('Ctrl Pts',(8.55250194661,-35.2208633123,2.54573382886));
#53001=CARTESIAN_POINT('Ctrl Pts',(8.51670661225,-35.3325772847,2.50053061213));
#53002=CARTESIAN_POINT('Ctrl Pts',(8.49508702343,-35.4522342523,2.46647865078));
#53003=CARTESIAN_POINT('Ctrl Pts',(8.4883597474,-35.5758682626,2.44470657499));
#53004=CARTESIAN_POINT('Ctrl Pts',(8.49626469614,-35.699502273,2.4355053823));
#53005=CARTESIAN_POINT('',(8.60091080648026,-35.1203221517964,2.60032836406496));
#53006=CARTESIAN_POINT('Origin',(9.25479801252791,-35.6995101749192,3.0871775403849));
#53007=CARTESIAN_POINT('Ctrl Pts',(8.8232168869647,-35.1473420700646,2.219025543263));
#53008=CARTESIAN_POINT('Ctrl Pts',(8.79610687645427,-35.1440374725036,2.27108634121779));
#53009=CARTESIAN_POINT('Ctrl Pts',(8.76980417777782,-35.1408675387765,2.31968006431244));
#53010=CARTESIAN_POINT('Ctrl Pts',(8.74448255430243,-35.1378266460975,2.36475221674184));
#53011=CARTESIAN_POINT('Ctrl Pts',(8.72419021923815,-35.1353897244209,2.40087230280402));
#53012=CARTESIAN_POINT('Ctrl Pts',(8.7045250357025,-35.1330382006051,2.43472924958153));
#53013=CARTESIAN_POINT('Ctrl Pts',(8.68559135386596,-35.1307504362116,2.46631895241685));
#53014=CARTESIAN_POINT('Ctrl Pts',(8.6808987964871,-35.1301834326157,2.47414820054808));
#53015=CARTESIAN_POINT('Ctrl Pts',(8.67625129609282,-35.1296202164936,2.4818383635054));
#53016=CARTESIAN_POINT('Ctrl Pts',(8.67165065750585,-35.1290602421153,2.48938977693137));
#53017=CARTESIAN_POINT('Ctrl Pts',(8.6629063577104,-35.1279959151206,2.50374252853918));
#53018=CARTESIAN_POINT('Ctrl Pts',(8.6543265999625,-35.1269464169891,2.51759656768404));
#53019=CARTESIAN_POINT('Ctrl Pts',(8.64591696339239,-35.1259138536027,2.5309581417663));
#53020=CARTESIAN_POINT('Ctrl Pts',(8.63747144758885,-35.1248768848437,2.54437672224015));
#53021=CARTESIAN_POINT('Ctrl Pts',(8.62920242176465,-35.1238537026323,2.55729591434691));
#53022=CARTESIAN_POINT('Ctrl Pts',(8.62111895312701,-35.1228449173309,2.56972204618431));
#53023=CARTESIAN_POINT('Ctrl Pts',(8.61425477167297,-35.121988294306,2.58027385599854));
#53024=CARTESIAN_POINT('Ctrl Pts',(8.60752448890165,-35.1211420059566,2.59047010569892));
#53025=CARTESIAN_POINT('Ctrl Pts',(8.60091082397732,-35.1203221021009,2.60032837167017));
#53026=CARTESIAN_POINT('Ctrl Pts',(8.60091079918,-35.1203221982,2.60032832802));
#53027=CARTESIAN_POINT('Ctrl Pts',(8.55250196755,-35.2208633974,2.5457337616));
#53028=CARTESIAN_POINT('Ctrl Pts',(8.51670667214,-35.3325773527,2.50053052804));
#53029=CARTESIAN_POINT('Ctrl Pts',(8.49508712358,-35.4522342996,2.46647854203));
#53030=CARTESIAN_POINT('Ctrl Pts',(8.48835988758,-35.5758682873,2.44470643423));
#53031=CARTESIAN_POINT('Ctrl Pts',(8.49626487495,-35.6995022751,2.43550520334));
#53032=CARTESIAN_POINT('Ctrl Pts',(8.56160117875,-35.1140346808,2.66060541831));
#53033=CARTESIAN_POINT('Ctrl Pts',(8.51158038352,-35.2164638336,2.60178050099));
#53034=CARTESIAN_POINT('Ctrl Pts',(8.47440952478,-35.3311106273,2.55334779448));
#53035=CARTESIAN_POINT('Ctrl Pts',(8.45180416694,-35.454476252,2.51731779839));
#53036=CARTESIAN_POINT('Ctrl Pts',(8.44456120074,-35.5822080931,2.49495976327));
#53037=CARTESIAN_POINT('Ctrl Pts',(8.45240512852,-35.7099399342,2.48655698047));
#53038=CARTESIAN_POINT('Ctrl Pts',(8.51829161967,-35.1086508497,2.71924356476));
#53039=CARTESIAN_POINT('Ctrl Pts',(8.4676782837,-35.2126508331,2.65547482048));
#53040=CARTESIAN_POINT('Ctrl Pts',(8.42997337302,-35.3299187074,2.6031885652));
#53041=CARTESIAN_POINT('Ctrl Pts',(8.40701812301,-35.4566921944,2.56468900549));
#53042=CARTESIAN_POINT('Ctrl Pts',(8.39967272263,-35.5882267707,2.5414121675));
#53043=CARTESIAN_POINT('Ctrl Pts',(8.40764108873,-35.7197613468,2.53363446576));
#53044=CARTESIAN_POINT('Ctrl Pts',(8.47165311425,-35.1035435988,2.77475885702));
#53045=CARTESIAN_POINT('Ctrl Pts',(8.42103112523,-35.2090000749,2.7055559059));
#53046=CARTESIAN_POINT('Ctrl Pts',(8.38318247508,-35.3288584812,2.64914965253));
#53047=CARTESIAN_POINT('Ctrl Pts',(8.36006509714,-35.4590804193,2.60819117966));
#53048=CARTESIAN_POINT('Ctrl Pts',(8.35259991719,-35.5944943118,2.58430328363));
#53049=CARTESIAN_POINT('Ctrl Pts',(8.36047222003,-35.7299082045,2.5777319381));
#53050=CARTESIAN_POINT('Ctrl Pts',(8.35159188251,-35.0922845623,2.89275323394));
#53051=CARTESIAN_POINT('Ctrl Pts',(8.3050322624,-35.2005432762,2.80975608337));
#53052=CARTESIAN_POINT('Ctrl Pts',(8.26959869952,-35.3257180408,2.7430273545));
#53053=CARTESIAN_POINT('Ctrl Pts',(8.2473160419,-35.4631716043,2.69610840641));
#53054=CARTESIAN_POINT('Ctrl Pts',(8.23918506507,-35.6067794199,2.67107903223));
#53055=CARTESIAN_POINT('Ctrl Pts',(8.24494252704,-35.7503872354,2.66806485365));
#53056=CARTESIAN_POINT('Ctrl Pts',(8.20219946581,-35.0869079403,2.96964215712));
#53057=CARTESIAN_POINT('Ctrl Pts',(8.17044511261,-35.196070615,2.87494321335));
#53058=CARTESIAN_POINT('Ctrl Pts',(8.14524485361,-35.3234854768,2.79971065515));
#53059=CARTESIAN_POINT('Ctrl Pts',(8.12806473503,-35.4642227883,2.74824760952));
#53060=CARTESIAN_POINT('Ctrl Pts',(8.11972374517,-35.6116396625,2.72298240153));
#53061=CARTESIAN_POINT('Ctrl Pts',(8.12018530542,-35.7590565367,2.723855906));
#53062=CARTESIAN_POINT('Ctrl Pts',(8.10597427981,-35.0887550559,2.98941073315));
#53063=CARTESIAN_POINT('Ctrl Pts',(8.08828816032,-35.1976252196,2.89277147723));
#53064=CARTESIAN_POINT('Ctrl Pts',(8.07262669454,-35.3241767484,2.81647388405));
#53065=CARTESIAN_POINT('Ctrl Pts',(8.05970660483,-35.4635970156,2.76481016119));
#53066=CARTESIAN_POINT('Ctrl Pts',(8.05010223161,-35.6094680649,2.74015988873));
#53067=CARTESIAN_POINT('Ctrl Pts',(8.0441099093,-35.7553391142,2.74240669266));
#53068=CARTESIAN_POINT('Ctrl Pts',(7.82075728158,-35.1140008873,2.95981413055));
#53069=CARTESIAN_POINT('Ctrl Pts',(7.83753302833,-35.2174511648,2.88177682176));
#53070=CARTESIAN_POINT('Ctrl Pts',(7.84624727736,-35.3324220766,2.81978760483));
#53071=CARTESIAN_POINT('Ctrl Pts',(7.84611816579,-35.4555224941,2.77624706117));
#53072=CARTESIAN_POINT('Ctrl Pts',(7.83704746541,-35.5826911821,2.75255272839));
#53073=CARTESIAN_POINT('Ctrl Pts',(7.81966214074,-35.7098598702,2.74888110871));
#53074=CARTESIAN_POINT('Ctrl Pts',(7.56538653659,-35.1573736159,2.76989788484));
#53075=CARTESIAN_POINT('Ctrl Pts',(7.58792144694,-35.2456787757,2.72783328434));
#53076=CARTESIAN_POINT('Ctrl Pts',(7.60265321273,-35.3389337113,2.69350582125));
#53077=CARTESIAN_POINT('Ctrl Pts',(7.60913119693,-35.4355529064,2.66745188002));
#53078=CARTESIAN_POINT('Ctrl Pts',(7.60718914349,-35.5338539365,2.65003275892));
#53079=CARTESIAN_POINT('Ctrl Pts',(7.59696106493,-35.6321549665,2.64143245401));
#53080=CARTESIAN_POINT('Ctrl Pts',(7.43180190579,-35.1865123729,2.62065670169));
#53081=CARTESIAN_POINT('Ctrl Pts',(7.44817986306,-35.2646063876,2.59073345827));
#53082=CARTESIAN_POINT('Ctrl Pts',(7.45830517498,-35.3457624596,2.56600593478));
#53083=CARTESIAN_POINT('Ctrl Pts',(7.46204607379,-35.4290060284,2.5468488602));
#53084=CARTESIAN_POINT('Ctrl Pts',(7.45940380717,-35.5132946093,2.53351481199));
#53085=CARTESIAN_POINT('Ctrl Pts',(7.45050807009,-35.5975831903,2.52611015512));
#53086=CARTESIAN_POINT('Ctrl Pts',(7.32065041948,-35.231204862,2.4495725015));
#53087=CARTESIAN_POINT('Ctrl Pts',(7.32870713782,-35.2926200315,2.43080253154));
#53088=CARTESIAN_POINT('Ctrl Pts',(7.33308472128,-35.3551340146,2.41429805269));
#53089=CARTESIAN_POINT('Ctrl Pts',(7.33374284515,-35.4183882264,2.40016471574));
#53090=CARTESIAN_POINT('Ctrl Pts',(7.33068095224,-35.4820120082,2.3884845177));
#53091=CARTESIAN_POINT('Ctrl Pts',(7.3239386903,-35.5456357901,2.37931366962));
#53092=CARTESIAN_POINT('Ctrl Pts',(7.23545016815,-35.2863172732,2.26690461593));
#53093=CARTESIAN_POINT('Ctrl Pts',(7.23845227406,-35.3245433701,2.25650461508));
#53094=CARTESIAN_POINT('Ctrl Pts',(7.23974688842,-35.3631516089,2.24701631825));
#53095=CARTESIAN_POINT('Ctrl Pts',(7.23932413184,-35.4020162898,2.23847392839));
#53096=CARTESIAN_POINT('Ctrl Pts',(7.23718539906,-35.4410091937,2.23090562784));
#53097=CARTESIAN_POINT('Ctrl Pts',(7.23334333153,-35.4800020975,2.22433302544));
#53098=CARTESIAN_POINT('',(7.23545016824,-35.2863172732,2.26690461571));
#53099=CARTESIAN_POINT('Origin',(6.36960344412454,-35.479838822465,2.72827074076366));
#53100=CARTESIAN_POINT('Ctrl Pts',(8.60091078277638,-35.1203221955763,2.60032835317319));
#53101=CARTESIAN_POINT('Ctrl Pts',(8.58917610193419,-35.1184452509957,2.61832222716226));
#53102=CARTESIAN_POINT('Ctrl Pts',(8.57728470874417,-35.1167058413131,2.63573050335558));
#53103=CARTESIAN_POINT('Ctrl Pts',(8.56529427331913,-35.1150637609194,2.65251831753478));
#53104=CARTESIAN_POINT('Ctrl Pts',(8.55099972592246,-35.1131061342624,2.67253211995018));
#53105=CARTESIAN_POINT('Ctrl Pts',(8.53656330828631,-35.111286670445,2.69166387430586));
#53106=CARTESIAN_POINT('Ctrl Pts',(8.52202055329917,-35.1095697609073,2.70987559519324));
#53107=CARTESIAN_POINT('Ctrl Pts',(8.50426881377531,-35.1074740004461,2.73210588964294));
#53108=CARTESIAN_POINT('Ctrl Pts',(8.486356211608,-35.1055309944711,2.75296492849583));
#53109=CARTESIAN_POINT('Ctrl Pts',(8.46829397397454,-35.1037232384762,2.77241831890468));
#53110=CARTESIAN_POINT('Ctrl Pts',(8.46261694272413,-35.1031550537648,2.77853259486088));
#53111=CARTESIAN_POINT('Ctrl Pts',(8.45692495431307,-35.1026005215558,2.78450824985457));
#53112=CARTESIAN_POINT('Ctrl Pts',(8.45121810078767,-35.1020597946337,2.79034482063747));
#53113=CARTESIAN_POINT('Ctrl Pts',(8.43432545266925,-35.1004592086746,2.80762144005914));
#53114=CARTESIAN_POINT('Ctrl Pts',(8.41733375422917,-35.0989820350092,2.82364203030634));
#53115=CARTESIAN_POINT('Ctrl Pts',(8.40032031728529,-35.0976458319203,2.83837096012391));
#53116=CARTESIAN_POINT('Ctrl Pts',(8.38795424262058,-35.0966746238558,2.84907655984819));
#53117=CARTESIAN_POINT('Ctrl Pts',(8.37557737559973,-35.0957782495222,2.85910048902354));
#53118=CARTESIAN_POINT('Ctrl Pts',(8.3632291411423,-35.0949650753447,2.86844300309122));
#53119=CARTESIAN_POINT('Ctrl Pts',(8.3539353921421,-35.0943530496559,2.87547453307028));
#53120=CARTESIAN_POINT('Ctrl Pts',(8.34465680857996,-35.093788343402,2.88212050144329));
#53121=CARTESIAN_POINT('Ctrl Pts',(8.3354083784926,-35.0932769063359,2.88837545665666));
#53122=CARTESIAN_POINT('Ctrl Pts',(8.32900129505229,-35.0929225953959,2.89270873480106));
#53123=CARTESIAN_POINT('Ctrl Pts',(8.32260855403078,-35.092593762051,2.89685478584779));
#53124=CARTESIAN_POINT('Ctrl Pts',(8.31623077045352,-35.0923064282237,2.90080259475859));
#53125=CARTESIAN_POINT('Ctrl Pts',(8.31280674181222,-35.0921521678536,2.90292204748338));
#53126=CARTESIAN_POINT('Ctrl Pts',(8.30969504858464,-35.0920187697158,2.90480270397685));
#53127=CARTESIAN_POINT('Ctrl Pts',(8.30640603496327,-35.0918832744635,2.90674804194051));
#53128=CARTESIAN_POINT('Ctrl Pts',(8.30356875138995,-35.091766388826,2.90842619718226));
#53129=CARTESIAN_POINT('Ctrl Pts',(8.30059929606858,-35.091647958914,2.91015229702004));
#53130=CARTESIAN_POINT('Ctrl Pts',(8.29716922778335,-35.0915180419732,2.91209426874943));
#53131=CARTESIAN_POINT('Ctrl Pts',(8.27979366790461,-35.090859926916,2.92193163735584));
#53132=CARTESIAN_POINT('Ctrl Pts',(8.26173356240834,-35.0904306146764,2.93082766696923));
#53133=CARTESIAN_POINT('Ctrl Pts',(8.24304079174056,-35.0902526066801,2.93858623998578));
#53134=CARTESIAN_POINT('Ctrl Pts',(8.22466218351964,-35.090077590398,2.94621441755019));
#53135=CARTESIAN_POINT('Ctrl Pts',(8.20567267299626,-35.0901458262032,2.95274233402127));
#53136=CARTESIAN_POINT('Ctrl Pts',(8.18615591579075,-35.0904679947241,2.95801774934341));
#53137=CARTESIAN_POINT('Ctrl Pts',(8.16746736263975,-35.090776491851,2.96306929958833));
#53138=CARTESIAN_POINT('Ctrl Pts',(8.14829603416996,-35.0913180639787,2.96697197928371));
#53139=CARTESIAN_POINT('Ctrl Pts',(8.12873716243942,-35.0920882419806,2.96963148379715));
#53140=CARTESIAN_POINT('Ctrl Pts',(8.11865524740541,-35.0924852418322,2.97100236545671));
#53141=CARTESIAN_POINT('Ctrl Pts',(8.10847066029314,-35.0929427332427,2.97204361753943));
#53142=CARTESIAN_POINT('Ctrl Pts',(8.0981980181784,-35.0934582459642,2.97274725844121));
#53143=CARTESIAN_POINT('Ctrl Pts',(8.08015267138847,-35.0943638168709,2.97398330306794));
#53144=CARTESIAN_POINT('Ctrl Pts',(8.06184274437113,-35.0954494821579,2.97417418802722));
#53145=CARTESIAN_POINT('Ctrl Pts',(8.04334631915808,-35.0967195517063,2.97328424046987));
#53146=CARTESIAN_POINT('Ctrl Pts',(8.02484989394504,-35.0979896212546,2.97239429291251));
#53147=CARTESIAN_POINT('Ctrl Pts',(8.00616731932893,-35.0994444577115,2.97042256570926));
#53148=CARTESIAN_POINT('Ctrl Pts',(7.98738597285875,-35.1010686618494,2.9673822556833));
#53149=CARTESIAN_POINT('Ctrl Pts',(7.97066809495794,-35.1025144179621,2.96467597837378));
#53150=CARTESIAN_POINT('Ctrl Pts',(7.95387087369368,-35.1040979718286,2.96112003542471));
#53151=CARTESIAN_POINT('Ctrl Pts',(7.93704940278452,-35.1058237688537,2.95673871879764));
#53152=CARTESIAN_POINT('Ctrl Pts',(7.93497314784849,-35.1060367820089,2.95619793789196));
#53153=CARTESIAN_POINT('Ctrl Pts',(7.93289652996833,-35.1062519371957,2.95564464311045));
#53154=CARTESIAN_POINT('Ctrl Pts',(7.93081965722235,-35.1064692208014,2.95507893330937));
#53155=CARTESIAN_POINT('Ctrl Pts',(7.92521992861369,-35.1070550675875,2.95355364902636));
#53156=CARTESIAN_POINT('Ctrl Pts',(7.91978314717724,-35.1076390206973,2.95198445505272));
#53157=CARTESIAN_POINT('Ctrl Pts',(7.91436359224073,-35.10823574807,2.95033900501678));
#53158=CARTESIAN_POINT('Ctrl Pts',(7.90716727929602,-35.1090281077686,2.94815410726553));
#53159=CARTESIAN_POINT('Ctrl Pts',(7.90000082482723,-35.109842835178,2.94583637364108));
#53160=CARTESIAN_POINT('Ctrl Pts',(7.89252934979934,-35.1107229006809,2.94326130335969));
#53161=CARTESIAN_POINT('Ctrl Pts',(7.88663293685535,-35.1114174395241,2.94122908379365));
#53162=CARTESIAN_POINT('Ctrl Pts',(7.88054664524848,-35.1121527743485,2.93903571473777));
#53163=CARTESIAN_POINT('Ctrl Pts',(7.87411160248055,-35.1129524516452,2.93659796655904));
#53164=CARTESIAN_POINT('Ctrl Pts',(7.85178409221608,-35.1157270723736,2.92813977141633));
#53165=CARTESIAN_POINT('Ctrl Pts',(7.83002035558917,-35.1185929240505,2.91859695159043));
#53166=CARTESIAN_POINT('Ctrl Pts',(7.80885347336691,-35.1215334987328,2.90819436721776));
#53167=CARTESIAN_POINT('Ctrl Pts',(7.78669331944508,-35.1246120620703,2.89730363383233));
#53168=CARTESIAN_POINT('Ctrl Pts',(7.76518706636089,-35.1277727811105,2.8854701648589));
#53169=CARTESIAN_POINT('Ctrl Pts',(7.74434798348236,-35.131009993278,2.87289903692657));
#53170=CARTESIAN_POINT('Ctrl Pts',(7.72194176304155,-35.1344906497859,2.85938253693071));
#53171=CARTESIAN_POINT('Ctrl Pts',(7.70030659658197,-35.13805998044,2.84501305436895));
#53172=CARTESIAN_POINT('Ctrl Pts',(7.67943512205773,-35.1417219917774,2.82999016953254));
#53173=CARTESIAN_POINT('Ctrl Pts',(7.66940064330848,-35.1434825945035,2.82276754525325));
#53174=CARTESIAN_POINT('Ctrl Pts',(7.65954237285627,-35.145264752053,2.81539312665641));
#53175=CARTESIAN_POINT('Ctrl Pts',(7.64985798668585,-35.1470694734924,2.80788525165147));
#53176=CARTESIAN_POINT('Ctrl Pts',(7.62746593570419,-35.1512423156082,2.79052568782199));
#53177=CARTESIAN_POINT('Ctrl Pts',(7.605962048854,-35.1555301903078,2.77243218743555));
#53178=CARTESIAN_POINT('Ctrl Pts',(7.58531700118153,-35.1599302545228,2.75379953157052));
#53179=CARTESIAN_POINT('Ctrl Pts',(7.56258151710616,-35.1647758519502,2.73328020618935));
#53180=CARTESIAN_POINT('Ctrl Pts',(7.54088706090647,-35.1697577951558,2.71210682642349));
#53181=CARTESIAN_POINT('Ctrl Pts',(7.52017550611949,-35.1748791194298,2.69047562713645));
#53182=CARTESIAN_POINT('Ctrl Pts',(7.50387682178431,-35.1789092778886,2.67345324071511));
#53183=CARTESIAN_POINT('Ctrl Pts',(7.48818634156458,-35.1830259232671,2.65614587070935));
#53184=CARTESIAN_POINT('Ctrl Pts',(7.47307198757317,-35.1872314367054,2.63862717712488));
#53185=CARTESIAN_POINT('Ctrl Pts',(7.44966633781327,-35.1937439727128,2.61149823687892));
#53186=CARTESIAN_POINT('Ctrl Pts',(7.42764987581756,-35.2004199946401,2.5839035859179));
#53187=CARTESIAN_POINT('Ctrl Pts',(7.40692166842936,-35.2073161032801,2.55604515563927));
#53188=CARTESIAN_POINT('Ctrl Pts',(7.38524454731482,-35.2145279079194,2.52691139815117));
#53189=CARTESIAN_POINT('Ctrl Pts',(7.36497569430883,-35.2219812711745,2.49748815499357));
#53190=CARTESIAN_POINT('Ctrl Pts',(7.34600061535571,-35.2297053851017,2.46796359042044));
#53191=CARTESIAN_POINT('Ctrl Pts',(7.32695265854947,-35.2374591651421,2.43832563043612));
#53192=CARTESIAN_POINT('Ctrl Pts',(7.30920790752505,-35.2454861433858,2.40858460195775));
#53193=CARTESIAN_POINT('Ctrl Pts',(7.29266038923334,-35.2537717794306,2.37890422579583));
#53194=CARTESIAN_POINT('Ctrl Pts',(7.27609198391715,-35.2620678739792,2.34918638572348));
#53195=CARTESIAN_POINT('Ctrl Pts',(7.26072345811695,-35.2706233461039,2.31952874737719));
#53196=CARTESIAN_POINT('Ctrl Pts',(7.24646506941255,-35.2793763104888,2.29008084435969));
#53197=CARTESIAN_POINT('Ctrl Pts',(7.24271708980018,-35.281677126713,2.28234012818025));
#53198=CARTESIAN_POINT('Ctrl Pts',(7.23904592126134,-35.2839913349288,2.2746138487812));
#53199=CARTESIAN_POINT('Ctrl Pts',(7.23545016815,-35.2863172732,2.26690461593));
#53200=CARTESIAN_POINT('Ctrl Pts',(7.23545146011,-35.2863120169,2.26690923839));
#53201=CARTESIAN_POINT('Ctrl Pts',(7.2384543,-35.3245396537,2.25650943661));
#53202=CARTESIAN_POINT('Ctrl Pts',(7.23974953205,-35.3631494767,2.24702142178));
#53203=CARTESIAN_POINT('Ctrl Pts',(7.23932727374,-35.4020157716,2.23847939875));
#53204=CARTESIAN_POINT('Ctrl Pts',(7.23718891826,-35.4410103045,2.23091155076));
#53205=CARTESIAN_POINT('Ctrl Pts',(7.23334710717,-35.4800048374,2.2243394865));
#53206=CARTESIAN_POINT('Ctrl Pts',(7.23162479878,-35.288610995,2.25877896783));
#53207=CARTESIAN_POINT('Ctrl Pts',(7.23442685161,-35.3258445567,2.2487681051));
#53208=CARTESIAN_POINT('Ctrl Pts',(7.23560643854,-35.3634294381,2.2396106895));
#53209=CARTESIAN_POINT('Ctrl Pts',(7.2351548746,-35.4012499853,2.23133779585));
#53210=CARTESIAN_POINT('Ctrl Pts',(7.2330735745,-35.4391883682,2.22397519179));
#53211=CARTESIAN_POINT('Ctrl Pts',(7.22937402512,-35.477126751,2.21754286118));
#53212=CARTESIAN_POINT('Ctrl Pts',(7.22786970762,-35.291024056,2.2506285999));
#53213=CARTESIAN_POINT('Ctrl Pts',(7.23046153941,-35.32723074,2.24098939513));
#53214=CARTESIAN_POINT('Ctrl Pts',(7.23151609908,-35.3637591309,2.23214656382));
#53215=CARTESIAN_POINT('Ctrl Pts',(7.23102584019,-35.4005032431,2.22412829997));
#53216=CARTESIAN_POINT('Ctrl Pts',(7.22899220964,-35.437355218,2.21695813089));
#53217=CARTESIAN_POINT('Ctrl Pts',(7.22542564343,-35.4742071929,2.21065452768));
#53218=CARTESIAN_POINT('Ctrl Pts',(7.22418450574,-35.2935251725,2.24246594859));
#53219=CARTESIAN_POINT('Ctrl Pts',(7.22656046023,-35.328675405,2.23318153594));
#53220=CARTESIAN_POINT('Ctrl Pts',(7.22748386956,-35.3641192075,2.22463810729));
#53221=CARTESIAN_POINT('Ctrl Pts',(7.22694822371,-35.3997598036,2.21686121842));
#53222=CARTESIAN_POINT('Ctrl Pts',(7.22495501199,-35.4354987894,2.20987233634));
#53223=CARTESIAN_POINT('Ctrl Pts',(7.22151371785,-35.4712377752,2.20368850558));
#53224=CARTESIAN_POINT('Ctrl Pts',(7.22057030307,-35.2960900286,2.23430349206));
#53225=CARTESIAN_POINT('Ctrl Pts',(7.22272782881,-35.3301573964,2.22535702652));
#53226=CARTESIAN_POINT('Ctrl Pts',(7.22351653394,-35.364491827,2.21709818648));
#53227=CARTESIAN_POINT('Ctrl Pts',(7.22293085753,-35.3990052196,2.20955010655));
#53228=CARTESIAN_POINT('Ctrl Pts',(7.22097232999,-35.4336080936,2.20273236154));
#53229=CARTESIAN_POINT('Ctrl Pts',(7.21764954964,-35.4682109676,2.19666066586));
#53230=CARTESIAN_POINT('Ctrl Pts',(7.21702826363,-35.2986939836,2.22615331206));
#53231=CARTESIAN_POINT('Ctrl Pts',(7.21896725362,-35.3316545144,2.21752775213));
#53232=CARTESIAN_POINT('Ctrl Pts',(7.21961969567,-35.3648573041,2.20953871906));
#53233=CARTESIAN_POINT('Ctrl Pts',(7.21898088241,-35.3982223851,2.20220714146));
#53234=CARTESIAN_POINT('Ctrl Pts',(7.21705236747,-35.4316686126,2.19555084997));
#53235=CARTESIAN_POINT('Ctrl Pts',(7.2138419429,-35.46511484,2.18958431883));
#53236=CARTESIAN_POINT('',(7.21702820316688,-35.2986940627524,2.2261532291923));
#53237=CARTESIAN_POINT('Origin',(6.33322480789846,-35.4651139210737,2.66341322968104));
#53238=CARTESIAN_POINT('Ctrl Pts',(7.23545016822504,-35.2863172732034,2.26690461571799));
#53239=CARTESIAN_POINT('Ctrl Pts',(7.22907209381996,-35.2901447245619,2.25335534879862));
#53240=CARTESIAN_POINT('Ctrl Pts',(7.22293091414826,-35.2943546089202,2.23973522296192));
#53241=CARTESIAN_POINT('Ctrl Pts',(7.21702826419444,-35.298693983185,2.22615331335877));
#53242=CARTESIAN_POINT('Ctrl Pts',(7.07911993306,-35.3742356128,1.41233341424));
#53243=CARTESIAN_POINT('Ctrl Pts',(7.50890612221,-32.4742356128,3.82595376918));
#53244=CARTESIAN_POINT('Ctrl Pts',(7.09439816601,-35.3742356128,1.56936058085));
#53245=CARTESIAN_POINT('Ctrl Pts',(7.59518497882,-32.4742356128,4.00539873882));
#53246=CARTESIAN_POINT('Ctrl Pts',(7.10532841684,-35.3742356128,1.72680313633));
#53247=CARTESIAN_POINT('Ctrl Pts',(7.6797307274,-32.4742356128,4.18568800425));
#53248=CARTESIAN_POINT('Ctrl Pts',(7.08904842402,-35.3742356128,1.89842406838));
#53249=CARTESIAN_POINT('Ctrl Pts',(7.76642508589,-32.4742356128,4.37540694872));
#53250=CARTESIAN_POINT('Ctrl Pts',(7.1390862001,-35.3742356128,2.05065495714));
#53251=CARTESIAN_POINT('Ctrl Pts',(7.84739395748,-32.4742356128,4.5573230698));
#53252=CARTESIAN_POINT('Ctrl Pts',(7.21384189758,-35.3742356128,2.18958432614));
#53253=CARTESIAN_POINT('Ctrl Pts',(7.92659403983,-32.4742356128,4.74000601033));
#53254=CARTESIAN_POINT('Ctrl Pts',(7.21702817531,-35.2986941477,2.22615317529));
#53255=CARTESIAN_POINT('Ctrl Pts',(7.20692741189441,-35.3061131910589,2.20294516691052));
#53256=CARTESIAN_POINT('Ctrl Pts',(7.19719329525834,-35.3141912841077,2.17900438661006));
#53257=CARTESIAN_POINT('Ctrl Pts',(7.18796980246911,-35.3226070668248,2.15465538142052));
#53258=CARTESIAN_POINT('Ctrl Pts',(7.18234237094649,-35.3277416987947,2.1397995819442));
#53259=CARTESIAN_POINT('Ctrl Pts',(7.17690465211826,-35.3330009806929,2.12479257546628));
#53260=CARTESIAN_POINT('Ctrl Pts',(7.17168536591732,-35.3383049690758,2.10971258769397));
#53261=CARTESIAN_POINT('Ctrl Pts',(7.16774304131616,-35.342311272444,2.0983221016215));
#53262=CARTESIAN_POINT('Ctrl Pts',(7.16392050826559,-35.3463755747386,2.08687105022291));
#53263=CARTESIAN_POINT('Ctrl Pts',(7.160224977354,-35.3504229454298,2.07538760256753));
#53264=CARTESIAN_POINT('Ctrl Pts',(7.15647459950107,-35.3545303848657,2.06373372419597));
#53265=CARTESIAN_POINT('Ctrl Pts',(7.15285530677851,-35.3586203097449,2.05204630782424));
#53266=CARTESIAN_POINT('Ctrl Pts',(7.14937553131797,-35.3626673165653,2.0403417618537));
#53267=CARTESIAN_POINT('Ctrl Pts',(7.14731388684394,-35.3650650256538,2.0334072303603));
#53268=CARTESIAN_POINT('Ctrl Pts',(7.14530121097212,-35.3674486946293,2.02646644336296));
#53269=CARTESIAN_POINT('Ctrl Pts',(7.14333877168014,-35.3698214557652,2.01952124225387));
#53270=CARTESIAN_POINT('Ctrl Pts',(7.14233333890139,-35.3710371121333,2.01596294983756));
#53271=CARTESIAN_POINT('Ctrl Pts',(7.14133929086511,-35.3722572507634,2.01239698022069));
#53272=CARTESIAN_POINT('Ctrl Pts',(7.14035958693292,-35.3734664689908,2.00883384018665));
#53273=CARTESIAN_POINT('Ctrl Pts',(7.1401507215652,-35.3737242650467,2.00807420604723));
#53274=CARTESIAN_POINT('Ctrl Pts',(7.13994249884667,-35.3739817495794,2.00731466330882));
#53275=CARTESIAN_POINT('Ctrl Pts',(7.13973493084178,-35.3742390721046,2.00655525500559));
#53276=CARTESIAN_POINT('',(7.50890612221,-32.4742356128,3.82595376918));
#53277=CARTESIAN_POINT('',(7.07911993306,-35.3742356128,1.41233341424));
#53278=CARTESIAN_POINT('',(7.92659403983,-32.4742356128,4.74000601033));
#53279=CARTESIAN_POINT('Ctrl Pts',(7.92659403983,-32.4742356128,4.74000601033));
#53280=CARTESIAN_POINT('Ctrl Pts',(7.85943746120676,-32.4742356128,4.5851026201465));
#53281=CARTESIAN_POINT('Ctrl Pts',(7.79122837465513,-32.4742356128,4.43204332025208));
#53282=CARTESIAN_POINT('Ctrl Pts',(7.65314300948379,-32.4742356128,4.12986259549018));
#53283=CARTESIAN_POINT('Ctrl Pts',(7.58206613679357,-32.4742356128,3.97811383610292));
#53284=CARTESIAN_POINT('Ctrl Pts',(7.50890612221,-32.4742356128,3.82595376918));
#53285=CARTESIAN_POINT('',(7.23545016824,-35.2863172732,2.26690461571));
#53286=CARTESIAN_POINT('Ctrl Pts',(7.21702817531,-35.2986941477,2.22615317529));
#53287=CARTESIAN_POINT('Ctrl Pts',(7.21896716995,-35.3316547085,2.21752764579));
#53288=CARTESIAN_POINT('Ctrl Pts',(7.21961961863,-35.364857528,2.20953864245));
#53289=CARTESIAN_POINT('Ctrl Pts',(7.218980814,-35.3982226387,2.20220709377));
#53290=CARTESIAN_POINT('Ctrl Pts',(7.21705230964,-35.4316688958,2.19555083028));
#53291=CARTESIAN_POINT('Ctrl Pts',(7.21384189758,-35.4651151528,2.18958432614));
#53292=CARTESIAN_POINT('Ctrl Pts',(7.18673962782,-35.3208994409,2.15657660598));
#53293=CARTESIAN_POINT('Ctrl Pts',(7.18679863605,-35.3444227249,2.15079574742));
#53294=CARTESIAN_POINT('Ctrl Pts',(7.18629633971,-35.3679639778,2.14519357364));
#53295=CARTESIAN_POINT('Ctrl Pts',(7.18523498451,-35.3915169062,2.13977082956));
#53296=CARTESIAN_POINT('Ctrl Pts',(7.18361579364,-35.4150756718,2.13452906411));
#53297=CARTESIAN_POINT('Ctrl Pts',(7.18143896677,-35.4386344375,2.12947072768));
#53298=CARTESIAN_POINT('Ctrl Pts',(7.16019775778,-35.3488473737,2.08142068745));
#53299=CARTESIAN_POINT('Ctrl Pts',(7.15961328066171,-35.3598678430844,2.07926829342153));
#53300=CARTESIAN_POINT('Ctrl Pts',(7.15902631490073,-35.370880846883,2.07710680880288));
#53301=CARTESIAN_POINT('Ctrl Pts',(7.15843669056073,-35.3818889651522,2.07493560863704));
#53302=CARTESIAN_POINT('Ctrl Pts',(7.15784419952897,-35.3928946462221,2.07275392853839));
#53303=CARTESIAN_POINT('Ctrl Pts',(7.15724858875,-35.4039003382,2.07056083977));
#53304=CARTESIAN_POINT('Ctrl Pts',(7.13973478936,-35.3742392475,2.00655473738));
#53305=CARTESIAN_POINT('Ctrl Pts',(7.13973478936,-35.3742392475,2.00655473738));
#53306=CARTESIAN_POINT('Ctrl Pts',(7.13973478936,-35.3742392475,2.00655473738));
#53307=CARTESIAN_POINT('Ctrl Pts',(7.13973478936,-35.3742392475,2.00655473738));
#53308=CARTESIAN_POINT('Ctrl Pts',(7.13973478936,-35.3742392475,2.00655473738));
#53309=CARTESIAN_POINT('Ctrl Pts',(7.13973478936,-35.3742392475,2.00655473738));
#53310=CARTESIAN_POINT('Ctrl Pts',(3.67755458085804,-35.3742402223328,-3.05915165400695));
#53311=CARTESIAN_POINT('Ctrl Pts',(3.32386409198,-32.4742356128,-2.36922853848));
#53312=CARTESIAN_POINT('Ctrl Pts',(4.22884588785004,-35.3742402223328,-2.83736811841901));
#53313=CARTESIAN_POINT('Ctrl Pts',(3.82968047509,-32.4742356128,-1.81532491987));
#53314=CARTESIAN_POINT('Ctrl Pts',(4.75872544102183,-35.3742402223328,-2.56236102730882));
#53315=CARTESIAN_POINT('Ctrl Pts',(4.31529317605,-32.4742356128,-1.24297128633));
#53316=CARTESIAN_POINT('Ctrl Pts',(5.25779635164618,-35.3742402223328,-2.22278760948228));
#53317=CARTESIAN_POINT('Ctrl Pts',(4.78073424536,-32.4742356128,-0.651925339842));
#53318=CARTESIAN_POINT('Ctrl Pts',(6.13376882180498,-35.3742402223328,-1.39617398295829));
#53319=CARTESIAN_POINT('Ctrl Pts',(5.66596200411,-32.4742356128,0.560784091783));
#53320=CARTESIAN_POINT('Ctrl Pts',(6.70708269922301,-35.3742402223328,-0.336673954678897));
#53321=CARTESIAN_POINT('Ctrl Pts',(6.46037298138,-32.4742356128,1.83459706183));
#53322=CARTESIAN_POINT('Ctrl Pts',(6.9022352637703,-35.3742402223328,0.234415037002724));
#53323=CARTESIAN_POINT('Ctrl Pts',(6.83383584614,-32.4742356128,2.48513748583));
#53324=CARTESIAN_POINT('Ctrl Pts',(7.02153268112224,-35.3742402223328,0.820426030514367));
#53325=CARTESIAN_POINT('Ctrl Pts',(7.18368375786,-32.4742356128,3.149547989));
#53326=CARTESIAN_POINT('Ctrl Pts',(7.07911924991741,-35.3742402223328,1.41232957780478));
#53327=CARTESIAN_POINT('Ctrl Pts',(7.50890612221,-32.4742356128,3.82595376918));
#53328=CARTESIAN_POINT('',(3.68960640636,-35.2436867043,-3.0159715009));
#53329=CARTESIAN_POINT('Ctrl Pts',(7.05021190275,-35.3742261151,1.16209541223));
#53330=CARTESIAN_POINT('Ctrl Pts',(7.04171869097663,-35.3624916648819,1.09881053133014));
#53331=CARTESIAN_POINT('Ctrl Pts',(7.03181610669979,-35.3514001191425,1.03686583093715));
#53332=CARTESIAN_POINT('Ctrl Pts',(7.0207453922348,-35.3409464539044,0.976289133858449));
#53333=CARTESIAN_POINT('Ctrl Pts',(7.01066574355577,-35.3314286153456,0.921135347115895));
#53334=CARTESIAN_POINT('Ctrl Pts',(6.99961668359083,-35.3224388134776,0.867117344000881));
#53335=CARTESIAN_POINT('Ctrl Pts',(6.98777529211479,-35.313982662876,0.814283056917023));
#53336=CARTESIAN_POINT('Ctrl Pts',(6.97535175743496,-35.3051107933437,0.758851345264047));
#53337=CARTESIAN_POINT('Ctrl Pts',(6.96205390136742,-35.296823127841,0.704712867921782));
#53338=CARTESIAN_POINT('Ctrl Pts',(6.94807400250197,-35.2891198857226,0.651894013352573));
#53339=CARTESIAN_POINT('Ctrl Pts',(6.94099303581381,-35.2852181120863,0.625140704669078));
#53340=CARTESIAN_POINT('Ctrl Pts',(6.9338550959053,-35.2815270633348,0.599156040997984));
#53341=CARTESIAN_POINT('Ctrl Pts',(6.92651065807691,-35.2779519219061,0.573287683597755));
#53342=CARTESIAN_POINT('Ctrl Pts',(6.91935502796454,-35.2744686887082,0.548084339040236));
#53343=CARTESIAN_POINT('Ctrl Pts',(6.91200294794405,-35.2710955431516,0.522991274887046));
#53344=CARTESIAN_POINT('Ctrl Pts',(6.90427337831988,-35.2677637793526,0.497412802476387));
#53345=CARTESIAN_POINT('Ctrl Pts',(6.88496491533278,-35.2594410342163,0.433517784794682));
#53346=CARTESIAN_POINT('Ctrl Pts',(6.86393740024656,-35.2516146076784,0.368816956298559));
#53347=CARTESIAN_POINT('Ctrl Pts',(6.84113206475727,-35.2442990466695,0.30341006480746));
#53348=CARTESIAN_POINT('Ctrl Pts',(6.8269378687566,-35.2397457917145,0.262700370444246));
#53349=CARTESIAN_POINT('Ctrl Pts',(6.81205496222768,-35.2353893754627,0.221717668954711));
#53350=CARTESIAN_POINT('Ctrl Pts',(6.79646754329069,-35.2312242157789,0.180490035754024));
#53351=CARTESIAN_POINT('Ctrl Pts',(6.77615194395067,-35.2257956252171,0.126756695986382));
#53352=CARTESIAN_POINT('Ctrl Pts',(6.75464085353844,-35.2206974783671,0.0726059083119251));
#53353=CARTESIAN_POINT('Ctrl Pts',(6.73190164180915,-35.215929423835,0.018102116016296));
#53354=CARTESIAN_POINT('Ctrl Pts',(6.72053203594451,-35.213545396569,-0.00914978013151847));
#53355=CARTESIAN_POINT('Ctrl Pts',(6.70885536061968,-35.2112439023798,-0.0364899155650709));
#53356=CARTESIAN_POINT('Ctrl Pts',(6.69686742451631,-35.2090249653309,-0.0639095636244658));
#53357=CARTESIAN_POINT('Ctrl Pts',(6.69087345646463,-35.2079154968065,-0.0776193876541635));
#53358=CARTESIAN_POINT('Ctrl Pts',(6.68480166933077,-35.2068266690482,-0.0913490882232204));
#53359=CARTESIAN_POINT('Ctrl Pts',(6.67865151973405,-35.2057584963529,-0.105097545261577));
#53360=CARTESIAN_POINT('Ctrl Pts',(6.67557644493569,-35.2052244100052,-0.111971773780756));
#53361=CARTESIAN_POINT('Ctrl Pts',(6.67248177922061,-35.2046954875616,-0.118850691268574));
#53362=CARTESIAN_POINT('Ctrl Pts',(6.66936745357457,-35.2041717316032,-0.125734154730951));
#53363=CARTESIAN_POINT('Ctrl Pts',(6.66656635998883,-35.2037006538733,-0.131925294497191));
#53364=CARTESIAN_POINT('Ctrl Pts',(6.66323174472111,-35.2031491115,-0.139253712594071));
#53365=CARTESIAN_POINT('Ctrl Pts',(6.66076014103221,-35.2027456430887,-0.144660488535147));
#53366=CARTESIAN_POINT('Ctrl Pts',(6.66048375415258,-35.2027005252668,-0.145265100810923));
#53367=CARTESIAN_POINT('Ctrl Pts',(6.66021820472302,-35.202657240603,-0.145845705952771));
#53368=CARTESIAN_POINT('Ctrl Pts',(6.65996547595427,-35.2026160964162,-0.146398041643693));
#53369=CARTESIAN_POINT('Ctrl Pts',(6.65530185568993,-35.201856860086,-0.156590327760148));
#53370=CARTESIAN_POINT('Ctrl Pts',(6.65058095734713,-35.201106489467,-0.166823005033949));
#53371=CARTESIAN_POINT('Ctrl Pts',(6.64580190445704,-35.2003651216435,-0.177095363302161));
#53372=CARTESIAN_POINT('Ctrl Pts',(6.61069329351012,-35.1949187716898,-0.252559736314997));
#53373=CARTESIAN_POINT('Ctrl Pts',(6.57244820855811,-35.1899609730455,-0.330168424696878));
#53374=CARTESIAN_POINT('Ctrl Pts',(6.53073543904713,-35.1855053802243,-0.409584960026447));
#53375=CARTESIAN_POINT('Ctrl Pts',(6.48776104603538,-35.1809150257778,-0.491403488043048));
#53376=CARTESIAN_POINT('Ctrl Pts',(6.44110689190624,-35.1768571692308,-0.57514009064432));
#53377=CARTESIAN_POINT('Ctrl Pts',(6.39037514193269,-35.1733163496887,-0.660398503439087));
#53378=CARTESIAN_POINT('Ctrl Pts',(6.38148185565513,-35.1726956432897,-0.67534432086013));
#53379=CARTESIAN_POINT('Ctrl Pts',(6.37246316017652,-35.1720907665111,-0.690336853378118));
#53380=CARTESIAN_POINT('Ctrl Pts',(6.36331677581195,-35.1715015691976,-0.705373909880942));
#53381=CARTESIAN_POINT('Ctrl Pts',(6.30388704247073,-35.1676731887326,-0.803078994489163));
#53382=CARTESIAN_POINT('Ctrl Pts',(6.23908435969954,-35.1645227437922,-0.902647167291049));
#53383=CARTESIAN_POINT('Ctrl Pts',(6.16840308024187,-35.1620509040348,-1.00331561529873));
#53384=CARTESIAN_POINT('Ctrl Pts',(6.13306244051303,-35.160814984156,-1.05364983930258));
#53385=CARTESIAN_POINT('Ctrl Pts',(6.09625340225616,-35.1597487257998,-1.10425697375371));
#53386=CARTESIAN_POINT('Ctrl Pts',(6.05792492906513,-35.1588540447982,-1.15502954954102));
#53387=CARTESIAN_POINT('Ctrl Pts',(6.03876069246962,-35.1584067042974,-1.18041583743468));
#53388=CARTESIAN_POINT('Ctrl Pts',(6.01921696940969,-35.1580026386106,-1.20584339585966));
#53389=CARTESIAN_POINT('Ctrl Pts',(5.99928741736408,-35.1576402865646,-1.23129781727104));
#53390=CARTESIAN_POINT('Ctrl Pts',(5.9930558832247,-35.1575269870213,-1.2392568569755));
#53391=CARTESIAN_POINT('Ctrl Pts',(5.98678662972843,-35.1574177663938,-1.24721852373888));
#53392=CARTESIAN_POINT('Ctrl Pts',(5.98047948632145,-35.1573126270196,-1.25518239795847));
#53393=CARTESIAN_POINT('Ctrl Pts',(5.97709234955469,-35.1572561638291,-1.25945925190557));
#53394=CARTESIAN_POINT('Ctrl Pts',(5.97369428525231,-35.1572008777147,-1.26373674254876));
#53395=CARTESIAN_POINT('Ctrl Pts',(5.97028526725492,-35.1571467692569,-1.26801480530466));
#53396=CARTESIAN_POINT('Ctrl Pts',(5.9693721506115,-35.1571322761291,-1.26916069843488));
#53397=CARTESIAN_POINT('Ctrl Pts',(5.96845945509689,-35.1571178857888,-1.2703051263329));
#53398=CARTESIAN_POINT('Ctrl Pts',(5.96753501358586,-35.1571034095411,-1.27146331299833));
#53399=CARTESIAN_POINT('Ctrl Pts',(5.96178354348352,-35.15701334467,-1.27866904305232));
#53400=CARTESIAN_POINT('Ctrl Pts',(5.95569562279192,-35.156922109887,-1.28625626414113));
#53401=CARTESIAN_POINT('Ctrl Pts',(5.94987658651169,-35.1568387908094,-1.29347002265334));
#53402=CARTESIAN_POINT('Ctrl Pts',(5.94714891325534,-35.1567997349917,-1.29685147195594));
#53403=CARTESIAN_POINT('Ctrl Pts',(5.94448055637157,-35.1567623743348,-1.30015103597856));
#53404=CARTESIAN_POINT('Ctrl Pts',(5.94193503261732,-35.1567274276868,-1.30329182385335));
#53405=CARTESIAN_POINT('Ctrl Pts',(5.94114899344845,-35.1567166364169,-1.30426167624093));
#53406=CARTESIAN_POINT('Ctrl Pts',(5.94037467162046,-35.1567060744422,-1.30521639244965));
#53407=CARTESIAN_POINT('Ctrl Pts',(5.93961394956819,-35.1566957606942,-1.30615371755976));
#53408=CARTESIAN_POINT('Ctrl Pts',(5.93911292116412,-35.1566889678311,-1.30677106065191));
#53409=CARTESIAN_POINT('Ctrl Pts',(5.93861924218642,-35.1566823021108,-1.30737907499651));
#53410=CARTESIAN_POINT('Ctrl Pts',(5.93812871462457,-35.156675705061,-1.30798294841254));
#53411=CARTESIAN_POINT('Ctrl Pts',(5.87593085307289,-35.1558392130501,-1.38455282551269));
#53412=CARTESIAN_POINT('Ctrl Pts',(5.8117184053166,-35.1553981914991,-1.45937109845001));
#53413=CARTESIAN_POINT('Ctrl Pts',(5.74566148136113,-35.1553170792143,-1.53233725834745));
#53414=CARTESIAN_POINT('Ctrl Pts',(5.73362228837958,-35.1553022961092,-1.54563569290247));
#53415=CARTESIAN_POINT('Ctrl Pts',(5.72152191691934,-35.1552995512701,-1.55887267409941));
#53416=CARTESIAN_POINT('Ctrl Pts',(5.70936152340078,-35.1553087395002,-1.57204767529075));
#53417=CARTESIAN_POINT('Ctrl Pts',(5.64244874495201,-35.1553592978972,-1.64454335024017));
#53418=CARTESIAN_POINT('Ctrl Pts',(5.57371424926814,-35.1557687251983,-1.71516187978632));
#53419=CARTESIAN_POINT('Ctrl Pts',(5.50335441612892,-35.1565210085082,-1.78383223993651));
#53420=CARTESIAN_POINT('Ctrl Pts',(5.42259868323553,-35.1573844441835,-1.86264887457815));
#53421=CARTESIAN_POINT('Ctrl Pts',(5.33970816688366,-35.1586996156632,-1.9388943604782));
#53422=CARTESIAN_POINT('Ctrl Pts',(5.25498407598778,-35.1604819759236,-2.01253312819369));
#53423=CARTESIAN_POINT('Ctrl Pts',(5.23950411866333,-35.1608076313597,-2.02598768367616));
#53424=CARTESIAN_POINT('Ctrl Pts',(5.22396310231098,-35.1611489673329,-2.03935522430689));
#53425=CARTESIAN_POINT('Ctrl Pts',(5.20836307072808,-35.1615061778703,-2.05263552943471));
#53426=CARTESIAN_POINT('Ctrl Pts',(5.16450464390509,-35.1625104509792,-2.08997220324466));
#53427=CARTESIAN_POINT('Ctrl Pts',(5.1201784455238,-35.1636401475021,-2.12662037226471));
#53428=CARTESIAN_POINT('Ctrl Pts',(5.07542573898653,-35.1649015036721,-2.16258044277949));
#53429=CARTESIAN_POINT('Ctrl Pts',(5.0530493857179,-35.165532181757,-2.18056047803688));
#53430=CARTESIAN_POINT('Ctrl Pts',(5.03056805256408,-35.1662020708006,-2.19837117024708));
#53431=CARTESIAN_POINT('Ctrl Pts',(5.00798440517391,-35.1669035211473,-2.21600920760725));
#53432=CARTESIAN_POINT('Ctrl Pts',(4.99669258147882,-35.1672542463207,-2.22482822628733));
#53433=CARTESIAN_POINT('Ctrl Pts',(4.9853751902225,-35.1676128672095,-2.23360408292936));
#53434=CARTESIAN_POINT('Ctrl Pts',(4.97403283155191,-35.1679793842306,-2.24233677376295));
#53435=CARTESIAN_POINT('Ctrl Pts',(4.96545811282785,-35.168256467724,-2.24893860762987));
#53436=CARTESIAN_POINT('Ctrl Pts',(4.95768844276382,-35.1685110573609,-2.25489001680632));
#53437=CARTESIAN_POINT('Ctrl Pts',(4.94886665918735,-35.1688042254875,-2.26161082038719));
#53438=CARTESIAN_POINT('Ctrl Pts',(4.94601927475276,-35.168898850611,-2.26378007690297));
#53439=CARTESIAN_POINT('Ctrl Pts',(4.94306199125833,-35.1689975616605,-2.26602925228609));
#53440=CARTESIAN_POINT('Ctrl Pts',(4.93993145158124,-35.1691026237342,-2.26840534922387));
#53441=CARTESIAN_POINT('Ctrl Pts',(4.84275788847932,-35.1723638045837,-2.34216062132897));
#53442=CARTESIAN_POINT('Ctrl Pts',(4.74472048608218,-35.1762164066117,-2.4121183656713));
#53443=CARTESIAN_POINT('Ctrl Pts',(4.64620631975456,-35.1806916453217,-2.47851432158574));
#53444=CARTESIAN_POINT('Ctrl Pts',(4.54898668486911,-35.1851080768831,-2.54403779737098));
#53445=CARTESIAN_POINT('Ctrl Pts',(4.45130321877941,-35.1901317337284,-2.60609180771767));
#53446=CARTESIAN_POINT('Ctrl Pts',(4.35349606022021,-35.1957786691155,-2.66486634866325));
#53447=CARTESIAN_POINT('Ctrl Pts',(4.25606761878344,-35.2014037391182,-2.72341330989639));
#53448=CARTESIAN_POINT('Ctrl Pts',(4.15851669162129,-35.2076476179274,-2.77870563852987));
#53449=CARTESIAN_POINT('Ctrl Pts',(4.06114220912171,-35.2145035862827,-2.83090328273477));
#53450=CARTESIAN_POINT('Ctrl Pts',(3.96303037677852,-35.2214114701611,-2.88349618372362));
#53451=CARTESIAN_POINT('Ctrl Pts',(3.86509781141783,-35.2289408247001,-2.93294695745577));
#53452=CARTESIAN_POINT('Ctrl Pts',(3.76760937528583,-35.2370586591497,-2.97939765302607));
#53453=CARTESIAN_POINT('Ctrl Pts',(3.74157542818244,-35.2392264985473,-2.99180214938864));
#53454=CARTESIAN_POINT('Ctrl Pts',(3.71557292416585,-35.2414361600975,-3.00399259842331));
#53455=CARTESIAN_POINT('Ctrl Pts',(3.68960640636835,-35.2436867042943,-3.01597150091916));
#53456=CARTESIAN_POINT('',(3.66207294829051,-35.2473021020985,-3.02895254909592));
#53457=CARTESIAN_POINT('Origin',(3.70338411396943,-35.4162358614354,-3.04861059388952));
#53458=CARTESIAN_POINT('',(3.32386409198,-32.4742356128,-2.36922853848));
#53459=CARTESIAN_POINT('',(3.66207294829,-35.2473021021,-3.02895254909));
#53460=CARTESIAN_POINT('Ctrl Pts',(7.50890612221,-32.4742356128,3.82595376918));
#53461=CARTESIAN_POINT('Ctrl Pts',(6.96684511245223,-32.4742356128,2.69856143580474));
#53462=CARTESIAN_POINT('Ctrl Pts',(6.3432119791806,-32.4742356128,1.61223864180823));
#53463=CARTESIAN_POINT('Ctrl Pts',(4.94263675758286,-32.4742356128,-0.46110591833064));
#53464=CARTESIAN_POINT('Ctrl Pts',(4.16753771932367,-32.4742356128,-1.44534807371885));
#53465=CARTESIAN_POINT('Ctrl Pts',(3.32386409198,-32.4742356128,-2.36922853848));
#53466=CARTESIAN_POINT('Ctrl Pts',(7.05021190275,-35.3742261151,1.16209541223));
#53467=CARTESIAN_POINT('Ctrl Pts',(7.05021190275,-35.3742261151,1.16209541223));
#53468=CARTESIAN_POINT('Ctrl Pts',(7.05021190275,-35.3742261151,1.16209541223));
#53469=CARTESIAN_POINT('Ctrl Pts',(7.05021190275,-35.3742261151,1.16209541223));
#53470=CARTESIAN_POINT('Ctrl Pts',(7.05021190275,-35.3742261151,1.16209541223));
#53471=CARTESIAN_POINT('Ctrl Pts',(7.05021190275,-35.3742261151,1.16209541223));
#53472=CARTESIAN_POINT('Ctrl Pts',(7.01340171355,-35.3233663073,0.887814197822));
#53473=CARTESIAN_POINT('Ctrl Pts',(7.01381986471783,-35.3413180972,0.890929938671949));
#53474=CARTESIAN_POINT('Ctrl Pts',(7.01423801594781,-35.3592698878,0.894045679984952));
#53475=CARTESIAN_POINT('Ctrl Pts',(7.01465616709811,-35.377221677,0.897161420704254));
#53476=CARTESIAN_POINT('Ctrl Pts',(7.01507431822199,-35.3951734669,0.900277161226733));
#53477=CARTESIAN_POINT('Ctrl Pts',(7.01549246939,-35.4131252568,0.903392902078));
#53478=CARTESIAN_POINT('Ctrl Pts',(6.95185482919,-35.2775995372,0.614848488511));
#53479=CARTESIAN_POINT('Ctrl Pts',(6.95711039026,-35.3122184667,0.620033495106));
#53480=CARTESIAN_POINT('Ctrl Pts',(6.96131634916,-35.3468297586,0.625353240693));
#53481=CARTESIAN_POINT('Ctrl Pts',(6.96447793891,-35.3814361808,0.630808421027));
#53482=CARTESIAN_POINT('Ctrl Pts',(6.96659784091,-35.4160401708,0.636399696014));
#53483=CARTESIAN_POINT('Ctrl Pts',(6.96767646618,-35.4506441608,0.642127552041));
#53484=CARTESIAN_POINT('Ctrl Pts',(6.8673530143,-35.2439788226,0.343363482131));
#53485=CARTESIAN_POINT('Ctrl Pts',(6.87994051011,-35.2916209137,0.34796525773));
#53486=CARTESIAN_POINT('Ctrl Pts',(6.88986767191,-35.3397700495,0.353240035009));
#53487=CARTESIAN_POINT('Ctrl Pts',(6.89711069428,-35.38825575,0.359155938781));
#53488=CARTESIAN_POINT('Ctrl Pts',(6.90165550114,-35.4369097195,0.365681814414));
#53489=CARTESIAN_POINT('Ctrl Pts',(6.90349674466,-35.485563689,0.372787607728));
#53490=CARTESIAN_POINT('Ctrl Pts',(6.64187024435,-35.1886753155,-0.23870995558));
#53491=CARTESIAN_POINT('Ctrl Pts',(6.66955139679,-35.2585364198,-0.239842936739));
#53492=CARTESIAN_POINT('Ctrl Pts',(6.691390474,-35.3305802147,-0.238616506959));
#53493=CARTESIAN_POINT('Ctrl Pts',(6.70712809876,-35.4041022846,-0.23504887133));
#53494=CARTESIAN_POINT('Ctrl Pts',(6.71661554426,-35.4783635248,-0.229196354076));
#53495=CARTESIAN_POINT('Ctrl Pts',(6.71982081074,-35.5526247648,-0.221149174844));
#53496=CARTESIAN_POINT('Ctrl Pts',(6.335633879,-35.1655247078,-0.779903703387));
#53497=CARTESIAN_POINT('Ctrl Pts',(6.37258533768,-35.2460676029,-0.793096558606));
#53498=CARTESIAN_POINT('Ctrl Pts',(6.40175618506,-35.3308011559,-0.801727405553));
#53499=CARTESIAN_POINT('Ctrl Pts',(6.42255691503,-35.4184152395,-0.805611032625));
#53500=CARTESIAN_POINT('Ctrl Pts',(6.43465051901,-35.5074700242,-0.804704006103));
#53501=CARTESIAN_POINT('Ctrl Pts',(6.43798249823,-35.5965248091,-0.799107100072));
#53502=CARTESIAN_POINT('Ctrl Pts',(6.1477485618,-35.1585065417,-1.0593892471));
#53503=CARTESIAN_POINT('Ctrl Pts',(6.1862455007,-35.2425122041,-1.07972455995));
#53504=CARTESIAN_POINT('Ctrl Pts',(6.21657209688,-35.331564736,-1.09437680653));
#53505=CARTESIAN_POINT('Ctrl Pts',(6.23800931387,-35.4241081414,-1.10297704478));
#53506=CARTESIAN_POINT('Ctrl Pts',(6.25014939755,-35.5183977765,-1.10536973107));
#53507=CARTESIAN_POINT('Ctrl Pts',(6.25293978467,-35.6126874115,-1.1016283265));
#53508=CARTESIAN_POINT('Ctrl Pts',(5.64263928747,-35.1503549657,-1.69778761613));
#53509=CARTESIAN_POINT('Ctrl Pts',(5.6781072677,-35.2388302664,-1.73263418024));
#53510=CARTESIAN_POINT('Ctrl Pts',(5.70553308479,-35.3334375132,-1.75965360778));
#53511=CARTESIAN_POINT('Ctrl Pts',(5.72416357539,-35.4323082835,-1.77811755991));
#53512=CARTESIAN_POINT('Ctrl Pts',(5.7335949111,-35.5333121034,-1.78763419493));
#53513=CARTESIAN_POINT('Ctrl Pts',(5.73382235555,-35.6343159234,-1.78819570677));
#53514=CARTESIAN_POINT('Ctrl Pts',(5.01710815157,-35.1629277461,-2.24626629333));
#53515=CARTESIAN_POINT('Ctrl Pts',(5.03812134505,-35.2465940911,-2.28433468893));
#53516=CARTESIAN_POINT('Ctrl Pts',(5.05330548672,-35.3352292266,-2.31441076458));
#53517=CARTESIAN_POINT('Ctrl Pts',(5.06229638123,-35.4272996663,-2.33577662822));
#53518=CARTESIAN_POINT('Ctrl Pts',(5.06494250992,-35.5210885082,-2.34802021045));
#53519=CARTESIAN_POINT('Ctrl Pts',(5.06131871348,-35.6148773502,-2.35107992573));
#53520=CARTESIAN_POINT('Ctrl Pts',(4.60859161999,-35.1762367254,-2.53785301358));
#53521=CARTESIAN_POINT('Ctrl Pts',(4.61998718798,-35.2544472454,-2.57156731299));
#53522=CARTESIAN_POINT('Ctrl Pts',(4.62723219199,-35.3360986017,-2.59812098394));
#53523=CARTESIAN_POINT('Ctrl Pts',(4.63022512886,-35.4200944121,-2.61708014375));
#53524=CARTESIAN_POINT('Ctrl Pts',(4.62896118843,-35.5052625726,-2.62819842135));
#53525=CARTESIAN_POINT('Ctrl Pts',(4.62352979415,-35.5904307331,-2.63143094545));
#53526=CARTESIAN_POINT('Ctrl Pts',(4.16372827527,-35.2025940852,-2.79724907986));
#53527=CARTESIAN_POINT('Ctrl Pts',(4.16779886982,-35.2702188379,-2.82151459563));
#53528=CARTESIAN_POINT('Ctrl Pts',(4.16935260067,-35.3397404397,-2.84063625327));
#53529=CARTESIAN_POINT('Ctrl Pts',(4.16836377754,-35.4105469366,-2.8544077757));
#53530=CARTESIAN_POINT('Ctrl Pts',(4.16484831327,-35.4819959329,-2.86271080605));
#53531=CARTESIAN_POINT('Ctrl Pts',(4.15886281142,-35.5534449291,-2.86552034537));
#53532=CARTESIAN_POINT('Ctrl Pts',(3.68960640598,-35.2436867043,-3.01597150109));
#53533=CARTESIAN_POINT('Ctrl Pts',(3.68994006034,-35.2950048916,-3.03107790462));
#53534=CARTESIAN_POINT('Ctrl Pts',(3.68889543294,-35.347263528,-3.04301993645));
#53535=CARTESIAN_POINT('Ctrl Pts',(3.68647051499,-35.4001566504,-3.05170748242));
#53536=CARTESIAN_POINT('Ctrl Pts',(3.68267984997,-35.4533670311,-3.0570884388));
#53537=CARTESIAN_POINT('Ctrl Pts',(3.67755401867,-35.5065774118,-3.05915055738));
#53538=CARTESIAN_POINT('Origin',(3.30432478182257,-35.5065775309065,-2.13141045451377));
#53539=CARTESIAN_POINT('Ctrl Pts',(3.50597880735,-35.2696545374,-3.18321831335));
#53540=CARTESIAN_POINT('Ctrl Pts',(3.51333803189,-35.3113514663,-3.18868569298));
#53541=CARTESIAN_POINT('Ctrl Pts',(3.51870881162,-35.353530752,-3.19315085121));
#53542=CARTESIAN_POINT('Ctrl Pts',(3.52206318971,-35.3960340603,-3.19659302084));
#53543=CARTESIAN_POINT('Ctrl Pts',(3.52338838043,-35.4386993829,-3.1989990815));
#53544=CARTESIAN_POINT('Ctrl Pts',(3.52268705855,-35.4813647056,-3.20036385665));
#53545=CARTESIAN_POINT('Ctrl Pts',(3.50256004198,-35.268393509,-3.18939410052));
#53546=CARTESIAN_POINT('Ctrl Pts',(3.51052316476,-35.3102955518,-3.1938621313));
#53547=CARTESIAN_POINT('Ctrl Pts',(3.51648359784,-35.3526863763,-3.19731644996));
#53548=CARTESIAN_POINT('Ctrl Pts',(3.52041085984,-35.3954055593,-3.19973991273));
#53549=CARTESIAN_POINT('Ctrl Pts',(3.52228987577,-35.4382889251,-3.2011231722));
#53550=CARTESIAN_POINT('Ctrl Pts',(3.52212131885,-35.4811722908,-3.20146489487));
#53551=CARTESIAN_POINT('Ctrl Pts',(3.49913203155,-35.2673150056,-3.1956382498));
#53552=CARTESIAN_POINT('Ctrl Pts',(3.50770826391,-35.3094204104,-3.19910017162));
#53553=CARTESIAN_POINT('Ctrl Pts',(3.51426388564,-35.3520219724,-3.20153494382));
#53554=CARTESIAN_POINT('Ctrl Pts',(3.5187657727,-35.3949568785,-3.20292908338));
#53555=CARTESIAN_POINT('Ctrl Pts',(3.52119645205,-35.4380584515,-3.20327716833));
#53556=CARTESIAN_POINT('Ctrl Pts',(3.52155459752,-35.4811600245,-3.20258180379));
#53557=CARTESIAN_POINT('Ctrl Pts',(3.49570498282,-35.2664275319,-3.20193555292));
#53558=CARTESIAN_POINT('Ctrl Pts',(3.5049017062,-35.3087336513,-3.20438752525));
#53559=CARTESIAN_POINT('Ctrl Pts',(3.51205619329,-35.3515442739,-3.2057969486));
#53560=CARTESIAN_POINT('Ctrl Pts',(3.51713243885,-35.3946938503,-3.20615423225));
#53561=CARTESIAN_POINT('Ctrl Pts',(3.52011064813,-35.4380129429,-3.20545771792));
#53562=CARTESIAN_POINT('Ctrl Pts',(3.52098739307,-35.4813320354,-3.20371424309));
#53563=CARTESIAN_POINT('Ctrl Pts',(3.49229725928,-35.2657414976,-3.2082566117));
#53564=CARTESIAN_POINT('Ctrl Pts',(3.50211831443,-35.308244275,-3.20970015733));
#53565=CARTESIAN_POINT('Ctrl Pts',(3.50987186481,-35.3512608603,-3.21008384904));
#53566=CARTESIAN_POINT('Ctrl Pts',(3.51551898686,-35.3946227115,-3.20940189333));
#53567=CARTESIAN_POINT('Ctrl Pts',(3.51903723035,-35.4381571989,-3.20765694424));
#53568=CARTESIAN_POINT('Ctrl Pts',(3.52042115146,-35.4816916863,-3.20486003554));
#53569=CARTESIAN_POINT('Ctrl Pts',(3.4889030666,-35.265254082,-3.21461371656));
#53570=CARTESIAN_POINT('Ctrl Pts',(3.49935367791,-35.3079501561,-3.21504791216));
#53571=CARTESIAN_POINT('Ctrl Pts',(3.50770783634,-35.3511703481,-3.21440295273));
#53572=CARTESIAN_POINT('Ctrl Pts',(3.51392345649,-35.3947427765,-3.21267708331));
#53573=CARTESIAN_POINT('Ctrl Pts',(3.51797541562,-35.4384913269,-3.20987727967));
#53574=CARTESIAN_POINT('Ctrl Pts',(3.51985615629,-35.4822398773,-3.20601908088));
#53575=CARTESIAN_POINT('',(3.50597898435511,-35.2696545360883,-3.18321830583732));
#53576=CARTESIAN_POINT('Origin',(3.5116682051481,-35.3848727889406,-3.20631688515481));
#53577=CARTESIAN_POINT('Origin',(2.63323785737633,-35.4813643327716,-2.74332899791331));
#53578=CARTESIAN_POINT('Ctrl Pts',(3.66378622939474,-35.2464640243768,-3.0279781015246));
#53579=CARTESIAN_POINT('Ctrl Pts',(3.66837475167183,-35.2970123124896,-3.04073454824404));
#53580=CARTESIAN_POINT('Ctrl Pts',(3.67167460756035,-35.3484462252211,-3.0504452225707));
#53581=CARTESIAN_POINT('Ctrl Pts',(3.67365999774165,-35.4004772676907,-3.05703724741477));
#53582=CARTESIAN_POINT('Ctrl Pts',(3.67431938153269,-35.4528069345301,-3.06047287388992));
#53583=CARTESIAN_POINT('Ctrl Pts',(3.673656359803,-35.5051366012576,-3.06075050068259));
#53584=CARTESIAN_POINT('Ctrl Pts',(3.64685377738682,-35.2475881828974,-3.03546815079806));
#53585=CARTESIAN_POINT('Ctrl Pts',(3.65197996915299,-35.2977377775771,-3.04779720191966));
#53586=CARTESIAN_POINT('Ctrl Pts',(3.65566459258164,-35.3487504451489,-3.05720437609867));
#53587=CARTESIAN_POINT('Ctrl Pts',(3.65787487045666,-35.4003455971741,-3.06362096615626));
#53588=CARTESIAN_POINT('Ctrl Pts',(3.65859977260828,-35.4522315476326,-3.06701003015053));
#53589=CARTESIAN_POINT('Ctrl Pts',(3.65784552585749,-35.5041174980908,-3.06737014843955));
#53590=CARTESIAN_POINT('Ctrl Pts',(3.63069497520593,-35.2488274318634,-3.04411012182609));
#53591=CARTESIAN_POINT('Ctrl Pts',(3.63621005013032,-35.2985088014843,-3.05599604307844));
#53592=CARTESIAN_POINT('Ctrl Pts',(3.6401348662033,-35.3490281789965,-3.06510435036028));
#53593=CARTESIAN_POINT('Ctrl Pts',(3.64244429896267,-35.4001115250326,-3.0713693085073));
#53594=CARTESIAN_POINT('Ctrl Pts',(3.6431236689932,-35.451477515452,-3.07475727773419));
#53595=CARTESIAN_POINT('Ctrl Pts',(3.64217553898255,-35.5028435058782,-3.07526460898209));
#53596=CARTESIAN_POINT('Ctrl Pts',(3.6149475468118,-35.2501319216701,-3.05405854836525));
#53597=CARTESIAN_POINT('Ctrl Pts',(3.62087332233153,-35.2992445854584,-3.06542135460391));
#53598=CARTESIAN_POINT('Ctrl Pts',(3.6250932299558,-35.3491642058263,-3.07416948701838));
#53599=CARTESIAN_POINT('Ctrl Pts',(3.62757315136577,-35.3996287881775,-3.08023942083983));
#53600=CARTESIAN_POINT('Ctrl Pts',(3.62829959911055,-35.4503649729954,-3.08359895575808));
#53601=CARTESIAN_POINT('Ctrl Pts',(3.62728035817098,-35.5011011577074,-3.0842466362974));
#53602=CARTESIAN_POINT('Ctrl Pts',(3.57804594423897,-35.2537396575121,-3.08151411792311));
#53603=CARTESIAN_POINT('Ctrl Pts',(3.58490210551495,-35.3013209015024,-3.09141036639288));
#53604=CARTESIAN_POINT('Ctrl Pts',(3.58981192437177,-35.3496314438259,-3.09910496604094));
#53605=CARTESIAN_POINT('Ctrl Pts',(3.59274404424921,-35.3984313240945,-3.10455252216444));
#53606=CARTESIAN_POINT('Ctrl Pts',(3.59368370155741,-35.4474771670055,-3.10772506981888));
#53607=CARTESIAN_POINT('Ctrl Pts',(3.59263285291033,-35.4965230101221,-3.10861522294742));
#53608=CARTESIAN_POINT('Ctrl Pts',(3.54614995886284,-35.2585698054349,-3.11565459351817));
#53609=CARTESIAN_POINT('Ctrl Pts',(3.55365282508503,-35.3042784980418,-3.1238029213662));
#53610=CARTESIAN_POINT('Ctrl Pts',(3.55910677430424,-35.3506275899982,-3.13019982938299));
#53611=CARTESIAN_POINT('Ctrl Pts',(3.56247248748482,-35.3974100369749,-3.13480265896626));
#53612=CARTESIAN_POINT('Ctrl Pts',(3.56373415608727,-35.4444073086632,-3.13759135387308));
#53613=CARTESIAN_POINT('Ctrl Pts',(3.56290037565488,-35.4914045803479,-3.1385656230307));
#53614=CARTESIAN_POINT('Ctrl Pts',(3.5297693370109,-35.262096319147,-3.13775667457677));
#53615=CARTESIAN_POINT('Ctrl Pts',(3.53742200429963,-35.3066260775261,-3.14485178755018));
#53616=CARTESIAN_POINT('Ctrl Pts',(3.54299253665026,-35.3517487998208,-3.15044517412045));
#53617=CARTESIAN_POINT('Ctrl Pts',(3.54645603898634,-35.3972616314089,-3.15453043124095));
#53618=CARTESIAN_POINT('Ctrl Pts',(3.54780199054788,-35.4429759293891,-3.15708363433905));
#53619=CARTESIAN_POINT('Ctrl Pts',(3.54701944502996,-35.4886902276847,-3.15808466613649));
#53620=CARTESIAN_POINT('Ctrl Pts',(3.51627715008437,-35.265772097736,-3.16057033053923));
#53621=CARTESIAN_POINT('Ctrl Pts',(3.52379883042827,-35.3089013381962,-3.16688771508641));
#53622=CARTESIAN_POINT('Ctrl Pts',(3.52927202428577,-35.3525623688612,-3.17198724899732));
#53623=CARTESIAN_POINT('Ctrl Pts',(3.53266012631829,-35.3965870683247,-3.17582587319325));
#53624=CARTESIAN_POINT('Ctrl Pts',(3.53394593132937,-35.4407889521592,-3.17839253457853));
#53625=CARTESIAN_POINT('Ctrl Pts',(3.53314312461956,-35.4849908356552,-3.17969330859528));
#53626=CARTESIAN_POINT('Ctrl Pts',(3.50505237127691,-35.269315766807,-3.18490659755473));
#53627=CARTESIAN_POINT('Ctrl Pts',(3.5124462254045,-35.3110230787235,-3.19033652396823));
#53628=CARTESIAN_POINT('Ctrl Pts',(3.51784430886608,-35.35321329042,-3.19477526792434));
#53629=CARTESIAN_POINT('Ctrl Pts',(3.52121894386514,-35.395727447307,-3.19820343835999));
#53630=CARTESIAN_POINT('Ctrl Pts',(3.52255749924592,-35.4384039093696,-3.20060764124573));
#53631=CARTESIAN_POINT('Ctrl Pts',(3.5218618906809,-35.4810803715647,-3.20198185530188));
#53632=CARTESIAN_POINT('Ctrl Pts',(3.66207294829203,-35.247302102094,-3.02895254911367));
#53633=CARTESIAN_POINT('Ctrl Pts',(3.65265573864293,-35.2479321008334,-3.03318696750315));
#53634=CARTESIAN_POINT('Ctrl Pts',(3.64324606816193,-35.2486494149569,-3.03798955551632));
#53635=CARTESIAN_POINT('Ctrl Pts',(3.63389358932175,-35.2494540499443,-3.04342239580713));
#53636=CARTESIAN_POINT('Ctrl Pts',(3.62444446054903,-35.2502670001515,-3.04891137989217));
#53637=CARTESIAN_POINT('Ctrl Pts',(3.61505379466542,-35.251169085322,-3.0550438523311));
#53638=CARTESIAN_POINT('Ctrl Pts',(3.60581140686814,-35.2521603111073,-3.06184608738143));
#53639=CARTESIAN_POINT('Ctrl Pts',(3.59604940078202,-35.2532072648125,-3.06903075236379));
#53640=CARTESIAN_POINT('Ctrl Pts',(3.58645323658232,-35.2543536640781,-3.07696257748029));
#53641=CARTESIAN_POINT('Ctrl Pts',(3.577168615446,-35.2555995155633,-3.08562884702655));
#53642=CARTESIAN_POINT('Ctrl Pts',(3.56445418506134,-35.2573055940071,-3.09749650206843));
#53643=CARTESIAN_POINT('Ctrl Pts',(3.55232717675937,-35.2591981729177,-3.11074138259069));
#53644=CARTESIAN_POINT('Ctrl Pts',(3.54121912889871,-35.2612772693964,-3.12523908272482));
#53645=CARTESIAN_POINT('Ctrl Pts',(3.53419394128748,-35.2625921757604,-3.13440802623778));
#53646=CARTESIAN_POINT('Ctrl Pts',(3.52757805820054,-35.2639816857809,-3.14407554672188));
#53647=CARTESIAN_POINT('Ctrl Pts',(3.52146452079015,-35.2654458037837,-3.1542111523752));
#53648=CARTESIAN_POINT('Ctrl Pts',(3.51586767175993,-35.2667861811912,-3.16349014273109));
#53649=CARTESIAN_POINT('Ctrl Pts',(3.51069302206195,-35.2681890884407,-3.17316034952375));
#53650=CARTESIAN_POINT('Ctrl Pts',(3.50597898250972,-35.2696545288516,-3.18321830602679));
#53651=CARTESIAN_POINT('Origin',(3.28043975923886,-35.505031377995,-2.14129772753315));
#53652=CARTESIAN_POINT('Ctrl Pts',(3.68960640636,-35.2436867043,-3.0159715009));
#53653=CARTESIAN_POINT('Ctrl Pts',(3.68994006064,-35.2950048915,-3.03107790447));
#53654=CARTESIAN_POINT('Ctrl Pts',(3.68889543318,-35.347263528,-3.04301993635));
#53655=CARTESIAN_POINT('Ctrl Pts',(3.68647051515,-35.4001566503,-3.05170748236));
#53656=CARTESIAN_POINT('Ctrl Pts',(3.68267985005,-35.4533670311,-3.05708843877));
#53657=CARTESIAN_POINT('Ctrl Pts',(3.67755401867,-35.5065774118,-3.05915055738));
#53658=CARTESIAN_POINT('Ctrl Pts',(3.68406493808,-35.2441669878,-3.01852789669));
#53659=CARTESIAN_POINT('Ctrl Pts',(3.6852545996,-35.2952993243,-3.03313678947));
#53660=CARTESIAN_POINT('Ctrl Pts',(3.68508444483,-35.3473574121,-3.04461628848));
#53661=CARTESIAN_POINT('Ctrl Pts',(3.68354738519,-35.4000399811,-3.05288030368));
#53662=CARTESIAN_POINT('Ctrl Pts',(3.68065246874,-35.4530348056,-3.05787988529));
#53663=CARTESIAN_POINT('Ctrl Pts',(3.67642456268,-35.5060296301,-3.05960493674));
#53664=CARTESIAN_POINT('Ctrl Pts',(3.67853556896,-35.2447691838,-3.02110736508));
#53665=CARTESIAN_POINT('Ctrl Pts',(3.68058228399,-35.295713802,-3.03522035827));
#53666=CARTESIAN_POINT('Ctrl Pts',(3.68128649848,-35.3475703565,-3.04623632347));
#53667=CARTESIAN_POINT('Ctrl Pts',(3.68063618362,-35.4000419929,-3.05407302366));
#53668=CARTESIAN_POINT('Ctrl Pts',(3.67863507204,-35.4528211843,-3.05868456544));
#53669=CARTESIAN_POINT('Ctrl Pts',(3.67530251301,-35.5056003757,-3.0600629924));
#53670=CARTESIAN_POINT('Ctrl Pts',(3.67302394084,-35.2454929622,-3.02370658462));
#53671=CARTESIAN_POINT('Ctrl Pts',(3.6759278736,-35.2962481955,-3.03732595805));
#53672=CARTESIAN_POINT('Ctrl Pts',(3.67750544789,-35.3479024371,-3.04787800394));
#53673=CARTESIAN_POINT('Ctrl Pts',(3.67773982365,-35.4001629685,-3.05528416988));
#53674=CARTESIAN_POINT('Ctrl Pts',(3.67662956704,-35.4527266586,-3.05950153137));
#53675=CARTESIAN_POINT('Ctrl Pts',(3.67418869929,-35.5052903486,-3.06052426199));
#53676=CARTESIAN_POINT('Ctrl Pts',(3.6675348968,-35.2463373792,-3.02632251085));
#53677=CARTESIAN_POINT('Ctrl Pts',(3.67129543056,-35.2969017565,-3.03945109726));
#53678=CARTESIAN_POINT('Ctrl Pts',(3.67374456646,-35.348353094,-3.04953936585));
#53679=CARTESIAN_POINT('Ctrl Pts',(3.67486076111,-35.4004025315,-3.05651229579));
#53680=CARTESIAN_POINT('Ctrl Pts',(3.67463755638,-35.4527510324,-3.06032984675));
#53681=CARTESIAN_POINT('Ctrl Pts',(3.67308380368,-35.5050995333,-3.0609883158));
#53682=CARTESIAN_POINT('Ctrl Pts',(3.66207264655,-35.2473009405,-3.02895231242));
#53683=CARTESIAN_POINT('Ctrl Pts',(3.66668846955,-35.2976731782,-3.04159341678));
#53684=CARTESIAN_POINT('Ctrl Pts',(3.67000667781,-35.348921195,-3.05121851933));
#53685=CARTESIAN_POINT('Ctrl Pts',(3.67200111268,-35.4007597143,-3.05775598766));
#53686=CARTESIAN_POINT('Ctrl Pts',(3.67266041516,-35.4528934978,-3.0611685886));
#53687=CARTESIAN_POINT('Ctrl Pts',(3.67198840819,-35.5050272814,-3.06145474134));
#53688=CARTESIAN_POINT('Ctrl Pts',(-1.69382496103,-35.2682576589,-5.01043544546));
#53689=CARTESIAN_POINT('Ctrl Pts',(-1.69402179658,-35.3094043143,-5.02023549828));
#53690=CARTESIAN_POINT('Ctrl Pts',(-1.69321049045,-35.351018059,-5.02809467113));
#53691=CARTESIAN_POINT('Ctrl Pts',(-1.69139030338,-35.3929455262,-5.03397642476));
#53692=CARTESIAN_POINT('Ctrl Pts',(-1.68856804502,-35.4350298576,-5.03785875444));
#53693=CARTESIAN_POINT('Ctrl Pts',(-1.6847579226,-35.4771141891,-5.03973467901));
#53694=CARTESIAN_POINT('Ctrl Pts',(-1.68490151218,-35.268974041,-5.01524294734));
#53695=CARTESIAN_POINT('Ctrl Pts',(-1.68651188124,-35.3098358784,-5.02415397172));
#53696=CARTESIAN_POINT('Ctrl Pts',(-1.68714086448,-35.3511508863,-5.03116493545));
#53697=CARTESIAN_POINT('Ctrl Pts',(-1.68678246934,-35.3927702163,-5.03624343644));
#53698=CARTESIAN_POINT('Ctrl Pts',(-1.68543788474,-35.4345417096,-5.03937097175));
#53699=CARTESIAN_POINT('Ctrl Pts',(-1.68311545107,-35.4763132029,-5.04054334111));
#53700=CARTESIAN_POINT('Ctrl Pts',(-1.67612908012,-35.2701100859,-5.02003914153));
#53701=CARTESIAN_POINT('Ctrl Pts',(-1.67913856906,-35.3106802184,-5.02807779826));
#53702=CARTESIAN_POINT('Ctrl Pts',(-1.68118935788,-35.3516915586,-5.03424982493));
#53703=CARTESIAN_POINT('Ctrl Pts',(-1.6822703811,-35.3929991785,-5.03852665843));
#53704=CARTESIAN_POINT('Ctrl Pts',(-1.68237796302,-35.4344548915,-5.04089285688));
#53705=CARTESIAN_POINT('Ctrl Pts',(-1.68151488066,-35.4759106045,-5.04134696784));
#53706=CARTESIAN_POINT('Ctrl Pts',(-1.66745641736,-35.2716459733,-5.02484351574));
#53707=CARTESIAN_POINT('Ctrl Pts',(-1.67185679176,-35.3119189644,-5.03202383893));
#53708=CARTESIAN_POINT('Ctrl Pts',(-1.67531720482,-35.3526230495,-5.03736380107));
#53709=CARTESIAN_POINT('Ctrl Pts',(-1.67782194293,-35.3936164734,-5.04083824001));
#53710=CARTESIAN_POINT('Ctrl Pts',(-1.67936231019,-35.4347546994,-5.04243484007));
#53711=CARTESIAN_POINT('Ctrl Pts',(-1.67993607839,-35.4758929253,-5.04215470289));
#53712=CARTESIAN_POINT('Ctrl Pts',(-1.65900707813,-35.2735686701,-5.02958783575));
#53713=CARTESIAN_POINT('Ctrl Pts',(-1.66477502429,-35.3135351172,-5.03593051298));
#53714=CARTESIAN_POINT('Ctrl Pts',(-1.6696184323,-35.3539241381,-5.04045242297));
#53715=CARTESIAN_POINT('Ctrl Pts',(-1.67351721006,-35.3945968399,-5.04313153636));
#53716=CARTESIAN_POINT('Ctrl Pts',(-1.67645771737,-35.4354113842,-5.0439585342));
#53717=CARTESIAN_POINT('Ctrl Pts',(-1.67843305643,-35.4762259285,-5.04293699751));
#53718=CARTESIAN_POINT('Ctrl Pts',(-1.65073625045,-35.2758278019,-5.0342827697));
#53719=CARTESIAN_POINT('Ctrl Pts',(-1.65785005217,-35.3154860139,-5.03981027692));
#53720=CARTESIAN_POINT('Ctrl Pts',(-1.66405116082,-35.3555599215,-5.04352991245));
#53721=CARTESIAN_POINT('Ctrl Pts',(-1.66931505993,-35.3959128757,-5.04542262153));
#53722=CARTESIAN_POINT('Ctrl Pts',(-1.67362354949,-35.4364053554,-5.04548186008));
#53723=CARTESIAN_POINT('Ctrl Pts',(-1.67696511998,-35.4768978351,-5.04371372921));
#53724=CARTESIAN_POINT('',(-1.69382496553272,-35.2682576607491,-5.01043544611819));
#53725=CARTESIAN_POINT('Origin',(-1.24303989658678,-35.4771141385556,-4.14258040411198));
#53726=CARTESIAN_POINT('',(-1.65073615062032,-35.2758275456167,-5.03428276116393));
#53727=CARTESIAN_POINT('Ctrl Pts',(-1.69382496014738,-35.268257661,-5.01043544642385));
#53728=CARTESIAN_POINT('Ctrl Pts',(-1.68803312612198,-35.2687226336122,
-5.01355579279809));
#53729=CARTESIAN_POINT('Ctrl Pts',(-1.68231297816127,-35.2693997637279,
-5.01667279399805));
#53730=CARTESIAN_POINT('Ctrl Pts',(-1.67666523914987,-35.2702777195431,
-5.0197822570377));
#53731=CARTESIAN_POINT('Ctrl Pts',(-1.67037182346692,-35.2712560474872,
-5.02324720883873));
#53732=CARTESIAN_POINT('Ctrl Pts',(-1.66417391129964,-35.2724846442873,
-5.02670011798684));
#53733=CARTESIAN_POINT('Ctrl Pts',(-1.65809711371162,-35.2739404345783,
-5.03012131671218));
#53734=CARTESIAN_POINT('Ctrl Pts',(-1.65562402628534,-35.2745329006942,
-5.03151364933934));
#53735=CARTESIAN_POINT('Ctrl Pts',(-1.65317074085282,-35.2751628346991,
-5.03290083178419));
#53736=CARTESIAN_POINT('Ctrl Pts',(-1.65073625045,-35.2758278019,-5.0342827697));
#53737=CARTESIAN_POINT('Origin',(-1.20926787984816,-35.4768981557406,-4.15982468247784));
#53738=CARTESIAN_POINT('Ctrl Pts',(-1.65073607085,-35.2758272825,-5.03428274092));
#53739=CARTESIAN_POINT('Ctrl Pts',(-1.65784980534,-35.3154856499,-5.03981034314));
#53740=CARTESIAN_POINT('Ctrl Pts',(-1.66405083454,-35.3555597177,-5.04353006314));
#53741=CARTESIAN_POINT('Ctrl Pts',(-1.66931464207,-35.3959128353,-5.04542284568));
#53742=CARTESIAN_POINT('Ctrl Pts',(-1.67362302807,-35.4364054801,-5.0454821464));
#53743=CARTESIAN_POINT('Ctrl Pts',(-1.67696448333,-35.4768981249,-5.04371406628));
#53744=CARTESIAN_POINT('Ctrl Pts',(-1.61326364266,-35.2619218696,-5.05000316771));
#53745=CARTESIAN_POINT('Ctrl Pts',(-1.62236549352,-35.3070877788,-5.05662956819));
#53746=CARTESIAN_POINT('Ctrl Pts',(-1.63007921825,-35.3528484277,-5.0610482607));
#53747=CARTESIAN_POINT('Ctrl Pts',(-1.63636464034,-35.3990097556,-5.06322951683));
#53748=CARTESIAN_POINT('Ctrl Pts',(-1.64119504878,-35.4453707616,-5.06316361876));
#53749=CARTESIAN_POINT('Ctrl Pts',(-1.64455688984,-35.4917317677,-5.06086202998));
#53750=CARTESIAN_POINT('Ctrl Pts',(-1.57763814761,-35.2502524393,-5.07162003768));
#53751=CARTESIAN_POINT('Ctrl Pts',(-1.58925529962,-35.3001212511,-5.07894359568));
#53752=CARTESIAN_POINT('Ctrl Pts',(-1.59886212553,-35.350806501,-5.08374537669));
#53753=CARTESIAN_POINT('Ctrl Pts',(-1.60640164997,-35.4020401921,-5.08598819927));
#53754=CARTESIAN_POINT('Ctrl Pts',(-1.6118338475,-35.4535491166,-5.08566006898));
#53755=CARTESIAN_POINT('Ctrl Pts',(-1.61513825447,-35.505058041,-5.08277314744));
#53756=CARTESIAN_POINT('Ctrl Pts',(-1.5467652741,-35.2408307961,-5.09796224817));
#53757=CARTESIAN_POINT('Ctrl Pts',(-1.56082810828,-35.2948250485,-5.10559533807));
#53758=CARTESIAN_POINT('Ctrl Pts',(-1.5721279205,-35.3498911181,-5.11056679276));
#53759=CARTESIAN_POINT('Ctrl Pts',(-1.58057518036,-35.4056813318,-5.11281573481));
#53760=CARTESIAN_POINT('Ctrl Pts',(-1.58611547612,-35.4618331019,-5.11233170678));
#53761=CARTESIAN_POINT('Ctrl Pts',(-1.58873141496,-35.5179848719,-5.10914094848));
#53762=CARTESIAN_POINT('Ctrl Pts',(-1.50094788409,-35.2255784603,-5.15114151002));
#53763=CARTESIAN_POINT('Ctrl Pts',(-1.51919307915,-35.2853745424,-5.15844241592));
#53764=CARTESIAN_POINT('Ctrl Pts',(-1.53333303669,-35.34668297,-5.16330955045));
#53765=CARTESIAN_POINT('Ctrl Pts',(-1.54322139667,-35.4090153954,-5.16568966994));
#53766=CARTESIAN_POINT('Ctrl Pts',(-1.54877729981,-35.471860276,-5.16555970229));
#53767=CARTESIAN_POINT('Ctrl Pts',(-1.54998925981,-35.5347051565,-5.16293840519));
#53768=CARTESIAN_POINT('Ctrl Pts',(-1.47301395752,-35.2164048258,-5.21579034781));
#53769=CARTESIAN_POINT('Ctrl Pts',(-1.49420720065,-35.2792319381,-5.22072059065));
#53770=CARTESIAN_POINT('Ctrl Pts',(-1.51037196702,-35.3438574448,-5.22412710654));
#53771=CARTESIAN_POINT('Ctrl Pts',(-1.52131309724,-35.4097044807,-5.22595779822));
#53772=CARTESIAN_POINT('Ctrl Pts',(-1.52692924844,-35.4761620333,-5.22619785569));
#53773=CARTESIAN_POINT('Ctrl Pts',(-1.52721834654,-35.5426195859,-5.22486268019));
#53774=CARTESIAN_POINT('Ctrl Pts',(-1.46470315626,-35.213766631,-5.24531814123));
#53775=CARTESIAN_POINT('Ctrl Pts',(-1.48680690707,-35.277355512,-5.24884399471));
#53776=CARTESIAN_POINT('Ctrl Pts',(-1.50361778858,-35.3428209065,-5.25131648121));
#53777=CARTESIAN_POINT('Ctrl Pts',(-1.51492750077,-35.4095603027,-5.25272449316));
#53778=CARTESIAN_POINT('Ctrl Pts',(-1.52062825527,-35.4769374515,-5.25304460068));
#53779=CARTESIAN_POINT('Ctrl Pts',(-1.52071813077,-35.5443146003,-5.25227472437));
#53780=CARTESIAN_POINT('Ctrl Pts',(-1.46069629729,-35.2129478838,-5.27610920663));
#53781=CARTESIAN_POINT('Ctrl Pts',(-1.48316494179,-35.2768382352,-5.27796326442));
#53782=CARTESIAN_POINT('Ctrl Pts',(-1.50022470946,-35.3426337834,-5.2792979259));
#53783=CARTESIAN_POINT('Ctrl Pts',(-1.51165995618,-35.4097245745,-5.28008044471));
#53784=CARTESIAN_POINT('Ctrl Pts',(-1.51736021529,-35.4774626159,-5.28030986048));
#53785=CARTESIAN_POINT('Ctrl Pts',(-1.51732687674,-35.5452006575,-5.27999548691));
#53786=CARTESIAN_POINT('Ctrl Pts',(-1.46090316329,-35.2135376551,-5.30645216923));
#53787=CARTESIAN_POINT('Ctrl Pts',(-1.48323786433,-35.277208474,-5.30683297122));
#53788=CARTESIAN_POINT('Ctrl Pts',(-1.50020219619,-35.3427631323,-5.30721377032));
#53789=CARTESIAN_POINT('Ctrl Pts',(-1.51158410625,-35.4095977304,-5.30759095434));
#53790=CARTESIAN_POINT('Ctrl Pts',(-1.51727462121,-35.4770723771,-5.30796091202));
#53791=CARTESIAN_POINT('Ctrl Pts',(-1.51727394979,-35.5445470238,-5.30832023528));
#53792=CARTESIAN_POINT('Ctrl Pts',(-1.65073607089,-35.2758272825,-5.03428274092));
#53793=CARTESIAN_POINT('Ctrl Pts',(-1.61326364266,-35.2619218696,-5.05000316771));
#53794=CARTESIAN_POINT('Ctrl Pts',(-1.57763814761,-35.2502524393,-5.07162003768));
#53795=CARTESIAN_POINT('Ctrl Pts',(-1.5467652741,-35.2408307961,-5.09796224817));
#53796=CARTESIAN_POINT('Ctrl Pts',(-1.50094788409,-35.2255784603,-5.15114151002));
#53797=CARTESIAN_POINT('Ctrl Pts',(-1.47301395752,-35.2164048258,-5.21579034781));
#53798=CARTESIAN_POINT('Ctrl Pts',(-1.46470315626,-35.213766631,-5.24531814123));
#53799=CARTESIAN_POINT('Ctrl Pts',(-1.46069629729,-35.2129478838,-5.27610920663));
#53800=CARTESIAN_POINT('Ctrl Pts',(-1.46090316329,-35.2135376551,-5.30645216923));
#53801=CARTESIAN_POINT('Origin',(-0.517273476326547,-35.5445474017573,-5.30645165992553));
#53802=CARTESIAN_POINT('Ctrl Pts',(-3.48890306473,-35.2652540838,-3.21461371005));
#53803=CARTESIAN_POINT('Ctrl Pts',(-3.49935367494,-35.3079501575,-3.21504790568));
#53804=CARTESIAN_POINT('Ctrl Pts',(-3.50770783242,-35.351170349,-3.21440294636));
#53805=CARTESIAN_POINT('Ctrl Pts',(-3.51392345177,-35.3947427768,-3.21267707712));
#53806=CARTESIAN_POINT('Ctrl Pts',(-3.51797541026,-35.4384913267,-3.20987727374));
#53807=CARTESIAN_POINT('Ctrl Pts',(-3.51985615043,-35.4822398766,-3.20601907528));
#53808=CARTESIAN_POINT('Ctrl Pts',(-3.24150677815,-35.2297273503,-3.67797056337));
#53809=CARTESIAN_POINT('Ctrl Pts',(-3.25788366108,-35.2867834422,-3.68259788135));
#53810=CARTESIAN_POINT('Ctrl Pts',(-3.2708619246,-35.3449131549,-3.6851550674));
#53811=CARTESIAN_POINT('Ctrl Pts',(-3.28034612237,-35.4037663878,-3.68562224436));
#53812=CARTESIAN_POINT('Ctrl Pts',(-3.28628025023,-35.4629813934,-3.68400243047));
#53813=CARTESIAN_POINT('Ctrl Pts',(-3.28864951001,-35.5221963991,-3.68032135));
#53814=CARTESIAN_POINT('Ctrl Pts',(-2.93020007641,-35.2159821642,-4.09471223066));
#53815=CARTESIAN_POINT('Ctrl Pts',(-2.94976329618,-35.2791022779,-4.10741039029));
#53816=CARTESIAN_POINT('Ctrl Pts',(-2.96507838407,-35.3440365738,-4.11671739461));
#53817=CARTESIAN_POINT('Ctrl Pts',(-2.97596822876,-35.4101991223,-4.12255014873));
#53818=CARTESIAN_POINT('Ctrl Pts',(-2.98233164479,-35.4769758456,-4.12487890497));
#53819=CARTESIAN_POINT('Ctrl Pts',(-2.984147828,-35.543752569,-4.12372796686));
#53820=CARTESIAN_POINT('Ctrl Pts',(-2.57349039398,-35.21650702,-4.45141980073));
#53821=CARTESIAN_POINT('Ctrl Pts',(-2.58535390407,-35.2792535748,-4.47101557567));
#53822=CARTESIAN_POINT('Ctrl Pts',(-2.59391358392,-35.3437511415,-4.48640413787));
#53823=CARTESIAN_POINT('Ctrl Pts',(-2.59909669842,-35.4094332325,-4.49741590343));
#53824=CARTESIAN_POINT('Ctrl Pts',(-2.60088024578,-35.4757076219,-4.50395318786));
#53825=CARTESIAN_POINT('Ctrl Pts',(-2.59929137485,-35.5419820113,-4.50599426346));
#53826=CARTESIAN_POINT('Ctrl Pts',(-2.15330460094,-35.2313461468,-4.76288665231));
#53827=CARTESIAN_POINT('Ctrl Pts',(-2.15740174514,-35.2874140925,-4.77869293776));
#53828=CARTESIAN_POINT('Ctrl Pts',(-2.15952364918,-35.3444755753,-4.7912469843));
#53829=CARTESIAN_POINT('Ctrl Pts',(-2.15965446887,-35.4022061334,-4.8004623347));
#53830=CARTESIAN_POINT('Ctrl Pts',(-2.15779886139,-35.4602712393,-4.80628788231));
#53831=CARTESIAN_POINT('Ctrl Pts',(-2.15398176798,-35.5183363452,-4.80870937341));
#53832=CARTESIAN_POINT('Ctrl Pts',(-1.69382497102,-35.2682575054,-5.0104353994));
#53833=CARTESIAN_POINT('Ctrl Pts',(-1.69402180198,-35.3094041642,-5.02023545326));
#53834=CARTESIAN_POINT('Ctrl Pts',(-1.69321049227,-35.3510179116,-5.02809462923));
#53835=CARTESIAN_POINT('Ctrl Pts',(-1.69139030263,-35.3929453813,-5.0339763881));
#53836=CARTESIAN_POINT('Ctrl Pts',(-1.68856804274,-35.4350297152,-5.03785872515));
#53837=CARTESIAN_POINT('Ctrl Pts',(-1.68475791979,-35.477114049,-5.03973465917));
#53838=CARTESIAN_POINT('',(-3.48890306745266,-35.2652540841568,-3.21461371228527));
#53839=CARTESIAN_POINT('Origin',(-2.62096730277507,-35.4822399141373,-2.76784133732473));
#53840=CARTESIAN_POINT('Ctrl Pts',(-3.48890306888,-35.2652540838,-3.21461371302));
#53841=CARTESIAN_POINT('Ctrl Pts',(-3.24150677815,-35.2297273503,-3.67797056337));
#53842=CARTESIAN_POINT('Ctrl Pts',(-2.93020007641,-35.2159821642,-4.09471223066));
#53843=CARTESIAN_POINT('Ctrl Pts',(-2.57349039398,-35.21650702,-4.45141980073));
#53844=CARTESIAN_POINT('Ctrl Pts',(-2.15330460094,-35.2313461468,-4.76288665231));
#53845=CARTESIAN_POINT('Ctrl Pts',(-1.69382496468,-35.2682576589,-5.01043545515));
#53846=CARTESIAN_POINT('Ctrl Pts',(-3.68960640636,-35.2436867043,-3.0159715009));
#53847=CARTESIAN_POINT('Ctrl Pts',(-3.68994006064,-35.2950048915,-3.03107790447));
#53848=CARTESIAN_POINT('Ctrl Pts',(-3.68889543318,-35.347263528,-3.04301993635));
#53849=CARTESIAN_POINT('Ctrl Pts',(-3.68647051515,-35.4001566503,-3.05170748236));
#53850=CARTESIAN_POINT('Ctrl Pts',(-3.68267985005,-35.4533670311,-3.05708843877));
#53851=CARTESIAN_POINT('Ctrl Pts',(-3.67755401867,-35.5065774118,-3.05915055738));
#53852=CARTESIAN_POINT('Ctrl Pts',(-3.68406493808,-35.2441669878,-3.01852789669));
#53853=CARTESIAN_POINT('Ctrl Pts',(-3.6852545996,-35.2952993243,-3.03313678947));
#53854=CARTESIAN_POINT('Ctrl Pts',(-3.68508444483,-35.3473574121,-3.04461628848));
#53855=CARTESIAN_POINT('Ctrl Pts',(-3.68354738519,-35.4000399811,-3.05288030368));
#53856=CARTESIAN_POINT('Ctrl Pts',(-3.68065246874,-35.4530348056,-3.05787988529));
#53857=CARTESIAN_POINT('Ctrl Pts',(-3.67642456268,-35.5060296301,-3.05960493674));
#53858=CARTESIAN_POINT('Ctrl Pts',(-3.67853556896,-35.2447691838,-3.02110736508));
#53859=CARTESIAN_POINT('Ctrl Pts',(-3.68058228399,-35.295713802,-3.03522035827));
#53860=CARTESIAN_POINT('Ctrl Pts',(-3.68128649848,-35.3475703565,-3.04623632347));
#53861=CARTESIAN_POINT('Ctrl Pts',(-3.68063618362,-35.4000419929,-3.05407302366));
#53862=CARTESIAN_POINT('Ctrl Pts',(-3.67863507204,-35.4528211843,-3.05868456544));
#53863=CARTESIAN_POINT('Ctrl Pts',(-3.67530251301,-35.5056003757,-3.0600629924));
#53864=CARTESIAN_POINT('Ctrl Pts',(-3.67302394084,-35.2454929622,-3.02370658462));
#53865=CARTESIAN_POINT('Ctrl Pts',(-3.6759278736,-35.2962481955,-3.03732595805));
#53866=CARTESIAN_POINT('Ctrl Pts',(-3.67750544789,-35.3479024371,-3.04787800394));
#53867=CARTESIAN_POINT('Ctrl Pts',(-3.67773982365,-35.4001629685,-3.05528416988));
#53868=CARTESIAN_POINT('Ctrl Pts',(-3.67662956704,-35.4527266586,-3.05950153137));
#53869=CARTESIAN_POINT('Ctrl Pts',(-3.67418869929,-35.5052903486,-3.06052426199));
#53870=CARTESIAN_POINT('Ctrl Pts',(-3.6675348968,-35.2463373792,-3.02632251085));
#53871=CARTESIAN_POINT('Ctrl Pts',(-3.67129543056,-35.2969017565,-3.03945109726));
#53872=CARTESIAN_POINT('Ctrl Pts',(-3.67374456646,-35.348353094,-3.04953936585));
#53873=CARTESIAN_POINT('Ctrl Pts',(-3.67486076111,-35.4004025315,-3.05651229579));
#53874=CARTESIAN_POINT('Ctrl Pts',(-3.67463755638,-35.4527510324,-3.06032984675));
#53875=CARTESIAN_POINT('Ctrl Pts',(-3.67308380368,-35.5050995333,-3.0609883158));
#53876=CARTESIAN_POINT('Ctrl Pts',(-3.66207264655,-35.2473009405,-3.02895231242));
#53877=CARTESIAN_POINT('Ctrl Pts',(-3.66668846955,-35.2976731782,-3.04159341678));
#53878=CARTESIAN_POINT('Ctrl Pts',(-3.67000667781,-35.348921195,-3.05121851933));
#53879=CARTESIAN_POINT('Ctrl Pts',(-3.67200111268,-35.4007597143,-3.05775598766));
#53880=CARTESIAN_POINT('Ctrl Pts',(-3.67266041516,-35.4528934978,-3.0611685886));
#53881=CARTESIAN_POINT('Ctrl Pts',(-3.67198840819,-35.5050272814,-3.06145474134));
#53882=CARTESIAN_POINT('',(-3.68960640636,-35.2436867043,-3.0159715009));
#53883=CARTESIAN_POINT('Origin',(-3.30432478046144,-35.5065775306539,-2.13141045567169));
#53884=CARTESIAN_POINT('Origin',(-3.69828822169992,-35.4059562737349,-3.04854457261671));
#53885=CARTESIAN_POINT('Origin',(-3.28022457192059,-35.5050282606332,-2.14138812518752));
#53886=CARTESIAN_POINT('Ctrl Pts',(-3.66207294828,-35.2473021021,-3.02895254907));
#53887=CARTESIAN_POINT('Ctrl Pts',(-3.66668938645,-35.2976742927,-3.04159327346));
#53888=CARTESIAN_POINT('Ctrl Pts',(-3.67000827764,-35.3489222549,-3.05121799304));
#53889=CARTESIAN_POINT('Ctrl Pts',(-3.67200345992,-35.4007607145,-3.05775507809));
#53890=CARTESIAN_POINT('Ctrl Pts',(-3.6726635701,-35.4528944359,-3.06116729793));
#53891=CARTESIAN_POINT('Ctrl Pts',(-3.67199242621,-35.5050281572,-3.06145307387));
#53892=CARTESIAN_POINT('Ctrl Pts',(-3.64556722008,-35.248406313,-3.03637428958));
#53893=CARTESIAN_POINT('Ctrl Pts',(-3.65069501362,-35.2983832695,-3.04859774823));
#53894=CARTESIAN_POINT('Ctrl Pts',(-3.65437679925,-35.3492138965,-3.0579274977));
#53895=CARTESIAN_POINT('Ctrl Pts',(-3.65658079285,-35.4006204961,-3.06429584207));
#53896=CARTESIAN_POINT('Ctrl Pts',(-3.65729581475,-35.4523147284,-3.06766652406));
#53897=CARTESIAN_POINT('Ctrl Pts',(-3.65652775557,-35.5040089607,-3.06803796128));
#53898=CARTESIAN_POINT('Ctrl Pts',(-3.62977987226,-35.2496170208,-3.04490879463));
#53899=CARTESIAN_POINT('Ctrl Pts',(-3.63528692384,-35.2991304944,-3.05669637995));
#53900=CARTESIAN_POINT('Ctrl Pts',(-3.63920530469,-35.3494729369,-3.06573183442));
#53901=CARTESIAN_POINT('Ctrl Pts',(-3.6415096169,-35.4003733514,-3.07195030901));
#53902=CARTESIAN_POINT('Ctrl Pts',(-3.6421854279,-35.4515533116,-3.07531862585));
#53903=CARTESIAN_POINT('Ctrl Pts',(-3.64123559569,-35.5027332718,-3.07583329833));
#53904=CARTESIAN_POINT('Ctrl Pts',(-3.61439747244,-35.2508930805,-3.05469265108));
#53905=CARTESIAN_POINT('Ctrl Pts',(-3.62030288916,-35.2998487222,-3.06596829565));
#53906=CARTESIAN_POINT('Ctrl Pts',(-3.62450774723,-35.349603179,-3.07465066951));
#53907=CARTESIAN_POINT('Ctrl Pts',(-3.62697838143,-35.3998970016,-3.08067727275));
#53908=CARTESIAN_POINT('Ctrl Pts',(-3.6277014573,-35.4504596751,-3.08401633821));
#53909=CARTESIAN_POINT('Ctrl Pts',(-3.62668459499,-35.5010223485,-3.0846663226));
#53910=CARTESIAN_POINT('Ctrl Pts',(-3.57818606717,-35.254427601,-3.08171182978));
#53911=CARTESIAN_POINT('Ctrl Pts',(-3.58499819528,-35.3018787149,-3.09155249699));
#53912=CARTESIAN_POINT('Ctrl Pts',(-3.58987595331,-35.3500528463,-3.09920396626));
#53913=CARTESIAN_POINT('Ctrl Pts',(-3.59278825537,-35.398712151,-3.1046211988));
#53914=CARTESIAN_POINT('Ctrl Pts',(-3.5937205131,-35.4476152765,-3.10777655729));
#53915=CARTESIAN_POINT('Ctrl Pts',(-3.59267477187,-35.4965184022,-3.10866282874));
#53916=CARTESIAN_POINT('Ctrl Pts',(-3.54680562214,-35.2591381386,-3.11518399273));
#53917=CARTESIAN_POINT('Ctrl Pts',(-3.55425275129,-35.3047560463,-3.12331909977));
#53918=CARTESIAN_POINT('Ctrl Pts',(-3.55966404915,-35.3510104673,-3.12970468618));
#53919=CARTESIAN_POINT('Ctrl Pts',(-3.56300079879,-35.3976954964,-3.13429853608));
#53920=CARTESIAN_POINT('Ctrl Pts',(-3.56424741272,-35.4445940509,-3.13708068529));
#53921=CARTESIAN_POINT('Ctrl Pts',(-3.56341230092,-35.4914926054,-3.13805072514));
#53922=CARTESIAN_POINT('Ctrl Pts',(-3.53059439149,-35.2625776925,-3.1368950068));
#53923=CARTESIAN_POINT('Ctrl Pts',(-3.53819496617,-35.3070386414,-3.14399854711));
#53924=CARTESIAN_POINT('Ctrl Pts',(-3.54372649014,-35.3520895186,-3.14959798998));
#53925=CARTESIAN_POINT('Ctrl Pts',(-3.5471637516,-35.3975290806,-3.15368535098));
#53926=CARTESIAN_POINT('Ctrl Pts',(-3.54849609615,-35.4431689738,-3.15623708405));
#53927=CARTESIAN_POINT('Ctrl Pts',(-3.54771350151,-35.4888088673,-3.15723408602));
#53928=CARTESIAN_POINT('Ctrl Pts',(-3.51717283568,-35.2661737422,-3.15933443135));
#53929=CARTESIAN_POINT('Ctrl Pts',(-3.52465704951,-35.3092672059,-3.16566526845));
#53930=CARTESIAN_POINT('Ctrl Pts',(-3.53010225982,-35.3528915117,-3.17076845393));
#53931=CARTESIAN_POINT('Ctrl Pts',(-3.53347292436,-35.3968779115,-3.17460348458));
#53932=CARTESIAN_POINT('Ctrl Pts',(-3.53475243752,-35.4410413734,-3.17715872601));
#53933=CARTESIAN_POINT('Ctrl Pts',(-3.53395300191,-35.485204835,-3.17843874804));
#53934=CARTESIAN_POINT('Ctrl Pts',(-3.50597877122,-35.2696531524,-3.18321806272));
#53935=CARTESIAN_POINT('Ctrl Pts',(-3.51333812365,-35.3113502754,-3.18868521568));
#53936=CARTESIAN_POINT('Ctrl Pts',(-3.51870904583,-35.3535297557,-3.19315013683));
#53937=CARTESIAN_POINT('Ctrl Pts',(-3.52206358055,-35.3960332589,-3.19659205988));
#53938=CARTESIAN_POINT('Ctrl Pts',(-3.52338894151,-35.4386987766,-3.19899786544));
#53939=CARTESIAN_POINT('Ctrl Pts',(-3.5226878028,-35.4813642944,-3.200362378));
#53940=CARTESIAN_POINT('Origin',(-2.63323785737628,-35.4813643327716,-2.74332899791325));
#53941=CARTESIAN_POINT('Ctrl Pts',(-3.50597880735,-35.2696545374,-3.18321831335));
#53942=CARTESIAN_POINT('Ctrl Pts',(-3.51333803189,-35.3113514663,-3.18868569298));
#53943=CARTESIAN_POINT('Ctrl Pts',(-3.51870881162,-35.353530752,-3.19315085121));
#53944=CARTESIAN_POINT('Ctrl Pts',(-3.52206318971,-35.3960340603,-3.19659302084));
#53945=CARTESIAN_POINT('Ctrl Pts',(-3.52338838043,-35.4386993829,-3.1989990815));
#53946=CARTESIAN_POINT('Ctrl Pts',(-3.52268705855,-35.4813647056,-3.20036385665));
#53947=CARTESIAN_POINT('Ctrl Pts',(-3.50256004198,-35.268393509,-3.18939410052));
#53948=CARTESIAN_POINT('Ctrl Pts',(-3.51052316476,-35.3102955518,-3.1938621313));
#53949=CARTESIAN_POINT('Ctrl Pts',(-3.51648359784,-35.3526863763,-3.19731644996));
#53950=CARTESIAN_POINT('Ctrl Pts',(-3.52041085984,-35.3954055593,-3.19973991273));
#53951=CARTESIAN_POINT('Ctrl Pts',(-3.52228987577,-35.4382889251,-3.2011231722));
#53952=CARTESIAN_POINT('Ctrl Pts',(-3.52212131885,-35.4811722908,-3.20146489487));
#53953=CARTESIAN_POINT('Ctrl Pts',(-3.49913203155,-35.2673150056,-3.1956382498));
#53954=CARTESIAN_POINT('Ctrl Pts',(-3.50770826391,-35.3094204104,-3.19910017162));
#53955=CARTESIAN_POINT('Ctrl Pts',(-3.51426388564,-35.3520219724,-3.20153494382));
#53956=CARTESIAN_POINT('Ctrl Pts',(-3.5187657727,-35.3949568785,-3.20292908338));
#53957=CARTESIAN_POINT('Ctrl Pts',(-3.52119645205,-35.4380584515,-3.20327716833));
#53958=CARTESIAN_POINT('Ctrl Pts',(-3.52155459752,-35.4811600245,-3.20258180379));
#53959=CARTESIAN_POINT('Ctrl Pts',(-3.49570498282,-35.2664275319,-3.20193555292));
#53960=CARTESIAN_POINT('Ctrl Pts',(-3.5049017062,-35.3087336513,-3.20438752525));
#53961=CARTESIAN_POINT('Ctrl Pts',(-3.51205619329,-35.3515442739,-3.2057969486));
#53962=CARTESIAN_POINT('Ctrl Pts',(-3.51713243885,-35.3946938503,-3.20615423225));
#53963=CARTESIAN_POINT('Ctrl Pts',(-3.52011064813,-35.4380129429,-3.20545771792));
#53964=CARTESIAN_POINT('Ctrl Pts',(-3.52098739307,-35.4813320354,-3.20371424309));
#53965=CARTESIAN_POINT('Ctrl Pts',(-3.49229725928,-35.2657414976,-3.2082566117));
#53966=CARTESIAN_POINT('Ctrl Pts',(-3.50211831443,-35.308244275,-3.20970015733));
#53967=CARTESIAN_POINT('Ctrl Pts',(-3.50987186481,-35.3512608603,-3.21008384904));
#53968=CARTESIAN_POINT('Ctrl Pts',(-3.51551898686,-35.3946227115,-3.20940189333));
#53969=CARTESIAN_POINT('Ctrl Pts',(-3.51903723035,-35.4381571989,-3.20765694424));
#53970=CARTESIAN_POINT('Ctrl Pts',(-3.52042115146,-35.4816916863,-3.20486003554));
#53971=CARTESIAN_POINT('Ctrl Pts',(-3.4889030666,-35.265254082,-3.21461371656));
#53972=CARTESIAN_POINT('Ctrl Pts',(-3.49935367791,-35.3079501561,-3.21504791216));
#53973=CARTESIAN_POINT('Ctrl Pts',(-3.50770783634,-35.3511703481,-3.21440295273));
#53974=CARTESIAN_POINT('Ctrl Pts',(-3.51392345649,-35.3947427765,-3.21267708331));
#53975=CARTESIAN_POINT('Ctrl Pts',(-3.51797541562,-35.4384913269,-3.20987727967));
#53976=CARTESIAN_POINT('Ctrl Pts',(-3.51985615629,-35.4822398773,-3.20601908088));
#53977=CARTESIAN_POINT('Origin',(-3.5116682051481,-35.3848727889406,-3.20631688515481));
#53978=CARTESIAN_POINT('Ctrl Pts',(-7.05021190275,-35.3742261151,1.16209541223));
#53979=CARTESIAN_POINT('Ctrl Pts',(-7.05021190275,-35.3742261151,1.16209541223));
#53980=CARTESIAN_POINT('Ctrl Pts',(-7.05021190275,-35.3742261151,1.16209541223));
#53981=CARTESIAN_POINT('Ctrl Pts',(-7.05021190275,-35.3742261151,1.16209541223));
#53982=CARTESIAN_POINT('Ctrl Pts',(-7.05021190275,-35.3742261151,1.16209541223));
#53983=CARTESIAN_POINT('Ctrl Pts',(-7.05021190275,-35.3742261151,1.16209541223));
#53984=CARTESIAN_POINT('Ctrl Pts',(-7.01340171355,-35.3233663073,0.887814197822));
#53985=CARTESIAN_POINT('Ctrl Pts',(-7.01381986471783,-35.3413180972,0.890929938671949));
#53986=CARTESIAN_POINT('Ctrl Pts',(-7.01423801594781,-35.3592698878,0.894045679984952));
#53987=CARTESIAN_POINT('Ctrl Pts',(-7.01465616709811,-35.377221677,0.897161420704254));
#53988=CARTESIAN_POINT('Ctrl Pts',(-7.01507431822199,-35.3951734669,0.900277161226733));
#53989=CARTESIAN_POINT('Ctrl Pts',(-7.01549246939,-35.4131252568,0.903392902078));
#53990=CARTESIAN_POINT('Ctrl Pts',(-6.95185482919,-35.2775995372,0.614848488511));
#53991=CARTESIAN_POINT('Ctrl Pts',(-6.95711039026,-35.3122184667,0.620033495106));
#53992=CARTESIAN_POINT('Ctrl Pts',(-6.96131634916,-35.3468297586,0.625353240693));
#53993=CARTESIAN_POINT('Ctrl Pts',(-6.96447793891,-35.3814361808,0.630808421027));
#53994=CARTESIAN_POINT('Ctrl Pts',(-6.96659784091,-35.4160401708,0.636399696014));
#53995=CARTESIAN_POINT('Ctrl Pts',(-6.96767646618,-35.4506441608,0.642127552041));
#53996=CARTESIAN_POINT('Ctrl Pts',(-6.8673530143,-35.2439788226,0.343363482131));
#53997=CARTESIAN_POINT('Ctrl Pts',(-6.87994051011,-35.2916209137,0.34796525773));
#53998=CARTESIAN_POINT('Ctrl Pts',(-6.88986767191,-35.3397700495,0.353240035009));
#53999=CARTESIAN_POINT('Ctrl Pts',(-6.89711069428,-35.38825575,0.359155938781));
#54000=CARTESIAN_POINT('Ctrl Pts',(-6.90165550114,-35.4369097195,0.365681814414));
#54001=CARTESIAN_POINT('Ctrl Pts',(-6.90349674466,-35.485563689,0.372787607728));
#54002=CARTESIAN_POINT('Ctrl Pts',(-6.64187024435,-35.1886753155,-0.23870995558));
#54003=CARTESIAN_POINT('Ctrl Pts',(-6.66955139679,-35.2585364198,-0.239842936739));
#54004=CARTESIAN_POINT('Ctrl Pts',(-6.691390474,-35.3305802147,-0.238616506959));
#54005=CARTESIAN_POINT('Ctrl Pts',(-6.70712809876,-35.4041022846,-0.23504887133));
#54006=CARTESIAN_POINT('Ctrl Pts',(-6.71661554426,-35.4783635248,-0.229196354076));
#54007=CARTESIAN_POINT('Ctrl Pts',(-6.71982081074,-35.5526247648,-0.221149174844));
#54008=CARTESIAN_POINT('Ctrl Pts',(-6.335633879,-35.1655247078,-0.779903703387));
#54009=CARTESIAN_POINT('Ctrl Pts',(-6.37258533768,-35.2460676029,-0.793096558606));
#54010=CARTESIAN_POINT('Ctrl Pts',(-6.40175618506,-35.3308011559,-0.801727405553));
#54011=CARTESIAN_POINT('Ctrl Pts',(-6.42255691503,-35.4184152395,-0.805611032625));
#54012=CARTESIAN_POINT('Ctrl Pts',(-6.43465051901,-35.5074700242,-0.804704006103));
#54013=CARTESIAN_POINT('Ctrl Pts',(-6.43798249823,-35.5965248091,-0.799107100072));
#54014=CARTESIAN_POINT('Ctrl Pts',(-6.1477485618,-35.1585065417,-1.0593892471));
#54015=CARTESIAN_POINT('Ctrl Pts',(-6.1862455007,-35.2425122041,-1.07972455995));
#54016=CARTESIAN_POINT('Ctrl Pts',(-6.21657209688,-35.331564736,-1.09437680653));
#54017=CARTESIAN_POINT('Ctrl Pts',(-6.23800931387,-35.4241081414,-1.10297704478));
#54018=CARTESIAN_POINT('Ctrl Pts',(-6.25014939755,-35.5183977765,-1.10536973107));
#54019=CARTESIAN_POINT('Ctrl Pts',(-6.25293978467,-35.6126874115,-1.1016283265));
#54020=CARTESIAN_POINT('Ctrl Pts',(-5.64263928747,-35.1503549657,-1.69778761613));
#54021=CARTESIAN_POINT('Ctrl Pts',(-5.6781072677,-35.2388302664,-1.73263418024));
#54022=CARTESIAN_POINT('Ctrl Pts',(-5.70553308479,-35.3334375132,-1.75965360778));
#54023=CARTESIAN_POINT('Ctrl Pts',(-5.72416357539,-35.4323082835,-1.77811755991));
#54024=CARTESIAN_POINT('Ctrl Pts',(-5.7335949111,-35.5333121034,-1.78763419494));
#54025=CARTESIAN_POINT('Ctrl Pts',(-5.73382235555,-35.6343159234,-1.78819570677));
#54026=CARTESIAN_POINT('Ctrl Pts',(-5.01710815157,-35.1629277461,-2.24626629333));
#54027=CARTESIAN_POINT('Ctrl Pts',(-5.03812134505,-35.2465940911,-2.28433468893));
#54028=CARTESIAN_POINT('Ctrl Pts',(-5.05330548672,-35.3352292266,-2.31441076458));
#54029=CARTESIAN_POINT('Ctrl Pts',(-5.06229638123,-35.4272996663,-2.33577662822));
#54030=CARTESIAN_POINT('Ctrl Pts',(-5.06494250992,-35.5210885082,-2.34802021045));
#54031=CARTESIAN_POINT('Ctrl Pts',(-5.06131871348,-35.6148773502,-2.35107992573));
#54032=CARTESIAN_POINT('Ctrl Pts',(-4.60859161999,-35.1762367254,-2.53785301358));
#54033=CARTESIAN_POINT('Ctrl Pts',(-4.61998718798,-35.2544472454,-2.57156731299));
#54034=CARTESIAN_POINT('Ctrl Pts',(-4.62723219199,-35.3360986017,-2.59812098394));
#54035=CARTESIAN_POINT('Ctrl Pts',(-4.63022512886,-35.4200944121,-2.61708014375));
#54036=CARTESIAN_POINT('Ctrl Pts',(-4.62896118843,-35.5052625726,-2.62819842135));
#54037=CARTESIAN_POINT('Ctrl Pts',(-4.62352979415,-35.5904307331,-2.63143094545));
#54038=CARTESIAN_POINT('Ctrl Pts',(-4.16372827527,-35.2025940852,-2.79724907986));
#54039=CARTESIAN_POINT('Ctrl Pts',(-4.16779886982,-35.2702188379,-2.82151459563));
#54040=CARTESIAN_POINT('Ctrl Pts',(-4.16935260067,-35.3397404397,-2.84063625327));
#54041=CARTESIAN_POINT('Ctrl Pts',(-4.16836377754,-35.4105469366,-2.8544077757));
#54042=CARTESIAN_POINT('Ctrl Pts',(-4.16484831327,-35.4819959329,-2.86271080605));
#54043=CARTESIAN_POINT('Ctrl Pts',(-4.15886281142,-35.5534449291,-2.86552034537));
#54044=CARTESIAN_POINT('Ctrl Pts',(-3.68960640598,-35.2436867043,-3.01597150109));
#54045=CARTESIAN_POINT('Ctrl Pts',(-3.68994006034,-35.2950048916,-3.03107790462));
#54046=CARTESIAN_POINT('Ctrl Pts',(-3.68889543294,-35.347263528,-3.04301993645));
#54047=CARTESIAN_POINT('Ctrl Pts',(-3.68647051499,-35.4001566504,-3.05170748242));
#54048=CARTESIAN_POINT('Ctrl Pts',(-3.68267984997,-35.4533670311,-3.0570884388));
#54049=CARTESIAN_POINT('Ctrl Pts',(-3.67755401867,-35.5065774118,-3.05915055738));
#54050=CARTESIAN_POINT('Ctrl Pts',(-7.05021189275609,-35.3742261012918,
1.16209533776304));
#54051=CARTESIAN_POINT('Ctrl Pts',(-7.01340171769854,-35.3233670493629,
0.887814269053016));
#54052=CARTESIAN_POINT('Ctrl Pts',(-6.95185503558031,-35.2776009819157,
0.614848661487126));
#54053=CARTESIAN_POINT('Ctrl Pts',(-6.86735353046522,-35.2439808156064,
0.343363646181602));
#54054=CARTESIAN_POINT('Ctrl Pts',(-6.641871396359,-35.188678241423,-0.23871001639011));
#54055=CARTESIAN_POINT('Ctrl Pts',(-6.33563542689691,-35.1655280817574,
-0.779904256034562));
#54056=CARTESIAN_POINT('Ctrl Pts',(-6.14775017443704,-35.1585100607139,
-1.05939009894544));
#54057=CARTESIAN_POINT('Ctrl Pts',(-5.64264077322358,-35.1503586719484,
-1.69778907585251));
#54058=CARTESIAN_POINT('Ctrl Pts',(-5.01710903181186,-35.1629312508997,
-2.24626788801542));
#54059=CARTESIAN_POINT('Ctrl Pts',(-4.60859209734921,-35.1762400016533,
-2.53785442587224));
#54060=CARTESIAN_POINT('Ctrl Pts',(-4.16372844578607,-35.2025969180128,
-2.79725009634263));
#54061=CARTESIAN_POINT('Ctrl Pts',(-3.68960640636,-35.2436867043,-3.0159715009));
#54062=CARTESIAN_POINT('Ctrl Pts',(-3.67755550257331,-35.3742477797272,
-3.0591534519424));
#54063=CARTESIAN_POINT('Ctrl Pts',(-3.32386409198,-32.4742356128,-2.36922853848));
#54064=CARTESIAN_POINT('Ctrl Pts',(-4.22884692807269,-35.3742477797272,
-2.83737078185739));
#54065=CARTESIAN_POINT('Ctrl Pts',(-3.82968047509,-32.4742356128,-1.81532491987));
#54066=CARTESIAN_POINT('Ctrl Pts',(-4.75872659660362,-35.3742477797272,
-2.56236446563048));
#54067=CARTESIAN_POINT('Ctrl Pts',(-4.31529317605,-32.4742356128,-1.24297128633));
#54068=CARTESIAN_POINT('Ctrl Pts',(-5.25779759486713,-35.3742477797272,
-2.22279170313982));
#54069=CARTESIAN_POINT('Ctrl Pts',(-4.78073424536,-32.4742356128,-0.651925339842));
#54070=CARTESIAN_POINT('Ctrl Pts',(-6.1337700409067,-35.3742477797272,-1.39617908277916));
#54071=CARTESIAN_POINT('Ctrl Pts',(-5.66596200411,-32.4742356128,0.560784091783));
#54072=CARTESIAN_POINT('Ctrl Pts',(-6.70708334214704,-35.3742477797272,
-0.336679612997994));
#54073=CARTESIAN_POINT('Ctrl Pts',(-6.46037298138,-32.4742356128,1.83459706183));
#54074=CARTESIAN_POINT('Ctrl Pts',(-6.90223544201876,-35.3742477797272,
0.234409171633676));
#54075=CARTESIAN_POINT('Ctrl Pts',(-6.83383584614,-32.4742356128,2.48513748583));
#54076=CARTESIAN_POINT('Ctrl Pts',(-7.02153225855751,-35.3742477797272,
0.820419960836672));
#54077=CARTESIAN_POINT('Ctrl Pts',(-7.18368375786,-32.4742356128,3.149547989));
#54078=CARTESIAN_POINT('Ctrl Pts',(-7.07911812989542,-35.3742477797272,
1.41232328791478));
#54079=CARTESIAN_POINT('Ctrl Pts',(-7.50890612221,-32.4742356128,3.82595376918));
#54080=CARTESIAN_POINT('',(-7.50890612221,-32.4742356128,3.82595376918));
#54081=CARTESIAN_POINT('',(-7.07911993306,-35.3742356128,1.41233341424));
#54082=CARTESIAN_POINT('Ctrl Pts',(-7.50890612221,-32.4742356128,3.82595376918));
#54083=CARTESIAN_POINT('Ctrl Pts',(-6.96684733231567,-32.4742356128,2.69856605273344));
#54084=CARTESIAN_POINT('Ctrl Pts',(-6.34321709883092,-32.4742356128,1.612247552867));
#54085=CARTESIAN_POINT('Ctrl Pts',(-4.9426430764693,-32.4742356128,-0.461097896531036));
#54086=CARTESIAN_POINT('Ctrl Pts',(-4.1675411517523,-32.4742356128,-1.44534431497417));
#54087=CARTESIAN_POINT('Ctrl Pts',(-3.32386409198001,-32.4742356128,-2.36922853847999));
#54088=CARTESIAN_POINT('Ctrl Pts',(-7.07911993306,-35.3742356128,1.41233341424));
#54089=CARTESIAN_POINT('Ctrl Pts',(-7.50890612221,-32.4742356128,3.82595376918));
#54090=CARTESIAN_POINT('Ctrl Pts',(-7.09439816601,-35.3742356128,1.56936058085));
#54091=CARTESIAN_POINT('Ctrl Pts',(-7.59518497882,-32.4742356128,4.00539873882));
#54092=CARTESIAN_POINT('Ctrl Pts',(-7.10532841684,-35.3742356128,1.72680313633));
#54093=CARTESIAN_POINT('Ctrl Pts',(-7.6797307274,-32.4742356128,4.18568800425));
#54094=CARTESIAN_POINT('Ctrl Pts',(-7.08904842402,-35.3742356128,1.89842406838));
#54095=CARTESIAN_POINT('Ctrl Pts',(-7.76642508589,-32.4742356128,4.37540694872));
#54096=CARTESIAN_POINT('Ctrl Pts',(-7.1390862001,-35.3742356128,2.05065495714));
#54097=CARTESIAN_POINT('Ctrl Pts',(-7.84739395748,-32.4742356128,4.5573230698));
#54098=CARTESIAN_POINT('Ctrl Pts',(-7.21384189759,-35.3742356128,2.18958432614));
#54099=CARTESIAN_POINT('Ctrl Pts',(-7.92659403983,-32.4742356128,4.74000601033));
#54100=CARTESIAN_POINT('Ctrl Pts',(-7.92659403983,-32.4742356128,4.74000601033));
#54101=CARTESIAN_POINT('Ctrl Pts',(-7.85943746154874,-32.4742356128,4.58510262093531));
#54102=CARTESIAN_POINT('Ctrl Pts',(-7.79122837535821,-32.4742356128,4.43204332182943));
#54103=CARTESIAN_POINT('Ctrl Pts',(-7.65314301021617,-32.4742356128,4.12986259705412));
#54104=CARTESIAN_POINT('Ctrl Pts',(-7.58206613716612,-32.4742356128,3.97811383687775));
#54105=CARTESIAN_POINT('Ctrl Pts',(-7.50890612221,-32.4742356128,3.82595376918));
#54106=CARTESIAN_POINT('',(-7.21702818953265,-35.2986940617107,2.22615323676817));
#54107=CARTESIAN_POINT('Ctrl Pts',(-7.21702817531,-35.2986941477,2.22615317529));
#54108=CARTESIAN_POINT('Ctrl Pts',(-7.20692741189441,-35.3061131910589,
2.20294516691052));
#54109=CARTESIAN_POINT('Ctrl Pts',(-7.19719329525834,-35.3141912841077,
2.17900438661006));
#54110=CARTESIAN_POINT('Ctrl Pts',(-7.18796980246911,-35.3226070668248,
2.15465538142052));
#54111=CARTESIAN_POINT('Ctrl Pts',(-7.18234237094649,-35.3277416987947,
2.1397995819442));
#54112=CARTESIAN_POINT('Ctrl Pts',(-7.17690465211826,-35.3330009806929,
2.12479257546628));
#54113=CARTESIAN_POINT('Ctrl Pts',(-7.17168536591732,-35.3383049690758,
2.10971258769397));
#54114=CARTESIAN_POINT('Ctrl Pts',(-7.16774304131616,-35.342311272444,2.0983221016215));
#54115=CARTESIAN_POINT('Ctrl Pts',(-7.16392050826559,-35.3463755747386,
2.08687105022291));
#54116=CARTESIAN_POINT('Ctrl Pts',(-7.160224977354,-35.3504229454298,2.07538760256753));
#54117=CARTESIAN_POINT('Ctrl Pts',(-7.15647459950107,-35.3545303848657,
2.06373372419597));
#54118=CARTESIAN_POINT('Ctrl Pts',(-7.15285530677851,-35.3586203097449,
2.05204630782424));
#54119=CARTESIAN_POINT('Ctrl Pts',(-7.14937553131797,-35.3626673165653,
2.0403417618537));
#54120=CARTESIAN_POINT('Ctrl Pts',(-7.14731388684394,-35.3650650256538,
2.0334072303603));
#54121=CARTESIAN_POINT('Ctrl Pts',(-7.14530121097212,-35.3674486946293,
2.02646644336296));
#54122=CARTESIAN_POINT('Ctrl Pts',(-7.14333877168014,-35.3698214557652,
2.01952124225387));
#54123=CARTESIAN_POINT('Ctrl Pts',(-7.14233333890139,-35.3710371121333,
2.01596294983756));
#54124=CARTESIAN_POINT('Ctrl Pts',(-7.14133929086512,-35.3722572507634,
2.01239698022069));
#54125=CARTESIAN_POINT('Ctrl Pts',(-7.14035958693292,-35.3734664689908,
2.00883384018666));
#54126=CARTESIAN_POINT('Ctrl Pts',(-7.14015072156521,-35.3737242650467,
2.00807420604724));
#54127=CARTESIAN_POINT('Ctrl Pts',(-7.13994249884667,-35.3739817495794,
2.00731466330883));
#54128=CARTESIAN_POINT('Ctrl Pts',(-7.13973493084178,-35.3742390721046,
2.00655525500559));
#54129=CARTESIAN_POINT('Ctrl Pts',(-7.23545016824,-35.2863172732,2.26690461571));
#54130=CARTESIAN_POINT('Ctrl Pts',(-7.23162479878,-35.288610995,2.25877896783));
#54131=CARTESIAN_POINT('Ctrl Pts',(-7.22786970762,-35.291024056,2.2506285999));
#54132=CARTESIAN_POINT('Ctrl Pts',(-7.22418450574,-35.2935251725,2.24246594859));
#54133=CARTESIAN_POINT('Ctrl Pts',(-7.22057030307,-35.2960900286,2.23430349206));
#54134=CARTESIAN_POINT('Ctrl Pts',(-7.2170282235,-35.2986939836,2.22615333516));
#54135=CARTESIAN_POINT('Ctrl Pts',(-7.21702817531,-35.2986941477,2.22615317529));
#54136=CARTESIAN_POINT('Ctrl Pts',(-7.21896716995,-35.3316547085,2.21752764579));
#54137=CARTESIAN_POINT('Ctrl Pts',(-7.21961961863,-35.364857528,2.20953864245));
#54138=CARTESIAN_POINT('Ctrl Pts',(-7.218980814,-35.3982226387,2.20220709377));
#54139=CARTESIAN_POINT('Ctrl Pts',(-7.21705230964,-35.4316688958,2.19555083028));
#54140=CARTESIAN_POINT('Ctrl Pts',(-7.21384189759,-35.4651151528,2.18958432614));
#54141=CARTESIAN_POINT('Ctrl Pts',(-7.18673962782,-35.3208994409,2.15657660598));
#54142=CARTESIAN_POINT('Ctrl Pts',(-7.18679863605,-35.3444227249,2.15079574742));
#54143=CARTESIAN_POINT('Ctrl Pts',(-7.18629633971,-35.3679639778,2.14519357364));
#54144=CARTESIAN_POINT('Ctrl Pts',(-7.18523498451,-35.3915169062,2.13977082956));
#54145=CARTESIAN_POINT('Ctrl Pts',(-7.18361579364,-35.4150756718,2.13452906411));
#54146=CARTESIAN_POINT('Ctrl Pts',(-7.18143896677,-35.4386344375,2.12947072768));
#54147=CARTESIAN_POINT('Ctrl Pts',(-7.16019775778,-35.3488473737,2.08142068745));
#54148=CARTESIAN_POINT('Ctrl Pts',(-7.15961328066171,-35.3598678430844,
2.07926829342153));
#54149=CARTESIAN_POINT('Ctrl Pts',(-7.15902631490073,-35.370880846883,2.07710680880288));
#54150=CARTESIAN_POINT('Ctrl Pts',(-7.15843669056073,-35.3818889651522,
2.07493560863704));
#54151=CARTESIAN_POINT('Ctrl Pts',(-7.15784419952897,-35.3928946462221,
2.07275392853839));
#54152=CARTESIAN_POINT('Ctrl Pts',(-7.15724858875,-35.4039003382,2.07056083977));
#54153=CARTESIAN_POINT('Ctrl Pts',(-7.13973478936,-35.3742392475,2.00655473738));
#54154=CARTESIAN_POINT('Ctrl Pts',(-7.13973478936,-35.3742392475,2.00655473738));
#54155=CARTESIAN_POINT('Ctrl Pts',(-7.13973478936,-35.3742392475,2.00655473738));
#54156=CARTESIAN_POINT('Ctrl Pts',(-7.13973478936,-35.3742392475,2.00655473738));
#54157=CARTESIAN_POINT('Ctrl Pts',(-7.13973478936,-35.3742392475,2.00655473738));
#54158=CARTESIAN_POINT('Ctrl Pts',(-7.13973478936,-35.3742392475,2.00655473738));
#54159=CARTESIAN_POINT('Origin',(-6.33322471801445,-35.4651138830689,2.6634130643161));
#54160=CARTESIAN_POINT('Ctrl Pts',(-7.23545146011,-35.2863120169,2.26690923839));
#54161=CARTESIAN_POINT('Ctrl Pts',(-7.2384543,-35.3245396537,2.25650943661));
#54162=CARTESIAN_POINT('Ctrl Pts',(-7.23974953205,-35.3631494767,2.24702142178));
#54163=CARTESIAN_POINT('Ctrl Pts',(-7.23932727374,-35.4020157716,2.23847939875));
#54164=CARTESIAN_POINT('Ctrl Pts',(-7.23718891826,-35.4410103045,2.23091155076));
#54165=CARTESIAN_POINT('Ctrl Pts',(-7.23334710717,-35.4800048374,2.2243394865));
#54166=CARTESIAN_POINT('Ctrl Pts',(-7.23162479878,-35.288610995,2.25877896783));
#54167=CARTESIAN_POINT('Ctrl Pts',(-7.23442685161,-35.3258445567,2.2487681051));
#54168=CARTESIAN_POINT('Ctrl Pts',(-7.23560643854,-35.3634294381,2.2396106895));
#54169=CARTESIAN_POINT('Ctrl Pts',(-7.2351548746,-35.4012499853,2.23133779585));
#54170=CARTESIAN_POINT('Ctrl Pts',(-7.2330735745,-35.4391883682,2.22397519179));
#54171=CARTESIAN_POINT('Ctrl Pts',(-7.22937402512,-35.477126751,2.21754286118));
#54172=CARTESIAN_POINT('Ctrl Pts',(-7.22786970762,-35.291024056,2.2506285999));
#54173=CARTESIAN_POINT('Ctrl Pts',(-7.23046153941,-35.32723074,2.24098939513));
#54174=CARTESIAN_POINT('Ctrl Pts',(-7.23151609908,-35.3637591309,2.23214656382));
#54175=CARTESIAN_POINT('Ctrl Pts',(-7.23102584019,-35.4005032431,2.22412829997));
#54176=CARTESIAN_POINT('Ctrl Pts',(-7.22899220964,-35.437355218,2.21695813089));
#54177=CARTESIAN_POINT('Ctrl Pts',(-7.22542564343,-35.4742071929,2.21065452768));
#54178=CARTESIAN_POINT('Ctrl Pts',(-7.22418450574,-35.2935251725,2.24246594859));
#54179=CARTESIAN_POINT('Ctrl Pts',(-7.22656046023,-35.328675405,2.23318153594));
#54180=CARTESIAN_POINT('Ctrl Pts',(-7.22748386956,-35.3641192075,2.22463810729));
#54181=CARTESIAN_POINT('Ctrl Pts',(-7.22694822371,-35.3997598036,2.21686121842));
#54182=CARTESIAN_POINT('Ctrl Pts',(-7.22495501199,-35.4354987894,2.20987233634));
#54183=CARTESIAN_POINT('Ctrl Pts',(-7.22151371785,-35.4712377752,2.20368850558));
#54184=CARTESIAN_POINT('Ctrl Pts',(-7.22057030307,-35.2960900286,2.23430349206));
#54185=CARTESIAN_POINT('Ctrl Pts',(-7.22272782881,-35.3301573964,2.22535702652));
#54186=CARTESIAN_POINT('Ctrl Pts',(-7.22351653394,-35.364491827,2.21709818648));
#54187=CARTESIAN_POINT('Ctrl Pts',(-7.22293085753,-35.3990052196,2.20955010655));
#54188=CARTESIAN_POINT('Ctrl Pts',(-7.22097232999,-35.4336080936,2.20273236154));
#54189=CARTESIAN_POINT('Ctrl Pts',(-7.21764954964,-35.4682109676,2.19666066586));
#54190=CARTESIAN_POINT('Ctrl Pts',(-7.21702826363,-35.2986939836,2.22615331206));
#54191=CARTESIAN_POINT('Ctrl Pts',(-7.21896725362,-35.3316545144,2.21752775213));
#54192=CARTESIAN_POINT('Ctrl Pts',(-7.21961969567,-35.3648573041,2.20953871906));
#54193=CARTESIAN_POINT('Ctrl Pts',(-7.21898088241,-35.3982223851,2.20220714146));
#54194=CARTESIAN_POINT('Ctrl Pts',(-7.21705236747,-35.4316686126,2.19555084997));
#54195=CARTESIAN_POINT('Ctrl Pts',(-7.2138419429,-35.46511484,2.18958431883));
#54196=CARTESIAN_POINT('Origin',(-6.37002476138651,-35.4800021287416,2.72899290183013));
#54197=CARTESIAN_POINT('Ctrl Pts',(-8.60091079918,-35.1203221982,2.60032832802));
#54198=CARTESIAN_POINT('Ctrl Pts',(-8.55250196755,-35.2208633974,2.5457337616));
#54199=CARTESIAN_POINT('Ctrl Pts',(-8.51670667214,-35.3325773527,2.50053052804));
#54200=CARTESIAN_POINT('Ctrl Pts',(-8.49508712358,-35.4522342996,2.46647854203));
#54201=CARTESIAN_POINT('Ctrl Pts',(-8.48835988758,-35.5758682873,2.44470643423));
#54202=CARTESIAN_POINT('Ctrl Pts',(-8.49626487495,-35.6995022751,2.43550520334));
#54203=CARTESIAN_POINT('Ctrl Pts',(-8.56160117875,-35.1140346808,2.66060541831));
#54204=CARTESIAN_POINT('Ctrl Pts',(-8.51158038352,-35.2164638336,2.60178050099));
#54205=CARTESIAN_POINT('Ctrl Pts',(-8.47440952478,-35.3311106273,2.55334779448));
#54206=CARTESIAN_POINT('Ctrl Pts',(-8.45180416694,-35.454476252,2.51731779839));
#54207=CARTESIAN_POINT('Ctrl Pts',(-8.44456120074,-35.5822080931,2.49495976327));
#54208=CARTESIAN_POINT('Ctrl Pts',(-8.45240512852,-35.7099399342,2.48655698047));
#54209=CARTESIAN_POINT('Ctrl Pts',(-8.51829161967,-35.1086508497,2.71924356476));
#54210=CARTESIAN_POINT('Ctrl Pts',(-8.4676782837,-35.2126508331,2.65547482048));
#54211=CARTESIAN_POINT('Ctrl Pts',(-8.42997337302,-35.3299187074,2.6031885652));
#54212=CARTESIAN_POINT('Ctrl Pts',(-8.40701812301,-35.4566921944,2.56468900549));
#54213=CARTESIAN_POINT('Ctrl Pts',(-8.39967272263,-35.5882267707,2.5414121675));
#54214=CARTESIAN_POINT('Ctrl Pts',(-8.40764108873,-35.7197613468,2.53363446576));
#54215=CARTESIAN_POINT('Ctrl Pts',(-8.47165311425,-35.1035435988,2.77475885702));
#54216=CARTESIAN_POINT('Ctrl Pts',(-8.42103112523,-35.2090000749,2.7055559059));
#54217=CARTESIAN_POINT('Ctrl Pts',(-8.38318247508,-35.3288584812,2.64914965253));
#54218=CARTESIAN_POINT('Ctrl Pts',(-8.36006509714,-35.4590804193,2.60819117966));
#54219=CARTESIAN_POINT('Ctrl Pts',(-8.35259991719,-35.5944943118,2.58430328363));
#54220=CARTESIAN_POINT('Ctrl Pts',(-8.36047222003,-35.7299082045,2.5777319381));
#54221=CARTESIAN_POINT('Ctrl Pts',(-8.35159188251,-35.0922845623,2.89275323394));
#54222=CARTESIAN_POINT('Ctrl Pts',(-8.3050322624,-35.2005432762,2.80975608337));
#54223=CARTESIAN_POINT('Ctrl Pts',(-8.26959869952,-35.3257180408,2.7430273545));
#54224=CARTESIAN_POINT('Ctrl Pts',(-8.2473160419,-35.4631716043,2.69610840641));
#54225=CARTESIAN_POINT('Ctrl Pts',(-8.23918506507,-35.6067794199,2.67107903223));
#54226=CARTESIAN_POINT('Ctrl Pts',(-8.24494252704,-35.7503872354,2.66806485365));
#54227=CARTESIAN_POINT('Ctrl Pts',(-8.20219946581,-35.0869079403,2.96964215712));
#54228=CARTESIAN_POINT('Ctrl Pts',(-8.17044511261,-35.196070615,2.87494321335));
#54229=CARTESIAN_POINT('Ctrl Pts',(-8.14524485361,-35.3234854768,2.79971065515));
#54230=CARTESIAN_POINT('Ctrl Pts',(-8.12806473503,-35.4642227883,2.74824760952));
#54231=CARTESIAN_POINT('Ctrl Pts',(-8.11972374517,-35.6116396625,2.72298240153));
#54232=CARTESIAN_POINT('Ctrl Pts',(-8.12018530542,-35.7590565367,2.723855906));
#54233=CARTESIAN_POINT('Ctrl Pts',(-8.10597427981,-35.0887550559,2.98941073315));
#54234=CARTESIAN_POINT('Ctrl Pts',(-8.08828816032,-35.1976252196,2.89277147723));
#54235=CARTESIAN_POINT('Ctrl Pts',(-8.07262669454,-35.3241767484,2.81647388405));
#54236=CARTESIAN_POINT('Ctrl Pts',(-8.05970660483,-35.4635970156,2.76481016119));
#54237=CARTESIAN_POINT('Ctrl Pts',(-8.05010223161,-35.6094680649,2.74015988873));
#54238=CARTESIAN_POINT('Ctrl Pts',(-8.0441099093,-35.7553391142,2.74240669266));
#54239=CARTESIAN_POINT('Ctrl Pts',(-7.82075728158,-35.1140008873,2.95981413055));
#54240=CARTESIAN_POINT('Ctrl Pts',(-7.83753302833,-35.2174511648,2.88177682176));
#54241=CARTESIAN_POINT('Ctrl Pts',(-7.84624727736,-35.3324220766,2.81978760483));
#54242=CARTESIAN_POINT('Ctrl Pts',(-7.84611816579,-35.4555224941,2.77624706117));
#54243=CARTESIAN_POINT('Ctrl Pts',(-7.83704746541,-35.5826911821,2.75255272839));
#54244=CARTESIAN_POINT('Ctrl Pts',(-7.81966214074,-35.7098598702,2.74888110871));
#54245=CARTESIAN_POINT('Ctrl Pts',(-7.56538653659,-35.1573736159,2.76989788484));
#54246=CARTESIAN_POINT('Ctrl Pts',(-7.58792144694,-35.2456787757,2.72783328434));
#54247=CARTESIAN_POINT('Ctrl Pts',(-7.60265321273,-35.3389337113,2.69350582125));
#54248=CARTESIAN_POINT('Ctrl Pts',(-7.60913119693,-35.4355529064,2.66745188002));
#54249=CARTESIAN_POINT('Ctrl Pts',(-7.60718914349,-35.5338539365,2.65003275892));
#54250=CARTESIAN_POINT('Ctrl Pts',(-7.59696106493,-35.6321549665,2.64143245401));
#54251=CARTESIAN_POINT('Ctrl Pts',(-7.43180190579,-35.1865123729,2.62065670169));
#54252=CARTESIAN_POINT('Ctrl Pts',(-7.44817986306,-35.2646063876,2.59073345827));
#54253=CARTESIAN_POINT('Ctrl Pts',(-7.45830517498,-35.3457624596,2.56600593478));
#54254=CARTESIAN_POINT('Ctrl Pts',(-7.46204607379,-35.4290060284,2.5468488602));
#54255=CARTESIAN_POINT('Ctrl Pts',(-7.45940380717,-35.5132946093,2.53351481199));
#54256=CARTESIAN_POINT('Ctrl Pts',(-7.45050807009,-35.5975831903,2.52611015512));
#54257=CARTESIAN_POINT('Ctrl Pts',(-7.32065041948,-35.231204862,2.4495725015));
#54258=CARTESIAN_POINT('Ctrl Pts',(-7.32870713782,-35.2926200315,2.43080253154));
#54259=CARTESIAN_POINT('Ctrl Pts',(-7.33308472128,-35.3551340146,2.41429805269));
#54260=CARTESIAN_POINT('Ctrl Pts',(-7.33374284515,-35.4183882264,2.40016471574));
#54261=CARTESIAN_POINT('Ctrl Pts',(-7.33068095224,-35.4820120082,2.3884845177));
#54262=CARTESIAN_POINT('Ctrl Pts',(-7.3239386903,-35.5456357901,2.37931366962));
#54263=CARTESIAN_POINT('Ctrl Pts',(-7.23545016815,-35.2863172732,2.26690461593));
#54264=CARTESIAN_POINT('Ctrl Pts',(-7.23845227406,-35.3245433701,2.25650461508));
#54265=CARTESIAN_POINT('Ctrl Pts',(-7.23974688842,-35.3631516089,2.24701631825));
#54266=CARTESIAN_POINT('Ctrl Pts',(-7.23932413184,-35.4020162898,2.23847392839));
#54267=CARTESIAN_POINT('Ctrl Pts',(-7.23718539906,-35.4410091937,2.23090562784));
#54268=CARTESIAN_POINT('Ctrl Pts',(-7.23334333153,-35.4800020975,2.22433302544));
#54269=CARTESIAN_POINT('Origin',(-9.25479694586426,-35.6995103355176,3.08717878194488));
#54270=CARTESIAN_POINT('Ctrl Pts',(-8.82321783753,-35.1473399652,2.21902634713));
#54271=CARTESIAN_POINT('Ctrl Pts',(-8.78215068074,-35.2382758927,2.18429700681));
#54272=CARTESIAN_POINT('Ctrl Pts',(-8.75159630524,-35.3362200688,2.15548691366));
#54273=CARTESIAN_POINT('Ctrl Pts',(-8.73251216058,-35.4390587483,2.13340513227));
#54274=CARTESIAN_POINT('Ctrl Pts',(-8.72535205902,-35.5443464741,2.11857675734));
#54275=CARTESIAN_POINT('Ctrl Pts',(-8.73000528472,-35.6496341999,2.11117245845));
#54276=CARTESIAN_POINT('Ctrl Pts',(-8.7950132494,-35.1439026605,2.27318832802));
#54277=CARTESIAN_POINT('Ctrl Pts',(-8.75278762749,-35.2361296908,2.23654747651));
#54278=CARTESIAN_POINT('Ctrl Pts',(-8.72137526051,-35.3357860213,2.20615712169));
#54279=CARTESIAN_POINT('Ctrl Pts',(-8.70180041036,-35.4406403454,2.18290446914));
#54280=CARTESIAN_POINT('Ctrl Pts',(-8.69454777529,-35.548095721,2.16736469093));
#54281=CARTESIAN_POINT('Ctrl Pts',(-8.69949502688,-35.6555510966,2.15972094562));
#54282=CARTESIAN_POINT('Ctrl Pts',(-8.76584958693,-35.140386513,2.32745356943));
#54283=CARTESIAN_POINT('Ctrl Pts',(-8.72246681666,-35.2339199765,2.28869203429));
#54284=CARTESIAN_POINT('Ctrl Pts',(-8.69020329348,-35.3353435452,2.25654623894));
#54285=CARTESIAN_POINT('Ctrl Pts',(-8.67015581074,-35.4422984936,2.23199348318));
#54286=CARTESIAN_POINT('Ctrl Pts',(-8.66284221447,-35.5520214947,2.21566670729));
#54287=CARTESIAN_POINT('Ctrl Pts',(-8.66812648429,-35.6617444959,2.20776307897));
#54288=CARTESIAN_POINT('Ctrl Pts',(-8.7356657971,-35.1367480171,2.38172554964));
#54289=CARTESIAN_POINT('Ctrl Pts',(-8.69113780582,-35.2316121539,2.34057114953));
#54290=CARTESIAN_POINT('Ctrl Pts',(-8.65803763705,-35.3348781572,2.30644499517));
#54291=CARTESIAN_POINT('Ctrl Pts',(-8.63754180367,-35.4440469154,2.28042962134));
#54292=CARTESIAN_POINT('Ctrl Pts',(-8.63020353714,-35.5561701517,2.26322602866));
#54293=CARTESIAN_POINT('Ctrl Pts',(-8.63587110442,-35.668293388,2.25504712403));
#54294=CARTESIAN_POINT('Ctrl Pts',(-8.69114735744,-35.1314764865,2.45847308227));
#54295=CARTESIAN_POINT('Ctrl Pts',(-8.64510845073,-35.2282535188,2.41340322951));
#54296=CARTESIAN_POINT('Ctrl Pts',(-8.61094346222,-35.3342411346,2.37601936382));
#54297=CARTESIAN_POINT('Ctrl Pts',(-8.58994905716,-35.4467225347,2.34758564448));
#54298=CARTESIAN_POINT('Ctrl Pts',(-8.58273119234,-35.5624541016,2.32891916373));
#54299=CARTESIAN_POINT('Ctrl Pts',(-8.58910725848,-35.6781856686,2.32025995821));
#54300=CARTESIAN_POINT('Ctrl Pts',(-8.64411242258,-35.1256902423,2.53413655954));
#54301=CARTESIAN_POINT('Ctrl Pts',(-8.59671994041,-35.2244531785,2.48429647903));
#54302=CARTESIAN_POINT('Ctrl Pts',(-8.56161211733,-35.333412859,2.44298795985));
#54303=CARTESIAN_POINT('Ctrl Pts',(-8.54022333506,-35.4495924912,2.41171677405));
#54304=CARTESIAN_POINT('Ctrl Pts',(-8.53321738738,-35.5693865938,2.39145291764));
#54305=CARTESIAN_POINT('Ctrl Pts',(-8.54037362589,-35.6891806965,2.38246370607));
#54306=CARTESIAN_POINT('Ctrl Pts',(-8.62993676763,-35.1239763388,2.55637951988));
#54307=CARTESIAN_POINT('Ctrl Pts',(-8.58219189761,-35.2233231665,2.50503392418));
#54308=CARTESIAN_POINT('Ctrl Pts',(-8.54685013234,-35.3331714269,2.46248222847));
#54309=CARTESIAN_POINT('Ctrl Pts',(-8.52538633662,-35.4504650834,2.43030855578));
#54310=CARTESIAN_POINT('Ctrl Pts',(-8.51848133158,-35.5714859455,2.4095318701));
#54311=CARTESIAN_POINT('Ctrl Pts',(-8.52590127043,-35.6925068075,2.40042817508));
#54312=CARTESIAN_POINT('Ctrl Pts',(-8.61560772534,-35.1221440943,2.57842131078));
#54313=CARTESIAN_POINT('Ctrl Pts',(-8.56749228928,-35.2220926432,2.52550930797));
#54314=CARTESIAN_POINT('Ctrl Pts',(-8.53188890827,-35.3328708509,2.48168265536));
#54315=CARTESIAN_POINT('Ctrl Pts',(-8.5103168202,-35.4513369446,2.44860878814));
#54316=CARTESIAN_POINT('Ctrl Pts',(-8.50347493534,-35.5736522798,2.42735915225));
#54317=CARTESIAN_POINT('Ctrl Pts',(-8.51111753906,-35.695967615,2.41821700034));
#54318=CARTESIAN_POINT('Ctrl Pts',(-8.60091081429,-35.1203221009,2.60032838611));
#54319=CARTESIAN_POINT('Ctrl Pts',(-8.55250194661,-35.2208633123,2.54573382886));
#54320=CARTESIAN_POINT('Ctrl Pts',(-8.51670661225,-35.3325772847,2.50053061213));
#54321=CARTESIAN_POINT('Ctrl Pts',(-8.49508702343,-35.4522342523,2.46647865078));
#54322=CARTESIAN_POINT('Ctrl Pts',(-8.4883597474,-35.5758682626,2.44470657499));
#54323=CARTESIAN_POINT('Ctrl Pts',(-8.49626469614,-35.699502273,2.4355053823));
#54324=CARTESIAN_POINT('Origin',(-9.57674350374405,-35.6496306966926,2.64320593658555));
#54325=CARTESIAN_POINT('Ctrl Pts',(-8.84972761074,-35.1509187546,2.16704276679));
#54326=CARTESIAN_POINT('Ctrl Pts',(-8.80995141052,-35.2405485577,2.13393459289));
#54327=CARTESIAN_POINT('Ctrl Pts',(-8.78039709025,-35.3367789605,2.10641485522));
#54328=CARTESIAN_POINT('Ctrl Pts',(-8.7619545083,-35.4376105338,2.08522367244));
#54329=CARTESIAN_POINT('Ctrl Pts',(-8.75504416849,-35.5407442468,2.0708442184));
#54330=CARTESIAN_POINT('Ctrl Pts',(-8.75956299023,-35.6438779598,2.0634404101));
#54331=CARTESIAN_POINT('Ctrl Pts',(-8.84456885861,-35.1501669799,2.17736664036));
#54332=CARTESIAN_POINT('Ctrl Pts',(-8.80450316343,-35.2400691335,2.14397755154));
#54333=CARTESIAN_POINT('Ctrl Pts',(-8.77471769299,-35.3366533562,2.11624485706));
#54334=CARTESIAN_POINT('Ctrl Pts',(-8.75611631291,-35.437897274,2.0949212219));
#54335=CARTESIAN_POINT('Ctrl Pts',(-8.74912677261,-35.5414726393,2.08049700356));
#54336=CARTESIAN_POINT('Ctrl Pts',(-8.75364509765,-35.6450480046,2.07313650893));
#54337=CARTESIAN_POINT('Ctrl Pts',(-8.83934134903,-35.1494257084,2.1877279664));
#54338=CARTESIAN_POINT('Ctrl Pts',(-8.79900028815,-35.2395949404,2.15403728116));
#54339=CARTESIAN_POINT('Ctrl Pts',(-8.76899769743,-35.3365278505,2.12607022447));
#54340=CARTESIAN_POINT('Ctrl Pts',(-8.75025126803,-35.4381791278,2.10459258862));
#54341=CARTESIAN_POINT('Ctrl Pts',(-8.74319574656,-35.5421912387,2.09010248095));
#54342=CARTESIAN_POINT('Ctrl Pts',(-8.74772599292,-35.6462033496,2.08276502103));
#54343=CARTESIAN_POINT('Ctrl Pts',(-8.83403961773,-35.1487041475,2.19812825065));
#54344=CARTESIAN_POINT('Ctrl Pts',(-8.79343976066,-35.2391345884,2.16411346789));
#54345=CARTESIAN_POINT('Ctrl Pts',(-8.76323651939,-35.3364102747,2.1358885387));
#54346=CARTESIAN_POINT('Ctrl Pts',(-8.74436113276,-35.4384630225,2.11423302609));
#54347=CARTESIAN_POINT('Ctrl Pts',(-8.73725504684,-35.5429059973,2.0996533862));
#54348=CARTESIAN_POINT('Ctrl Pts',(-8.74181161845,-35.6473489721,2.09231606717));
#54349=CARTESIAN_POINT('Ctrl Pts',(-8.82866432718,-35.1480081194,2.20856250217));
#54350=CARTESIAN_POINT('Ctrl Pts',(-8.78782272692,-35.2386939519,2.17420118315));
#54351=CARTESIAN_POINT('Ctrl Pts',(-8.75743582295,-35.3363065177,2.14569487681));
#54352=CARTESIAN_POINT('Ctrl Pts',(-8.73844810187,-35.4387548314,2.12383756828));
#54353=CARTESIAN_POINT('Ctrl Pts',(-8.73130736324,-35.5436227636,2.10914471028));
#54354=CARTESIAN_POINT('Ctrl Pts',(-8.73590510583,-35.6484906957,2.1017846051));
#54355=CARTESIAN_POINT('Ctrl Pts',(-8.82321744436,-35.1473421125,2.21902489656));
#54356=CARTESIAN_POINT('Ctrl Pts',(-8.78215104537,-35.2382777414,2.18429511356));
#54357=CARTESIAN_POINT('Ctrl Pts',(-8.75159740651,-35.3362215383,2.15548447298));
#54358=CARTESIAN_POINT('Ctrl Pts',(-8.73251395256,-35.4390597803,2.13340204369));
#54359=CARTESIAN_POINT('Ctrl Pts',(-8.72535447592,-35.5443470397,2.11857293178));
#54360=CARTESIAN_POINT('Ctrl Pts',(-8.73000824887,-35.6496342991,2.1111678244));
#54361=CARTESIAN_POINT('Origin',(-9.61320752990433,-35.6438714700362,2.58431858586112));
#54362=CARTESIAN_POINT('Ctrl Pts',(-8.84973117353,-35.1509193731,2.1670354781));
#54363=CARTESIAN_POINT('Ctrl Pts',(-8.80995437067,-35.2405490067,2.13392896451));
#54364=CARTESIAN_POINT('Ctrl Pts',(-8.78039938016,-35.3367791654,2.10641082417));
#54365=CARTESIAN_POINT('Ctrl Pts',(-8.76195606614,-35.4376104406,2.08522113231));
#54366=CARTESIAN_POINT('Ctrl Pts',(-8.75504494547,-35.5407438285,2.07084302459));
#54367=CARTESIAN_POINT('Ctrl Pts',(-8.75956295656,-35.6438772164,2.06344039042));
#54368=CARTESIAN_POINT('Ctrl Pts',(-8.91091202313,-35.1598372898,2.04459467569));
#54369=CARTESIAN_POINT('Ctrl Pts',(-8.87455647002,-35.246237181,2.01484191076));
#54370=CARTESIAN_POINT('Ctrl Pts',(-8.84773035639,-35.3382711138,1.98987130618));
#54371=CARTESIAN_POINT('Ctrl Pts',(-8.83115765576,-35.4342118768,1.97027362582));
#54372=CARTESIAN_POINT('Ctrl Pts',(-8.82517322934,-35.532107067,1.95644630565));
#54373=CARTESIAN_POINT('Ctrl Pts',(-8.82968488575,-35.6300022572,1.94854820039));
#54374=CARTESIAN_POINT('Ctrl Pts',(-8.96795816735,-35.1710296589,1.91634945111));
#54375=CARTESIAN_POINT('Ctrl Pts',(-8.93494048323,-35.2532459987,1.89161496085));
#54376=CARTESIAN_POINT('Ctrl Pts',(-8.91060835461,-35.3400086156,1.87063336475));
#54377=CARTESIAN_POINT('Ctrl Pts',(-8.89552405555,-35.4299031373,1.85381398232));
#54378=CARTESIAN_POINT('Ctrl Pts',(-8.88994864311,-35.5213641494,1.84144178963));
#54379=CARTESIAN_POINT('Ctrl Pts',(-8.89381707546,-35.6128251616,1.83365112687));
#54380=CARTESIAN_POINT('Ctrl Pts',(-9.01653709076,-35.1835781664,1.78332507658));
#54381=CARTESIAN_POINT('Ctrl Pts',(-8.98711360766,-35.260897748,1.76325201128));
#54382=CARTESIAN_POINT('Ctrl Pts',(-8.96538998881,-35.341846639,1.74604152846));
#54383=CARTESIAN_POINT('Ctrl Pts',(-8.95179602076,-35.4252853121,1.73198094156));
#54384=CARTESIAN_POINT('Ctrl Pts',(-8.94653331601,-35.5099692034,1.72127486801));
#54385=CARTESIAN_POINT('Ctrl Pts',(-8.9495584777,-35.5946530947,1.71402843838));
#54386=CARTESIAN_POINT('Ctrl Pts',(-9.1140028877,-35.2108461818,1.46157810716));
#54387=CARTESIAN_POINT('Ctrl Pts',(-9.09197113076,-35.2771127336,1.45066936239));
#54388=CARTESIAN_POINT('Ctrl Pts',(-9.07556758896,-35.3453927996,1.44108450365));
#54389=CARTESIAN_POINT('Ctrl Pts',(-9.06500040952,-35.4150382685,1.43291495679));
#54390=CARTESIAN_POINT('Ctrl Pts',(-9.06037122564,-35.4853665076,1.42623124853));
#54391=CARTESIAN_POINT('Ctrl Pts',(-9.06167021042,-35.5556947466,1.4210802448));
#54392=CARTESIAN_POINT('Ctrl Pts',(-9.17852891179,-35.2281865303,1.13254165139));
#54393=CARTESIAN_POINT('Ctrl Pts',(-9.16069403398,-35.2869558429,1.12639249526));
#54394=CARTESIAN_POINT('Ctrl Pts',(-9.14729128577,-35.3471459486,1.12104732689));
#54395=CARTESIAN_POINT('Ctrl Pts',(-9.13845933491,-35.4082985485,1.1165532711));
#54396=CARTESIAN_POINT('Ctrl Pts',(-9.13426752236,-35.4699324162,1.11294417189));
#54397=CARTESIAN_POINT('Ctrl Pts',(-9.13471251897,-35.531566284,1.1102388653));
#54398=CARTESIAN_POINT('Ctrl Pts',(-9.20897519651,-35.2324135956,0.943972367435));
#54399=CARTESIAN_POINT('Ctrl Pts',(-9.19209813045,-35.2892087111,0.939475719579));
#54400=CARTESIAN_POINT('Ctrl Pts',(-9.17938477515,-35.3472963111,0.935686471687));
#54401=CARTESIAN_POINT('Ctrl Pts',(-9.1709591607,-35.4062580486,0.93263706468));
#54402=CARTESIAN_POINT('Ctrl Pts',(-9.16688368582,-35.4656570006,0.930349922162));
#54403=CARTESIAN_POINT('Ctrl Pts',(-9.1671566108,-35.5250559527,0.928836133483));
#54404=CARTESIAN_POINT('Ctrl Pts',(-9.23916608575,-35.2348774759,0.761379139513));
#54405=CARTESIAN_POINT('Ctrl Pts',(-9.22290027765,-35.2906450094,0.757499573794));
#54406=CARTESIAN_POINT('Ctrl Pts',(-9.21063507987,-35.3476242625,0.754282164424));
#54407=CARTESIAN_POINT('Ctrl Pts',(-9.20248495391,-35.4054228352,0.75175437252));
#54408=CARTESIAN_POINT('Ctrl Pts',(-9.19850755669,-35.4636310173,0.749934120027));
#54409=CARTESIAN_POINT('Ctrl Pts',(-9.19870123297,-35.5218391995,0.748829315604));
#54410=CARTESIAN_POINT('Ctrl Pts',(-9.26569123725,-35.2394333704,0.579580156823));
#54411=CARTESIAN_POINT('Ctrl Pts',(-9.25048972376,-35.2934591001,0.575764245003));
#54412=CARTESIAN_POINT('Ctrl Pts',(-9.23904456924,-35.3485824305,0.57252390595));
#54413=CARTESIAN_POINT('Ctrl Pts',(-9.2314560575,-35.4044472049,0.569884306758));
#54414=CARTESIAN_POINT('Ctrl Pts',(-9.22777454338,-35.4606827234,0.567862962924));
#54415=CARTESIAN_POINT('Ctrl Pts',(-9.22799848318,-35.5169182418,0.566469053265));
#54416=CARTESIAN_POINT('Origin',(-10.2153564537533,-35.5169155168785,0.724979907680837));
#54417=CARTESIAN_POINT('Ctrl Pts',(-9.26569107955,-35.2394341184,0.579579770152));
#54418=CARTESIAN_POINT('Ctrl Pts',(-9.25048970237,-35.2934597015,0.575763550708));
#54419=CARTESIAN_POINT('Ctrl Pts',(-9.23904466522,-35.3485828761,0.57252289393));
#54420=CARTESIAN_POINT('Ctrl Pts',(-9.23145625045,-35.4044474883,0.569882968796));
#54421=CARTESIAN_POINT('Ctrl Pts',(-9.22777481195,-35.4606828414,0.567861292872));
#54422=CARTESIAN_POINT('Ctrl Pts',(-9.22799880569,-35.5169181946,0.566467047136));
#54423=CARTESIAN_POINT('Ctrl Pts',(-9.26734254057,-35.2397154298,0.568265288566));
#54424=CARTESIAN_POINT('Ctrl Pts',(-9.25220700276,-35.2936330337,0.564453943744));
#54425=CARTESIAN_POINT('Ctrl Pts',(-9.24081265384,-35.3486411511,0.561212799914));
#54426=CARTESIAN_POINT('Ctrl Pts',(-9.23325890658,-35.4043858824,0.558566884261));
#54427=CARTESIAN_POINT('Ctrl Pts',(-9.22959566517,-35.4604989426,0.556533678149));
#54428=CARTESIAN_POINT('Ctrl Pts',(-9.22982138229,-35.5166120028,0.55512243494));
#54429=CARTESIAN_POINT('Ctrl Pts',(-9.26898307793,-35.2399973473,0.556947742073));
#54430=CARTESIAN_POINT('Ctrl Pts',(-9.25391368938,-35.2938057049,0.55314265644));
#54431=CARTESIAN_POINT('Ctrl Pts',(-9.24257020144,-35.3486974567,0.549902346095));
#54432=CARTESIAN_POINT('Ctrl Pts',(-9.23505116442,-35.4043209585,0.547251660046));
#54433=CARTESIAN_POINT('Ctrl Pts',(-9.23140601814,-35.4603103757,0.54520808798));
#54434=CARTESIAN_POINT('Ctrl Pts',(-9.23163322063,-35.516299793,0.543780919912));
#54435=CARTESIAN_POINT('Ctrl Pts',(-9.2706134925,-35.2402652369,0.545649357377));
#54436=CARTESIAN_POINT('Ctrl Pts',(-9.25560999309,-35.2939662109,0.541842800001));
#54437=CARTESIAN_POINT('Ctrl Pts',(-9.24431742891,-35.3487436319,0.53859575027));
#54438=CARTESIAN_POINT('Ctrl Pts',(-9.23683343793,-35.4042480754,0.535933346844));
#54439=CARTESIAN_POINT('Ctrl Pts',(-9.23320713925,-35.460116063,0.533872309581));
#54440=CARTESIAN_POINT('Ctrl Pts',(-9.23343691736,-35.5159840505,0.532422414623));
#54441=CARTESIAN_POINT('Ctrl Pts',(-9.2722446143,-35.2405353461,0.534265835364));
#54442=CARTESIAN_POINT('Ctrl Pts',(-9.25730181761,-35.294127701,0.530496224362));
#54443=CARTESIAN_POINT('Ctrl Pts',(-9.24605472348,-35.3487894773,0.527280786202));
#54444=CARTESIAN_POINT('Ctrl Pts',(-9.2386001998,-35.4041734976,0.524643949807));
#54445=CARTESIAN_POINT('Ctrl Pts',(-9.23498684878,-35.4599186602,0.522602910424));
#54446=CARTESIAN_POINT('Ctrl Pts',(-9.23521314025,-35.5156638228,0.521166956934));
#54447=CARTESIAN_POINT('Ctrl Pts',(-9.27386188355,-35.2408046483,0.522899878387));
#54448=CARTESIAN_POINT('Ctrl Pts',(-9.25898070438,-35.2942887003,0.519158423034));
#54449=CARTESIAN_POINT('Ctrl Pts',(-9.24778011027,-35.34883522,0.515965854318));
#54450=CARTESIAN_POINT('Ctrl Pts',(-9.24035614735,-35.4040992464,0.513346314134));
#54451=CARTESIAN_POINT('Ctrl Pts',(-9.23675700648,-35.4597220466,0.511316806589));
#54452=CARTESIAN_POINT('Ctrl Pts',(-9.23698117862,-35.5153448469,0.509886547139));
#54453=CARTESIAN_POINT('Origin',(-10.224921002496,-35.5153449894579,0.664731520865732));
#54454=CARTESIAN_POINT('Ctrl Pts',(-9.01911953995,-35.2680044421,-3.13244837682));
#54455=CARTESIAN_POINT('Ctrl Pts',(-9.01128290018,-35.3096899679,-3.12777753845));
#54456=CARTESIAN_POINT('Ctrl Pts',(-9.00550173203,-35.3518572367,-3.12395745117));
#54457=CARTESIAN_POINT('Ctrl Pts',(-9.00180577632,-35.3943481132,-3.12100583911));
#54458=CARTESIAN_POINT('Ctrl Pts',(-9.00020910686,-35.4370007968,-3.11893394172));
#54459=CARTESIAN_POINT('Ctrl Pts',(-9.00070981215,-35.4796534803,-3.1177462595));
#54460=CARTESIAN_POINT('Ctrl Pts',(-9.17544595344,-35.2835018925,-2.74597776201));
#54461=CARTESIAN_POINT('Ctrl Pts',(-9.16933554333,-35.3193494556,-2.74372235315));
#54462=CARTESIAN_POINT('Ctrl Pts',(-9.16476148349,-35.3554672008,-2.74189804713));
#54463=CARTESIAN_POINT('Ctrl Pts',(-9.1617381998,-35.3917657165,-2.74050818076));
#54464=CARTESIAN_POINT('Ctrl Pts',(-9.1602730438,-35.428154617,-2.73955472374));
#54465=CARTESIAN_POINT('Ctrl Pts',(-9.16036621938,-35.4645435174,-2.73903830807));
#54466=CARTESIAN_POINT('Ctrl Pts',(-9.29269126807,-35.2907452551,-2.34477529883));
#54467=CARTESIAN_POINT('Ctrl Pts',(-9.28707239127,-35.3238061129,-2.34352966982));
#54468=CARTESIAN_POINT('Ctrl Pts',(-9.282834933,-35.3571174391,-2.34257541991));
#54469=CARTESIAN_POINT('Ctrl Pts',(-9.27999356004,-35.3905967652,-2.34191674071));
#54470=CARTESIAN_POINT('Ctrl Pts',(-9.27855558309,-35.424160093,-2.3415559411));
#54471=CARTESIAN_POINT('Ctrl Pts',(-9.27852082014,-35.4577234207,-2.34149337034));
#54472=CARTESIAN_POINT('Ctrl Pts',(-9.36191429928,-35.2893802972,-1.92981468559));
#54473=CARTESIAN_POINT('Ctrl Pts',(-9.3560452611,-35.3232454878,-1.92921642136));
#54474=CARTESIAN_POINT('Ctrl Pts',(-9.35161541947,-35.3573586818,-1.92882344418));
#54475=CARTESIAN_POINT('Ctrl Pts',(-9.34863880943,-35.3916379824,-1.92863719423));
#54476=CARTESIAN_POINT('Ctrl Pts',(-9.3471225791,-35.4260003368,-1.92865812789));
#54477=CARTESIAN_POINT('Ctrl Pts',(-9.3470668903,-35.4603626911,-1.92888572013));
#54478=CARTESIAN_POINT('Ctrl Pts',(-9.4171903904,-35.2789856765,-1.18748239275));
#54479=CARTESIAN_POINT('Ctrl Pts',(-9.40981639515,-35.3169659165,-1.18801696878));
#54480=CARTESIAN_POINT('Ctrl Pts',(-9.40425718706,-35.3552891517,-1.18859518921));
#54481=CARTESIAN_POINT('Ctrl Pts',(-9.40053397643,-35.3938423214,-1.18921641071));
#54482=CARTESIAN_POINT('Ctrl Pts',(-9.39865750897,-35.4325104595,-1.18987939995));
#54483=CARTESIAN_POINT('Ctrl Pts',(-9.39862789646,-35.4711785976,-1.19058233503));
#54484=CARTESIAN_POINT('Ctrl Pts',(-9.38314539193,-35.2631816303,-0.439456405049));
#54485=CARTESIAN_POINT('Ctrl Pts',(-9.37293597078,-35.3077684071,-0.441248963721));
#54486=CARTESIAN_POINT('Ctrl Pts',(-9.36525594777,-35.3529358557,-0.442871125473));
#54487=CARTESIAN_POINT('Ctrl Pts',(-9.36014835673,-35.3984936385,-0.444315444411));
#54488=CARTESIAN_POINT('Ctrl Pts',(-9.35763482817,-35.4442465927,-0.44557584201));
#54489=CARTESIAN_POINT('Ctrl Pts',(-9.3577150604,-35.489999547,-0.446647757649));
#54490=CARTESIAN_POINT('Ctrl Pts',(-9.3558891039,-35.2557890156,-0.116721794816));
#54491=CARTESIAN_POINT('Ctrl Pts',(-9.34426128655,-35.3033050214,-0.118995176137));
#54492=CARTESIAN_POINT('Ctrl Pts',(-9.33551278911,-35.3515333802,-0.120988679218));
#54493=CARTESIAN_POINT('Ctrl Pts',(-9.3296998933,-35.4002411909,-0.122691582222));
#54494=CARTESIAN_POINT('Ctrl Pts',(-9.32685085926,-35.4491887348,-0.124095735733));
#54495=CARTESIAN_POINT('Ctrl Pts',(-9.32696513263,-35.4981362787,-0.12519578818));
#54496=CARTESIAN_POINT('Ctrl Pts',(-9.3192256268,-35.2483585547,0.204089324846));
#54497=CARTESIAN_POINT('Ctrl Pts',(-9.30607279618,-35.2988047548,0.201137625763));
#54498=CARTESIAN_POINT('Ctrl Pts',(-9.29617649939,-35.3501183672,0.198586534665));
#54499=CARTESIAN_POINT('Ctrl Pts',(-9.28960975953,-35.4020166188,0.196452114669));
#54500=CARTESIAN_POINT('Ctrl Pts',(-9.28640921473,-35.4542072015,0.194746107875));
#54501=CARTESIAN_POINT('Ctrl Pts',(-9.28657394094,-35.5063977842,0.193475565417));
#54502=CARTESIAN_POINT('Ctrl Pts',(-9.27386188307,-35.2408046524,0.522899877563));
#54503=CARTESIAN_POINT('Ctrl Pts',(-9.25898070398,-35.2942887044,0.519158422332));
#54504=CARTESIAN_POINT('Ctrl Pts',(-9.24778010992,-35.3488352241,0.515965853737));
#54505=CARTESIAN_POINT('Ctrl Pts',(-9.24035614705,-35.4040992505,0.513346313675));
#54506=CARTESIAN_POINT('Ctrl Pts',(-9.2367570062,-35.4597220507,0.511316806249));
#54507=CARTESIAN_POINT('Ctrl Pts',(-9.23698117834,-35.5153448509,0.509886546917));
#54508=CARTESIAN_POINT('Origin',(-9.92303703930928,-35.4797547933065,-3.50659112139201));
#54509=CARTESIAN_POINT('Ctrl Pts',(-8.93444595596,-35.2748053687,-3.31652394249));
#54510=CARTESIAN_POINT('Ctrl Pts',(-8.92616317166,-35.3147866052,-3.31461891577));
#54511=CARTESIAN_POINT('Ctrl Pts',(-8.91971750036,-35.3551912403,-3.31361234962));
#54512=CARTESIAN_POINT('Ctrl Pts',(-8.91513778092,-35.3958801128,-3.31351087925));
#54513=CARTESIAN_POINT('Ctrl Pts',(-8.91244000919,-35.4367111064,-3.31431485906));
#54514=CARTESIAN_POINT('Ctrl Pts',(-8.91162700591,-35.4775421,-3.31601835533));
#54515=CARTESIAN_POINT('Ctrl Pts',(-8.94734368663,-35.2728133782,-3.29109023634));
#54516=CARTESIAN_POINT('Ctrl Pts',(-8.93895107582,-35.3135017401,-3.28875572575));
#54517=CARTESIAN_POINT('Ctrl Pts',(-8.93246763725,-35.3546364096,-3.28733586636));
#54518=CARTESIAN_POINT('Ctrl Pts',(-8.9279236303,-35.3960707679,-3.28683902656));
#54519=CARTESIAN_POINT('Ctrl Pts',(-8.92533550226,-35.4376549725,-3.28726695529));
#54520=CARTESIAN_POINT('Ctrl Pts',(-8.92470553582,-35.4792391771,-3.28861474271));
#54521=CARTESIAN_POINT('Ctrl Pts',(-8.95983458954,-35.2711079221,-3.26569669172));
#54522=CARTESIAN_POINT('Ctrl Pts',(-8.95141175919,-35.3123562177,-3.2628807422));
#54523=CARTESIAN_POINT('Ctrl Pts',(-8.94495906105,-35.354070024,-3.26098724776));
#54524=CARTESIAN_POINT('Ctrl Pts',(-8.94050773142,-35.3960964758,-3.260026589));
#54525=CARTESIAN_POINT('Ctrl Pts',(-8.93807435022,-35.4382792543,-3.26000227455));
#54526=CARTESIAN_POINT('Ctrl Pts',(-8.93766047318,-35.4804620328,-3.26091086944));
#54527=CARTESIAN_POINT('Ctrl Pts',(-8.97214212604,-35.2697920542,-3.23978066277));
#54528=CARTESIAN_POINT('Ctrl Pts',(-8.9637190734,-35.311417995,-3.23656869462));
#54529=CARTESIAN_POINT('Ctrl Pts',(-8.95731138416,-35.3535230656,-3.23427864864));
#54530=CARTESIAN_POINT('Ctrl Pts',(-8.95295080025,-35.3959499382,-3.2329226531));
#54531=CARTESIAN_POINT('Ctrl Pts',(-8.95065387904,-35.4385377451,-3.23250578662));
#54532=CARTESIAN_POINT('Ctrl Pts',(-8.95042158697,-35.481125552,-3.23302610121));
#54533=CARTESIAN_POINT('Ctrl Pts',(-8.98911618271,-35.268630653,-3.20263013659));
#54534=CARTESIAN_POINT('Ctrl Pts',(-8.98077765617,-35.3105436223,-3.19892614932));
#54535=CARTESIAN_POINT('Ctrl Pts',(-8.97449392264,-35.3529460311,-3.19613159274));
#54536=CARTESIAN_POINT('Ctrl Pts',(-8.97029699893,-35.3956772608,-3.19426066196));
#54537=CARTESIAN_POINT('Ctrl Pts',(-8.96820302947,-35.4385728912,-3.19332056844));
#54538=CARTESIAN_POINT('Ctrl Pts',(-8.96821193143,-35.4814685217,-3.19331131722));
#54539=CARTESIAN_POINT('Ctrl Pts',(-9.00517206358,-35.2680735988,-3.16566118546));
#54540=CARTESIAN_POINT('Ctrl Pts',(-8.99706509175,-35.3099657558,-3.16142494219));
#54541=CARTESIAN_POINT('Ctrl Pts',(-8.99102314624,-35.3523468191,-3.15807110791));
#54542=CARTESIAN_POINT('Ctrl Pts',(-8.98707727301,-35.395056319,-3.15561591639));
#54543=CARTESIAN_POINT('Ctrl Pts',(-8.9852426452,-35.4379300459,-3.15406880151));
#54544=CARTESIAN_POINT('Ctrl Pts',(-8.98551821082,-35.4808037728,-3.15343220651));
#54545=CARTESIAN_POINT('Ctrl Pts',(-9.00990494748,-35.2680166859,-3.15455724964));
#54546=CARTESIAN_POINT('Ctrl Pts',(-9.00187362208,-35.3098646744,-3.1501873274));
#54547=CARTESIAN_POINT('Ctrl Pts',(-8.99590638677,-35.3522000159,-3.14669037035));
#54548=CARTESIAN_POINT('Ctrl Pts',(-8.99203402793,-35.3948627823,-3.14408308561));
#54549=CARTESIAN_POINT('Ctrl Pts',(-8.9902713955,-35.4376892422,-3.1423755103));
#54550=CARTESIAN_POINT('Ctrl Pts',(-8.9906170886,-35.480515702,-3.141570683));
#54551=CARTESIAN_POINT('Ctrl Pts',(-9.01453522232,-35.2679213672,-3.1435714055));
#54552=CARTESIAN_POINT('Ctrl Pts',(-9.00660223792,-35.3097130029,-3.13902110731));
#54553=CARTESIAN_POINT('Ctrl Pts',(-9.00073178209,-35.3519900952,-3.13533334259));
#54554=CARTESIAN_POINT('Ctrl Pts',(-8.99695406159,-35.3945932824,-3.13252547117));
#54555=CARTESIAN_POINT('Ctrl Pts',(-8.99528353801,-35.4373595352,-3.13060822223));
#54556=CARTESIAN_POINT('Ctrl Pts',(-8.99571858313,-35.480125788,-3.12958551692));
#54557=CARTESIAN_POINT('Ctrl Pts',(-9.01911869111,-35.2680072167,-3.13244884091));
#54558=CARTESIAN_POINT('Ctrl Pts',(-9.01128168784,-35.3096922673,-3.12777947274));
#54559=CARTESIAN_POINT('Ctrl Pts',(-9.00550009533,-35.3518590427,-3.12396085378));
#54560=CARTESIAN_POINT('Ctrl Pts',(-9.00180365501,-35.3943494134,-3.12101070215));
#54561=CARTESIAN_POINT('Ctrl Pts',(-9.00020644216,-35.4370015851,-3.1189402514));
#54562=CARTESIAN_POINT('Ctrl Pts',(-9.0007065476,-35.4796537567,-3.11775399652));
#54563=CARTESIAN_POINT('Origin',(-9.81411538991078,-35.4775422485357,-3.74673324846717));
#54564=CARTESIAN_POINT('Ctrl Pts',(-2.02882252548,-35.2583787857,-8.24404394735));
#54565=CARTESIAN_POINT('Ctrl Pts',(-2.02793435434,-35.304849438,-8.23266211897));
#54566=CARTESIAN_POINT('Ctrl Pts',(-2.0275994353,-35.3519981482,-8.22400554803));
#54567=CARTESIAN_POINT('Ctrl Pts',(-2.02782201048,-35.3996032301,-8.21812855721));
#54568=CARTESIAN_POINT('Ctrl Pts',(-2.02860101303,-35.4474365049,-8.21505931587));
#54569=CARTESIAN_POINT('Ctrl Pts',(-2.02993009745,-35.4952697797,-8.21479904026));
#54570=CARTESIAN_POINT('Ctrl Pts',(-2.7603704221,-35.2788135941,-8.09044877058));
#54571=CARTESIAN_POINT('Ctrl Pts',(-2.75916038902,-35.3170950643,-8.08332087145));
#54572=CARTESIAN_POINT('Ctrl Pts',(-2.75848926909,-35.3556762451,-8.07788965412));
#54573=CARTESIAN_POINT('Ctrl Pts',(-2.75836124945,-35.3944575182,-8.07416878882));
#54574=CARTESIAN_POINT('Ctrl Pts',(-2.75877734505,-35.4333388354,-8.07216551353));
#54575=CARTESIAN_POINT('Ctrl Pts',(-2.75973535856,-35.4722201525,-8.07188072536));
#54576=CARTESIAN_POINT('Ctrl Pts',(-3.46770746463,-35.2977417588,-7.8780751558));
#54577=CARTESIAN_POINT('Ctrl Pts',(-3.46660967304,-35.3282659767,-7.87385395784));
#54578=CARTESIAN_POINT('Ctrl Pts',(-3.46593509074,-35.3589261674,-7.87061653092));
#54579=CARTESIAN_POINT('Ctrl Pts',(-3.4656850911,-35.3896774143,-7.8683685806));
#54580=CARTESIAN_POINT('Ctrl Pts',(-3.46586006339,-35.420474191,-7.86711317222));
#54581=CARTESIAN_POINT('Ctrl Pts',(-3.46645942733,-35.4512709677,-7.86685062308));
#54582=CARTESIAN_POINT('Ctrl Pts',(-4.1448564034,-35.31305193,-7.60417987874));
#54583=CARTESIAN_POINT('Ctrl Pts',(-4.14387911843,-35.3375078051,-7.60136146782));
#54584=CARTESIAN_POINT('Ctrl Pts',(-4.14322007764,-35.3620512903,-7.59920530757));
#54585=CARTESIAN_POINT('Ctrl Pts',(-4.14288053918,-35.3866532884,-7.59771461525));
#54586=CARTESIAN_POINT('Ctrl Pts',(-4.14286096901,-35.4112845426,-7.59689108063));
#54587=CARTESIAN_POINT('Ctrl Pts',(-4.14316103429,-35.4359157968,-7.59673486922));
#54588=CARTESIAN_POINT('Ctrl Pts',(-5.21843923371,-35.3262967395,-7.044990155));
#54589=CARTESIAN_POINT('Ctrl Pts',(-5.21754878579,-35.3454147425,-7.04339100369));
#54590=CARTESIAN_POINT('Ctrl Pts',(-5.21690210383,-35.3645740899,-7.04217483695));
#54591=CARTESIAN_POINT('Ctrl Pts',(-5.21649981226,-35.3837610519,-7.04134271025));
#54592=CARTESIAN_POINT('Ctrl Pts',(-5.21634220772,-35.4029618215,-7.04089517538));
#54593=CARTESIAN_POINT('Ctrl Pts',(-5.21642926006,-35.422162591,-7.04083226933));
#54594=CARTESIAN_POINT('Ctrl Pts',(-6.21090480851,-35.3291957718,-6.34191684905));
#54595=CARTESIAN_POINT('Ctrl Pts',(-6.20990218356,-35.347292328,-6.34059495831));
#54596=CARTESIAN_POINT('Ctrl Pts',(-6.20914711064,-35.3654273382,-6.33960321184));
#54597=CARTESIAN_POINT('Ctrl Pts',(-6.20864031997,-35.3835880114,-6.33894257829));
#54598=CARTESIAN_POINT('Ctrl Pts',(-6.20838217516,-35.401761516,-6.33861353938));
#54599=CARTESIAN_POINT('Ctrl Pts',(-6.20837267016,-35.4199350207,-6.33861609384));
#54600=CARTESIAN_POINT('Ctrl Pts',(-6.59524089295,-35.3292320711,-6.04038307893));
#54601=CARTESIAN_POINT('Ctrl Pts',(-6.59420777333,-35.3473355691,-6.03905690773));
#54602=CARTESIAN_POINT('Ctrl Pts',(-6.59343802139,-35.3654739877,-6.03805312954));
#54603=CARTESIAN_POINT('Ctrl Pts',(-6.59293154067,-35.3836356047,-6.03737283826));
#54604=CARTESIAN_POINT('Ctrl Pts',(-6.59268825297,-35.4018088233,-6.03701670404));
#54605=CARTESIAN_POINT('Ctrl Pts',(-6.59270812441,-35.4199820418,-6.03698498184));
#54606=CARTESIAN_POINT('Ctrl Pts',(-7.36674622516,-35.3292429118,-5.37908303219));
#54607=CARTESIAN_POINT('Ctrl Pts',(-7.36563384979,-35.3471062503,-5.37795639383));
#54608=CARTESIAN_POINT('Ctrl Pts',(-7.36479211144,-35.3650081661,-5.37711871787));
#54609=CARTESIAN_POINT('Ctrl Pts',(-7.36422260417,-35.3829359555,-5.37657056503));
#54610=CARTESIAN_POINT('Ctrl Pts',(-7.36392615799,-35.4008766793,-5.37631208835));
#54611=CARTESIAN_POINT('Ctrl Pts',(-7.36390280813,-35.4188174032,-5.37634302053));
#54612=CARTESIAN_POINT('Ctrl Pts',(-8.06644392307,-35.3242511579,-4.63577831824));
#54613=CARTESIAN_POINT('Ctrl Pts',(-8.06481498329,-35.3443613723,-4.63450682037));
#54614=CARTESIAN_POINT('Ctrl Pts',(-8.06356784153,-35.3645192368,-4.63357464248));
#54615=CARTESIAN_POINT('Ctrl Pts',(-8.06270291188,-35.3847087915,-4.63298305339));
#54616=CARTESIAN_POINT('Ctrl Pts',(-8.06222041463,-35.4049141939,-4.63273277941));
#54617=CARTESIAN_POINT('Ctrl Pts',(-8.06212040397,-35.4251195963,-4.63282401372));
#54618=CARTESIAN_POINT('Ctrl Pts',(-8.40676939645,-35.318254221,-4.22563363488));
#54619=CARTESIAN_POINT('Ctrl Pts',(-8.40459143683,-35.3405015468,-4.22453866256));
#54620=CARTESIAN_POINT('Ctrl Pts',(-8.40288571682,-35.3628356427,-4.22380563891));
#54621=CARTESIAN_POINT('Ctrl Pts',(-8.40165936546,-35.3852283571,-4.22343491308));
#54622=CARTESIAN_POINT('Ctrl Pts',(-8.40091620766,-35.4076503711,-4.22342586623));
#54623=CARTESIAN_POINT('Ctrl Pts',(-8.40065659496,-35.4300723851,-4.22377686476));
#54624=CARTESIAN_POINT('Ctrl Pts',(-8.6986202738,-35.3007569312,-3.78649453504));
#54625=CARTESIAN_POINT('Ctrl Pts',(-8.69512018043,-35.3302263046,-3.78463499808));
#54626=CARTESIAN_POINT('Ctrl Pts',(-8.69237513121,-35.3597713122,-3.78337739168));
#54627=CARTESIAN_POINT('Ctrl Pts',(-8.69038139929,-35.3893659949,-3.78272454109));
#54628=CARTESIAN_POINT('Ctrl Pts',(-8.68913711634,-35.4189855209,-3.78267851397));
#54629=CARTESIAN_POINT('Ctrl Pts',(-8.68864247336,-35.4486050468,-3.78324063488));
#54630=CARTESIAN_POINT('Ctrl Pts',(-8.93444618031,-35.2748044449,-3.31652377072));
#54631=CARTESIAN_POINT('Ctrl Pts',(-8.92616350743,-35.3147858017,-3.31461838858));
#54632=CARTESIAN_POINT('Ctrl Pts',(-8.91971795914,-35.3551905608,-3.31361146728));
#54633=CARTESIAN_POINT('Ctrl Pts',(-8.91513837409,-35.3958795596,-3.31350964329));
#54634=CARTESIAN_POINT('Ctrl Pts',(-8.91244074774,-35.4367106808,-3.31431327227));
#54635=CARTESIAN_POINT('Ctrl Pts',(-8.91162790031,-35.4775418019,-3.31601642165));
#54636=CARTESIAN_POINT('Origin',(-2.2221106022258,-35.495269847715,-9.19615921132892));
#54637=CARTESIAN_POINT('Ctrl Pts',(-1.88395974093662,-35.2523605115009,
-8.27259966015858));
#54638=CARTESIAN_POINT('Ctrl Pts',(-1.88009563783341,-35.2998111449227,
-8.26124833618188));
#54639=CARTESIAN_POINT('Ctrl Pts',(-1.8767191336114,-35.3479866024315,-8.25276092720707));
#54640=CARTESIAN_POINT('Ctrl Pts',(-1.87384951644931,-35.3966500949375,
-8.24719410915978));
#54641=CARTESIAN_POINT('Ctrl Pts',(-1.87150117757236,-35.4455575723249,
-8.24457579968163));
#54642=CARTESIAN_POINT('Ctrl Pts',(-1.86968318420237,-35.4944649688017,
-8.24490433018094));
#54643=CARTESIAN_POINT('Ctrl Pts',(-1.91300759658597,-35.2527339398473,
-8.26755957224482));
#54644=CARTESIAN_POINT('Ctrl Pts',(-1.9097199029017,-35.3003685469398,-8.25602454207901));
#54645=CARTESIAN_POINT('Ctrl Pts',(-1.90694145962302,-35.3487360921407,
-8.24737013222748));
#54646=CARTESIAN_POINT('Ctrl Pts',(-1.90468881485147,-35.3975971714161,
-8.24165434232319));
#54647=CARTESIAN_POINT('Ctrl Pts',(-1.90297337398542,-35.4467049836923,
-8.23890603779062));
#54648=CARTESIAN_POINT('Ctrl Pts',(-1.90180104448326,-35.4958127139372,
-8.23912408927851));
#54649=CARTESIAN_POINT('Ctrl Pts',(-1.94218018572405,-35.2535044474158,
-8.2621591143811));
#54650=CARTESIAN_POINT('Ctrl Pts',(-1.93948439180326,-35.3011355726151,
-8.25052643519998));
#54651=CARTESIAN_POINT('Ctrl Pts',(-1.93731618833942,-35.3494991334594,
-8.24176908020048));
#54652=CARTESIAN_POINT('Ctrl Pts',(-1.9356894040532,-35.3983557916441,-8.23594548297372));
#54653=CARTESIAN_POINT('Ctrl Pts',(-1.93461165570096,-35.4474591093103,
-8.23308511017217));
#54654=CARTESIAN_POINT('Ctrl Pts',(-1.93408585739421,-35.4965623450722,
-8.23318738466497));
#54655=CARTESIAN_POINT('Ctrl Pts',(-1.9724911224602,-35.2538279318595,-8.25640089670514));
#54656=CARTESIAN_POINT('Ctrl Pts',(-1.96989995083931,-35.3014474096544,
-8.2447738198874));
#54657=CARTESIAN_POINT('Ctrl Pts',(-1.96784715401122,-35.3497975316059,
-8.23601549714894));
#54658=CARTESIAN_POINT('Ctrl Pts',(-1.96632241972348,-35.3986473889607,
-8.23018671944173));
#54659=CARTESIAN_POINT('Ctrl Pts',(-1.96537905911117,-35.4477354015217,
-8.22731155195785));
#54660=CARTESIAN_POINT('Ctrl Pts',(-1.9649957888598,-35.4968233351047,-8.22739248875143));
#54661=CARTESIAN_POINT('Ctrl Pts',(-2.00036048734845,-35.2563328498845,
-8.25033564485486));
#54662=CARTESIAN_POINT('Ctrl Pts',(-1.9989276215456,-35.3033816639248,-8.23877146644499));
#54663=CARTESIAN_POINT('Ctrl Pts',(-1.9980459932212,-35.3511346917004,-8.2300037370207));
#54664=CARTESIAN_POINT('Ctrl Pts',(-1.99772296424743,-35.3993616720185,
-8.22408907865538));
#54665=CARTESIAN_POINT('Ctrl Pts',(-1.99795923658066,-35.4478257884428,
-8.2210566696507));
#54666=CARTESIAN_POINT('Ctrl Pts',(-1.99875127112907,-35.4962898261243,
-8.22090710192112));
#54667=CARTESIAN_POINT('Ctrl Pts',(-2.02950436722481,-35.2581725723914,
-8.2439568163922));
#54668=CARTESIAN_POINT('Ctrl Pts',(-2.02862442295225,-35.3046828131338,
-8.23255380319936));
#54669=CARTESIAN_POINT('Ctrl Pts',(-2.0282990861559,-35.3518728653025,-8.22388078348058));
#54670=CARTESIAN_POINT('Ctrl Pts',(-2.02853256285331,-35.3995204524209,
-8.2179922787766));
#54671=CARTESIAN_POINT('Ctrl Pts',(-2.0293237410715,-35.4473967740714,-8.2149165636107));
#54672=CARTESIAN_POINT('Ctrl Pts',(-2.03066619547392,-35.4952730196676,
-8.2146548655385));
#54673=CARTESIAN_POINT('Origin',(-2.04762566711772,-35.4944692176037,-9.22894616712353));
#54674=CARTESIAN_POINT('Ctrl Pts',(-1.46090085849,-35.2135310847,-7.94951679032));
#54675=CARTESIAN_POINT('Ctrl Pts',(-1.48323559961,-35.2772019758,-7.94951679554));
#54676=CARTESIAN_POINT('Ctrl Pts',(-1.50020012625,-35.3427566518,-7.94951680076));
#54677=CARTESIAN_POINT('Ctrl Pts',(-1.51158239151,-35.4095912303,-7.94951680594));
#54678=CARTESIAN_POINT('Ctrl Pts',(-1.51727342189,-35.4770658384,-7.94951681101));
#54679=CARTESIAN_POINT('Ctrl Pts',(-1.5172734197,-35.5445404466,-7.94951681593));
#54680=CARTESIAN_POINT('Ctrl Pts',(-1.46090084734,-35.2135310529,-7.95714134841));
#54681=CARTESIAN_POINT('Ctrl Pts',(-1.48323559207,-35.2772019436,-7.95594579353));
#54682=CARTESIAN_POINT('Ctrl Pts',(-1.50020012179,-35.3427566195,-7.95475023866));
#54683=CARTESIAN_POINT('Ctrl Pts',(-1.51158238894,-35.4095911981,-7.95356602458));
#54684=CARTESIAN_POINT('Ctrl Pts',(-1.51727341997,-35.4770658064,-7.95240448782));
#54685=CARTESIAN_POINT('Ctrl Pts',(-1.51727341782,-35.5445404148,-7.95127632944));
#54686=CARTESIAN_POINT('Ctrl Pts',(-1.46095673562,-35.2136903768,-7.96472994159));
#54687=CARTESIAN_POINT('Ctrl Pts',(-1.48329083274,-35.277359414,-7.96234446573));
#54688=CARTESIAN_POINT('Ctrl Pts',(-1.50025081243,-35.3429136053,-7.95995898987));
#54689=CARTESIAN_POINT('Ctrl Pts',(-1.51162447777,-35.4097486473,-7.95759614371));
#54690=CARTESIAN_POINT('Ctrl Pts',(-1.51730285882,-35.477224193,-7.95527854376));
#54691=CARTESIAN_POINT('Ctrl Pts',(-1.51728631578,-35.5446997387,-7.9530275433));
#54692=CARTESIAN_POINT('Ctrl Pts',(-1.46106747229,-35.2140060602,-7.97227569366));
#54693=CARTESIAN_POINT('Ctrl Pts',(-1.48340028139,-35.277671426,-7.9687069317));
#54694=CARTESIAN_POINT('Ctrl Pts',(-1.50035124089,-35.3432246581,-7.96513816975));
#54695=CARTESIAN_POINT('Ctrl Pts',(-1.51170786352,-35.4100606172,-7.96160330128));
#54696=CARTESIAN_POINT('Ctrl Pts',(-1.51736118389,-35.4775380197,-7.95813620969));
#54697=CARTESIAN_POINT('Ctrl Pts',(-1.51731187088,-35.5450154221,-7.95476887067));
#54698=CARTESIAN_POINT('Ctrl Pts',(-1.4612316362,-35.2144740518,-7.97977268509));
#54699=CARTESIAN_POINT('Ctrl Pts',(-1.48356253349,-35.2781339746,-7.97502812195));
#54700=CARTESIAN_POINT('Ctrl Pts',(-1.50050012169,-35.3436857837,-7.9702835588));
#54701=CARTESIAN_POINT('Ctrl Pts',(-1.51183147778,-35.4105231034,-7.96558416229));
#54702=CARTESIAN_POINT('Ctrl Pts',(-1.51744764399,-35.4780032585,-7.96097508922));
#54703=CARTESIAN_POINT('Ctrl Pts',(-1.51734975497,-35.5454834136,-7.95649894554));
#54704=CARTESIAN_POINT('Ctrl Pts',(-1.461447583,-35.2150896638,-7.9872159128));
#54705=CARTESIAN_POINT('Ctrl Pts',(-1.48377596485,-35.2787424258,-7.98130374694));
#54706=CARTESIAN_POINT('Ctrl Pts',(-1.50069596198,-35.3442923623,-7.97539158107));
#54707=CARTESIAN_POINT('Ctrl Pts',(-1.51199407822,-35.4111314721,-7.96953589364));
#54708=CARTESIAN_POINT('Ctrl Pts',(-1.51756136975,-35.4786152489,-7.963793149));
#54709=CARTESIAN_POINT('Ctrl Pts',(-1.5173995886,-35.5460990256,-7.95821661336));
#54710=CARTESIAN_POINT('Origin',(-0.517271904869316,-35.5445407938528,-7.94950153701101));
#54711=CARTESIAN_POINT('Origin',(-0.517817922218787,-35.5460995791193,-7.98721621984755));
#54712=CARTESIAN_POINT('Ctrl Pts',(-1.46144763142,-35.2150898018,-7.98721591698));
#54713=CARTESIAN_POINT('Ctrl Pts',(-1.48377600029,-35.278742568,-7.9813037531));
#54714=CARTESIAN_POINT('Ctrl Pts',(-1.50069598676,-35.344292508,-7.97539158967));
#54715=CARTESIAN_POINT('Ctrl Pts',(-1.51199409489,-35.4111316208,-7.96953590506));
#54716=CARTESIAN_POINT('Ctrl Pts',(-1.51756138096,-35.4786154003,-7.96379316359));
#54717=CARTESIAN_POINT('Ctrl Pts',(-1.51739959704,-35.5460991799,-7.95821663141));
#54718=CARTESIAN_POINT('Ctrl Pts',(-1.45535023282,-35.1977075828,-8.04883580535));
#54719=CARTESIAN_POINT('Ctrl Pts',(-1.48166949688,-35.2678829449,-8.03945279279));
#54720=CARTESIAN_POINT('Ctrl Pts',(-1.50141667723,-35.3406016986,-8.03107453153));
#54721=CARTESIAN_POINT('Ctrl Pts',(-1.51429114701,-35.4150544061,-8.02380364128));
#54722=CARTESIAN_POINT('Ctrl Pts',(-1.52014358616,-35.4903742161,-8.01772327965));
#54723=CARTESIAN_POINT('Ctrl Pts',(-1.51898580713,-35.5656940262,-8.01289172937));
#54724=CARTESIAN_POINT('Ctrl Pts',(-1.46435245205,-35.1856198088,-8.11169781125));
#54725=CARTESIAN_POINT('Ctrl Pts',(-1.49329848629,-35.2601192136,-8.09750578865));
#54726=CARTESIAN_POINT('Ctrl Pts',(-1.51493019199,-35.3378102208,-8.08590190484));
#54727=CARTESIAN_POINT('Ctrl Pts',(-1.52885470957,-35.4176855473,-8.07706315905));
#54728=CARTESIAN_POINT('Ctrl Pts',(-1.53488112404,-35.4986532993,-8.07110658123));
#54729=CARTESIAN_POINT('Ctrl Pts',(-1.53303520019,-35.5796210507,-8.06808053282));
#54730=CARTESIAN_POINT('Ctrl Pts',(-1.49172176542,-35.1799552596,-8.17111299923));
#54731=CARTESIAN_POINT('Ctrl Pts',(-1.51992397896,-35.2563325377,-8.15127801209));
#54732=CARTESIAN_POINT('Ctrl Pts',(-1.54120100093,-35.3362785459,-8.13597848758));
#54733=CARTESIAN_POINT('Ctrl Pts',(-1.5551380035,-35.4186751656,-8.12550808337));
#54734=CARTESIAN_POINT('Ctrl Pts',(-1.56152781403,-35.5022972201,-8.12002297191));
#54735=CARTESIAN_POINT('Ctrl Pts',(-1.5603885908,-35.5859192753,-8.11952822853));
#54736=CARTESIAN_POINT('Ctrl Pts',(-1.57027832078,-35.1818573291,-8.25620202557));
#54737=CARTESIAN_POINT('Ctrl Pts',(-1.59174100272,-35.2575761439,-8.2305972979));
#54738=CARTESIAN_POINT('Ctrl Pts',(-1.60864769834,-35.3366611931,-8.21163579835));
#54739=CARTESIAN_POINT('Ctrl Pts',(-1.62070812016,-35.4180526309,-8.19967893383));
#54740=CARTESIAN_POINT('Ctrl Pts',(-1.62775389781,-35.5005977196,-8.19489712008));
#54741=CARTESIAN_POINT('Ctrl Pts',(-1.62975211946,-35.5831428078,-8.19725603749));
#54742=CARTESIAN_POINT('Ctrl Pts',(-1.67937525828,-35.2054111593,-8.29244102122));
#54743=CARTESIAN_POINT('Ctrl Pts',(-1.69139601914,-35.2726177891,-8.26960761361));
#54744=CARTESIAN_POINT('Ctrl Pts',(-1.70188615133,-35.3420423454,-8.25274940255));
#54745=CARTESIAN_POINT('Ctrl Pts',(-1.7107273602,-35.4129758871,-8.24210785095));
#54746=CARTESIAN_POINT('Ctrl Pts',(-1.71782785643,-35.4846639068,-8.23779633493));
#54747=CARTESIAN_POINT('Ctrl Pts',(-1.72312748813,-35.5563519268,-8.23979333534));
#54748=CARTESIAN_POINT('Ctrl Pts',(-1.73126212215,-35.2199435259,-8.29740056817));
#54749=CARTESIAN_POINT('Ctrl Pts',(-1.73944999004,-35.2817848557,-8.27769690404));
#54750=CARTESIAN_POINT('Ctrl Pts',(-1.74724337723,-35.3452273068,-8.26303381776));
#54751=CARTESIAN_POINT('Ctrl Pts',(-1.75458028421,-35.4097526752,-8.25356881995));
#54752=CARTESIAN_POINT('Ctrl Pts',(-1.76140026731,-35.4748200605,-8.24938018459));
#54753=CARTESIAN_POINT('Ctrl Pts',(-1.7676477796,-35.5398874456,-8.25046377193));
#54754=CARTESIAN_POINT('Ctrl Pts',(-1.78213085799,-35.2383375006,-8.29255588031));
#54755=CARTESIAN_POINT('Ctrl Pts',(-1.7878752107,-35.2931533399,-8.27665796781));
#54756=CARTESIAN_POINT('Ctrl Pts',(-1.79382722081,-35.3490506456,-8.26463904937));
#54757=CARTESIAN_POINT('Ctrl Pts',(-1.79995135062,-35.4056781551,-8.25659979182));
#54758=CARTESIAN_POINT('Ctrl Pts',(-1.80620870196,-35.4626704426,-8.2525916122));
#54759=CARTESIAN_POINT('Ctrl Pts',(-1.81255794182,-35.5196627301,-8.25261467335));
#54760=CARTESIAN_POINT('Ctrl Pts',(-1.83110005152,-35.2589529157,-8.27964657201));
#54761=CARTESIAN_POINT('Ctrl Pts',(-1.83516520879,-35.3056415029,-8.26740924886));
#54762=CARTESIAN_POINT('Ctrl Pts',(-1.83967790698,-35.3530283973,-8.25798482029));
#54763=CARTESIAN_POINT('Ctrl Pts',(-1.84461828078,-35.4008854025,-8.25143312625));
#54764=CARTESIAN_POINT('Ctrl Pts',(-1.84996206575,-35.4489774707,-8.24778634512));
#54765=CARTESIAN_POINT('Ctrl Pts',(-1.85568130399,-35.4970695389,-8.24704805785));
#54766=CARTESIAN_POINT('Origin',(-1.98370762109533,-35.4970695944798,-9.23881946100821));
#54767=CARTESIAN_POINT('Ctrl Pts',(-1.8311006173,-35.2589545751,-8.27964607156));
#54768=CARTESIAN_POINT('Ctrl Pts',(-1.83516599722,-35.30564267,-8.26740892391));
#54769=CARTESIAN_POINT('Ctrl Pts',(-1.83967892993,-35.3530290502,-8.25798461135));
#54770=CARTESIAN_POINT('Ctrl Pts',(-1.84461954945,-35.4008855262,-8.25143297176));
#54771=CARTESIAN_POINT('Ctrl Pts',(-1.84996359063,-35.4489770577,-8.24778618257));
#54772=CARTESIAN_POINT('Ctrl Pts',(-1.85568309486,-35.4970685893,-8.24704782502));
#54773=CARTESIAN_POINT('Ctrl Pts',(-1.8411549102,-35.2563947443,-8.27868180069));
#54774=CARTESIAN_POINT('Ctrl Pts',(-1.84372513023,-35.3033039498,-8.26655797443));
#54775=CARTESIAN_POINT('Ctrl Pts',(-1.84674896075,-35.3509164835,-8.25725221826));
#54776=CARTESIAN_POINT('Ctrl Pts',(-1.85021379554,-35.3990025183,-8.25082395949));
#54777=CARTESIAN_POINT('Ctrl Pts',(-1.85410255764,-35.447325312,-8.24730484866));
#54778=CARTESIAN_POINT('Ctrl Pts',(-1.85839419939,-35.4956481058,-8.24669783586));
#54779=CARTESIAN_POINT('Ctrl Pts',(-1.8515433823,-35.25441601,-8.27750101411));
#54780=CARTESIAN_POINT('Ctrl Pts',(-1.85257607592,-35.3015060532,-8.26552228872));
#54781=CARTESIAN_POINT('Ctrl Pts',(-1.85406935318,-35.3493041477,-8.25636790881));
#54782=CARTESIAN_POINT('Ctrl Pts',(-1.85601808078,-35.3975789365,-8.25009675826));
#54783=CARTESIAN_POINT('Ctrl Pts',(-1.8584126658,-35.4460920799,-8.24673979731));
#54784=CARTESIAN_POINT('Ctrl Pts',(-1.86123915467,-35.4946052233,-8.24629917315));
#54785=CARTESIAN_POINT('Ctrl Pts',(-1.86227923956,-35.2530824801,-8.2760758565));
#54786=CARTESIAN_POINT('Ctrl Pts',(-1.86172760863,-35.3003142451,-8.26427721621));
#54787=CARTESIAN_POINT('Ctrl Pts',(-1.86164442165,-35.3482586468,-8.25531090742));
#54788=CARTESIAN_POINT('Ctrl Pts',(-1.86203232275,-35.3966828431,-8.24923515298));
#54789=CARTESIAN_POINT('Ctrl Pts',(-1.86288941138,-35.4453469517,-8.24608002563));
#54790=CARTESIAN_POINT('Ctrl Pts',(-1.86420909862,-35.4940110603,-8.24584666363));
#54791=CARTESIAN_POINT('Ctrl Pts',(-1.8733302454,-35.2524719557,-8.27438297071));
#54792=CARTESIAN_POINT('Ctrl Pts',(-1.87114978057,-35.2998071163,-8.26280107324));
#54793=CARTESIAN_POINT('Ctrl Pts',(-1.86944655662,-35.34785966,-8.25406232754));
#54794=CARTESIAN_POINT('Ctrl Pts',(-1.8682313281,-35.3963952193,-8.24822411924));
#54795=CARTESIAN_POINT('Ctrl Pts',(-1.8675100956,-35.4451722935,-8.24531550566));
#54796=CARTESIAN_POINT('Ctrl Pts',(-1.86728392959,-35.4939493677,-8.24533636007));
#54797=CARTESIAN_POINT('Ctrl Pts',(-1.88461561635,-35.2526204897,-8.27242216736));
#54798=CARTESIAN_POINT('Ctrl Pts',(-1.88077145213,-35.3000228694,-8.26109202298));
#54799=CARTESIAN_POINT('Ctrl Pts',(-1.87741430691,-35.3481478104,-8.25261964893));
#54800=CARTESIAN_POINT('Ctrl Pts',(-1.87456332753,-35.3967592797,-8.24706149184));
#54801=CARTESIAN_POINT('Ctrl Pts',(-1.87223278053,-35.4456140212,-8.24444536521));
#54802=CARTESIAN_POINT('Ctrl Pts',(-1.87043162953,-35.4944687629,-8.2447696254));
#54803=CARTESIAN_POINT('Origin',(-0.517276095271889,-35.5445396177181,-6.5565839998119));
#54804=CARTESIAN_POINT('Origin',(-4.19954447987E-15,-32.5742356128,1.22464679915E-17));
#54805=CARTESIAN_POINT('',(9.27193478991,-32.4742356128,12.7934055377));
#54806=CARTESIAN_POINT('Origin',(9.27193478991,-32.5742356128,12.7934055377));
#54807=CARTESIAN_POINT('',(-8.84971102033,-32.4742356128,13.0890265053));
#54808=CARTESIAN_POINT('Origin',(9.55224857921E-16,-32.4742356128,-1.40227797601E-15));
#54809=CARTESIAN_POINT('Origin',(-8.84971102033,-32.5742356128,13.0890265053));
#54810=CARTESIAN_POINT('Origin',(9.15456852675,-32.5742356128,12.6314636954));
#54811=CARTESIAN_POINT('',(9.29417531907,-32.4742356128,12.4882507647));
#54812=CARTESIAN_POINT('Origin',(9.29417531907,-32.5742356128,12.4882507647));
#54813=CARTESIAN_POINT('Origin',(9.15456852675,-32.4742356128,12.6314636954));
#54814=CARTESIAN_POINT('Origin',(-0.316839226711,-32.5742356128,3.11924403781));
#54815=CARTESIAN_POINT('',(8.12053083925,-32.4742356128,11.3441589548));
#54816=CARTESIAN_POINT('Origin',(8.12053083925,-32.5742356128,11.3441589548));
#54817=CARTESIAN_POINT('',(8.70735307916,-32.4742356128,11.9162048597));
#54818=CARTESIAN_POINT('Origin',(8.39974442389,-32.5742356128,11.0577330933));
#54819=CARTESIAN_POINT('',(8.11331856237,-32.4742356128,10.7785195086));
#54820=CARTESIAN_POINT('Origin',(8.11331856237,-32.5742356128,10.7785195086));
#54821=CARTESIAN_POINT('Origin',(8.39974442389,-32.4742356128,11.0577330933));
#54822=CARTESIAN_POINT('Origin',(8.43647932171,-32.5742356128,10.447011287));
#54823=CARTESIAN_POINT('',(11.1212648448,-32.4742356128,7.69287592692));
#54824=CARTESIAN_POINT('Origin',(11.1212648448,-32.5742356128,7.69287592692));
#54825=CARTESIAN_POINT('',(9.6172917036,-32.4742356128,9.23569771778));
#54826=CARTESIAN_POINT('Origin',(11.4076907064,-32.5742356128,7.97208951156));
#54827=CARTESIAN_POINT('',(11.686904291,-32.4742356128,7.68566365004));
#54828=CARTESIAN_POINT('Origin',(11.686904291,-32.5742356128,7.68566365004));
#54829=CARTESIAN_POINT('Origin',(11.4076907064,-32.4742356128,7.97208951156));
#54830=CARTESIAN_POINT('Origin',(0.45986885604,-32.5742356128,-3.25867214427));
#54831=CARTESIAN_POINT('',(12.8348977878,-32.4742356128,8.80475037519));
#54832=CARTESIAN_POINT('Origin',(12.8348977878,-32.5742356128,8.80475037519));
#54833=CARTESIAN_POINT('',(12.2609010394,-32.4742356128,8.24520701262));
#54834=CARTESIAN_POINT('Origin',(12.9745045801,-32.5742356128,8.66153744443));
#54835=CARTESIAN_POINT('',(13.1408443824,-32.4742356128,8.77258279628));
#54836=CARTESIAN_POINT('Origin',(13.1408443824,-32.5742356128,8.77258279628));
#54837=CARTESIAN_POINT('Origin',(12.9745045801,-32.4742356128,8.66153744443));
#54838=CARTESIAN_POINT('Origin',(6.68547290961E-14,-32.5742356128,3.37630264166E-14));
#54839=CARTESIAN_POINT('',(14.1086187499,-32.4742356128,7.11244521731));
#54840=CARTESIAN_POINT('Origin',(14.1086187499,-32.5742356128,7.11244521731));
#54841=CARTESIAN_POINT('Origin',(-1.78359931397E-15,-32.4742356128,7.01138988003E-16));
#54842=CARTESIAN_POINT('Origin',(13.7514385284,-32.5742356128,6.93238331308));
#54843=CARTESIAN_POINT('',(14.1514385284,-32.4742356128,6.93238331308));
#54844=CARTESIAN_POINT('Origin',(14.1514385284,-32.5742356128,6.93238331308));
#54845=CARTESIAN_POINT('Origin',(13.7514385284,-32.4742356128,6.93238331308));
#54846=CARTESIAN_POINT('Origin',(14.1514385284,-32.5742356128,5.21140063714E-15));
#54847=CARTESIAN_POINT('',(14.1514385284,-32.4742356128,-6.93238331308));
#54848=CARTESIAN_POINT('Origin',(14.1514385284,-32.5742356128,-6.93238331308));
#54849=CARTESIAN_POINT('',(14.1514385284,-32.4742356128,6.2172489379E-15));
#54850=CARTESIAN_POINT('Origin',(13.7514385284,-32.5742356128,-6.93238331308));
#54851=CARTESIAN_POINT('',(14.1086187499,-32.4742356128,-7.11244521731));
#54852=CARTESIAN_POINT('Origin',(14.1086187499,-32.5742356128,-7.11244521731));
#54853=CARTESIAN_POINT('Origin',(13.7514385284,-32.4742356128,-6.93238331308));
#54854=CARTESIAN_POINT('Origin',(1.12952603833E-15,-32.5742356128,1.22464679915E-17));
#54855=CARTESIAN_POINT('',(13.1408443824,-32.4742356128,-8.77258279628));
#54856=CARTESIAN_POINT('Origin',(13.1408443824,-32.5742356128,-8.77258279628));
#54857=CARTESIAN_POINT('Origin',(-1.78359931397E-15,-32.4742356128,7.01138988003E-16));
#54858=CARTESIAN_POINT('Origin',(12.9745045801,-32.5742356128,-8.66153744443));
#54859=CARTESIAN_POINT('',(12.8348977878,-32.4742356128,-8.80475037519));
#54860=CARTESIAN_POINT('Origin',(12.8348977878,-32.5742356128,-8.80475037519));
#54861=CARTESIAN_POINT('Origin',(12.9745045801,-32.4742356128,-8.66153744443));
#54862=CARTESIAN_POINT('Origin',(0.45986885604,-32.5742356128,3.25867214427));
#54863=CARTESIAN_POINT('',(11.686904291,-32.4742356128,-7.68566365004));
#54864=CARTESIAN_POINT('Origin',(11.686904291,-32.5742356128,-7.68566365004));
#54865=CARTESIAN_POINT('',(12.2609010394,-32.4742356128,-8.24520701262));
#54866=CARTESIAN_POINT('Origin',(11.4076907064,-32.5742356128,-7.97208951156));
#54867=CARTESIAN_POINT('',(11.1212648448,-32.4742356128,-7.69287592692));
#54868=CARTESIAN_POINT('Origin',(11.1212648448,-32.5742356128,-7.69287592692));
#54869=CARTESIAN_POINT('Origin',(11.4076907064,-32.4742356128,-7.97208951156));
#54870=CARTESIAN_POINT('Origin',(8.43647932171,-32.5742356128,-10.447011287));
#54871=CARTESIAN_POINT('',(8.11331856237,-32.4742356128,-10.7785195086));
#54872=CARTESIAN_POINT('Origin',(8.11331856237,-32.5742356128,-10.7785195086));
#54873=CARTESIAN_POINT('',(9.6172917036,-32.4742356128,-9.23569771778));
#54874=CARTESIAN_POINT('Origin',(8.39974442389,-32.5742356128,-11.0577330933));
#54875=CARTESIAN_POINT('',(8.12053083925,-32.4742356128,-11.3441589548));
#54876=CARTESIAN_POINT('Origin',(8.12053083925,-32.5742356128,-11.3441589548));
#54877=CARTESIAN_POINT('Origin',(8.39974442389,-32.4742356128,-11.0577330933));
#54878=CARTESIAN_POINT('Origin',(-0.316839226711,-32.5742356128,-3.11924403781));
#54879=CARTESIAN_POINT('',(9.29417531907,-32.4742356128,-12.4882507647));
#54880=CARTESIAN_POINT('Origin',(9.29417531907,-32.5742356128,-12.4882507647));
#54881=CARTESIAN_POINT('',(8.70735307916,-32.4742356128,-11.9162048597));
#54882=CARTESIAN_POINT('Origin',(9.15456852675,-32.5742356128,-12.6314636954));
#54883=CARTESIAN_POINT('',(9.27193478991,-32.4742356128,-12.7934055377));
#54884=CARTESIAN_POINT('Origin',(9.27193478991,-32.5742356128,-12.7934055377));
#54885=CARTESIAN_POINT('Origin',(9.15456852675,-32.4742356128,-12.6314636954));
#54886=CARTESIAN_POINT('Origin',(1.12952603833E-15,-32.5742356128,-1.76411037141E-15));
#54887=CARTESIAN_POINT('',(-9.27193478991,-32.4742356128,-12.7934055377));
#54888=CARTESIAN_POINT('Origin',(-9.27193478991,-32.5742356128,-12.7934055377));
#54889=CARTESIAN_POINT('Origin',(-1.78359931397E-15,-32.4742356128,7.01138988003E-16));
#54890=CARTESIAN_POINT('Origin',(-9.15456852675,-32.5742356128,-12.6314636954));
#54891=CARTESIAN_POINT('',(-9.29417531907,-32.4742356128,-12.4882507647));
#54892=CARTESIAN_POINT('Origin',(-9.29417531907,-32.5742356128,-12.4882507647));
#54893=CARTESIAN_POINT('Origin',(-9.15456852675,-32.4742356128,-12.6314636954));
#54894=CARTESIAN_POINT('Origin',(0.316839226711,-32.5742356128,-3.11924403781));
#54895=CARTESIAN_POINT('',(-8.12053083925,-32.4742356128,-11.3441589548));
#54896=CARTESIAN_POINT('Origin',(-8.12053083925,-32.5742356128,-11.3441589548));
#54897=CARTESIAN_POINT('',(-8.70735307916,-32.4742356128,-11.9162048597));
#54898=CARTESIAN_POINT('Origin',(-8.39974442389,-32.5742356128,-11.0577330933));
#54899=CARTESIAN_POINT('',(-8.11331856237,-32.4742356128,-10.7785195086));
#54900=CARTESIAN_POINT('Origin',(-8.11331856237,-32.5742356128,-10.7785195086));
#54901=CARTESIAN_POINT('Origin',(-8.39974442389,-32.4742356128,-11.0577330933));
#54902=CARTESIAN_POINT('Origin',(-8.43647932171,-32.5742356128,-10.447011287));
#54903=CARTESIAN_POINT('',(-11.1212648448,-32.4742356128,-7.69287592692));
#54904=CARTESIAN_POINT('Origin',(-11.1212648448,-32.5742356128,-7.69287592692));
#54905=CARTESIAN_POINT('',(-9.6172917036,-32.4742356128,-9.23569771778));
#54906=CARTESIAN_POINT('Origin',(-11.4076907064,-32.5742356128,-7.97208951156));
#54907=CARTESIAN_POINT('',(-11.686904291,-32.4742356128,-7.68566365004));
#54908=CARTESIAN_POINT('Origin',(-11.686904291,-32.5742356128,-7.68566365004));
#54909=CARTESIAN_POINT('Origin',(-11.4076907064,-32.4742356128,-7.97208951156));
#54910=CARTESIAN_POINT('Origin',(-0.45986885604,-32.5742356128,3.25867214427));
#54911=CARTESIAN_POINT('',(-12.8348977878,-32.4742356128,-8.80475037519));
#54912=CARTESIAN_POINT('Origin',(-12.8348977878,-32.5742356128,-8.80475037519));
#54913=CARTESIAN_POINT('',(-12.2609010394,-32.4742356128,-8.24520701262));
#54914=CARTESIAN_POINT('Origin',(-12.9745045801,-32.5742356128,-8.66153744443));
#54915=CARTESIAN_POINT('',(-13.1408443824,-32.4742356128,-8.77258279628));
#54916=CARTESIAN_POINT('Origin',(-13.1408443824,-32.5742356128,-8.77258279628));
#54917=CARTESIAN_POINT('Origin',(-12.9745045801,-32.4742356128,-8.66153744443));
#54918=CARTESIAN_POINT('Origin',(1.12952603833E-15,-32.5742356128,1.22464679915E-17));
#54919=CARTESIAN_POINT('',(-14.1086187499,-32.4742356128,-7.11244521731));
#54920=CARTESIAN_POINT('Origin',(-14.1086187499,-32.5742356128,-7.11244521731));
#54921=CARTESIAN_POINT('Origin',(9.55224857921E-16,-32.4742356128,-1.40227797601E-15));
#54922=CARTESIAN_POINT('Origin',(-13.7514385284,-32.5742356128,-6.93238331308));
#54923=CARTESIAN_POINT('',(-14.1514385284,-32.4742356128,-6.93238331308));
#54924=CARTESIAN_POINT('Origin',(-14.1514385284,-32.5742356128,-6.93238331308));
#54925=CARTESIAN_POINT('Origin',(-13.7514385284,-32.4742356128,-6.93238331308));
#54926=CARTESIAN_POINT('Origin',(-14.1514385284,-32.5742356128,-5.18690770115E-15));
#54927=CARTESIAN_POINT('',(-14.1514385284,-32.4742356128,6.93238331308));
#54928=CARTESIAN_POINT('Origin',(-14.1514385284,-32.5742356128,6.93238331308));
#54929=CARTESIAN_POINT('',(-14.1514385284,-32.4742356128,-2.6645352591E-15));
#54930=CARTESIAN_POINT('Origin',(-13.7514385284,-32.5742356128,6.93238331308));
#54931=CARTESIAN_POINT('',(-14.1086187499,-32.4742356128,7.11244521731));
#54932=CARTESIAN_POINT('Origin',(-14.1086187499,-32.5742356128,7.11244521731));
#54933=CARTESIAN_POINT('Origin',(-13.7514385284,-32.4742356128,6.93238331308));
#54934=CARTESIAN_POINT('Origin',(6.95023748177E-12,-32.5742356128,-3.88843287498E-12));
#54935=CARTESIAN_POINT('',(-13.4206904888,-32.4742356128,8.33816927169));
#54936=CARTESIAN_POINT('Origin',(-13.4206904888,-32.5742356128,8.33816927169));
#54937=CARTESIAN_POINT('Origin',(9.55224857921E-16,-32.4742356128,-1.40227797601E-15));
#54938=CARTESIAN_POINT('Origin',(-13.2508083307,-32.5742356128,8.23262282521));
#54939=CARTESIAN_POINT('',(-13.1112015384,-32.4742356128,8.37583575597));
#54940=CARTESIAN_POINT('Origin',(-13.1112015384,-32.5742356128,8.37583575597));
#54941=CARTESIAN_POINT('Origin',(-13.2508083307,-32.4742356128,8.23262282521));
#54942=CARTESIAN_POINT('Origin',(-0.818017619209,-32.5742356128,-3.60780262944));
#54943=CARTESIAN_POINT('',(-12.0359212718,-32.4742356128,7.32763132313));
#54944=CARTESIAN_POINT('Origin',(-12.0359212718,-32.5742356128,7.32763132313));
#54945=CARTESIAN_POINT('',(-12.5735614051,-32.4742356128,7.85173353955));
#54946=CARTESIAN_POINT('Origin',(-11.7567076872,-32.5742356128,7.61405718465));
#54947=CARTESIAN_POINT('',(-11.4702818256,-32.4742356128,7.33484360001));
#54948=CARTESIAN_POINT('Origin',(-11.4702818256,-32.5742356128,7.33484360001));
#54949=CARTESIAN_POINT('Origin',(-11.7567076872,-32.4742356128,7.61405718465));
#54950=CARTESIAN_POINT('Origin',(-8.43647932171,-32.5742356128,10.447011287));
#54951=CARTESIAN_POINT('',(-7.76430158156,-32.4742356128,11.1365518355));
#54952=CARTESIAN_POINT('Origin',(-7.76430158156,-32.5742356128,11.1365518355));
#54953=CARTESIAN_POINT('',(-9.6172917036,-32.4742356128,9.23569771778));
#54954=CARTESIAN_POINT('Origin',(-8.73768936184,-32.5742356128,12.9233426255));
#54955=CARTESIAN_POINT('',(-8.87729615416,-32.4742356128,12.7801296947));
#54956=CARTESIAN_POINT('Origin',(-8.73768936184,-32.4742356128,12.9233426255));
#54957=CARTESIAN_POINT('Origin',(-8.87729615416,-32.5742356128,12.7801296947));
#54958=CARTESIAN_POINT('Origin',(-8.05072744309,-32.5742356128,11.4157654202));
#54959=CARTESIAN_POINT('',(-7.77151385845,-32.4742356128,11.7021912817));
#54960=CARTESIAN_POINT('Origin',(-7.77151385845,-32.5742356128,11.7021912817));
#54961=CARTESIAN_POINT('Origin',(-8.05072744309,-32.4742356128,11.4157654202));
#54962=CARTESIAN_POINT('Origin',(0.67498798988,-32.5742356128,3.46837452298));
#54963=CARTESIAN_POINT('',(-8.3244050063,-32.4742356128,12.2411604882));
#54964=CARTESIAN_POINT('Origin',(-6.22337865086E-16,-32.4742356128,0.));
#54965=CARTESIAN_POINT('',(12.4493324411,-32.4742356128,6.47376294621));
#54966=CARTESIAN_POINT('',(12.3114960897,-32.4742356128,6.33939734959));
#54967=CARTESIAN_POINT('',(10.328184518,-32.4742356128,6.50080898452));
#54968=CARTESIAN_POINT('Origin',(11.4022814987,-32.4742356128,7.54785992694));
#54969=CARTESIAN_POINT('',(6.90141785854,-32.4742356128,10.0160913585));
#54970=CARTESIAN_POINT('',(8.61480118826,-32.4742356128,8.25845017153));
#54971=CARTESIAN_POINT('',(6.92846389685,-32.4742356128,12.1372392817));
#54972=CARTESIAN_POINT('Origin',(7.97551483927,-32.4742356128,11.0631423009));
#54973=CARTESIAN_POINT('',(7.24427528424,-32.4742356128,12.4450984571));
#54974=CARTESIAN_POINT('',(6.79621292104,-32.4742356128,12.0083184194));
#54975=CARTESIAN_POINT('',(-6.7887641255,-32.4742356128,12.6993181568));
#54976=CARTESIAN_POINT('Origin',(-6.22337865086E-16,-32.4742356128,-9.86076131526E-32));
#54977=CARTESIAN_POINT('',(-6.57944691605,-32.4742356128,12.4952716086));
#54978=CARTESIAN_POINT('',(-6.14705703041,-32.4742356128,12.0737694115));
#54979=CARTESIAN_POINT('',(-6.55240087774,-32.4742356128,10.3741236854));
#54980=CARTESIAN_POINT('Origin',(-7.62649785846,-32.4742356128,11.4211746278));
#54981=CARTESIAN_POINT('',(-10.6782005908,-32.4742356128,6.14175175838));
#54982=CARTESIAN_POINT('',(-8.61480118826,-32.4742356128,8.25845017153));
#54983=CARTESIAN_POINT('Origin',(-11.7522975715,-32.4742356128,7.18880270079));
#54984=CARTESIAN_POINT('',(-10.328184518,-32.4742356128,-6.50080898452));
#54985=CARTESIAN_POINT('Origin',(-11.4022814987,-32.4742356128,-7.54785992694));
#54986=CARTESIAN_POINT('',(-6.90141785854,-32.4742356128,-10.0160913585));
#54987=CARTESIAN_POINT('',(-8.61480118826,-32.4742356128,-8.25845017153));
#54988=CARTESIAN_POINT('',(-6.92846389685,-32.4742356128,-12.1372392817));
#54989=CARTESIAN_POINT('Origin',(-7.97551483927,-32.4742356128,-11.0631423009));
#54990=CARTESIAN_POINT('',(-7.24427528424,-32.4742356128,-12.4450984571));
#54991=CARTESIAN_POINT('',(-6.79621292104,-32.4742356128,-12.0083184194));
#54992=CARTESIAN_POINT('',(7.24427528424,-32.4742356128,-12.4450984571));
#54993=CARTESIAN_POINT('Origin',(-6.22337865086E-16,-32.4742356128,-9.86076131526E-32));
#54994=CARTESIAN_POINT('',(6.92846389685,-32.4742356128,-12.1372392817));
#54995=CARTESIAN_POINT('',(6.79621292104,-32.4742356128,-12.0083184194));
#54996=CARTESIAN_POINT('',(6.90141785854,-32.4742356128,-10.0160913585));
#54997=CARTESIAN_POINT('Origin',(7.97551483927,-32.4742356128,-11.0631423009));
#54998=CARTESIAN_POINT('',(10.328184518,-32.4742356128,-6.50080898452));
#54999=CARTESIAN_POINT('',(8.61480118826,-32.4742356128,-8.25845017153));
#55000=CARTESIAN_POINT('Origin',(11.4022814987,-32.4742356128,-7.54785992694));
#55001=CARTESIAN_POINT('Origin',(-1.09995011675E-15,-34.4242356128,2.38806125834E-16));
#55002=CARTESIAN_POINT('',(7.24427528424,-32.8742356128,-12.4450984571));
#55003=CARTESIAN_POINT('',(7.24427528424,-33.6742356128,-12.4450984571));
#55004=CARTESIAN_POINT('',(-7.24427528424,-32.8742356128,-12.4450984571));
#55005=CARTESIAN_POINT('',(-7.24427528424,-33.6742356128,-12.4450984571));
#55006=CARTESIAN_POINT('Origin',(5.26886406864393E-14,-32.8742356128,2.66453525910038E-14));
#55007=CARTESIAN_POINT('Origin',(12.4493324411,-32.4742356128,6.47376294621));
#55008=CARTESIAN_POINT('',(12.4493324411,-32.8742356128,6.47376294621));
#55009=CARTESIAN_POINT('',(12.4493324411,-32.8742356128,6.47376294621));
#55010=CARTESIAN_POINT('',(12.4493324411,-32.6742356128,6.47376294621));
#55011=CARTESIAN_POINT('Origin',(6.92846389685,-32.4742356128,-12.1372392817));
#55012=CARTESIAN_POINT('',(6.92846389685,-32.8742356128,-12.1372392817));
#55013=CARTESIAN_POINT('',(6.92846389685,-32.8742356128,-12.1372392817));
#55014=CARTESIAN_POINT('',(6.92846389685,-32.6742356128,-12.1372392817));
#55015=CARTESIAN_POINT('Origin',(7.97551483927,-32.6742356128,-11.0631423009));
#55016=CARTESIAN_POINT('',(6.90141785854,-32.8742356128,-10.0160913585));
#55017=CARTESIAN_POINT('Origin',(7.97551483927,-32.8742356128,-11.0631423009));
#55018=CARTESIAN_POINT('',(6.90141785854,-33.6742356128,-10.0160913585));
#55019=CARTESIAN_POINT('Origin',(10.328184518,-32.4742356128,-6.50080898452));
#55020=CARTESIAN_POINT('',(10.328184518,-32.8742356128,-6.50080898452));
#55021=CARTESIAN_POINT('',(10.328184518,-32.8742356128,-6.50080898452));
#55022=CARTESIAN_POINT('',(10.328184518,-32.6742356128,-6.50080898452));
#55023=CARTESIAN_POINT('Origin',(11.4022814987,-32.6742356128,-7.54785992694));
#55024=CARTESIAN_POINT('Origin',(11.4022814987,-32.8742356128,-7.54785992694));
#55025=CARTESIAN_POINT('Origin',(10.328184518,-32.4742356128,6.50080898452));
#55026=CARTESIAN_POINT('',(10.328184518,-32.8742356128,6.50080898452));
#55027=CARTESIAN_POINT('',(10.328184518,-32.6742356128,6.50080898452));
#55028=CARTESIAN_POINT('',(6.90141785854,-32.8742356128,10.0160913585));
#55029=CARTESIAN_POINT('',(10.328184518,-32.8742356128,6.50080898452));
#55030=CARTESIAN_POINT('',(6.90141785854,-32.6742356128,10.0160913585));
#55031=CARTESIAN_POINT('Origin',(11.4022814987,-32.6742356128,7.54785992694));
#55032=CARTESIAN_POINT('Origin',(11.4022814987,-32.8742356128,7.54785992694));
#55033=CARTESIAN_POINT('Origin',(7.97551483927,-32.6742356128,11.0631423009));
#55034=CARTESIAN_POINT('',(6.92846389685,-32.8742356128,12.1372392817));
#55035=CARTESIAN_POINT('Origin',(7.97551483927,-32.8742356128,11.0631423009));
#55036=CARTESIAN_POINT('',(6.92846389685,-33.6742356128,12.1372392817));
#55037=CARTESIAN_POINT('Origin',(6.92846389685,-32.4742356128,12.1372392817));
#55038=CARTESIAN_POINT('',(7.24427528424,-32.8742356128,12.4450984571));
#55039=CARTESIAN_POINT('',(6.92846389685,-32.8742356128,12.1372392817));
#55040=CARTESIAN_POINT('',(7.24427528424,-33.6742356128,12.4450984571));
#55041=CARTESIAN_POINT('Origin',(-1.09995011675E-15,-34.4242356128,2.38806125834E-16));
#55042=CARTESIAN_POINT('',(-6.7887641255,-32.8742356128,12.6993181568));
#55043=CARTESIAN_POINT('Origin',(5.21804821573824E-14,-32.8742356128,8.88178419700125E-15));
#55044=CARTESIAN_POINT('',(-6.7887641255,-33.6742356128,12.6993181568));
#55045=CARTESIAN_POINT('Origin',(-6.92846389685,-32.4742356128,-12.1372392817));
#55046=CARTESIAN_POINT('',(-6.92846389685,-32.8742356128,-12.1372392817));
#55047=CARTESIAN_POINT('',(-6.92846389685,-32.6742356128,-12.1372392817));
#55048=CARTESIAN_POINT('',(-6.92846389685,-32.8742356128,-12.1372392817));
#55049=CARTESIAN_POINT('Origin',(-7.97551483927,-32.6742356128,-11.0631423009));
#55050=CARTESIAN_POINT('',(-6.90141785854,-32.8742356128,-10.0160913585));
#55051=CARTESIAN_POINT('Origin',(-7.97551483927,-32.8742356128,-11.0631423009));
#55052=CARTESIAN_POINT('',(-6.90141785854,-33.6742356128,-10.0160913585));
#55053=CARTESIAN_POINT('Origin',(-10.328184518,-32.4742356128,-6.50080898452));
#55054=CARTESIAN_POINT('',(-10.328184518,-32.8742356128,-6.50080898452));
#55055=CARTESIAN_POINT('',(-10.328184518,-32.6742356128,-6.50080898452));
#55056=CARTESIAN_POINT('',(-10.328184518,-32.8742356128,-6.50080898452));
#55057=CARTESIAN_POINT('Origin',(-11.7522975715,-32.6742356128,7.18880270079));
#55058=CARTESIAN_POINT('',(-10.6782005908,-32.8742356128,6.14175175838));
#55059=CARTESIAN_POINT('Origin',(-11.7522975715,-32.8742356128,7.18880270079));
#55060=CARTESIAN_POINT('',(-10.6782005908,-33.6742356128,6.14175175838));
#55061=CARTESIAN_POINT('Origin',(-10.328184518,-32.4742356128,6.50080898452));
#55062=CARTESIAN_POINT('',(-6.55240087774,-32.8742356128,10.3741236854));
#55063=CARTESIAN_POINT('',(-6.55240087774,-32.6742356128,10.3741236854));
#55064=CARTESIAN_POINT('',(-10.6782005908,-32.8742356128,6.14175175838));
#55065=CARTESIAN_POINT('Origin',(-7.62649785846,-32.6742356128,11.4211746278));
#55066=CARTESIAN_POINT('',(-6.57944691605,-32.8742356128,12.4952716086));
#55067=CARTESIAN_POINT('Origin',(-7.62649785846,-32.8742356128,11.4211746278));
#55068=CARTESIAN_POINT('',(-6.57944691605,-32.6742356128,12.4952716086));
#55069=CARTESIAN_POINT('Origin',(-6.57944691605,-32.4742356128,12.4952716086));
#55070=CARTESIAN_POINT('',(-6.57944691605,-32.8742356128,12.4952716086));
#55071=CARTESIAN_POINT('Ctrl Pts',(1.68475792039,-35.3742356128,-5.03973467448));
#55072=CARTESIAN_POINT('Ctrl Pts',(0.682166339124,-32.4742356128,-4.8790713724));
#55073=CARTESIAN_POINT('Ctrl Pts',(2.15538022242,-35.3742356128,-4.8080213959));
#55074=CARTESIAN_POINT('Ctrl Pts',(1.20736921572,-32.4742356128,-4.44659694115));
#55075=CARTESIAN_POINT('Ctrl Pts',(2.59973387128,-35.3742356128,-4.50528924317));
#55076=CARTESIAN_POINT('Ctrl Pts',(1.71079094607,-32.4742356128,-4.00290111016));
#55077=CARTESIAN_POINT('Ctrl Pts',(2.98121657961,-35.3742356128,-4.12686323533));
#55078=CARTESIAN_POINT('Ctrl Pts',(2.19825830329,-32.4742356128,-3.54512092123));
#55079=CARTESIAN_POINT('Ctrl Pts',(3.28679922947,-35.3742356128,-3.68411804659));
#55080=CARTESIAN_POINT('Ctrl Pts',(2.67474264449,-32.4742356128,-3.06699209341));
#55081=CARTESIAN_POINT('Ctrl Pts',(3.51985615629,-35.3742356128,-3.20601908088));
#55082=CARTESIAN_POINT('Ctrl Pts',(3.1350457731,-32.4742356128,-2.57376246377));
#55083=CARTESIAN_POINT('',(0.682166339124,-32.4742356128,-4.8790713724));
#55084=CARTESIAN_POINT('',(1.65073607089,-35.2758272825,-5.03428274092));
#55085=CARTESIAN_POINT('',(3.1350457731,-32.4742356128,-2.57376246377));
#55086=CARTESIAN_POINT('Ctrl Pts',(3.1350457731,-32.4742356128,-2.57376246377));
#55087=CARTESIAN_POINT('Ctrl Pts',(3.04574386842478,-32.4742356128,-2.66945233123215));
#55088=CARTESIAN_POINT('Ctrl Pts',(2.95565520899676,-32.4742356128,-2.76451972688002));
#55089=CARTESIAN_POINT('Ctrl Pts',(2.86486097840212,-32.4742356128,-2.85887905523607));
#55090=CARTESIAN_POINT('Ctrl Pts',(2.76926551199805,-32.4742356128,-2.95822814321991));
#55091=CARTESIAN_POINT('Ctrl Pts',(2.67288792014402,-32.4742356128,-3.05679239893703));
#55092=CARTESIAN_POINT('Ctrl Pts',(2.57578459070286,-32.4742356128,-3.15451622941541));
#55093=CARTESIAN_POINT('Ctrl Pts',(2.47439813201672,-32.4742356128001,-3.25655055880935));
#55094=CARTESIAN_POINT('Ctrl Pts',(2.37222039913981,-32.4742356128001,-3.35766900818225));
#55095=CARTESIAN_POINT('Ctrl Pts',(2.2692753175773,-32.4742356128001,-3.45785202544386));
#55096=CARTESIAN_POINT('Ctrl Pts',(2.16032661276555,-32.4742356128001,-3.56387758595748));
#55097=CARTESIAN_POINT('Ctrl Pts',(2.05051830060976,-32.4742356128001,-3.66885589509191));
#55098=CARTESIAN_POINT('Ctrl Pts',(1.93983639318639,-32.4742356128001,-3.77280566427766));
#55099=CARTESIAN_POINT('Ctrl Pts',(1.81352928403153,-32.4742356128001,-3.89143024483304));
#55100=CARTESIAN_POINT('Ctrl Pts',(1.68608466211416,-32.4742356128001,-4.00871596374921));
#55101=CARTESIAN_POINT('Ctrl Pts',(1.55742711564637,-32.4742356128001,-4.1247361422481));
#55102=CARTESIAN_POINT('Ctrl Pts',(1.40954803390843,-32.4742356128001,-4.25808982363347));
#55103=CARTESIAN_POINT('Ctrl Pts',(1.26006594487636,-32.4742356128001,-4.38977385603739));
#55104=CARTESIAN_POINT('Ctrl Pts',(1.10880104134623,-32.4742356128001,-4.51993332529904));
#55105=CARTESIAN_POINT('Ctrl Pts',(0.968189500144993,-32.4742356128001,
-4.64092585659807));
#55106=CARTESIAN_POINT('Ctrl Pts',(0.826035174351419,-32.4742356128001,
-4.760603642191));
#55107=CARTESIAN_POINT('Ctrl Pts',(0.682166339124,-32.4742356128,-4.8790713724));
#55108=CARTESIAN_POINT('',(3.50597895501,-35.2696545374,-3.18321836469));
#55109=CARTESIAN_POINT('Ctrl Pts',(1.51727342606,-35.3742356128,-5.3088808072));
#55110=CARTESIAN_POINT('Ctrl Pts',(0.5,-32.4742356128,-5.26505293156));
#55111=CARTESIAN_POINT('Ctrl Pts',(1.51727346704,-35.3742356128,-5.24111839755));
#55112=CARTESIAN_POINT('Ctrl Pts',(0.49999996933,-32.4742356128,-5.17707576222));
#55113=CARTESIAN_POINT('Ctrl Pts',(1.53640667867,-35.3742356128,-5.1734830193));
#55114=CARTESIAN_POINT('Ctrl Pts',(0.519349085752,-32.4742356128,-5.08894068096));
#55115=CARTESIAN_POINT('Ctrl Pts',(1.57167084987,-35.3742356128,-5.11676901693));
#55116=CARTESIAN_POINT('Ctrl Pts',(0.558553592228,-32.4742356128,-5.00590412413));
#55117=CARTESIAN_POINT('Ctrl Pts',(1.62392373781,-35.3742356128,-5.06968674937));
#55118=CARTESIAN_POINT('Ctrl Pts',(0.614278309582,-32.4742356128,-4.93497322721));
#55119=CARTESIAN_POINT('Ctrl Pts',(1.68475792039,-35.3742356128,-5.03973467448));
#55120=CARTESIAN_POINT('Ctrl Pts',(0.682166339124,-32.4742356128,-4.8790713724));
#55121=CARTESIAN_POINT('',(0.5,-32.4742356128,-5.26505293156));
#55122=CARTESIAN_POINT('',(1.46090316329,-35.2135376551,-5.30645216923));
#55123=CARTESIAN_POINT('Ctrl Pts',(0.5,-32.4742356128,-5.26505293156));
#55124=CARTESIAN_POINT('Ctrl Pts',(0.499999987183553,-32.4742356128,-5.22828883820323));
#55125=CARTESIAN_POINT('Ctrl Pts',(0.504054600653073,-32.4742356128085,
-5.19170069064497));
#55126=CARTESIAN_POINT('Ctrl Pts',(0.520156709880915,-32.4742356128085,
-5.1199141043431));
#55127=CARTESIAN_POINT('Ctrl Pts',(0.532168073174417,-32.4742356128085,
-5.08496970255448));
#55128=CARTESIAN_POINT('Ctrl Pts',(0.56359844412932,-32.4742356128085,-5.0183737839542));
#55129=CARTESIAN_POINT('Ctrl Pts',(0.582941481982889,-32.4742356128085,
-4.98688524144264));
#55130=CARTESIAN_POINT('Ctrl Pts',(0.628123824966223,-32.4742356128085,
-4.9288235651309));
#55131=CARTESIAN_POINT('Ctrl Pts',(0.653788606277979,-32.4742356128,-4.90243878948513));
#55132=CARTESIAN_POINT('Ctrl Pts',(0.682166339124,-32.4742356128,-4.8790713724));
#55133=CARTESIAN_POINT('Origin',(1.51727342606,-35.3742356128,-6.62635333853281));
#55134=CARTESIAN_POINT('',(0.5,-32.4742356128,-8.63648038577));
#55135=CARTESIAN_POINT('',(1.46144758302801,-35.2150896637902,-7.9872159496586));
#55136=CARTESIAN_POINT('',(0.5,-32.4742356128,-5.26505293156));
#55137=CARTESIAN_POINT('Ctrl Pts',(2.06618662358,-35.3742356128,-8.20763292551));
#55138=CARTESIAN_POINT('Ctrl Pts',(1.13092983125,-32.4742356128,-9.11903336658));
#55139=CARTESIAN_POINT('Ctrl Pts',(2.02728693019,-35.3742356128,-8.21539237438));
#55140=CARTESIAN_POINT('Ctrl Pts',(1.08254865919,-32.4742356128,-9.13216050293));
#55141=CARTESIAN_POINT('Ctrl Pts',(1.98835267261,-35.3742356128,-8.22296816028));
#55142=CARTESIAN_POINT('Ctrl Pts',(1.03251986746,-32.4742356128,-9.13922496193));
#55143=CARTESIAN_POINT('Ctrl Pts',(1.94830447917,-35.3742356128,-8.23056358523));
#55144=CARTESIAN_POINT('Ctrl Pts',(0.980045978296,-32.4742356128,-9.13989363405));
#55145=CARTESIAN_POINT('Ctrl Pts',(1.90939289225,-35.3742356128,-8.23775490438));
#55146=CARTESIAN_POINT('Ctrl Pts',(0.929775106566,-32.4742356128,-9.13406227499));
#55147=CARTESIAN_POINT('Ctrl Pts',(1.87043161103,-35.3742356128,-8.24476960824));
#55148=CARTESIAN_POINT('Ctrl Pts',(0.881024471639,-32.4742356128,-9.12211895883));
#55149=CARTESIAN_POINT('',(1.13092983125,-32.4742356128,-9.11903336658));
#55150=CARTESIAN_POINT('',(2.02882173043,-35.2583763205,-8.24404472212));
#55151=CARTESIAN_POINT('',(0.881024471639,-32.4742356128,-9.12211895883));
#55152=CARTESIAN_POINT('Ctrl Pts',(0.881024471639,-32.4742356128,-9.12211895883));
#55153=CARTESIAN_POINT('Ctrl Pts',(0.922203022128766,-32.4742356128,-9.13220720584968));
#55154=CARTESIAN_POINT('Ctrl Pts',(0.964264761466657,-32.4742356129145,
-9.13687601608875));
#55155=CARTESIAN_POINT('Ctrl Pts',(1.04807643550279,-32.4742356129145,-9.13584111848088));
#55156=CARTESIAN_POINT('Ctrl Pts',(1.09001173360473,-32.4742356128,-9.13013556654957));
#55157=CARTESIAN_POINT('Ctrl Pts',(1.13092983125,-32.4742356128,-9.11903336658));
#55158=CARTESIAN_POINT('',(1.83110005118,-35.2589529157,-8.27964657357));
#55159=CARTESIAN_POINT('Ctrl Pts',(1.87043161103,-35.3742356128,-8.24476960824));
#55160=CARTESIAN_POINT('Ctrl Pts',(0.881024471639,-32.4742356128,-9.12211895883));
#55161=CARTESIAN_POINT('Ctrl Pts',(1.76698369017,-35.3742356128,-8.26339468616));
#55162=CARTESIAN_POINT('Ctrl Pts',(0.751586859387,-32.4742356128,-9.0904082994));
#55163=CARTESIAN_POINT('Ctrl Pts',(1.65525765665,-35.3742356128,-8.23673498884));
#55164=CARTESIAN_POINT('Ctrl Pts',(0.632864708596,-32.4742356128,-9.01561057704));
#55165=CARTESIAN_POINT('Ctrl Pts',(1.56310817921,-35.3742356128,-8.15928174403));
#55166=CARTESIAN_POINT('Ctrl Pts',(0.544519454171,-32.4742356128,-8.90337130527));
#55167=CARTESIAN_POINT('Ctrl Pts',(1.51727343488,-35.3742356128,-8.05439924541));
#55168=CARTESIAN_POINT('Ctrl Pts',(0.500000005883,-32.4742356128,-8.76992589769));
#55169=CARTESIAN_POINT('Ctrl Pts',(1.51727342606,-35.3742356128,-7.9495168227));
#55170=CARTESIAN_POINT('Ctrl Pts',(0.5,-32.4742356128,-8.63648038577));
#55171=CARTESIAN_POINT('Ctrl Pts',(0.881024471639,-32.4742356128,-9.12211895883));
#55172=CARTESIAN_POINT('Ctrl Pts',(0.827016089126107,-32.4742356128,-9.10888755418313));
#55173=CARTESIAN_POINT('Ctrl Pts',(0.775540637915395,-32.4742356128,-9.08673032516009));
#55174=CARTESIAN_POINT('Ctrl Pts',(0.682134270020786,-32.4742356128,-9.02649837726588));
#55175=CARTESIAN_POINT('Ctrl Pts',(0.640813901103346,-32.4742356141908,
-8.98885840070038));
#55176=CARTESIAN_POINT('Ctrl Pts',(0.57228055336198,-32.4742356141908,-8.901510263898));
#55177=CARTESIAN_POINT('Ctrl Pts',(0.545563385694432,-32.4742356128,-8.85244719394298));
#55178=CARTESIAN_POINT('Ctrl Pts',(0.509276617611064,-32.4742356128,-8.74739553291418));
#55179=CARTESIAN_POINT('Ctrl Pts',(0.500000002452142,-32.4742356128,-8.69210290609089));
#55180=CARTESIAN_POINT('Ctrl Pts',(0.5,-32.4742356128,-8.63648038577));
#55181=CARTESIAN_POINT('Ctrl Pts',(8.90408048591,-35.3742356128,-3.33175685019));
#55182=CARTESIAN_POINT('Ctrl Pts',(9.78972512979,-32.4742356128,-2.88747118331));
#55183=CARTESIAN_POINT('Ctrl Pts',(8.6873937464,-35.3742356128,-3.78156218415));
#55184=CARTESIAN_POINT('Ctrl Pts',(9.44154892618,-32.4742356128,-3.40960230403));
#55185=CARTESIAN_POINT('Ctrl Pts',(8.41228804471,-35.3742356128,-4.20311089247));
#55186=CARTESIAN_POINT('Ctrl Pts',(9.06633060557,-32.4742356128,-3.9138589137));
#55187=CARTESIAN_POINT('Ctrl Pts',(8.09063109224,-35.3742356128,-4.59678365893));
#55188=CARTESIAN_POINT('Ctrl Pts',(8.6592141531,-32.4742356128,-4.40538764451));
#55189=CARTESIAN_POINT('Ctrl Pts',(7.360622472,-35.3742356128,-5.38465519647));
#55190=CARTESIAN_POINT('Ctrl Pts',(7.74414150515,-32.4742356128,-5.40001779324));
#55191=CARTESIAN_POINT('Ctrl Pts',(6.54392160985,-35.3742356128,-6.08248533528));
#55192=CARTESIAN_POINT('Ctrl Pts',(6.72376489891,-32.4742356128,-6.28784412471));
#55193=CARTESIAN_POINT('Ctrl Pts',(6.08996440487,-35.3742356128,-6.43395446983));
#55194=CARTESIAN_POINT('Ctrl Pts',(6.15045388192,-32.4742356128,-6.72961730824));
#55195=CARTESIAN_POINT('Ctrl Pts',(5.07098217764,-35.3742356128,-7.12903795521));
#55196=CARTESIAN_POINT('Ctrl Pts',(4.8659622122,-32.4742356128,-7.60280558321));
#55197=CARTESIAN_POINT('Ctrl Pts',(3.96068628695,-35.3742356128,-7.66774624913));
#55198=CARTESIAN_POINT('Ctrl Pts',(3.47975995949,-32.4742356128,-8.30623076748));
#55199=CARTESIAN_POINT('Ctrl Pts',(3.34362139801,-35.3742356128,-7.90067576649));
#55200=CARTESIAN_POINT('Ctrl Pts',(2.71614717835,-32.4742356128,-8.63027694049));
#55201=CARTESIAN_POINT('Ctrl Pts',(2.70966555084,-35.3742356128,-8.07927608136));
#55202=CARTESIAN_POINT('Ctrl Pts',(1.93124535238,-32.4742356128,-8.90188586102));
#55203=CARTESIAN_POINT('Ctrl Pts',(2.06618662358,-35.3742356128,-8.20763292551));
#55204=CARTESIAN_POINT('Ctrl Pts',(1.13092983125,-32.4742356128,-9.11903336658));
#55205=CARTESIAN_POINT('',(9.78972512979,-32.4742356128,-2.88747118331));
#55206=CARTESIAN_POINT('',(8.93444623808,-35.2748044449,-3.31652380097));
#55207=CARTESIAN_POINT('Ctrl Pts',(1.13092983125,-32.4742356128,-9.11903336658));
#55208=CARTESIAN_POINT('Ctrl Pts',(1.35748096440087,-32.4742356128002,-9.05756384343984));
#55209=CARTESIAN_POINT('Ctrl Pts',(1.58257164660585,-32.4742356128003,-8.99085150410091));
#55210=CARTESIAN_POINT('Ctrl Pts',(1.80593829563056,-32.4742356128004,-8.91898444731663));
#55211=CARTESIAN_POINT('Ctrl Pts',(2.06358605409587,-32.4742356128005,-8.83608762199012));
#55212=CARTESIAN_POINT('Ctrl Pts',(2.31894092044636,-32.4742356128005,-8.74633156326516));
#55213=CARTESIAN_POINT('Ctrl Pts',(2.57167018297851,-32.4742356128005,-8.6498360378973));
#55214=CARTESIAN_POINT('Ctrl Pts',(2.87961762633398,-32.4742356128005,-8.53225744792893));
#55215=CARTESIAN_POINT('Ctrl Pts',(3.18367140744747,-32.4742356128005,-8.40466930268279));
#55216=CARTESIAN_POINT('Ctrl Pts',(3.48328763307677,-32.4742356128004,-8.26730091093105));
#55217=CARTESIAN_POINT('Ctrl Pts',(3.71568832582298,-32.4742356128003,-8.16074957400834));
#55218=CARTESIAN_POINT('Ctrl Pts',(3.94542176433015,-32.4742356128003,-8.0483135945673));
#55219=CARTESIAN_POINT('Ctrl Pts',(4.17221459820387,-32.4742356128002,-7.93012756314153));
#55220=CARTESIAN_POINT('Ctrl Pts',(4.3691051862723,-32.4742356128002,-7.82752415706631));
#55221=CARTESIAN_POINT('Ctrl Pts',(4.56378009094538,-32.4742356128001,-7.72058696590365));
#55222=CARTESIAN_POINT('Ctrl Pts',(4.75602733655703,-32.4742356128001,-7.60942955096299));
#55223=CARTESIAN_POINT('Ctrl Pts',(4.81482808842437,-32.4742356128001,-7.57543093863777));
#55224=CARTESIAN_POINT('Ctrl Pts',(4.87340144129883,-32.4742356128001,-7.54103772494405));
#55225=CARTESIAN_POINT('Ctrl Pts',(4.93174048144869,-32.4742356128001,-7.50625373162201));
#55226=CARTESIAN_POINT('Ctrl Pts',(5.17371609272893,-32.4742356128,-7.36197850828535));
#55227=CARTESIAN_POINT('Ctrl Pts',(5.41165903155182,-32.4742356128,-7.21097959772054));
#55228=CARTESIAN_POINT('Ctrl Pts',(5.64521361977431,-32.4742356128,-7.0534854983882));
#55229=CARTESIAN_POINT('Ctrl Pts',(5.92854786582719,-32.4742356128,-6.86242321940786));
#55230=CARTESIAN_POINT('Ctrl Pts',(6.20541886627958,-32.4742356128,-6.66180293529635));
#55231=CARTESIAN_POINT('Ctrl Pts',(6.47520523011177,-32.4742356128,-6.45207607376425));
#55232=CARTESIAN_POINT('Ctrl Pts',(6.7042174903774,-32.4742356128001,-6.27404623594872));
#55233=CARTESIAN_POINT('Ctrl Pts',(6.92812568553406,-32.4742356128001,-6.08945471655604));
#55234=CARTESIAN_POINT('Ctrl Pts',(7.14656401932481,-32.4742356128001,-5.89860434351618));
#55235=CARTESIAN_POINT('Ctrl Pts',(7.30145174556248,-32.4742356128002,-5.76327836927544));
#55236=CARTESIAN_POINT('Ctrl Pts',(7.4535896236381,-32.4742356128002,-5.62480608682023));
#55237=CARTESIAN_POINT('Ctrl Pts',(7.60284952378423,-32.4742356128003,-5.48330473081067));
#55238=CARTESIAN_POINT('Ctrl Pts',(7.66409102798865,-32.4742356128003,-5.42524656595522));
#55239=CARTESIAN_POINT('Ctrl Pts',(7.72484844931582,-32.4742356128003,-5.36667817449847));
#55240=CARTESIAN_POINT('Ctrl Pts',(7.78511221664714,-32.4742356128003,-5.30760881482714));
#55241=CARTESIAN_POINT('Ctrl Pts',(7.86083082414573,-32.4742356128003,-5.23339092473813));
#55242=CARTESIAN_POINT('Ctrl Pts',(7.9357705171939,-32.4742356128004,-5.1583808441567));
#55243=CARTESIAN_POINT('Ctrl Pts',(8.00994285087825,-32.4742356128004,-5.08255688170474));
#55244=CARTESIAN_POINT('Ctrl Pts',(8.09229096248547,-32.4742356128004,-4.99837508759984));
#55245=CARTESIAN_POINT('Ctrl Pts',(8.17369314495629,-32.4742356128004,-4.91319009037416));
#55246=CARTESIAN_POINT('Ctrl Pts',(8.25412492760548,-32.4742356128004,-4.82702704996663));
#55247=CARTESIAN_POINT('Ctrl Pts',(8.31333790947206,-32.4742356128004,-4.76359478002089));
#55248=CARTESIAN_POINT('Ctrl Pts',(8.37202401218054,-32.4742356128004,-4.69963371548019));
#55249=CARTESIAN_POINT('Ctrl Pts',(8.43016285000587,-32.4742356128004,-4.63516899165583));
#55250=CARTESIAN_POINT('Ctrl Pts',(8.45791646133128,-32.4742356128004,-4.60439560580666));
#55251=CARTESIAN_POINT('Ctrl Pts',(8.48554521988306,-32.4742356128004,-4.57350770746612));
#55252=CARTESIAN_POINT('Ctrl Pts',(8.51305689825755,-32.4742356128004,-4.54249677272974));
#55253=CARTESIAN_POINT('Ctrl Pts',(8.62342507636421,-32.4742356128004,-4.41809068155457));
#55254=CARTESIAN_POINT('Ctrl Pts',(8.7318733436495,-32.4742356128004,-4.29174315144362));
#55255=CARTESIAN_POINT('Ctrl Pts',(8.8382486463566,-32.4742356128004,-4.16363335145393));
#55256=CARTESIAN_POINT('Ctrl Pts',(8.93277342320662,-32.4742356128004,-4.04979536511541));
#55257=CARTESIAN_POINT('Ctrl Pts',(9.02565819435723,-32.4742356128005,-3.93456977982075));
#55258=CARTESIAN_POINT('Ctrl Pts',(9.11679326953606,-32.4742356128005,-3.81808802140576));
#55259=CARTESIAN_POINT('Ctrl Pts',(9.19450142462868,-32.4742356128005,-3.7187675069868));
#55260=CARTESIAN_POINT('Ctrl Pts',(9.2709365589139,-32.4742356128005,-3.61853483930442));
#55261=CARTESIAN_POINT('Ctrl Pts',(9.34605185297795,-32.4742356128005,-3.51744756155323));
#55262=CARTESIAN_POINT('Ctrl Pts',(9.41503263776077,-32.4742356128005,-3.42461587078078));
#55263=CARTESIAN_POINT('Ctrl Pts',(9.48289988060696,-32.4742356128004,-3.33106404763001));
#55264=CARTESIAN_POINT('Ctrl Pts',(9.54964545463381,-32.4742356128004,-3.23680385237855));
#55265=CARTESIAN_POINT('Ctrl Pts',(9.6112390224299,-32.4742356128003,-3.14981948208372));
#55266=CARTESIAN_POINT('Ctrl Pts',(9.67187720579196,-32.4742356128002,-3.0622321188807));
#55267=CARTESIAN_POINT('Ctrl Pts',(9.73158294374893,-32.4742356128001,-2.97401646795334));
#55268=CARTESIAN_POINT('Ctrl Pts',(9.75106213192314,-32.4742356128001,-2.94523582938955));
#55269=CARTESIAN_POINT('Ctrl Pts',(9.77044232827666,-32.4742356128,-2.91638800950429));
#55270=CARTESIAN_POINT('Ctrl Pts',(9.78972512979,-32.4742356128,-2.88747118331));
#55271=CARTESIAN_POINT('Ctrl Pts',(8.98669828191,-35.3742356128,-3.15062625521));
#55272=CARTESIAN_POINT('Ctrl Pts',(9.87176476169,-32.4742356128,-2.65438916225));
#55273=CARTESIAN_POINT('Ctrl Pts',(8.97105229548,-35.3742356128,-3.18695239061));
#55274=CARTESIAN_POINT('Ctrl Pts',(9.86736571705,-32.4742356128,-2.70382530588));
#55275=CARTESIAN_POINT('Ctrl Pts',(8.95501903475,-35.3742356128,-3.22311199053));
#55276=CARTESIAN_POINT('Ctrl Pts',(9.85683264819,-32.4742356128,-2.75271530399));
#55277=CARTESIAN_POINT('Ctrl Pts',(8.93801024352,-35.3742356128,-3.26038797601));
#55278=CARTESIAN_POINT('Ctrl Pts',(9.83970156009,-32.4742356128,-2.80141079064));
#55279=CARTESIAN_POINT('Ctrl Pts',(8.92122822926,-35.3742356128,-3.29616101079));
#55280=CARTESIAN_POINT('Ctrl Pts',(9.81727888481,-32.4742356128,-2.84615108413));
#55281=CARTESIAN_POINT('Ctrl Pts',(8.90408048591,-35.3742356128,-3.33175685019));
#55282=CARTESIAN_POINT('Ctrl Pts',(9.78972512979,-32.4742356128,-2.88747118331));
#55283=CARTESIAN_POINT('',(9.87176476169,-32.4742356128,-2.65438916225));
#55284=CARTESIAN_POINT('',(9.01911869317,-35.2680072167,-3.13244885159));
#55285=CARTESIAN_POINT('Ctrl Pts',(9.78972512979,-32.4742356128,-2.88747118331));
#55286=CARTESIAN_POINT('Ctrl Pts',(9.81295259231924,-32.4742356128,-2.85263886899527));
#55287=CARTESIAN_POINT('Ctrl Pts',(9.83153875118569,-32.4742356128031,-2.81516874103241));
#55288=CARTESIAN_POINT('Ctrl Pts',(9.85907250604964,-32.4742356128031,-2.7369427732809));
#55289=CARTESIAN_POINT('Ctrl Pts',(9.86805391811268,-32.4742356128,-2.69609135240486));
#55290=CARTESIAN_POINT('Ctrl Pts',(9.87176476169,-32.4742356128,-2.65438916225));
#55291=CARTESIAN_POINT('Ctrl Pts',(9.23698117862,-35.3742356128,0.509886547139));
#55292=CARTESIAN_POINT('Ctrl Pts',(9.85462053301,-32.4742356128,2.00920484002));
#55293=CARTESIAN_POINT('Ctrl Pts',(9.29448486778,-35.3742356128,0.14300248283));
#55294=CARTESIAN_POINT('Ctrl Pts',(9.89942675021,-32.4742356128,1.54440936128));
#55295=CARTESIAN_POINT('Ctrl Pts',(9.33952412131,-35.3742356128,-0.225988266205));
#55296=CARTESIAN_POINT('Ctrl Pts',(9.93347655148,-32.4742356128,1.07876884298));
#55297=CARTESIAN_POINT('Ctrl Pts',(9.37147906182,-35.3742356128,-0.598052135313));
#55298=CARTESIAN_POINT('Ctrl Pts',(9.95684539874,-32.4742356128,0.6105872463));
#55299=CARTESIAN_POINT('Ctrl Pts',(9.39776085185,-35.3742356128,-1.34354990637));
#55300=CARTESIAN_POINT('Ctrl Pts',(9.98182966629,-32.4742356128,-0.323612218818));
#55301=CARTESIAN_POINT('Ctrl Pts',(9.31944120585,-35.3742356128,-2.08553948714));
#55302=CARTESIAN_POINT('Ctrl Pts',(9.96363436978,-32.4742356128,-1.25779968708));
#55303=CARTESIAN_POINT('Ctrl Pts',(9.24709061054,-35.3742356128,-2.45151005123));
#55304=CARTESIAN_POINT('Ctrl Pts',(9.943864011,-32.4742356128,-1.72215443881));
#55305=CARTESIAN_POINT('Ctrl Pts',(9.13406983882,-35.3742356128,-2.80846571914));
#55306=CARTESIAN_POINT('Ctrl Pts',(9.91319925962,-32.4742356128,-2.18875096266));
#55307=CARTESIAN_POINT('Ctrl Pts',(8.98669828191,-35.3742356128,-3.15062625521));
#55308=CARTESIAN_POINT('Ctrl Pts',(9.87176476169,-32.4742356128,-2.65438916225));
#55309=CARTESIAN_POINT('',(9.85462053301,-32.4742356128,2.00920484002));
#55310=CARTESIAN_POINT('',(9.26569107792,-35.2394341184,0.579579770069));
#55311=CARTESIAN_POINT('Ctrl Pts',(9.87176476169,-32.4742356128,-2.65438916225));
#55312=CARTESIAN_POINT('Ctrl Pts',(9.88154386677506,-32.4742356128,-2.54449221374346));
#55313=CARTESIAN_POINT('Ctrl Pts',(9.89059756234382,-32.4742356128,-2.43459652045344));
#55314=CARTESIAN_POINT('Ctrl Pts',(9.8989264871901,-32.4742356128,-2.32475313888866));
#55315=CARTESIAN_POINT('Ctrl Pts',(9.9081500912099,-32.4742356128,-2.20311056503328));
#55316=CARTESIAN_POINT('Ctrl Pts',(9.91648489987761,-32.4742356128,-2.08153136407751));
#55317=CARTESIAN_POINT('Ctrl Pts',(9.92393401731845,-32.4742356128,-1.96001454973233));
#55318=CARTESIAN_POINT('Ctrl Pts',(9.93353796504327,-32.4742356128,-1.80334617365589));
#55319=CARTESIAN_POINT('Ctrl Pts',(9.94166984694101,-32.4742356128,-1.64677964259028));
#55320=CARTESIAN_POINT('Ctrl Pts',(9.94833842889768,-32.4742356128,-1.49021719058124));
#55321=CARTESIAN_POINT('Ctrl Pts',(9.95450935391368,-32.4742356128,-1.34533854052529));
#55322=CARTESIAN_POINT('Ctrl Pts',(9.95942746092287,-32.4742356128,-1.20045751698348));
#55323=CARTESIAN_POINT('Ctrl Pts',(9.96309809061568,-32.4742356128,-1.05549464624314));
#55324=CARTESIAN_POINT('Ctrl Pts',(9.96618761475916,-32.4742356128,-0.933481169934575));
#55325=CARTESIAN_POINT('Ctrl Pts',(9.96839341766342,-32.4742356128,-0.811408131094685));
#55326=CARTESIAN_POINT('Ctrl Pts',(9.96971606220048,-32.4742356128,-0.689268635606535));
#55327=CARTESIAN_POINT('Ctrl Pts',(9.97087661179947,-32.4742356128,-0.582097783168821));
#55328=CARTESIAN_POINT('Ctrl Pts',(9.97135721001099,-32.4742356128,-0.474875416188859));
#55329=CARTESIAN_POINT('Ctrl Pts',(9.9711558159983,-32.4742356128,-0.367641445316077));
#55330=CARTESIAN_POINT('Ctrl Pts',(9.97112768712725,-32.4742356128,-0.352663986460755));
#55331=CARTESIAN_POINT('Ctrl Pts',(9.97108624965007,-32.4742356128,-0.337686384785283));
#55332=CARTESIAN_POINT('Ctrl Pts',(9.97103149360754,-32.4742356128,-0.322708834412021));
#55333=CARTESIAN_POINT('Ctrl Pts',(9.97058233383006,-32.4742356128,-0.199849093595623));
#55334=CARTESIAN_POINT('Ctrl Pts',(9.96923674804115,-32.4742356128,-0.0769878672143817));
#55335=CARTESIAN_POINT('Ctrl Pts',(9.96699184142756,-32.4742356128,0.045914908526925));
#55336=CARTESIAN_POINT('Ctrl Pts',(9.96446705860022,-32.4742356128,0.18414017622627));
#55337=CARTESIAN_POINT('Ctrl Pts',(9.96080479842082,-32.4742356128,0.322417042225777));
#55338=CARTESIAN_POINT('Ctrl Pts',(9.95600414301969,-32.4742356128,0.46073214033741));
#55339=CARTESIAN_POINT('Ctrl Pts',(9.94704210756475,-32.4742356128,0.718943719727021));
#55340=CARTESIAN_POINT('Ctrl Pts',(9.93411358948493,-32.4742356128,0.9772793342408));
#55341=CARTESIAN_POINT('Ctrl Pts',(9.91721974812435,-32.4742356128,1.23541623248458));
#55342=CARTESIAN_POINT('Ctrl Pts',(9.90877282744406,-32.4742356128,1.36448468160648));
#55343=CARTESIAN_POINT('Ctrl Pts',(9.89933452477601,-32.4742356128,1.4935023352826));
#55344=CARTESIAN_POINT('Ctrl Pts',(9.88890261150967,-32.4742356128,1.62246096624871));
#55345=CARTESIAN_POINT('Ctrl Pts',(9.87934749865317,-32.4742356128,1.74058064777235));
#55346=CARTESIAN_POINT('Ctrl Pts',(9.86895881847276,-32.4742356128,1.85865002300787));
#55347=CARTESIAN_POINT('Ctrl Pts',(9.85773224379276,-32.4742356128,1.97670577301818));
#55348=CARTESIAN_POINT('Ctrl Pts',(9.85670206597819,-32.4742356128,1.98753885594941));
#55349=CARTESIAN_POINT('Ctrl Pts',(9.85566483062434,-32.4742356128,1.99837186102877));
#55350=CARTESIAN_POINT('Ctrl Pts',(9.85462053301,-32.4742356128,2.00920484002));
#55351=CARTESIAN_POINT('Ctrl Pts',(8.75956299023,-35.3742356128,2.0634404101));
#55352=CARTESIAN_POINT('Ctrl Pts',(9.5731487029,-32.4742356128,4.05201631342));
#55353=CARTESIAN_POINT('Ctrl Pts',(8.9288627266048,-35.3742356128,1.78605452583546));
#55354=CARTESIAN_POINT('Ctrl Pts',(9.64554803760896,-32.4742356128,3.64899532239734));
#55355=CARTESIAN_POINT('Ctrl Pts',(9.07284086761294,-35.3742356128,1.49321342917581));
#55356=CARTESIAN_POINT('Ctrl Pts',(9.7097825158037,-32.4742356128,3.24450758797157));
#55357=CARTESIAN_POINT('Ctrl Pts',(9.12665675685958,-35.3742356128,1.15111702356286));
#55358=CARTESIAN_POINT('Ctrl Pts',(9.76785698810379,-32.4742356128,2.82296397732709));
#55359=CARTESIAN_POINT('Ctrl Pts',(9.18661000883968,-35.3742356128,0.831274530260112));
#55360=CARTESIAN_POINT('Ctrl Pts',(9.81537216530061,-32.4742356128,2.41636233386422));
#55361=CARTESIAN_POINT('Ctrl Pts',(9.2369929572006,-35.3742356128,0.509811396507259));
#55362=CARTESIAN_POINT('Ctrl Pts',(9.85462971069928,-32.4742356128,2.00910963374492));
#55363=CARTESIAN_POINT('',(9.5731487029,-32.4742356128,4.05201631342));
#55364=CARTESIAN_POINT('',(8.82321723512,-35.1473421125,2.21902487472));
#55365=CARTESIAN_POINT('Ctrl Pts',(9.5731487029,-32.4742356128,4.05201631342));
#55366=CARTESIAN_POINT('Ctrl Pts',(9.58385803994689,-32.4742356128002,3.99240129558575));
#55367=CARTESIAN_POINT('Ctrl Pts',(9.5943536855861,-32.4742356128003,3.93274277792962));
#55368=CARTESIAN_POINT('Ctrl Pts',(9.60464591256779,-32.4742356128005,3.87295958919005));
#55369=CARTESIAN_POINT('Ctrl Pts',(9.61549552175361,-32.4742356128006,3.80993880322598));
#55370=CARTESIAN_POINT('Ctrl Pts',(9.62611903415596,-32.4742356128007,3.74677981964133));
#55371=CARTESIAN_POINT('Ctrl Pts',(9.63652068269621,-32.4742356128008,3.6834457777419));
#55372=CARTESIAN_POINT('Ctrl Pts',(9.64770872862421,-32.4742356128009,3.61532348281571));
#55373=CARTESIAN_POINT('Ctrl Pts',(9.65864002597334,-32.4742356128009,3.5469991384311));
#55374=CARTESIAN_POINT('Ctrl Pts',(9.66931194496842,-32.4742356128009,3.47848631183157));
#55375=CARTESIAN_POINT('Ctrl Pts',(9.68148004640576,-32.474235612801,3.40036811919857));
#55376=CARTESIAN_POINT('Ctrl Pts',(9.69331083177808,-32.474235612801,3.32200562453762));
#55377=CARTESIAN_POINT('Ctrl Pts',(9.70479179824438,-32.4742356128009,3.24348485468374));
#55378=CARTESIAN_POINT('Ctrl Pts',(9.72018567223827,-32.4742356128009,3.13820287859042));
#55379=CARTESIAN_POINT('Ctrl Pts',(9.73495007583224,-32.4742356128008,3.0326400564569));
#55380=CARTESIAN_POINT('Ctrl Pts',(9.74904466851696,-32.4742356128007,2.92708814611498));
#55381=CARTESIAN_POINT('Ctrl Pts',(9.75943548222612,-32.4742356128006,2.84927318107538));
#55382=CARTESIAN_POINT('Ctrl Pts',(9.76946187459548,-32.4742356128006,2.77146717702865));
#55383=CARTESIAN_POINT('Ctrl Pts',(9.77911025980367,-32.4742356128005,2.69377242009859));
#55384=CARTESIAN_POINT('Ctrl Pts',(9.7877997086789,-32.4742356128004,2.62379961079951));
#55385=CARTESIAN_POINT('Ctrl Pts',(9.79618242234148,-32.4742356128003,2.55391804485846));
#55386=CARTESIAN_POINT('Ctrl Pts',(9.80425367824051,-32.4742356128003,2.484167083785));
#55387=CARTESIAN_POINT('Ctrl Pts',(9.81180034779321,-32.4742356128002,2.41894954381484));
#55388=CARTESIAN_POINT('Ctrl Pts',(9.81907464790267,-32.4742356128002,2.35384679982263));
#55389=CARTESIAN_POINT('Ctrl Pts',(9.82607895911491,-32.4742356128001,2.28884751742804));
#55390=CARTESIAN_POINT('Ctrl Pts',(9.83260578437976,-32.4742356128001,2.22827925515719));
#55391=CARTESIAN_POINT('Ctrl Pts',(9.83889814477805,-32.4742356128,2.1678010763369));
#55392=CARTESIAN_POINT('Ctrl Pts',(9.84496431448895,-32.4742356128,2.10735907911611));
#55393=CARTESIAN_POINT('Ctrl Pts',(9.84824849657925,-32.4742356128,2.07463620220458));
#55394=CARTESIAN_POINT('Ctrl Pts',(9.85146649575577,-32.4742356128,2.04192311779301));
#55395=CARTESIAN_POINT('Ctrl Pts',(9.85462053301,-32.4742356128,2.00920484002));
#55396=CARTESIAN_POINT('Ctrl Pts',(8.51721509197,-35.3742356128,2.41066261776));
#55397=CARTESIAN_POINT('Ctrl Pts',(9.47312185748,-32.4742356128,4.57687569684));
#55398=CARTESIAN_POINT('Ctrl Pts',(8.57124548357,-35.3742356128,2.34542388422));
#55399=CARTESIAN_POINT('Ctrl Pts',(9.49423281845,-32.4742356128,4.47213748961));
#55400=CARTESIAN_POINT('Ctrl Pts',(8.62160287869,-35.3742356128,2.27713826199));
#55401=CARTESIAN_POINT('Ctrl Pts',(9.51478914505,-32.4742356128,4.367292468));
#55402=CARTESIAN_POINT('Ctrl Pts',(8.66952448488,-35.3742356128,2.20708948255));
#55403=CARTESIAN_POINT('Ctrl Pts',(9.53482564259,-32.4742356128,4.26215510362));
#55404=CARTESIAN_POINT('Ctrl Pts',(8.71540499967,-35.3742356128,2.13579061508));
#55405=CARTESIAN_POINT('Ctrl Pts',(9.55426490812,-32.4742356128,4.15713558997));
#55406=CARTESIAN_POINT('Ctrl Pts',(8.75956299023,-35.3742356128,2.0634404101));
#55407=CARTESIAN_POINT('Ctrl Pts',(9.5731487029,-32.4742356128,4.05201631342));
#55408=CARTESIAN_POINT('',(9.47312185748,-32.4742356128,4.57687569684));
#55409=CARTESIAN_POINT('',(8.60091083124725,-35.1203221008745,2.60032840068696));
#55410=CARTESIAN_POINT('Origin',(-15.3007564523972,-32.4742356010378,-0.416450801703818));
#55411=CARTESIAN_POINT('Ctrl Pts',(7.21384189758,-35.3742356128,2.18958432614));
#55412=CARTESIAN_POINT('Ctrl Pts',(7.92659403983,-32.4742356128,4.74000601033));
#55413=CARTESIAN_POINT('Ctrl Pts',(7.26623945249,-35.3742356128,2.28696407666));
#55414=CARTESIAN_POINT('Ctrl Pts',(7.98210778857,-32.4742356128,4.86805404157));
#55415=CARTESIAN_POINT('Ctrl Pts',(7.33077888815,-35.3742356128,2.37781046265));
#55416=CARTESIAN_POINT('Ctrl Pts',(8.06503365985,-32.4742356128,4.98421786182));
#55417=CARTESIAN_POINT('Ctrl Pts',(7.40436869293,-35.3742356128,2.46126398331));
#55418=CARTESIAN_POINT('Ctrl Pts',(8.17216612273,-32.4742356128,5.0807589417));
#55419=CARTESIAN_POINT('Ctrl Pts',(7.56704033307,-35.3742356128,2.61160417272));
#55420=CARTESIAN_POINT('Ctrl Pts',(8.41851793763,-32.4742356128,5.22052728604));
#55421=CARTESIAN_POINT('Ctrl Pts',(7.76385631892,-35.3742356128,2.71310420624));
#55422=CARTESIAN_POINT('Ctrl Pts',(8.70021558456,-32.4742356128,5.24806936162));
#55423=CARTESIAN_POINT('Ctrl Pts',(7.87246551919,-35.3742356128,2.74929666995));
#55424=CARTESIAN_POINT('Ctrl Pts',(8.84211900681,-32.4742356128,5.23137961658));
#55425=CARTESIAN_POINT('Ctrl Pts',(8.09632446877,-35.3742356128,2.75144961057));
#55426=CARTESIAN_POINT('Ctrl Pts',(9.10596900702,-32.4742356128,5.14052628192));
#55427=CARTESIAN_POINT('Ctrl Pts',(8.29201770973,-35.3742356128,2.64306639111));
#55428=CARTESIAN_POINT('Ctrl Pts',(9.31107389815,-32.4742356128,4.95155477014));
#55429=CARTESIAN_POINT('Ctrl Pts',(8.37411601908,-35.3742356128,2.57138954697));
#55430=CARTESIAN_POINT('Ctrl Pts',(9.39185739171,-32.4742356128,4.83723274541));
#55431=CARTESIAN_POINT('Ctrl Pts',(8.4486251678,-35.3742356128,2.49348119172));
#55432=CARTESIAN_POINT('Ctrl Pts',(9.44632201614,-32.4742356128,4.7098382487));
#55433=CARTESIAN_POINT('Ctrl Pts',(8.51721509197,-35.3742356128,2.41066261776));
#55434=CARTESIAN_POINT('Ctrl Pts',(9.47312185748,-32.4742356128,4.57687569684));
#55435=CARTESIAN_POINT('Ctrl Pts',(9.47312185748,-32.4742356128,4.57687569684));
#55436=CARTESIAN_POINT('Ctrl Pts',(9.46576357172862,-32.4742356128,4.61338249695149));
#55437=CARTESIAN_POINT('Ctrl Pts',(9.45589852782759,-32.4742356128,4.64938312384879));
#55438=CARTESIAN_POINT('Ctrl Pts',(9.4436151767327,-32.4742356128001,4.68454468695718));
#55439=CARTESIAN_POINT('Ctrl Pts',(9.43116790267184,-32.4742356128001,4.72017548583586));
#55440=CARTESIAN_POINT('Ctrl Pts',(9.41623764589746,-32.4742356128001,4.75494407050594));
#55441=CARTESIAN_POINT('Ctrl Pts',(9.39896958249035,-32.4742356128001,4.78851518953424));
#55442=CARTESIAN_POINT('Ctrl Pts',(9.38152489595556,-32.4742356128002,4.82242968441788));
#55443=CARTESIAN_POINT('Ctrl Pts',(9.36169469208315,-32.4742356128002,4.85512144315062));
#55444=CARTESIAN_POINT('Ctrl Pts',(9.33967747672362,-32.4742356128002,4.88626565542905));
#55445=CARTESIAN_POINT('Ctrl Pts',(9.32473727646168,-32.4742356128002,4.90739915305088));
#55446=CARTESIAN_POINT('Ctrl Pts',(9.30879106644691,-32.4742356128002,4.92782051201125));
#55447=CARTESIAN_POINT('Ctrl Pts',(9.29191215925214,-32.4742356128002,4.94743594307661));
#55448=CARTESIAN_POINT('Ctrl Pts',(9.26807208685844,-32.4742356128001,4.97514113105093));
#55449=CARTESIAN_POINT('Ctrl Pts',(9.2423551960503,-32.4742356128002,5.00125358349318));
#55450=CARTESIAN_POINT('Ctrl Pts',(9.21499925935546,-32.4742356128004,5.02552229400269));
#55451=CARTESIAN_POINT('Ctrl Pts',(9.18812489694226,-32.4742356128005,5.04936377780233));
#55452=CARTESIAN_POINT('Ctrl Pts',(9.15966921110771,-32.4742356128007,5.07142540239296));
#55453=CARTESIAN_POINT('Ctrl Pts',(9.12988757458161,-32.4742356128009,5.09150932334396));
#55454=CARTESIAN_POINT('Ctrl Pts',(9.1177306388397,-32.474235612801,5.09970762823674));
#55455=CARTESIAN_POINT('Ctrl Pts',(9.10535306806464,-32.474235612801,5.1075768984626));
#55456=CARTESIAN_POINT('Ctrl Pts',(9.09277339742187,-32.4742356128011,5.11510591129192));
#55457=CARTESIAN_POINT('Ctrl Pts',(9.06401134948185,-32.4742356128012,5.13232017978011));
#55458=CARTESIAN_POINT('Ctrl Pts',(9.03418916029184,-32.4742356128013,5.1477537113724));
#55459=CARTESIAN_POINT('Ctrl Pts',(9.00352034950314,-32.4742356128012,5.1612883287322));
#55460=CARTESIAN_POINT('Ctrl Pts',(8.98613398992056,-32.4742356128012,5.16896119631913));
#55461=CARTESIAN_POINT('Ctrl Pts',(8.9684764199063,-32.4742356128011,5.17602435236192));
#55462=CARTESIAN_POINT('Ctrl Pts',(8.95059220546224,-32.474235612801,5.1824608849134));
#55463=CARTESIAN_POINT('Ctrl Pts',(8.91460611802292,-32.4742356128007,5.19541228537485));
#55464=CARTESIAN_POINT('Ctrl Pts',(8.8776867278997,-32.4742356128005,5.20582893332123));
#55465=CARTESIAN_POINT('Ctrl Pts',(8.84020622755982,-32.4742356128004,5.21361149973278));
#55466=CARTESIAN_POINT('Ctrl Pts',(8.80212100914067,-32.4742356128002,5.22151963166691));
#55467=CARTESIAN_POINT('Ctrl Pts',(8.76345811848754,-32.4742356128002,5.22670768415973));
#55468=CARTESIAN_POINT('Ctrl Pts',(8.72463030839696,-32.4742356128002,5.22912100680538));
#55469=CARTESIAN_POINT('Ctrl Pts',(8.68739236868495,-32.4742356128002,5.23143551187209));
#55470=CARTESIAN_POINT('Ctrl Pts',(8.65000425691521,-32.4742356128002,5.23119800092422));
#55471=CARTESIAN_POINT('Ctrl Pts',(8.6128267026259,-32.4742356128003,5.22840604118267));
#55472=CARTESIAN_POINT('Ctrl Pts',(8.58737790569537,-32.4742356128003,5.22649488758855));
#55473=CARTESIAN_POINT('Ctrl Pts',(8.56202769486349,-32.4742356128004,5.22338772754605));
#55474=CARTESIAN_POINT('Ctrl Pts',(8.53688547477249,-32.4742356128005,5.21909660544825));
#55475=CARTESIAN_POINT('Ctrl Pts',(8.50390469579943,-32.4742356128006,5.21346764551782));
#55476=CARTESIAN_POINT('Ctrl Pts',(8.47128746528097,-32.4742356128007,5.20580045842078));
#55477=CARTESIAN_POINT('Ctrl Pts',(8.4392653732531,-32.4742356128007,5.19615646079357));
#55478=CARTESIAN_POINT('Ctrl Pts',(8.43597511948344,-32.4742356128007,5.19516554491213));
#55479=CARTESIAN_POINT('Ctrl Pts',(8.43269111740371,-32.4742356128007,5.19415379222059));
#55480=CARTESIAN_POINT('Ctrl Pts',(8.42941359545578,-32.4742356128007,5.19312129233961));
#55481=CARTESIAN_POINT('Ctrl Pts',(8.3944144019285,-32.4742356128007,5.18209568710319));
#55482=CARTESIAN_POINT('Ctrl Pts',(8.36015521648491,-32.4742356128006,5.16869999519598));
#55483=CARTESIAN_POINT('Ctrl Pts',(8.32695087107122,-32.4742356128006,5.15305321371686));
#55484=CARTESIAN_POINT('Ctrl Pts',(8.29319095413242,-32.4742356128005,5.13714463197815));
#55485=CARTESIAN_POINT('Ctrl Pts',(8.26052202447813,-32.4742356128004,5.11890928463567));
#55486=CARTESIAN_POINT('Ctrl Pts',(8.22925624736326,-32.4742356128004,5.09852305936231));
#55487=CARTESIAN_POINT('Ctrl Pts',(8.20513847568554,-32.4742356128003,5.08279754821614));
#55488=CARTESIAN_POINT('Ctrl Pts',(8.18185530346072,-32.4742356128002,5.06579330067018));
#55489=CARTESIAN_POINT('Ctrl Pts',(8.15953944897647,-32.4742356128002,5.04760937719499));
#55490=CARTESIAN_POINT('Ctrl Pts',(8.13000306159537,-32.4742356128001,5.02354185120129));
#55491=CARTESIAN_POINT('Ctrl Pts',(8.1021534308539,-32.4742356128001,4.99739923287759));
#55492=CARTESIAN_POINT('Ctrl Pts',(8.07626720330521,-32.4742356128001,4.96943994770265));
#55493=CARTESIAN_POINT('Ctrl Pts',(8.0505351356036,-32.4742356128,4.94164716802253));
#55494=CARTESIAN_POINT('Ctrl Pts',(8.0267436078806,-32.4742356128,4.91205976688404));
#55495=CARTESIAN_POINT('Ctrl Pts',(8.00512575620472,-32.4742356128,4.88096523499291));
#55496=CARTESIAN_POINT('Ctrl Pts',(7.98386071885989,-32.4742356128,4.85037818167243));
#55497=CARTESIAN_POINT('Ctrl Pts',(7.96469932551459,-32.4742356128,4.81833327235114));
#55498=CARTESIAN_POINT('Ctrl Pts',(7.94782028391973,-32.4742356128,4.78512968374919));
#55499=CARTESIAN_POINT('Ctrl Pts',(7.94028653932774,-32.4742356128,4.77030968614097));
#55500=CARTESIAN_POINT('Ctrl Pts',(7.93320686704621,-32.4742356128,4.75525915977829));
#55501=CARTESIAN_POINT('Ctrl Pts',(7.92659403983,-32.4742356128,4.74000601033));
#55502=CARTESIAN_POINT('Origin',(-11.4022814987,-32.6742356128,-7.54785992694));
#55503=CARTESIAN_POINT('Origin',(-11.4022814987,-32.8742356128,-7.54785992694));
#55504=CARTESIAN_POINT('Ctrl Pts',(3.51985615629,-35.3742356128,-3.20601908088));
#55505=CARTESIAN_POINT('Ctrl Pts',(3.1350457731,-32.4742356128,-2.57376246377));
#55506=CARTESIAN_POINT('Ctrl Pts',(3.5389561844,-35.3742356128,-3.1668368061));
#55507=CARTESIAN_POINT('Ctrl Pts',(3.17276903042,-32.4742356128,-2.53334077836));
#55508=CARTESIAN_POINT('Ctrl Pts',(3.56517269185,-35.3742356128,-3.13112318899));
#55509=CARTESIAN_POINT('Ctrl Pts',(3.21038331308,-32.4742356128,-2.49281798697));
#55510=CARTESIAN_POINT('Ctrl Pts',(3.59940527056,-35.3742356128,-3.09917422736));
#55511=CARTESIAN_POINT('Ctrl Pts',(3.24932685202,-32.4742356128,-2.45063230102));
#55512=CARTESIAN_POINT('Ctrl Pts',(3.63699355357,-35.3742356128,-3.07546800882));
#55513=CARTESIAN_POINT('Ctrl Pts',(3.28665002885,-32.4742356128,-2.40998048911));
#55514=CARTESIAN_POINT('Ctrl Pts',(3.67755401867,-35.3742356128,-3.05915055738));
#55515=CARTESIAN_POINT('Ctrl Pts',(3.32386409198,-32.4742356128,-2.36922853848));
#55516=CARTESIAN_POINT('Origin',(-15.769898679409,-32.4742355606854,15.0680202722476));
#55517=CARTESIAN_POINT('Ctrl Pts',(-1.68475792039,-35.3742356128,-5.03973467448));
#55518=CARTESIAN_POINT('Ctrl Pts',(-0.682166339124,-32.4742356128,-4.8790713724));
#55519=CARTESIAN_POINT('Ctrl Pts',(-2.15538022242,-35.3742356128,-4.8080213959));
#55520=CARTESIAN_POINT('Ctrl Pts',(-1.20736921572,-32.4742356128,-4.44659694115));
#55521=CARTESIAN_POINT('Ctrl Pts',(-2.59973387128,-35.3742356128,-4.50528924317));
#55522=CARTESIAN_POINT('Ctrl Pts',(-1.71079094607,-32.4742356128,-4.00290111016));
#55523=CARTESIAN_POINT('Ctrl Pts',(-2.98121657961,-35.3742356128,-4.12686323533));
#55524=CARTESIAN_POINT('Ctrl Pts',(-2.19825830329,-32.4742356128,-3.54512092123));
#55525=CARTESIAN_POINT('Ctrl Pts',(-3.28679922947,-35.3742356128,-3.68411804659));
#55526=CARTESIAN_POINT('Ctrl Pts',(-2.67474264449,-32.4742356128,-3.06699209341));
#55527=CARTESIAN_POINT('Ctrl Pts',(-3.51985615629,-35.3742356128,-3.20601908088));
#55528=CARTESIAN_POINT('Ctrl Pts',(-3.1350457731,-32.4742356128,-2.57376246377));
#55529=CARTESIAN_POINT('',(-0.682166339124,-32.4742356128,-4.8790713724));
#55530=CARTESIAN_POINT('Ctrl Pts',(-3.1350457731,-32.4742356128,-2.57376246377));
#55531=CARTESIAN_POINT('Ctrl Pts',(-3.04574386842478,-32.4742356128,-2.66945233123215));
#55532=CARTESIAN_POINT('Ctrl Pts',(-2.95565520899676,-32.4742356128,-2.76451972688002));
#55533=CARTESIAN_POINT('Ctrl Pts',(-2.86486097840212,-32.4742356128,-2.85887905523607));
#55534=CARTESIAN_POINT('Ctrl Pts',(-2.76926551199805,-32.4742356128,-2.95822814321991));
#55535=CARTESIAN_POINT('Ctrl Pts',(-2.67288792014402,-32.4742356128,-3.05679239893703));
#55536=CARTESIAN_POINT('Ctrl Pts',(-2.57578459070286,-32.4742356128,-3.15451622941541));
#55537=CARTESIAN_POINT('Ctrl Pts',(-2.47439813201672,-32.4742356128001,
-3.25655055880935));
#55538=CARTESIAN_POINT('Ctrl Pts',(-2.37222039913981,-32.4742356128001,
-3.35766900818225));
#55539=CARTESIAN_POINT('Ctrl Pts',(-2.2692753175773,-32.4742356128001,-3.45785202544386));
#55540=CARTESIAN_POINT('Ctrl Pts',(-2.16032661276555,-32.4742356128001,
-3.56387758595748));
#55541=CARTESIAN_POINT('Ctrl Pts',(-2.05051830060976,-32.4742356128001,
-3.66885589509191));
#55542=CARTESIAN_POINT('Ctrl Pts',(-1.93983639318639,-32.4742356128001,
-3.77280566427766));
#55543=CARTESIAN_POINT('Ctrl Pts',(-1.81352928403153,-32.4742356128001,
-3.89143024483304));
#55544=CARTESIAN_POINT('Ctrl Pts',(-1.68608466211416,-32.4742356128001,
-4.00871596374921));
#55545=CARTESIAN_POINT('Ctrl Pts',(-1.55742711564637,-32.4742356128001,
-4.1247361422481));
#55546=CARTESIAN_POINT('Ctrl Pts',(-1.40954803390843,-32.4742356128001,
-4.25808982363347));
#55547=CARTESIAN_POINT('Ctrl Pts',(-1.26006594487636,-32.4742356128001,
-4.38977385603739));
#55548=CARTESIAN_POINT('Ctrl Pts',(-1.10880104134623,-32.4742356128001,
-4.51993332529904));
#55549=CARTESIAN_POINT('Ctrl Pts',(-0.968189500144993,-32.4742356128001,
-4.64092585659807));
#55550=CARTESIAN_POINT('Ctrl Pts',(-0.826035174351419,-32.4742356128001,
-4.760603642191));
#55551=CARTESIAN_POINT('Ctrl Pts',(-0.682166339124,-32.4742356128,-4.8790713724));
#55552=CARTESIAN_POINT('',(-1.65073607089,-35.2758272825,-5.03428274092));
#55553=CARTESIAN_POINT('Ctrl Pts',(-1.51727342606,-35.3742356128,-5.3088808072));
#55554=CARTESIAN_POINT('Ctrl Pts',(-0.5,-32.4742356128,-5.26505293156));
#55555=CARTESIAN_POINT('Ctrl Pts',(-1.51727346704,-35.3742356128,-5.24111839755));
#55556=CARTESIAN_POINT('Ctrl Pts',(-0.49999996933,-32.4742356128,-5.17707576222));
#55557=CARTESIAN_POINT('Ctrl Pts',(-1.53640667867,-35.3742356128,-5.1734830193));
#55558=CARTESIAN_POINT('Ctrl Pts',(-0.519349085752,-32.4742356128,-5.08894068096));
#55559=CARTESIAN_POINT('Ctrl Pts',(-1.57167084987,-35.3742356128,-5.11676901693));
#55560=CARTESIAN_POINT('Ctrl Pts',(-0.558553592228,-32.4742356128,-5.00590412413));
#55561=CARTESIAN_POINT('Ctrl Pts',(-1.62392373781,-35.3742356128,-5.06968674937));
#55562=CARTESIAN_POINT('Ctrl Pts',(-0.614278309582,-32.4742356128,-4.93497322721));
#55563=CARTESIAN_POINT('Ctrl Pts',(-1.68475792039,-35.3742356128,-5.03973467448));
#55564=CARTESIAN_POINT('Ctrl Pts',(-0.682166339124,-32.4742356128,-4.8790713724));
#55565=CARTESIAN_POINT('Ctrl Pts',(-0.5,-32.4742356128,-5.26505293156));
#55566=CARTESIAN_POINT('Ctrl Pts',(-0.499999987183553,-32.4742356128,-5.22828883820323));
#55567=CARTESIAN_POINT('Ctrl Pts',(-0.504054600653073,-32.4742356128085,
-5.19170069064497));
#55568=CARTESIAN_POINT('Ctrl Pts',(-0.520156709880915,-32.4742356128085,
-5.1199141043431));
#55569=CARTESIAN_POINT('Ctrl Pts',(-0.532168073174417,-32.4742356128085,
-5.08496970255448));
#55570=CARTESIAN_POINT('Ctrl Pts',(-0.56359844412932,-32.4742356128085,
-5.0183737839542));
#55571=CARTESIAN_POINT('Ctrl Pts',(-0.582941481982889,-32.4742356128085,
-4.98688524144264));
#55572=CARTESIAN_POINT('Ctrl Pts',(-0.628123824966223,-32.4742356128085,
-4.9288235651309));
#55573=CARTESIAN_POINT('Ctrl Pts',(-0.653788606277979,-32.4742356128,-4.90243878948513));
#55574=CARTESIAN_POINT('Ctrl Pts',(-0.682166339124,-32.4742356128,-4.8790713724));
#55575=CARTESIAN_POINT('Ctrl Pts',(-4.28541380927,-35.2854532781,6.68742874581));
#55576=CARTESIAN_POINT('Ctrl Pts',(-4.25138913038,-35.3190062343,6.67597344224));
#55577=CARTESIAN_POINT('Ctrl Pts',(-4.2237811371,-35.3599069399,6.66698101926));
#55578=CARTESIAN_POINT('Ctrl Pts',(-4.2045020858,-35.4062855354,6.66109563973));
#55579=CARTESIAN_POINT('Ctrl Pts',(-4.19468576835,-35.4554145177,6.65866342004));
#55580=CARTESIAN_POINT('Ctrl Pts',(-4.1943405118,-35.5045435,6.65962650016));
#55581=CARTESIAN_POINT('Ctrl Pts',(-4.11397205127,-35.2871903778,7.1289134397));
#55582=CARTESIAN_POINT('Ctrl Pts',(-4.08555020042,-35.3204422988,7.11511826715));
#55583=CARTESIAN_POINT('Ctrl Pts',(-4.06274263182,-35.3595779076,7.10432325981));
#55584=CARTESIAN_POINT('Ctrl Pts',(-4.04686969309,-35.4030115592,7.09721073519));
#55585=CARTESIAN_POINT('Ctrl Pts',(-4.03869401208,-35.448599951,7.09414682081));
#55586=CARTESIAN_POINT('Ctrl Pts',(-4.0382327119,-35.4941883428,7.09508332647));
#55587=CARTESIAN_POINT('Ctrl Pts',(-3.87798979897,-35.2903697142,7.5452931056));
#55588=CARTESIAN_POINT('Ctrl Pts',(-3.85569645887,-35.322762315,7.53067170905));
#55589=CARTESIAN_POINT('Ctrl Pts',(-3.8380083558,-35.3595811789,7.5193382333));
#55590=CARTESIAN_POINT('Ctrl Pts',(-3.82572295419,-35.3995642149,7.51187390423));
#55591=CARTESIAN_POINT('Ctrl Pts',(-3.81928961916,-35.4411316076,7.50858298657));
#55592=CARTESIAN_POINT('Ctrl Pts',(-3.81872923728,-35.4826990003,7.50943133393));
#55593=CARTESIAN_POINT('Ctrl Pts',(-3.58317382243,-35.2955286211,7.92387042867));
#55594=CARTESIAN_POINT('Ctrl Pts',(-3.566682617,-35.3261714515,7.91016667743));
#55595=CARTESIAN_POINT('Ctrl Pts',(-3.5536607286,-35.359954842,7.89965095547));
#55596=CARTESIAN_POINT('Ctrl Pts',(-3.54456703401,-35.395950925,7.89273240615));
#55597=CARTESIAN_POINT('Ctrl Pts',(-3.53965943927,-35.4330544417,7.88962174402));
#55598=CARTESIAN_POINT('Ctrl Pts',(-3.53895593719,-35.4701579585,7.89029829102));
#55599=CARTESIAN_POINT('Ctrl Pts',(-2.78825930398,-35.3119546911,8.68818242005));
#55600=CARTESIAN_POINT('Ctrl Pts',(-2.78273620813,-35.3367578784,8.67851811171));
#55601=CARTESIAN_POINT('Ctrl Pts',(-2.77847903433,-35.3625424695,8.67123634585));
#55602=CARTESIAN_POINT('Ctrl Pts',(-2.77550319185,-35.3889828306,8.66644973332));
#55603=CARTESIAN_POINT('Ctrl Pts',(-2.77381592126,-35.4157508538,8.66421370085));
#55604=CARTESIAN_POINT('Ctrl Pts',(-2.77342331871,-35.442518877,8.6645265191));
#55605=CARTESIAN_POINT('Ctrl Pts',(-1.7897157019,-35.3293337971,9.16292213266));
#55606=CARTESIAN_POINT('Ctrl Pts',(-1.78817752192,-35.3471147636,9.15782929567));
#55607=CARTESIAN_POINT('Ctrl Pts',(-1.78691123053,-35.3652255624,9.15399062253));
#55608=CARTESIAN_POINT('Ctrl Pts',(-1.78592585783,-35.383560442,9.15142772658));
#55609=CARTESIAN_POINT('Ctrl Pts',(-1.78522811689,-35.4020074661,9.15015177013));
#55610=CARTESIAN_POINT('Ctrl Pts',(-1.78481951479,-35.4204544903,9.15016319792));
#55611=CARTESIAN_POINT('Ctrl Pts',(-1.17958127456,-35.3376427744,9.32328709823));
#55612=CARTESIAN_POINT('Ctrl Pts',(-1.17951808488,-35.3526513961,9.31932369186));
#55613=CARTESIAN_POINT('Ctrl Pts',(-1.17962222045,-35.3679411233,9.31634876039));
#55614=CARTESIAN_POINT('Ctrl Pts',(-1.17989211248,-35.3834200246,9.31438871901));
#55615=CARTESIAN_POINT('Ctrl Pts',(-1.18032484655,-35.3989934955,9.31345658462));
#55616=CARTESIAN_POINT('Ctrl Pts',(-1.18091694182,-35.4145669664,9.31355164802));
#55617=CARTESIAN_POINT('Ctrl Pts',(-0.559260434794,-35.3376563848,9.36581532526));
#55618=CARTESIAN_POINT('Ctrl Pts',(-0.558548188498,-35.3519108871,9.36216300672));
#55619=CARTESIAN_POINT('Ctrl Pts',(-0.557879709548,-35.3663773783,9.35938680253));
#55620=CARTESIAN_POINT('Ctrl Pts',(-0.557259801436,-35.3809865088,9.35750427431));
#55621=CARTESIAN_POINT('Ctrl Pts',(-0.556692506327,-35.395666961,9.35652455583));
#55622=CARTESIAN_POINT('Ctrl Pts',(-0.556180950878,-35.4103474131,9.35644810405));
#55623=CARTESIAN_POINT('Ctrl Pts',(0.051310852811,-35.3354014219,9.29455995377));
#55624=CARTESIAN_POINT('Ctrl Pts',(0.0507151654701,-35.3508336959,9.290385971));
#55625=CARTESIAN_POINT('Ctrl Pts',(0.050239745093,-35.3665469388,9.28723363732));
#55626=CARTESIAN_POINT('Ctrl Pts',(0.0498881224817,-35.3824497265,9.28512769558));
#55627=CARTESIAN_POINT('Ctrl Pts',(0.0496623930249,-35.3984472911,9.28408069549));
#55628=CARTESIAN_POINT('Ctrl Pts',(0.0495631429636,-35.4144448557,9.28409255206));
#55629=CARTESIAN_POINT('',(-4.19434053880571,-35.5045435019704,6.65962642488774));
#55630=CARTESIAN_POINT('',(1.28564320474754E-7,-35.4141727791362,9.28969993583948));
#55631=CARTESIAN_POINT('Ctrl Pts',(-4.1943405118,-35.5045435,6.65962650016));
#55632=CARTESIAN_POINT('Ctrl Pts',(-4.17837930200538,-35.5034847390595,
6.70414969352822));
#55633=CARTESIAN_POINT('Ctrl Pts',(-4.16055959096817,-35.5023336268611,
6.75138464945794));
#55634=CARTESIAN_POINT('Ctrl Pts',(-4.14055681322333,-35.501089684398,6.80116841245276));
#55635=CARTESIAN_POINT('Ctrl Pts',(-4.12081028160109,-35.4998616774933,
6.85031441921199));
#55636=CARTESIAN_POINT('Ctrl Pts',(-4.09893583753898,-35.4985431603648,
6.9019447557283));
#55637=CARTESIAN_POINT('Ctrl Pts',(-4.07459349579852,-35.4971338643656,
6.95586055718833));
#55638=CARTESIAN_POINT('Ctrl Pts',(-4.05079014661857,-35.4957557732549,
7.00858254516111));
#55639=CARTESIAN_POINT('Ctrl Pts',(-4.02462648621315,-35.4942908306056,
7.06349021451113));
#55640=CARTESIAN_POINT('Ctrl Pts',(-3.99576468989804,-35.4927396443495,
7.12035197690877));
#55641=CARTESIAN_POINT('Ctrl Pts',(-3.98674519606888,-35.4922548888369,
7.13812163717041));
#55642=CARTESIAN_POINT('Ctrl Pts',(-3.97746208240242,-35.4917617201085,
7.15608177491406));
#55643=CARTESIAN_POINT('Ctrl Pts',(-3.96790474909657,-35.4912601864692,
7.17422430572546));
#55644=CARTESIAN_POINT('Ctrl Pts',(-3.93844658680729,-35.4897143306466,
7.23014425743976));
#55645=CARTESIAN_POINT('Ctrl Pts',(-3.90638395378748,-35.4880887908298,
7.28780020932287));
#55646=CARTESIAN_POINT('Ctrl Pts',(-3.8714013263532,-35.4863824392708,7.3469238129564));
#55647=CARTESIAN_POINT('Ctrl Pts',(-3.84516841075404,-35.4851028733916,
7.3912596624277));
#55648=CARTESIAN_POINT('Ctrl Pts',(-3.81729326251427,-35.4837779059508,
7.43641988355906));
#55649=CARTESIAN_POINT('Ctrl Pts',(-3.78764191907141,-35.4824082052946,
7.48227203951716));
#55650=CARTESIAN_POINT('Ctrl Pts',(-3.753045629466,-35.4808100800473,7.53577094656048));
#55651=CARTESIAN_POINT('Ctrl Pts',(-3.7160309687385,-35.4791503927134,7.5902128072203));
#55652=CARTESIAN_POINT('Ctrl Pts',(-3.6763871268798,-35.477419112457,7.64535684101877));
#55653=CARTESIAN_POINT('Ctrl Pts',(-3.65839989873091,-35.4766335949213,
7.67037682572456));
#55654=CARTESIAN_POINT('Ctrl Pts',(-3.64011367909671,-35.4758458242437,
7.69521128373181));
#55655=CARTESIAN_POINT('Ctrl Pts',(-3.62118640362598,-35.4750423837516,
7.72028918556664));
#55656=CARTESIAN_POINT('Ctrl Pts',(-3.60273483893631,-35.4742591366203,
7.7447367891693));
#55657=CARTESIAN_POINT('Ctrl Pts',(-3.58367398448364,-35.4734609836787,
7.76941596024569));
#55658=CARTESIAN_POINT('Ctrl Pts',(-3.56364805841191,-35.4726355159181,
7.79469365798657));
#55659=CARTESIAN_POINT('Ctrl Pts',(-3.55894115415355,-35.4724414975389,
7.80063494143642));
#55660=CARTESIAN_POINT('Ctrl Pts',(-3.55418076305494,-35.4722459707925,
7.80660914540214));
#55661=CARTESIAN_POINT('Ctrl Pts',(-3.54936194187392,-35.4720487760647,
7.812620756905));
#55662=CARTESIAN_POINT('Ctrl Pts',(-3.50132504757105,-35.4700830209682,
7.87254809919573));
#55663=CARTESIAN_POINT('Ctrl Pts',(-3.45312102456255,-35.4681824662924,
7.92915836150545));
#55664=CARTESIAN_POINT('Ctrl Pts',(-3.40514157153254,-35.4663543570109,
7.98262940663339));
#55665=CARTESIAN_POINT('Ctrl Pts',(-3.3545301321423,-35.4644259639957,8.03903368781461));
#55666=CARTESIAN_POINT('Ctrl Pts',(-3.30416891042736,-35.4625781811888,
8.09194534533543));
#55667=CARTESIAN_POINT('Ctrl Pts',(-3.2544613417438,-35.4608154968839,8.14159549761834));
#55668=CARTESIAN_POINT('Ctrl Pts',(-3.20479882986081,-35.4590544103421,
8.19120064514505));
#55669=CARTESIAN_POINT('Ctrl Pts',(-3.15578853664244,-35.4573782131692,
8.23755081827941));
#55670=CARTESIAN_POINT('Ctrl Pts',(-3.10777820415445,-35.4557879751255,
8.28088966193874));
#55671=CARTESIAN_POINT('Ctrl Pts',(-3.05787405529245,-35.4541350085255,
8.32593805034603));
#55672=CARTESIAN_POINT('Ctrl Pts',(-3.0090492646001,-35.4525748349097,8.36773430141987));
#55673=CARTESIAN_POINT('Ctrl Pts',(-2.96164060662634,-35.4511058720778,
8.40655378230749));
#55674=CARTESIAN_POINT('Ctrl Pts',(-2.91770603913525,-35.4497445543473,
8.44252858471531));
#55675=CARTESIAN_POINT('Ctrl Pts',(-2.87498738991999,-35.4484615152779,
8.47594687353619));
#55676=CARTESIAN_POINT('Ctrl Pts',(-2.83371152617201,-35.4472539635573,
8.50702594740405));
#55677=CARTESIAN_POINT('Ctrl Pts',(-2.7881274088724,-35.4459203711313,8.54134896381397));
#55678=CARTESIAN_POINT('Ctrl Pts',(-2.74430435080188,-35.4446791995284,
8.57281938357731));
#55679=CARTESIAN_POINT('Ctrl Pts',(-2.70250195888283,-35.4435296775847,
8.60172084488821));
#55680=CARTESIAN_POINT('Ctrl Pts',(-2.66331221645872,-35.4424520007626,
8.62881596486717));
#55681=CARTESIAN_POINT('Ctrl Pts',(-2.62589740734801,-35.4414547032728,
8.65365341888502));
#55682=CARTESIAN_POINT('Ctrl Pts',(-2.59043271192644,-35.4405342286928,
8.67645002768075));
#55683=CARTESIAN_POINT('Ctrl Pts',(-2.58212067393701,-35.4403184924631,
8.68179298286726));
#55684=CARTESIAN_POINT('Ctrl Pts',(-2.57391560780485,-35.4401069682295,
8.68702375355189));
#55685=CARTESIAN_POINT('Ctrl Pts',(-2.56581950543256,-35.4398995977304,
8.69214497970277));
#55686=CARTESIAN_POINT('Ctrl Pts',(-2.56543203379652,-35.4398896731787,
8.69239007663757));
#55687=CARTESIAN_POINT('Ctrl Pts',(-2.56504481172373,-35.4398797581405,
8.69263492264965));
#55688=CARTESIAN_POINT('Ctrl Pts',(-2.56465783942697,-35.4398698526091,
8.69287951802502));
#55689=CARTESIAN_POINT('Ctrl Pts',(-2.56441498501931,-35.4398636361384,
8.69303302013744));
#55690=CARTESIAN_POINT('Ctrl Pts',(-2.56417222898623,-35.439857423412,8.69318642353627));
#55691=CARTESIAN_POINT('Ctrl Pts',(-2.56392957138023,-35.4398512144283,
8.69333972829214));
#55692=CARTESIAN_POINT('Ctrl Pts',(-2.56376214454781,-35.4398469304065,
8.69344550420451));
#55693=CARTESIAN_POINT('Ctrl Pts',(-2.56359473338293,-35.4398426473919,
8.69355125215866));
#55694=CARTESIAN_POINT('Ctrl Pts',(-2.56343784477848,-35.4398386340855,
8.69365033845224));
#55695=CARTESIAN_POINT('Ctrl Pts',(-2.56250776449831,-35.4398148420632,
8.69423775018949));
#55696=CARTESIAN_POINT('Ctrl Pts',(-2.56183838046285,-35.439797731233,8.69466014382177));
#55697=CARTESIAN_POINT('Ctrl Pts',(-2.56096334291628,-35.4397753772487,
8.69521189922955));
#55698=CARTESIAN_POINT('Ctrl Pts',(-2.56052667867185,-35.4397642220867,
8.6954872381098));
#55699=CARTESIAN_POINT('Ctrl Pts',(-2.56003879045694,-35.4397517617935,
8.69579477361531));
#55700=CARTESIAN_POINT('Ctrl Pts',(-2.55944163055637,-35.4397365191539,
8.69617093880344));
#55701=CARTESIAN_POINT('Ctrl Pts',(-2.55918938502879,-35.4397300805305,
8.69632983424542));
#55702=CARTESIAN_POINT('Ctrl Pts',(-2.55891764121507,-35.4397231455062,
8.69650097358499));
#55703=CARTESIAN_POINT('Ctrl Pts',(-2.55862201831283,-35.439715603024,8.69668709372278));
#55704=CARTESIAN_POINT('Ctrl Pts',(-2.55841357168626,-35.4397102847453,
8.69681832886919));
#55705=CARTESIAN_POINT('Ctrl Pts',(-2.55819325278148,-35.4397046644545,
8.6969570120502));
#55706=CARTESIAN_POINT('Ctrl Pts',(-2.55795952442937,-35.4396987032875,
8.69710410051035));
#55707=CARTESIAN_POINT('Ctrl Pts',(-2.55777101635765,-35.4396938954494,
8.69722273122736));
#55708=CARTESIAN_POINT('Ctrl Pts',(-2.55757624887405,-35.4396889287289,
8.69734527846241));
#55709=CARTESIAN_POINT('Ctrl Pts',(-2.55738401031714,-35.4396840272794,
8.69746621131631));
#55710=CARTESIAN_POINT('Ctrl Pts',(-2.46893434127246,-35.4374288522792,
8.75310786341616));
#55711=CARTESIAN_POINT('Ctrl Pts',(-2.37904006043683,-35.4353007995903,
8.80483067803399));
#55712=CARTESIAN_POINT('Ctrl Pts',(-2.28808612479403,-35.4333174785345,
8.85264623177789));
#55713=CARTESIAN_POINT('Ctrl Pts',(-2.19146999759537,-35.4312106890036,
8.90343846621994));
#55714=CARTESIAN_POINT('Ctrl Pts',(-2.09365805541918,-35.4292668399415,
8.9498217080444));
#55715=CARTESIAN_POINT('Ctrl Pts',(-1.99507393204673,-35.4274916884687,
8.99185359254555));
#55716=CARTESIAN_POINT('Ctrl Pts',(-1.89277409786276,-35.4256496301829,
9.03546969083616));
#55717=CARTESIAN_POINT('Ctrl Pts',(-1.78964251137895,-35.4239887620901,
9.07440034576536));
#55718=CARTESIAN_POINT('Ctrl Pts',(-1.68611634000585,-35.4225062084511,
9.10875546973269));
#55719=CARTESIAN_POINT('Ctrl Pts',(-1.5875040832196,-35.4210940248629,9.14147991285326));
#55720=CARTESIAN_POINT('Ctrl Pts',(-1.48853326431828,-35.4198432538259,
9.17005348776741));
#55721=CARTESIAN_POINT('Ctrl Pts',(-1.38955619837585,-35.4187494160414,
9.1946054037486));
#55722=CARTESIAN_POINT('Ctrl Pts',(-1.31611675982145,-35.4179378054729,
9.21282254231424));
#55723=CARTESIAN_POINT('Ctrl Pts',(-1.24267047477725,-35.4172125277507,
9.22882666254555));
#55724=CARTESIAN_POINT('Ctrl Pts',(-1.16937199814094,-35.4165726765175,
9.24267804009084));
#55725=CARTESIAN_POINT('Ctrl Pts',(-1.04699987075702,-35.4155044420848,
9.2658029754947));
#55726=CARTESIAN_POINT('Ctrl Pts',(-0.925027460321667,-35.4146731250409,
9.28293054387911));
#55727=CARTESIAN_POINT('Ctrl Pts',(-0.803994903273425,-35.414083580067,
9.29440967641859));
#55728=CARTESIAN_POINT('Ctrl Pts',(-0.677910364703607,-35.4134694270836,
9.30636795578342));
#55729=CARTESIAN_POINT('Ctrl Pts',(-0.552845273492524,-35.4131170907703,
9.31219700428478));
#55730=CARTESIAN_POINT('Ctrl Pts',(-0.429367066302641,-35.4130544209605,
9.31232207470645));
#55731=CARTESIAN_POINT('Ctrl Pts',(-0.299788995201549,-35.4129886552416,
9.31245332364794));
#55732=CARTESIAN_POINT('Ctrl Pts',(-0.171958012842119,-35.4132413396774,
9.30630375762155));
#55733=CARTESIAN_POINT('Ctrl Pts',(-0.0464907907025172,-35.4138776107364,
9.29438835716944));
#55734=CARTESIAN_POINT('Ctrl Pts',(-0.030957288939788,-35.4139563844387,
9.29291316794655));
#55735=CARTESIAN_POINT('Ctrl Pts',(-0.0154599763576345,-35.4140410829517,
9.29134962256341));
#55736=CARTESIAN_POINT('Ctrl Pts',(1.08019642119928E-8,-35.4141318686722,
9.28969871436959));
#55737=CARTESIAN_POINT('',(-4.28541381254212,-35.2854532749087,6.68742874666406));
#55738=CARTESIAN_POINT('Origin',(-4.4767627864762,-35.5045528948602,6.76087185974608));
#55739=CARTESIAN_POINT('',(6.71017130748908E-10,-35.3356164375956,9.30022551106375));
#55740=CARTESIAN_POINT('Ctrl Pts',(-4.28541380927,-35.2854532781,6.68742874581));
#55741=CARTESIAN_POINT('Ctrl Pts',(-4.24121616134092,-35.2859025484266,
6.80123908869553));
#55742=CARTESIAN_POINT('Ctrl Pts',(-4.19186847493088,-35.2864674277753,
6.91304437631602));
#55743=CARTESIAN_POINT('Ctrl Pts',(-4.13760176200921,-35.2871642627959,
7.02239230617209));
#55744=CARTESIAN_POINT('Ctrl Pts',(-4.08296289616635,-35.2878658766059,
7.13249012761604));
#55745=CARTESIAN_POINT('Ctrl Pts',(-4.0233374286172,-35.2887014167807,7.24009677953585));
#55746=CARTESIAN_POINT('Ctrl Pts',(-3.95899998176384,-35.2896788346738,
7.34478595162515));
#55747=CARTESIAN_POINT('Ctrl Pts',(-3.89400268928686,-35.2906662769765,
7.4505488171142));
#55748=CARTESIAN_POINT('Ctrl Pts',(-3.82419638177896,-35.2917986928545,
7.55333404201523));
#55749=CARTESIAN_POINT('Ctrl Pts',(-3.74990195024538,-35.293072923249,7.65273807851349));
#55750=CARTESIAN_POINT('Ctrl Pts',(-3.70090134743733,-35.2939133369403,
7.71829962342909));
#55751=CARTESIAN_POINT('Ctrl Pts',(-3.64994917793588,-35.2948152022339,
7.78239108781155));
#55752=CARTESIAN_POINT('Ctrl Pts',(-3.59714596398303,-35.2957744035521,
7.844905146357));
#55753=CARTESIAN_POINT('Ctrl Pts',(-3.51612022470366,-35.2972462835781,
7.94083203091221));
#55754=CARTESIAN_POINT('Ctrl Pts',(-3.43073437116214,-35.2988540402996,
8.03304296381226));
#55755=CARTESIAN_POINT('Ctrl Pts',(-3.34138037370368,-35.3005693892819,
8.12118035250671));
#55756=CARTESIAN_POINT('Ctrl Pts',(-3.25130839572758,-35.3022985214993,
8.21002594597945));
#55757=CARTESIAN_POINT('Ctrl Pts',(-3.15720439860138,-35.3041371751793,
8.29473227506716));
#55758=CARTESIAN_POINT('Ctrl Pts',(-3.05950307372847,-35.306037411305,8.37496990585234));
#55759=CARTESIAN_POINT('Ctrl Pts',(-2.99330872457544,-35.3073248543745,
8.42933229811585));
#55760=CARTESIAN_POINT('Ctrl Pts',(-2.92546378256917,-35.3086401700654,
8.48164418952771));
#55761=CARTESIAN_POINT('Ctrl Pts',(-2.85611143541241,-35.3099628824964,
8.53181257836513));
#55762=CARTESIAN_POINT('Ctrl Pts',(-2.7579102438772,-35.3118358102646,8.60284976402952));
#55763=CARTESIAN_POINT('Ctrl Pts',(-2.65668403889593,-35.3137240757601,
8.6695883304476));
#55764=CARTESIAN_POINT('Ctrl Pts',(-2.55280108748868,-35.3155893473178,
8.73178544516782));
#55765=CARTESIAN_POINT('Ctrl Pts',(-2.44221408927618,-35.3175749934669,
8.79799642705862));
#55766=CARTESIAN_POINT('Ctrl Pts',(-2.32861692417884,-35.3195340519872,
8.85906027617959));
#55767=CARTESIAN_POINT('Ctrl Pts',(-2.2124999638606,-35.3214069653231,8.9147190921565));
#55768=CARTESIAN_POINT('Ctrl Pts',(-2.09381254498969,-35.3233213389771,
8.97161001651075));
#55769=CARTESIAN_POINT('Ctrl Pts',(-1.97249361548399,-35.325144935522,9.02285350430027));
#55770=CARTESIAN_POINT('Ctrl Pts',(-1.84910037198909,-35.3268109971623,
9.06821758004431));
#55771=CARTESIAN_POINT('Ctrl Pts',(-1.72708337710787,-35.3284584766262,
9.11307569416042));
#55772=CARTESIAN_POINT('Ctrl Pts',(-1.60303930200272,-35.3299511497321,
9.15218460722));
#55773=CARTESIAN_POINT('Ctrl Pts',(-1.47752178591338,-35.3312330133406,
9.18536663014834));
#55774=CARTESIAN_POINT('Ctrl Pts',(-1.42949741113993,-35.3317234683803,
9.19806243512044));
#55775=CARTESIAN_POINT('Ctrl Pts',(-1.38125739859416,-35.3321832123494,
9.20989110168217));
#55776=CARTESIAN_POINT('Ctrl Pts',(-1.3328327737408,-35.3326098028966,9.22084461008599));
#55777=CARTESIAN_POINT('Ctrl Pts',(-1.2154203786744,-35.3336441323935,9.24740295018603));
#55778=CARTESIAN_POINT('Ctrl Pts',(-1.09692351296306,-35.3344820309447,
9.26881355340909));
#55779=CARTESIAN_POINT('Ctrl Pts',(-0.977777965211198,-35.3351024675867,
9.28498986052386));
#55780=CARTESIAN_POINT('Ctrl Pts',(-0.862993660581534,-35.3357001935602,
9.30057404473115));
#55781=CARTESIAN_POINT('Ctrl Pts',(-0.747607895410976,-35.3360957669442,
9.31130017226629));
#55782=CARTESIAN_POINT('Ctrl Pts',(-0.631993617559925,-35.336293183438,
9.31712752395354));
#55783=CARTESIAN_POINT('Ctrl Pts',(-0.522375721082263,-35.3364803608454,
9.322652637684));
#55784=CARTESIAN_POINT('Ctrl Pts',(-0.412552756634451,-35.3364892580904,
9.32377410534818));
#55785=CARTESIAN_POINT('Ctrl Pts',(-0.302820690862792,-35.3363472934361,
9.32048915886595));
#55786=CARTESIAN_POINT('Ctrl Pts',(-0.201733708311387,-35.3362165132632,
9.31746301217496));
#55787=CARTESIAN_POINT('Ctrl Pts',(-0.100723941336883,-35.3359577568238,
9.31069766500961));
#55788=CARTESIAN_POINT('Ctrl Pts',(-1.0275302666507E-6,-35.335613767487,
9.30021571851796));
#55789=CARTESIAN_POINT('Ctrl Pts',(-5.55111512312578E-16,-35.3356137401038,
9.30021561809536));
#55790=CARTESIAN_POINT('Ctrl Pts',(-3.26505811906785E-15,-35.3545578006911,
9.29505018686761));
#55791=CARTESIAN_POINT('Ctrl Pts',(8.15014156923914E-10,-35.3739634390451,
9.29176495584985));
#55792=CARTESIAN_POINT('Ctrl Pts',(7.95444545790306E-10,-35.4004018758749,
9.28993613405734));
#55793=CARTESIAN_POINT('Ctrl Pts',(-3.35855341939055E-14,-35.4072658059936,
9.28969890048895));
#55794=CARTESIAN_POINT('Ctrl Pts',(-5.77315972805081E-14,-35.4141318686725,
9.28969871552309));
#55795=CARTESIAN_POINT('Ctrl Pts',(-4.4921212186,-35.2852060642,5.83250225932));
#55796=CARTESIAN_POINT('Ctrl Pts',(-4.45609896257,-35.3187908592,5.82727337616));
#55797=CARTESIAN_POINT('Ctrl Pts',(-4.42697003004,-35.3598847848,5.82278643887));
#55798=CARTESIAN_POINT('Ctrl Pts',(-4.40679129181,-35.4065868334,5.81933970701));
#55799=CARTESIAN_POINT('Ctrl Pts',(-4.39676908915,-35.4561050262,5.81713923581));
#55800=CARTESIAN_POINT('Ctrl Pts',(-4.39688470965,-35.505623219,5.81623490373));
#55801=CARTESIAN_POINT('Ctrl Pts',(-4.47934426829,-35.2848180141,5.95513865982));
#55802=CARTESIAN_POINT('Ctrl Pts',(-4.44240767125,-35.3184648135,5.94886804446));
#55803=CARTESIAN_POINT('Ctrl Pts',(-4.41246275486,-35.3599636587,5.94360014588));
#55804=CARTESIAN_POINT('Ctrl Pts',(-4.39168683777,-35.4073477788,5.9397026792));
#55805=CARTESIAN_POINT('Ctrl Pts',(-4.38136362076,-35.457688004,5.93741576176));
#55806=CARTESIAN_POINT('Ctrl Pts',(-4.38147338286,-35.5080282291,5.93677544119));
#55807=CARTESIAN_POINT('Ctrl Pts',(-4.46080331489,-35.2846612104,6.0774500678));
#55808=CARTESIAN_POINT('Ctrl Pts',(-4.42339099946,-35.3183175745,6.07010629864));
#55809=CARTESIAN_POINT('Ctrl Pts',(-4.39300176947,-35.3600459293,6.06403311375));
#55810=CARTESIAN_POINT('Ctrl Pts',(-4.37188741448,-35.4078395887,6.05967077608));
#55811=CARTESIAN_POINT('Ctrl Pts',(-4.36138132105,-35.4586803826,6.05729403028));
#55812=CARTESIAN_POINT('Ctrl Pts',(-4.36146441688,-35.5095211765,6.05692288884));
#55813=CARTESIAN_POINT('Ctrl Pts',(-4.43653605144,-35.2846213402,6.19885974208));
#55814=CARTESIAN_POINT('Ctrl Pts',(-4.39907245731,-35.3182793407,6.19048378347));
#55815=CARTESIAN_POINT('Ctrl Pts',(-4.36860698734,-35.360098105,6.18364473746));
#55816=CARTESIAN_POINT('Ctrl Pts',(-4.34741298485,-35.4080551513,6.17885069748));
#55817=CARTESIAN_POINT('Ctrl Pts',(-4.33684033846,-35.4590962326,6.17640727689));
#55818=CARTESIAN_POINT('Ctrl Pts',(-4.33687279452,-35.5101373139,6.17631673235));
#55819=CARTESIAN_POINT('Ctrl Pts',(-4.39382617826,-35.2846522393,6.3704629655));
#55820=CARTESIAN_POINT('Ctrl Pts',(-4.35687304692,-35.3183144911,6.36073630622));
#55821=CARTESIAN_POINT('Ctrl Pts',(-4.32681014412,-35.360077369,6.35290824863));
#55822=CARTESIAN_POINT('Ctrl Pts',(-4.3058660926,-35.4079286751,6.34756704555));
#55823=CARTESIAN_POINT('Ctrl Pts',(-4.295366459,-35.4588388005,6.34505127094));
#55824=CARTESIAN_POINT('Ctrl Pts',(-4.29530142772,-35.5097489259,6.34533949948));
#55825=CARTESIAN_POINT('Ctrl Pts',(-4.33989513123,-35.2849598896,6.53848806555));
#55826=CARTESIAN_POINT('Ctrl Pts',(-4.30425869633,-35.3185874247,6.5277361976));
#55827=CARTESIAN_POINT('Ctrl Pts',(-4.27529524943,-35.3599922268,6.51919887852));
#55828=CARTESIAN_POINT('Ctrl Pts',(-4.25509182459,-35.4072223024,6.51350637116));
#55829=CARTESIAN_POINT('Ctrl Pts',(-4.2448885603,-35.4573782014,6.51100829607));
#55830=CARTESIAN_POINT('Ctrl Pts',(-4.2446848137,-35.5075341005,6.51166242388));
#55831=CARTESIAN_POINT('Ctrl Pts',(-4.32271334112,-35.2850814359,6.58854936739));
#55832=CARTESIAN_POINT('Ctrl Pts',(-4.28754475087,-35.3186934865,6.57751968609));
#55833=CARTESIAN_POINT('Ctrl Pts',(-4.25897443759,-35.3599624877,6.56879320674));
#55834=CARTESIAN_POINT('Ctrl Pts',(-4.23903851349,-35.4069590258,6.56300941547));
#55835=CARTESIAN_POINT('Ctrl Pts',(-4.22894623833,-35.4568320218,6.56051917828));
#55836=CARTESIAN_POINT('Ctrl Pts',(-4.22869977692,-35.5067050179,6.56127483435));
#55837=CARTESIAN_POINT('Ctrl Pts',(-4.30455023491,-35.2852434072,6.6381975116));
#55838=CARTESIAN_POINT('Ctrl Pts',(-4.26991817238,-35.3188318732,6.62693608199));
#55839=CARTESIAN_POINT('Ctrl Pts',(-4.24179867527,-35.3599337083,6.61806209525));
#55840=CARTESIAN_POINT('Ctrl Pts',(-4.22216945818,-35.4066468932,6.61221922778));
#55841=CARTESIAN_POINT('Ctrl Pts',(-4.21220416739,-35.4561778332,6.6097570786));
#55842=CARTESIAN_POINT('Ctrl Pts',(-4.21190811788,-35.5057087732,6.61062231004));
#55843=CARTESIAN_POINT('Ctrl Pts',(-4.28541381497,-35.285453273,6.6874287475));
#55844=CARTESIAN_POINT('Ctrl Pts',(-4.251389142,-35.3190062299,6.67597342108));
#55845=CARTESIAN_POINT('Ctrl Pts',(-4.22378115684,-35.359906937,6.66698096996));
#55846=CARTESIAN_POINT('Ctrl Pts',(-4.20450211564,-35.4062855347,6.66109555831));
#55847=CARTESIAN_POINT('Ctrl Pts',(-4.19468580977,-35.4554145194,6.65866330444));
#55848=CARTESIAN_POINT('Ctrl Pts',(-4.1943405656,-35.5045435041,6.65962635024));
#55849=CARTESIAN_POINT('',(-4.39688473843144,-35.505623218299,5.81623468041465));
#55850=CARTESIAN_POINT('',(-4.49212120371157,-35.2852060781985,5.83250225674026));
#55851=CARTESIAN_POINT('Origin',(-4.69448488168448,-35.505632917967,5.85428086421669));
#55852=CARTESIAN_POINT('Ctrl Pts',(-4.49212120371,-35.2852060782,5.83250225674));
#55853=CARTESIAN_POINT('Ctrl Pts',(-4.47934426829,-35.2848180141,5.95513865982));
#55854=CARTESIAN_POINT('Ctrl Pts',(-4.46080331489,-35.2846612104,6.0774500678));
#55855=CARTESIAN_POINT('Ctrl Pts',(-4.43653605144,-35.2846213402,6.19885974208));
#55856=CARTESIAN_POINT('Ctrl Pts',(-4.39382617826,-35.2846522393,6.3704629655));
#55857=CARTESIAN_POINT('Ctrl Pts',(-4.33989513123,-35.2849598896,6.53848806555));
#55858=CARTESIAN_POINT('Ctrl Pts',(-4.32271334112,-35.2850814359,6.58854936739));
#55859=CARTESIAN_POINT('Ctrl Pts',(-4.30455023491,-35.2852434072,6.6381975116));
#55860=CARTESIAN_POINT('Ctrl Pts',(-4.2854138145,-35.285453273,6.68742874721));
#55861=CARTESIAN_POINT('Ctrl Pts',(-4.39688470965,-35.505623219,5.81623490373));
#55862=CARTESIAN_POINT('Ctrl Pts',(-4.38545059998313,-35.507407563559,5.90566741939867));
#55863=CARTESIAN_POINT('Ctrl Pts',(-4.37100172655426,-35.5085885511775,
5.99465197633656));
#55864=CARTESIAN_POINT('Ctrl Pts',(-4.35358930347287,-35.5091884954551,
6.08296676348967));
#55865=CARTESIAN_POINT('Ctrl Pts',(-4.33595593723731,-35.5097960523195,
6.17240216134366));
#55866=CARTESIAN_POINT('Ctrl Pts',(-4.31528465861745,-35.5098065202248,
6.26115007221233));
#55867=CARTESIAN_POINT('Ctrl Pts',(-4.29163457916425,-35.5092195580943,
6.34902509595134));
#55868=CARTESIAN_POINT('Ctrl Pts',(-4.28600488465352,-35.5090798368941,
6.36994297657631));
#55869=CARTESIAN_POINT('Ctrl Pts',(-4.28020637624591,-35.5089062055461,
6.39081161831919));
#55870=CARTESIAN_POINT('Ctrl Pts',(-4.2742397731198,-35.5086985824798,6.41162895166904));
#55871=CARTESIAN_POINT('Ctrl Pts',(-4.26005358598373,-35.5082049381717,
6.46112421393691));
#55872=CARTESIAN_POINT('Ctrl Pts',(-4.24491858163952,-35.5075194868754,
6.51032521145546));
#55873=CARTESIAN_POINT('Ctrl Pts',(-4.22884677793683,-35.506639317091,6.55919989334204));
#55874=CARTESIAN_POINT('Ctrl Pts',(-4.21778592957061,-35.5060335714819,
6.59283615815062));
#55875=CARTESIAN_POINT('Ctrl Pts',(-4.20628031810575,-35.5053354769618,
6.62632085027922));
#55876=CARTESIAN_POINT('Ctrl Pts',(-4.1943405656018,-35.5045435041,6.65962635023498));
#55877=CARTESIAN_POINT('Ctrl Pts',(-3.30528115437,-35.2990850504,2.45651113175));
#55878=CARTESIAN_POINT('Ctrl Pts',(-3.29174997169,-35.3282258256,2.47004153063));
#55879=CARTESIAN_POINT('Ctrl Pts',(-3.28123332764,-35.3601461205,2.48060031812));
#55880=CARTESIAN_POINT('Ctrl Pts',(-3.27411296889,-35.3940266351,2.48780578271));
#55881=CARTESIAN_POINT('Ctrl Pts',(-3.27059465556,-35.4288883092,2.49144970493));
#55882=CARTESIAN_POINT('Ctrl Pts',(-3.2706750272,-35.4637499833,2.49153088745));
#55883=CARTESIAN_POINT('Ctrl Pts',(-3.52263014734,-35.2997786652,2.67764867799));
#55884=CARTESIAN_POINT('Ctrl Pts',(-3.50832158865,-35.3287004593,2.68978061947));
#55885=CARTESIAN_POINT('Ctrl Pts',(-3.49718986878,-35.3603042564,2.69922432977));
#55886=CARTESIAN_POINT('Ctrl Pts',(-3.48962934617,-35.3937968185,2.70564685787));
#55887=CARTESIAN_POINT('Ctrl Pts',(-3.48585336684,-35.4282347239,2.70886780417));
#55888=CARTESIAN_POINT('Ctrl Pts',(-3.48586067783,-35.4626726292,2.70888759263));
#55889=CARTESIAN_POINT('Ctrl Pts',(-3.71975032728,-35.2998840308,2.91888544948));
#55890=CARTESIAN_POINT('Ctrl Pts',(-3.70452693031,-35.3287908762,2.92986690945));
#55891=CARTESIAN_POINT('Ctrl Pts',(-3.69266813705,-35.3603788898,2.93839702263));
#55892=CARTESIAN_POINT('Ctrl Pts',(-3.68459264153,-35.3938552567,2.94417305658));
#55893=CARTESIAN_POINT('Ctrl Pts',(-3.68052780808,-35.4282767651,2.94703197385));
#55894=CARTESIAN_POINT('Ctrl Pts',(-3.68047391974,-35.4626982735,2.94697615221));
#55895=CARTESIAN_POINT('Ctrl Pts',(-3.89420210101,-35.2992579912,3.17776652664));
#55896=CARTESIAN_POINT('Ctrl Pts',(-3.87780196962,-35.3284044612,3.18777591948));
#55897=CARTESIAN_POINT('Ctrl Pts',(-3.86500520386,-35.3603251829,3.19553496378));
#55898=CARTESIAN_POINT('Ctrl Pts',(-3.85627187964,-35.3942021449,3.20076023088));
#55899=CARTESIAN_POINT('Ctrl Pts',(-3.85185292871,-35.4290582738,3.20330006316));
#55900=CARTESIAN_POINT('Ctrl Pts',(-3.85174986217,-35.4639144026,3.20315896516));
#55901=CARTESIAN_POINT('Ctrl Pts',(-4.25043308745,-35.2963608901,3.82861914207));
#55902=CARTESIAN_POINT('Ctrl Pts',(-4.23039390269,-35.3265730217,3.83636634601));
#55903=CARTESIAN_POINT('Ctrl Pts',(-4.21468510082,-35.3600305104,3.84233146345));
#55904=CARTESIAN_POINT('Ctrl Pts',(-4.20392503792,-35.3957885434,3.84626231873));
#55905=CARTESIAN_POINT('Ctrl Pts',(-4.19845399885,-35.4326982838,3.848026993));
#55906=CARTESIAN_POINT('Ctrl Pts',(-4.19827560656,-35.4696080243,3.84763795769));
#55907=CARTESIAN_POINT('Ctrl Pts',(-4.45858902825,-35.291449905,4.54475674437));
#55908=CARTESIAN_POINT('Ctrl Pts',(-4.43308531823,-35.3233621358,4.54953750297));
#55909=CARTESIAN_POINT('Ctrl Pts',(-4.41292476175,-35.3596262841,4.55315251935));
#55910=CARTESIAN_POINT('Ctrl Pts',(-4.39907396454,-35.3990181868,4.55540464772));
#55911=CARTESIAN_POINT('Ctrl Pts',(-4.39207409827,-35.4399769064,4.55619669281));
#55912=CARTESIAN_POINT('Ctrl Pts',(-4.39192731775,-35.480935626,4.55555318454));
#55913=CARTESIAN_POINT('Ctrl Pts',(-4.52558545037,-35.2885903077,4.9733945174));
#55914=CARTESIAN_POINT('Ctrl Pts',(-4.4963387214,-35.3214318737,4.97577624036));
#55915=CARTESIAN_POINT('Ctrl Pts',(-4.4730869275,-35.3595080502,4.97747837329));
#55916=CARTESIAN_POINT('Ctrl Pts',(-4.45708682842,-35.4013807813,4.97836774601));
#55917=CARTESIAN_POINT('Ctrl Pts',(-4.44904844444,-35.4451561726,4.97838721155));
#55918=CARTESIAN_POINT('Ctrl Pts',(-4.44897072855,-35.4889315639,4.97757277822));
#55919=CARTESIAN_POINT('Ctrl Pts',(-4.53663898841,-35.2864927806,5.40585813039));
#55920=CARTESIAN_POINT('Ctrl Pts',(-4.5036945439,-35.3198754069,5.40486687422));
#55921=CARTESIAN_POINT('Ctrl Pts',(-4.4772847339,-35.3595850208,5.403864254));
#55922=CARTESIAN_POINT('Ctrl Pts',(-4.45905487062,-35.4039471568,5.40287237975));
#55923=CARTESIAN_POINT('Ctrl Pts',(-4.44995084219,-35.450642856,5.40192600583));
#55924=CARTESIAN_POINT('Ctrl Pts',(-4.44996438067,-35.4973385552,5.40106825188));
#55925=CARTESIAN_POINT('Ctrl Pts',(-4.49212121119,-35.2852060782,5.83250225872));
#55926=CARTESIAN_POINT('Ctrl Pts',(-4.45609896624,-35.3187908717,5.82727331029));
#55927=CARTESIAN_POINT('Ctrl Pts',(-4.42697004659,-35.3598847947,5.82278629135));
#55928=CARTESIAN_POINT('Ctrl Pts',(-4.40679132226,-35.4065868399,5.81933946513));
#55929=CARTESIAN_POINT('Ctrl Pts',(-4.39676913356,-35.4561050288,5.8171388925));
#55930=CARTESIAN_POINT('Ctrl Pts',(-4.39688476736,-35.5056232176,5.81623445774));
#55931=CARTESIAN_POINT('',(-3.27067489002724,-35.4637499841709,2.49153074894399));
#55932=CARTESIAN_POINT('',(-3.30528109761575,-35.2990851340947,2.45651115243885));
#55933=CARTESIAN_POINT('Origin',(-3.48386983245681,-35.4637516974525,2.2804588998513));
#55934=CARTESIAN_POINT('Ctrl Pts',(-3.30528109741,-35.2990851344,2.45651115251));
#55935=CARTESIAN_POINT('Ctrl Pts',(-3.52263014734,-35.2997786652,2.67764867799));
#55936=CARTESIAN_POINT('Ctrl Pts',(-3.71975032728,-35.2998840308,2.91888544948));
#55937=CARTESIAN_POINT('Ctrl Pts',(-3.89420210101,-35.2992579912,3.17776652664));
#55938=CARTESIAN_POINT('Ctrl Pts',(-4.25043308745,-35.2963608901,3.82861914207));
#55939=CARTESIAN_POINT('Ctrl Pts',(-4.45858902825,-35.291449905,4.54475674437));
#55940=CARTESIAN_POINT('Ctrl Pts',(-4.52558545037,-35.2885903077,4.9733945174));
#55941=CARTESIAN_POINT('Ctrl Pts',(-4.53663898841,-35.2864927806,5.40585813039));
#55942=CARTESIAN_POINT('Ctrl Pts',(-4.49212120371,-35.2852060782,5.83250225674));
#55943=CARTESIAN_POINT('Ctrl Pts',(-3.2706750272,-35.4637499833,2.49153088745));
#55944=CARTESIAN_POINT('Ctrl Pts',(-3.34813707187767,-35.4633621598035,
2.56977446344287));
#55945=CARTESIAN_POINT('Ctrl Pts',(-3.42304337318045,-35.4631429472603,
2.65189514109921));
#55946=CARTESIAN_POINT('Ctrl Pts',(-3.49496054014435,-35.463107855991,2.73777137044876));
#55947=CARTESIAN_POINT('Ctrl Pts',(-3.56711767566814,-35.4630726476315,
2.8239341460564));
#55948=CARTESIAN_POINT('Ctrl Pts',(-3.63626532925966,-35.4632228989124,
2.91387775343965));
#55949=CARTESIAN_POINT('Ctrl Pts',(-3.70196006654796,-35.4635695903925,
3.00742645561651));
#55950=CARTESIAN_POINT('Ctrl Pts',(-3.76774023884962,-35.4639167327395,
3.10109681646727));
#55951=CARTESIAN_POINT('Ctrl Pts',(-3.8300576443282,-35.4644609466404,3.19838101859501));
#55952=CARTESIAN_POINT('Ctrl Pts',(-3.88846922427447,-35.4652068351614,
3.29905040676408));
#55953=CARTESIAN_POINT('Ctrl Pts',(-3.9452868428507,-35.4659323695421,3.39697268355497));
#55954=CARTESIAN_POINT('Ctrl Pts',(-3.99840870171747,-35.4668488224885,
3.49809815904795));
#55955=CARTESIAN_POINT('Ctrl Pts',(-4.04743323499239,-35.4679527918964,
3.6021661231991));
#55956=CARTESIAN_POINT('Ctrl Pts',(-4.07131487842421,-35.4684905757773,
3.65286143525025));
#55957=CARTESIAN_POINT('Ctrl Pts',(-4.09422433966003,-35.4690727315529,
3.70425421846681));
#55958=CARTESIAN_POINT('Ctrl Pts',(-4.11611628683934,-35.4696980689031,
3.7563100790971));
#55959=CARTESIAN_POINT('Ctrl Pts',(-4.15139593057075,-35.470705822062,3.8401999314764));
#55960=CARTESIAN_POINT('Ctrl Pts',(-4.18403267406679,-35.4718258943186,
3.92581272262133));
#55961=CARTESIAN_POINT('Ctrl Pts',(-4.2138419733407,-35.4730506192599,4.01298809000643));
#55962=CARTESIAN_POINT('Ctrl Pts',(-4.21525776959202,-35.4731087877182,
4.01712849455661));
#55963=CARTESIAN_POINT('Ctrl Pts',(-4.21720500784041,-35.4731896392214,
4.02286090035683));
#55964=CARTESIAN_POINT('Ctrl Pts',(-4.21825549464136,-35.4732333631442,
4.02596768664432));
#55965=CARTESIAN_POINT('Ctrl Pts',(-4.21839192807396,-35.4732390418494,
4.02637118482935));
#55966=CARTESIAN_POINT('Ctrl Pts',(-4.21851330667239,-35.4732440920213,
4.02673037086751));
#55967=CARTESIAN_POINT('Ctrl Pts',(-4.2186165485839,-35.4732483811445,4.02703598966244));
#55968=CARTESIAN_POINT('Ctrl Pts',(-4.23183083826564,-35.4737973608668,
4.06615319729172));
#55969=CARTESIAN_POINT('Ctrl Pts',(-4.24548075738622,-35.474411102047,4.10854338064577));
#55970=CARTESIAN_POINT('Ctrl Pts',(-4.25925066744965,-35.4750969173758,
4.15428398502716));
#55971=CARTESIAN_POINT('Ctrl Pts',(-4.2727730646147,-35.4757704052354,4.1992024061472));
#55972=CARTESIAN_POINT('Ctrl Pts',(-4.28641108667379,-35.4765134451113,
4.24735239861612));
#55973=CARTESIAN_POINT('Ctrl Pts',(-4.2998170358193,-35.4773325193858,4.29879617118771));
#55974=CARTESIAN_POINT('Ctrl Pts',(-4.31304837859414,-35.4781409255916,
4.34956991209459));
#55975=CARTESIAN_POINT('Ctrl Pts',(-4.32605355488894,-35.4790234473957,
4.40355273662503));
#55976=CARTESIAN_POINT('Ctrl Pts',(-4.33845166412103,-35.4799851819289,
4.46078568264521));
#55977=CARTESIAN_POINT('Ctrl Pts',(-4.35057706096531,-35.4809257618718,
4.51675971627169));
#55978=CARTESIAN_POINT('Ctrl Pts',(-4.36212158350111,-35.4819421524447,
4.57584296420357));
#55979=CARTESIAN_POINT('Ctrl Pts',(-4.37268649070218,-35.4830373446617,
4.63804811399243));
#55980=CARTESIAN_POINT('Ctrl Pts',(-4.37771153255026,-35.4835582566411,
4.66763507343339));
#55981=CARTESIAN_POINT('Ctrl Pts',(-4.38251435031144,-35.4840969654634,
4.69792787163709));
#55982=CARTESIAN_POINT('Ctrl Pts',(-4.38704879694281,-35.4846536031822,
4.72892524743954));
#55983=CARTESIAN_POINT('Ctrl Pts',(-4.39625171328598,-35.4857833309696,
4.79183617782618));
#55984=CARTESIAN_POINT('Ctrl Pts',(-4.40435098438274,-35.4869880048322,
4.85764894737013));
#55985=CARTESIAN_POINT('Ctrl Pts',(-4.41093643203333,-35.488267734625,4.92633586345641));
#55986=CARTESIAN_POINT('Ctrl Pts',(-4.41730798087347,-35.4895058981198,
4.99279179230792));
#55987=CARTESIAN_POINT('Ctrl Pts',(-4.42226208806939,-35.4908143333423,
5.06193852712424));
#55988=CARTESIAN_POINT('Ctrl Pts',(-4.425397613255,-35.4921905896938,5.13371303089722));
#55989=CARTESIAN_POINT('Ctrl Pts',(-4.42847425789576,-35.4935410019781,
5.20413971520232));
#55990=CARTESIAN_POINT('Ctrl Pts',(-4.42979964382002,-35.4949567142392,
5.27709678642837));
#55991=CARTESIAN_POINT('Ctrl Pts',(-4.42897076191856,-35.4964327992564,
5.35248217910494));
#55992=CARTESIAN_POINT('Ctrl Pts',(-4.42816771303412,-35.4978628804589,
5.42551810302413));
#55993=CARTESIAN_POINT('Ctrl Pts',(-4.42534217899082,-35.499349607714,5.50083357556422));
#55994=CARTESIAN_POINT('Ctrl Pts',(-4.42011034884093,-35.5008861800709,
5.5782911933905));
#55995=CARTESIAN_POINT('Ctrl Pts',(-4.4148928306134,-35.5024185490605,5.65553692218727));
#55996=CARTESIAN_POINT('Ctrl Pts',(-4.40728176918284,-35.5040004542694,
5.73491352245175));
#55997=CARTESIAN_POINT('Ctrl Pts',(-4.39688476736,-35.5056232175999,5.81623445774));
#55998=CARTESIAN_POINT('Ctrl Pts',(-3.24268125491577,-35.2958973038634,
2.35935886017492));
#55999=CARTESIAN_POINT('Ctrl Pts',(-3.23323477285515,-35.3247273688969,
2.3897825108109));
#56000=CARTESIAN_POINT('Ctrl Pts',(-3.22952081745637,-35.3580485457362,
2.41773023191833));
#56001=CARTESIAN_POINT('Ctrl Pts',(-3.23194738647767,-35.3946308528826,
2.44189906566998));
#56002=CARTESIAN_POINT('Ctrl Pts',(-3.24040658365444,-35.43284772689,2.46121439404479));
#56003=CARTESIAN_POINT('Ctrl Pts',(-3.25430040542545,-35.4710646009975,
2.47508664859981));
#56004=CARTESIAN_POINT('Ctrl Pts',(-3.24863517715864,-35.2942729539699,
2.3701975687693));
#56005=CARTESIAN_POINT('Ctrl Pts',(-3.23915898528583,-35.3234246802185,
2.39878856453282));
#56006=CARTESIAN_POINT('Ctrl Pts',(-3.2350331221988,-35.3568426819669,2.42480698211996));
#56007=CARTESIAN_POINT('Ctrl Pts',(-3.23664595574859,-35.3933445979533,
2.44709362653317));
#56008=CARTESIAN_POINT('Ctrl Pts',(-3.24393136712945,-35.4313918582424,
2.46471330964264));
#56009=CARTESIAN_POINT('Ctrl Pts',(-3.25638336581306,-35.4694391186319,
2.47716637564742));
#56010=CARTESIAN_POINT('Ctrl Pts',(-3.2548709476279,-35.2930864761754,2.38098976678876));
#56011=CARTESIAN_POINT('Ctrl Pts',(-3.24525822198285,-35.3224889921552,
2.407755582698));
#56012=CARTESIAN_POINT('Ctrl Pts',(-3.24064139298909,-35.3559431246713,
2.43187281216271));
#56013=CARTESIAN_POINT('Ctrl Pts',(-3.24139525599044,-35.3923142407988,
2.45231077673936));
#56014=CARTESIAN_POINT('Ctrl Pts',(-3.2474923517538,-35.4301467373312,2.46825699792508));
#56015=CARTESIAN_POINT('Ctrl Pts',(-3.25850833911909,-35.4679792337635,
2.4792918557513));
#56016=CARTESIAN_POINT('Ctrl Pts',(-3.26132471448853,-35.2924161434336,
2.39170879431664));
#56017=CARTESIAN_POINT('Ctrl Pts',(-3.25147227203682,-35.3219985450907,
2.41665052924938));
#56018=CARTESIAN_POINT('Ctrl Pts',(-3.24628624189605,-35.3554285970707,
2.43888137042276));
#56019=CARTESIAN_POINT('Ctrl Pts',(-3.24613175788547,-35.3916164538002,
2.45749004094981));
#56020=CARTESIAN_POINT('Ctrl Pts',(-3.25101555797363,-35.4291873972929,
2.47177215112507));
#56021=CARTESIAN_POINT('Ctrl Pts',(-3.2605896658139,-35.4667583406855,2.481377904069));
#56022=CARTESIAN_POINT('Ctrl Pts',(-3.27381283591109,-35.2922258297676,
2.41169319642401));
#56023=CARTESIAN_POINT('Ctrl Pts',(-3.26330828363882,-35.3220055622133,
2.43319946208684));
#56024=CARTESIAN_POINT('Ctrl Pts',(-3.25689092113158,-35.3552658228255,
2.45190420521593));
#56025=CARTESIAN_POINT('Ctrl Pts',(-3.25491795867093,-35.3910088541773,
2.46708600579959));
#56026=CARTESIAN_POINT('Ctrl Pts',(-3.25746311070511,-35.4279936168047,
2.478225570397));
#56027=CARTESIAN_POINT('Ctrl Pts',(-3.26429697723892,-35.4649783794321,
2.48510059740241));
#56028=CARTESIAN_POINT('Ctrl Pts',(-3.28671058272193,-35.2940584356266,
2.43091393425374));
#56029=CARTESIAN_POINT('Ctrl Pts',(-3.27516135889415,-35.3237449318942,
2.44902623947939));
#56030=CARTESIAN_POINT('Ctrl Pts',(-3.26720601449316,-35.3565916803118,
2.46426478291748));
#56031=CARTESIAN_POINT('Ctrl Pts',(-3.26320423693874,-35.391677678938,2.47607271322631));
#56032=CARTESIAN_POINT('Ctrl Pts',(-3.26328413845668,-35.4278861002098,
2.48407552049272));
#56033=CARTESIAN_POINT('Ctrl Pts',(-3.26732385940126,-35.4640945215815,
2.48814889706368));
#56034=CARTESIAN_POINT('Ctrl Pts',(-3.29284930097053,-35.2953488394616,
2.43972797957268));
#56035=CARTESIAN_POINT('Ctrl Pts',(-3.28072374942692,-35.3249242484803,
2.45627460757783));
#56036=CARTESIAN_POINT('Ctrl Pts',(-3.27197784219537,-35.3575177795095,
2.46992291402891));
#56037=CARTESIAN_POINT('Ctrl Pts',(-3.26697872456239,-35.3922543161982,
2.48016821016769));
#56038=CARTESIAN_POINT('Ctrl Pts',(-3.26588739148542,-35.4280582492778,
2.4867007857863));
#56039=CARTESIAN_POINT('Ctrl Pts',(-3.26861320217918,-35.4638621823573,
2.48944916276422));
#56040=CARTESIAN_POINT('Ctrl Pts',(-3.29903564205108,-35.2970543501715,
2.44827686787325));
#56041=CARTESIAN_POINT('Ctrl Pts',(-3.28623988731176,-35.3264458529848,
2.46327459582849));
#56042=CARTESIAN_POINT('Ctrl Pts',(-3.27663206694421,-35.3587314714483,
2.47533376078653));
#56043=CARTESIAN_POINT('Ctrl Pts',(-3.27058251702853,-35.3930563620857,
2.48402805942754));
#56044=CARTESIAN_POINT('Ctrl Pts',(-3.26826827635479,-35.4284056459787,
2.4890983067967));
#56045=CARTESIAN_POINT('Ctrl Pts',(-3.26965563393973,-35.4637549298717,
2.49050120789989));
#56046=CARTESIAN_POINT('Ctrl Pts',(-3.30530033482775,-35.2990758150286,
2.45652194936013));
#56047=CARTESIAN_POINT('Ctrl Pts',(-3.29176525174297,-35.3282177516101,
2.47005157432767));
#56048=CARTESIAN_POINT('Ctrl Pts',(-3.28124477977141,-35.3601396973233,
2.48060908546945));
#56049=CARTESIAN_POINT('Ctrl Pts',(-3.27412082604265,-35.394022231877,2.48781273002727));
#56050=CARTESIAN_POINT('Ctrl Pts',(-3.27059928705473,-35.4288861031222,
2.4914543200214));
#56051=CARTESIAN_POINT('Ctrl Pts',(-3.27067686689488,-35.4637499744676,
2.49153274570348));
#56052=CARTESIAN_POINT('Ctrl Pts',(-3.24268782424592,-35.295907687789,2.35939289968608));
#56053=CARTESIAN_POINT('Ctrl Pts',(-3.25008684470559,-35.293890193334,2.37286023708758));
#56054=CARTESIAN_POINT('Ctrl Pts',(-3.25799757378118,-35.2927186181909,
2.38626991325058));
#56055=CARTESIAN_POINT('Ctrl Pts',(-3.26619360674797,-35.2925758914817,
2.39937991847623));
#56056=CARTESIAN_POINT('Ctrl Pts',(-3.26898632406456,-35.2925272587646,
2.40384702332593));
#56057=CARTESIAN_POINT('Ctrl Pts',(-3.27181181577843,-35.2925980792957,
2.4082795569164));
#56058=CARTESIAN_POINT('Ctrl Pts',(-3.27466035798211,-35.292795589977,2.41266929430184));
#56059=CARTESIAN_POINT('Ctrl Pts',(-3.2805841726001,-35.2932063322366,2.42179817098109));
#56060=CARTESIAN_POINT('Ctrl Pts',(-3.28660274669036,-35.2941627905457,
2.43072803182399));
#56061=CARTESIAN_POINT('Ctrl Pts',(-3.29270461274169,-35.2955791073848,
2.43934860706454));
#56062=CARTESIAN_POINT('Ctrl Pts',(-3.2968597946089,-35.2965435753031,2.44521895191039));
#56063=CARTESIAN_POINT('Ctrl Pts',(-3.30105340316511,-35.2977212882825,
2.45094670272042));
#56064=CARTESIAN_POINT('Ctrl Pts',(-3.30528109740205,-35.2990851343927,
2.45651115251783));
#56065=CARTESIAN_POINT('Origin',(-3.25603245768934,-35.4878985648969,2.47710123794777));
#56066=CARTESIAN_POINT('Origin',(-0.425321894002,-36.1242356128,5.30846337982));
#56067=CARTESIAN_POINT('',(-1.85962356625E-14,-36.1242356128,9.2896999221));
#56068=CARTESIAN_POINT('Origin',(0.425321894002,-36.1242356128,5.30846337982));
#56069=CARTESIAN_POINT('',(4.19434056524382,-35.5045435040676,6.6596263511468));
#56070=CARTESIAN_POINT('Ctrl Pts',(4.19434056523043,-35.5045435040781,6.65962635114224));
#56071=CARTESIAN_POINT('Ctrl Pts',(4.15305083902113,-35.50180461675,6.77480250110769));
#56072=CARTESIAN_POINT('Ctrl Pts',(4.10642935579663,-35.4989509433917,6.88821915911414));
#56073=CARTESIAN_POINT('Ctrl Pts',(4.05464196214409,-35.4960150956293,6.99937406998726));
#56074=CARTESIAN_POINT('Ctrl Pts',(4.00293218678962,-35.4930836480788,7.11036238326981));
#56075=CARTESIAN_POINT('Ctrl Pts',(3.94607207387214,-35.4900702722635,7.21909537875552));
#56076=CARTESIAN_POINT('Ctrl Pts',(3.88427619509728,-35.4870074333955,7.32508884382549));
#56077=CARTESIAN_POINT('Ctrl Pts',(3.82256508245509,-35.4839487958596,7.43093691641458));
#56078=CARTESIAN_POINT('Ctrl Pts',(3.75593187099409,-35.480840830876,7.53405263623836));
#56079=CARTESIAN_POINT('Ctrl Pts',(3.68463786454671,-35.4777158702413,7.63397461894421));
#56080=CARTESIAN_POINT('Ctrl Pts',(3.61346023977025,-35.4745960108509,7.73373348713474));
#56081=CARTESIAN_POINT('Ctrl Pts',(3.53763719705471,-35.4714592112521,7.83030872216152));
#56082=CARTESIAN_POINT('Ctrl Pts',(3.45747394171211,-35.4683376451628,7.92326682916533));
#56083=CARTESIAN_POINT('Ctrl Pts',(3.37739062673967,-35.4652191919604,8.01613223652201));
#56084=CARTESIAN_POINT('Ctrl Pts',(3.29297595264275,-35.4621159419002,8.1053874293973));
#56085=CARTESIAN_POINT('Ctrl Pts',(3.20457654052722,-35.4590599725433,8.19063039942675));
#56086=CARTESIAN_POINT('Ctrl Pts',(3.11627567267817,-35.4560074098636,8.27577834387001));
#56087=CARTESIAN_POINT('Ctrl Pts',(3.02399917934084,-35.4530020225324,8.35692273333336));
#56088=CARTESIAN_POINT('Ctrl Pts',(2.92813151663719,-35.4500757809538,8.43369730898203));
#56089=CARTESIAN_POINT('Ctrl Pts',(2.89703118657161,-35.4491264819266,8.45860367027196));
#56090=CARTESIAN_POINT('Ctrl Pts',(2.8655532088065,-35.448185512292,8.48305043444037));
#56091=CARTESIAN_POINT('Ctrl Pts',(2.83371152617554,-35.4472539635573,8.50702594740874));
#56092=CARTESIAN_POINT('Ctrl Pts',(2.73357926242005,-35.4443245303148,8.58242153551399));
#56093=CARTESIAN_POINT('Ctrl Pts',(2.62985289969705,-35.4415182005033,8.65314930294848));
#56094=CARTESIAN_POINT('Ctrl Pts',(2.52299764839741,-35.4388615158311,8.71887384610738));
#56095=CARTESIAN_POINT('Ctrl Pts',(2.4196792012438,-35.4362927648192,8.78242297126939));
#56096=CARTESIAN_POINT('Ctrl Pts',(2.31343605617025,-35.4338639166745,8.84129461962353));
#56097=CARTESIAN_POINT('Ctrl Pts',(2.20471825533705,-35.4315989638622,8.89522957075138));
#56098=CARTESIAN_POINT('Ctrl Pts',(2.09602580748759,-35.4293345392368,8.94915194425232));
#56099=CARTESIAN_POINT('Ctrl Pts',(1.98486018981476,-35.4272339335119,8.9981397472551));
#56100=CARTESIAN_POINT('Ctrl Pts',(1.87169528201999,-35.4253211223716,9.04198010558597));
#56101=CARTESIAN_POINT('Ctrl Pts',(1.75853751403165,-35.4234084319144,9.08581769793859));
#56102=CARTESIAN_POINT('Ctrl Pts',(1.64338105763938,-35.4216835123457,9.12450835777501));
#56103=CARTESIAN_POINT('Ctrl Pts',(1.52671874202298,-35.4201703348117,9.15788776566138));
#56104=CARTESIAN_POINT('Ctrl Pts',(1.41004394368312,-35.4186569953696,9.19127074510311));
#56105=CARTESIAN_POINT('Ctrl Pts',(1.29186332646816,-35.4173554432769,9.21934123844898));
#56106=CARTESIAN_POINT('Ctrl Pts',(1.1726835767396,-35.4162896573753,9.24198516497849));
#56107=CARTESIAN_POINT('Ctrl Pts',(1.05342866422859,-35.4152231993173,9.2646433722942));
#56108=CARTESIAN_POINT('Ctrl Pts',(0.93317372977555,-35.4143928049242,9.28186810641652));
#56109=CARTESIAN_POINT('Ctrl Pts',(0.81243462455955,-35.4138224984343,9.29359660883269));
#56110=CARTESIAN_POINT('Ctrl Pts',(0.691652882104724,-35.413251990549,9.30532925299696));
#56111=CARTESIAN_POINT('Ctrl Pts',(0.570387002637427,-35.4129417542919,
9.31156176915144));
#56112=CARTESIAN_POINT('Ctrl Pts',(0.449155981586392,-35.4129158393615,
9.31228343764101));
#56113=CARTESIAN_POINT('Ctrl Pts',(0.327819079588126,-35.4128899017975,
9.3130057364226));
#56114=CARTESIAN_POINT('Ctrl Pts',(0.206517472293906,-35.4131487824193,
9.308207582444));
#56115=CARTESIAN_POINT('Ctrl Pts',(0.0857684745831489,-35.4137165939942,
9.29793033600623));
#56116=CARTESIAN_POINT('Ctrl Pts',(0.0571457260649734,-35.4138511899595,
9.29549418294637));
#56117=CARTESIAN_POINT('Ctrl Pts',(0.0285540008339206,-35.414003144618,
9.29275039094128));
#56118=CARTESIAN_POINT('Ctrl Pts',(1.28564320530265E-7,-35.4141727791362,
9.28969993583948));
#56119=CARTESIAN_POINT('',(4.39688473843144,-35.505623218299,5.81623468041465));
#56120=CARTESIAN_POINT('Ctrl Pts',(4.39688470965,-35.505623219,5.81623490373));
#56121=CARTESIAN_POINT('Ctrl Pts',(4.38573643649444,-35.5073629552901,5.90343173345355));
#56122=CARTESIAN_POINT('Ctrl Pts',(4.37169824303641,-35.5085322020161,5.99037898434775));
#56123=CARTESIAN_POINT('Ctrl Pts',(4.35480069027969,-35.5091456409943,6.07679716182491));
#56124=CARTESIAN_POINT('Ctrl Pts',(4.33760460211872,-35.5097699178291,6.16474212166635));
#56125=CARTESIAN_POINT('Ctrl Pts',(4.31744838415589,-35.5098175202228,6.25213819810706));
#56126=CARTESIAN_POINT('Ctrl Pts',(4.29439012671324,-35.5092855518098,6.33873192964319));
#56127=CARTESIAN_POINT('Ctrl Pts',(4.28790249453768,-35.5091358780801,6.36309579496619));
#56128=CARTESIAN_POINT('Ctrl Pts',(4.28118522482724,-35.508940268535,6.3873964394));
#56129=CARTESIAN_POINT('Ctrl Pts',(4.27423977311736,-35.508698583756,6.41162895167755));
#56130=CARTESIAN_POINT('Ctrl Pts',(4.25993397822891,-35.5082007769869,6.46154152248722));
#56131=CARTESIAN_POINT('Ctrl Pts',(4.24466258667264,-35.5075078797346,6.51115697796593));
#56132=CARTESIAN_POINT('Ctrl Pts',(4.22844025810848,-35.5066170237349,6.56043545201076));
#56133=CARTESIAN_POINT('Ctrl Pts',(4.21772914646967,-35.5060288185319,6.59297253414401));
#56134=CARTESIAN_POINT('Ctrl Pts',(4.20660257847504,-35.5053541998305,6.62536529996203));
#56135=CARTESIAN_POINT('Ctrl Pts',(4.19507102909248,-35.5045918749017,6.65758701234463));
#56136=CARTESIAN_POINT('Ctrl Pts',(4.19482771075667,-35.504575789671,6.65826689786338));
#56137=CARTESIAN_POINT('Ctrl Pts',(4.19458421244928,-35.5045596653808,6.65894670632568));
#56138=CARTESIAN_POINT('Ctrl Pts',(4.1943405656018,-35.5045435041,6.65962635023499));
#56139=CARTESIAN_POINT('',(3.27067475303001,-35.4637499849021,2.49153061051667));
#56140=CARTESIAN_POINT('Ctrl Pts',(3.27067475303,-35.4637499849,2.49153061052));
#56141=CARTESIAN_POINT('Ctrl Pts',(3.48586067783,-35.4626726292,2.70888759263));
#56142=CARTESIAN_POINT('Ctrl Pts',(3.68047391974,-35.4626982735,2.94697615221));
#56143=CARTESIAN_POINT('Ctrl Pts',(3.85174834775,-35.4639143567,3.20314921651));
#56144=CARTESIAN_POINT('Ctrl Pts',(4.09456241628,-35.4679039697,3.65475367055));
#56145=CARTESIAN_POINT('Ctrl Pts',(4.26231352009,-35.4746596511,4.1374772467));
#56146=CARTESIAN_POINT('Ctrl Pts',(4.31696935237,-35.4777519322,4.33446216267));
#56147=CARTESIAN_POINT('Ctrl Pts',(4.40337102111,-35.4847566344,4.74599500874));
#56148=CARTESIAN_POINT('Ctrl Pts',(4.4353410064,-35.4927030817,5.16452779898));
#56149=CARTESIAN_POINT('Ctrl Pts',(4.43724557978,-35.4969389179,5.38040371826));
#56150=CARTESIAN_POINT('Ctrl Pts',(4.42458344919,-35.5012499248,5.59703086423));
#56151=CARTESIAN_POINT('Ctrl Pts',(4.3974872235,-35.5055288233,5.81150364203));
#56152=CARTESIAN_POINT('Ctrl Pts',(4.39728717711,-35.5055602891,5.81308076015));
#56153=CARTESIAN_POINT('Ctrl Pts',(4.39708635746,-35.5055917535,5.81465770549));
#56154=CARTESIAN_POINT('Ctrl Pts',(4.39688476668,-35.5056232176,5.81623445766));
#56155=CARTESIAN_POINT('',(3.25430421882,-35.4710616254,2.47509045608));
#56156=CARTESIAN_POINT('Origin',(3.25603245768934,-35.4878985648969,2.47710123794777));
#56157=CARTESIAN_POINT('',(3.25430421882,-36.1242356128,2.47509045608));
#56158=CARTESIAN_POINT('Origin',(3.46627170195,-36.1242356128,2.26279399804));
#56159=CARTESIAN_POINT('',(3.16691857253,-35.4710616262,2.28248419619));
#56160=CARTESIAN_POINT('Origin',(3.46627170195,-35.4710616316899,2.26279399804));
#56161=CARTESIAN_POINT('',(3.16691857253,-35.9226486195,2.28248419619));
#56162=CARTESIAN_POINT('Origin',(3.0399446742,-32.4742356128,0.352080371467));
#56163=CARTESIAN_POINT('',(3.16549337405758,-35.4651789109462,2.26081668330539));
#56164=CARTESIAN_POINT('Origin',(3.16701457909211,-35.4948316439558,2.28394383708707));
#56165=CARTESIAN_POINT('',(3.04626146311845,-35.4033959728417,0.448115484591892));
#56166=CARTESIAN_POINT('Ctrl Pts',(3.04626151745,-35.4033927946,0.44811631692));
#56167=CARTESIAN_POINT('Ctrl Pts',(3.05294917186292,-35.4075920678871,0.549789759532655));
#56168=CARTESIAN_POINT('Ctrl Pts',(3.05964380945705,-35.4116947932727,0.651569369125622));
#56169=CARTESIAN_POINT('Ctrl Pts',(3.06633992560627,-35.415674424655,0.753371458620647));
#56170=CARTESIAN_POINT('Ctrl Pts',(3.07076632608472,-35.4183051201002,0.820666709719334));
#56171=CARTESIAN_POINT('Ctrl Pts',(3.07519346050157,-35.4208822031627,0.887973119277254));
#56172=CARTESIAN_POINT('Ctrl Pts',(3.07962053317529,-35.4233996000391,0.955278587451633));
#56173=CARTESIAN_POINT('Ctrl Pts',(3.08757598305295,-35.4279233623867,1.07622651806314));
#56174=CARTESIAN_POINT('Ctrl Pts',(3.0955499343282,-35.4322756333094,1.19745572859887));
#56175=CARTESIAN_POINT('Ctrl Pts',(3.10353553487434,-35.436446582721,1.3188620493187));
#56176=CARTESIAN_POINT('Ctrl Pts',(3.11356049330208,-35.4416827066937,1.47127304346359));
#56177=CARTESIAN_POINT('Ctrl Pts',(3.12360407993767,-35.4466333489527,1.62396725231241));
#56178=CARTESIAN_POINT('Ctrl Pts',(3.13365681361421,-35.4513048687405,1.77680052285555));
#56179=CARTESIAN_POINT('Ctrl Pts',(3.14185238055679,-35.4551133604778,1.90139899925928));
#56180=CARTESIAN_POINT('Ctrl Pts',(3.15005425524475,-35.458737299182,2.02609337075221));
#56181=CARTESIAN_POINT('Ctrl Pts',(3.15825582228838,-35.4621835807124,2.15078306376021));
#56182=CARTESIAN_POINT('Ctrl Pts',(3.16011434868278,-35.4629645296643,2.17903852815273));
#56183=CARTESIAN_POINT('Ctrl Pts',(3.16197284588703,-35.4637363447115,2.20729354873459));
#56184=CARTESIAN_POINT('Ctrl Pts',(3.16383120921193,-35.4644990738493,2.23554653393125));
#56185=CARTESIAN_POINT('Ctrl Pts',(3.16438523801469,-35.4647264642123,2.24396951955144));
#56186=CARTESIAN_POINT('Ctrl Pts',(3.16493929387688,-35.4649530731761,2.25239291656041));
#56187=CARTESIAN_POINT('Ctrl Pts',(3.16549337399,-35.4651789177,2.26081668226));
#56188=CARTESIAN_POINT('',(3.0462613877,-36.1242356128,0.448114344193));
#56189=CARTESIAN_POINT('Origin',(2.74690825827,-36.1242356128,0.467804542343));
#56190=CARTESIAN_POINT('',(3.04580294830778,-35.403525641014,0.442075686711352));
#56191=CARTESIAN_POINT('Origin',(2.97884827228343,-36.1481218195378,0.517617073024758));
#56192=CARTESIAN_POINT('',(2.97642257187428,-35.4237537116948,0.274612461594352));
#56193=CARTESIAN_POINT('Ctrl Pts',(2.97642257183112,-35.4237537093279,0.274612461466193));
#56194=CARTESIAN_POINT('Ctrl Pts',(2.98268497977946,-35.4228712901646,0.282052265727931));
#56195=CARTESIAN_POINT('Ctrl Pts',(2.98861404818367,-35.4219372537485,0.289833403879586));
#56196=CARTESIAN_POINT('Ctrl Pts',(2.99415416837544,-35.4209522031331,0.297895150451187));
#56197=CARTESIAN_POINT('Ctrl Pts',(2.99845521021089,-35.4201874645066,0.304153843055496));
#56198=CARTESIAN_POINT('Ctrl Pts',(3.00252275175911,-35.419393257241,0.310582180982538));
#56199=CARTESIAN_POINT('Ctrl Pts',(3.0063416756095,-35.418580198429,0.317158978249665));
#56200=CARTESIAN_POINT('Ctrl Pts',(3.01229565803106,-35.4173125800988,0.327412687632905));
#56201=CARTESIAN_POINT('Ctrl Pts',(3.0176461231883,-35.4160018511495,0.338028142723121));
#56202=CARTESIAN_POINT('Ctrl Pts',(3.02235637061599,-35.4146845316183,0.348942894945375));
#56203=CARTESIAN_POINT('Ctrl Pts',(3.02459478869408,-35.4140585110326,0.354129836622479));
#56204=CARTESIAN_POINT('Ctrl Pts',(3.02668885469369,-35.4134305994858,0.359384645117005));
#56205=CARTESIAN_POINT('Ctrl Pts',(3.0286346903702,-35.4128001572719,0.364701596418767));
#56206=CARTESIAN_POINT('Ctrl Pts',(3.03270900261687,-35.4114800979968,0.375834561070054));
#56207=CARTESIAN_POINT('Ctrl Pts',(3.03613450666436,-35.4101527558927,0.387242594903746));
#56208=CARTESIAN_POINT('Ctrl Pts',(3.03887458843745,-35.4087853617665,0.398842878730332));
#56209=CARTESIAN_POINT('Ctrl Pts',(3.040216923218,-35.4081154909939,0.404525725351026));
#56210=CARTESIAN_POINT('Ctrl Pts',(3.04139473737179,-35.4074348945344,0.410254824444013));
#56211=CARTESIAN_POINT('Ctrl Pts',(3.04240435417873,-35.4067400123833,0.416016088194172));
#56212=CARTESIAN_POINT('Ctrl Pts',(3.04355345657699,-35.4059491274249,0.422573310644067));
#56213=CARTESIAN_POINT('Ctrl Pts',(3.04448461205505,-35.4051386165017,0.429172218461528));
#56214=CARTESIAN_POINT('Ctrl Pts',(3.0451946497264,-35.4043135059583,0.435785984618936));
#56215=CARTESIAN_POINT('Ctrl Pts',(3.04531298939742,-35.4041759874657,0.436888279529325));
#56216=CARTESIAN_POINT('Ctrl Pts',(3.04542519152073,-35.4040380979892,0.437990972110662));
#56217=CARTESIAN_POINT('Ctrl Pts',(3.04553124611257,-35.4038999032468,0.439093919456291));
#56218=CARTESIAN_POINT('Ctrl Pts',(3.04562679829713,-35.4037753936965,0.440087643787353));
#56219=CARTESIAN_POINT('Ctrl Pts',(3.04571743289771,-35.4036505377665,0.441082415444004));
#56220=CARTESIAN_POINT('Ctrl Pts',(3.04580293259,-35.4035256929,0.442075691324));
#56221=CARTESIAN_POINT('',(2.97642257165,-36.1242356128,0.274612461872));
#56222=CARTESIAN_POINT('Origin',(-1.14194680047E-14,-36.1242356128,2.77999550541));
#56223=CARTESIAN_POINT('',(2.97099134009343,-35.4239899492211,0.268174258363064));
#56224=CARTESIAN_POINT('Origin',(-0.668003013044919,-15.7697206409511,-2.44335760989475));
#56225=CARTESIAN_POINT('',(1.05706468499156E-8,-35.5025703486183,-1.11050957416386));
#56226=CARTESIAN_POINT('Ctrl Pts',(2.35228951035953E-7,-35.502578684161,
-1.11051031257002));
#56227=CARTESIAN_POINT('Ctrl Pts',(0.241185384589035,-35.4960792051353,
-1.11050007271629));
#56228=CARTESIAN_POINT('Ctrl Pts',(0.484484691878602,-35.4895467242639,
-1.09177342402401));
#56229=CARTESIAN_POINT('Ctrl Pts',(0.724399361223006,-35.4822690330674,
-1.05406906565677));
#56230=CARTESIAN_POINT('Ctrl Pts',(1.38288114101671,-35.4625880852057,-0.897498063662974));
#56231=CARTESIAN_POINT('Ctrl Pts',(1.99837189146,-35.4437584036,-0.600230058024));
#56232=CARTESIAN_POINT('Ctrl Pts',(2.36450092427,-35.4339226943,-0.355565614957));
#56233=CARTESIAN_POINT('Ctrl Pts',(2.69092668038,-35.4272067546,-0.063087197317));
#56234=CARTESIAN_POINT('Ctrl Pts',(2.97099133973,-35.4239899499,0.268174257969));
#56235=CARTESIAN_POINT('',(-2.97099136809806,-35.4239899489092,0.268174291485618));
#56236=CARTESIAN_POINT('Ctrl Pts',(1.28924120788854E-7,-35.5025659486026,
-1.11050920496303));
#56237=CARTESIAN_POINT('Ctrl Pts',(-0.0429285569203519,-35.501411371073,
-1.1105075801006));
#56238=CARTESIAN_POINT('Ctrl Pts',(-0.0888321496125025,-35.5001747157574,
-1.10979779951855));
#56239=CARTESIAN_POINT('Ctrl Pts',(-0.13767716483008,-35.4988459736367,
-1.10806788123278));
#56240=CARTESIAN_POINT('Ctrl Pts',(-0.187515186117301,-35.4974902185449,
-1.10630279417186));
#56241=CARTESIAN_POINT('Ctrl Pts',(-0.240415157899067,-35.496038308208,
-1.10347576735259));
#56242=CARTESIAN_POINT('Ctrl Pts',(-0.296310996488047,-35.4944803392224,
-1.09921026463204));
#56243=CARTESIAN_POINT('Ctrl Pts',(-0.319133473410654,-35.4938442147431,
-1.09746864414901));
#56244=CARTESIAN_POINT('Ctrl Pts',(-0.342455076056133,-35.49319044283,-1.0954866896958));
#56245=CARTESIAN_POINT('Ctrl Pts',(-0.366270077451304,-35.4925185684443,
-1.09323663399743));
#56246=CARTESIAN_POINT('Ctrl Pts',(-0.427112374729311,-35.4908020713328,
-1.08748821704709));
#56247=CARTESIAN_POINT('Ctrl Pts',(-0.49117761483286,-35.4889758457042,
-1.07999285810841));
#56248=CARTESIAN_POINT('Ctrl Pts',(-0.558324085371852,-35.4870390748949,
-1.07025766102687));
#56249=CARTESIAN_POINT('Ctrl Pts',(-0.56804788363689,-35.4867586019455,
-1.06884786105181));
#56250=CARTESIAN_POINT('Ctrl Pts',(-0.577836253131251,-35.4864758297699,
-1.06739101520041));
#56251=CARTESIAN_POINT('Ctrl Pts',(-0.58768871401166,-35.4861907759962,
-1.06588555345568));
#56252=CARTESIAN_POINT('Ctrl Pts',(-0.626632411505944,-35.4850640475507,
-1.0599349338605));
#56253=CARTESIAN_POINT('Ctrl Pts',(-0.666576942127623,-35.4839012711429,
-1.05322514711936));
#56254=CARTESIAN_POINT('Ctrl Pts',(-0.707485482952031,-35.482702446971,
-1.04565773996551));
#56255=CARTESIAN_POINT('Ctrl Pts',(-0.727939753364235,-35.482103034885,
-1.04187403638858));
#56256=CARTESIAN_POINT('Ctrl Pts',(-0.748635013460178,-35.4814946108542,
-1.03787586244271));
#56257=CARTESIAN_POINT('Ctrl Pts',(-0.769565863763876,-35.4808771748401,
-1.03365067292279));
#56258=CARTESIAN_POINT('Ctrl Pts',(-0.780031288915725,-35.480568456833,
-1.03153807816284));
#56259=CARTESIAN_POINT('Ctrl Pts',(-0.790555611097553,-35.4802574858298,
-1.02936872577934));
#56260=CARTESIAN_POINT('Ctrl Pts',(-0.801138124773163,-35.4799442618238,
-1.02714103006202));
#56261=CARTESIAN_POINT('Ctrl Pts',(-0.809329380747585,-35.4797018148883,
-1.02541671139699));
#56262=CARTESIAN_POINT('Ctrl Pts',(-0.8167401543102,-35.4794822111352,-1.02383326583324));
#56263=CARTESIAN_POINT('Ctrl Pts',(-0.825263582189491,-35.4792289838017,
-1.0219824928238));
#56264=CARTESIAN_POINT('Ctrl Pts',(-0.827751810200008,-35.4791550596302,
-1.02144220019642));
#56265=CARTESIAN_POINT('Ctrl Pts',(-0.830334803420739,-35.4790782692507,
-1.02087881128024));
#56266=CARTESIAN_POINT('Ctrl Pts',(-0.833059501712441,-35.4789972063979,
-1.02028131764937));
#56267=CARTESIAN_POINT('Ctrl Pts',(-0.896234129185903,-35.4771176898513,
-1.00642788012826));
#56268=CARTESIAN_POINT('Ctrl Pts',(-0.956086609344959,-35.4753254377988,
-0.991656089473372));
#56269=CARTESIAN_POINT('Ctrl Pts',(-1.01266007696826,-35.4736283141261,
-0.976403962012024));
#56270=CARTESIAN_POINT('Ctrl Pts',(-1.06934213433761,-35.4719279329152,
-0.961122558907563));
#56271=CARTESIAN_POINT('Ctrl Pts',(-1.12273264082248,-35.4703228587348,
-0.945359005522279));
#56272=CARTESIAN_POINT('Ctrl Pts',(-1.17288344770512,-35.4688128161094,
-0.929502923302393));
#56273=CARTESIAN_POINT('Ctrl Pts',(-1.18001070035384,-35.4685982142721,
-0.927249513815593));
#56274=CARTESIAN_POINT('Ctrl Pts',(-1.18707253564867,-35.4683855215034,
-0.92499415151587));
#56275=CARTESIAN_POINT('Ctrl Pts',(-1.19406911857269,-35.4681747277853,
-0.922737871423588));
#56276=CARTESIAN_POINT('Ctrl Pts',(-1.23876490132943,-35.4668281289759,
-0.908324234661447));
#56277=CARTESIAN_POINT('Ctrl Pts',(-1.28079731020406,-35.465559275466,-0.893875904218736));
#56278=CARTESIAN_POINT('Ctrl Pts',(-1.3202373196139,-35.4643698991371,-0.879643438297542));
#56279=CARTESIAN_POINT('Ctrl Pts',(-1.36483738969774,-35.4630249129564,
-0.863548894025125));
#56280=CARTESIAN_POINT('Ctrl Pts',(-1.40611459487719,-35.4617817653164,
-0.847734025493257));
#56281=CARTESIAN_POINT('Ctrl Pts',(-1.44416237838903,-35.460639586592,-0.832516813766869));
#56282=CARTESIAN_POINT('Ctrl Pts',(-1.48259275197378,-35.4594859226719,
-0.817146585133672));
#56283=CARTESIAN_POINT('Ctrl Pts',(-1.51772886531389,-35.4584351742648,
-0.802386075087822));
#56284=CARTESIAN_POINT('Ctrl Pts',(-1.54966719455541,-35.4574841305407,
-0.788509495887233));
#56285=CARTESIAN_POINT('Ctrl Pts',(-1.57705388851693,-35.4566686231539,
-0.776610513165711));
#56286=CARTESIAN_POINT('Ctrl Pts',(-1.60208946323774,-35.455926364652,-0.76536053708072));
#56287=CARTESIAN_POINT('Ctrl Pts',(-1.62483092434311,-35.4552547109233,
-0.75490221309079));
#56288=CARTESIAN_POINT('Ctrl Pts',(-1.62604898179027,-35.4552187364174,
-0.754342053857323));
#56289=CARTESIAN_POINT('Ctrl Pts',(-1.62726045663906,-35.4551829644016,
-0.753784159209078));
#56290=CARTESIAN_POINT('Ctrl Pts',(-1.62846535718975,-35.4551473944535,
-0.753228548869446));
#56291=CARTESIAN_POINT('Ctrl Pts',(-1.62907016078648,-35.4551295400068,
-0.752949658523185));
#56292=CARTESIAN_POINT('Ctrl Pts',(-1.62940227027742,-35.4551197369896,
-0.752796401278891));
#56293=CARTESIAN_POINT('Ctrl Pts',(-1.62986987180753,-35.4551059353078,
-0.752580552869857));
#56294=CARTESIAN_POINT('Ctrl Pts',(-1.63010321593046,-35.4550990479451,
-0.752472839454802));
#56295=CARTESIAN_POINT('Ctrl Pts',(-1.63037029720969,-35.4550911650331,
-0.752349530937011));
#56296=CARTESIAN_POINT('Ctrl Pts',(-1.63072180996005,-35.4550807909207,
-0.752187167151381));
#56297=CARTESIAN_POINT('Ctrl Pts',(-1.63091011889002,-35.455075233404,-0.752100187231861));
#56298=CARTESIAN_POINT('Ctrl Pts',(-1.63112265799355,-35.455068960974,-0.752001998070547));
#56299=CARTESIAN_POINT('Ctrl Pts',(-1.63136721640979,-35.4550617439627,
-0.751888982288285));
#56300=CARTESIAN_POINT('Ctrl Pts',(-1.63155281040024,-35.4550562670139,
-0.751803215254229));
#56301=CARTESIAN_POINT('Ctrl Pts',(-1.63175684491654,-35.4550502460645,
-0.751708909138482));
#56302=CARTESIAN_POINT('Ctrl Pts',(-1.63198272234932,-35.4550435808507,
-0.75160447847866));
#56303=CARTESIAN_POINT('Ctrl Pts',(-1.63212306043723,-35.4550394397404,
-0.751539595506779));
#56304=CARTESIAN_POINT('Ctrl Pts',(-1.63226874903872,-35.4550351408601,
-0.751472228292576));
#56305=CARTESIAN_POINT('Ctrl Pts',(-1.63241217610713,-35.4550309088282,
-0.751405896014871));
#56306=CARTESIAN_POINT('Ctrl Pts',(-1.72111413665979,-35.4524136237535,
-0.710382934689245));
#56307=CARTESIAN_POINT('Ctrl Pts',(-1.80669687851978,-35.4499330427393,
-0.666746612081371));
#56308=CARTESIAN_POINT('Ctrl Pts',(-1.88910495946924,-35.4476091955558,
-0.620961007577427));
#56309=CARTESIAN_POINT('Ctrl Pts',(-1.97097206739186,-35.4453006034132,
-0.575475965551931));
#56310=CARTESIAN_POINT('Ctrl Pts',(-2.04970609269493,-35.4431465042315,
-0.527870081781686));
#56311=CARTESIAN_POINT('Ctrl Pts',(-2.12529624088428,-35.4411565189214,
-0.47857300423023));
#56312=CARTESIAN_POINT('Ctrl Pts',(-2.20107691690407,-35.4391615177779,
-0.429151671528354));
#56313=CARTESIAN_POINT('Ctrl Pts',(-2.27369798971146,-35.4373313167143,
-0.378030843835462));
#56314=CARTESIAN_POINT('Ctrl Pts',(-2.34319122334006,-35.4356679682213,
-0.325613711291171));
#56315=CARTESIAN_POINT('Ctrl Pts',(-2.41869584596948,-35.4338607347151,
-0.2686623276036));
#56316=CARTESIAN_POINT('Ctrl Pts',(-2.49051042940222,-35.4322503580634,
-0.210179038333438));
#56317=CARTESIAN_POINT('Ctrl Pts',(-2.55871897458397,-35.4308321175166,
-0.15064584251512));
#56318=CARTESIAN_POINT('Ctrl Pts',(-2.6234258658855,-35.4294866858459,-0.0941689301226338));
#56319=CARTESIAN_POINT('Ctrl Pts',(-2.68488662251831,-35.4283140496414,
-0.0367481610854193));
#56320=CARTESIAN_POINT('Ctrl Pts',(-2.74321026116799,-35.4273054357926,
0.021236660147039));
#56321=CARTESIAN_POINT('Ctrl Pts',(-2.80304899701284,-35.4262706207663,
0.080727776975007));
#56322=CARTESIAN_POINT('Ctrl Pts',(-2.85958585165633,-35.4254083825495,
0.14081243092363));
#56323=CARTESIAN_POINT('Ctrl Pts',(-2.9129769049787,-35.4247056624346,0.2011197359036));
#56324=CARTESIAN_POINT('Ctrl Pts',(-2.93274284262472,-35.4244455079497,
0.22344614371272));
#56325=CARTESIAN_POINT('Ctrl Pts',(-2.95207797270929,-35.4242071876201,
0.24580346143632));
#56326=CARTESIAN_POINT('Ctrl Pts',(-2.97099133978,-35.4239899499,0.268174257926));
#56327=CARTESIAN_POINT('',(-2.97642257185497,-35.4237537116948,0.274612461610598));
#56328=CARTESIAN_POINT('Origin',(0.668003013044919,-15.7697206409511,-2.44335760989475));
#56329=CARTESIAN_POINT('',(-2.97642257165,-36.1242356128,0.274612461872));
#56330=CARTESIAN_POINT('Origin',(-2.74690825827,-36.1242356128,0.467804542343));
#56331=CARTESIAN_POINT('',(-3.04580294830777,-35.403525641014,0.442075686711237));
#56332=CARTESIAN_POINT('Ctrl Pts',(-2.97642257183112,-35.4237537093279,
0.274612461466193));
#56333=CARTESIAN_POINT('Ctrl Pts',(-2.98268497977946,-35.4228712901646,
0.282052265727931));
#56334=CARTESIAN_POINT('Ctrl Pts',(-2.98861404818367,-35.4219372537485,
0.289833403879585));
#56335=CARTESIAN_POINT('Ctrl Pts',(-2.99415416837544,-35.4209522031331,
0.297895150451187));
#56336=CARTESIAN_POINT('Ctrl Pts',(-2.99845521021089,-35.4201874645066,
0.304153843055496));
#56337=CARTESIAN_POINT('Ctrl Pts',(-3.00252275175911,-35.419393257241,0.310582180982538));
#56338=CARTESIAN_POINT('Ctrl Pts',(-3.0063416756095,-35.418580198429,0.317158978249665));
#56339=CARTESIAN_POINT('Ctrl Pts',(-3.01229565803106,-35.4173125800988,
0.327412687632905));
#56340=CARTESIAN_POINT('Ctrl Pts',(-3.0176461231883,-35.4160018511495,0.338028142723121));
#56341=CARTESIAN_POINT('Ctrl Pts',(-3.02235637061599,-35.4146845316183,
0.348942894945375));
#56342=CARTESIAN_POINT('Ctrl Pts',(-3.02459478869408,-35.4140585110326,
0.354129836622479));
#56343=CARTESIAN_POINT('Ctrl Pts',(-3.02668885469369,-35.4134305994858,
0.359384645117005));
#56344=CARTESIAN_POINT('Ctrl Pts',(-3.0286346903702,-35.4128001572719,0.364701596418767));
#56345=CARTESIAN_POINT('Ctrl Pts',(-3.03270900261686,-35.4114800979968,
0.375834561070049));
#56346=CARTESIAN_POINT('Ctrl Pts',(-3.03613450666436,-35.4101527558927,
0.387242594903735));
#56347=CARTESIAN_POINT('Ctrl Pts',(-3.03887458843745,-35.4087853617665,
0.398842878730315));
#56348=CARTESIAN_POINT('Ctrl Pts',(-3.04021692321799,-35.4081154909939,
0.404525725351014));
#56349=CARTESIAN_POINT('Ctrl Pts',(-3.04139473737179,-35.4074348945344,
0.410254824444007));
#56350=CARTESIAN_POINT('Ctrl Pts',(-3.04240435417873,-35.4067400123833,
0.416016088194172));
#56351=CARTESIAN_POINT('Ctrl Pts',(-3.04355345657699,-35.4059491274249,
0.422573310644067));
#56352=CARTESIAN_POINT('Ctrl Pts',(-3.04448461205505,-35.4051386165017,
0.429172218461528));
#56353=CARTESIAN_POINT('Ctrl Pts',(-3.0451946497264,-35.4043135059583,0.435785984618936));
#56354=CARTESIAN_POINT('Ctrl Pts',(-3.04531298939742,-35.4041759874657,
0.436888279529325));
#56355=CARTESIAN_POINT('Ctrl Pts',(-3.04542519152073,-35.4040380979892,
0.437990972110662));
#56356=CARTESIAN_POINT('Ctrl Pts',(-3.04553124611257,-35.4038999032468,
0.439093919456291));
#56357=CARTESIAN_POINT('Ctrl Pts',(-3.04562679829713,-35.4037753936965,
0.440087643787354));
#56358=CARTESIAN_POINT('Ctrl Pts',(-3.04571743289771,-35.4036505377665,
0.441082415444004));
#56359=CARTESIAN_POINT('Ctrl Pts',(-3.04580293259,-35.4035256929,0.442075691324));
#56360=CARTESIAN_POINT('',(-3.04626146311845,-35.4033959728417,0.448115484591892));
#56361=CARTESIAN_POINT('Origin',(-2.97884827228343,-36.1481218195378,0.517617073024758));
#56362=CARTESIAN_POINT('',(-3.0462613877,-35.8888189474,0.448114344193));
#56363=CARTESIAN_POINT('Origin',(-3.0399446742,-32.4742356128,0.352080371467));
#56364=CARTESIAN_POINT('',(-3.16549337405758,-35.4651789109462,2.2608166833054));
#56365=CARTESIAN_POINT('Ctrl Pts',(-3.04626151745,-35.4033927946,0.44811631692));
#56366=CARTESIAN_POINT('Ctrl Pts',(-3.05294917186292,-35.4075920678871,
0.54978975953267));
#56367=CARTESIAN_POINT('Ctrl Pts',(-3.05964380945705,-35.4116947932727,
0.651569369125652));
#56368=CARTESIAN_POINT('Ctrl Pts',(-3.06633992560627,-35.415674424655,0.753371458620691));
#56369=CARTESIAN_POINT('Ctrl Pts',(-3.07076632608472,-35.4183051201002,
0.820666709719363));
#56370=CARTESIAN_POINT('Ctrl Pts',(-3.07519346050157,-35.4208822031628,
0.887973119277269));
#56371=CARTESIAN_POINT('Ctrl Pts',(-3.07962053317529,-35.4233996000391,
0.955278587451633));
#56372=CARTESIAN_POINT('Ctrl Pts',(-3.08757598305296,-35.4279233623867,
1.07622651806343));
#56373=CARTESIAN_POINT('Ctrl Pts',(-3.09554993432824,-35.4322756333094,
1.19745572859944));
#56374=CARTESIAN_POINT('Ctrl Pts',(-3.1035355348744,-35.436446582721,1.31886204931956));
#56375=CARTESIAN_POINT('Ctrl Pts',(-3.11356049330213,-35.4416827066937,
1.4712730434643));
#56376=CARTESIAN_POINT('Ctrl Pts',(-3.12360407993771,-35.4466333489527,
1.62396725231298));
#56377=CARTESIAN_POINT('Ctrl Pts',(-3.13365681361424,-35.4513048687405,
1.77680052285598));
#56378=CARTESIAN_POINT('Ctrl Pts',(-3.14185238055683,-35.4551133604778,
1.90139899925985));
#56379=CARTESIAN_POINT('Ctrl Pts',(-3.1500542552448,-35.458737299182,2.02609337075293));
#56380=CARTESIAN_POINT('Ctrl Pts',(-3.15825582228844,-35.4621835807125,
2.15078306376108));
#56381=CARTESIAN_POINT('Ctrl Pts',(-3.16011434868282,-35.4629645296644,
2.1790385281533));
#56382=CARTESIAN_POINT('Ctrl Pts',(-3.16197284588705,-35.4637363447115,
2.20729354873488));
#56383=CARTESIAN_POINT('Ctrl Pts',(-3.16383120921194,-35.4644990738493,
2.23554653393125));
#56384=CARTESIAN_POINT('Ctrl Pts',(-3.16438523801469,-35.4647264642123,
2.24396951955144));
#56385=CARTESIAN_POINT('Ctrl Pts',(-3.16493929387688,-35.4649530731761,
2.25239291656041));
#56386=CARTESIAN_POINT('Ctrl Pts',(-3.16549337399,-35.4651789177,2.26081668226));
#56387=CARTESIAN_POINT('Origin',(-3.16701457909211,-35.4948316439558,2.28394383708707));
#56388=CARTESIAN_POINT('Ctrl Pts',(-3.21673308013,-35.297826519,2.26193293676));
#56389=CARTESIAN_POINT('Ctrl Pts',(-3.19690170746,-35.3272920967,2.26244743731));
#56390=CARTESIAN_POINT('Ctrl Pts',(-3.18141841353,-35.3596904513,2.26259731642));
#56391=CARTESIAN_POINT('Ctrl Pts',(-3.17086410369,-35.3941615562,2.26236742048));
#56392=CARTESIAN_POINT('Ctrl Pts',(-3.16555572757,-35.4296702319,2.26176465335));
#56393=CARTESIAN_POINT('Ctrl Pts',(-3.16549338332,-35.4651789077,2.26081682416));
#56394=CARTESIAN_POINT('Ctrl Pts',(-3.22044227874,-35.2947170616,2.28115435818));
#56395=CARTESIAN_POINT('Ctrl Pts',(-3.19950860612,-35.3245433432,2.27888894627));
#56396=CARTESIAN_POINT('Ctrl Pts',(-3.18307576937,-35.3575027832,2.27596054224));
#56397=CARTESIAN_POINT('Ctrl Pts',(-3.17178564006,-35.3926825601,2.27243438801));
#56398=CARTESIAN_POINT('Ctrl Pts',(-3.16599327189,-35.4289738974,2.26841670742));
#56399=CARTESIAN_POINT('Ctrl Pts',(-3.16570519157,-35.4652652348,2.26403697776));
#56400=CARTESIAN_POINT('Ctrl Pts',(-3.22504500396,-35.2927962885,2.30073764763));
#56401=CARTESIAN_POINT('Ctrl Pts',(-3.20268941154,-35.3227611226,2.2957495854));
#56402=CARTESIAN_POINT('Ctrl Pts',(-3.18504154424,-35.3561044246,2.28975874044));
#56403=CARTESIAN_POINT('Ctrl Pts',(-3.1728278134,-35.3918504917,2.28291889281));
#56404=CARTESIAN_POINT('Ctrl Pts',(-3.16645576111,-35.428799749,2.27544850897));
#56405=CARTESIAN_POINT('Ctrl Pts',(-3.16593909074,-35.4657490064,2.26759298308));
#56406=CARTESIAN_POINT('Ctrl Pts',(-3.23041275638,-35.292377214,2.32058136088));
#56407=CARTESIAN_POINT('Ctrl Pts',(-3.20637961829,-35.3222393286,2.31311572454));
#56408=CARTESIAN_POINT('Ctrl Pts',(-3.18729883271,-35.3557626768,2.30425560397));
#56409=CARTESIAN_POINT('Ctrl Pts',(-3.1740077501,-35.391902145,2.29425266577));
#56410=CARTESIAN_POINT('Ctrl Pts',(-3.16698247964,-35.4293517376,2.28345602024));
#56411=CARTESIAN_POINT('Ctrl Pts',(-3.16624513219,-35.4668013301,2.2722457786));
#56412=CARTESIAN_POINT('Ctrl Pts',(-3.2362706081,-35.293523699,2.3402171845));
#56413=CARTESIAN_POINT('Ctrl Pts',(-3.21039981727,-35.3231016776,2.33049644021));
#56414=CARTESIAN_POINT('Ctrl Pts',(-3.18974009686,-35.3566452436,2.31893365909));
#56415=CARTESIAN_POINT('Ctrl Pts',(-3.17526480943,-35.3930381712,2.30588852441));
#56416=CARTESIAN_POINT('Ctrl Pts',(-3.16753533529,-35.4308584528,2.2918609559));
#56417=CARTESIAN_POINT('Ctrl Pts',(-3.16658333925,-35.4686787344,2.27738759286));
#56418=CARTESIAN_POINT('Ctrl Pts',(-3.24268782164,-35.2959076878,2.35939290014));
#56419=CARTESIAN_POINT('Ctrl Pts',(-3.21479367828,-35.3250197311,2.34761644611));
#56420=CARTESIAN_POINT('Ctrl Pts',(-3.19237820629,-35.3584237245,2.33347294503));
#56421=CARTESIAN_POINT('Ctrl Pts',(-3.17658501762,-35.3949324563,2.31744225071));
#56422=CARTESIAN_POINT('Ctrl Pts',(-3.16808413932,-35.4329970413,2.30020446638));
#56423=CARTESIAN_POINT('Ctrl Pts',(-3.16691857253,-35.4710616262,2.28248419619));
#56424=CARTESIAN_POINT('',(-3.21673309784852,-35.2978264918237,2.26193292933744));
#56425=CARTESIAN_POINT('Origin',(-3.46485248098951,-35.4651807159992,2.24112377406711));
#56426=CARTESIAN_POINT('Ctrl Pts',(-3.2167330984,-35.297826491,2.26193292922));
#56427=CARTESIAN_POINT('Ctrl Pts',(-3.22044227874,-35.2947170616,2.28115435818));
#56428=CARTESIAN_POINT('Ctrl Pts',(-3.22504500396,-35.2927962885,2.30073764763));
#56429=CARTESIAN_POINT('Ctrl Pts',(-3.23041275638,-35.292377214,2.32058136088));
#56430=CARTESIAN_POINT('Ctrl Pts',(-3.2362706081,-35.293523699,2.3402171845));
#56431=CARTESIAN_POINT('Ctrl Pts',(-3.24268782426,-35.2959076878,2.35939289968));
#56432=CARTESIAN_POINT('Ctrl Pts',(-3.05220590584922,-35.3446113342728,
0.449759468615835));
#56433=CARTESIAN_POINT('Ctrl Pts',(-3.04985791657899,-35.3562114182906,
0.449434297522738));
#56434=CARTESIAN_POINT('Ctrl Pts',(-3.04808113948102,-35.367925917271,0.449066823931494));
#56435=CARTESIAN_POINT('Ctrl Pts',(-3.04688319620433,-35.3797171894883,
0.44865810283722));
#56436=CARTESIAN_POINT('Ctrl Pts',(-3.04626798656282,-35.3915468489271,
0.448209464821468));
#56437=CARTESIAN_POINT('Ctrl Pts',(-3.0462356131786,-35.4033765082655,0.447722490273414));
#56438=CARTESIAN_POINT('Ctrl Pts',(-3.08188318868537,-35.3301475098315,
0.811344942556501));
#56439=CARTESIAN_POINT('Ctrl Pts',(-3.07718994972766,-35.3473935565693,
0.81096891066994));
#56440=CARTESIAN_POINT('Ctrl Pts',(-3.07363512368023,-35.3649271660184,
0.810506388572203));
#56441=CARTESIAN_POINT('Ctrl Pts',(-3.07124167037135,-35.3826542366648,
0.809959664856562));
#56442=CARTESIAN_POINT('Ctrl Pts',(-3.07002134535006,-35.4004780406225,
0.809331871876777));
#56443=CARTESIAN_POINT('Ctrl Pts',(-3.06997439732721,-35.4183018444796,
0.808626899063583));
#56444=CARTESIAN_POINT('Ctrl Pts',(-3.11480925207767,-35.3179426439912,
1.17419373715894));
#56445=CARTESIAN_POINT('Ctrl Pts',(-3.10654154250054,-35.3399109405316,
1.17393374594204));
#56446=CARTESIAN_POINT('Ctrl Pts',(-3.10026058630755,-35.3625419436199,
1.17351742209672));
#56447=CARTESIAN_POINT('Ctrl Pts',(-3.09603218734286,-35.3856208231373,
1.17294874807696));
#56448=CARTESIAN_POINT('Ctrl Pts',(-3.09389012681207,-35.4089236557388,
1.17223417157854));
#56449=CARTESIAN_POINT('Ctrl Pts',(-3.09383493395118,-35.4322264883404,
1.17138232965865));
#56450=CARTESIAN_POINT('Ctrl Pts',(-3.1489742418356,-35.3091111400076,1.53615855019239));
#56451=CARTESIAN_POINT('Ctrl Pts',(-3.13669434443428,-35.3344038135106,
1.53611929468437));
#56452=CARTESIAN_POINT('Ctrl Pts',(-3.12728783123044,-35.3610192894964,
1.53584317267495));
#56453=CARTESIAN_POINT('Ctrl Pts',(-3.12093413395616,-35.388538471225,1.53533340697713));
#56454=CARTESIAN_POINT('Ctrl Pts',(-3.11772590791843,-35.4165095347782,
1.5346003353224));
#56455=CARTESIAN_POINT('Ctrl Pts',(-3.11766406573072,-35.4444805983314,
1.53366030754776));
#56456=CARTESIAN_POINT('Ctrl Pts',(-3.18313684691208,-35.302468660032,1.89896579328351));
#56457=CARTESIAN_POINT('Ctrl Pts',(-3.1669425809763,-35.3302070617239,1.89920832725791));
#56458=CARTESIAN_POINT('Ctrl Pts',(-3.15441608130232,-35.3600495371066,
1.8991452966041));
#56459=CARTESIAN_POINT('Ctrl Pts',(-3.14591669935255,-35.3913550667249,
1.89877256662065));
#56460=CARTESIAN_POINT('Ctrl Pts',(-3.14163538349214,-35.4233924917858,
1.89809997064137));
#56461=CARTESIAN_POINT('Ctrl Pts',(-3.14157289101662,-35.4554299168467,
1.89714987809648));
#56462=CARTESIAN_POINT('Ctrl Pts',(-3.21697740925793,-35.2975133737574,
2.26232402686368));
#56463=CARTESIAN_POINT('Ctrl Pts',(-3.19706412796009,-35.32701786522,2.26284293679389));
#56464=CARTESIAN_POINT('Ctrl Pts',(-3.18151421558404,-35.3594737404149,
2.26299572724175));
#56465=CARTESIAN_POINT('Ctrl Pts',(-3.17091358409877,-35.3940160628362,
2.26276704500176));
#56466=CARTESIAN_POINT('Ctrl Pts',(-3.16558198118586,-35.4296028155102,
2.26216379089102));
#56467=CARTESIAN_POINT('Ctrl Pts',(-3.16551950497327,-35.4651895681841,
2.2612139556422));
#56468=CARTESIAN_POINT('',(-3.0522160941314,-35.3447053607003,0.450150554362896));
#56469=CARTESIAN_POINT('Origin',(-3.3455585084964,-35.4033872464943,0.428430041357342));
#56470=CARTESIAN_POINT('Ctrl Pts',(-3.0522160941314,-35.3447053607003,0.450150554362896));
#56471=CARTESIAN_POINT('Ctrl Pts',(-3.06245426700421,-35.3397367883934,
0.574985908505038));
#56472=CARTESIAN_POINT('Ctrl Pts',(-3.0731265985084,-35.3351675822744,0.699868808724409));
#56473=CARTESIAN_POINT('Ctrl Pts',(-3.0840963191387,-35.3309723772982,0.824833541278553));
#56474=CARTESIAN_POINT('Ctrl Pts',(-3.09693619197235,-35.3260619606868,
0.971102651382724));
#56475=CARTESIAN_POINT('Ctrl Pts',(-3.1101827780043,-35.3216639371358,1.11748237059042));
#56476=CARTESIAN_POINT('Ctrl Pts',(-3.12364374625223,-35.3177376313134,
1.26396179960472));
#56477=CARTESIAN_POINT('Ctrl Pts',(-3.13890997728794,-35.3132847650189,
1.43008571908232));
#56478=CARTESIAN_POINT('Ctrl Pts',(-3.15445073095059,-35.3094386256381,
1.59633247350827));
#56479=CARTESIAN_POINT('Ctrl Pts',(-3.17003379270651,-35.3061398799808,
1.762664238938));
#56480=CARTESIAN_POINT('Ctrl Pts',(-3.18219023638189,-35.3035665079176,
1.89242068664661));
#56481=CARTESIAN_POINT('Ctrl Pts',(-3.19437337743973,-35.3013262609218,
2.02222732843154));
#56482=CARTESIAN_POINT('Ctrl Pts',(-3.20649671361591,-35.2993909708028,
2.15209574766422));
#56483=CARTESIAN_POINT('Ctrl Pts',(-3.20991399946423,-35.2988454576338,
2.18870262754769));
#56484=CARTESIAN_POINT('Ctrl Pts',(-3.21332666694494,-35.298324174651,2.22531468874872));
#56485=CARTESIAN_POINT('Ctrl Pts',(-3.21673309838426,-35.2978264909894,
2.26193292922132));
#56486=CARTESIAN_POINT('Ctrl Pts',(-3.05109049587,-35.3458529008,0.437996404741));
#56487=CARTESIAN_POINT('Ctrl Pts',(-3.04891977816,-35.3572426278,0.438898953129));
#56488=CARTESIAN_POINT('Ctrl Pts',(-3.04730060509,-35.3687406938,0.439760831884));
#56489=CARTESIAN_POINT('Ctrl Pts',(-3.04623977506,-35.3803114393,0.440579215085));
#56490=CARTESIAN_POINT('Ctrl Pts',(-3.04574061974,-35.3919185251,0.441351532501));
#56491=CARTESIAN_POINT('Ctrl Pts',(-3.04580294181,-35.4035256109,0.442075517619));
#56492=CARTESIAN_POINT('Ctrl Pts',(-3.05133592857,-35.3454968218,0.440376332259));
#56493=CARTESIAN_POINT('Ctrl Pts',(-3.049131145,-35.3569269779,0.441037311376));
#56494=CARTESIAN_POINT('Ctrl Pts',(-3.04748040649,-35.368466371,0.44165738234));
#56495=CARTESIAN_POINT('Ctrl Pts',(-3.04639064899,-35.3800790478,0.442234462677));
#56496=CARTESIAN_POINT('Ctrl Pts',(-3.04586531061,-35.3917283673,0.442766727044));
#56497=CARTESIAN_POINT('Ctrl Pts',(-3.04590426722,-35.4033776868,0.443252644519));
#56498=CARTESIAN_POINT('Ctrl Pts',(-3.05157202469,-35.345201709,0.44278366337));
#56499=CARTESIAN_POINT('Ctrl Pts',(-3.04933300313,-35.3566718646,0.443200875235));
#56500=CARTESIAN_POINT('Ctrl Pts',(-3.04765109714,-35.3682522692,0.443576907233));
#56501=CARTESIAN_POINT('Ctrl Pts',(-3.04653338889,-35.3799066391,0.443910429375));
#56502=CARTESIAN_POINT('Ctrl Pts',(-3.04598342453,-35.3915979921,0.44420038209));
#56503=CARTESIAN_POINT('Ctrl Pts',(-3.0460011471,-35.4032893451,0.444445979659));
#56504=CARTESIAN_POINT('Ctrl Pts',(-3.05179796269,-35.3449700438,0.445216729023));
#56505=CARTESIAN_POINT('Ctrl Pts',(-3.04952458771,-35.3564797113,0.445388154931));
#56506=CARTESIAN_POINT('Ctrl Pts',(-3.04781198307,-35.3681007576,0.445518095267));
#56507=CARTESIAN_POINT('Ctrl Pts',(-3.04666739039,-35.3797965316,0.445605990135));
#56508=CARTESIAN_POINT('Ctrl Pts',(-3.04609446477,-35.3915296692,0.44565156091));
#56509=CARTESIAN_POINT('Ctrl Pts',(-3.04609320711,-35.4032628068,0.445654782512));
#56510=CARTESIAN_POINT('Ctrl Pts',(-3.05201291474,-35.344804036,0.447673318567));
#56511=CARTESIAN_POINT('Ctrl Pts',(-3.04970513582,-35.3563526648,0.447597170527));
#56512=CARTESIAN_POINT('Ctrl Pts',(-3.04796238182,-35.3680139256,0.447479196662));
#56513=CARTESIAN_POINT('Ctrl Pts',(-3.04679206061,-35.3797507581,0.447319633895));
#56514=CARTESIAN_POINT('Ctrl Pts',(-3.04619793931,-35.3915253768,0.447118989828));
#56515=CARTESIAN_POINT('Ctrl Pts',(-3.04618007217,-35.4032999955,0.446878030094));
#56516=CARTESIAN_POINT('Ctrl Pts',(-3.05221609529,-35.3447053607,0.45015055449));
#56517=CARTESIAN_POINT('Ctrl Pts',(-3.04987393679,-35.3562923356,0.449825338819));
#56518=CARTESIAN_POINT('Ctrl Pts',(-3.04810166196,-35.3679933207,0.449457922766));
#56519=CARTESIAN_POINT('Ctrl Pts',(-3.04690685539,-35.3797708063,0.449049358968));
#56520=CARTESIAN_POINT('Ctrl Pts',(-3.04629339744,-35.3915865426,0.448600974315));
#56521=CARTESIAN_POINT('Ctrl Pts',(-3.0462613893,-35.403402279,0.448114344323));
#56522=CARTESIAN_POINT('',(-3.05109044990346,-35.3458530848237,0.437996448767244));
#56523=CARTESIAN_POINT('Origin',(-3.34464260822978,-35.4035208271414,0.416342692624979));
#56524=CARTESIAN_POINT('Origin',(-3.03578495082005,-35.4311381890655,0.45269626373329));
#56525=CARTESIAN_POINT('Ctrl Pts',(-2.98571747284,-35.3277286717,0.261093980788));
#56526=CARTESIAN_POINT('Ctrl Pts',(-2.981461349,-35.3462477664,0.265774778659));
#56527=CARTESIAN_POINT('Ctrl Pts',(-2.97837661309,-35.3652776361,0.269499859243));
#56528=CARTESIAN_POINT('Ctrl Pts',(-2.97650103488,-35.3846541126,0.272227694446));
#56529=CARTESIAN_POINT('Ctrl Pts',(-2.97585138777,-35.4042039111,0.273933889101));
#56530=CARTESIAN_POINT('Ctrl Pts',(-2.9764225699,-35.4237537096,0.274612459172));
#56531=CARTESIAN_POINT('Ctrl Pts',(-2.99904170374,-35.3293548375,0.278294108299));
#56532=CARTESIAN_POINT('Ctrl Pts',(-2.99483616983,-35.347248816,0.282402750811));
#56533=CARTESIAN_POINT('Ctrl Pts',(-2.99178501636,-35.3655962934,0.285705549944));
#56534=CARTESIAN_POINT('Ctrl Pts',(-2.98992270743,-35.3842510435,0.288169202034));
#56535=CARTESIAN_POINT('Ctrl Pts',(-2.98926461676,-35.4030594457,0.289773532404));
#56536=CARTESIAN_POINT('Ctrl Pts',(-2.98980629628,-35.4218678479,0.290512461752));
#56537=CARTESIAN_POINT('Ctrl Pts',(-3.01081156168,-35.3311436809,0.296626108381));
#56538=CARTESIAN_POINT('Ctrl Pts',(-3.00676278967,-35.3483431627,0.300206793547));
#56539=CARTESIAN_POINT('Ctrl Pts',(-3.00382878865,-35.3659388616,0.303127857359));
#56540=CARTESIAN_POINT('Ctrl Pts',(-3.00203974789,-35.3838026166,0.305362985112));
#56541=CARTESIAN_POINT('Ctrl Pts',(-3.00140909733,-35.4018004061,0.306895543103));
#56542=CARTESIAN_POINT('Ctrl Pts',(-3.00193290967,-35.4197981956,0.307719289765));
#56543=CARTESIAN_POINT('Ctrl Pts',(-3.0211060441,-35.3328533463,0.316096062934));
#56544=CARTESIAN_POINT('Ctrl Pts',(-3.01723125611,-35.3493133446,0.319149425303));
#56545=CARTESIAN_POINT('Ctrl Pts',(-3.01441086074,-35.3661160441,0.321674359752));
#56546=CARTESIAN_POINT('Ctrl Pts',(-3.01267195982,-35.3831506732,0.32365017578));
#56547=CARTESIAN_POINT('Ctrl Pts',(-3.01202647228,-35.4003009737,0.325063889692));
#56548=CARTESIAN_POINT('Ctrl Pts',(-3.01247041893,-35.4174512741,0.325909903855));
#56549=CARTESIAN_POINT('Ctrl Pts',(-3.03608811322,-35.3362145716,0.351770920136));
#56550=CARTESIAN_POINT('Ctrl Pts',(-3.03261306094,-35.3513090757,0.353941667697));
#56551=CARTESIAN_POINT('Ctrl Pts',(-3.03006547046,-35.366660463,0.355785992804));
#56552=CARTESIAN_POINT('Ctrl Pts',(-3.02846382328,-35.3821846623,0.357292574606));
#56553=CARTESIAN_POINT('Ctrl Pts',(-3.02781696962,-35.3977954963,0.3584530028));
#56554=CARTESIAN_POINT('Ctrl Pts',(-3.02812402787,-35.4134063304,0.35926266557));
#56555=CARTESIAN_POINT('Ctrl Pts',(-3.04544130267,-35.3402488915,0.389133416749));
#56556=CARTESIAN_POINT('Ctrl Pts',(-3.04250648845,-35.3538042987,0.390631987385));
#56557=CARTESIAN_POINT('Ctrl Pts',(-3.040339577,-35.3675437775,0.391955910767));
#56558=CARTESIAN_POINT('Ctrl Pts',(-3.03895408512,-35.3814072732,0.393098415575));
#56559=CARTESIAN_POINT('Ctrl Pts',(-3.03835622743,-35.3953326096,0.394054612964));
#56560=CARTESIAN_POINT('Ctrl Pts',(-3.03854461847,-35.4092579459,0.394821151154));
#56561=CARTESIAN_POINT('Ctrl Pts',(-3.04837800292,-35.3421028535,0.405371326337));
#56562=CARTESIAN_POINT('Ctrl Pts',(-3.04569735965,-35.354968334,0.406623296912));
#56563=CARTESIAN_POINT('Ctrl Pts',(-3.04371425581,-35.367989887,0.407755259395));
#56564=CARTESIAN_POINT('Ctrl Pts',(-3.04243717253,-35.3811153925,0.408763338852));
#56565=CARTESIAN_POINT('Ctrl Pts',(-3.0418710033,-35.3942935555,0.40964296396));
#56566=CARTESIAN_POINT('Ctrl Pts',(-3.0420174994,-35.4074717185,0.410390857869));
#56567=CARTESIAN_POINT('Ctrl Pts',(-3.0502457294,-35.3440064303,0.421621283978));
#56568=CARTESIAN_POINT('Ctrl Pts',(-3.04782750294,-35.3561342576,0.422702630881));
#56569=CARTESIAN_POINT('Ctrl Pts',(-3.04603083038,-35.3683919899,0.423709393311));
#56570=CARTESIAN_POINT('Ctrl Pts',(-3.04486559316,-35.3807375362,0.424637122745));
#56571=CARTESIAN_POINT('Ctrl Pts',(-3.04433601307,-35.3931265369,0.425482937737));
#56572=CARTESIAN_POINT('Ctrl Pts',(-3.04444019246,-35.4055155376,0.426244325555));
#56573=CARTESIAN_POINT('Ctrl Pts',(-3.05109044578,-35.345853084,0.437996449073));
#56574=CARTESIAN_POINT('Ctrl Pts',(-3.04891974336,-35.357242792,0.438899021788));
#56575=CARTESIAN_POINT('Ctrl Pts',(-3.0473005821,-35.368740838,0.439760925705));
#56576=CARTESIAN_POINT('Ctrl Pts',(-3.04623976029,-35.380311563,0.440579334845));
#56577=CARTESIAN_POINT('Ctrl Pts',(-3.04574060956,-35.391918628,0.441351678913));
#56578=CARTESIAN_POINT('Ctrl Pts',(-3.04580293259,-35.4035256929,0.442075691324));
#56579=CARTESIAN_POINT('',(-2.98571747517108,-35.3277286769967,0.261093984850969));
#56580=CARTESIAN_POINT('Origin',(-3.20593730394412,-35.4237537994827,0.0814200323574604));
#56581=CARTESIAN_POINT('Ctrl Pts',(-2.98571747472,-35.3277286768,0.261093985219));
#56582=CARTESIAN_POINT('Ctrl Pts',(-2.99904170374,-35.3293548375,0.278294108299));
#56583=CARTESIAN_POINT('Ctrl Pts',(-3.01081156168,-35.3311436809,0.296626108381));
#56584=CARTESIAN_POINT('Ctrl Pts',(-3.0211060441,-35.3328533463,0.316096062934));
#56585=CARTESIAN_POINT('Ctrl Pts',(-3.03608811322,-35.3362145716,0.351770920136));
#56586=CARTESIAN_POINT('Ctrl Pts',(-3.04544130267,-35.3402488915,0.389133416749));
#56587=CARTESIAN_POINT('Ctrl Pts',(-3.04837800292,-35.3421028535,0.405371326337));
#56588=CARTESIAN_POINT('Ctrl Pts',(-3.0502457294,-35.3440064303,0.421621283978));
#56589=CARTESIAN_POINT('Ctrl Pts',(-3.05109044571,-35.345853084,0.437996449075));
#56590=CARTESIAN_POINT('Ctrl Pts',(-2.98281092022,-35.3272070934,0.257308726577));
#56591=CARTESIAN_POINT('Ctrl Pts',(-2.97803806995,-35.345862362,0.261512162033));
#56592=CARTESIAN_POINT('Ctrl Pts',(-2.97443750788,-35.3650398118,0.264729196731));
#56593=CARTESIAN_POINT('Ctrl Pts',(-2.97205219293,-35.3845716985,0.266921998871));
#56594=CARTESIAN_POINT('Ctrl Pts',(-2.97090376513,-35.4042808232,0.268070674403));
#56595=CARTESIAN_POINT('Ctrl Pts',(-2.97099139651,-35.4239899479,0.268174325124));
#56596=CARTESIAN_POINT('Ctrl Pts',(-2.98353703291,-35.3273786743,0.258262507142));
#56597=CARTESIAN_POINT('Ctrl Pts',(-2.97889447281,-35.3460005999,0.262582653758));
#56598=CARTESIAN_POINT('Ctrl Pts',(-2.97542363609,-35.3651416718,0.26592442057));
#56599=CARTESIAN_POINT('Ctrl Pts',(-2.97316614056,-35.3846350952,0.268249073819));
#56600=CARTESIAN_POINT('Ctrl Pts',(-2.97214238275,-35.4043047141,0.26953560217));
#56601=CARTESIAN_POINT('Ctrl Pts',(-2.97235045678,-35.4239743331,0.269781826657));
#56602=CARTESIAN_POINT('Ctrl Pts',(-2.98426364409,-35.3275231471,0.259211611404));
#56603=CARTESIAN_POINT('Ctrl Pts',(-2.97975071316,-35.3461112518,0.263650265626));
#56604=CARTESIAN_POINT('Ctrl Pts',(-2.97640915872,-35.3652155879,0.267118330752));
#56605=CARTESIAN_POINT('Ctrl Pts',(-2.97427928943,-35.3846702746,0.269576156755));
#56606=CARTESIAN_POINT('Ctrl Pts',(-2.97338027656,-35.4043001557,0.271001608633));
#56607=CARTESIAN_POINT('Ctrl Pts',(-2.97370914102,-35.4239300369,0.271391235523));
#56608=CARTESIAN_POINT('Ctrl Pts',(-2.98499053061,-35.3276399509,0.260155575417));
#56609=CARTESIAN_POINT('Ctrl Pts',(-2.98060644818,-35.3461937726,0.264714470388));
#56610=CARTESIAN_POINT('Ctrl Pts',(-2.97739362648,-35.3652610343,0.268310331454));
#56611=CARTESIAN_POINT('Ctrl Pts',(-2.97539109347,-35.3846767315,0.270902576923));
#56612=CARTESIAN_POINT('Ctrl Pts',(-2.9746168118,-35.404266665,0.272467944099));
#56613=CARTESIAN_POINT('Ctrl Pts',(-2.97506673688,-35.4238565985,0.27300171487));
#56614=CARTESIAN_POINT('Ctrl Pts',(-2.98571747678,-35.3277286766,0.26109398396));
#56615=CARTESIAN_POINT('Ctrl Pts',(-2.98146135285,-35.3462477712,0.26577478149));
#56616=CARTESIAN_POINT('Ctrl Pts',(-2.97837661705,-35.3652776408,0.269499861748));
#56617=CARTESIAN_POINT('Ctrl Pts',(-2.97650103844,-35.384654117,0.272227696729));
#56618=CARTESIAN_POINT('Ctrl Pts',(-2.97585139066,-35.4042039153,0.273933891593));
#56619=CARTESIAN_POINT('Ctrl Pts',(-2.97642257226,-35.4237537135,0.274612461819));
#56620=CARTESIAN_POINT('',(-2.98281092160732,-35.3272070855929,0.257308724107702));
#56621=CARTESIAN_POINT('Origin',(-3.20008735670538,-35.4239900447452,0.074485419786941));
#56622=CARTESIAN_POINT('Ctrl Pts',(-2.98281092022,-35.3272070934,0.257308726577));
#56623=CARTESIAN_POINT('Ctrl Pts',(-2.9837790702192,-35.3274358680927,0.258580433779342));
#56624=CARTESIAN_POINT('Ctrl Pts',(-2.98474821549444,-35.3276103756947,
0.259842772924741));
#56625=CARTESIAN_POINT('Ctrl Pts',(-2.98571747633655,-35.3277286775049,
0.261093983900082));
#56626=CARTESIAN_POINT('Ctrl Pts',(0.0562124907764,-35.2853263177,-1.2047009047));
#56627=CARTESIAN_POINT('Ctrl Pts',(0.0549190904069,-35.3188634055,-1.16900714311));
#56628=CARTESIAN_POINT('Ctrl Pts',(0.0535306616313,-35.3596876325,-1.14016366385));
#56629=CARTESIAN_POINT('Ctrl Pts',(0.0521190751148,-35.4059409749,-1.1201647488));
#56630=CARTESIAN_POINT('Ctrl Pts',(0.0507668332647,-35.454920083,-1.11017926619));
#56631=CARTESIAN_POINT('Ctrl Pts',(0.0495419561802,-35.503899191,-1.11019486262));
#56632=CARTESIAN_POINT('Ctrl Pts',(-0.201788256316,-35.2863590312,-1.20002331734));
#56633=CARTESIAN_POINT('Ctrl Pts',(-0.20059637751,-35.3196953033,-1.1671828612));
#56634=CARTESIAN_POINT('Ctrl Pts',(-0.199891058502,-35.3593803738,-1.14082521527));
#56635=CARTESIAN_POINT('Ctrl Pts',(-0.199745892902,-35.4037391848,-1.12259845523));
#56636=CARTESIAN_POINT('Ctrl Pts',(-0.200177402058,-35.4504424505,-1.11345401234));
#56637=CARTESIAN_POINT('Ctrl Pts',(-0.201137869134,-35.4971457162,-1.11338731493));
#56638=CARTESIAN_POINT('Ctrl Pts',(-0.458005640948,-35.2884465433,-1.1743412925));
#56639=CARTESIAN_POINT('Ctrl Pts',(-0.45532002803,-35.3213377511,-1.14466296307));
#56640=CARTESIAN_POINT('Ctrl Pts',(-0.4535812271,-35.3596601469,-1.12100512273));
#56641=CARTESIAN_POINT('Ctrl Pts',(-0.452922785697,-35.4019345515,-1.1046878387));
#56642=CARTESIAN_POINT('Ctrl Pts',(-0.453380153067,-35.4461899162,-1.09646210546));
#56643=CARTESIAN_POINT('Ctrl Pts',(-0.454881185093,-35.4904452809,-1.09632868214));
#56644=CARTESIAN_POINT('Ctrl Pts',(-0.713379137931,-35.2906784141,-1.12765964252));
#56645=CARTESIAN_POINT('Ctrl Pts',(-0.709079348273,-35.3228447776,-1.10136638154));
#56646=CARTESIAN_POINT('Ctrl Pts',(-0.70594831441,-35.3595655977,-1.08053117586));
#56647=CARTESIAN_POINT('Ctrl Pts',(-0.704166625027,-35.3995661124,-1.06618227068));
#56648=CARTESIAN_POINT('Ctrl Pts',(-0.703813714965,-35.4412096849,-1.05889834036));
#56649=CARTESIAN_POINT('Ctrl Pts',(-0.70484928931,-35.4828532574,-1.05868437313));
#56650=CARTESIAN_POINT('Ctrl Pts',(-1.38784510535,-35.2993373321,-0.947254707752));
#56651=CARTESIAN_POINT('Ctrl Pts',(-1.38135732447,-35.3286900482,-0.929878628182));
#56652=CARTESIAN_POINT('Ctrl Pts',(-1.37657158883,-35.3605166385,-0.91635466331));
#56653=CARTESIAN_POINT('Ctrl Pts',(-1.37367161422,-35.3940608782,-0.907077564055));
#56654=CARTESIAN_POINT('Ctrl Pts',(-1.37274039474,-35.4284641756,-0.90225909603));
#56655=CARTESIAN_POINT('Ctrl Pts',(-1.37374872204,-35.4628674729,-0.901908813904));
#56656=CARTESIAN_POINT('Ctrl Pts',(-2.01355395003,-35.311130732,-0.626706350821));
#56657=CARTESIAN_POINT('Ctrl Pts',(-2.00730643429,-35.336016544,-0.616608977986));
#56658=CARTESIAN_POINT('Ctrl Pts',(-2.00258568894,-35.3621198501,-0.608811606003));
#56659=CARTESIAN_POINT('Ctrl Pts',(-1.9994933297,-35.389055262,-0.603446176196));
#56660=CARTESIAN_POINT('Ctrl Pts',(-1.99808657075,-35.4164068328,-0.600583823803));
#56661=CARTESIAN_POINT('Ctrl Pts',(-1.99837189146,-35.4437584036,-0.600230058024));
#56662=CARTESIAN_POINT('Ctrl Pts',(-2.37717939564,-35.3191393972,-0.374243399004));
#56663=CARTESIAN_POINT('Ctrl Pts',(-2.37186878863,-35.3409656481,-0.367119757236));
#56664=CARTESIAN_POINT('Ctrl Pts',(-2.36789713578,-35.363631483,-0.361625053168));
#56665=CARTESIAN_POINT('Ctrl Pts',(-2.36532978406,-35.3868707128,-0.35784451611));
#56666=CARTESIAN_POINT('Ctrl Pts',(-2.36419887789,-35.4103967036,-0.355823775657));
#56667=CARTESIAN_POINT('Ctrl Pts',(-2.36450092427,-35.4339226943,-0.355565614957));
#56668=CARTESIAN_POINT('Ctrl Pts',(-2.70262665161,-35.324607016,-0.0770523694869));
#56669=CARTESIAN_POINT('Ctrl Pts',(-2.69780857299,-35.3442953406,-0.0717175970589));
#56670=CARTESIAN_POINT('Ctrl Pts',(-2.69419322648,-35.3646024007,-0.067613422701));
#56671=CARTESIAN_POINT('Ctrl Pts',(-2.69182933906,-35.3853302459,-0.0647926244646));
#56672=CARTESIAN_POINT('Ctrl Pts',(-2.69074110489,-35.4062685003,-0.0632832758083));
#56673=CARTESIAN_POINT('Ctrl Pts',(-2.69092668038,-35.4272067546,-0.063087197317));
#56674=CARTESIAN_POINT('Ctrl Pts',(-2.98281092266,-35.3272070795,0.257308721393));
#56675=CARTESIAN_POINT('Ctrl Pts',(-2.97803806023,-35.345862351,0.261512145638));
#56676=CARTESIAN_POINT('Ctrl Pts',(-2.97443748635,-35.3650398039,0.264729168335));
#56677=CARTESIAN_POINT('Ctrl Pts',(-2.97205215937,-35.3845716938,0.266921957853));
#56678=CARTESIAN_POINT('Ctrl Pts',(-2.97090371967,-35.4042808219,0.268070620572));
#56679=CARTESIAN_POINT('Ctrl Pts',(-2.97099133978,-35.4239899499,0.268174257926));
#56680=CARTESIAN_POINT('',(-9.45935213686968E-8,-35.2855840760402,-1.203282378976));
#56681=CARTESIAN_POINT('Ctrl Pts',(-9.45935213686968E-8,-35.2855840760402,
-1.203282378976));
#56682=CARTESIAN_POINT('Ctrl Pts',(-0.246462141036511,-35.2867310709528,
-1.19529915853671));
#56683=CARTESIAN_POINT('Ctrl Pts',(-0.491376340832031,-35.2887499565309,
-1.16811525832979));
#56684=CARTESIAN_POINT('Ctrl Pts',(-0.735140444018721,-35.2909646174122,
-1.121794106446));
#56685=CARTESIAN_POINT('Ctrl Pts',(-1.3979442783783,-35.2995330331731,-0.942077192818583));
#56686=CARTESIAN_POINT('Ctrl Pts',(-2.01355281302879,-35.3111352611287,
-0.626704513172324));
#56687=CARTESIAN_POINT('Ctrl Pts',(-2.37717842914973,-35.3191433694965,
-0.37424210255291));
#56688=CARTESIAN_POINT('Ctrl Pts',(-2.702625774756,-35.3246105992,-0.0770513985971862));
#56689=CARTESIAN_POINT('Ctrl Pts',(-2.98281092224,-35.3272070795,0.257308721649));
#56690=CARTESIAN_POINT('Origin',(1.43496042263357E-12,-35.5025674380817,
-1.41067474285734));
#56691=CARTESIAN_POINT('Ctrl Pts',(-0.0562124907764,-35.2853263177,-1.2047009047));
#56692=CARTESIAN_POINT('Ctrl Pts',(-0.0549190904069,-35.3188634055,-1.16900714311));
#56693=CARTESIAN_POINT('Ctrl Pts',(-0.0535306616313,-35.3596876325,-1.14016366385));
#56694=CARTESIAN_POINT('Ctrl Pts',(-0.0521190751148,-35.4059409749,-1.1201647488));
#56695=CARTESIAN_POINT('Ctrl Pts',(-0.0507668332647,-35.454920083,-1.11017926619));
#56696=CARTESIAN_POINT('Ctrl Pts',(-0.0495419561802,-35.503899191,-1.11019486262));
#56697=CARTESIAN_POINT('Ctrl Pts',(0.201788256316,-35.2863590312,-1.20002331734));
#56698=CARTESIAN_POINT('Ctrl Pts',(0.20059637751,-35.3196953033,-1.1671828612));
#56699=CARTESIAN_POINT('Ctrl Pts',(0.199891058502,-35.3593803738,-1.14082521527));
#56700=CARTESIAN_POINT('Ctrl Pts',(0.199745892902,-35.4037391848,-1.12259845523));
#56701=CARTESIAN_POINT('Ctrl Pts',(0.200177402058,-35.4504424505,-1.11345401234));
#56702=CARTESIAN_POINT('Ctrl Pts',(0.201137869134,-35.4971457162,-1.11338731493));
#56703=CARTESIAN_POINT('Ctrl Pts',(0.458005640948,-35.2884465433,-1.1743412925));
#56704=CARTESIAN_POINT('Ctrl Pts',(0.45532002803,-35.3213377511,-1.14466296307));
#56705=CARTESIAN_POINT('Ctrl Pts',(0.4535812271,-35.3596601469,-1.12100512273));
#56706=CARTESIAN_POINT('Ctrl Pts',(0.452922785697,-35.4019345515,-1.1046878387));
#56707=CARTESIAN_POINT('Ctrl Pts',(0.453380153067,-35.4461899162,-1.09646210546));
#56708=CARTESIAN_POINT('Ctrl Pts',(0.454881185093,-35.4904452809,-1.09632868214));
#56709=CARTESIAN_POINT('Ctrl Pts',(0.713379137931,-35.2906784141,-1.12765964252));
#56710=CARTESIAN_POINT('Ctrl Pts',(0.709079348273,-35.3228447776,-1.10136638154));
#56711=CARTESIAN_POINT('Ctrl Pts',(0.70594831441,-35.3595655977,-1.08053117586));
#56712=CARTESIAN_POINT('Ctrl Pts',(0.704166625027,-35.3995661124,-1.06618227068));
#56713=CARTESIAN_POINT('Ctrl Pts',(0.703813714965,-35.4412096849,-1.05889834036));
#56714=CARTESIAN_POINT('Ctrl Pts',(0.70484928931,-35.4828532574,-1.05868437313));
#56715=CARTESIAN_POINT('Ctrl Pts',(1.38784510535,-35.2993373321,-0.947254707752));
#56716=CARTESIAN_POINT('Ctrl Pts',(1.38135732447,-35.3286900482,-0.929878628182));
#56717=CARTESIAN_POINT('Ctrl Pts',(1.37657158883,-35.3605166385,-0.91635466331));
#56718=CARTESIAN_POINT('Ctrl Pts',(1.37367161422,-35.3940608782,-0.907077564055));
#56719=CARTESIAN_POINT('Ctrl Pts',(1.37274039474,-35.4284641756,-0.90225909603));
#56720=CARTESIAN_POINT('Ctrl Pts',(1.37374872204,-35.4628674729,-0.901908813904));
#56721=CARTESIAN_POINT('Ctrl Pts',(2.01355395003,-35.311130732,-0.626706350821));
#56722=CARTESIAN_POINT('Ctrl Pts',(2.00730643429,-35.336016544,-0.616608977986));
#56723=CARTESIAN_POINT('Ctrl Pts',(2.00258568894,-35.3621198501,-0.608811606003));
#56724=CARTESIAN_POINT('Ctrl Pts',(1.9994933297,-35.389055262,-0.603446176196));
#56725=CARTESIAN_POINT('Ctrl Pts',(1.99808657075,-35.4164068328,-0.600583823803));
#56726=CARTESIAN_POINT('Ctrl Pts',(1.99837189146,-35.4437584036,-0.600230058024));
#56727=CARTESIAN_POINT('Ctrl Pts',(2.37717939564,-35.3191393972,-0.374243399004));
#56728=CARTESIAN_POINT('Ctrl Pts',(2.37186878863,-35.3409656481,-0.367119757236));
#56729=CARTESIAN_POINT('Ctrl Pts',(2.36789713578,-35.363631483,-0.361625053168));
#56730=CARTESIAN_POINT('Ctrl Pts',(2.36532978406,-35.3868707128,-0.35784451611));
#56731=CARTESIAN_POINT('Ctrl Pts',(2.36419887789,-35.4103967036,-0.355823775657));
#56732=CARTESIAN_POINT('Ctrl Pts',(2.36450092427,-35.4339226943,-0.355565614957));
#56733=CARTESIAN_POINT('Ctrl Pts',(2.70262665161,-35.324607016,-0.0770523694869));
#56734=CARTESIAN_POINT('Ctrl Pts',(2.69780857299,-35.3442953406,-0.0717175970589));
#56735=CARTESIAN_POINT('Ctrl Pts',(2.69419322648,-35.3646024007,-0.067613422701));
#56736=CARTESIAN_POINT('Ctrl Pts',(2.69182933906,-35.3853302459,-0.0647926244646));
#56737=CARTESIAN_POINT('Ctrl Pts',(2.69074110489,-35.4062685003,-0.0632832758083));
#56738=CARTESIAN_POINT('Ctrl Pts',(2.69092668038,-35.4272067546,-0.063087197317));
#56739=CARTESIAN_POINT('Ctrl Pts',(2.98281092266,-35.3272070795,0.257308721393));
#56740=CARTESIAN_POINT('Ctrl Pts',(2.97803806023,-35.345862351,0.261512145638));
#56741=CARTESIAN_POINT('Ctrl Pts',(2.97443748635,-35.3650398039,0.264729168335));
#56742=CARTESIAN_POINT('Ctrl Pts',(2.97205215937,-35.3845716938,0.266921957853));
#56743=CARTESIAN_POINT('Ctrl Pts',(2.97090371967,-35.4042808219,0.268070620572));
#56744=CARTESIAN_POINT('Ctrl Pts',(2.97099133978,-35.4239899499,0.268174257926));
#56745=CARTESIAN_POINT('',(2.98281092138865,-35.3272070856442,0.257308723513503));
#56746=CARTESIAN_POINT('Origin',(3.20008730232451,-35.423990048778,0.074485335177551));
#56747=CARTESIAN_POINT('Ctrl Pts',(-9.45222527193312E-8,-35.285576877971,
-1.20327550011348));
#56748=CARTESIAN_POINT('Ctrl Pts',(0.0614972181873807,-35.2858729988589,
-1.20127673805126));
#56749=CARTESIAN_POINT('Ctrl Pts',(0.12475096035803,-35.2862554013519,-1.19776918615153));
#56750=CARTESIAN_POINT('Ctrl Pts',(0.189714992976335,-35.286710572023,-1.19250029860945));
#56751=CARTESIAN_POINT('Ctrl Pts',(0.253080303565567,-35.2871545412439,
-1.18736107491739));
#56752=CARTESIAN_POINT('Ctrl Pts',(0.318073164574926,-35.2876676839599,
-1.18054592797751));
#56753=CARTESIAN_POINT('Ctrl Pts',(0.384603016748727,-35.2882448843954,
-1.17181797651484));
#56754=CARTESIAN_POINT('Ctrl Pts',(0.453001767346575,-35.2888382990407,
-1.16284484707266));
#56755=CARTESIAN_POINT('Ctrl Pts',(0.523025330275769,-35.2894995032065,
-1.15184974180236));
#56756=CARTESIAN_POINT('Ctrl Pts',(0.59451821079149,-35.2902309277385,-1.13857562603336));
#56757=CARTESIAN_POINT('Ctrl Pts',(0.651801537075522,-35.290816978123,-1.12793980468663));
#56758=CARTESIAN_POINT('Ctrl Pts',(0.710026730424283,-35.2914483971486,
-1.11584085180069));
#56759=CARTESIAN_POINT('Ctrl Pts',(0.769089812910904,-35.2921284387114,
-1.10214793193385));
#56760=CARTESIAN_POINT('Ctrl Pts',(0.859844617649464,-35.2931733729857,
-1.08110774546716));
#56761=CARTESIAN_POINT('Ctrl Pts',(0.952636103171223,-35.2943240410569,
-1.05629997486956));
#56762=CARTESIAN_POINT('Ctrl Pts',(1.04705097486316,-35.2955911403668,-1.02723022917726));
#56763=CARTESIAN_POINT('Ctrl Pts',(1.09723468979318,-35.2962646333179,-1.01177897870402));
#56764=CARTESIAN_POINT('Ctrl Pts',(1.14787610914596,-35.2969706853886,-0.995123811975983));
#56765=CARTESIAN_POINT('Ctrl Pts',(1.19891695691765,-35.2977048215787,-0.977191637208916));
#56766=CARTESIAN_POINT('Ctrl Pts',(1.20129469642974,-35.2977390213364,-0.976356266278715));
#56767=CARTESIAN_POINT('Ctrl Pts',(1.20367328632146,-35.2977732882489,-0.975518124932157));
#56768=CARTESIAN_POINT('Ctrl Pts',(1.20605272170261,-35.2978076216918,-0.974677205666163));
#56769=CARTESIAN_POINT('Ctrl Pts',(1.27725989092447,-35.2988350869861,-0.949511789975523));
#56770=CARTESIAN_POINT('Ctrl Pts',(1.34922652726592,-35.2999228250693,-0.921858000564636));
#56771=CARTESIAN_POINT('Ctrl Pts',(1.42174183512206,-35.3010717162344,-0.891524167229231));
#56772=CARTESIAN_POINT('Ctrl Pts',(1.4592110629062,-35.3016653573019,-0.875850437855217));
#56773=CARTESIAN_POINT('Ctrl Pts',(1.49682629106069,-35.3022752902411,-0.859461217061494));
#56774=CARTESIAN_POINT('Ctrl Pts',(1.53455512107422,-35.3029014543288,-0.842330615007104));
#56775=CARTESIAN_POINT('Ctrl Pts',(1.55341953608098,-35.3032145363727,-0.833765313979908));
#56776=CARTESIAN_POINT('Ctrl Pts',(1.57231234894133,-35.3035316723579,-0.825014661717318));
#56777=CARTESIAN_POINT('Ctrl Pts',(1.59122924975292,-35.3038528498659,-0.816075491944981));
#56778=CARTESIAN_POINT('Ctrl Pts',(1.60068770015871,-35.3040134386198,-0.811605907058813));
#56779=CARTESIAN_POINT('Ctrl Pts',(1.61015217242701,-35.3041750376006,-0.807089192543942));
#56780=CARTESIAN_POINT('Ctrl Pts',(1.61962211971477,-35.304337644519,-0.802524954373084));
#56781=CARTESIAN_POINT('Ctrl Pts',(1.62435709335865,-35.3044189479782,-0.800242835287656));
#56782=CARTESIAN_POINT('Ctrl Pts',(1.62909343574822,-35.3045005034126,-0.797948835272099));
#56783=CARTESIAN_POINT('Ctrl Pts',(1.63383107763051,-35.3045823105274,-0.795642905349689));
#56784=CARTESIAN_POINT('Ctrl Pts',(1.63619989857166,-35.3046232140848,-0.794489940388483));
#56785=CARTESIAN_POINT('Ctrl Pts',(1.63856904438543,-35.3046641805619,-0.793333992949638));
#56786=CARTESIAN_POINT('Ctrl Pts',(1.64093850635605,-35.3047052099212,-0.792175056930587));
#56787=CARTESIAN_POINT('Ctrl Pts',(1.64330796832666,-35.3047462392806,-0.791016120911536));
#56788=CARTESIAN_POINT('Ctrl Pts',(1.6443966453675,-35.3047650866673,-0.79048386835501));
#56789=CARTESIAN_POINT('Ctrl Pts',(1.6480476607185,-35.3048292587342,-0.788688863658591));
#56790=CARTESIAN_POINT('Ctrl Pts',(1.70123429550726,-35.3057640935558,-0.762539902327496));
#56791=CARTESIAN_POINT('Ctrl Pts',(1.75111821236543,-35.3066639064797,-0.736590388689801));
#56792=CARTESIAN_POINT('Ctrl Pts',(1.79782737592309,-35.3075185789543,-0.711197975455024));
#56793=CARTESIAN_POINT('Ctrl Pts',(1.84589424537922,-35.3083980943884,-0.685067475159823));
#56794=CARTESIAN_POINT('Ctrl Pts',(1.89059973686305,-35.3092298180379,-0.659526935062845));
#56795=CARTESIAN_POINT('Ctrl Pts',(1.93209089082562,-35.3100071852016,-0.634911745427993));
#56796=CARTESIAN_POINT('Ctrl Pts',(1.97408375056434,-35.3107939521907,-0.609998912039198));
#56797=CARTESIAN_POINT('Ctrl Pts',(2.0127846495597,-35.3115250983264,-0.586033789444093));
#56798=CARTESIAN_POINT('Ctrl Pts',(2.04834444134429,-35.3121977596016,-0.563310572130525));
#56799=CARTESIAN_POINT('Ctrl Pts',(2.0843157894759,-35.3128782060185,-0.54032436440446));
#56800=CARTESIAN_POINT('Ctrl Pts',(2.11707341328875,-35.3134988804558,-0.518608822018224));
#56801=CARTESIAN_POINT('Ctrl Pts',(2.14676353560029,-35.3140598031597,-0.498416392096874));
#56802=CARTESIAN_POINT('Ctrl Pts',(2.1543486405602,-35.3142031052836,-0.49325771680608));
#56803=CARTESIAN_POINT('Ctrl Pts',(2.16173346496828,-35.3143425193064,-0.488198196245356));
#56804=CARTESIAN_POINT('Ctrl Pts',(2.16892028603487,-35.3144780671423,-0.483241521533293));
#56805=CARTESIAN_POINT('Ctrl Pts',(2.19778835526041,-35.315022536564,-0.463331518572251));
#56806=CARTESIAN_POINT('Ctrl Pts',(2.22346417948716,-35.315504554706,-0.445084466403678));
#56807=CARTESIAN_POINT('Ctrl Pts',(2.24608377138598,-35.3159269723923,-0.428705133107888));
#56808=CARTESIAN_POINT('Ctrl Pts',(2.26830884505752,-35.3163420225063,-0.412611478950989));
#56809=CARTESIAN_POINT('Ctrl Pts',(2.28758359799759,-35.3166995980441,-0.398320624291156));
#56810=CARTESIAN_POINT('Ctrl Pts',(2.30401276785091,-35.3170028614933,-0.385979989195755));
#56811=CARTESIAN_POINT('Ctrl Pts',(2.32087939004264,-35.317314199806,-0.373310765393305));
#56812=CARTESIAN_POINT('Ctrl Pts',(2.33474734337766,-35.3175683488764,-0.362696973253167));
#56813=CARTESIAN_POINT('Ctrl Pts',(2.34570019490273,-35.3177683471626,-0.354249400480844));
#56814=CARTESIAN_POINT('Ctrl Pts',(2.35117662066526,-35.3178683463057,-0.350025614094683));
#56815=CARTESIAN_POINT('Ctrl Pts',(2.35592376016089,-35.3179547964115,-0.346342639570059));
#56816=CARTESIAN_POINT('Ctrl Pts',(2.3599489400905,-35.3180279872108,-0.34320990432561));
#56817=CARTESIAN_POINT('Ctrl Pts',(2.3619615300553,-35.3180645826105,-0.341643536703386));
#56818=CARTESIAN_POINT('Ctrl Pts',(2.36379359571024,-35.3180978620434,-0.340214684300089));
#56819=CARTESIAN_POINT('Ctrl Pts',(2.36544584989918,-35.318127854485,-0.338924255123493));
#56820=CARTESIAN_POINT('Ctrl Pts',(2.36638037096635,-35.3181448183206,-0.338194383618681));
#56821=CARTESIAN_POINT('Ctrl Pts',(2.3672573665503,-35.3181607305319,-0.337508791467333));
#56822=CARTESIAN_POINT('Ctrl Pts',(2.36807694618827,-35.3181755956209,-0.336867617636297));
#56823=CARTESIAN_POINT('Ctrl Pts',(2.36866408946375,-35.3181862449057,-0.336408283502235));
#56824=CARTESIAN_POINT('Ctrl Pts',(2.36922497418766,-35.3181964149313,-0.335969231388025));
#56825=CARTESIAN_POINT('Ctrl Pts',(2.36974609787095,-35.3182058617932,-0.335561112266989));
#56826=CARTESIAN_POINT('Ctrl Pts',(2.36978365244749,-35.3182065425777,-0.335531701320494));
#56827=CARTESIAN_POINT('Ctrl Pts',(2.36982098686393,-35.3182072193589,-0.335502461737859));
#56828=CARTESIAN_POINT('Ctrl Pts',(2.36985809230613,-35.3182078919776,-0.335473400459684));
#56829=CARTESIAN_POINT('Ctrl Pts',(2.3701780251888,-35.3182136914725,-0.335222826475173));
#56830=CARTESIAN_POINT('Ctrl Pts',(2.37049274317138,-35.318219406958,-0.334977240828002));
#56831=CARTESIAN_POINT('Ctrl Pts',(2.37249838105661,-35.3182557329203,-0.333403765987897));
#56832=CARTESIAN_POINT('Ctrl Pts',(2.436709599302,-35.3194187216703,-0.283028403064282));
#56833=CARTESIAN_POINT('Ctrl Pts',(2.49734850532433,-35.3204801616452,-0.232367280315841));
#56834=CARTESIAN_POINT('Ctrl Pts',(2.55458115188229,-35.3214330129731,-0.181871002070266));
#56835=CARTESIAN_POINT('Ctrl Pts',(2.61305107463453,-35.3224064633879,-0.130283076893613));
#56836=CARTESIAN_POINT('Ctrl Pts',(2.66796645352324,-35.3232666833824,-0.0788672652294133));
#56837=CARTESIAN_POINT('Ctrl Pts',(2.71953139329132,-35.3240162990872,-0.0280559043515061));
#56838=CARTESIAN_POINT('Ctrl Pts',(2.77276235772848,-35.3247901343153,0.0243971336246918));
#56839=CARTESIAN_POINT('Ctrl Pts',(2.82242345816926,-35.3254462594998,0.0762059115642822));
#56840=CARTESIAN_POINT('Ctrl Pts',(2.86875884666911,-35.3259962351236,0.12694712440495));
#56841=CARTESIAN_POINT('Ctrl Pts',(2.90926007567917,-35.3264769624771,0.171299433688266));
#56842=CARTESIAN_POINT('Ctrl Pts',(2.94722090693888,-35.326876810181,0.214836970860647));
#56843=CARTESIAN_POINT('Ctrl Pts',(2.9828109225733,-35.3272070796485,0.257308721368552));
#56844=CARTESIAN_POINT('Ctrl Pts',(2.98281092022,-35.3272070934,0.257308726577));
#56845=CARTESIAN_POINT('Ctrl Pts',(2.97803806995,-35.345862362,0.261512162033));
#56846=CARTESIAN_POINT('Ctrl Pts',(2.97443750788,-35.3650398118,0.264729196731));
#56847=CARTESIAN_POINT('Ctrl Pts',(2.97205219293,-35.3845716985,0.266921998871));
#56848=CARTESIAN_POINT('Ctrl Pts',(2.97090376513,-35.4042808232,0.268070674403));
#56849=CARTESIAN_POINT('Ctrl Pts',(2.97099139651,-35.4239899479,0.268174325124));
#56850=CARTESIAN_POINT('Ctrl Pts',(2.98353703291,-35.3273786743,0.258262507142));
#56851=CARTESIAN_POINT('Ctrl Pts',(2.97889447281,-35.3460005999,0.262582653758));
#56852=CARTESIAN_POINT('Ctrl Pts',(2.97542363609,-35.3651416718,0.26592442057));
#56853=CARTESIAN_POINT('Ctrl Pts',(2.97316614056,-35.3846350952,0.268249073819));
#56854=CARTESIAN_POINT('Ctrl Pts',(2.97214238275,-35.4043047141,0.26953560217));
#56855=CARTESIAN_POINT('Ctrl Pts',(2.97235045678,-35.4239743331,0.269781826657));
#56856=CARTESIAN_POINT('Ctrl Pts',(2.98426364409,-35.3275231471,0.259211611404));
#56857=CARTESIAN_POINT('Ctrl Pts',(2.97975071316,-35.3461112518,0.263650265626));
#56858=CARTESIAN_POINT('Ctrl Pts',(2.97640915872,-35.3652155879,0.267118330752));
#56859=CARTESIAN_POINT('Ctrl Pts',(2.97427928943,-35.3846702746,0.269576156755));
#56860=CARTESIAN_POINT('Ctrl Pts',(2.97338027656,-35.4043001557,0.271001608633));
#56861=CARTESIAN_POINT('Ctrl Pts',(2.97370914102,-35.4239300369,0.271391235523));
#56862=CARTESIAN_POINT('Ctrl Pts',(2.98499053061,-35.3276399509,0.260155575417));
#56863=CARTESIAN_POINT('Ctrl Pts',(2.98060644818,-35.3461937726,0.264714470388));
#56864=CARTESIAN_POINT('Ctrl Pts',(2.97739362648,-35.3652610343,0.268310331454));
#56865=CARTESIAN_POINT('Ctrl Pts',(2.97539109347,-35.3846767315,0.270902576923));
#56866=CARTESIAN_POINT('Ctrl Pts',(2.9746168118,-35.404266665,0.272467944099));
#56867=CARTESIAN_POINT('Ctrl Pts',(2.97506673688,-35.4238565985,0.27300171487));
#56868=CARTESIAN_POINT('Ctrl Pts',(2.98571747678,-35.3277286766,0.26109398396));
#56869=CARTESIAN_POINT('Ctrl Pts',(2.98146135285,-35.3462477712,0.26577478149));
#56870=CARTESIAN_POINT('Ctrl Pts',(2.97837661705,-35.3652776408,0.269499861748));
#56871=CARTESIAN_POINT('Ctrl Pts',(2.97650103844,-35.384654117,0.272227696729));
#56872=CARTESIAN_POINT('Ctrl Pts',(2.97585139066,-35.4042039153,0.273933891593));
#56873=CARTESIAN_POINT('Ctrl Pts',(2.97642257226,-35.4237537135,0.274612461819));
#56874=CARTESIAN_POINT('',(2.98571747516532,-35.3277286769942,0.261093984855667));
#56875=CARTESIAN_POINT('Origin',(3.20593733485692,-35.4237538137774,0.0814200066647186));
#56876=CARTESIAN_POINT('Ctrl Pts',(2.98281092022,-35.3272070934,0.257308726577));
#56877=CARTESIAN_POINT('Ctrl Pts',(2.9837790702192,-35.3274358680927,0.258580433779342));
#56878=CARTESIAN_POINT('Ctrl Pts',(2.98474821549444,-35.3276103756947,0.259842772924741));
#56879=CARTESIAN_POINT('Ctrl Pts',(2.98571747633655,-35.3277286775049,0.261093983900082));
#56880=CARTESIAN_POINT('Ctrl Pts',(2.98571747284,-35.3277286717,0.261093980788));
#56881=CARTESIAN_POINT('Ctrl Pts',(2.981461349,-35.3462477664,0.265774778659));
#56882=CARTESIAN_POINT('Ctrl Pts',(2.97837661309,-35.3652776361,0.269499859243));
#56883=CARTESIAN_POINT('Ctrl Pts',(2.97650103488,-35.3846541126,0.272227694446));
#56884=CARTESIAN_POINT('Ctrl Pts',(2.97585138777,-35.4042039111,0.273933889101));
#56885=CARTESIAN_POINT('Ctrl Pts',(2.9764225699,-35.4237537096,0.274612459172));
#56886=CARTESIAN_POINT('Ctrl Pts',(2.99904170374,-35.3293548375,0.278294108299));
#56887=CARTESIAN_POINT('Ctrl Pts',(2.99483616983,-35.347248816,0.282402750811));
#56888=CARTESIAN_POINT('Ctrl Pts',(2.99178501636,-35.3655962934,0.285705549944));
#56889=CARTESIAN_POINT('Ctrl Pts',(2.98992270743,-35.3842510435,0.288169202034));
#56890=CARTESIAN_POINT('Ctrl Pts',(2.98926461676,-35.4030594457,0.289773532404));
#56891=CARTESIAN_POINT('Ctrl Pts',(2.98980629628,-35.4218678479,0.290512461752));
#56892=CARTESIAN_POINT('Ctrl Pts',(3.01081156168,-35.3311436809,0.296626108381));
#56893=CARTESIAN_POINT('Ctrl Pts',(3.00676278967,-35.3483431627,0.300206793547));
#56894=CARTESIAN_POINT('Ctrl Pts',(3.00382878865,-35.3659388616,0.303127857359));
#56895=CARTESIAN_POINT('Ctrl Pts',(3.00203974789,-35.3838026166,0.305362985112));
#56896=CARTESIAN_POINT('Ctrl Pts',(3.00140909733,-35.4018004061,0.306895543103));
#56897=CARTESIAN_POINT('Ctrl Pts',(3.00193290967,-35.4197981956,0.307719289765));
#56898=CARTESIAN_POINT('Ctrl Pts',(3.0211060441,-35.3328533463,0.316096062934));
#56899=CARTESIAN_POINT('Ctrl Pts',(3.01723125611,-35.3493133446,0.319149425303));
#56900=CARTESIAN_POINT('Ctrl Pts',(3.01441086074,-35.3661160441,0.321674359752));
#56901=CARTESIAN_POINT('Ctrl Pts',(3.01267195982,-35.3831506732,0.32365017578));
#56902=CARTESIAN_POINT('Ctrl Pts',(3.01202647228,-35.4003009737,0.325063889693));
#56903=CARTESIAN_POINT('Ctrl Pts',(3.01247041893,-35.4174512741,0.325909903855));
#56904=CARTESIAN_POINT('Ctrl Pts',(3.03608811322,-35.3362145716,0.351770920136));
#56905=CARTESIAN_POINT('Ctrl Pts',(3.03261306094,-35.3513090757,0.353941667697));
#56906=CARTESIAN_POINT('Ctrl Pts',(3.03006547046,-35.366660463,0.355785992804));
#56907=CARTESIAN_POINT('Ctrl Pts',(3.02846382328,-35.3821846623,0.357292574606));
#56908=CARTESIAN_POINT('Ctrl Pts',(3.02781696962,-35.3977954963,0.3584530028));
#56909=CARTESIAN_POINT('Ctrl Pts',(3.02812402787,-35.4134063304,0.35926266557));
#56910=CARTESIAN_POINT('Ctrl Pts',(3.04544130267,-35.3402488915,0.389133416749));
#56911=CARTESIAN_POINT('Ctrl Pts',(3.04250648845,-35.3538042987,0.390631987385));
#56912=CARTESIAN_POINT('Ctrl Pts',(3.040339577,-35.3675437775,0.391955910767));
#56913=CARTESIAN_POINT('Ctrl Pts',(3.03895408512,-35.3814072732,0.393098415575));
#56914=CARTESIAN_POINT('Ctrl Pts',(3.03835622743,-35.3953326096,0.394054612964));
#56915=CARTESIAN_POINT('Ctrl Pts',(3.03854461847,-35.4092579459,0.394821151154));
#56916=CARTESIAN_POINT('Ctrl Pts',(3.04837800292,-35.3421028535,0.405371326337));
#56917=CARTESIAN_POINT('Ctrl Pts',(3.04569735965,-35.354968334,0.406623296912));
#56918=CARTESIAN_POINT('Ctrl Pts',(3.04371425581,-35.367989887,0.407755259395));
#56919=CARTESIAN_POINT('Ctrl Pts',(3.04243717253,-35.3811153925,0.408763338852));
#56920=CARTESIAN_POINT('Ctrl Pts',(3.0418710033,-35.3942935555,0.40964296396));
#56921=CARTESIAN_POINT('Ctrl Pts',(3.0420174994,-35.4074717185,0.410390857869));
#56922=CARTESIAN_POINT('Ctrl Pts',(3.0502457294,-35.3440064303,0.421621283978));
#56923=CARTESIAN_POINT('Ctrl Pts',(3.04782750294,-35.3561342576,0.422702630881));
#56924=CARTESIAN_POINT('Ctrl Pts',(3.04603083038,-35.3683919899,0.423709393311));
#56925=CARTESIAN_POINT('Ctrl Pts',(3.04486559316,-35.3807375362,0.424637122745));
#56926=CARTESIAN_POINT('Ctrl Pts',(3.04433601307,-35.3931265369,0.425482937737));
#56927=CARTESIAN_POINT('Ctrl Pts',(3.04444019246,-35.4055155376,0.426244325555));
#56928=CARTESIAN_POINT('Ctrl Pts',(3.05109044578,-35.345853084,0.437996449073));
#56929=CARTESIAN_POINT('Ctrl Pts',(3.04891974336,-35.357242792,0.438899021788));
#56930=CARTESIAN_POINT('Ctrl Pts',(3.0473005821,-35.368740838,0.439760925705));
#56931=CARTESIAN_POINT('Ctrl Pts',(3.04623976029,-35.380311563,0.440579334845));
#56932=CARTESIAN_POINT('Ctrl Pts',(3.04574060956,-35.391918628,0.441351678913));
#56933=CARTESIAN_POINT('Ctrl Pts',(3.04580293259,-35.4035256929,0.442075691324));
#56934=CARTESIAN_POINT('',(3.05109044990354,-35.3458530848239,0.437996448765818));
#56935=CARTESIAN_POINT('Origin',(3.34464449040265,-35.4035194920317,0.416364015877388));
#56936=CARTESIAN_POINT('Ctrl Pts',(2.9857174744567,-35.3277286766852,0.261093985433823));
#56937=CARTESIAN_POINT('Ctrl Pts',(2.99164509856773,-35.3284521172012,0.268745900785589));
#56938=CARTESIAN_POINT('Ctrl Pts',(2.99729005843478,-35.3292209076218,0.276777206877757));
#56939=CARTESIAN_POINT('Ctrl Pts',(3.00261892051309,-35.3300138265231,0.285196864882465));
#56940=CARTESIAN_POINT('Ctrl Pts',(3.00830106634229,-35.3308593130007,0.294174714920944));
#56941=CARTESIAN_POINT('Ctrl Pts',(3.01362328701173,-35.3317331213617,0.303594619723798));
#56942=CARTESIAN_POINT('Ctrl Pts',(3.01851367686819,-35.3326519248837,0.313432781673084));
#56943=CARTESIAN_POINT('Ctrl Pts',(3.02375368720857,-35.3336364148931,0.323974286922699));
#56944=CARTESIAN_POINT('Ctrl Pts',(3.02849607780734,-35.3346755074925,0.334996514888742));
#56945=CARTESIAN_POINT('Ctrl Pts',(3.03263528909564,-35.3358079210548,0.346423067558966));
#56946=CARTESIAN_POINT('Ctrl Pts',(3.03394300126408,-35.3361656875209,0.350033089113673));
#56947=CARTESIAN_POINT('Ctrl Pts',(3.03519051631512,-35.3365326913694,0.353683104974461));
#56948=CARTESIAN_POINT('Ctrl Pts',(3.0363747716968,-35.3369095627627,0.357369717393274));
#56949=CARTESIAN_POINT('Ctrl Pts',(3.03988840496031,-35.3380277234941,0.368307733149693));
#56950=CARTESIAN_POINT('Ctrl Pts',(3.04284311652455,-35.3392359571205,0.379569460963959));
#56951=CARTESIAN_POINT('Ctrl Pts',(3.04517508581328,-35.3405165043927,0.391069582657007));
#56952=CARTESIAN_POINT('Ctrl Pts',(3.04698057772651,-35.3415079487294,0.399973377753454));
#56953=CARTESIAN_POINT('Ctrl Pts',(3.04841326094402,-35.3425418417111,0.409017474653859));
#56954=CARTESIAN_POINT('Ctrl Pts',(3.04945570098349,-35.3435920710794,0.418177350402306));
#56955=CARTESIAN_POINT('Ctrl Pts',(3.05020053253474,-35.344342468167,0.424722153177225));
#56956=CARTESIAN_POINT('Ctrl Pts',(3.05074635985724,-35.3451008715098,0.43132620995016));
#56957=CARTESIAN_POINT('Ctrl Pts',(3.05109044577719,-35.3458530840132,0.437996449070046));
#56958=CARTESIAN_POINT('Ctrl Pts',(3.05109049587,-35.3458529008,0.437996404741));
#56959=CARTESIAN_POINT('Ctrl Pts',(3.04891977816,-35.3572426278,0.438898953129));
#56960=CARTESIAN_POINT('Ctrl Pts',(3.04730060509,-35.3687406938,0.439760831884));
#56961=CARTESIAN_POINT('Ctrl Pts',(3.04623977506,-35.3803114393,0.440579215085));
#56962=CARTESIAN_POINT('Ctrl Pts',(3.04574061974,-35.3919185251,0.441351532501));
#56963=CARTESIAN_POINT('Ctrl Pts',(3.04580294181,-35.4035256109,0.442075517619));
#56964=CARTESIAN_POINT('Ctrl Pts',(3.05133592857,-35.3454968218,0.440376332259));
#56965=CARTESIAN_POINT('Ctrl Pts',(3.049131145,-35.3569269779,0.441037311376));
#56966=CARTESIAN_POINT('Ctrl Pts',(3.04748040649,-35.368466371,0.44165738234));
#56967=CARTESIAN_POINT('Ctrl Pts',(3.04639064899,-35.3800790478,0.442234462677));
#56968=CARTESIAN_POINT('Ctrl Pts',(3.04586531061,-35.3917283673,0.442766727044));
#56969=CARTESIAN_POINT('Ctrl Pts',(3.04590426722,-35.4033776868,0.443252644519));
#56970=CARTESIAN_POINT('Ctrl Pts',(3.05157202469,-35.345201709,0.44278366337));
#56971=CARTESIAN_POINT('Ctrl Pts',(3.04933300313,-35.3566718646,0.443200875235));
#56972=CARTESIAN_POINT('Ctrl Pts',(3.04765109714,-35.3682522692,0.443576907233));
#56973=CARTESIAN_POINT('Ctrl Pts',(3.04653338889,-35.3799066391,0.443910429375));
#56974=CARTESIAN_POINT('Ctrl Pts',(3.04598342453,-35.3915979921,0.44420038209));
#56975=CARTESIAN_POINT('Ctrl Pts',(3.0460011471,-35.4032893451,0.444445979659));
#56976=CARTESIAN_POINT('Ctrl Pts',(3.05179796269,-35.3449700438,0.445216729023));
#56977=CARTESIAN_POINT('Ctrl Pts',(3.04952458771,-35.3564797113,0.445388154931));
#56978=CARTESIAN_POINT('Ctrl Pts',(3.04781198307,-35.3681007576,0.445518095267));
#56979=CARTESIAN_POINT('Ctrl Pts',(3.04666739039,-35.3797965316,0.445605990135));
#56980=CARTESIAN_POINT('Ctrl Pts',(3.04609446477,-35.3915296692,0.44565156091));
#56981=CARTESIAN_POINT('Ctrl Pts',(3.04609320711,-35.4032628068,0.445654782512));
#56982=CARTESIAN_POINT('Ctrl Pts',(3.05201291474,-35.344804036,0.447673318567));
#56983=CARTESIAN_POINT('Ctrl Pts',(3.04970513582,-35.3563526648,0.447597170527));
#56984=CARTESIAN_POINT('Ctrl Pts',(3.04796238182,-35.3680139256,0.447479196662));
#56985=CARTESIAN_POINT('Ctrl Pts',(3.04679206061,-35.3797507581,0.447319633895));
#56986=CARTESIAN_POINT('Ctrl Pts',(3.04619793931,-35.3915253768,0.447118989828));
#56987=CARTESIAN_POINT('Ctrl Pts',(3.04618007217,-35.4032999955,0.446878030094));
#56988=CARTESIAN_POINT('Ctrl Pts',(3.05221609529,-35.3447053607,0.45015055449));
#56989=CARTESIAN_POINT('Ctrl Pts',(3.04987393679,-35.3562923356,0.449825338819));
#56990=CARTESIAN_POINT('Ctrl Pts',(3.04810166196,-35.3679933207,0.449457922766));
#56991=CARTESIAN_POINT('Ctrl Pts',(3.04690685539,-35.3797708063,0.449049358968));
#56992=CARTESIAN_POINT('Ctrl Pts',(3.04629339744,-35.3915865426,0.448600974315));
#56993=CARTESIAN_POINT('Ctrl Pts',(3.0462613893,-35.403402279,0.448114344323));
#56994=CARTESIAN_POINT('',(3.05221609413,-35.3447053607,0.450150554363));
#56995=CARTESIAN_POINT('Origin',(3.34555850698237,-35.4033872461924,0.428430037062882));
#56996=CARTESIAN_POINT('Origin',(3.03578495082005,-35.4311381890655,0.45269626373329));
#56997=CARTESIAN_POINT('Ctrl Pts',(3.05220443551777,-35.344591778873,0.449686712477512));
#56998=CARTESIAN_POINT('Ctrl Pts',(3.0498551255609,-35.3561950376791,0.449361491242345));
#56999=CARTESIAN_POINT('Ctrl Pts',(3.04807734683564,-35.3679128088571,0.448993942438477));
#57000=CARTESIAN_POINT('Ctrl Pts',(3.04687872963453,-35.3797074189195,0.448585121824359));
#57001=CARTESIAN_POINT('Ctrl Pts',(3.04626317818814,-35.3915404490275,0.448136361067163));
#57002=CARTESIAN_POINT('Ctrl Pts',(3.04623079520836,-35.4033734790351,0.447649241926326));
#57003=CARTESIAN_POINT('Ctrl Pts',(3.08188814853274,-35.3301154645781,0.811301434518424));
#57004=CARTESIAN_POINT('Ctrl Pts',(3.07719180838287,-35.3473672155455,0.810925370095392));
#57005=CARTESIAN_POINT('Ctrl Pts',(3.07363462275993,-35.3649068079318,0.810462755253741));
#57006=CARTESIAN_POINT('Ctrl Pts',(3.07123958057232,-35.3826400500681,0.809915880370152));
#57007=CARTESIAN_POINT('Ctrl Pts',(3.07001845225687,-35.4004701197944,0.809287880684534));
#57008=CARTESIAN_POINT('Ctrl Pts',(3.06997148677425,-35.41830018942,0.808582649476606));
#57009=CARTESIAN_POINT('Ctrl Pts',(3.11482379895319,-35.3179001315653,1.1741796201593));
#57010=CARTESIAN_POINT('Ctrl Pts',(3.10654999847949,-35.3398758977186,1.17391975325062));
#57011=CARTESIAN_POINT('Ctrl Pts',(3.10026437692076,-35.3625150846797,1.17350343193823));
#57012=CARTESIAN_POINT('Ctrl Pts',(3.09603282920114,-35.3856026344426,1.17293464162748));
#57013=CARTESIAN_POINT('Ctrl Pts',(3.09388918336483,-35.4089143804985,1.17221983646385));
#57014=CARTESIAN_POINT('Ctrl Pts',(3.09383396923983,-35.4322261265545,1.17136766300268));
#57015=CARTESIAN_POINT('Ctrl Pts',(3.14899944508157,-35.3090615611284,1.53617325026364));
#57016=CARTESIAN_POINT('Ctrl Pts',(3.1367101555031,-35.3343621966333,1.53613435112931));
#57017=CARTESIAN_POINT('Ctrl Pts',(3.12729631378655,-35.3609871657593,1.53585839375451));
#57018=CARTESIAN_POINT('Ctrl Pts',(3.12093762711669,-35.3885169025336,1.53534859968354));
#57019=CARTESIAN_POINT('Ctrl Pts',(3.11772689345012,-35.4164990521042,1.53461531686096));
#57020=CARTESIAN_POINT('Ctrl Pts',(3.11766502652187,-35.4444812016747,1.53367491460431));
#57021=CARTESIAN_POINT('Ctrl Pts',(3.18317242840243,-35.3024139984956,1.89900948084932));
#57022=CARTESIAN_POINT('Ctrl Pts',(3.16696570563031,-35.3301602171214,1.89925261763301));
#57023=CARTESIAN_POINT('Ctrl Pts',(3.15442927680899,-35.3600129806224,1.89918994885649));
#57024=CARTESIAN_POINT('Ctrl Pts',(3.14592306246191,-35.3913305665038,1.89881732341841));
#57025=CARTESIAN_POINT('Ctrl Pts',(3.14163831779052,-35.4233809324929,1.89814458126707));
#57026=CARTESIAN_POINT('Ctrl Pts',(3.14157580097331,-35.4554312984821,1.89719411861838));
#57027=CARTESIAN_POINT('Ctrl Pts',(3.21702289873695,-35.2974551605344,2.2623967664111));
#57028=CARTESIAN_POINT('Ctrl Pts',(3.19709436867799,-35.3269668716473,2.26291650186676));
#57029=CARTESIAN_POINT('Ctrl Pts',(3.18153205145727,-35.3594334352724,2.26306983940211));
#57030=CARTESIAN_POINT('Ctrl Pts',(3.17092279371148,-35.3939890002597,2.26284138838012));
#57031=CARTESIAN_POINT('Ctrl Pts',(3.16558686556525,-35.429590274611,2.26223804886464));
#57032=CARTESIAN_POINT('Ctrl Pts',(3.16552436512682,-35.4651915489622,2.26128784530879));
#57033=CARTESIAN_POINT('',(3.21673308953453,-35.2978265044789,2.26193293203227));
#57034=CARTESIAN_POINT('Origin',(3.46485271691158,-35.4651808043912,2.24112619649787));
#57035=CARTESIAN_POINT('Ctrl Pts',(3.05221609413,-35.3447053607,0.450150554363));
#57036=CARTESIAN_POINT('Ctrl Pts',(3.09862686998935,-35.32217505587,1.01604816889915));
#57037=CARTESIAN_POINT('Ctrl Pts',(3.15705633676715,-35.3065450332706,1.62042102657061));
#57038=CARTESIAN_POINT('Ctrl Pts',(3.2167330984,-35.297826491,2.26193292922));
#57039=CARTESIAN_POINT('Ctrl Pts',(3.21673308013,-35.297826519,2.26193293676));
#57040=CARTESIAN_POINT('Ctrl Pts',(3.19690170746,-35.3272920967,2.26244743731));
#57041=CARTESIAN_POINT('Ctrl Pts',(3.18141841353,-35.3596904513,2.26259731642));
#57042=CARTESIAN_POINT('Ctrl Pts',(3.17086410369,-35.3941615562,2.26236742048));
#57043=CARTESIAN_POINT('Ctrl Pts',(3.16555572757,-35.4296702319,2.26176465335));
#57044=CARTESIAN_POINT('Ctrl Pts',(3.16549338332,-35.4651789077,2.26081682416));
#57045=CARTESIAN_POINT('Ctrl Pts',(3.22044227874,-35.2947170616,2.28115435818));
#57046=CARTESIAN_POINT('Ctrl Pts',(3.19950860612,-35.3245433432,2.27888894627));
#57047=CARTESIAN_POINT('Ctrl Pts',(3.18307576937,-35.3575027832,2.27596054224));
#57048=CARTESIAN_POINT('Ctrl Pts',(3.17178564006,-35.3926825601,2.27243438801));
#57049=CARTESIAN_POINT('Ctrl Pts',(3.16599327189,-35.4289738974,2.26841670742));
#57050=CARTESIAN_POINT('Ctrl Pts',(3.16570519157,-35.4652652348,2.26403697776));
#57051=CARTESIAN_POINT('Ctrl Pts',(3.22504500396,-35.2927962885,2.30073764763));
#57052=CARTESIAN_POINT('Ctrl Pts',(3.20268941154,-35.3227611226,2.2957495854));
#57053=CARTESIAN_POINT('Ctrl Pts',(3.18504154424,-35.3561044246,2.28975874044));
#57054=CARTESIAN_POINT('Ctrl Pts',(3.1728278134,-35.3918504917,2.28291889281));
#57055=CARTESIAN_POINT('Ctrl Pts',(3.16645576111,-35.428799749,2.27544850897));
#57056=CARTESIAN_POINT('Ctrl Pts',(3.16593909074,-35.4657490064,2.26759298308));
#57057=CARTESIAN_POINT('Ctrl Pts',(3.23041275638,-35.292377214,2.32058136088));
#57058=CARTESIAN_POINT('Ctrl Pts',(3.20637961829,-35.3222393286,2.31311572454));
#57059=CARTESIAN_POINT('Ctrl Pts',(3.18729883271,-35.3557626768,2.30425560397));
#57060=CARTESIAN_POINT('Ctrl Pts',(3.1740077501,-35.391902145,2.29425266577));
#57061=CARTESIAN_POINT('Ctrl Pts',(3.16698247964,-35.4293517376,2.28345602024));
#57062=CARTESIAN_POINT('Ctrl Pts',(3.16624513219,-35.4668013301,2.2722457786));
#57063=CARTESIAN_POINT('Ctrl Pts',(3.2362706081,-35.293523699,2.3402171845));
#57064=CARTESIAN_POINT('Ctrl Pts',(3.21039981727,-35.3231016776,2.33049644021));
#57065=CARTESIAN_POINT('Ctrl Pts',(3.18974009686,-35.3566452436,2.31893365909));
#57066=CARTESIAN_POINT('Ctrl Pts',(3.17526480943,-35.3930381712,2.30588852441));
#57067=CARTESIAN_POINT('Ctrl Pts',(3.16753533529,-35.4308584528,2.2918609559));
#57068=CARTESIAN_POINT('Ctrl Pts',(3.16658333925,-35.4686787344,2.27738759286));
#57069=CARTESIAN_POINT('Ctrl Pts',(3.24268782164,-35.2959076878,2.35939290014));
#57070=CARTESIAN_POINT('Ctrl Pts',(3.21479367828,-35.3250197311,2.34761644611));
#57071=CARTESIAN_POINT('Ctrl Pts',(3.19237820629,-35.3584237245,2.33347294503));
#57072=CARTESIAN_POINT('Ctrl Pts',(3.17658501762,-35.3949324563,2.31744225071));
#57073=CARTESIAN_POINT('Ctrl Pts',(3.16808413932,-35.4329970413,2.30020446638));
#57074=CARTESIAN_POINT('Ctrl Pts',(3.16691857253,-35.4710616262,2.28248419619));
#57075=CARTESIAN_POINT('',(3.24268782128875,-35.2959076708926,2.35939286373149));
#57076=CARTESIAN_POINT('Origin',(3.46627170195,-35.4710616254,2.26279399804));
#57077=CARTESIAN_POINT('Ctrl Pts',(3.21673308013,-35.297826519,2.26193293676));
#57078=CARTESIAN_POINT('Ctrl Pts',(3.21862893786144,-35.2962372030246,2.27175745310809));
#57079=CARTESIAN_POINT('Ctrl Pts',(3.22079144998373,-35.2950355889071,2.28162723545145));
#57080=CARTESIAN_POINT('Ctrl Pts',(3.22317351887659,-35.2942698852058,2.29151507432848));
#57081=CARTESIAN_POINT('Ctrl Pts',(3.22559924436156,-35.2934901483192,2.30158412935339));
#57082=CARTESIAN_POINT('Ctrl Pts',(3.22825105142807,-35.2931626326134,2.31167001671416));
#57083=CARTESIAN_POINT('Ctrl Pts',(3.23108861335652,-35.2932948476651,2.32171513954936));
#57084=CARTESIAN_POINT('Ctrl Pts',(3.23368257328602,-35.2934157121801,2.33089789812114));
#57085=CARTESIAN_POINT('Ctrl Pts',(3.23643096040602,-35.2939205810558,2.34004530617035));
#57086=CARTESIAN_POINT('Ctrl Pts',(3.23932672580918,-35.2947802838016,2.34911168757664));
#57087=CARTESIAN_POINT('Ctrl Pts',(3.2404252315784,-35.2951064111961,2.35255101048238));
#57088=CARTESIAN_POINT('Ctrl Pts',(3.24154526402325,-35.2954832297334,2.35597874623171));
#57089=CARTESIAN_POINT('Ctrl Pts',(3.24268781017429,-35.2959076835405,2.35939286587855));
#57090=CARTESIAN_POINT('Origin',(3.46627170195,-35.4710616254,2.26279399804));
#57091=CARTESIAN_POINT('Origin',(3.46628252368698,-35.4710657830243,2.26278661726328));
#57092=CARTESIAN_POINT('Ctrl Pts',(3.24268777888,-35.2959076894,2.3593927975));
#57093=CARTESIAN_POINT('Ctrl Pts',(3.23324424211,-35.3247373359,2.38980935628));
#57094=CARTESIAN_POINT('Ctrl Pts',(3.22953158346,-35.3580565085,2.41774990543));
#57095=CARTESIAN_POINT('Ctrl Pts',(3.23195755579,-35.3946355813,2.44191215472));
#57096=CARTESIAN_POINT('Ctrl Pts',(3.24041432389,-35.4328486033,2.46122208494));
#57097=CARTESIAN_POINT('Ctrl Pts',(3.25430421882,-35.4710616254,2.47509045608));
#57098=CARTESIAN_POINT('Ctrl Pts',(3.24863991984,-35.2942847243,2.3702266206));
#57099=CARTESIAN_POINT('Ctrl Pts',(3.23916638892,-35.3234356974,2.39881134044));
#57100=CARTESIAN_POINT('Ctrl Pts',(3.23504178418,-35.3568515124,2.42482352544));
#57101=CARTESIAN_POINT('Ctrl Pts',(3.23665426145,-35.3933501406,2.4471045325));
#57102=CARTESIAN_POINT('Ctrl Pts',(3.24393773616,-35.4313935606,2.46471965345));
#57103=CARTESIAN_POINT('Ctrl Pts',(3.25638647798,-35.4694369807,2.47716948856));
#57104=CARTESIAN_POINT('Ctrl Pts',(3.25487358313,-35.2930993638,2.38101394136));
#57105=CARTESIAN_POINT('Ctrl Pts',(3.24526333648,-35.3225008542,2.40777429176));
#57106=CARTESIAN_POINT('Ctrl Pts',(3.24064780293,-35.3559526709,2.43188619171));
#57107=CARTESIAN_POINT('Ctrl Pts',(3.24140158851,-35.3923204861,2.45231942081));
#57108=CARTESIAN_POINT('Ctrl Pts',(3.24749724241,-35.4301491895,2.46826188149));
#57109=CARTESIAN_POINT('Ctrl Pts',(3.25851062528,-35.4679778928,2.4792941471));
#57110=CARTESIAN_POINT('Ctrl Pts',(3.26132499233,-35.2924297767,2.39172809926));
#57111=CARTESIAN_POINT('Ctrl Pts',(3.25147493949,-35.3220109395,2.41666518604));
#57112=CARTESIAN_POINT('Ctrl Pts',(3.24629031107,-35.3554385943,2.43889159306));
#57113=CARTESIAN_POINT('Ctrl Pts',(3.24613606992,-35.3916231814,2.45749640868));
#57114=CARTESIAN_POINT('Ctrl Pts',(3.25101894524,-35.429190416,2.4717755436));
#57115=CARTESIAN_POINT('Ctrl Pts',(3.26059110338,-35.4667576505,2.4813793476));
#57116=CARTESIAN_POINT('Ctrl Pts',(3.27380803754,-35.2922400204,2.41170299529));
#57117=CARTESIAN_POINT('Ctrl Pts',(3.26330589806,-35.3220182267,2.4332062407));
#57118=CARTESIAN_POINT('Ctrl Pts',(3.25689030732,-35.3552760482,2.4519082859));
#57119=CARTESIAN_POINT('Ctrl Pts',(3.2549183258,-35.3910159567,2.4670879438));
#57120=CARTESIAN_POINT('Ctrl Pts',(3.25746361688,-35.4279972557,2.47822608485));
#57121=CARTESIAN_POINT('Ctrl Pts',(3.26429684209,-35.4649785547,2.48510046341));
#57122=CARTESIAN_POINT('Ctrl Pts',(3.28670020806,-35.294071477,2.43091483974));
#57123=CARTESIAN_POINT('Ctrl Pts',(3.27515379345,-35.3237564299,2.44902572332));
#57124=CARTESIAN_POINT('Ctrl Pts',(3.26720088432,-35.356600918,2.46426325104));
#57125=CARTESIAN_POINT('Ctrl Pts',(3.26320102423,-35.3916841292,2.47607069605));
#57126=CARTESIAN_POINT('Ctrl Pts',(3.26328224545,-35.4278894975,2.48407361934));
#57127=CARTESIAN_POINT('Ctrl Pts',(3.26732268033,-35.4640948659,2.48814770965));
#57128=CARTESIAN_POINT('Ctrl Pts',(3.29283605957,-35.2953609408,2.43972470037));
#57129=CARTESIAN_POINT('Ctrl Pts',(3.28071360005,-35.3249348657,2.4562706651));
#57130=CARTESIAN_POINT('Ctrl Pts',(3.27197052657,-35.3575262865,2.46991873562));
#57131=CARTESIAN_POINT('Ctrl Pts',(3.2669738349,-35.392260236,2.48016433481));
#57132=CARTESIAN_POINT('Ctrl Pts',(3.26588441111,-35.4280613535,2.48669778017));
#57133=CARTESIAN_POINT('Ctrl Pts',(3.26861160084,-35.463862471,2.48944754786));
#57134=CARTESIAN_POINT('Ctrl Pts',(3.29901947016,-35.297065145,2.44826966141));
#57135=CARTESIAN_POINT('Ctrl Pts',(3.28622719246,-35.3264553013,2.46326747504));
#57136=CARTESIAN_POINT('Ctrl Pts',(3.27662267867,-35.3587390046,2.47532721835));
#57137=CARTESIAN_POINT('Ctrl Pts',(3.27057612082,-35.3930615858,2.48402260776));
#57138=CARTESIAN_POINT('Ctrl Pts',(3.26826446238,-35.4284083467,2.48909446671));
#57139=CARTESIAN_POINT('Ctrl Pts',(3.26965390752,-35.4637551076,2.49049946556));
#57140=CARTESIAN_POINT('Ctrl Pts',(3.30528109747,-35.2990851344,2.45651115245));
#57141=CARTESIAN_POINT('Ctrl Pts',(3.29174991618,-35.3282259173,2.47004146075));
#57142=CARTESIAN_POINT('Ctrl Pts',(3.28123325218,-35.3601462025,2.48060016935));
#57143=CARTESIAN_POINT('Ctrl Pts',(3.27411284989,-35.3940266946,2.48780557152));
#57144=CARTESIAN_POINT('Ctrl Pts',(3.2705944695,-35.4288883397,2.49144945081));
#57145=CARTESIAN_POINT('Ctrl Pts',(3.27067475303,-35.4637499849,2.49153061051));
#57146=CARTESIAN_POINT('',(3.30528110210951,-35.2990851341165,2.45651115699452));
#57147=CARTESIAN_POINT('Origin',(3.48387386404311,-35.4637520991879,2.28046099487966));
#57148=CARTESIAN_POINT('Ctrl Pts',(3.24268782427112,-35.2959076878087,2.35939289967519));
#57149=CARTESIAN_POINT('Ctrl Pts',(3.24767529781159,-35.2945477578349,2.3684708690015));
#57150=CARTESIAN_POINT('Ctrl Pts',(3.25287413301336,-35.2935658779458,2.37746859783919));
#57151=CARTESIAN_POINT('Ctrl Pts',(3.25822104692206,-35.2930305733796,2.38636188968886));
#57152=CARTESIAN_POINT('Ctrl Pts',(3.26356796083076,-35.2924952688133,2.39525518153853));
#57153=CARTESIAN_POINT('Ctrl Pts',(3.26906288166411,-35.2924074772293,2.40404332277373));
#57154=CARTESIAN_POINT('Ctrl Pts',(3.27466035755344,-35.2927955912655,2.41266929519308));
#57155=CARTESIAN_POINT('Ctrl Pts',(3.27960885693669,-35.2931387070033,2.42029516443148));
#57156=CARTESIAN_POINT('Ctrl Pts',(3.28463783441383,-35.2938512388069,2.42779111046201));
#57157=CARTESIAN_POINT('Ctrl Pts',(3.28973967766946,-35.2949119682808,2.43511159557974));
#57158=CARTESIAN_POINT('Ctrl Pts',(3.29414279634187,-35.2958274252085,2.44142950130478));
#57159=CARTESIAN_POINT('Ctrl Pts',(3.29859918080919,-35.2970041061196,2.44761753756102));
#57160=CARTESIAN_POINT('Ctrl Pts',(3.30312239520438,-35.2984029479339,2.45365075531648));
#57161=CARTESIAN_POINT('Ctrl Pts',(3.3038401776055,-35.2986249281339,2.45460815798385));
#57162=CARTESIAN_POINT('Ctrl Pts',(3.30455970208021,-35.2988524136235,2.45556165911652));
#57163=CARTESIAN_POINT('Ctrl Pts',(3.30528109745196,-35.2990851344388,2.45651115246804));
#57164=CARTESIAN_POINT('Ctrl Pts',(3.30528115437,-35.2990850504,2.45651113175));
#57165=CARTESIAN_POINT('Ctrl Pts',(3.29174997169,-35.3282258256,2.47004153063));
#57166=CARTESIAN_POINT('Ctrl Pts',(3.28123332764,-35.3601461205,2.48060031812));
#57167=CARTESIAN_POINT('Ctrl Pts',(3.27411296889,-35.3940266351,2.48780578271));
#57168=CARTESIAN_POINT('Ctrl Pts',(3.27059465556,-35.4288883092,2.49144970493));
#57169=CARTESIAN_POINT('Ctrl Pts',(3.2706750272,-35.4637499833,2.49153088745));
#57170=CARTESIAN_POINT('Ctrl Pts',(3.52263014734,-35.2997786652,2.67764867799));
#57171=CARTESIAN_POINT('Ctrl Pts',(3.50832158865,-35.3287004593,2.68978061947));
#57172=CARTESIAN_POINT('Ctrl Pts',(3.49718986878,-35.3603042564,2.69922432977));
#57173=CARTESIAN_POINT('Ctrl Pts',(3.48962934617,-35.3937968185,2.70564685787));
#57174=CARTESIAN_POINT('Ctrl Pts',(3.48585336684,-35.4282347239,2.70886780417));
#57175=CARTESIAN_POINT('Ctrl Pts',(3.48586067783,-35.4626726292,2.70888759263));
#57176=CARTESIAN_POINT('Ctrl Pts',(3.71975032728,-35.2998840308,2.91888544948));
#57177=CARTESIAN_POINT('Ctrl Pts',(3.70452693031,-35.3287908762,2.92986690945));
#57178=CARTESIAN_POINT('Ctrl Pts',(3.69266813705,-35.3603788898,2.93839702263));
#57179=CARTESIAN_POINT('Ctrl Pts',(3.68459264153,-35.3938552567,2.94417305658));
#57180=CARTESIAN_POINT('Ctrl Pts',(3.68052780808,-35.4282767651,2.94703197385));
#57181=CARTESIAN_POINT('Ctrl Pts',(3.68047391974,-35.4626982735,2.94697615221));
#57182=CARTESIAN_POINT('Ctrl Pts',(3.89420210101,-35.2992579912,3.17776652664));
#57183=CARTESIAN_POINT('Ctrl Pts',(3.87780196962,-35.3284044612,3.18777591948));
#57184=CARTESIAN_POINT('Ctrl Pts',(3.86500520386,-35.3603251829,3.19553496378));
#57185=CARTESIAN_POINT('Ctrl Pts',(3.85627187964,-35.3942021449,3.20076023088));
#57186=CARTESIAN_POINT('Ctrl Pts',(3.85185292871,-35.4290582738,3.20330006316));
#57187=CARTESIAN_POINT('Ctrl Pts',(3.85174986217,-35.4639144026,3.20315896516));
#57188=CARTESIAN_POINT('Ctrl Pts',(4.25043308745,-35.2963608901,3.82861914207));
#57189=CARTESIAN_POINT('Ctrl Pts',(4.23039390269,-35.3265730217,3.83636634601));
#57190=CARTESIAN_POINT('Ctrl Pts',(4.21468510082,-35.3600305104,3.84233146345));
#57191=CARTESIAN_POINT('Ctrl Pts',(4.20392503792,-35.3957885434,3.84626231873));
#57192=CARTESIAN_POINT('Ctrl Pts',(4.19845399885,-35.4326982838,3.848026993));
#57193=CARTESIAN_POINT('Ctrl Pts',(4.19827560656,-35.4696080243,3.84763795769));
#57194=CARTESIAN_POINT('Ctrl Pts',(4.45858902825,-35.291449905,4.54475674437));
#57195=CARTESIAN_POINT('Ctrl Pts',(4.43308531823,-35.3233621358,4.54953750297));
#57196=CARTESIAN_POINT('Ctrl Pts',(4.41292476175,-35.3596262841,4.55315251935));
#57197=CARTESIAN_POINT('Ctrl Pts',(4.39907396454,-35.3990181868,4.55540464772));
#57198=CARTESIAN_POINT('Ctrl Pts',(4.39207409827,-35.4399769064,4.55619669281));
#57199=CARTESIAN_POINT('Ctrl Pts',(4.39192731775,-35.480935626,4.55555318454));
#57200=CARTESIAN_POINT('Ctrl Pts',(4.52558545037,-35.2885903077,4.9733945174));
#57201=CARTESIAN_POINT('Ctrl Pts',(4.4963387214,-35.3214318737,4.97577624036));
#57202=CARTESIAN_POINT('Ctrl Pts',(4.4730869275,-35.3595080502,4.97747837329));
#57203=CARTESIAN_POINT('Ctrl Pts',(4.45708682842,-35.4013807813,4.97836774601));
#57204=CARTESIAN_POINT('Ctrl Pts',(4.44904844444,-35.4451561726,4.97838721155));
#57205=CARTESIAN_POINT('Ctrl Pts',(4.44897072855,-35.4889315639,4.97757277822));
#57206=CARTESIAN_POINT('Ctrl Pts',(4.53663898841,-35.2864927806,5.40585813039));
#57207=CARTESIAN_POINT('Ctrl Pts',(4.5036945439,-35.3198754069,5.40486687422));
#57208=CARTESIAN_POINT('Ctrl Pts',(4.4772847339,-35.3595850208,5.403864254));
#57209=CARTESIAN_POINT('Ctrl Pts',(4.45905487062,-35.4039471568,5.40287237975));
#57210=CARTESIAN_POINT('Ctrl Pts',(4.44995084219,-35.450642856,5.40192600583));
#57211=CARTESIAN_POINT('Ctrl Pts',(4.44996438067,-35.4973385552,5.40106825188));
#57212=CARTESIAN_POINT('Ctrl Pts',(4.49212121119,-35.2852060782,5.83250225872));
#57213=CARTESIAN_POINT('Ctrl Pts',(4.45609896624,-35.3187908717,5.82727331029));
#57214=CARTESIAN_POINT('Ctrl Pts',(4.42697004659,-35.3598847947,5.82278629135));
#57215=CARTESIAN_POINT('Ctrl Pts',(4.40679132226,-35.4065868399,5.81933946513));
#57216=CARTESIAN_POINT('Ctrl Pts',(4.39676913356,-35.4561050288,5.8171388925));
#57217=CARTESIAN_POINT('Ctrl Pts',(4.39688476736,-35.5056232176,5.81623445774));
#57218=CARTESIAN_POINT('',(4.49212120455654,-35.2852060791303,5.8325022569351));
#57219=CARTESIAN_POINT('Origin',(4.69448464672372,-35.5056329710941,5.8542829595805));
#57220=CARTESIAN_POINT('Ctrl Pts',(3.30528111534306,-35.2990851344485,2.45651117077468));
#57221=CARTESIAN_POINT('Ctrl Pts',(3.36062613515312,-35.2992617286018,2.5128208708643));
#57222=CARTESIAN_POINT('Ctrl Pts',(3.416086838459,-35.2993978352638,2.57241171064848));
#57223=CARTESIAN_POINT('Ctrl Pts',(3.47126284716246,-35.2994805332259,2.63546717927527));
#57224=CARTESIAN_POINT('Ctrl Pts',(3.52540792063213,-35.2995616860193,2.69734448902798));
#57225=CARTESIAN_POINT('Ctrl Pts',(3.5792787609624,-35.299591322044,2.76255861405961));
#57226=CARTESIAN_POINT('Ctrl Pts',(3.63245486835527,-35.2995592106656,2.83125670383386));
#57227=CARTESIAN_POINT('Ctrl Pts',(3.68420374847358,-35.2995279611448,2.89811096200321));
#57228=CARTESIAN_POINT('Ctrl Pts',(3.73529451314419,-35.2994381618817,2.96826505591086));
#57229=CARTESIAN_POINT('Ctrl Pts',(3.78530126722225,-35.2992834232217,3.04182356895941));
#57230=CARTESIAN_POINT('Ctrl Pts',(3.80177924062247,-35.2992324345189,3.06606219919488));
#57231=CARTESIAN_POINT('Ctrl Pts',(3.81813920729258,-35.2991744243497,3.09067020136823));
#57232=CARTESIAN_POINT('Ctrl Pts',(3.83436503438466,-35.2991092594134,3.11565044021741));
#57233=CARTESIAN_POINT('Ctrl Pts',(3.88203349803657,-35.2989178169445,3.18903773818631));
#57234=CARTESIAN_POINT('Ctrl Pts',(3.92854659437473,-35.2986642858774,3.26564064025194));
#57235=CARTESIAN_POINT('Ctrl Pts',(3.97347340024928,-35.2983481716719,3.34550625691759));
#57236=CARTESIAN_POINT('Ctrl Pts',(4.01705811664467,-35.2980415006827,3.4229860640028));
#57237=CARTESIAN_POINT('Ctrl Pts',(4.05914965679832,-35.2976758978132,3.50353684824634));
#57238=CARTESIAN_POINT('Ctrl Pts',(4.09932647608738,-35.2972554741226,3.58716217895609));
#57239=CARTESIAN_POINT('Ctrl Pts',(4.12275798127302,-35.2970102790062,3.63593327146291));
#57240=CARTESIAN_POINT('Ctrl Pts',(4.14553770629444,-35.2967465263988,3.68574934450856));
#57241=CARTESIAN_POINT('Ctrl Pts',(4.16757792554145,-35.296465838294,3.73660398153786));
#57242=CARTESIAN_POINT('Ctrl Pts',(4.201498880351,-35.2960338458346,3.81487170769765));
#57243=CARTESIAN_POINT('Ctrl Pts',(4.23366892450562,-35.2955616315989,3.89560128685815));
#57244=CARTESIAN_POINT('Ctrl Pts',(4.26375490829378,-35.2950584202033,3.97874208646125));
#57245=CARTESIAN_POINT('Ctrl Pts',(4.26669543912757,-35.2950092375462,3.98686806587081));
#57246=CARTESIAN_POINT('Ctrl Pts',(4.26993248876024,-35.2949543601435,3.9959049877927));
#57247=CARTESIAN_POINT('Ctrl Pts',(4.2727290262001,-35.2949073184052,4.00379030146189));
#57248=CARTESIAN_POINT('Ctrl Pts',(4.27354346307177,-35.2948936184184,4.00608674495136));
#57249=CARTESIAN_POINT('Ctrl Pts',(4.27432087485892,-35.2948805857688,4.00828539207123));
#57250=CARTESIAN_POINT('Ctrl Pts',(4.27504380979966,-35.294868560589,4.01033502539987));
#57251=CARTESIAN_POINT('Ctrl Pts',(4.31123404893338,-35.294266578163,4.11293999871085));
#57252=CARTESIAN_POINT('Ctrl Pts',(4.34336177273321,-35.2936522261943,4.21671280069685));
#57253=CARTESIAN_POINT('Ctrl Pts',(4.37143663731291,-35.293027724738,4.32157074836816));
#57254=CARTESIAN_POINT('Ctrl Pts',(4.39964431341538,-35.2924002690024,4.42692473916969));
#57255=CARTESIAN_POINT('Ctrl Pts',(4.42376085007101,-35.2917625780507,4.53337486959008));
#57256=CARTESIAN_POINT('Ctrl Pts',(4.44374590523629,-35.2911134178544,4.64085244068075));
#57257=CARTESIAN_POINT('Ctrl Pts',(4.46024409592059,-35.2905775189733,4.72957801323864));
#57258=CARTESIAN_POINT('Ctrl Pts',(4.47392582307022,-35.2900337287775,4.81900424037342));
#57259=CARTESIAN_POINT('Ctrl Pts',(4.48474179324417,-35.2894796369031,4.90909506800667));
#57260=CARTESIAN_POINT('Ctrl Pts',(4.49963111233193,-35.2887168712344,5.03311455566615));
#57261=CARTESIAN_POINT('Ctrl Pts',(4.50891101504119,-35.288019710402,5.15755949064399));
#57262=CARTESIAN_POINT('Ctrl Pts',(4.51258247618356,-35.2874031701943,5.28190637099523));
#57263=CARTESIAN_POINT('Ctrl Pts',(4.51618936873142,-35.2867974728454,5.40406640992722));
#57264=CARTESIAN_POINT('Ctrl Pts',(4.51438337543916,-35.2862696797958,5.52613139504472));
#57265=CARTESIAN_POINT('Ctrl Pts',(4.50721377571749,-35.285823887096,5.64761401154141));
#57266=CARTESIAN_POINT('Ctrl Pts',(4.50356644424897,-35.2855971026443,5.70941486336414));
#57267=CARTESIAN_POINT('Ctrl Pts',(4.4985318012427,-35.285391367349,5.77106518411329));
#57268=CARTESIAN_POINT('Ctrl Pts',(4.49212120720968,-35.2852060820123,5.83250225711667));
#57269=CARTESIAN_POINT('Ctrl Pts',(4.4921212186,-35.2852060642,5.83250225932));
#57270=CARTESIAN_POINT('Ctrl Pts',(4.45609896257,-35.3187908592,5.82727337616));
#57271=CARTESIAN_POINT('Ctrl Pts',(4.42697003004,-35.3598847848,5.82278643887));
#57272=CARTESIAN_POINT('Ctrl Pts',(4.40679129181,-35.4065868334,5.81933970701));
#57273=CARTESIAN_POINT('Ctrl Pts',(4.39676908915,-35.4561050262,5.81713923581));
#57274=CARTESIAN_POINT('Ctrl Pts',(4.39688470965,-35.505623219,5.81623490373));
#57275=CARTESIAN_POINT('Ctrl Pts',(4.47934426829,-35.2848180141,5.95513865982));
#57276=CARTESIAN_POINT('Ctrl Pts',(4.44240767125,-35.3184648135,5.94886804446));
#57277=CARTESIAN_POINT('Ctrl Pts',(4.41246275486,-35.3599636587,5.94360014588));
#57278=CARTESIAN_POINT('Ctrl Pts',(4.39168683777,-35.4073477788,5.9397026792));
#57279=CARTESIAN_POINT('Ctrl Pts',(4.38136362076,-35.457688004,5.93741576176));
#57280=CARTESIAN_POINT('Ctrl Pts',(4.38147338286,-35.5080282291,5.93677544119));
#57281=CARTESIAN_POINT('Ctrl Pts',(4.46080331489,-35.2846612104,6.0774500678));
#57282=CARTESIAN_POINT('Ctrl Pts',(4.42339099946,-35.3183175745,6.07010629864));
#57283=CARTESIAN_POINT('Ctrl Pts',(4.39300176947,-35.3600459293,6.06403311375));
#57284=CARTESIAN_POINT('Ctrl Pts',(4.37188741448,-35.4078395887,6.05967077608));
#57285=CARTESIAN_POINT('Ctrl Pts',(4.36138132105,-35.4586803826,6.05729403028));
#57286=CARTESIAN_POINT('Ctrl Pts',(4.36146441688,-35.5095211765,6.05692288884));
#57287=CARTESIAN_POINT('Ctrl Pts',(4.43653605144,-35.2846213402,6.19885974208));
#57288=CARTESIAN_POINT('Ctrl Pts',(4.39907245731,-35.3182793407,6.19048378347));
#57289=CARTESIAN_POINT('Ctrl Pts',(4.36860698734,-35.360098105,6.18364473746));
#57290=CARTESIAN_POINT('Ctrl Pts',(4.34741298485,-35.4080551513,6.17885069748));
#57291=CARTESIAN_POINT('Ctrl Pts',(4.33684033846,-35.4590962326,6.17640727689));
#57292=CARTESIAN_POINT('Ctrl Pts',(4.33687279452,-35.5101373139,6.17631673235));
#57293=CARTESIAN_POINT('Ctrl Pts',(4.39382617826,-35.2846522393,6.3704629655));
#57294=CARTESIAN_POINT('Ctrl Pts',(4.35687304692,-35.3183144911,6.36073630622));
#57295=CARTESIAN_POINT('Ctrl Pts',(4.32681014412,-35.360077369,6.35290824863));
#57296=CARTESIAN_POINT('Ctrl Pts',(4.3058660926,-35.4079286751,6.34756704555));
#57297=CARTESIAN_POINT('Ctrl Pts',(4.295366459,-35.4588388005,6.34505127094));
#57298=CARTESIAN_POINT('Ctrl Pts',(4.29530142772,-35.5097489259,6.34533949948));
#57299=CARTESIAN_POINT('Ctrl Pts',(4.33989513123,-35.2849598896,6.53848806555));
#57300=CARTESIAN_POINT('Ctrl Pts',(4.30425869633,-35.3185874247,6.5277361976));
#57301=CARTESIAN_POINT('Ctrl Pts',(4.27529524943,-35.3599922268,6.51919887852));
#57302=CARTESIAN_POINT('Ctrl Pts',(4.25509182459,-35.4072223024,6.51350637116));
#57303=CARTESIAN_POINT('Ctrl Pts',(4.2448885603,-35.4573782014,6.51100829607));
#57304=CARTESIAN_POINT('Ctrl Pts',(4.2446848137,-35.5075341005,6.51166242388));
#57305=CARTESIAN_POINT('Ctrl Pts',(4.32271334112,-35.2850814359,6.58854936739));
#57306=CARTESIAN_POINT('Ctrl Pts',(4.28754475087,-35.3186934865,6.57751968609));
#57307=CARTESIAN_POINT('Ctrl Pts',(4.25897443759,-35.3599624877,6.56879320674));
#57308=CARTESIAN_POINT('Ctrl Pts',(4.23903851349,-35.4069590258,6.56300941547));
#57309=CARTESIAN_POINT('Ctrl Pts',(4.22894623833,-35.4568320218,6.56051917828));
#57310=CARTESIAN_POINT('Ctrl Pts',(4.22869977692,-35.5067050179,6.56127483435));
#57311=CARTESIAN_POINT('Ctrl Pts',(4.30455023491,-35.2852434072,6.6381975116));
#57312=CARTESIAN_POINT('Ctrl Pts',(4.26991817238,-35.3188318732,6.62693608199));
#57313=CARTESIAN_POINT('Ctrl Pts',(4.24179867527,-35.3599337083,6.61806209525));
#57314=CARTESIAN_POINT('Ctrl Pts',(4.22216945818,-35.4066468932,6.61221922778));
#57315=CARTESIAN_POINT('Ctrl Pts',(4.21220416739,-35.4561778332,6.6097570786));
#57316=CARTESIAN_POINT('Ctrl Pts',(4.21190811788,-35.5057087732,6.61062231004));
#57317=CARTESIAN_POINT('Ctrl Pts',(4.28541381497,-35.285453273,6.6874287475));
#57318=CARTESIAN_POINT('Ctrl Pts',(4.251389142,-35.3190062299,6.67597342108));
#57319=CARTESIAN_POINT('Ctrl Pts',(4.22378115684,-35.359906937,6.66698096996));
#57320=CARTESIAN_POINT('Ctrl Pts',(4.20450211564,-35.4062855347,6.66109555831));
#57321=CARTESIAN_POINT('Ctrl Pts',(4.19468580977,-35.4554145194,6.65866330444));
#57322=CARTESIAN_POINT('Ctrl Pts',(4.1943405656,-35.5045435041,6.65962635024));
#57323=CARTESIAN_POINT('',(4.28541381260123,-35.2854532749764,6.68742874668675));
#57324=CARTESIAN_POINT('Origin',(4.4767625297971,-35.5045528794638,6.76087257923098));
#57325=CARTESIAN_POINT('Ctrl Pts',(4.49212120362943,-35.2852060781576,5.83250225714692));
#57326=CARTESIAN_POINT('Ctrl Pts',(4.48501821379885,-35.28499034928,5.90067858056652));
#57327=CARTESIAN_POINT('Ctrl Pts',(4.475829510371,-35.2848603581573,5.96821991475356));
#57328=CARTESIAN_POINT('Ctrl Pts',(4.46467408476022,-35.2847795393672,6.03493028032477));
#57329=CARTESIAN_POINT('Ctrl Pts',(4.45188175642594,-35.2846868615497,6.1114294592411));
#57330=CARTESIAN_POINT('Ctrl Pts',(4.43650318723529,-35.2846578504948,6.18683720321124));
#57331=CARTESIAN_POINT('Ctrl Pts',(4.41873689817154,-35.2846719377395,6.26092150264478));
#57332=CARTESIAN_POINT('Ctrl Pts',(4.4044190107383,-35.2846832906779,6.32062618582616));
#57333=CARTESIAN_POINT('Ctrl Pts',(4.38855082920743,-35.2847233237578,6.3794730929799));
#57334=CARTESIAN_POINT('Ctrl Pts',(4.37124286446852,-35.2848002119189,6.43735428099128));
#57335=CARTESIAN_POINT('Ctrl Pts',(4.35373712223533,-35.2848779786783,6.49589687526874));
#57336=CARTESIAN_POINT('Ctrl Pts',(4.33475645529202,-35.2849936461652,6.55345665712876));
#57337=CARTESIAN_POINT('Ctrl Pts',(4.31442499448376,-35.2851691523084,6.60992387941392));
#57338=CARTESIAN_POINT('Ctrl Pts',(4.30503833801705,-35.2852501802231,6.63599374336607));
#57339=CARTESIAN_POINT('Ctrl Pts',(4.29536409669719,-35.2853441502275,6.66183019340778));
#57340=CARTESIAN_POINT('Ctrl Pts',(4.28541381473644,-35.2854532732707,6.68742874730075));
#57341=CARTESIAN_POINT('Ctrl Pts',(4.2857571149995,-35.2854498008873,6.68654438213887));
#57342=CARTESIAN_POINT('Ctrl Pts',(4.25155378038641,-35.3191684201121,6.67503743859588));
#57343=CARTESIAN_POINT('Ctrl Pts',(4.22383204100074,-35.3603102200634,6.6660165794383));
#57344=CARTESIAN_POINT('Ctrl Pts',(4.20453371664109,-35.4069770322371,6.66013544312534));
#57345=CARTESIAN_POINT('Ctrl Pts',(4.19480628016729,-35.4563954305725,6.65774375063294));
#57346=CARTESIAN_POINT('Ctrl Pts',(4.19464691082663,-35.5057728190552,6.65877872825311));
#57347=CARTESIAN_POINT('Ctrl Pts',(4.11435014520936,-35.2871852849674,7.12824617423143));
#57348=CARTESIAN_POINT('Ctrl Pts',(4.08577860869936,-35.3206021659747,7.11438447090243));
#57349=CARTESIAN_POINT('Ctrl Pts',(4.06287836005714,-35.3599631233916,7.10355205693462));
#57350=CARTESIAN_POINT('Ctrl Pts',(4.04699017908423,-35.4036584698343,7.09644153341169));
#57351=CARTESIAN_POINT('Ctrl Pts',(4.03888572751518,-35.4495094136804,7.09342297952844));
#57352=CARTESIAN_POINT('Ctrl Pts',(4.03857492304847,-35.4953282298792,7.09444332714258));
#57353=CARTESIAN_POINT('Ctrl Pts',(3.87834409676772,-35.2903635149614,7.54483809333952));
#57354=CARTESIAN_POINT('Ctrl Pts',(3.85593408038674,-35.3229175784704,7.53014366147255));
#57355=CARTESIAN_POINT('Ctrl Pts',(3.83817610056273,-35.3599431212855,7.51876969980455));
#57356=CARTESIAN_POINT('Ctrl Pts',(3.82587986171587,-35.4001589270382,7.51130626410611));
#57357=CARTESIAN_POINT('Ctrl Pts',(3.81949988822795,-35.4419595846812,7.5080608625387));
#57358=CARTESIAN_POINT('Ctrl Pts',(3.819053097548,-35.4837366209665,7.5089954441848));
#57359=CARTESIAN_POINT('Ctrl Pts',(3.58344977045482,-35.2955229188271,7.9236050894372));
#57360=CARTESIAN_POINT('Ctrl Pts',(3.56687361287628,-35.3263185284973,7.90983251579037));
#57361=CARTESIAN_POINT('Ctrl Pts',(3.55380176218302,-35.3602864301414,7.89927969686287));
#57362=CARTESIAN_POINT('Ctrl Pts',(3.54470005686475,-35.3964847830565,7.892361948371));
#57363=CARTESIAN_POINT('Ctrl Pts',(3.53982931256782,-35.433790776985,7.88929217376211));
#57364=CARTESIAN_POINT('Ctrl Pts',(3.53920539592514,-35.4710802621639,7.89004706986091));
#57365=CARTESIAN_POINT('Ctrl Pts',(2.7884326259249,-35.3119516745262,8.68810001722839));
#57366=CARTESIAN_POINT('Ctrl Pts',(2.78288166507677,-35.3368781016926,8.6783873695996));
#57367=CARTESIAN_POINT('Ctrl Pts',(2.77860928612365,-35.362795726313,8.67108096090887));
#57368=CARTESIAN_POINT('Ctrl Pts',(2.7756311279895,-35.3893740464784,8.66629508813301));
#57369=CARTESIAN_POINT('Ctrl Pts',(2.77395449793439,-35.4162800377925,8.66408572229646));
#57370=CARTESIAN_POINT('Ctrl Pts',(2.77358557207991,-35.4431811452579,8.66445053727045));
#57371=CARTESIAN_POINT('Ctrl Pts',(1.7897157019,-35.3293337971,9.16292213266));
#57372=CARTESIAN_POINT('Ctrl Pts',(1.78816995510962,-35.3472022339894,9.15780424233925));
#57373=CARTESIAN_POINT('Ctrl Pts',(1.78689877850668,-35.3654037562666,9.15395288550329));
#57374=CARTESIAN_POINT('Ctrl Pts',(1.78591133611386,-35.3838310440629,9.15138999603306));
#57375=CARTESIAN_POINT('Ctrl Pts',(1.78521442899343,-35.4023704701083,9.15012684960892));
#57376=CARTESIAN_POINT('Ctrl Pts',(1.78480953452593,-35.4209082248919,9.15016379054982));
#57377=CARTESIAN_POINT('Ctrl Pts',(1.17958127456,-35.3376427744,9.32328709823));
#57378=CARTESIAN_POINT('Ctrl Pts',(1.1795177740293,-35.3527252284187,9.31930419456785));
#57379=CARTESIAN_POINT('Ctrl Pts',(1.17962324905309,-35.3680915604398,9.31631951498919));
#57380=CARTESIAN_POINT('Ctrl Pts',(1.17989610757511,-35.3836484756564,9.31435986643977));
#57381=CARTESIAN_POINT('Ctrl Pts',(1.18033338523472,-35.3992999531728,9.31343839198126));
#57382=CARTESIAN_POINT('Ctrl Pts',(1.18093154393229,-35.4149500212705,9.31355423483848));
#57383=CARTESIAN_POINT('Ctrl Pts',(0.559260434794,-35.3376563848,9.36581532526));
#57384=CARTESIAN_POINT('Ctrl Pts',(0.558544684725532,-35.3519810096587,
9.36214503977062));
#57385=CARTESIAN_POINT('Ctrl Pts',(0.557873133674002,-35.366519714233,9.35935950961906));
#57386=CARTESIAN_POINT('Ctrl Pts',(0.557250656370557,-35.3812021204197,
9.35747655687641));
#57387=CARTESIAN_POINT('Ctrl Pts',(0.55668135112757,-35.3959558431041,9.35650540869865));
#57388=CARTESIAN_POINT('Ctrl Pts',(0.556168381827813,-35.4107085027404,
9.35644644218252));
#57389=CARTESIAN_POINT('Ctrl Pts',(-0.051310852811,-35.3354014219,9.29455995377));
#57390=CARTESIAN_POINT('Ctrl Pts',(-0.0507122350892525,-35.3509096123029,
9.29036543781367));
#57391=CARTESIAN_POINT('Ctrl Pts',(-0.0502350705067947,-35.366701542761,
9.28720264732302));
#57392=CARTESIAN_POINT('Ctrl Pts',(-0.0498829422298899,-35.3826844332909,
9.28509669210183));
#57393=CARTESIAN_POINT('Ctrl Pts',(-0.0496579695573275,-35.3987620938252,
9.28406024710945));
#57394=CARTESIAN_POINT('Ctrl Pts',(-0.049560732354575,-35.4148383418483,
9.28409309993256));
#57395=CARTESIAN_POINT('Ctrl Pts',(4.28541380927,-35.2854532781,6.68742874581));
#57396=CARTESIAN_POINT('Ctrl Pts',(4.24024106746993,-35.2859109819706,6.80375439668074));
#57397=CARTESIAN_POINT('Ctrl Pts',(4.18962800213566,-35.2865074754667,6.91808857909236));
#57398=CARTESIAN_POINT('Ctrl Pts',(4.1338105460796,-35.2872466077222,7.02993790187778));
#57399=CARTESIAN_POINT('Ctrl Pts',(4.08906901210241,-35.2878390731132,7.11959283474865));
#57400=CARTESIAN_POINT('Ctrl Pts',(4.04098438539919,-35.2885230593247,7.20765199327025));
#57401=CARTESIAN_POINT('Ctrl Pts',(3.98969543243286,-35.2892965735864,7.29387761510677));
#57402=CARTESIAN_POINT('Ctrl Pts',(3.93205810027539,-35.2901658309188,7.39077596297399));
#57403=CARTESIAN_POINT('Ctrl Pts',(3.87037356895584,-35.2911490776896,7.4853566990516));
#57404=CARTESIAN_POINT('Ctrl Pts',(3.80486079630046,-35.292245051124,7.57729493777813));
#57405=CARTESIAN_POINT('Ctrl Pts',(3.77210440997277,-35.2927930378412,7.62326405714139));
#57406=CARTESIAN_POINT('Ctrl Pts',(3.73839133114429,-35.2933692054693,7.66857282309408));
#57407=CARTESIAN_POINT('Ctrl Pts',(3.70375113596166,-35.2939734289908,7.71318231425977));
#57408=CARTESIAN_POINT('Ctrl Pts',(3.68643103837034,-35.2942755407515,7.73548705984261));
#57409=CARTESIAN_POINT('Ctrl Pts',(3.66887917674681,-35.2945846811323,7.75761699771901));
#57410=CARTESIAN_POINT('Ctrl Pts',(3.65109939460978,-35.2949008234548,7.77956738237956));
#57411=CARTESIAN_POINT('Ctrl Pts',(3.64220950354126,-35.295058894616,7.79054257470984));
#57412=CARTESIAN_POINT('Ctrl Pts',(3.63326263329915,-35.2952187171955,7.80147287941059));
#57413=CARTESIAN_POINT('Ctrl Pts',(3.62425927144795,-35.2953802907213,7.81235770916504));
#57414=CARTESIAN_POINT('Ctrl Pts',(3.61975759052235,-35.2954610774842,7.81780012404226));
#57415=CARTESIAN_POINT('Ctrl Pts',(3.61524178675509,-35.2955423020413,7.82323117023066));
#57416=CARTESIAN_POINT('Ctrl Pts',(3.61071192163445,-35.2956239643472,7.8286507747736));
#57417=CARTESIAN_POINT('Ctrl Pts',(3.60844698907413,-35.2956647955002,7.83136057704507));
#57418=CARTESIAN_POINT('Ctrl Pts',(3.60617854117927,-35.295705736094,7.8340675189082));
#57419=CARTESIAN_POINT('Ctrl Pts',(3.60390658567017,-35.2957467861229,7.83677159127279));
#57420=CARTESIAN_POINT('Ctrl Pts',(3.60163463016106,-35.2957878361517,7.83947566363739));
#57421=CARTESIAN_POINT('Ctrl Pts',(3.5984657767767,-35.295845173692,7.84323465315565));
#57422=CARTESIAN_POINT('Ctrl Pts',(3.59708020403902,-35.2958702645169,7.84487519079636));
#57423=CARTESIAN_POINT('Ctrl Pts',(3.57251009288989,-35.2963151955827,7.87396654852909));
#57424=CARTESIAN_POINT('Ctrl Pts',(3.54536199564617,-35.2968211811022,7.90528994862769));
#57425=CARTESIAN_POINT('Ctrl Pts',(3.51542410262016,-35.2973885258685,7.9386354704925));
#57426=CARTESIAN_POINT('Ctrl Pts',(3.48572084541715,-35.2979514241158,7.97171964951802));
#57427=CARTESIAN_POINT('Ctrl Pts',(3.45327090926628,-35.2985747630115,8.00679463923754));
#57428=CARTESIAN_POINT('Ctrl Pts',(3.41784676062168,-35.2992589206647,8.0436089066258));
#57429=CARTESIAN_POINT('Ctrl Pts',(3.38301285837218,-35.2999316787048,8.07980976509822));
#57430=CARTESIAN_POINT('Ctrl Pts',(3.34530251111634,-35.3006633028627,8.11769260113828));
#57431=CARTESIAN_POINT('Ctrl Pts',(3.30448645840364,-35.3014535220577,8.15696995549352));
#57432=CARTESIAN_POINT('Ctrl Pts',(3.27765591397394,-35.3019729748174,8.18278903232897));
#57433=CARTESIAN_POINT('Ctrl Pts',(3.24948309679918,-35.3025177359954,8.20920970917208));
#57434=CARTESIAN_POINT('Ctrl Pts',(3.21990151995639,-35.3030873574058,8.23613808459519));
#57435=CARTESIAN_POINT('Ctrl Pts',(3.17653599361247,-35.30392240188,8.27561411320639));
#57436=CARTESIAN_POINT('Ctrl Pts',(3.13014290708392,-35.3048106190462,8.31618346611674));
#57437=CARTESIAN_POINT('Ctrl Pts',(3.08051048119044,-35.305754786797,8.35750853562693));
#57438=CARTESIAN_POINT('Ctrl Pts',(3.03487856903338,-35.3066228519598,8.3955026877931));
#57439=CARTESIAN_POINT('Ctrl Pts',(2.98650811680595,-35.3075382802448,8.43413524351376));
#57440=CARTESIAN_POINT('Ctrl Pts',(2.93524278845432,-35.308499231208,8.47310597847456));
#57441=CARTESIAN_POINT('Ctrl Pts',(2.90959514805766,-35.3089799874137,8.49260273053693));
#57442=CARTESIAN_POINT('Ctrl Pts',(2.88322259430676,-35.3094725726033,8.51218358748032));
#57443=CARTESIAN_POINT('Ctrl Pts',(2.85610655008563,-35.3099778173175,8.53180663003467));
#57444=CARTESIAN_POINT('Ctrl Pts',(2.82664631909365,-35.3105267405256,8.55312608805378));
#57445=CARTESIAN_POINT('Ctrl Pts',(2.79630846918575,-35.3110906045039,8.57449539050833));
#57446=CARTESIAN_POINT('Ctrl Pts',(2.76506896671193,-35.3116707290185,8.59585757517973));
#57447=CARTESIAN_POINT('Ctrl Pts',(2.73507234703232,-35.3122277729229,8.61636985221264));
#57448=CARTESIAN_POINT('Ctrl Pts',(2.70424395977659,-35.3128021725465,8.63687447551125));
#57449=CARTESIAN_POINT('Ctrl Pts',(2.67256696449636,-35.313386467183,8.65732090004896));
#57450=CARTESIAN_POINT('Ctrl Pts',(2.66415276262506,-35.3135416704458,8.66275198156678));
#57451=CARTESIAN_POINT('Ctrl Pts',(2.65567867942147,-35.3136975738044,8.66817894503978));
#57452=CARTESIAN_POINT('Ctrl Pts',(2.6471443888335,-35.3138541517961,8.67360075492415));
#57453=CARTESIAN_POINT('Ctrl Pts',(2.64294391768473,-35.3139312175265,8.67626930197661));
#57454=CARTESIAN_POINT('Ctrl Pts',(2.63872886152726,-35.3140084466549,8.67893660035388));
#57455=CARTESIAN_POINT('Ctrl Pts',(2.63449918232813,-35.3140858359642,8.68160252527109));
#57456=CARTESIAN_POINT('Ctrl Pts',(2.63190476989879,-35.3141333052347,8.68323775773561));
#57457=CARTESIAN_POINT('Ctrl Pts',(2.62930485572997,-35.314180834769,8.68487247343467));
#57458=CARTESIAN_POINT('Ctrl Pts',(2.62669943115083,-35.314228423802,8.6865066434089));
#57459=CARTESIAN_POINT('Ctrl Pts',(2.62514069149448,-35.3142568947521,8.68748431344565));
#57460=CARTESIAN_POINT('Ctrl Pts',(2.62358292210444,-35.3142853333759,8.68845995462797));
#57461=CARTESIAN_POINT('Ctrl Pts',(2.6220064146994,-35.3143140988695,8.68944586462671));
#57462=CARTESIAN_POINT('Ctrl Pts',(2.61354724677354,-35.3144684477419,8.6947360257845));
#57463=CARTESIAN_POINT('Ctrl Pts',(2.60467180624005,-35.3146299330446,8.70024225252914));
#57464=CARTESIAN_POINT('Ctrl Pts',(2.59602944765013,-35.3147866965919,8.70555954544832));
#57465=CARTESIAN_POINT('Ctrl Pts',(2.59177578678166,-35.3148638536503,8.70817665055698));
#57466=CARTESIAN_POINT('Ctrl Pts',(2.58757877086762,-35.3149398678404,8.71074828419458));
#57467=CARTESIAN_POINT('Ctrl Pts',(2.58351682731367,-35.3150133321632,8.71322783392397));
#57468=CARTESIAN_POINT('Ctrl Pts',(2.58099028799958,-35.3150590271605,8.71477012021853));
#57469=CARTESIAN_POINT('Ctrl Pts',(2.57851601941034,-35.3151037357486,8.71627680231907));
#57470=CARTESIAN_POINT('Ctrl Pts',(2.57611300778938,-35.3151471203659,8.71773685678189));
#57471=CARTESIAN_POINT('Ctrl Pts',(2.57520999908579,-35.3151634235276,8.71828551908388));
#57472=CARTESIAN_POINT('Ctrl Pts',(2.57431880219543,-35.3151795082263,8.71882654127799));
#57473=CARTESIAN_POINT('Ctrl Pts',(2.57342464839827,-35.3151956411518,8.71936890343435));
#57474=CARTESIAN_POINT('Ctrl Pts',(2.50161040160182,-35.3164913621921,8.76292889263726));
#57475=CARTESIAN_POINT('Ctrl Pts',(2.43070155120575,-35.3177371289784,8.80298312010605));
#57476=CARTESIAN_POINT('Ctrl Pts',(2.36103654431604,-35.3189216230598,8.83985681612805));
#57477=CARTESIAN_POINT('Ctrl Pts',(2.29054178984295,-35.3201202251008,8.87716969763973));
#57478=CARTESIAN_POINT('Ctrl Pts',(2.22132063725928,-35.3212560237631,8.91122630180714));
#57479=CARTESIAN_POINT('Ctrl Pts',(2.1536701020784,-35.3223214184583,8.94236687148854));
#57480=CARTESIAN_POINT('Ctrl Pts',(2.08494789805377,-35.3234036903342,8.97400074662887));
#57481=CARTESIAN_POINT('Ctrl Pts',(2.0178463214947,-35.3244133041604,9.00262592005154));
#57482=CARTESIAN_POINT('Ctrl Pts',(1.95262311278269,-35.3253470381652,9.02859536222033));
#57483=CARTESIAN_POINT('Ctrl Pts',(1.88507526932016,-35.3263140515894,9.05549038699859));
#57484=CARTESIAN_POINT('Ctrl Pts',(1.81954192555313,-35.3271997062196,9.0795375553486));
#57485=CARTESIAN_POINT('Ctrl Pts',(1.75625188784759,-35.3280053709617,9.10111818708299));
#57486=CARTESIAN_POINT('Ctrl Pts',(1.69179021281346,-35.3288259503242,9.12309832361515));
#57487=CARTESIAN_POINT('Ctrl Pts',(1.62965570329652,-35.3295636157407,9.14252004395282));
#57488=CARTESIAN_POINT('Ctrl Pts',(1.57003931091995,-35.3302240353103,9.15976651693667));
#57489=CARTESIAN_POINT('Ctrl Pts',(1.5279546430745,-35.3306902416191,9.17194122355841));
#57490=CARTESIAN_POINT('Ctrl Pts',(1.48712382691784,-35.3311180448658,9.18303150086806));
#57491=CARTESIAN_POINT('Ctrl Pts',(1.44760068982356,-35.3315103566297,9.19316480258379));
#57492=CARTESIAN_POINT('Ctrl Pts',(1.42783912127643,-35.3317065125117,9.19823145344166));
#57493=CARTESIAN_POINT('Ctrl Pts',(1.40840430687648,-35.331893805453,9.20305875978609));
#57494=CARTESIAN_POINT('Ctrl Pts',(1.38930206702301,-35.332072648973,9.20766201286909));
#57495=CARTESIAN_POINT('Ctrl Pts',(1.37975094709627,-35.332162070733,9.20996363941059));
#57496=CARTESIAN_POINT('Ctrl Pts',(1.37028296542892,-35.3322493805427,9.21220924488872));
#57497=CARTESIAN_POINT('Ctrl Pts',(1.36089878598297,-35.3323346325335,9.21440070110702));
#57498=CARTESIAN_POINT('Ctrl Pts',(1.35855274112149,-35.3323559455312,9.2149485651616));
#57499=CARTESIAN_POINT('Ctrl Pts',(1.3562119338634,-35.3323771299207,9.21549304471547));
#57500=CARTESIAN_POINT('Ctrl Pts',(1.3538763743911,-35.3323981865595,9.21603416870073));
#57501=CARTESIAN_POINT('Ctrl Pts',(1.35212470478687,-35.3324139790386,9.21644001168968));
#57502=CARTESIAN_POINT('Ctrl Pts',(1.35037598705937,-35.332429699658,9.21684396716901));
#57503=CARTESIAN_POINT('Ctrl Pts',(1.34863022545477,-35.3324453487813,9.21724604730288));
#57504=CARTESIAN_POINT('Ctrl Pts',(1.34825195219046,-35.3324487396481,9.21733317040397));
#57505=CARTESIAN_POINT('Ctrl Pts',(1.34787429415118,-35.3324521228457,9.21742009462205));
#57506=CARTESIAN_POINT('Ctrl Pts',(1.34750862334315,-35.3324553967057,9.21750420799601));
#57507=CARTESIAN_POINT('Ctrl Pts',(1.34322339306478,-35.332493762481,9.21848991746203));
#57508=CARTESIAN_POINT('Ctrl Pts',(1.3401117239812,-35.3325214994015,9.2192024335089));
#57509=CARTESIAN_POINT('Ctrl Pts',(1.33464358697006,-35.3325697621369,9.2204418813168));
#57510=CARTESIAN_POINT('Ctrl Pts',(1.33411798538048,-35.3325744011886,9.22056101800571));
#57511=CARTESIAN_POINT('Ctrl Pts',(1.33357060365973,-35.3325792284085,9.22068498414979));
#57512=CARTESIAN_POINT('Ctrl Pts',(1.33299830070387,-35.3325842703551,9.22081446104479));
#57513=CARTESIAN_POINT('Ctrl Pts',(1.22309618033819,-35.3335524998829,9.24567853898191));
#57514=CARTESIAN_POINT('Ctrl Pts',(1.11238400514564,-35.3343710619394,9.26599310258083));
#57515=CARTESIAN_POINT('Ctrl Pts',(1.0012607468286,-35.3350043564305,9.28172514514179));
#57516=CARTESIAN_POINT('Ctrl Pts',(0.892850208941656,-35.3356221910536,
9.29707313998935));
#57517=CARTESIAN_POINT('Ctrl Pts',(0.784048819329241,-35.3360637385827,
9.3080595459942));
#57518=CARTESIAN_POINT('Ctrl Pts',(0.675207822854559,-35.3363181886785,
9.31469184807216));
#57519=CARTESIAN_POINT('Ctrl Pts',(0.568801182897241,-35.3365669476995,
9.32117581093685));
#57520=CARTESIAN_POINT('Ctrl Pts',(0.462357137263987,-35.3366369812772,
9.32349823724202));
#57521=CARTESIAN_POINT('Ctrl Pts',(0.356179114394229,-35.3365386439424,
9.32170372792902));
#57522=CARTESIAN_POINT('Ctrl Pts',(0.253833191420349,-35.3364438557272,
9.31997398473961));
#57523=CARTESIAN_POINT('Ctrl Pts',(0.151734892334258,-35.3361927823853,
9.31441921880504));
#57524=CARTESIAN_POINT('Ctrl Pts',(0.0501262832644089,-35.3358120216967,
9.30511395701379));
#57525=CARTESIAN_POINT('Ctrl Pts',(0.0334043515955558,-35.3357493591499,
9.3035825715017));
#57526=CARTESIAN_POINT('Ctrl Pts',(0.0166956057676047,-35.3356832206361,
9.30194968430529));
#57527=CARTESIAN_POINT('Ctrl Pts',(1.02886205599617E-6,-35.3356137675225,
9.30021571864812));
#57528=CARTESIAN_POINT('Ctrl Pts',(-2.60523473148,-35.3742356128,8.65541043601));
#57529=CARTESIAN_POINT('Ctrl Pts',(-2.76838711967,-34.7942356128,8.92400932641));
#57530=CARTESIAN_POINT('Ctrl Pts',(-2.93016897988,-34.2142356128,9.19332068473));
#57531=CARTESIAN_POINT('Ctrl Pts',(-3.09077135202,-33.6342356128,9.46303508034));
#57532=CARTESIAN_POINT('Ctrl Pts',(-3.25037602177,-33.0542356128,9.73294848656));
#57533=CARTESIAN_POINT('Ctrl Pts',(-3.40914395912,-32.4742356128,10.0029291615));
#57534=CARTESIAN_POINT('Ctrl Pts',(-2.08749540657,-35.3742356128,8.79956130216));
#57535=CARTESIAN_POINT('Ctrl Pts',(-2.20333316497,-34.7942356128,9.04664158555));
#57536=CARTESIAN_POINT('Ctrl Pts',(-2.31825723806,-34.2142356128,9.29419684756));
#57537=CARTESIAN_POINT('Ctrl Pts',(-2.43239498576,-33.6342356128,9.5420208011));
#57538=CARTESIAN_POINT('Ctrl Pts',(-2.54586759853,-33.0542356128,9.78997742837));
#57539=CARTESIAN_POINT('Ctrl Pts',(-2.6587823897,-32.4742356128,10.0379789015));
#57540=CARTESIAN_POINT('Ctrl Pts',(-1.56975608167,-35.3742356128,8.94371216831));
#57541=CARTESIAN_POINT('Ctrl Pts',(-1.63827921028,-34.7942356128,9.1692738447));
#57542=CARTESIAN_POINT('Ctrl Pts',(-1.70634549623,-34.2142356128,9.39507301039));
#57543=CARTESIAN_POINT('Ctrl Pts',(-1.77401861949,-33.6342356128,9.62100652185));
#57544=CARTESIAN_POINT('Ctrl Pts',(-1.84135917528,-33.0542356128,9.84700637017));
#57545=CARTESIAN_POINT('Ctrl Pts',(-1.90842082028,-32.4742356128,10.0730286414));
#57546=CARTESIAN_POINT('Ctrl Pts',(-1.05201675677,-35.3742356128,9.08786303446));
#57547=CARTESIAN_POINT('Ctrl Pts',(-1.07322525559,-34.7942356128,9.29190610384));
#57548=CARTESIAN_POINT('Ctrl Pts',(-1.09443375441,-34.2142356128,9.49594917322));
#57549=CARTESIAN_POINT('Ctrl Pts',(-1.11564225322,-33.6342356128,9.6999922426));
#57550=CARTESIAN_POINT('Ctrl Pts',(-1.13685075204,-33.0542356128,9.90403531198));
#57551=CARTESIAN_POINT('Ctrl Pts',(-1.15805925086,-32.4742356128,10.1080783814));
#57552=CARTESIAN_POINT('Ctrl Pts',(0.511836420903,-35.3742356128,9.5232767248));
#57553=CARTESIAN_POINT('Ctrl Pts',(0.628849173616,-34.7942356128,9.66130309814));
#57554=CARTESIAN_POINT('Ctrl Pts',(0.745861926328,-34.2142356128,9.79932947148));
#57555=CARTESIAN_POINT('Ctrl Pts',(0.862874679041,-33.6342356128,9.93735584482));
#57556=CARTESIAN_POINT('Ctrl Pts',(0.979887431754,-33.0542356128,10.0753822182));
#57557=CARTESIAN_POINT('Ctrl Pts',(1.09690018447,-32.4742356128,10.2134085915));
#57558=CARTESIAN_POINT('Ctrl Pts',(2.16072134347,-35.3742356128,9.16274026182));
#57559=CARTESIAN_POINT('Ctrl Pts',(2.3948826075,-34.7942356128,9.28181994923));
#57560=CARTESIAN_POINT('Ctrl Pts',(2.62904387153,-34.2142356128,9.40089963664));
#57561=CARTESIAN_POINT('Ctrl Pts',(2.86320513556,-33.6342356128,9.51997932405));
#57562=CARTESIAN_POINT('Ctrl Pts',(3.09736639959,-33.0542356128,9.63905901146));
#57563=CARTESIAN_POINT('Ctrl Pts',(3.33152766362,-32.4742356128,9.75813869887));
#57564=CARTESIAN_POINT('Ctrl Pts',(3.13619409311,-35.3742356128,8.55164595878));
#57565=CARTESIAN_POINT('Ctrl Pts',(3.45938700394,-34.7942356128,8.6832339856));
#57566=CARTESIAN_POINT('Ctrl Pts',(3.78257991477,-34.2142356128,8.81482201242));
#57567=CARTESIAN_POINT('Ctrl Pts',(4.1057728256,-33.6342356128,8.94641003924));
#57568=CARTESIAN_POINT('Ctrl Pts',(4.42896573643,-33.0542356128,9.07799806607));
#57569=CARTESIAN_POINT('Ctrl Pts',(4.75215864726,-32.4742356128,9.20958609289));
#57570=CARTESIAN_POINT('Ctrl Pts',(3.83208911107,-35.3742356128,7.6674137228));
#57571=CARTESIAN_POINT('Ctrl Pts',(4.27752956283,-34.7942356128,7.82055675035));
#57572=CARTESIAN_POINT('Ctrl Pts',(4.7229700146,-34.2142356128,7.97369977791));
#57573=CARTESIAN_POINT('Ctrl Pts',(5.16841046636,-33.6342356128,8.12684280547));
#57574=CARTESIAN_POINT('Ctrl Pts',(5.61385091813,-33.0542356128,8.27998583302));
#57575=CARTESIAN_POINT('Ctrl Pts',(6.05929136989,-32.4742356128,8.43312886058));
#57576=CARTESIAN_POINT('Ctrl Pts',(4.19318797439,-35.3742356128,6.66283715371));
#57577=CARTESIAN_POINT('Ctrl Pts',(4.79568377915,-34.7942356128,6.82348987203));
#57578=CARTESIAN_POINT('Ctrl Pts',(5.3981795839,-34.2142356128,6.98414259034));
#57579=CARTESIAN_POINT('Ctrl Pts',(6.00067538866,-33.6342356128,7.14479530865));
#57580=CARTESIAN_POINT('Ctrl Pts',(6.60317119342,-33.0542356128,7.30544802697));
#57581=CARTESIAN_POINT('Ctrl Pts',(7.20566699818,-32.4742356128,7.46610074528));
#57582=CARTESIAN_POINT('',(-1.71543475557812E-5,-32.7425794170381,10.0435077220134));
#57583=CARTESIAN_POINT('Ctrl Pts',(6.71017463815815E-10,-35.3356164375956,
9.30022551106375));
#57584=CARTESIAN_POINT('Ctrl Pts',(9.35141029305416E-9,-35.1420353216907,
9.35303380178583));
#57585=CARTESIAN_POINT('Ctrl Pts',(-5.65694962445924E-5,-34.9391902220334,
9.40909973890534));
#57586=CARTESIAN_POINT('Ctrl Pts',(-0.000103461444640018,-34.72708113854,
9.46852350682398));
#57587=CARTESIAN_POINT('Ctrl Pts',(-0.000150448019398666,-34.514544026102,
9.52806718989308));
#57588=CARTESIAN_POINT('Ctrl Pts',(-0.000187656962521676,-34.2927055032922,
9.59098216616354));
#57589=CARTESIAN_POINT('Ctrl Pts',(-0.000191091383847208,-34.0615655700265,
9.6573387038564));
#57590=CARTESIAN_POINT('Ctrl Pts',(-0.000194539831505515,-33.8294816507689,
9.72396624466482));
#57591=CARTESIAN_POINT('Ctrl Pts',(-0.000163896434727065,-33.5880201911472,
9.79406343861578));
#57592=CARTESIAN_POINT('Ctrl Pts',(-0.000118572553254648,-33.337181191076,
9.86767201279748));
#57593=CARTESIAN_POINT('Ctrl Pts',(-8.37595163062467E-5,-33.1445130635043,
9.92421037468217));
#57594=CARTESIAN_POINT('Ctrl Pts',(-4.11726282365265E-5,-32.9463124721712,
9.98281974137946));
#57595=CARTESIAN_POINT('Ctrl Pts',(-1.71543475557812E-5,-32.7425794170381,
10.0435077220134));
#57596=CARTESIAN_POINT('',(-7.77156117238E-15,-32.4742356128,10.1236848855));
#57597=CARTESIAN_POINT('Ctrl Pts',(-1.71543475557812E-5,-32.7425794170381,
10.0435077220134));
#57598=CARTESIAN_POINT('Ctrl Pts',(-6.73205891155968E-6,-32.6541732261376,
10.0698421486866));
#57599=CARTESIAN_POINT('Ctrl Pts',(5.83743083992971E-14,-32.5647252913926,
10.0965678485074));
#57600=CARTESIAN_POINT('Ctrl Pts',(8.39328606616618E-14,-32.4742356128,
10.1236848854971));
#57601=CARTESIAN_POINT('',(7.20566699818,-32.4742356128,7.46610074528));
#57602=CARTESIAN_POINT('Ctrl Pts',(-7.77156117238E-15,-32.4742356128,10.1236848855));
#57603=CARTESIAN_POINT('Ctrl Pts',(0.0686255073634253,-32.4742356128,10.1230144724525));
#57604=CARTESIAN_POINT('Ctrl Pts',(0.137239296162275,-32.4742356128,10.1219531731961));
#57605=CARTESIAN_POINT('Ctrl Pts',(0.205839273380599,-32.4742356128,10.1204615805581));
#57606=CARTESIAN_POINT('Ctrl Pts',(1.77362452481901,-32.4742356128,10.0755367445611));
#57607=CARTESIAN_POINT('Ctrl Pts',(3.33152766362,-32.4742356128,9.75813869887));
#57608=CARTESIAN_POINT('Ctrl Pts',(4.75215864726,-32.4742356128,9.20958609289));
#57609=CARTESIAN_POINT('Ctrl Pts',(6.05929136989,-32.4742356128,8.43312886058));
#57610=CARTESIAN_POINT('Ctrl Pts',(7.20566699818,-32.4742356128,7.46610074528));
#57611=CARTESIAN_POINT('',(4.2854138145,-35.285453273,6.68742874721));
#57612=CARTESIAN_POINT('Ctrl Pts',(2.60523473148,-35.3742356128,8.65541043601));
#57613=CARTESIAN_POINT('Ctrl Pts',(2.76838711967,-34.7942356128,8.92400932641));
#57614=CARTESIAN_POINT('Ctrl Pts',(2.93016897988,-34.2142356128,9.19332068473));
#57615=CARTESIAN_POINT('Ctrl Pts',(3.09077135202,-33.6342356128,9.46303508034));
#57616=CARTESIAN_POINT('Ctrl Pts',(3.25037602177,-33.0542356128,9.73294848656));
#57617=CARTESIAN_POINT('Ctrl Pts',(3.40914395912,-32.4742356128,10.0029291615));
#57618=CARTESIAN_POINT('Ctrl Pts',(2.08749540657,-35.3742356128,8.79956130216));
#57619=CARTESIAN_POINT('Ctrl Pts',(2.20333316497,-34.7942356128,9.04664158555));
#57620=CARTESIAN_POINT('Ctrl Pts',(2.31825723806,-34.2142356128,9.29419684756));
#57621=CARTESIAN_POINT('Ctrl Pts',(2.43239498576,-33.6342356128,9.5420208011));
#57622=CARTESIAN_POINT('Ctrl Pts',(2.54586759853,-33.0542356128,9.78997742837));
#57623=CARTESIAN_POINT('Ctrl Pts',(2.6587823897,-32.4742356128,10.0379789015));
#57624=CARTESIAN_POINT('Ctrl Pts',(1.56975608167,-35.3742356128,8.94371216831));
#57625=CARTESIAN_POINT('Ctrl Pts',(1.63827921028,-34.7942356128,9.1692738447));
#57626=CARTESIAN_POINT('Ctrl Pts',(1.70634549623,-34.2142356128,9.39507301039));
#57627=CARTESIAN_POINT('Ctrl Pts',(1.77401861949,-33.6342356128,9.62100652185));
#57628=CARTESIAN_POINT('Ctrl Pts',(1.84135917528,-33.0542356128,9.84700637017));
#57629=CARTESIAN_POINT('Ctrl Pts',(1.90842082028,-32.4742356128,10.0730286414));
#57630=CARTESIAN_POINT('Ctrl Pts',(1.05201675677,-35.3742356128,9.08786303446));
#57631=CARTESIAN_POINT('Ctrl Pts',(1.07322525559,-34.7942356128,9.29190610384));
#57632=CARTESIAN_POINT('Ctrl Pts',(1.09443375441,-34.2142356128,9.49594917322));
#57633=CARTESIAN_POINT('Ctrl Pts',(1.11564225322,-33.6342356128,9.6999922426));
#57634=CARTESIAN_POINT('Ctrl Pts',(1.13685075204,-33.0542356128,9.90403531198));
#57635=CARTESIAN_POINT('Ctrl Pts',(1.15805925086,-32.4742356128,10.1080783814));
#57636=CARTESIAN_POINT('Ctrl Pts',(-0.511836420903,-35.3742356128,9.5232767248));
#57637=CARTESIAN_POINT('Ctrl Pts',(-0.628849173616,-34.7942356128,9.66130309814));
#57638=CARTESIAN_POINT('Ctrl Pts',(-0.745861926328,-34.2142356128,9.79932947148));
#57639=CARTESIAN_POINT('Ctrl Pts',(-0.862874679041,-33.6342356128,9.93735584482));
#57640=CARTESIAN_POINT('Ctrl Pts',(-0.979887431754,-33.0542356128,10.0753822182));
#57641=CARTESIAN_POINT('Ctrl Pts',(-1.09690018447,-32.4742356128,10.2134085915));
#57642=CARTESIAN_POINT('Ctrl Pts',(-2.16072134347,-35.3742356128,9.16274026182));
#57643=CARTESIAN_POINT('Ctrl Pts',(-2.3948826075,-34.7942356128,9.28181994923));
#57644=CARTESIAN_POINT('Ctrl Pts',(-2.62904387153,-34.2142356128,9.40089963664));
#57645=CARTESIAN_POINT('Ctrl Pts',(-2.86320513556,-33.6342356128,9.51997932405));
#57646=CARTESIAN_POINT('Ctrl Pts',(-3.09736639959,-33.0542356128,9.63905901146));
#57647=CARTESIAN_POINT('Ctrl Pts',(-3.33152766362,-32.4742356128,9.75813869887));
#57648=CARTESIAN_POINT('Ctrl Pts',(-3.13619409311,-35.3742356128,8.55164595878));
#57649=CARTESIAN_POINT('Ctrl Pts',(-3.45938700394,-34.7942356128,8.6832339856));
#57650=CARTESIAN_POINT('Ctrl Pts',(-3.78257991477,-34.2142356128,8.81482201242));
#57651=CARTESIAN_POINT('Ctrl Pts',(-4.1057728256,-33.6342356128,8.94641003924));
#57652=CARTESIAN_POINT('Ctrl Pts',(-4.42896573643,-33.0542356128,9.07799806607));
#57653=CARTESIAN_POINT('Ctrl Pts',(-4.75215864726,-32.4742356128,9.20958609289));
#57654=CARTESIAN_POINT('Ctrl Pts',(-3.83208911107,-35.3742356128,7.6674137228));
#57655=CARTESIAN_POINT('Ctrl Pts',(-4.27752956283,-34.7942356128,7.82055675035));
#57656=CARTESIAN_POINT('Ctrl Pts',(-4.7229700146,-34.2142356128,7.97369977791));
#57657=CARTESIAN_POINT('Ctrl Pts',(-5.16841046636,-33.6342356128,8.12684280547));
#57658=CARTESIAN_POINT('Ctrl Pts',(-5.61385091813,-33.0542356128,8.27998583302));
#57659=CARTESIAN_POINT('Ctrl Pts',(-6.05929136989,-32.4742356128,8.43312886058));
#57660=CARTESIAN_POINT('Ctrl Pts',(-4.19318797439,-35.3742356128,6.66283715371));
#57661=CARTESIAN_POINT('Ctrl Pts',(-4.79568377915,-34.7942356128,6.82348987203));
#57662=CARTESIAN_POINT('Ctrl Pts',(-5.3981795839,-34.2142356128,6.98414259034));
#57663=CARTESIAN_POINT('Ctrl Pts',(-6.00067538866,-33.6342356128,7.14479530865));
#57664=CARTESIAN_POINT('Ctrl Pts',(-6.60317119342,-33.0542356128,7.30544802697));
#57665=CARTESIAN_POINT('Ctrl Pts',(-7.20566699818,-32.4742356128,7.46610074528));
#57666=CARTESIAN_POINT('',(-7.20566699818,-32.4742356128,7.46610074528));
#57667=CARTESIAN_POINT('',(-4.2854138145,-35.285453273,6.68742874721));
#57668=CARTESIAN_POINT('Ctrl Pts',(2.05391259555654E-14,-32.4742356128,
10.1236848854971));
#57669=CARTESIAN_POINT('Ctrl Pts',(-0.723226925025329,-32.4742356128,10.1166195707796));
#57670=CARTESIAN_POINT('Ctrl Pts',(-2.22086602908888,-32.4742356128001,
10.0501259104731));
#57671=CARTESIAN_POINT('Ctrl Pts',(-5.15748989495571,-32.4742356128001,
8.91985491792444));
#57672=CARTESIAN_POINT('Ctrl Pts',(-6.24653783595315,-32.4742356128,8.27517662162345));
#57673=CARTESIAN_POINT('Ctrl Pts',(-7.20566699818,-32.4742356128,7.46610074528));
#57674=CARTESIAN_POINT('Ctrl Pts',(-4.19318797439,-35.3742356128,6.66283715371));
#57675=CARTESIAN_POINT('Ctrl Pts',(-7.20566699818,-32.4742356128,7.46610074528));
#57676=CARTESIAN_POINT('Ctrl Pts',(-4.25225922259,-35.3742356128,6.49850101766));
#57677=CARTESIAN_POINT('Ctrl Pts',(-7.39320029639,-32.4742356128,7.30790654658));
#57678=CARTESIAN_POINT('Ctrl Pts',(-4.30237103799,-35.3742356128,6.33094436873));
#57679=CARTESIAN_POINT('Ctrl Pts',(-7.53221837753,-32.4742356128,7.09219938589));
#57680=CARTESIAN_POINT('Ctrl Pts',(-4.34319574155,-35.3742356128,6.16124819217));
#57681=CARTESIAN_POINT('Ctrl Pts',(-7.59868325739,-32.4742356128,6.83930575178));
#57682=CARTESIAN_POINT('Ctrl Pts',(-4.37477641654,-35.3742356128,5.98923343741));
#57683=CARTESIAN_POINT('Ctrl Pts',(-7.58368665883,-32.4742356128,6.58312083129));
#57684=CARTESIAN_POINT('Ctrl Pts',(-4.3969132289,-35.3742356128,5.81601178901));
#57685=CARTESIAN_POINT('Ctrl Pts',(-7.49816640227,-32.4742356128,6.35316338263));
#57686=CARTESIAN_POINT('',(-7.49816640227,-32.4742356128,6.35316338263));
#57687=CARTESIAN_POINT('',(-4.49212120371,-35.2852060782,5.83250225674));
#57688=CARTESIAN_POINT('Origin',(-6.56088648981501,-32.4742356127961,6.70173548960406));
#57689=CARTESIAN_POINT('Ctrl Pts',(-4.3969132289,-35.3742356128,5.81601178901));
#57690=CARTESIAN_POINT('Ctrl Pts',(-7.49816640227,-32.4742356128,6.35316338263));
#57691=CARTESIAN_POINT('Ctrl Pts',(-4.48962392508,-35.3742356128,5.0905460197));
#57692=CARTESIAN_POINT('Ctrl Pts',(-7.14000207598,-32.4742356128,5.39008683572));
#57693=CARTESIAN_POINT('Ctrl Pts',(-4.41668920588,-35.3742356128,4.34391151104));
#57694=CARTESIAN_POINT('Ctrl Pts',(-6.73176998559,-32.4742356128,4.44563102148));
#57695=CARTESIAN_POINT('Ctrl Pts',(-4.17142295951,-35.3742356128,3.62676818174));
#57696=CARTESIAN_POINT('Ctrl Pts',(-6.27486238853,-32.4742356128,3.52346144896));
#57697=CARTESIAN_POINT('Ctrl Pts',(-3.771858743,-35.3742356128,2.99184297704));
#57698=CARTESIAN_POINT('Ctrl Pts',(-5.77073547798,-32.4742356128,2.62651750489));
#57699=CARTESIAN_POINT('Ctrl Pts',(-3.25430421882,-35.3742356128,2.47509045608));
#57700=CARTESIAN_POINT('Ctrl Pts',(-5.22146332445,-32.4742356128,1.7581292142));
#57701=CARTESIAN_POINT('',(-5.22146332445,-32.4742356128,1.7581292142));
#57702=CARTESIAN_POINT('',(-3.30528109741,-35.2990851344,2.45651115251));
#57703=CARTESIAN_POINT('Origin',(15.657527533216,-32.4742356128,14.9645861152497));
#57704=CARTESIAN_POINT('Ctrl Pts',(-3.25430421882,-35.3742356128,2.47509045608));
#57705=CARTESIAN_POINT('Ctrl Pts',(-5.22146332445,-32.4742356128,1.7581292142));
#57706=CARTESIAN_POINT('Ctrl Pts',(-3.2239318541,-35.3742356128,2.44476515183));
#57707=CARTESIAN_POINT('Ctrl Pts',(-5.1892302237,-32.4742356128,1.70716932646));
#57708=CARTESIAN_POINT('Ctrl Pts',(-3.19898265017,-35.3742356128,2.40900827334));
#57709=CARTESIAN_POINT('Ctrl Pts',(-5.15684165406,-32.4742356128,1.65630777433));
#57710=CARTESIAN_POINT('Ctrl Pts',(-3.18021147649,-35.3742356128,2.36763482469));
#57711=CARTESIAN_POINT('Ctrl Pts',(-5.1231181514,-32.4742356128,1.60370991526));
#57712=CARTESIAN_POINT('Ctrl Pts',(-3.16973557012,-35.3742356128,2.32531139715));
#57713=CARTESIAN_POINT('Ctrl Pts',(-5.09041537382,-32.4742356128,1.55304981975));
#57714=CARTESIAN_POINT('Ctrl Pts',(-3.16691857253,-35.3742356128,2.28248419619));
#57715=CARTESIAN_POINT('Ctrl Pts',(-5.05755834899,-32.4742356128,1.50248996551));
#57716=CARTESIAN_POINT('',(-5.05755834899,-32.4742356128,1.50248996551));
#57717=CARTESIAN_POINT('',(-3.2167330984,-35.297826491,2.26193292922));
#57718=CARTESIAN_POINT('Origin',(15.7711771435274,-32.4742356128,15.0373502450657));
#57719=CARTESIAN_POINT('Ctrl Pts',(-3.16691857253,-35.3742356128,2.28248419619));
#57720=CARTESIAN_POINT('Ctrl Pts',(-5.05755834899,-32.4742356128,1.50248996551));
#57721=CARTESIAN_POINT('Ctrl Pts',(-3.14279442744,-35.3742356128,1.91572108521));
#57722=CARTESIAN_POINT('Ctrl Pts',(-4.77617249442,-32.4742356128,1.06949799882));
#57723=CARTESIAN_POINT('Ctrl Pts',(-3.11867028235,-35.3742356128,1.54895799245));
#57724=CARTESIAN_POINT('Ctrl Pts',(-4.48347398519,-32.4742356128,0.643857892919));
#57725=CARTESIAN_POINT('Ctrl Pts',(-3.09450967796,-35.3742356128,1.18164054895));
#57726=CARTESIAN_POINT('Ctrl Pts',(-4.17925298698,-32.4742356128,0.225336592507));
#57727=CARTESIAN_POINT('Ctrl Pts',(-3.07038553283,-35.3742356128,0.814877455407));
#57728=CARTESIAN_POINT('Ctrl Pts',(-3.86470492801,-32.4742356128,-0.184421152381));
#57729=CARTESIAN_POINT('Ctrl Pts',(-3.0462613877,-35.3742356128,0.448114344193));
#57730=CARTESIAN_POINT('Ctrl Pts',(-3.53967296235,-32.4742356128,-0.585686978861));
#57731=CARTESIAN_POINT('',(-3.53967296235,-32.4742356128,-0.585686978861));
#57732=CARTESIAN_POINT('',(-3.05109044571,-35.345853084,0.437996449075));
#57733=CARTESIAN_POINT('Ctrl Pts',(-3.53967296235,-32.4742356128,-0.585686978860996));
#57734=CARTESIAN_POINT('Ctrl Pts',(-3.81069940134122,-32.4742356128,-0.251093278764725));
#57735=CARTESIAN_POINT('Ctrl Pts',(-4.07285675309246,-32.4742356128,0.0904475661883553));
#57736=CARTESIAN_POINT('Ctrl Pts',(-4.57894874401687,-32.4742356128,0.786685671920166));
#57737=CARTESIAN_POINT('Ctrl Pts',(-4.8229261644615,-32.4742356128,1.14144178423942));
#57738=CARTESIAN_POINT('Ctrl Pts',(-5.05755834899,-32.4742356128,1.50248996551));
#57739=CARTESIAN_POINT('Ctrl Pts',(-3.0462613877,-35.3742356128,0.448114344193));
#57740=CARTESIAN_POINT('Ctrl Pts',(-3.53967296235,-32.4742356128,-0.585686978861));
#57741=CARTESIAN_POINT('Ctrl Pts',(-3.04377855919,-35.3742356128,0.410367561768));
#57742=CARTESIAN_POINT('Ctrl Pts',(-3.50622171659,-32.4742356128,-0.626983968707));
#57743=CARTESIAN_POINT('Ctrl Pts',(-3.03534613584,-35.3742356128,0.373012120652));
#57744=CARTESIAN_POINT('Ctrl Pts',(-3.4726594259,-32.4742356128,-0.668191011718));
#57745=CARTESIAN_POINT('Ctrl Pts',(-3.02058192311,-35.3742356128,0.336333109732));
#57746=CARTESIAN_POINT('Ctrl Pts',(-3.4380400694,-32.4742356128,-0.710460650811));
#57747=CARTESIAN_POINT('Ctrl Pts',(-3.00078302788,-35.3742356128,0.30355295586));
#57748=CARTESIAN_POINT('Ctrl Pts',(-3.40425418736,-32.4742356128,-0.75148456633));
#57749=CARTESIAN_POINT('Ctrl Pts',(-2.97642257165,-35.3742356128,0.274612461872));
#57750=CARTESIAN_POINT('Ctrl Pts',(-3.37035823989,-32.4742356128,-0.792417339984));
#57751=CARTESIAN_POINT('',(-3.37035823989,-32.4742356128,-0.792417339984));
#57752=CARTESIAN_POINT('',(-2.98281092224,-35.3272070795,0.257308721649));
#57753=CARTESIAN_POINT('Origin',(-3.43621138602758,-32.4742356128,-0.673649465592228));
#57754=CARTESIAN_POINT('Ctrl Pts',(-2.97642257165,-35.3742356128,0.274612461872));
#57755=CARTESIAN_POINT('Ctrl Pts',(-3.37035823989,-32.4742356128,-0.792417339984));
#57756=CARTESIAN_POINT('Ctrl Pts',(-2.53990923767,-35.3742356128,-0.243970172904));
#57757=CARTESIAN_POINT('Ctrl Pts',(-2.76296793319,-32.4742356128,-1.52590236845));
#57758=CARTESIAN_POINT('Ctrl Pts',(-1.99045494271,-35.3742356128,-0.667485652616));
#57759=CARTESIAN_POINT('Ctrl Pts',(-2.12023572482,-32.4742356128,-2.23012174203));
#57760=CARTESIAN_POINT('Ctrl Pts',(-1.35568684616,-35.3742356128,-0.962884347862));
#57761=CARTESIAN_POINT('Ctrl Pts',(-1.44418220412,-32.4742356128,-2.90267037222));
#57762=CARTESIAN_POINT('Ctrl Pts',(-0.677843520645,-35.3742356128,-1.11051031269));
#57763=CARTESIAN_POINT('Ctrl Pts',(-0.736632181986,-32.4742356128,-3.54173296481));
#57764=CARTESIAN_POINT('Ctrl Pts',(-3.34917279095E-15,-35.3742356128,-1.11051031258));
#57765=CARTESIAN_POINT('Ctrl Pts',(-1.48930250848E-13,-32.4742356128,-4.14530259747));
#57766=CARTESIAN_POINT('',(-1.487698853E-13,-32.4742356128,-4.14530259747));
#57767=CARTESIAN_POINT('',(-7.77156117238E-15,-35.2855840756,-1.20328238204));
#57768=CARTESIAN_POINT('Origin',(15.6577121383952,-32.4742356128,14.9644107719153));
#57769=CARTESIAN_POINT('Ctrl Pts',(2.97642257165,-35.3742356128,0.274612461872));
#57770=CARTESIAN_POINT('Ctrl Pts',(3.37035823989,-32.4742356128,-0.792417339984));
#57771=CARTESIAN_POINT('Ctrl Pts',(2.53990923767,-35.3742356128,-0.243970172904));
#57772=CARTESIAN_POINT('Ctrl Pts',(2.76296793319,-32.4742356128,-1.52590236845));
#57773=CARTESIAN_POINT('Ctrl Pts',(1.99045494271,-35.3742356128,-0.667485652616));
#57774=CARTESIAN_POINT('Ctrl Pts',(2.12023572482,-32.4742356128,-2.23012174203));
#57775=CARTESIAN_POINT('Ctrl Pts',(1.35568684616,-35.3742356128,-0.962884347862));
#57776=CARTESIAN_POINT('Ctrl Pts',(1.44418220412,-32.4742356128,-2.90267037222));
#57777=CARTESIAN_POINT('Ctrl Pts',(0.677843520645,-35.3742356128,-1.11051031269));
#57778=CARTESIAN_POINT('Ctrl Pts',(0.736632181986,-32.4742356128,-3.54173296481));
#57779=CARTESIAN_POINT('Ctrl Pts',(1.42787016778E-15,-35.3742356128,-1.11051031258));
#57780=CARTESIAN_POINT('Ctrl Pts',(1.50638760725E-13,-32.4742356128,-4.14530259747));
#57781=CARTESIAN_POINT('',(3.37035823989,-32.4742356128,-0.792417339984));
#57782=CARTESIAN_POINT('',(2.98281092222467,-35.3272070794932,0.257308721661903));
#57783=CARTESIAN_POINT('Origin',(-15.6577121383927,-32.4742356127996,14.9644107719132));
#57784=CARTESIAN_POINT('Ctrl Pts',(3.0462613877,-35.3742356128,0.448114344193));
#57785=CARTESIAN_POINT('Ctrl Pts',(3.53967296235,-32.4742356128,-0.585686978861));
#57786=CARTESIAN_POINT('Ctrl Pts',(3.04377855919,-35.3742356128,0.410367561768));
#57787=CARTESIAN_POINT('Ctrl Pts',(3.50622171659,-32.4742356128,-0.626983968707));
#57788=CARTESIAN_POINT('Ctrl Pts',(3.03534613584,-35.3742356128,0.373012120652));
#57789=CARTESIAN_POINT('Ctrl Pts',(3.4726594259,-32.4742356128,-0.668191011718));
#57790=CARTESIAN_POINT('Ctrl Pts',(3.02058192311,-35.3742356128,0.336333109732));
#57791=CARTESIAN_POINT('Ctrl Pts',(3.4380400694,-32.4742356128,-0.710460650811));
#57792=CARTESIAN_POINT('Ctrl Pts',(3.00078302788,-35.3742356128,0.30355295586));
#57793=CARTESIAN_POINT('Ctrl Pts',(3.40425418736,-32.4742356128,-0.75148456633));
#57794=CARTESIAN_POINT('Ctrl Pts',(2.97642257165,-35.3742356128,0.274612461872));
#57795=CARTESIAN_POINT('Ctrl Pts',(3.37035823989,-32.4742356128,-0.792417339984));
#57796=CARTESIAN_POINT('',(3.53967296235,-32.4742356128,-0.585686978861));
#57797=CARTESIAN_POINT('',(3.05109044570917,-35.3458530839998,0.437996449075061));
#57798=CARTESIAN_POINT('Origin',(3.43621138602758,-32.4742356128,-0.673649465592228));
#57799=CARTESIAN_POINT('Ctrl Pts',(3.16691857253,-35.3742356128,2.28248419619));
#57800=CARTESIAN_POINT('Ctrl Pts',(5.05755834899,-32.4742356128,1.50248996551));
#57801=CARTESIAN_POINT('Ctrl Pts',(3.14279442744,-35.3742356128,1.91572108521));
#57802=CARTESIAN_POINT('Ctrl Pts',(4.77617249442,-32.4742356128,1.06949799882));
#57803=CARTESIAN_POINT('Ctrl Pts',(3.11867028235,-35.3742356128,1.54895799245));
#57804=CARTESIAN_POINT('Ctrl Pts',(4.48347398519,-32.4742356128,0.643857892919));
#57805=CARTESIAN_POINT('Ctrl Pts',(3.09450967796,-35.3742356128,1.18164054895));
#57806=CARTESIAN_POINT('Ctrl Pts',(4.17925298698,-32.4742356128,0.225336592507));
#57807=CARTESIAN_POINT('Ctrl Pts',(3.07038553283,-35.3742356128,0.814877455407));
#57808=CARTESIAN_POINT('Ctrl Pts',(3.86470492801,-32.4742356128,-0.184421152381));
#57809=CARTESIAN_POINT('Ctrl Pts',(3.0462613877,-35.3742356128,0.448114344193));
#57810=CARTESIAN_POINT('Ctrl Pts',(3.53967296235,-32.4742356128,-0.585686978861));
#57811=CARTESIAN_POINT('',(5.05755834899,-32.4742356128,1.50248996551));
#57812=CARTESIAN_POINT('',(3.21673309838426,-35.2978264909894,2.26193292922132));
#57813=CARTESIAN_POINT('Ctrl Pts',(3.53967296235,-32.4742356128,-0.585686978860997));
#57814=CARTESIAN_POINT('Ctrl Pts',(3.81069940134122,-32.4742356128,-0.251093278764735));
#57815=CARTESIAN_POINT('Ctrl Pts',(4.07285675309245,-32.4742356128,0.0904475661883362));
#57816=CARTESIAN_POINT('Ctrl Pts',(4.57894874401687,-32.4742356128,0.786685671920158));
#57817=CARTESIAN_POINT('Ctrl Pts',(4.8229261644615,-32.4742356128,1.14144178423942));
#57818=CARTESIAN_POINT('Ctrl Pts',(5.05755834899,-32.4742356128,1.50248996551));
#57819=CARTESIAN_POINT('Ctrl Pts',(3.25430421882,-35.3742356128,2.47509045608));
#57820=CARTESIAN_POINT('Ctrl Pts',(5.22146332445,-32.4742356128,1.7581292142));
#57821=CARTESIAN_POINT('Ctrl Pts',(3.2239318541,-35.3742356128,2.44476515183));
#57822=CARTESIAN_POINT('Ctrl Pts',(5.1892302237,-32.4742356128,1.70716932646));
#57823=CARTESIAN_POINT('Ctrl Pts',(3.19898265017,-35.3742356128,2.40900827334));
#57824=CARTESIAN_POINT('Ctrl Pts',(5.15684165406,-32.4742356128,1.65630777433));
#57825=CARTESIAN_POINT('Ctrl Pts',(3.18021147649,-35.3742356128,2.36763482469));
#57826=CARTESIAN_POINT('Ctrl Pts',(5.1231181514,-32.4742356128,1.60370991526));
#57827=CARTESIAN_POINT('Ctrl Pts',(3.16973557012,-35.3742356128,2.32531139715));
#57828=CARTESIAN_POINT('Ctrl Pts',(5.09041537382,-32.4742356128,1.55304981975));
#57829=CARTESIAN_POINT('Ctrl Pts',(3.16691857253,-35.3742356128,2.28248419619));
#57830=CARTESIAN_POINT('Ctrl Pts',(5.05755834899,-32.4742356128,1.50248996551));
#57831=CARTESIAN_POINT('',(5.22146332445,-32.4742356128,1.7581292142));
#57832=CARTESIAN_POINT('',(3.30528109740205,-35.2990851343927,2.45651115251783));
#57833=CARTESIAN_POINT('Origin',(-15.7711771435274,-32.4742356128,15.0373502450657));
#57834=CARTESIAN_POINT('Ctrl Pts',(4.3969132289,-35.3742356128,5.81601178901));
#57835=CARTESIAN_POINT('Ctrl Pts',(7.49816640227,-32.4742356128,6.35316338263));
#57836=CARTESIAN_POINT('Ctrl Pts',(4.48962392508,-35.3742356128,5.0905460197));
#57837=CARTESIAN_POINT('Ctrl Pts',(7.14000207598,-32.4742356128,5.39008683572));
#57838=CARTESIAN_POINT('Ctrl Pts',(4.41668920588,-35.3742356128,4.34391151104));
#57839=CARTESIAN_POINT('Ctrl Pts',(6.73176998559,-32.4742356128,4.44563102148));
#57840=CARTESIAN_POINT('Ctrl Pts',(4.17142295951,-35.3742356128,3.62676818174));
#57841=CARTESIAN_POINT('Ctrl Pts',(6.27486238853,-32.4742356128,3.52346144896));
#57842=CARTESIAN_POINT('Ctrl Pts',(3.771858743,-35.3742356128,2.99184297704));
#57843=CARTESIAN_POINT('Ctrl Pts',(5.77073547798,-32.4742356128,2.62651750489));
#57844=CARTESIAN_POINT('Ctrl Pts',(3.25430421882,-35.3742356128,2.47509045608));
#57845=CARTESIAN_POINT('Ctrl Pts',(5.22146332445,-32.4742356128,1.7581292142));
#57846=CARTESIAN_POINT('',(7.49816640227,-32.4742356128,6.35316338263));
#57847=CARTESIAN_POINT('',(4.49212120367077,-35.2852060781573,5.83250225673578));
#57848=CARTESIAN_POINT('Origin',(-15.657527533216,-32.4742356128,14.9645861152497));
#57849=CARTESIAN_POINT('Ctrl Pts',(4.19318797439,-35.3742356128,6.66283715371));
#57850=CARTESIAN_POINT('Ctrl Pts',(7.20566699818,-32.4742356128,7.46610074528));
#57851=CARTESIAN_POINT('Ctrl Pts',(4.25225922259,-35.3742356128,6.49850101766));
#57852=CARTESIAN_POINT('Ctrl Pts',(7.39320029639,-32.4742356128,7.30790654658));
#57853=CARTESIAN_POINT('Ctrl Pts',(4.30237103799,-35.3742356128,6.33094436873));
#57854=CARTESIAN_POINT('Ctrl Pts',(7.53221837753,-32.4742356128,7.09219938589));
#57855=CARTESIAN_POINT('Ctrl Pts',(4.34319574155,-35.3742356128,6.16124819217));
#57856=CARTESIAN_POINT('Ctrl Pts',(7.59868325739,-32.4742356128,6.83930575178));
#57857=CARTESIAN_POINT('Ctrl Pts',(4.37477641654,-35.3742356128,5.98923343741));
#57858=CARTESIAN_POINT('Ctrl Pts',(7.58368665883,-32.4742356128,6.58312083129));
#57859=CARTESIAN_POINT('Ctrl Pts',(4.3969132289,-35.3742356128,5.81601178901));
#57860=CARTESIAN_POINT('Ctrl Pts',(7.49816640227,-32.4742356128,6.35316338263));
#57861=CARTESIAN_POINT('Origin',(6.56088648981501,-32.4742356127961,6.70173548960406));
#57862=CARTESIAN_POINT('Origin',(-6.22337865086E-16,-32.4742356128,0.));
#57863=CARTESIAN_POINT('',(-1.27198391691,-32.4742356128,-10.1164167671));
#57864=CARTESIAN_POINT('',(1.27198391691,-32.4742356128,-10.1164167671));
#57865=CARTESIAN_POINT('Origin',(-4.01123091196E-15,-32.4742356128,-5.28091711198));
#57866=CARTESIAN_POINT('',(-10.831624024,-32.4742356128,-3.11921515388));
#57867=CARTESIAN_POINT('Origin',(2.84607155346,-32.4742356128,5.53854202767));
#57868=CARTESIAN_POINT('',(-10.32132295,-32.4742356128,5.39142026885));
#57869=CARTESIAN_POINT('Origin',(15.2935262605,-32.4742356128,-0.415072883442));
#57870=CARTESIAN_POINT('',(1.45716771982E-15,-32.4742356128,11.1232430723));
#57871=CARTESIAN_POINT('Origin',(0.0657457778947,-32.4742356128,-1.15388688513));
#57872=CARTESIAN_POINT('',(10.32132295,-32.4742356128,5.39142026885));
#57873=CARTESIAN_POINT('Origin',(-0.0657457778947,-32.4742356128,-1.15388688513));
#57874=CARTESIAN_POINT('',(10.831624024,-32.4742356128,-3.11921515388));
#57875=CARTESIAN_POINT('Origin',(-15.2935262605,-32.4742356128,-0.415072883442));
#57876=CARTESIAN_POINT('Origin',(-2.84607155346,-32.4742356128,5.53854202767));
#57877=CARTESIAN_POINT('Origin',(2.84607155346,-34.4242356128,5.53854202767));
#57878=CARTESIAN_POINT('',(-10.831624024,-32.8742356128,-3.11921515388));
#57879=CARTESIAN_POINT('',(-1.27198391691,-32.8742356128,-10.1164167671));
#57880=CARTESIAN_POINT('Origin',(2.84607155346,-32.8742356127999,5.53854202766998));
#57881=CARTESIAN_POINT('',(-10.831624024,-34.4242356128,-3.11921515388));
#57882=CARTESIAN_POINT('',(-1.27198391691,-32.6742356128,-10.1164167671));
#57883=CARTESIAN_POINT('Origin',(15.2935262605,-34.4242356128,-0.415072883442));
#57884=CARTESIAN_POINT('',(-10.32132295,-32.8742356128,5.39142026885));
#57885=CARTESIAN_POINT('',(-10.32132295,-34.4242356128,5.39142026885));
#57886=CARTESIAN_POINT('Origin',(15.2935262604996,-32.8742356127997,-0.415072883442075));
#57887=CARTESIAN_POINT('Origin',(0.0657457778947,-34.4242356128,-1.15388688513));
#57888=CARTESIAN_POINT('',(1.36002320517E-15,-32.8742356128,11.1232430723));
#57889=CARTESIAN_POINT('',(-1.1338152639E-14,-34.4242356128,11.1232430723));
#57890=CARTESIAN_POINT('Origin',(0.0657457778947039,-32.8742356128,-1.15388688512999));
#57891=CARTESIAN_POINT('Origin',(-0.0657457778947,-34.4242356128,-1.15388688513));
#57892=CARTESIAN_POINT('',(10.32132295,-32.8742356128,5.39142026885));
#57893=CARTESIAN_POINT('Origin',(-0.0657457778946926,-32.8742356128,-1.15388688513));
#57894=CARTESIAN_POINT('',(10.32132295,-34.4242356128,5.39142026885));
#57895=CARTESIAN_POINT('Origin',(-15.2935262605,-34.4242356128,-0.415072883442));
#57896=CARTESIAN_POINT('',(10.831624024,-32.8742356128,-3.11921515388));
#57897=CARTESIAN_POINT('Origin',(-15.2935262605,-32.8742356128002,-0.415072883441909));
#57898=CARTESIAN_POINT('',(10.831624024,-34.4242356128,-3.11921515388));
#57899=CARTESIAN_POINT('Origin',(-2.84607155346,-34.4242356128,5.53854202767));
#57900=CARTESIAN_POINT('',(1.27198391691,-32.8742356128,-10.1164167671));
#57901=CARTESIAN_POINT('Origin',(-2.84607155345998,-32.8742356128,5.53854202767));
#57902=CARTESIAN_POINT('',(1.27198391691,-32.6742356128,-10.1164167671));
#57903=CARTESIAN_POINT('Origin',(-4.06021678393E-15,-32.6742356128,-5.28091711198));
#57904=CARTESIAN_POINT('Origin',(3.05311331771918E-15,-32.8742356128,-5.28091711198007));
#57905=CARTESIAN_POINT('Origin',(-7.20309609018E-16,-32.8742356128,4.89858719659E-17));
#57906=CARTESIAN_POINT('',(0.,0.,0.));
#57907=CARTESIAN_POINT('Origin',(-3.35265884719E-30,-36.2742356128,3.15283103411E-22));
#57908=CARTESIAN_POINT('',(10.7486851001341,-36.2742356128,0.754201403925636));
#57909=CARTESIAN_POINT('',(1.34538289151,-36.2742356128,-9.83573536665));
#57910=CARTESIAN_POINT('Ctrl Pts',(10.7486858765334,-36.2742356128,0.754196450359814));
#57911=CARTESIAN_POINT('Ctrl Pts',(10.7489629244814,-36.2742356128,0.752428733958977));
#57912=CARTESIAN_POINT('Ctrl Pts',(10.7492374499617,-36.2742356128,0.750675177529054));
#57913=CARTESIAN_POINT('Ctrl Pts',(10.7495128278646,-36.2742356128,0.748914143783128));
#57914=CARTESIAN_POINT('Ctrl Pts',(10.7507758135579,-36.2742356128,0.74083738670444));
#57915=CARTESIAN_POINT('Ctrl Pts',(10.7520323311518,-36.2742356128,0.73275908912306));
#57916=CARTESIAN_POINT('Ctrl Pts',(10.7532823709248,-36.2742356128,0.724679179487232));
#57917=CARTESIAN_POINT('Ctrl Pts',(10.7678711925259,-36.2742356128005,0.630381091716242));
#57918=CARTESIAN_POINT('Ctrl Pts',(10.7815770251776,-36.2742356128038,0.535855381856853));
#57919=CARTESIAN_POINT('Ctrl Pts',(10.7943682424213,-36.2742356128065,0.441041993340083));
#57920=CARTESIAN_POINT('Ctrl Pts',(10.8075688570078,-36.2742356128093,0.343193995326961));
#57921=CARTESIAN_POINT('Ctrl Pts',(10.8197950578014,-36.2742356128115,0.245039728220827));
#57922=CARTESIAN_POINT('Ctrl Pts',(10.8309655494112,-36.2742356128255,0.146545962675994));
#57923=CARTESIAN_POINT('Ctrl Pts',(10.8427480065759,-36.2742356128402,0.0426563028413041));
#57924=CARTESIAN_POINT('Ctrl Pts',(10.8533556511679,-36.2742356128608,-0.0616110371222863));
#57925=CARTESIAN_POINT('Ctrl Pts',(10.8626464096652,-36.2742356129736,-0.166260199650818));
#57926=CARTESIAN_POINT('Ctrl Pts',(10.8657801493804,-36.2742356130117,-0.201557989048003));
#57927=CARTESIAN_POINT('Ctrl Pts',(10.8687637124405,-36.2742356130614,-0.236898940796127));
#57928=CARTESIAN_POINT('Ctrl Pts',(10.8715906326909,-36.274235613131,-0.272282403346824));
#57929=CARTESIAN_POINT('Ctrl Pts',(10.8812699153207,-36.2742356133694,-0.393434223744914));
#57930=CARTESIAN_POINT('Ctrl Pts',(10.8891344949282,-36.2742356141013,-0.515016935053823));
#57931=CARTESIAN_POINT('Ctrl Pts',(10.8948762742751,-36.2742356281832,-0.636806406497127));
#57932=CARTESIAN_POINT('Ctrl Pts',(10.8963186883058,-36.2742356317208,-0.66740159864657));
#57933=CARTESIAN_POINT('Ctrl Pts',(10.8976270296754,-36.2742356361001,-0.698009597208687));
#57934=CARTESIAN_POINT('Ctrl Pts',(10.8987962631872,-36.2742356414173,-0.728626390660339));
#57935=CARTESIAN_POINT('Ctrl Pts',(10.9038986843607,-36.2742356646208,-0.862235095504958));
#57936=CARTESIAN_POINT('Ctrl Pts',(10.9063461028681,-36.2742357053368,-0.99603469063249));
#57937=CARTESIAN_POINT('Ctrl Pts',(10.905701363612,-36.2742357223532,-1.12991502257281));
#57938=CARTESIAN_POINT('Ctrl Pts',(10.905610239575,-36.2742357247582,-1.14883696070543));
#57939=CARTESIAN_POINT('Ctrl Pts',(10.9054573112217,-36.274235726648,-1.167760435996));
#57940=CARTESIAN_POINT('Ctrl Pts',(10.9052413159717,-36.2742357279012,-1.18668506610303));
#57941=CARTESIAN_POINT('Ctrl Pts',(10.9036142484637,-36.2742357373409,-1.32924213971618));
#57942=CARTESIAN_POINT('Ctrl Pts',(10.8984251378642,-36.2742357268193,-1.47186368584055));
#57943=CARTESIAN_POINT('Ctrl Pts',(10.8892016012729,-36.2742357087315,-1.61424401603744));
#57944=CARTESIAN_POINT('Ctrl Pts',(10.8815756184603,-36.2742356937766,-1.73196349816884));
#57945=CARTESIAN_POINT('Ctrl Pts',(10.8711911520625,-36.2742356745366,-1.84951690288712));
#57946=CARTESIAN_POINT('Ctrl Pts',(10.8578169153327,-36.2742356586438,-1.96672376842866));
#57947=CARTESIAN_POINT('Ctrl Pts',(10.8453069774373,-36.2742356437781,-2.07635623856265));
#57948=CARTESIAN_POINT('Ctrl Pts',(10.8301806199933,-36.274235631925,-2.18568500938683));
#57949=CARTESIAN_POINT('Ctrl Pts',(10.8122909632233,-36.2742356246492,-2.29456528269846));
#57950=CARTESIAN_POINT('Ctrl Pts',(10.7957295635652,-36.2742356179135,-2.39536149943887));
#57951=CARTESIAN_POINT('Ctrl Pts',(10.7767997912498,-36.2742356149251,-2.49577308102596));
#57952=CARTESIAN_POINT('Ctrl Pts',(10.7554275183188,-36.2742356137244,-2.59569279244582));
#57953=CARTESIAN_POINT('Ctrl Pts',(10.7350120113479,-36.2742356125775,-2.69113942891732));
#57954=CARTESIAN_POINT('Ctrl Pts',(10.7123675696945,-36.2742356128,-2.78613705522593));
#57955=CARTESIAN_POINT('Ctrl Pts',(10.6874728382363,-36.2742356128,-2.88060265456909));
#57956=CARTESIAN_POINT('Ctrl Pts',(10.6628505227107,-36.2742356128,-2.97403454385301));
#57957=CARTESIAN_POINT('Ctrl Pts',(10.6360194039611,-36.2742356128,-3.06693894766016));
#57958=CARTESIAN_POINT('Ctrl Pts',(10.6069482491376,-36.2742356128,-3.15920931784575));
#57959=CARTESIAN_POINT('Ctrl Pts',(10.5762645045941,-36.2742356128,-3.2565979659714));
#57960=CARTESIAN_POINT('Ctrl Pts',(10.5430855146013,-36.2742356128,-3.35327963951917));
#57961=CARTESIAN_POINT('Ctrl Pts',(10.5074324792489,-36.2742356128003,-3.44913299552277));
#57962=CARTESIAN_POINT('Ctrl Pts',(10.4698050071003,-36.2742356128006,-3.55029463429309));
#57963=CARTESIAN_POINT('Ctrl Pts',(10.4294222890416,-36.2742356128012,-3.65053271747348));
#57964=CARTESIAN_POINT('Ctrl Pts',(10.3863673413088,-36.2742356128042,-3.74972158036864));
#57965=CARTESIAN_POINT('Ctrl Pts',(10.3433123935759,-36.2742356128072,-3.8489104432638));
#57966=CARTESIAN_POINT('Ctrl Pts',(10.2975862065294,-36.2742356128123,-3.94704921131114));
#57967=CARTESIAN_POINT('Ctrl Pts',(10.2493168210226,-36.2742356128257,-4.04404255191892));
#57968=CARTESIAN_POINT('Ctrl Pts',(10.200143434872,-36.2742356128393,-4.14285240710298));
#57969=CARTESIAN_POINT('Ctrl Pts',(10.1483512913797,-36.2742356129685,-4.24044318113654));
#57970=CARTESIAN_POINT('Ctrl Pts',(10.0940811009206,-36.2742356129563,-4.33679486057107));
#57971=CARTESIAN_POINT('Ctrl Pts',(10.0860953319727,-36.2742356129545,-4.35097285116214));
#57972=CARTESIAN_POINT('Ctrl Pts',(10.078055934547,-36.2742356129488,-4.36512410006593));
#57973=CARTESIAN_POINT('Ctrl Pts',(10.069963381529,-36.2742356129389,-4.37924863866557));
#57974=CARTESIAN_POINT('Ctrl Pts',(10.0206103075602,-36.274235612879,-4.46538825328766));
#57975=CARTESIAN_POINT('Ctrl Pts',(9.96927479557785,-36.2742356128063,-4.55054423432799));
#57976=CARTESIAN_POINT('Ctrl Pts',(9.91611980874301,-36.2742356128011,-4.63468661170844));
#57977=CARTESIAN_POINT('Ctrl Pts',(9.90132634625179,-36.2742356127997,-4.65810411546152));
#57978=CARTESIAN_POINT('Ctrl Pts',(9.88639201933375,-36.2742356128,-4.681443411214));
#57979=CARTESIAN_POINT('Ctrl Pts',(9.87132045450753,-36.2742356128,-4.70470457439913));
#57980=CARTESIAN_POINT('Ctrl Pts',(9.81905209423248,-36.2742356128,-4.7853745560365));
#57981=CARTESIAN_POINT('Ctrl Pts',(9.76511812234536,-36.2742356128,-4.86512219137804));
#57982=CARTESIAN_POINT('Ctrl Pts',(9.70971375293503,-36.2742356128,-4.94390068743296));
#57983=CARTESIAN_POINT('Ctrl Pts',(9.65177867900376,-36.2742356128,-5.02627754762849));
#57984=CARTESIAN_POINT('Ctrl Pts',(9.59223559676037,-36.2742356128,-5.1075953157557));
#57985=CARTESIAN_POINT('Ctrl Pts',(9.53126893611934,-36.2742356128,-5.18784861358279));
#57986=CARTESIAN_POINT('Ctrl Pts',(9.47173298842051,-36.2742356128,-5.26621859632177));
#57987=CARTESIAN_POINT('Ctrl Pts',(9.41083594231989,-36.2742356128,-5.34357802755611));
#57988=CARTESIAN_POINT('Ctrl Pts',(9.34873429723885,-36.2742356128,-5.41993655239066));
#57989=CARTESIAN_POINT('Ctrl Pts',(9.26848598527828,-36.2742356128,-5.51860773435008));
#57990=CARTESIAN_POINT('Ctrl Pts',(9.18622336300651,-36.2742356128,-5.61561399252855));
#57991=CARTESIAN_POINT('Ctrl Pts',(9.10218677827788,-36.2742356128,-5.71107162296444));
#57992=CARTESIAN_POINT('Ctrl Pts',(9.03699830774157,-36.2742356128,-5.78511957421366));
#57993=CARTESIAN_POINT('Ctrl Pts',(8.97073968508115,-36.2742356128,-5.85823828748615));
#57994=CARTESIAN_POINT('Ctrl Pts',(8.90351033446202,-36.2742356128,-5.93047839850826));
#57995=CARTESIAN_POINT('Ctrl Pts',(8.81845068839717,-36.2742356128,-6.02187773850837));
#57996=CARTESIAN_POINT('Ctrl Pts',(8.73184574609042,-36.2742356128,-6.11186368999363));
#57997=CARTESIAN_POINT('Ctrl Pts',(8.64390118549355,-36.2742356128,-6.20048968024117));
#57998=CARTESIAN_POINT('Ctrl Pts',(8.56984778372845,-36.2742356128,-6.2751168773991));
#57999=CARTESIAN_POINT('Ctrl Pts',(8.49484383511191,-36.2742356128,-6.34878012596499));
#58000=CARTESIAN_POINT('Ctrl Pts',(8.41901681523273,-36.2742356128,-6.42146890548941));
#58001=CARTESIAN_POINT('Ctrl Pts',(8.4047929558046,-36.2742356128,-6.43510408439536));
#58002=CARTESIAN_POINT('Ctrl Pts',(8.39054016429969,-36.2742356128,-6.4487048304708));
#58003=CARTESIAN_POINT('Ctrl Pts',(8.37625932979208,-36.2742356128,-6.46227086223795));
#58004=CARTESIAN_POINT('Ctrl Pts',(8.27691241049981,-36.2742356128,-6.55664514144192));
#58005=CARTESIAN_POINT('Ctrl Pts',(8.17619343587986,-36.2742356127799,-6.64936525637284));
#58006=CARTESIAN_POINT('Ctrl Pts',(8.07431943600004,-36.2742356130106,-6.74042458337472));
#58007=CARTESIAN_POINT('Ctrl Pts',(7.9740368388946,-36.2742356132376,-6.83006144668816));
#58008=CARTESIAN_POINT('Ctrl Pts',(7.8726372330311,-36.2742356137614,-6.91808713967223));
#58009=CARTESIAN_POINT('Ctrl Pts',(7.77030787671347,-36.2742356141754,-7.00445497976472));
#58010=CARTESIAN_POINT('Ctrl Pts',(7.69016343904083,-36.2742356144997,-7.07209834454587));
#58011=CARTESIAN_POINT('Ctrl Pts',(7.60944864485436,-36.2742356146977,-7.13872371640073));
#58012=CARTESIAN_POINT('Ctrl Pts',(7.52823172485476,-36.2742356144998,-7.20430188678942));
#58013=CARTESIAN_POINT('Ctrl Pts',(7.44113992314812,-36.2742356142876,-7.27462369918769));
#58014=CARTESIAN_POINT('Ctrl Pts',(7.35346425048188,-36.2742356138161,-7.34374843931962));
#58015=CARTESIAN_POINT('Ctrl Pts',(7.26526468412603,-36.2742356134793,-7.41163792641398));
#58016=CARTESIAN_POINT('Ctrl Pts',(7.20648357004512,-36.2742356132547,-7.45688327002131));
#58017=CARTESIAN_POINT('Ctrl Pts',(7.1474689412501,-36.274235613086,-7.50158006695547));
#58018=CARTESIAN_POINT('Ctrl Pts',(7.08822590343499,-36.2742356129864,-7.545720515055));
#58019=CARTESIAN_POINT('Ctrl Pts',(7.00824771615769,-36.2742356128519,-7.60531018423479));
#58020=CARTESIAN_POINT('Ctrl Pts',(6.92783272624198,-36.2742356128213,-7.66390180221629));
#58021=CARTESIAN_POINT('Ctrl Pts',(6.84694168646384,-36.2742356128083,-7.72149588608444));
#58022=CARTESIAN_POINT('Ctrl Pts',(6.77800623059529,-36.2742356127972,-7.77057764393639));
#58023=CARTESIAN_POINT('Ctrl Pts',(6.70872455283564,-36.2742356128,-7.8189350194394));
#58024=CARTESIAN_POINT('Ctrl Pts',(6.63904441016083,-36.2742356128,-7.86657935124075));
#58025=CARTESIAN_POINT('Ctrl Pts',(6.51500653126901,-36.2742356128,-7.95139120194889));
#58026=CARTESIAN_POINT('Ctrl Pts',(6.38973081761568,-36.2742356128,-8.03391823531077));
#58027=CARTESIAN_POINT('Ctrl Pts',(6.26311690885472,-36.2742356128,-8.11405915608162));
#58028=CARTESIAN_POINT('Ctrl Pts',(6.14082382425489,-36.2742356128,-8.19146518911263));
#58029=CARTESIAN_POINT('Ctrl Pts',(6.01728298717408,-36.2742356128,-8.26664531147886));
#58030=CARTESIAN_POINT('Ctrl Pts',(5.8924473777231,-36.2742356128,-8.33951374852886));
#58031=CARTESIAN_POINT('Ctrl Pts',(5.80107807308279,-36.2742356128,-8.39284739629784));
#58032=CARTESIAN_POINT('Ctrl Pts',(5.7090133522859,-36.2742356128,-8.4449442395566));
#58033=CARTESIAN_POINT('Ctrl Pts',(5.6162580577169,-36.2742356128,-8.4957663466978));
#58034=CARTESIAN_POINT('Ctrl Pts',(5.46867697199189,-36.2742356128,-8.57662838034864));
#58035=CARTESIAN_POINT('Ctrl Pts',(5.319347849749,-36.2742356128,-8.65426137281124));
#58036=CARTESIAN_POINT('Ctrl Pts',(5.16833129815377,-36.2742356128,-8.72852821430025));
#58037=CARTESIAN_POINT('Ctrl Pts',(5.0252243894345,-36.2742356128,-8.79890525571437));
#58038=CARTESIAN_POINT('Ctrl Pts',(4.88060325867337,-36.2742356128,-8.86625971607705));
#58039=CARTESIAN_POINT('Ctrl Pts',(4.73456180799277,-36.2742356128,-8.9304829996254));
#58040=CARTESIAN_POINT('Ctrl Pts',(4.56802863892683,-36.2742356128,-9.00371773460841));
#58041=CARTESIAN_POINT('Ctrl Pts',(4.39963331229614,-36.2742356128,-9.07288577272594));
#58042=CARTESIAN_POINT('Ctrl Pts',(4.22952064919205,-36.2742356128,-9.13789430463033));
#58043=CARTESIAN_POINT('Ctrl Pts',(4.07030290524576,-36.2742356128,-9.19873934460684));
#58044=CARTESIAN_POINT('Ctrl Pts',(3.90958104396924,-36.2742356128,-9.2559399870542));
#58045=CARTESIAN_POINT('Ctrl Pts',(3.74749475790497,-36.2742356128,-9.30946145440929));
#58046=CARTESIAN_POINT('Ctrl Pts',(3.73640355073492,-36.2742356128,-9.3131238104105));
#58047=CARTESIAN_POINT('Ctrl Pts',(3.72530596253903,-36.2742356128,-9.31676895825965));
#58048=CARTESIAN_POINT('Ctrl Pts',(3.71420204145765,-36.2742356128,-9.32039689553507));
#58049=CARTESIAN_POINT('Ctrl Pts',(3.64269698207382,-36.2742356128,-9.34375944183012));
#58050=CARTESIAN_POINT('Ctrl Pts',(3.57093421782095,-36.2742356128,-9.366407200153));
#58051=CARTESIAN_POINT('Ctrl Pts',(3.49894135622052,-36.2742356128,-9.38833730031651));
#58052=CARTESIAN_POINT('Ctrl Pts',(3.36037902120776,-36.2742356128,-9.43054545565535));
#58053=CARTESIAN_POINT('Ctrl Pts',(3.2209545156788,-36.2742356128,-9.47009577861699));
#58054=CARTESIAN_POINT('Ctrl Pts',(3.08060901729276,-36.2742356128,-9.50703410737918));
#58055=CARTESIAN_POINT('Ctrl Pts',(3.01043626809975,-36.2742356128,-9.52550327176028));
#58056=CARTESIAN_POINT('Ctrl Pts',(2.94003215345144,-36.2742356128,-9.54331999022258));
#58057=CARTESIAN_POINT('Ctrl Pts',(2.86942630620849,-36.2742356128,-9.56048475195216));
#58058=CARTESIAN_POINT('Ctrl Pts',(2.80680351316639,-36.2742356128,-9.57570877890434));
#58059=CARTESIAN_POINT('Ctrl Pts',(2.74402151902805,-36.2742356128,-9.59042005980405));
#58060=CARTESIAN_POINT('Ctrl Pts',(2.68114420127632,-36.2742356128,-9.60461135390141));
#58061=CARTESIAN_POINT('Ctrl Pts',(2.67312870066971,-36.2742356128,-9.60642043753464));
#58062=CARTESIAN_POINT('Ctrl Pts',(2.66511172001634,-36.2742356128,-9.60822105857561));
#58063=CARTESIAN_POINT('Ctrl Pts',(2.65709345518398,-36.2742356128,-9.61001319054557));
#58064=CARTESIAN_POINT('Ctrl Pts',(2.61808941652459,-36.2742356128,-9.61873083533534));
#58065=CARTESIAN_POINT('Ctrl Pts',(2.5790435824319,-36.2742356128,-9.62725011661459));
#58066=CARTESIAN_POINT('Ctrl Pts',(2.53993928470411,-36.2742356128,-9.63557594572615));
#58067=CARTESIAN_POINT('Ctrl Pts',(2.49942937662269,-36.2742356128,-9.64420104812176));
#58068=CARTESIAN_POINT('Ctrl Pts',(2.45885925103264,-36.2742356128,-9.65261800011732));
#58069=CARTESIAN_POINT('Ctrl Pts',(2.41824922175855,-36.2742356128,-9.66082393256145));
#58070=CARTESIAN_POINT('Ctrl Pts',(2.37659230003858,-36.2742356128,-9.66924140705173));
#58071=CARTESIAN_POINT('Ctrl Pts',(2.33480257980723,-36.2742356128,-9.67745500886163));
#58072=CARTESIAN_POINT('Ctrl Pts',(2.29293606002991,-36.2742356128,-9.68545254735298));
#58073=CARTESIAN_POINT('Ctrl Pts',(2.25459003428932,-36.2742356128,-9.69277758460188));
#58074=CARTESIAN_POINT('Ctrl Pts',(2.21618141740729,-36.2742356128,-9.69992099315214));
#58075=CARTESIAN_POINT('Ctrl Pts',(2.17771533929591,-36.2742356128,-9.7068828050064));
#58076=CARTESIAN_POINT('Ctrl Pts',(2.14430668976644,-36.2742356128,-9.71292929437441));
#58077=CARTESIAN_POINT('Ctrl Pts',(2.11089595707496,-36.2742356128,-9.71883173440012));
#58078=CARTESIAN_POINT('Ctrl Pts',(2.07730895436942,-36.2742356128,-9.72462310550832));
#58079=CARTESIAN_POINT('Ctrl Pts',(2.07044188243394,-36.2742356128,-9.7258071874091));
#58080=CARTESIAN_POINT('Ctrl Pts',(2.06356727156797,-36.2742356128,-9.72698664924094));
#58081=CARTESIAN_POINT('Ctrl Pts',(2.05668335047021,-36.2742356128,-9.72816181233373));
#58082=CARTESIAN_POINT('Ctrl Pts',(2.03915739474699,-36.2742356128,-9.73115369095048));
#58083=CARTESIAN_POINT('Ctrl Pts',(2.02157756711238,-36.2742356127996,-9.73411696258259));
#58084=CARTESIAN_POINT('Ctrl Pts',(2.00384190141366,-36.2742356128022,-9.7370687432509));
#58085=CARTESIAN_POINT('Ctrl Pts',(1.98521996349978,-36.2742356128049,-9.74016802789431));
#58086=CARTESIAN_POINT('Ctrl Pts',(1.9664264382516,-36.2742356128118,-9.74325461496629));
#58087=CARTESIAN_POINT('Ctrl Pts',(1.94740019190711,-36.2742356128226,-9.74634003414102));
#58088=CARTESIAN_POINT('Ctrl Pts',(1.94261758327247,-36.2742356128253,-9.74711561289257));
#58089=CARTESIAN_POINT('Ctrl Pts',(1.93782052766086,-36.2742356128282,-9.74789108023816));
#58090=CARTESIAN_POINT('Ctrl Pts',(1.93300854997167,-36.2742356128312,-9.74866654690155));
#58091=CARTESIAN_POINT('Ctrl Pts',(1.91128349112384,-36.2742356128447,-9.75216761444278));
#58092=CARTESIAN_POINT('Ctrl Pts',(1.88923535030687,-36.2742356128578,-9.75567154153552));
#58093=CARTESIAN_POINT('Ctrl Pts',(1.86684962573881,-36.2742356128663,-9.75918465724687));
#58094=CARTESIAN_POINT('Ctrl Pts',(1.84177859870743,-36.2742356128757,-9.76311919234293));
#58095=CARTESIAN_POINT('Ctrl Pts',(1.81628495192361,-36.2742356128796,-9.76706514100968));
#58096=CARTESIAN_POINT('Ctrl Pts',(1.79042259448784,-36.2742356128782,-9.77102027035687));
#58097=CARTESIAN_POINT('Ctrl Pts',(1.75485788918616,-36.2742356128763,-9.77645917939724));
#58098=CARTESIAN_POINT('Ctrl Pts',(1.71859866610285,-36.2742356128649,-9.78191510402332));
#58099=CARTESIAN_POINT('Ctrl Pts',(1.68190111891461,-36.2742356128521,-9.78736428204235));
#58100=CARTESIAN_POINT('Ctrl Pts',(1.65417492786119,-36.2742356128425,-9.79148131335413));
#58101=CARTESIAN_POINT('Ctrl Pts',(1.62620285863509,-36.2742356128323,-9.79559383857571));
#58102=CARTESIAN_POINT('Ctrl Pts',(1.59808657345918,-36.2742356128241,-9.79969240046506));
#58103=CARTESIAN_POINT('Ctrl Pts',(1.57334962904916,-36.2742356128169,-9.80329834972128));
#58104=CARTESIAN_POINT('Ctrl Pts',(1.5485022020045,-36.2742356128113,-9.80689331747091));
#58105=CARTESIAN_POINT('Ctrl Pts',(1.5235774246962,-36.2742356128076,-9.81047583278086));
#58106=CARTESIAN_POINT('Ctrl Pts',(1.50128004231585,-36.2742356128042,-9.8136807044939));
#58107=CARTESIAN_POINT('Ctrl Pts',(1.4789210815784,-36.2742356128023,-9.81687556029816));
#58108=CARTESIAN_POINT('Ctrl Pts',(1.45648473849049,-36.2742356128013,-9.82006491224659));
#58109=CARTESIAN_POINT('Ctrl Pts',(1.43437802239104,-36.2742356128003,-9.82320740733988));
#58110=CARTESIAN_POINT('Ctrl Pts',(1.41219693864792,-36.2742356128001,-9.82634444875315));
#58111=CARTESIAN_POINT('Ctrl Pts',(1.38987732415055,-36.2742356128,-9.82948731744555));
#58112=CARTESIAN_POINT('Ctrl Pts',(1.37512031792225,-36.2742356128,-9.8315652804352));
#58113=CARTESIAN_POINT('Ctrl Pts',(1.36029433326,-36.2742356128,-9.83364697235));
#58114=CARTESIAN_POINT('Ctrl Pts',(1.34538289151,-36.2742356128,-9.83573536665));
#58115=CARTESIAN_POINT('',(-1.34538336432,-36.2742356128,-9.83573530247));
#58116=CARTESIAN_POINT('Origin',(-0.000204993183026136,-36.2742356127865,
-2.71388259243404));
#58117=CARTESIAN_POINT('',(-10.7486857267508,-36.2742356128,0.754197292576714));
#58118=CARTESIAN_POINT('Ctrl Pts',(-1.34538336432,-36.2742356128,-9.83573530247));
#58119=CARTESIAN_POINT('Ctrl Pts',(-1.36873192615361,-36.2742356128,-9.83246526657691));
#58120=CARTESIAN_POINT('Ctrl Pts',(-1.39186001383178,-36.2742356128,-9.82921313015801));
#58121=CARTESIAN_POINT('Ctrl Pts',(-1.41485686696532,-36.2742356128,-9.82596411801518));
#58122=CARTESIAN_POINT('Ctrl Pts',(-1.43950188342316,-36.2742356128,-9.82248225215873));
#58123=CARTESIAN_POINT('Ctrl Pts',(-1.46399603833782,-36.2742356128,-9.81900399480443));
#58124=CARTESIAN_POINT('Ctrl Pts',(-1.48838901468098,-36.2742356128,-9.81551943919389));
#58125=CARTESIAN_POINT('Ctrl Pts',(-1.51553080490511,-36.2742356128,-9.81164221338614));
#58126=CARTESIAN_POINT('Ctrl Pts',(-1.54254718023759,-36.2742356128,-9.80775721188026));
#58127=CARTESIAN_POINT('Ctrl Pts',(-1.56943612727103,-36.2742356128,-9.803860463866));
#58128=CARTESIAN_POINT('Ctrl Pts',(-1.59559432632052,-36.2742356128,-9.80006961589876));
#58129=CARTESIAN_POINT('Ctrl Pts',(-1.62163027431294,-36.2742356128,-9.79626788013378));
#58130=CARTESIAN_POINT('Ctrl Pts',(-1.64749532464658,-36.2742356128,-9.79245800174802));
#58131=CARTESIAN_POINT('Ctrl Pts',(-1.68855743602486,-36.2742356128,-9.78640962184556));
#58132=CARTESIAN_POINT('Ctrl Pts',(-1.72915458194226,-36.2742356128,-9.78034584082381));
#58133=CARTESIAN_POINT('Ctrl Pts',(-1.76902422177875,-36.2742356128,-9.77428634403978));
#58134=CARTESIAN_POINT('Ctrl Pts',(-1.79804062664776,-36.2742356128,-9.76987635155655));
#58135=CARTESIAN_POINT('Ctrl Pts',(-1.82666762765698,-36.2742356128,-9.76546917205919));
#58136=CARTESIAN_POINT('Ctrl Pts',(-1.85481242636501,-36.2742356128,-9.76107078246235));
#58137=CARTESIAN_POINT('Ctrl Pts',(-1.88089833376722,-36.2742356128,-9.75699415057977));
#58138=CARTESIAN_POINT('Ctrl Pts',(-1.90656839898667,-36.2742356128,-9.75292529183231));
#58139=CARTESIAN_POINT('Ctrl Pts',(-1.93178873575894,-36.2742356128,-9.74886307273241));
#58140=CARTESIAN_POINT('Ctrl Pts',(-1.95424178948369,-36.2742356128,-9.74524657765879));
#58141=CARTESIAN_POINT('Ctrl Pts',(-1.97632472956562,-36.2742356128,-9.74163749451863));
#58142=CARTESIAN_POINT('Ctrl Pts',(-1.99819673805766,-36.2742356128,-9.73800714264926));
#58143=CARTESIAN_POINT('Ctrl Pts',(-2.02006874654969,-36.2742356128,-9.7343767907799));
#58144=CARTESIAN_POINT('Ctrl Pts',(-2.04172901427369,-36.2742356128,-9.73072531915584));
#58145=CARTESIAN_POINT('Ctrl Pts',(-2.06328081535604,-36.2742356128,-9.72703421190412));
#58146=CARTESIAN_POINT('Ctrl Pts',(-2.08754806620901,-36.2742356128,-9.72287803835462));
#58147=CARTESIAN_POINT('Ctrl Pts',(-2.11170713674881,-36.2742356128,-9.71866665247062));
#58148=CARTESIAN_POINT('Ctrl Pts',(-2.13583519969934,-36.2742356128,-9.71438572233037));
#58149=CARTESIAN_POINT('Ctrl Pts',(-2.1545635127234,-36.2742356128,-9.71106284473903));
#58150=CARTESIAN_POINT('Ctrl Pts',(-2.17327157628719,-36.2742356128,-9.70769835376932));
#58151=CARTESIAN_POINT('Ctrl Pts',(-2.19197454480384,-36.2742356128,-9.70428935658671));
#58152=CARTESIAN_POINT('Ctrl Pts',(-2.22291726659735,-36.2742356128,-9.69864941492063));
#58153=CARTESIAN_POINT('Ctrl Pts',(-2.25381741316753,-36.2742356128,-9.69289305897368));
#58154=CARTESIAN_POINT('Ctrl Pts',(-2.2846783512042,-36.2742356128,-9.6870198736353));
#58155=CARTESIAN_POINT('Ctrl Pts',(-2.3163344605537,-36.2742356128,-9.68099535820805));
#58156=CARTESIAN_POINT('Ctrl Pts',(-2.34794406706507,-36.2742356128,-9.67484888353989));
#58157=CARTESIAN_POINT('Ctrl Pts',(-2.37949158813658,-36.2742356128,-9.66858317796076));
#58158=CARTESIAN_POINT('Ctrl Pts',(-2.40226571075079,-36.2742356128,-9.66405997162704));
#58159=CARTESIAN_POINT('Ctrl Pts',(-2.42500680916096,-36.2742356128,-9.65947474510775));
#58160=CARTESIAN_POINT('Ctrl Pts',(-2.44772709714164,-36.2742356128,-9.65482507592072));
#58161=CARTESIAN_POINT('Ctrl Pts',(-2.56023068653774,-36.2742356128,-9.63180140326789));
#58162=CARTESIAN_POINT('Ctrl Pts',(-2.67239663947122,-36.2742356128,-9.60716179468203));
#58163=CARTESIAN_POINT('Ctrl Pts',(-2.78410583615521,-36.2742356128,-9.58089117609618));
#58164=CARTESIAN_POINT('Ctrl Pts',(-2.91213087583812,-36.2742356128,-9.5507835655611));
#58165=CARTESIAN_POINT('Ctrl Pts',(-3.03955637547996,-36.2742356128,-9.51853361892697));
#58166=CARTESIAN_POINT('Ctrl Pts',(-3.16627236350259,-36.2742356128,-9.48412781383033));
#58167=CARTESIAN_POINT('Ctrl Pts',(-3.33084393041467,-36.2742356128,-9.43944349779427));
#58168=CARTESIAN_POINT('Ctrl Pts',(-3.49422083013493,-36.2742356128,-9.39112237778561));
#58169=CARTESIAN_POINT('Ctrl Pts',(-3.65625877301338,-36.2742356128,-9.3391546000114));
#58170=CARTESIAN_POINT('Ctrl Pts',(-3.72138584122313,-36.2742356128,-9.31826746118647));
#58171=CARTESIAN_POINT('Ctrl Pts',(-3.78629724319742,-36.2742356128,-9.29679144790176));
#58172=CARTESIAN_POINT('Ctrl Pts',(-3.85098428965109,-36.2742356128,-9.27472670369536));
#58173=CARTESIAN_POINT('Ctrl Pts',(-3.9588347526871,-36.2742356128,-9.23793892298973));
#58174=CARTESIAN_POINT('Ctrl Pts',(-4.06606530659819,-36.2742356128,-9.19951199868619));
#58175=CARTESIAN_POINT('Ctrl Pts',(-4.17264953538524,-36.2742356128,-9.15944992060988));
#58176=CARTESIAN_POINT('Ctrl Pts',(-4.31330125818643,-36.2742356128,-9.10658280917554));
#58177=CARTESIAN_POINT('Ctrl Pts',(-4.45282276293723,-36.2742356128,-9.05086944491036));
#58178=CARTESIAN_POINT('Ctrl Pts',(-4.59109734883041,-36.2742356128,-8.99237091677724));
#58179=CARTESIAN_POINT('Ctrl Pts',(-4.68122888517629,-36.2742356128,-8.95423981567466));
#58180=CARTESIAN_POINT('Ctrl Pts',(-4.77082945282832,-36.2742356128,-8.91492649134275));
#58181=CARTESIAN_POINT('Ctrl Pts',(-4.85988107462091,-36.2742356128,-8.87444749687177));
#58182=CARTESIAN_POINT('Ctrl Pts',(-5.02447950840956,-36.2742356128,-8.79962820714811));
#58183=CARTESIAN_POINT('Ctrl Pts',(-5.1872188048343,-36.2742356128,-8.72081653937812));
#58184=CARTESIAN_POINT('Ctrl Pts',(-5.34797972852781,-36.2742356128,-8.63818055603731));
#58185=CARTESIAN_POINT('Ctrl Pts',(-5.48874063022716,-36.2742356128,-8.56582518969192));
#58186=CARTESIAN_POINT('Ctrl Pts',(-5.62798392544602,-36.2742356128,-8.49053890087286));
#58187=CARTESIAN_POINT('Ctrl Pts',(-5.76567045786445,-36.2742356128,-8.41244582504101));
#58188=CARTESIAN_POINT('Ctrl Pts',(-5.78523365789672,-36.2742356128,-8.40134996521508));
#58189=CARTESIAN_POINT('Ctrl Pts',(-5.80476551601904,-36.2742356128,-8.39019744922167));
#58190=CARTESIAN_POINT('Ctrl Pts',(-5.82426601120212,-36.2742356128,-8.37898863848497));
#58191=CARTESIAN_POINT('Ctrl Pts',(-5.94879618143595,-36.2742356128,-8.30740916852515));
#58192=CARTESIAN_POINT('Ctrl Pts',(-6.0720464167817,-36.2742356128013,-8.23353358940084));
#58193=CARTESIAN_POINT('Ctrl Pts',(-6.19404162526371,-36.2742356128036,
-8.15745074881589));
#58194=CARTESIAN_POINT('Ctrl Pts',(-6.22651395401904,-36.2742356128042,
-8.13719924022915));
#58195=CARTESIAN_POINT('Ctrl Pts',(-6.25889764340576,-36.2742356128047,
-8.11679132494019));
#58196=CARTESIAN_POINT('Ctrl Pts',(-6.29119380735,-36.2742356128048,-8.0962286165475));
#58197=CARTESIAN_POINT('Ctrl Pts',(-6.40358306597281,-36.2742356128052,
-8.02467127755451));
#58198=CARTESIAN_POINT('Ctrl Pts',(-6.51492060843053,-36.2742356128007,
-7.95123207123157));
#58199=CARTESIAN_POINT('Ctrl Pts',(-6.62528347199178,-36.2742356128002,
-7.87597629186123));
#58200=CARTESIAN_POINT('Ctrl Pts',(-6.66578018426995,-36.2742356128,-7.84836182494647));
#58201=CARTESIAN_POINT('Ctrl Pts',(-6.70614614403169,-36.2742356128,-7.82050268772187));
#58202=CARTESIAN_POINT('Ctrl Pts',(-6.74638693431083,-36.2742356128,-7.7924018035638));
#58203=CARTESIAN_POINT('Ctrl Pts',(-6.83209224893783,-36.2742356128,-7.73255220564692));
#58204=CARTESIAN_POINT('Ctrl Pts',(-6.91722166165999,-36.2742356127998,
-7.67161278498377));
#58205=CARTESIAN_POINT('Ctrl Pts',(-7.00186018562873,-36.2742356128002,
-7.60955849043406));
#58206=CARTESIAN_POINT('Ctrl Pts',(-7.06526117816682,-36.2742356128005,
-7.56307488366468));
#58207=CARTESIAN_POINT('Ctrl Pts',(-7.12838556141735,-36.2742356128008,
-7.51596612269866));
#58208=CARTESIAN_POINT('Ctrl Pts',(-7.19125084904421,-36.2742356128052,
-7.46822717531959));
#58209=CARTESIAN_POINT('Ctrl Pts',(-7.28093214970969,-36.2742356128117,
-7.40012455374617));
#58210=CARTESIAN_POINT('Ctrl Pts',(-7.37008459041437,-36.2742356128522,
-7.33074518643801));
#58211=CARTESIAN_POINT('Ctrl Pts',(-7.45866128730512,-36.2742356130763,
-7.26012267330857));
#58212=CARTESIAN_POINT('Ctrl Pts',(-7.51506525656589,-36.2742356132191,
-7.21515158949649));
#58213=CARTESIAN_POINT('Ctrl Pts',(-7.57123465324818,-36.2742356134335,
-7.16967680621853));
#58214=CARTESIAN_POINT('Ctrl Pts',(-7.62714692446239,-36.2742356136452,
-7.1237099999356));
#58215=CARTESIAN_POINT('Ctrl Pts',(-7.72186099987924,-36.2742356140038,
-7.04584330873512));
#58216=CARTESIAN_POINT('Ctrl Pts',(-7.81583817186816,-36.2742356139541,
-6.9665618692806));
#58217=CARTESIAN_POINT('Ctrl Pts',(-7.90897295499202,-36.2742356137047,
-6.88589608108511));
#58218=CARTESIAN_POINT('Ctrl Pts',(-8.00830703058412,-36.2742356134387,
-6.79986096902981));
#58219=CARTESIAN_POINT('Ctrl Pts',(-8.1066825535539,-36.2742356130684,-6.71225191373121));
#58220=CARTESIAN_POINT('Ctrl Pts',(-8.20390980861941,-36.2742356129219,
-6.6231017683274));
#58221=CARTESIAN_POINT('Ctrl Pts',(-8.29323343819682,-36.2742356127874,
-6.54119865834599));
#58222=CARTESIAN_POINT('Ctrl Pts',(-8.3815866134665,-36.2742356128,-6.45799529379827));
#58223=CARTESIAN_POINT('Ctrl Pts',(-8.46878561291554,-36.2742356128,-6.37350477083193));
#58224=CARTESIAN_POINT('Ctrl Pts',(-8.54861727170136,-36.2742356128,-6.29615275254384));
#58225=CARTESIAN_POINT('Ctrl Pts',(-8.62746167428925,-36.2742356128,-6.21773879006739));
#58226=CARTESIAN_POINT('Ctrl Pts',(-8.70522553838402,-36.2742356128,-6.13822690867235));
#58227=CARTESIAN_POINT('Ctrl Pts',(-8.78679099037235,-36.2742356128,-6.05482798527877));
#58228=CARTESIAN_POINT('Ctrl Pts',(-8.86716721026386,-36.2742356128,-5.97022079146199));
#58229=CARTESIAN_POINT('Ctrl Pts',(-8.94618759528663,-36.2742356128,-5.88435809015603));
#58230=CARTESIAN_POINT('Ctrl Pts',(-9.03255992341744,-36.2742356128,-5.79050684646417));
#58231=CARTESIAN_POINT('Ctrl Pts',(-9.11731190902216,-36.2742356128,-5.69515496172929));
#58232=CARTESIAN_POINT('Ctrl Pts',(-9.20016409670066,-36.2742356128,-5.59824222254515));
#58233=CARTESIAN_POINT('Ctrl Pts',(-9.21466058872522,-36.2742356128,-5.58128558217118));
#58234=CARTESIAN_POINT('Ctrl Pts',(-9.2290987929291,-36.2742356128,-5.56428117657646));
#58235=CARTESIAN_POINT('Ctrl Pts',(-9.24347706216678,-36.2742356128,-5.54722871240165));
#58236=CARTESIAN_POINT('Ctrl Pts',(-9.33736505491488,-36.2742356128,-5.4358786182898));
#58237=CARTESIAN_POINT('Ctrl Pts',(-9.42881343962009,-36.2742356128,-5.3223429594838));
#58238=CARTESIAN_POINT('Ctrl Pts',(-9.51727873836186,-36.2742356128,-5.20658874584902));
#58239=CARTESIAN_POINT('Ctrl Pts',(-9.60085311192403,-36.2742356128001,
-5.09723416242138));
#58240=CARTESIAN_POINT('Ctrl Pts',(-9.68176232664951,-36.2742356128,-4.98589877259242));
#58241=CARTESIAN_POINT('Ctrl Pts',(-9.75953527294624,-36.2742356128024,
-4.8725958051016));
#58242=CARTESIAN_POINT('Ctrl Pts',(-9.8278398193407,-36.2742356128045,-4.77308680913173));
#58243=CARTESIAN_POINT('Ctrl Pts',(-9.89372402734391,-36.2742356128084,
-4.67206030412638));
#58244=CARTESIAN_POINT('Ctrl Pts',(-9.95688389736168,-36.2742356128213,
-4.56956060979233));
#58245=CARTESIAN_POINT('Ctrl Pts',(-10.0093323537572,-36.2742356128319,
-4.48444405164669));
#58246=CARTESIAN_POINT('Ctrl Pts',(-10.0599020890899,-36.2742356128488,
-4.39831207412655));
#58247=CARTESIAN_POINT('Ctrl Pts',(-10.1084364459268,-36.2742356128813,
-4.3112115267652));
#58248=CARTESIAN_POINT('Ctrl Pts',(-10.16098590539,-36.2742356129165,-4.21690541082817));
#58249=CARTESIAN_POINT('Ctrl Pts',(-10.2111728748833,-36.2742356129955,
-4.12142324744));
#58250=CARTESIAN_POINT('Ctrl Pts',(-10.258847617925,-36.2742356129274,-4.0247804028775));
#58251=CARTESIAN_POINT('Ctrl Pts',(-10.3065223609667,-36.2742356128594,
-3.928137558315));
#58252=CARTESIAN_POINT('Ctrl Pts',(-10.3516784769153,-36.2742356128,-3.83034388890688));
#58253=CARTESIAN_POINT('Ctrl Pts',(-10.3941808250964,-36.2742356128,-3.73153260041563));
#58254=CARTESIAN_POINT('Ctrl Pts',(-10.4361612215928,-36.2742356128,-3.63393476766765));
#58255=CARTESIAN_POINT('Ctrl Pts',(-10.4755527962184,-36.2742356128,-3.53533183188484));
#58256=CARTESIAN_POINT('Ctrl Pts',(-10.5122849628678,-36.2742356128,-3.4358640110323));
#58257=CARTESIAN_POINT('Ctrl Pts',(-10.5499713898602,-36.2742356128,-3.33381212815696));
#58258=CARTESIAN_POINT('Ctrl Pts',(-10.5848585502045,-36.2742356128,-3.23084950337341));
#58259=CARTESIAN_POINT('Ctrl Pts',(-10.6169249038884,-36.2742356128,-3.12711324194226));
#58260=CARTESIAN_POINT('Ctrl Pts',(-10.6498801971988,-36.2742356128,-3.02050121626292));
#58261=CARTESIAN_POINT('Ctrl Pts',(-10.6798562655977,-36.2742356128,-2.91307165429687));
#58262=CARTESIAN_POINT('Ctrl Pts',(-10.7068847881371,-36.2742356128,-2.80496421163292));
#58263=CARTESIAN_POINT('Ctrl Pts',(-10.7351414874224,-36.2742356128,-2.69194436404779));
#58264=CARTESIAN_POINT('Ctrl Pts',(-10.7601767403046,-36.2742356128,-2.57818309705358));
#58265=CARTESIAN_POINT('Ctrl Pts',(-10.7820847464602,-36.2742356128,-2.46383743509071));
#58266=CARTESIAN_POINT('Ctrl Pts',(-10.804480029669,-36.2742356128,-2.34694850119332));
#58267=CARTESIAN_POINT('Ctrl Pts',(-10.8236077570002,-36.2742356128,-2.22944822633344));
#58268=CARTESIAN_POINT('Ctrl Pts',(-10.83962436159,-36.2742356128,-2.11151102066995));
#58269=CARTESIAN_POINT('Ctrl Pts',(-10.8560200341834,-36.2742356128,-1.99078257290199));
#58270=CARTESIAN_POINT('Ctrl Pts',(-10.8691559979564,-36.2742356128,-1.86959548423268));
#58271=CARTESIAN_POINT('Ctrl Pts',(-10.8792519960503,-36.2742356128,-1.74815488119674));
#58272=CARTESIAN_POINT('Ctrl Pts',(-10.8879558783918,-36.2742356128,-1.64345946520516));
#58273=CARTESIAN_POINT('Ctrl Pts',(-10.8944014197242,-36.2742356128,-1.53857564242055));
#58274=CARTESIAN_POINT('Ctrl Pts',(-10.8987553032475,-36.2742356128,-1.43365203176424));
#58275=CARTESIAN_POINT('Ctrl Pts',(-10.9028812002675,-36.2742356128,-1.33422263494579));
#58276=CARTESIAN_POINT('Ctrl Pts',(-10.9051326101663,-36.2742356128147,
-1.23473829160415));
#58277=CARTESIAN_POINT('Ctrl Pts',(-10.9056752402414,-36.2742356128297,
-1.13528552213591));
#58278=CARTESIAN_POINT('Ctrl Pts',(-10.905948870433,-36.2742356128373,-1.08513481796376));
#58279=CARTESIAN_POINT('Ctrl Pts',(-10.9057882730935,-36.2742356128356,
-1.03499309683131));
#58280=CARTESIAN_POINT('Ctrl Pts',(-10.9052159192415,-36.2742356128214,
-0.984876028825734));
#58281=CARTESIAN_POINT('Ctrl Pts',(-10.9036483921713,-36.2742356127825,
-0.847618525439958));
#58282=CARTESIAN_POINT('Ctrl Pts',(-10.8990065748664,-36.2742356128,-0.710462270989658));
#58283=CARTESIAN_POINT('Ctrl Pts',(-10.8917400860261,-36.2742356128,-0.573593958805236));
#58284=CARTESIAN_POINT('Ctrl Pts',(-10.89109179549,-36.2742356128,-0.561383050147837));
#58285=CARTESIAN_POINT('Ctrl Pts',(-10.8904225852203,-36.2742356128,-0.549174450233));
#58286=CARTESIAN_POINT('Ctrl Pts',(-10.8897327552813,-36.2742356128,-0.536968294734768));
#58287=CARTESIAN_POINT('Ctrl Pts',(-10.8837830369874,-36.2742356128,-0.431691352474246));
#58288=CARTESIAN_POINT('Ctrl Pts',(-10.8763040991208,-36.2742356127999,
-0.326639000646442));
#58289=CARTESIAN_POINT('Ctrl Pts',(-10.8674818264598,-36.2742356128008,
-0.22192376216726));
#58290=CARTESIAN_POINT('Ctrl Pts',(-10.8594054799106,-36.2742356128016,
-0.126062232215319));
#58291=CARTESIAN_POINT('Ctrl Pts',(-10.8502036955816,-36.2742356128034,
-0.0304844637507402));
#58292=CARTESIAN_POINT('Ctrl Pts',(-10.8399937081216,-36.2742356128072,
0.0647615827492694));
#58293=CARTESIAN_POINT('Ctrl Pts',(-10.8309039223079,-36.2742356128105,
0.149557589177328));
#58294=CARTESIAN_POINT('Ctrl Pts',(-10.821014992842,-36.2742356128154,0.234090431265654));
#58295=CARTESIAN_POINT('Ctrl Pts',(-10.8103871197297,-36.2742356128217,
0.318366652044579));
#58296=CARTESIAN_POINT('Ctrl Pts',(-10.8090773681909,-36.2742356128224,
0.328752635080224));
#58297=CARTESIAN_POINT('Ctrl Pts',(-10.8077563633402,-36.2742356128232,
0.339134778623737));
#58298=CARTESIAN_POINT('Ctrl Pts',(-10.8064241912105,-36.274235612824,0.349513145801407));
#58299=CARTESIAN_POINT('Ctrl Pts',(-10.7964147294364,-36.2742356128301,
0.427492460355431));
#58300=CARTESIAN_POINT('Ctrl Pts',(-10.7857704427514,-36.2742356128116,
0.505286572762631));
#58301=CARTESIAN_POINT('Ctrl Pts',(-10.7745234778453,-36.2742356128047,
0.582901949111922));
#58302=CARTESIAN_POINT('Ctrl Pts',(-10.7664801617643,-36.2742356127998,
0.638408924543487));
#58303=CARTESIAN_POINT('Ctrl Pts',(-10.7581282570519,-36.2742356128,0.693825319961049));
#58304=CARTESIAN_POINT('Ctrl Pts',(-10.7494730251887,-36.2742356128,0.749168689975769));
#58305=CARTESIAN_POINT('Ctrl Pts',(-10.7492108798837,-36.2742356128,0.750844902102528));
#58306=CARTESIAN_POINT('Ctrl Pts',(-10.7489485455957,-36.2742356128,0.752520471234549));
#58307=CARTESIAN_POINT('Ctrl Pts',(-10.7486857254,-36.2742356128,0.754197292365));
#58308=CARTESIAN_POINT('',(-10.0697229965085,-36.2742356128,2.85693688465354));
#58309=CARTESIAN_POINT('Ctrl Pts',(-10.7486857274262,-36.2742356128,0.754197292682571));
#58310=CARTESIAN_POINT('Ctrl Pts',(-10.7466347100106,-36.2742356128,0.76728316308377));
#58311=CARTESIAN_POINT('Ctrl Pts',(-10.7445707440896,-36.2742356128,0.780341200776172));
#58312=CARTESIAN_POINT('Ctrl Pts',(-10.7424805359006,-36.2742356128,0.793459979414592));
#58313=CARTESIAN_POINT('Ctrl Pts',(-10.7403033711681,-36.2742356128,0.807124523613989));
#58314=CARTESIAN_POINT('Ctrl Pts',(-10.7380978053388,-36.2742356128,0.820854571233398));
#58315=CARTESIAN_POINT('Ctrl Pts',(-10.735858085814,-36.2742356128,0.83469174146334));
#58316=CARTESIAN_POINT('Ctrl Pts',(-10.7334143699778,-36.2742356128,0.84978921757311));
#58317=CARTESIAN_POINT('Ctrl Pts',(-10.7309300554775,-36.2742356128,0.86501392019776));
#58318=CARTESIAN_POINT('Ctrl Pts',(-10.7284075639199,-36.2742356128,0.880356505459193));
#58319=CARTESIAN_POINT('Ctrl Pts',(-10.7271711788056,-36.2742356128,0.88787658772669));
#58320=CARTESIAN_POINT('Ctrl Pts',(-10.7259257592404,-36.2742356128,0.895424102088776));
#58321=CARTESIAN_POINT('Ctrl Pts',(-10.7246722509293,-36.2742356128,0.902993610477458));
#58322=CARTESIAN_POINT('Ctrl Pts',(-10.7214793362214,-36.2742356128,0.92227453143526));
#58323=CARTESIAN_POINT('Ctrl Pts',(-10.7182369499646,-36.2742356128,0.941680848865234));
#58324=CARTESIAN_POINT('Ctrl Pts',(-10.7149640328869,-36.2742356128,0.961095935537187));
#58325=CARTESIAN_POINT('Ctrl Pts',(-10.710943115382,-36.2742356128,0.984948193325674));
#58326=CARTESIAN_POINT('Ctrl Pts',(-10.7068773780433,-36.2742356128,1.00880694510491));
#58327=CARTESIAN_POINT('Ctrl Pts',(-10.7028050282133,-36.2742356128,1.0324118968847));
#58328=CARTESIAN_POINT('Ctrl Pts',(-10.7014661577841,-36.2742356128,1.04017251992562));
#58329=CARTESIAN_POINT('Ctrl Pts',(-10.700126495208,-36.2742356128,1.04790594476556));
#58330=CARTESIAN_POINT('Ctrl Pts',(-10.6987869997851,-36.2742356128,1.05560462756857));
#58331=CARTESIAN_POINT('Ctrl Pts',(-10.6948568818239,-36.2742356128,1.07819278355985));
#58332=CARTESIAN_POINT('Ctrl Pts',(-10.6909302150522,-36.2742356128003,
1.10047278567806));
#58333=CARTESIAN_POINT('Ctrl Pts',(-10.6869822640891,-36.2742356128002,
1.12254281928174));
#58334=CARTESIAN_POINT('Ctrl Pts',(-10.6865220270064,-36.2742356128002,
1.12511565971891));
#58335=CARTESIAN_POINT('Ctrl Pts',(-10.6860615104574,-36.2742356128001,
1.12768558829675));
#58336=CARTESIAN_POINT('Ctrl Pts',(-10.6856006835494,-36.2742356128001,
1.13025271194762));
#58337=CARTESIAN_POINT('Ctrl Pts',(-10.6817956442668,-36.2742356127999,
1.15144940460008));
#58338=CARTESIAN_POINT('Ctrl Pts',(-10.6779522323996,-36.2742356128,1.17255666838632));
#58339=CARTESIAN_POINT('Ctrl Pts',(-10.6740322378691,-36.2742356128,1.19373676928056));
#58340=CARTESIAN_POINT('Ctrl Pts',(-10.673405047118,-36.2742356128,1.1971255401797));
#58341=CARTESIAN_POINT('Ctrl Pts',(-10.6727759081903,-36.2742356128,1.20051606814297));
#58342=CARTESIAN_POINT('Ctrl Pts',(-10.6721446787479,-36.2742356128,1.20390889359303));
#58343=CARTESIAN_POINT('Ctrl Pts',(-10.66836441158,-36.2742356128,1.22422763317181));
#58344=CARTESIAN_POINT('Ctrl Pts',(-10.6645208672205,-36.2742356128,1.24456658224732));
#58345=CARTESIAN_POINT('Ctrl Pts',(-10.6605990453886,-36.2742356128,1.26495926229726));
#58346=CARTESIAN_POINT('Ctrl Pts',(-10.6567628806364,-36.2742356128,1.28490654286344));
#58347=CARTESIAN_POINT('Ctrl Pts',(-10.6528517834809,-36.2742356128,1.30490532216204));
#58348=CARTESIAN_POINT('Ctrl Pts',(-10.6488595061404,-36.2742356128,1.32493766270311));
#58349=CARTESIAN_POINT('Ctrl Pts',(-10.647051148248,-36.2742356128,1.3340115916994));
#58350=CARTESIAN_POINT('Ctrl Pts',(-10.6452262447456,-36.2742356128,1.34309171940456));
#58351=CARTESIAN_POINT('Ctrl Pts',(-10.6433847866665,-36.2742356128,1.35217287965678));
#58352=CARTESIAN_POINT('Ctrl Pts',(-10.6323806657411,-36.2742356128,1.4064397601746));
#58353=CARTESIAN_POINT('Ctrl Pts',(-10.6207566097892,-36.2742356127913,
1.46090931661876));
#58354=CARTESIAN_POINT('Ctrl Pts',(-10.6083335044896,-36.2742356130669,
1.51550391096666));
#58355=CARTESIAN_POINT('Ctrl Pts',(-10.5980828513871,-36.2742356132943,
1.56055144412652));
#58356=CARTESIAN_POINT('Ctrl Pts',(-10.5872879549167,-36.274235613725,1.60568467857377));
#58357=CARTESIAN_POINT('Ctrl Pts',(-10.5758640413931,-36.2742356139669,
1.65083743440026));
#58358=CARTESIAN_POINT('Ctrl Pts',(-10.5642537549898,-36.2742356142128,
1.69672682475306));
#58359=CARTESIAN_POINT('Ctrl Pts',(-10.5519752282585,-36.274235613683,1.74268958094638));
#58360=CARTESIAN_POINT('Ctrl Pts',(-10.5389566649902,-36.2742356133024,
1.78865941825916));
#58361=CARTESIAN_POINT('Ctrl Pts',(-10.526916197855,-36.2742356129504,1.8311755011765));
#58362=CARTESIAN_POINT('Ctrl Pts',(-10.5142426023854,-36.2742356128146,
1.87369793007753));
#58363=CARTESIAN_POINT('Ctrl Pts',(-10.5008991730841,-36.2742356128026,
1.91613325004487));
#58364=CARTESIAN_POINT('Ctrl Pts',(-10.4971520525212,-36.2742356127993,
1.9280499962163));
#58365=CARTESIAN_POINT('Ctrl Pts',(-10.4933522433736,-36.2742356128,1.9399595947355));
#58366=CARTESIAN_POINT('Ctrl Pts',(-10.4894992656358,-36.2742356128,1.95185928753506));
#58367=CARTESIAN_POINT('Ctrl Pts',(-10.4764630530136,-36.2742356128,1.99212085560819));
#58368=CARTESIAN_POINT('Ctrl Pts',(-10.4628146547796,-36.2742356128,2.03226539351294));
#58369=CARTESIAN_POINT('Ctrl Pts',(-10.4485531184273,-36.2742356128,2.0722161323579));
#58370=CARTESIAN_POINT('Ctrl Pts',(-10.4311510100196,-36.2742356128,2.12096453303303));
#58371=CARTESIAN_POINT('Ctrl Pts',(-10.4128342967672,-36.2742356128,2.16942495256767));
#58372=CARTESIAN_POINT('Ctrl Pts',(-10.3935735418708,-36.2742356128,2.21753443994428));
#58373=CARTESIAN_POINT('Ctrl Pts',(-10.3892397005709,-36.2742356128,2.22835950284712));
#58374=CARTESIAN_POINT('Ctrl Pts',(-10.3848580462214,-36.2742356128,2.23916701592833));
#58375=CARTESIAN_POINT('Ctrl Pts',(-10.3804282816357,-36.2742356128,2.24995656315333));
#58376=CARTESIAN_POINT('Ctrl Pts',(-10.3602858532663,-36.2742356128,2.29901733780848));
#58377=CARTESIAN_POINT('Ctrl Pts',(-10.3391381285185,-36.2742356127991,
2.34772286924062));
#58378=CARTESIAN_POINT('Ctrl Pts',(-10.3169784470883,-36.2742356128009,
2.39604450406616));
#58379=CARTESIAN_POINT('Ctrl Pts',(-10.2996209021515,-36.2742356128023,
2.43389454945364));
#58380=CARTESIAN_POINT('Ctrl Pts',(-10.2816424669362,-36.2742356128035,
2.47151008695783));
#58381=CARTESIAN_POINT('Ctrl Pts',(-10.2630751322098,-36.2742356128281,
2.50885913887986));
#58382=CARTESIAN_POINT('Ctrl Pts',(-10.2579382954049,-36.274235612835,2.51919212352028));
#58383=CARTESIAN_POINT('Ctrl Pts',(-10.2527566283131,-36.2742356128438,
2.52950454518725));
#58384=CARTESIAN_POINT('Ctrl Pts',(-10.2475314196008,-36.2742356128559,
2.53979528804326));
#58385=CARTESIAN_POINT('Ctrl Pts',(-10.2308331190384,-36.2742356128946,
2.57268161406069));
#58386=CARTESIAN_POINT('Ctrl Pts',(-10.2136865708931,-36.2742356129131,
2.60534561599341));
#58387=CARTESIAN_POINT('Ctrl Pts',(-10.1961534776876,-36.2742356129027,
2.63773913604163));
#58388=CARTESIAN_POINT('Ctrl Pts',(-10.1794029073218,-36.2742356128926,
2.66868689469456));
#58389=CARTESIAN_POINT('Ctrl Pts',(-10.1622992734439,-36.2742356128632,
2.69938813456047));
#58390=CARTESIAN_POINT('Ctrl Pts',(-10.1449311774068,-36.2742356128411,
2.72977010446408));
#58391=CARTESIAN_POINT('Ctrl Pts',(-10.1284729936058,-36.2742356128201,
2.75856036701445));
#58392=CARTESIAN_POINT('Ctrl Pts',(-10.1117772303903,-36.2742356128067,
2.78706411662779));
#58393=CARTESIAN_POINT('Ctrl Pts',(-10.0949536082382,-36.2742356128024,
2.81518754030304));
#58394=CARTESIAN_POINT('Ctrl Pts',(-10.0874038333031,-36.2742356128005,
2.82780821837302));
#58395=CARTESIAN_POINT('Ctrl Pts',(-10.0798287935207,-36.2742356128,2.84035184669534));
#58396=CARTESIAN_POINT('Ctrl Pts',(-10.0722409181048,-36.2742356128,2.852807544641));
#58397=CARTESIAN_POINT('Ctrl Pts',(-10.0714016752641,-36.2742356128,2.85418518393445));
#58398=CARTESIAN_POINT('Ctrl Pts',(-10.0705624326333,-36.2742356128,2.8555615233));
#58399=CARTESIAN_POINT('Ctrl Pts',(-10.0697233643,-36.2742356128,2.85693628205));
#58400=CARTESIAN_POINT('',(-6.79137755865781,-36.2742356128,3.87179939717186));
#58401=CARTESIAN_POINT('Ctrl Pts',(-10.0697226283806,-36.2742356128,2.85693748780849));
#58402=CARTESIAN_POINT('Ctrl Pts',(-10.0427054783743,-36.2742356128,2.90120340679101));
#58403=CARTESIAN_POINT('Ctrl Pts',(-10.0149092741399,-36.2742356127643,
2.94543590664087));
#58404=CARTESIAN_POINT('Ctrl Pts',(-9.98630861921963,-36.2742356129976,
2.98947462773241));
#58405=CARTESIAN_POINT('Ctrl Pts',(-9.95238280831748,-36.2742356132744,
3.04171291836917));
#58406=CARTESIAN_POINT('Ctrl Pts',(-9.91732467064534,-36.2742356140585,
3.09367893362379));
#58407=CARTESIAN_POINT('Ctrl Pts',(-9.8810149855395,-36.2742356151925,3.14509238921441));
#58408=CARTESIAN_POINT('Ctrl Pts',(-9.83360425537131,-36.2742356166732,
3.21222460098977));
#58409=CARTESIAN_POINT('Ctrl Pts',(-9.78405490480505,-36.2742356185765,
3.27841636101275));
#58410=CARTESIAN_POINT('Ctrl Pts',(-9.73201375282073,-36.2742356181146,
3.34300597725677));
#58411=CARTESIAN_POINT('Ctrl Pts',(-9.70350081936561,-36.2742356178616,
3.37839411452191));
#58412=CARTESIAN_POINT('Ctrl Pts',(-9.67423897805512,-36.2742356168433,
3.41330054426729));
#58413=CARTESIAN_POINT('Ctrl Pts',(-9.64417559703147,-36.274235615507,3.44761070496689));
#58414=CARTESIAN_POINT('Ctrl Pts',(-9.62933185379337,-36.2742356148472,
3.46455128844558));
#58415=CARTESIAN_POINT('Ctrl Pts',(-9.61430073230973,-36.2742356142845,
3.48133977663211));
#58416=CARTESIAN_POINT('Ctrl Pts',(-9.599046805007,-36.2742356137917,3.49799331944716));
#58417=CARTESIAN_POINT('Ctrl Pts',(-9.56787880217537,-36.2742356127846,
3.5320211248323));
#58418=CARTESIAN_POINT('Ctrl Pts',(-9.53575078071007,-36.2742356128432,
3.56552793219254));
#58419=CARTESIAN_POINT('Ctrl Pts',(-9.50271875164664,-36.2742356128141,
3.59827348432265));
#58420=CARTESIAN_POINT('Ctrl Pts',(-9.47108900403978,-36.2742356127862,
3.62962891656492));
#58421=CARTESIAN_POINT('Ctrl Pts',(-9.43863006930466,-36.2742356128,3.66028600049937));
#58422=CARTESIAN_POINT('Ctrl Pts',(-9.40543468805781,-36.2742356128,3.69004501056594));
#58423=CARTESIAN_POINT('Ctrl Pts',(-9.38837927873625,-36.2742356128,3.70533485146023));
#58424=CARTESIAN_POINT('Ctrl Pts',(-9.37111188743919,-36.2742356128,3.72040465547206));
#58425=CARTESIAN_POINT('Ctrl Pts',(-9.35361298710807,-36.2742356128,3.7352537065342));
#58426=CARTESIAN_POINT('Ctrl Pts',(-9.33611408677695,-36.2742356128,3.75010275759635));
#58427=CARTESIAN_POINT('Ctrl Pts',(-9.31839145737053,-36.2742356128,3.76472409613011));
#58428=CARTESIAN_POINT('Ctrl Pts',(-9.3004523225125,-36.2742356128,3.77909703529853));
#58429=CARTESIAN_POINT('Ctrl Pts',(-9.26457467434064,-36.2742356128,3.80784241565055));
#58430=CARTESIAN_POINT('Ctrl Pts',(-9.22782771264016,-36.2742356127664,
3.83559691701146));
#58431=CARTESIAN_POINT('Ctrl Pts',(-9.19027921250024,-36.2742356128789,
3.8622242824312));
#58432=CARTESIAN_POINT('Ctrl Pts',(-9.14099507705105,-36.2742356130266,
3.89717392566892));
#58433=CARTESIAN_POINT('Ctrl Pts',(-9.09031340536593,-36.2742356131635,
3.93018099942358));
#58434=CARTESIAN_POINT('Ctrl Pts',(-9.03839051489239,-36.2742356131207,
3.96101252749138));
#58435=CARTESIAN_POINT('Ctrl Pts',(-8.99022085714499,-36.2742356130811,
3.98961540651663));
#58436=CARTESIAN_POINT('Ctrl Pts',(-8.9409863450218,-36.2742356129554,4.01634539515136));
#58437=CARTESIAN_POINT('Ctrl Pts',(-8.89081544190779,-36.2742356128852,
4.04105717654398));
#58438=CARTESIAN_POINT('Ctrl Pts',(-8.84743531451334,-36.2742356128246,
4.06242414740595));
#58439=CARTESIAN_POINT('Ctrl Pts',(-8.80335630463337,-36.2742356128044,
4.0822825411275));
#58440=CARTESIAN_POINT('Ctrl Pts',(-8.75863697366334,-36.2742356128011,
4.10057022063283));
#58441=CARTESIAN_POINT('Ctrl Pts',(-8.74071780299924,-36.2742356127997,
4.10789814891347));
#58442=CARTESIAN_POINT('Ctrl Pts',(-8.72269543374841,-36.2742356128,4.11497425111613));
#58443=CARTESIAN_POINT('Ctrl Pts',(-8.70457175859042,-36.2742356128,4.12179612575218));
#58444=CARTESIAN_POINT('Ctrl Pts',(-8.6615121138754,-36.2742356128,4.13800406898433));
#58445=CARTESIAN_POINT('Ctrl Pts',(-8.61789280767915,-36.2742356128,4.15276924567355));
#58446=CARTESIAN_POINT('Ctrl Pts',(-8.5738109236211,-36.2742356128,4.16603168248515));
#58447=CARTESIAN_POINT('Ctrl Pts',(-8.5297290395644,-36.2742356128,4.17929411929633));
#58448=CARTESIAN_POINT('Ctrl Pts',(-8.48517579881231,-36.2742356128,4.19105632591689));
#58449=CARTESIAN_POINT('Ctrl Pts',(-8.44026209959521,-36.2742356128,4.20127113718018));
#58450=CARTESIAN_POINT('Ctrl Pts',(-8.38205916949961,-36.2742356128,4.21450834445235));
#58451=CARTESIAN_POINT('Ctrl Pts',(-8.32322710377887,-36.2742356127636,
4.22515208387702));
#58452=CARTESIAN_POINT('Ctrl Pts',(-8.26402667084017,-36.2742356128676,
4.23313872217696));
#58453=CARTESIAN_POINT('Ctrl Pts',(-8.23179791984128,-36.2742356129243,
4.23748665283067));
#58454=CARTESIAN_POINT('Ctrl Pts',(-8.19946018010296,-36.2742356130279,
4.24104800942531));
#58455=CARTESIAN_POINT('Ctrl Pts',(-8.16705632722208,-36.2742356133205,
4.24381893187712));
#58456=CARTESIAN_POINT('Ctrl Pts',(-8.12108841962377,-36.2742356137355,
4.24774974552742));
#58457=CARTESIAN_POINT('Ctrl Pts',(-8.07497261313446,-36.2742356144736,
4.25008843425972));
#58458=CARTESIAN_POINT('Ctrl Pts',(-8.0288281545193,-36.2742356152679,4.25083293408457));
#58459=CARTESIAN_POINT('Ctrl Pts',(-7.9826836958928,-36.2742356160621,4.25157743390961));
#58460=CARTESIAN_POINT('Ctrl Pts',(-7.93649883740971,-36.2742356168617,
4.250727941337));
#58461=CARTESIAN_POINT('Ctrl Pts',(-7.89039210993449,-36.2742356173469,
4.24829715711204));
#58462=CARTESIAN_POINT('Ctrl Pts',(-7.834906727744,-36.2742356179308,4.24537192257188));
#58463=CARTESIAN_POINT('Ctrl Pts',(-7.7794543674561,-36.2742356178824,4.24014910795062));
#58464=CARTESIAN_POINT('Ctrl Pts',(-7.72430050783329,-36.2742356176083,
4.23267735116746));
#58465=CARTESIAN_POINT('Ctrl Pts',(-7.68776143955221,-36.2742356174267,
4.22772736157206));
#58466=CARTESIAN_POINT('Ctrl Pts',(-7.65135327208932,-36.2742356171596,
4.22179141327856));
#58467=CARTESIAN_POINT('Ctrl Pts',(-7.6151500678385,-36.2742356169389,4.21489584135738));
#58468=CARTESIAN_POINT('Ctrl Pts',(-7.5697206010662,-36.2742356166621,4.20624295656578));
#58469=CARTESIAN_POINT('Ctrl Pts',(-7.52462017878676,-36.2742356157747,
4.19607685488961));
#58470=CARTESIAN_POINT('Ctrl Pts',(-7.47993901973256,-36.2742356147942,
4.18445357293978));
#58471=CARTESIAN_POINT('Ctrl Pts',(-7.43525786067835,-36.2742356138136,
4.17283029098994));
#58472=CARTESIAN_POINT('Ctrl Pts',(-7.3909849319815,-36.2742356131111,4.15974726321221));
#58473=CARTESIAN_POINT('Ctrl Pts',(-7.34717653623377,-36.2742356130129,
4.14527055133627));
#58474=CARTESIAN_POINT('Ctrl Pts',(-7.28763333788614,-36.2742356128795,
4.1255941922289));
#58475=CARTESIAN_POINT('Ctrl Pts',(-7.22891046922083,-36.2742356128427,
4.10330989587243));
#58476=CARTESIAN_POINT('Ctrl Pts',(-7.17122241053169,-36.2742356128223,
4.07858993246661));
#58477=CARTESIAN_POINT('Ctrl Pts',(-7.11432694101598,-36.2742356128022,
4.05420960218085));
#58478=CARTESIAN_POINT('Ctrl Pts',(-7.05843851288911,-36.2742356128016,
4.02746041159676));
#58479=CARTESIAN_POINT('Ctrl Pts',(-7.00372558585949,-36.2742356128006,
3.99854144870779));
#58480=CARTESIAN_POINT('Ctrl Pts',(-6.95016215270973,-36.2742356127996,
3.97023006016474));
#58481=CARTESIAN_POINT('Ctrl Pts',(-6.89772568521568,-36.2742356128,3.93983946721879));
#58482=CARTESIAN_POINT('Ctrl Pts',(-6.84653239340986,-36.2742356128,3.90758397389369));
#58483=CARTESIAN_POINT('Ctrl Pts',(-6.83371007465548,-36.2742356128,3.89950498146314));
#58484=CARTESIAN_POINT('Ctrl Pts',(-6.82096552334532,-36.2742356128,3.891309118064));
#58485=CARTESIAN_POINT('Ctrl Pts',(-6.8083001050419,-36.2742356128,3.88299998927819));
#58486=CARTESIAN_POINT('Ctrl Pts',(-6.80264328257797,-36.2742356128,3.87928883933863));
#58487=CARTESIAN_POINT('Ctrl Pts',(-6.79699868907667,-36.2742356128,3.87555272110333));
#58488=CARTESIAN_POINT('Ctrl Pts',(-6.79137755926,-36.2742356128,3.87179939627));
#58489=CARTESIAN_POINT('',(-5.86597168177314,-36.2742356128,4.46707928587636));
#58490=CARTESIAN_POINT('Ctrl Pts',(-6.79137755835672,-36.2742356128,3.87179939762279));
#58491=CARTESIAN_POINT('Ctrl Pts',(-6.76761184639918,-36.2742356128,3.85593061410674));
#58492=CARTESIAN_POINT('Ctrl Pts',(-6.74270438593246,-36.2742356128002,
3.84174534933221));
#58493=CARTESIAN_POINT('Ctrl Pts',(-6.71690530938368,-36.2742356128077,
3.82940307968605));
#58494=CARTESIAN_POINT('Ctrl Pts',(-6.69055450068662,-36.2742356128154,
3.81679686156354));
#58495=CARTESIAN_POINT('Ctrl Pts',(-6.66327401414774,-36.2742356128296,
3.80611343344803));
#58496=CARTESIAN_POINT('Ctrl Pts',(-6.63535439365547,-36.2742356128256,
3.797474184043));
#58497=CARTESIAN_POINT('Ctrl Pts',(-6.62783704541903,-36.2742356128245,
3.7951480691054));
#58498=CARTESIAN_POINT('Ctrl Pts',(-6.62027347180955,-36.2742356128222,
3.79296987495101));
#58499=CARTESIAN_POINT('Ctrl Pts',(-6.61266956107909,-36.2742356128189,
3.79094136987596));
#58500=CARTESIAN_POINT('Ctrl Pts',(-6.58404678702163,-36.2742356128064,
3.7833056355156));
#58501=CARTESIAN_POINT('Ctrl Pts',(-6.5548544424529,-36.2742356128063,3.77779824758968));
#58502=CARTESIAN_POINT('Ctrl Pts',(-6.52541631983754,-36.274235612809,3.77448101612473));
#58503=CARTESIAN_POINT('Ctrl Pts',(-6.49579762225793,-36.2742356128117,
3.77114343659068));
#58504=CARTESIAN_POINT('Ctrl Pts',(-6.4659307586813,-36.2742356128191,3.77002298684856));
#58505=CARTESIAN_POINT('Ctrl Pts',(-6.43615056222019,-36.2742356128416,
3.77113037025664));
#58506=CARTESIAN_POINT('Ctrl Pts',(-6.42803345799806,-36.2742356128477,
3.77143220663132));
#58507=CARTESIAN_POINT('Ctrl Pts',(-6.41992279052018,-36.274235612855,3.77189925623979));
#58508=CARTESIAN_POINT('Ctrl Pts',(-6.41182530777443,-36.2742356128637,
3.77253106516291));
#58509=CARTESIAN_POINT('Ctrl Pts',(-6.38224976818375,-36.2742356128954,
3.77483870698273));
#58510=CARTESIAN_POINT('Ctrl Pts',(-6.35285068902878,-36.2742356128708,
3.77934535731408));
#58511=CARTESIAN_POINT('Ctrl Pts',(-6.32395091201471,-36.2742356128434,
3.78599870729406));
#58512=CARTESIAN_POINT('Ctrl Pts',(-6.29548019782323,-36.2742356128164,
3.79255327778794));
#58513=CARTESIAN_POINT('Ctrl Pts',(-6.26749464288281,-36.2742356128016,
3.8011911613719));
#58514=CARTESIAN_POINT('Ctrl Pts',(-6.24028833581526,-36.2742356128003,
3.81181401814056));
#58515=CARTESIAN_POINT('Ctrl Pts',(-6.23221871909247,-36.2742356127999,
3.8149648457193));
#58516=CARTESIAN_POINT('Ctrl Pts',(-6.22421752784224,-36.2742356128,3.81828998335235));
#58517=CARTESIAN_POINT('Ctrl Pts',(-6.21629207071364,-36.2742356128,3.82178605280247));
#58518=CARTESIAN_POINT('Ctrl Pts',(-6.18903048380091,-36.2742356128,3.83381165582083));
#58519=CARTESIAN_POINT('Ctrl Pts',(-6.16266648013035,-36.2742356128015,
3.84786387672877));
#58520=CARTESIAN_POINT('Ctrl Pts',(-6.13748779945074,-36.2742356128333,
3.86379149731598));
#58521=CARTESIAN_POINT('Ctrl Pts',(-6.11197343727939,-36.2742356128655,
3.87993146451129));
#58522=CARTESIAN_POINT('Ctrl Pts',(-6.08767667101957,-36.2742356129214,
3.89799683301395));
#58523=CARTESIAN_POINT('Ctrl Pts',(-6.0648706288655,-36.2742356128984,3.91778392372097));
#58524=CARTESIAN_POINT('Ctrl Pts',(-6.05935038385834,-36.2742356128928,
3.92257342590393));
#58525=CARTESIAN_POINT('Ctrl Pts',(-6.05391734170426,-36.274235612883,3.92746360531471));
#58526=CARTESIAN_POINT('Ctrl Pts',(-6.04857510195205,-36.2742356128702,
3.93245120810224));
#58527=CARTESIAN_POINT('Ctrl Pts',(-6.02628005996784,-36.274235612817,3.95326622553057));
#58528=CARTESIAN_POINT('Ctrl Pts',(-6.00557086076768,-36.2742356128086,
3.97578568705138));
#58529=CARTESIAN_POINT('Ctrl Pts',(-5.98668919867165,-36.2742356128037,
3.99975188059635));
#58530=CARTESIAN_POINT('Ctrl Pts',(-5.96788968088333,-36.2742356127989,
4.02361380967733));
#58531=CARTESIAN_POINT('Ctrl Pts',(-5.95090221910612,-36.2742356128,4.04890948259598));
#58532=CARTESIAN_POINT('Ctrl Pts',(-5.93592640503596,-36.2742356128,4.0753508284618));
#58533=CARTESIAN_POINT('Ctrl Pts',(-5.9327569959689,-36.2742356128,4.08094674738412));
#58534=CARTESIAN_POINT('Ctrl Pts',(-5.92967753613311,-36.2742356128,4.08659387281414));
#58535=CARTESIAN_POINT('Ctrl Pts',(-5.92668966701898,-36.2742356128,4.09228930726427));
#58536=CARTESIAN_POINT('Ctrl Pts',(-5.91288634093118,-36.2742356128,4.11860101501454));
#58537=CARTESIAN_POINT('Ctrl Pts',(-5.90104238722179,-36.2742356127986,
4.14594540821402));
#58538=CARTESIAN_POINT('Ctrl Pts',(-5.89129324247737,-36.2742356128083,
4.17401939030619));
#58539=CARTESIAN_POINT('Ctrl Pts',(-5.88170403456135,-36.2742356128179,
4.20163281264937));
#58540=CARTESIAN_POINT('Ctrl Pts',(-5.87414169718084,-36.2742356128408,
4.22995165567001));
#58541=CARTESIAN_POINT('Ctrl Pts',(-5.86868793689861,-36.2742356128729,
4.25866970663748));
#58542=CARTESIAN_POINT('Ctrl Pts',(-5.86707823012509,-36.2742356128823,
4.26714599433122));
#58543=CARTESIAN_POINT('Ctrl Pts',(-5.86565188625897,-36.2742356128923,
4.27565696309787));
#58544=CARTESIAN_POINT('Ctrl Pts',(-5.86441015811822,-36.2742356129023,
4.28419451843095));
#58545=CARTESIAN_POINT('Ctrl Pts',(-5.86024059061394,-36.2742356129359,
4.31286255945746));
#58546=CARTESIAN_POINT('Ctrl Pts',(-5.85815474191147,-36.2742356128985,
4.34182710763987));
#58547=CARTESIAN_POINT('Ctrl Pts',(-5.85816763299558,-36.2742356128601,
4.37078377328871));
#58548=CARTESIAN_POINT('Ctrl Pts',(-5.85817731164302,-36.2742356128313,
4.39252448611661));
#58549=CARTESIAN_POINT('Ctrl Pts',(-5.85936912895101,-36.2742356128086,
4.41426052100927));
#58550=CARTESIAN_POINT('Ctrl Pts',(-5.86173021509392,-36.2742356128025,
4.43586047460259));
#58551=CARTESIAN_POINT('Ctrl Pts',(-5.8626477852411,-36.2742356128001,4.44425469294026));
#58552=CARTESIAN_POINT('Ctrl Pts',(-5.8637420657599,-36.2742356128,4.45263000166015));
#58553=CARTESIAN_POINT('Ctrl Pts',(-5.86501138994113,-36.2742356128,4.46097597332566));
#58554=CARTESIAN_POINT('Ctrl Pts',(-5.86532105398436,-36.2742356128,4.4630120547057));
#58555=CARTESIAN_POINT('Ctrl Pts',(-5.86564124357689,-36.2742356128,4.46504699468167));
#58556=CARTESIAN_POINT('Ctrl Pts',(-5.86597166755,-36.2742356128,4.4670791984));
#58557=CARTESIAN_POINT('',(2.00400681001E-5,-36.2742356128,11.3643459915));
#58558=CARTESIAN_POINT('Ctrl Pts',(-5.86597169611384,-36.2742356128,4.46707937407566));
#58559=CARTESIAN_POINT('Ctrl Pts',(-5.8917537841064,-36.2742356128,4.62564653271355));
#58560=CARTESIAN_POINT('Ctrl Pts',(-5.91113350168116,-36.2742356127996,
4.78526058020349));
#58561=CARTESIAN_POINT('Ctrl Pts',(-5.92402582739545,-36.2742356128017,
4.9453930553239));
#58562=CARTESIAN_POINT('Ctrl Pts',(-5.93703567776282,-36.2742356128039,
5.10698527587751));
#58563=CARTESIAN_POINT('Ctrl Pts',(-5.94343938459977,-36.2742356128092,
5.26910521717685));
#58564=CARTESIAN_POINT('Ctrl Pts',(-5.94320281925437,-36.2742356128227,
5.43120865955647));
#58565=CARTESIAN_POINT('Ctrl Pts',(-5.94296301946909,-36.2742356128364,
5.59552846138439));
#58566=CARTESIAN_POINT('Ctrl Pts',(-5.9359001599745,-36.2742356128589,5.75983108901504));
#58567=CARTESIAN_POINT('Ctrl Pts',(-5.92203248068316,-36.2742356128929,
5.92355170789826));
#58568=CARTESIAN_POINT('Ctrl Pts',(-5.90806831172284,-36.2742356129272,
6.08841147544444));
#58569=CARTESIAN_POINT('Ctrl Pts',(-5.88720439804731,-36.2742356129733,
6.25268087420031));
#58570=CARTESIAN_POINT('Ctrl Pts',(-5.85951245233149,-36.2742356130288,
6.41578866465459));
#58571=CARTESIAN_POINT('Ctrl Pts',(-5.83153691837167,-36.2742356130848,
6.58056681270492));
#58572=CARTESIAN_POINT('Ctrl Pts',(-5.79659286542048,-36.2742356131502,
6.74415918610583));
#58573=CARTESIAN_POINT('Ctrl Pts',(-5.75480692584564,-36.2742356132163,
6.90598606231219));
#58574=CARTESIAN_POINT('Ctrl Pts',(-5.71753047360896,-36.2742356132753,
7.05034878055894));
#58575=CARTESIAN_POINT('Ctrl Pts',(-5.67480998545357,-36.2742356133345,
7.19330651107798));
#58576=CARTESIAN_POINT('Ctrl Pts',(-5.6267692791197,-36.274235613385,7.334456277306));
#58577=CARTESIAN_POINT('Ctrl Pts',(-5.57231694921545,-36.2742356134422,
7.49444421718227));
#58578=CARTESIAN_POINT('Ctrl Pts',(-5.51102853554952,-36.2742356134451,
7.65210758867517));
#58579=CARTESIAN_POINT('Ctrl Pts',(-5.44313216551832,-36.2742356134085,
7.80687595572862));
#58580=CARTESIAN_POINT('Ctrl Pts',(-5.37497521134488,-36.2742356133719,
7.96223831892878));
#58581=CARTESIAN_POINT('Ctrl Pts',(-5.30015963440195,-36.2742356132978,
8.11468314343555));
#58582=CARTESIAN_POINT('Ctrl Pts',(-5.21896431965411,-36.274235613218,8.26365448761046));
#58583=CARTESIAN_POINT('Ctrl Pts',(-5.13753259016911,-36.274235613138,8.4130595886011));
#58584=CARTESIAN_POINT('Ctrl Pts',(-5.0496840815577,-36.2742356130535,8.55897068001005));
#58585=CARTESIAN_POINT('Ctrl Pts',(-4.95574602924874,-36.2742356129869,
8.70085219792462));
#58586=CARTESIAN_POINT('Ctrl Pts',(-4.86181143441669,-36.2742356129203,
8.84272849375868));
#58587=CARTESIAN_POINT('Ctrl Pts',(-4.76178793134922,-36.2742356128717,
8.98057525162899));
#58588=CARTESIAN_POINT('Ctrl Pts',(-4.65604588330678,-36.2742356128431,
9.11388616448563));
#58589=CARTESIAN_POINT('Ctrl Pts',(-4.55056648084933,-36.2742356128146,
9.24686595530198));
#58590=CARTESIAN_POINT('Ctrl Pts',(-4.4393971075515,-36.2742356128051,9.37533216035669));
#58591=CARTESIAN_POINT('Ctrl Pts',(-4.32294538768296,-36.2742356128018,
9.49881506179245));
#58592=CARTESIAN_POINT('Ctrl Pts',(-4.23823731799389,-36.2742356127995,
9.58863767868498));
#58593=CARTESIAN_POINT('Ctrl Pts',(-4.15073506984275,-36.2742356128,9.67582417482043));
#58594=CARTESIAN_POINT('Ctrl Pts',(-4.06060797518421,-36.2742356128,9.76020584146258));
#58595=CARTESIAN_POINT('Ctrl Pts',(-3.93701288663076,-36.2742356128,9.87592198210191));
#58596=CARTESIAN_POINT('Ctrl Pts',(-3.80848026352504,-36.2742356128,9.98636089573716));
#58597=CARTESIAN_POINT('Ctrl Pts',(-3.67547833414633,-36.2742356128,10.0911139764056));
#58598=CARTESIAN_POINT('Ctrl Pts',(-3.54294605058195,-36.2742356128,10.1954971613431));
#58599=CARTESIAN_POINT('Ctrl Pts',(-3.40597617606029,-36.2742356128,10.2942344499813));
#58600=CARTESIAN_POINT('Ctrl Pts',(-3.26506202837529,-36.2742356128,10.3869635798179));
#58601=CARTESIAN_POINT('Ctrl Pts',(-3.12463152047159,-36.2742356128,10.479374448523));
#58602=CARTESIAN_POINT('Ctrl Pts',(-2.98028396985441,-36.2742356128001,
10.5658181858481));
#58603=CARTESIAN_POINT('Ctrl Pts',(-2.83253445146773,-36.2742356128001,
10.6459802356601));
#58604=CARTESIAN_POINT('Ctrl Pts',(-2.68541849570139,-36.2742356128001,
10.72579854372));
#58605=CARTESIAN_POINT('Ctrl Pts',(-2.5349298855088,-36.2742356128002,10.7993887888944));
#58606=CARTESIAN_POINT('Ctrl Pts',(-2.38160072644212,-36.2742356128002,
10.8664861850762));
#58607=CARTESIAN_POINT('Ctrl Pts',(-2.22904444720905,-36.2742356128002,
10.9332453662393));
#58608=CARTESIAN_POINT('Ctrl Pts',(-2.0736763794413,-36.2742356128003,10.9935768682926));
#58609=CARTESIAN_POINT('Ctrl Pts',(-1.91604110659622,-36.2742356128003,
11.0472671542599));
#58610=CARTESIAN_POINT('Ctrl Pts',(-1.75983755284287,-36.2742356128003,
11.1004697993199));
#58611=CARTESIAN_POINT('Ctrl Pts',(-1.60140798882314,-36.2742356128004,
11.1471512359842));
#58612=CARTESIAN_POINT('Ctrl Pts',(-1.44129950961667,-36.2742356128003,
11.1871516829491));
#58613=CARTESIAN_POINT('Ctrl Pts',(-1.28207456984831,-36.2742356128003,
11.2269313922454));
#58614=CARTESIAN_POINT('Ctrl Pts',(-1.12118937306491,-36.2742356128003,
11.2601035402185));
#58615=CARTESIAN_POINT('Ctrl Pts',(-0.959196318817928,-36.2742356128003,
11.286560085187));
#58616=CARTESIAN_POINT('Ctrl Pts',(-0.798772591246272,-36.2742356128002,
11.3127603292791));
#58617=CARTESIAN_POINT('Ctrl Pts',(-0.637262545229791,-36.2742356128002,
11.3323743934019));
#58618=CARTESIAN_POINT('Ctrl Pts',(-0.475214087498627,-36.2742356128001,
11.34534683313));
#58619=CARTESIAN_POINT('Ctrl Pts',(-0.318810407195243,-36.2742356128,11.3578673923775));
#58620=CARTESIAN_POINT('Ctrl Pts',(-0.161905358524558,-36.2742356128,11.3642011232218));
#58621=CARTESIAN_POINT('Ctrl Pts',(-0.00499952426527361,-36.2742356128,
11.3643435450127));
#58622=CARTESIAN_POINT('Ctrl Pts',(-0.00332634407496558,-36.2742356128,
11.364345063741));
#58623=CARTESIAN_POINT('Ctrl Pts',(-0.00165316357213757,-36.2742356128,
11.3643458788333));
#58624=CARTESIAN_POINT('Ctrl Pts',(2.00400681000801E-5,-36.2742356128,11.3643459915));
#58625=CARTESIAN_POINT('',(5.86597167565,-36.2742356128,4.4670793309));
#58626=CARTESIAN_POINT('Ctrl Pts',(2.0040068100144E-5,-36.2742356128,11.3643459915));
#58627=CARTESIAN_POINT('Ctrl Pts',(0.160669261245717,-36.2742356128,11.3643342068985));
#58628=CARTESIAN_POINT('Ctrl Pts',(0.321323836354438,-36.2742356127995,
11.3578350469369));
#58629=CARTESIAN_POINT('Ctrl Pts',(0.48144851078575,-36.2742356128017,11.3448494418734));
#58630=CARTESIAN_POINT('Ctrl Pts',(0.643032821894107,-36.2742356128039,
11.3317454648881));
#58631=CARTESIAN_POINT('Ctrl Pts',(0.804077338593767,-36.2742356128091,
11.3120363431189));
#58632=CARTESIAN_POINT('Ctrl Pts',(0.96403942366694,-36.2742356128227,11.2857757694845));
#58633=CARTESIAN_POINT('Ctrl Pts',(1.12618852773305,-36.2742356128364,11.2591561584365));
#58634=CARTESIAN_POINT('Ctrl Pts',(1.28722518656786,-36.2742356128588,11.2258047936747));
#58635=CARTESIAN_POINT('Ctrl Pts',(1.44659482423436,-36.2742356128929,11.1858303670584));
#58636=CARTESIAN_POINT('Ctrl Pts',(1.60707331376536,-36.2742356129272,11.1455778089351));
#58637=CARTESIAN_POINT('Ctrl Pts',(1.76586129014309,-36.2742356129733,11.0986098401703));
#58638=CARTESIAN_POINT('Ctrl Pts',(1.92240644122734,-36.2742356130288,11.0450889599348));
#58639=CARTESIAN_POINT('Ctrl Pts',(2.08055469303748,-36.2742356130848,10.9910199990889));
#58640=CARTESIAN_POINT('Ctrl Pts',(2.23641371203394,-36.2742356131502,10.9302633474154));
#58641=CARTESIAN_POINT('Ctrl Pts',(2.38943163147733,-36.2742356132163,10.8630370730498));
#58642=CARTESIAN_POINT('Ctrl Pts',(2.52592578651562,-36.2742356132753,10.8030702825635));
#58643=CARTESIAN_POINT('Ctrl Pts',(2.66015944790375,-36.2742356133345,10.7379564690856));
#58644=CARTESIAN_POINT('Ctrl Pts',(2.79175483379253,-36.274235613385,10.6678825015028));
#58645=CARTESIAN_POINT('Ctrl Pts',(2.94092485046201,-36.2742356134422,10.5884501198747));
#58646=CARTESIAN_POINT('Ctrl Pts',(3.08670290511894,-36.2742356134451,10.5026435517876));
#58647=CARTESIAN_POINT('Ctrl Pts',(3.22856258818739,-36.2742356134085,10.4107795500798));
#58648=CARTESIAN_POINT('Ctrl Pts',(3.3709667242985,-36.2742356133719,10.3185629771964));
#58649=CARTESIAN_POINT('Ctrl Pts',(3.50942211228398,-36.2742356132978,10.2202425794934));
#58650=CARTESIAN_POINT('Ctrl Pts',(3.6434247982021,-36.274235613218,10.1161828818025));
#58651=CARTESIAN_POINT('Ctrl Pts',(3.77781765702698,-36.274235613138,10.0118201955973));
#58652=CARTESIAN_POINT('Ctrl Pts',(3.90773160377994,-36.2742356130535,9.90168494462553));
#58653=CARTESIAN_POINT('Ctrl Pts',(4.03269056067304,-36.2742356129869,9.78618610525616));
#58654=CARTESIAN_POINT('Ctrl Pts',(4.15764491834771,-36.2742356129203,9.67069151691772));
#58655=CARTESIAN_POINT('Ctrl Pts',(4.27764442325623,-36.2742356128717,9.54983396169469));
#58656=CARTESIAN_POINT('Ctrl Pts',(4.39224879920933,-36.2742356128431,9.42406028704545));
#58657=CARTESIAN_POINT('Ctrl Pts',(4.50656851704689,-36.2742356128146,9.29859901318294));
#58658=CARTESIAN_POINT('Ctrl Pts',(4.61551966406313,-36.2742356128051,9.16824624956892));
#58659=CARTESIAN_POINT('Ctrl Pts',(4.71870406094502,-36.2742356128018,9.0334797468142));
#58660=CARTESIAN_POINT('Ctrl Pts',(4.79376135581583,-36.2742356127995,8.93544933289853));
#58661=CARTESIAN_POINT('Ctrl Pts',(4.86576811547973,-36.2742356128,8.8350842239588));
#58662=CARTESIAN_POINT('Ctrl Pts',(4.93458500645283,-36.2742356128,8.73257864184937));
#58663=CARTESIAN_POINT('Ctrl Pts',(5.02895651343094,-36.2742356128,8.59200841089956));
#58664=CARTESIAN_POINT('Ctrl Pts',(5.11732652024821,-36.2742356128,8.44741196978782));
#58665=CARTESIAN_POINT('Ctrl Pts',(5.19936689681885,-36.2742356128,8.29931707527905));
#58666=CARTESIAN_POINT('Ctrl Pts',(5.2811175789149,-36.2742356128,8.15174512172261));
#58667=CARTESIAN_POINT('Ctrl Pts',(5.35658314132099,-36.2742356128,8.00069960672827));
#58668=CARTESIAN_POINT('Ctrl Pts',(5.42548522439472,-36.2742356128,7.84672561054384));
#58669=CARTESIAN_POINT('Ctrl Pts',(5.49415082453722,-36.2742356128,7.69328007765586));
#58670=CARTESIAN_POINT('Ctrl Pts',(5.55629781244997,-36.2742356128001,7.53692635372705));
#58671=CARTESIAN_POINT('Ctrl Pts',(5.61169840914281,-36.2742356128001,7.37822333453516));
#58672=CARTESIAN_POINT('Ctrl Pts',(5.66686144330851,-36.2742356128001,7.22020084754966));
#58673=CARTESIAN_POINT('Ctrl Pts',(5.71533572155684,-36.2742356128002,7.05984938881124));
#58674=CARTESIAN_POINT('Ctrl Pts',(5.75694532357763,-36.2742356128002,6.89773667307677));
#58675=CARTESIAN_POINT('Ctrl Pts',(5.79834518582213,-36.2742356128002,6.73644111211145));
#58676=CARTESIAN_POINT('Ctrl Pts',(5.83294931383753,-36.2742356128003,6.57340221821182));
#58677=CARTESIAN_POINT('Ctrl Pts',(5.86063437496362,-36.2742356128003,6.40919179399785));
#58678=CARTESIAN_POINT('Ctrl Pts',(5.88806798709023,-36.2742356128003,6.24647280759158));
#58679=CARTESIAN_POINT('Ctrl Pts',(5.90870759712497,-36.2742356128004,6.08260368375527));
#58680=CARTESIAN_POINT('Ctrl Pts',(5.92248333397203,-36.2742356128003,5.91815007354724));
#58681=CARTESIAN_POINT('Ctrl Pts',(5.93618305106614,-36.2742356128003,5.75460398087947));
#58682=CARTESIAN_POINT('Ctrl Pts',(5.94309436640146,-36.2742356128003,5.59048002886484));
#58683=CARTESIAN_POINT('Ctrl Pts',(5.9431993289485,-36.2742356128003,5.42634079730078));
#58684=CARTESIAN_POINT('Ctrl Pts',(5.94330327465857,-36.2742356128002,5.26379168378016));
#58685=CARTESIAN_POINT('Ctrl Pts',(5.93673206979469,-36.2742356128002,5.10122777113394));
#58686=CARTESIAN_POINT('Ctrl Pts',(5.92351895692325,-36.2742356128001,4.93919876000739));
#58687=CARTESIAN_POINT('Ctrl Pts',(5.91076610807552,-36.2742356128,4.78281384844637));
#58688=CARTESIAN_POINT('Ctrl Pts',(5.89182619464975,-36.2742356128,4.62692738262583));
#58689=CARTESIAN_POINT('Ctrl Pts',(5.86677516387858,-36.2742356128,4.47203417080732));
#58690=CARTESIAN_POINT('Ctrl Pts',(5.866508029849,-36.2742356128,4.47038245243268));
#58691=CARTESIAN_POINT('Ctrl Pts',(5.86624020126667,-36.2742356128,4.4687308467));
#58692=CARTESIAN_POINT('Ctrl Pts',(5.86597167565,-36.2742356128,4.4670793309));
#58693=CARTESIAN_POINT('',(6.79137814945778,-36.2742356128,3.87179980964612));
#58694=CARTESIAN_POINT('Ctrl Pts',(5.86597167565,-36.2742356128,4.4670793309));
#58695=CARTESIAN_POINT('Ctrl Pts',(5.86138310686398,-36.2742356128,4.43885832277569));
#58696=CARTESIAN_POINT('Ctrl Pts',(5.85880207480769,-36.2742356128002,4.41029637378214));
#58697=CARTESIAN_POINT('Ctrl Pts',(5.85826991574712,-36.2742356128077,4.38168750048739));
#58698=CARTESIAN_POINT('Ctrl Pts',(5.85772633902877,-36.2742356128154,4.35246481386365));
#58699=CARTESIAN_POINT('Ctrl Pts',(5.85932040979103,-36.2742356128296,4.32319365636273));
#58700=CARTESIAN_POINT('Ctrl Pts',(5.86304204786118,-36.2742356128256,4.29418908540444));
#58701=CARTESIAN_POINT('Ctrl Pts',(5.86403957209765,-36.2742356128245,4.28641488437951));
#58702=CARTESIAN_POINT('Ctrl Pts',(5.86518965424346,-36.2742356128222,4.27865982151693));
#58703=CARTESIAN_POINT('Ctrl Pts',(5.86649147241364,-36.2742356128189,4.27092991253681));
#58704=CARTESIAN_POINT('Ctrl Pts',(5.87141122237932,-36.2742356128064,4.24171752304138));
#58705=CARTESIAN_POINT('Ctrl Pts',(5.87850390340837,-36.2742356128063,4.2128693309871));
#58706=CARTESIAN_POINT('Ctrl Pts',(5.887691504304,-36.274235612809,4.18470561171533));
#58707=CARTESIAN_POINT('Ctrl Pts',(5.89693546242266,-36.2742356128117,4.15636913472078));
#58708=CARTESIAN_POINT('Ctrl Pts',(5.90829987588764,-36.2742356128191,4.12872614174051));
#58709=CARTESIAN_POINT('Ctrl Pts',(5.92165564928313,-36.2742356128416,4.10208576405828));
#58710=CARTESIAN_POINT('Ctrl Pts',(5.92529599468891,-36.2742356128477,4.09482447160953));
#58711=CARTESIAN_POINT('Ctrl Pts',(5.92908401278061,-36.274235612855,4.08763754057056));
#58712=CARTESIAN_POINT('Ctrl Pts',(5.93301649251076,-36.2742356128637,4.080530923298));
#58713=CARTESIAN_POINT('Ctrl Pts',(5.9473796244506,-36.2742356128954,4.05457445599592));
#58714=CARTESIAN_POINT('Ctrl Pts',(5.96367065437727,-36.2742356128708,4.02969036273551));
#58715=CARTESIAN_POINT('Ctrl Pts',(5.98170811879717,-36.2742356128434,4.00615073538495));
#58716=CARTESIAN_POINT('Ctrl Pts',(5.99947778858028,-36.2742356128164,3.98296059096665));
#58717=CARTESIAN_POINT('Ctrl Pts',(6.0189420762282,-36.2742356128016,3.96107576001189));
#58718=CARTESIAN_POINT('Ctrl Pts',(6.0398895528597,-36.2742356128003,3.94072308317647));
#58719=CARTESIAN_POINT('Ctrl Pts',(6.04610274843812,-36.2742356127999,3.93468631015854));
#58720=CARTESIAN_POINT('Ctrl Pts',(6.05244619165565,-36.2742356128,3.92878407929817));
#58721=CARTESIAN_POINT('Ctrl Pts',(6.0589137779052,-36.2742356128,3.92302164060569));
#58722=CARTESIAN_POINT('Ctrl Pts',(6.08116065440074,-36.2742356128,3.90320029505909));
#58723=CARTESIAN_POINT('Ctrl Pts',(6.10487954933902,-36.2742356128015,3.88503605466741));
#58724=CARTESIAN_POINT('Ctrl Pts',(6.12981354785304,-36.2742356128333,3.86872805722725));
#58725=CARTESIAN_POINT('Ctrl Pts',(6.15507996575881,-36.2742356128655,3.85220264200764));
#58726=CARTESIAN_POINT('Ctrl Pts',(6.1815936063361,-36.2742356129214,3.83758357031686));
#58727=CARTESIAN_POINT('Ctrl Pts',(6.20905587461221,-36.2742356128984,3.82503493124853));
#58728=CARTESIAN_POINT('Ctrl Pts',(6.21570316769405,-36.2742356128928,3.8219975098372));
#58729=CARTESIAN_POINT('Ctrl Pts',(6.22240591775922,-36.274235612883,3.81908118658232));
#58730=CARTESIAN_POINT('Ctrl Pts',(6.22915967133299,-36.2742356128702,3.81628788784265));
#58731=CARTESIAN_POINT('Ctrl Pts',(6.25734545658257,-36.274235612817,3.80463047133284));
#58732=CARTESIAN_POINT('Ctrl Pts',(6.28642470665912,-36.2742356128086,3.79512287984581));
#58733=CARTESIAN_POINT('Ctrl Pts',(6.31606269113364,-36.2742356128037,3.78787819386153));
#58734=CARTESIAN_POINT('Ctrl Pts',(6.34557173612636,-36.2742356127989,3.78066502574437));
#58735=CARTESIAN_POINT('Ctrl Pts',(6.37563411554278,-36.2742356128,3.77569529013553));
#58736=CARTESIAN_POINT('Ctrl Pts',(6.40590493031561,-36.2742356128,3.7730311667504));
#58737=CARTESIAN_POINT('Ctrl Pts',(6.41231129949293,-36.2742356128,3.77246734453197));
#58738=CARTESIAN_POINT('Ctrl Pts',(6.41872696926415,-36.2742356128,3.77200660708024));
#58739=CARTESIAN_POINT('Ctrl Pts',(6.42514862232994,-36.2742356128,3.77164924671227));
#58740=CARTESIAN_POINT('Ctrl Pts',(6.45481530760457,-36.2742356128,3.76999831704387));
#58741=CARTESIAN_POINT('Ctrl Pts',(6.48460928672341,-36.2742356127986,3.77055858065525));
#58742=CARTESIAN_POINT('Ctrl Pts',(6.51419858877646,-36.2742356128083,3.77332760680242));
#58743=CARTESIAN_POINT('Ctrl Pts',(6.54330247191718,-36.2742356128179,3.77605120647559));
#58744=CARTESIAN_POINT('Ctrl Pts',(6.57220785528294,-36.2742356128408,3.78091172458778));
#58745=CARTESIAN_POINT('Ctrl Pts',(6.60060221092621,-36.2742356128729,3.78785654476743));
#58746=CARTESIAN_POINT('Ctrl Pts',(6.60898295791085,-36.2742356128823,3.78990634584448));
#58747=CARTESIAN_POINT('Ctrl Pts',(6.61731923451022,-36.2742356128923,3.79213738464737));
#58748=CARTESIAN_POINT('Ctrl Pts',(6.62560315537363,-36.2742356129023,3.79454744491348));
#58749=CARTESIAN_POINT('Ctrl Pts',(6.65341952465768,-36.2742356129359,3.80264012559749));
#58750=CARTESIAN_POINT('Ctrl Pts',(6.68064171724888,-36.2742356128985,3.81275190378225));
#58751=CARTESIAN_POINT('Ctrl Pts',(6.70698651466996,-36.2742356128601,3.8247702360994));
#58752=CARTESIAN_POINT('Ctrl Pts',(6.72676623217281,-36.2742356128313,3.83379361989275));
#58753=CARTESIAN_POINT('Ctrl Pts',(6.74605153046156,-36.2742356128086,3.84389079290531));
#58754=CARTESIAN_POINT('Ctrl Pts',(6.76472817074846,-36.2742356128025,3.85499555865129));
#58755=CARTESIAN_POINT('Ctrl Pts',(6.77198632512756,-36.2742356128001,3.85931111556571));
#58756=CARTESIAN_POINT('Ctrl Pts',(6.77915400078233,-36.2742356128,3.86377963564129));
#58757=CARTESIAN_POINT('Ctrl Pts',(6.78622239998195,-36.2742356128,3.86839527856917));
#58758=CARTESIAN_POINT('Ctrl Pts',(6.78794680506907,-36.2742356128,3.86952130978507));
#58759=CARTESIAN_POINT('Ctrl Pts',(6.78966580718133,-36.2742356128,3.87065644581633));
#58760=CARTESIAN_POINT('Ctrl Pts',(6.79137807575,-36.2742356128,3.87179976043));
#58761=CARTESIAN_POINT('',(10.0697218907767,-36.2742356128,2.85693873298755));
#58762=CARTESIAN_POINT('Ctrl Pts',(6.79137822377471,-36.2742356128,3.871799859269));
#58763=CARTESIAN_POINT('Ctrl Pts',(6.84151938457836,-36.2742356128,3.90528008500436));
#58764=CARTESIAN_POINT('Ctrl Pts',(6.89293658842097,-36.2742356128,3.93699461273041));
#58765=CARTESIAN_POINT('Ctrl Pts',(6.94552480855072,-36.2742356128,3.96671973257289));
#58766=CARTESIAN_POINT('Ctrl Pts',(6.99923060295532,-36.2742356128,3.9970765533775));
#58767=CARTESIAN_POINT('Ctrl Pts',(7.05415741161727,-36.2742356128,4.02535798824697));
#58768=CARTESIAN_POINT('Ctrl Pts',(7.11014444075754,-36.2742356128,4.05135152058415));
#58769=CARTESIAN_POINT('Ctrl Pts',(7.16613146989781,-36.2742356128,4.07734505292132));
#58770=CARTESIAN_POINT('Ctrl Pts',(7.22317817849455,-36.2742356128,4.10105026459671));
#58771=CARTESIAN_POINT('Ctrl Pts',(7.28108200924425,-36.2742356128,4.12228714148679));
#58772=CARTESIAN_POINT('Ctrl Pts',(7.32228977760065,-36.2742356128,4.13740055094812));
#58773=CARTESIAN_POINT('Ctrl Pts',(7.36394849294144,-36.2742356128,4.15127161584809));
#58774=CARTESIAN_POINT('Ctrl Pts',(7.40600132539777,-36.2742356128,4.16384980223352));
#58775=CARTESIAN_POINT('Ctrl Pts',(7.44515714624124,-36.2742356128,4.17556147975619));
#58776=CARTESIAN_POINT('Ctrl Pts',(7.48466292267703,-36.2742356128,4.18615486043004));
#58777=CARTESIAN_POINT('Ctrl Pts',(7.52447163694981,-36.2742356128,4.19559140467563));
#58778=CARTESIAN_POINT('Ctrl Pts',(7.54665857513635,-36.2742356128,4.20085075624466));
#58779=CARTESIAN_POINT('Ctrl Pts',(7.56894070102147,-36.2742356128,4.20575111356474));
#58780=CARTESIAN_POINT('Ctrl Pts',(7.59131211993716,-36.2742356128,4.21028649976423));
#58781=CARTESIAN_POINT('Ctrl Pts',(7.64363395123072,-36.2742356128,4.22089377114362));
#58782=CARTESIAN_POINT('Ctrl Pts',(7.69642743540918,-36.2742356128,4.22949690219201));
#58783=CARTESIAN_POINT('Ctrl Pts',(7.74944318305338,-36.2742356128,4.2360142679208));
#58784=CARTESIAN_POINT('Ctrl Pts',(7.77661534855966,-36.2742356128,4.23935461391453));
#58785=CARTESIAN_POINT('Ctrl Pts',(7.80384358768627,-36.2742356128,4.24214768847752));
#58786=CARTESIAN_POINT('Ctrl Pts',(7.83109967842394,-36.2742356128,4.24438822334609));
#58787=CARTESIAN_POINT('Ctrl Pts',(7.88206506202742,-36.2742356128,4.24857773534005));
#58788=CARTESIAN_POINT('Ctrl Pts',(7.93314926842083,-36.2742356128,4.25083710134914));
#58789=CARTESIAN_POINT('Ctrl Pts',(7.98424169231689,-36.2742356128,4.25114613036265));
#58790=CARTESIAN_POINT('Ctrl Pts',(8.02711337374753,-36.2742356128,4.25140543678051));
#58791=CARTESIAN_POINT('Ctrl Pts',(8.06998494434458,-36.2742356128,4.25029122347823));
#58792=CARTESIAN_POINT('Ctrl Pts',(8.11277137057046,-36.2742356128,4.24780005442864));
#58793=CARTESIAN_POINT('Ctrl Pts',(8.17236599933709,-36.2742356128,4.24433025552743));
#58794=CARTESIAN_POINT('Ctrl Pts',(8.23180807055249,-36.2742356128,4.23818575219096));
#58795=CARTESIAN_POINT('Ctrl Pts',(8.29083353584622,-36.2742356128,4.22939425851744));
#58796=CARTESIAN_POINT('Ctrl Pts',(8.3177647922131,-36.2742356128,4.22538300729238));
#58797=CARTESIAN_POINT('Ctrl Pts',(8.34460932033512,-36.2742356128,4.22082141375137));
#58798=CARTESIAN_POINT('Ctrl Pts',(8.37134222810931,-36.2742356128,4.21571574014083));
#58799=CARTESIAN_POINT('Ctrl Pts',(8.43003512594198,-36.2742356128,4.20450608116464));
#58800=CARTESIAN_POINT('Ctrl Pts',(8.48821811216381,-36.2742356128,4.19066508416442));
#58801=CARTESIAN_POINT('Ctrl Pts',(8.54565009870481,-36.2742356128,4.17428481086938));
#58802=CARTESIAN_POINT('Ctrl Pts',(8.57686224125639,-36.2742356128,4.165382743295));
#58803=CARTESIAN_POINT('Ctrl Pts',(8.60785268188324,-36.2742356128,4.15573155832944));
#58804=CARTESIAN_POINT('Ctrl Pts',(8.63858384203004,-36.2742356128,4.14535244828011));
#58805=CARTESIAN_POINT('Ctrl Pts',(8.69362110899052,-36.2742356128,4.12676421900829));
#58806=CARTESIAN_POINT('Ctrl Pts',(8.74784697441915,-36.2742356128,4.10583276078715));
#58807=CARTESIAN_POINT('Ctrl Pts',(8.80112173381191,-36.2742356128,4.08265814640246));
#58808=CARTESIAN_POINT('Ctrl Pts',(8.83233010313792,-36.2742356128,4.06908245065182));
#58809=CARTESIAN_POINT('Ctrl Pts',(8.86321143979697,-36.2742356128,4.05473785563392));
#58810=CARTESIAN_POINT('Ctrl Pts',(8.89373446130519,-36.2742356128,4.03965203931799));
#58811=CARTESIAN_POINT('Ctrl Pts',(8.94582066834934,-36.2742356128,4.01390875070386));
#58812=CARTESIAN_POINT('Ctrl Pts',(8.99689375602961,-36.2742356128,3.9859890850355));
#58813=CARTESIAN_POINT('Ctrl Pts',(9.04679963513679,-36.2742356128,3.95605823396275));
#58814=CARTESIAN_POINT('Ctrl Pts',(9.09476983987168,-36.2742356128,3.92728829584052));
#58815=CARTESIAN_POINT('Ctrl Pts',(9.14166035956096,-36.2742356128,3.89666034325123));
#58816=CARTESIAN_POINT('Ctrl Pts',(9.1873503799917,-36.2742356128,3.86436442020436));
#58817=CARTESIAN_POINT('Ctrl Pts',(9.22551933413715,-36.2742356128,3.83738475168506));
#58818=CARTESIAN_POINT('Ctrl Pts',(9.26285040628098,-36.2742356128,3.80924177810094));
#58819=CARTESIAN_POINT('Ctrl Pts',(9.29929148141267,-36.2742356128,3.78006969542373));
#58820=CARTESIAN_POINT('Ctrl Pts',(9.31548964669419,-36.2742356128,3.76710261870868));
#58821=CARTESIAN_POINT('Ctrl Pts',(9.33151223703318,-36.2742356128,3.7539324919993));
#58822=CARTESIAN_POINT('Ctrl Pts',(9.34735616692466,-36.2742356128,3.74057247286867));
#58823=CARTESIAN_POINT('Ctrl Pts',(9.35985966791103,-36.2742356128,3.7300291914024));
#58824=CARTESIAN_POINT('Ctrl Pts',(9.37224859113989,-36.2742356128,3.71937049533655));
#58825=CARTESIAN_POINT('Ctrl Pts',(9.38452406192343,-36.2742356128,3.70860159408074));
#58826=CARTESIAN_POINT('Ctrl Pts',(9.39168770892528,-36.2742356128,3.70231714205812));
#58827=CARTESIAN_POINT('Ctrl Pts',(9.39881333926506,-36.2742356128,3.69599462972722));
#58828=CARTESIAN_POINT('Ctrl Pts',(9.40590237578182,-36.2742356128,3.68963402760814));
#58829=CARTESIAN_POINT('Ctrl Pts',(9.42297207364796,-36.2742356128,3.67431832763075));
#58830=CARTESIAN_POINT('Ctrl Pts',(9.43983678219286,-36.2742356128,3.65877516180039));
#58831=CARTESIAN_POINT('Ctrl Pts',(9.45650176318101,-36.2742356128,3.64301685700775));
#58832=CARTESIAN_POINT('Ctrl Pts',(9.48789581907781,-36.2742356128,3.6133308284518));
#58833=CARTESIAN_POINT('Ctrl Pts',(9.51857758677638,-36.2742356128,3.58287990661514));
#58834=CARTESIAN_POINT('Ctrl Pts',(9.54843599458563,-36.2742356128,3.55188465040527));
#58835=CARTESIAN_POINT('Ctrl Pts',(9.55027669304462,-36.2742356128,3.54997386799831));
#58836=CARTESIAN_POINT('Ctrl Pts',(9.55211427802768,-36.2742356128,3.54806102126526));
#58837=CARTESIAN_POINT('Ctrl Pts',(9.55394872954341,-36.2742356128,3.54614616349359));
#58838=CARTESIAN_POINT('Ctrl Pts',(9.57108594124286,-36.2742356128,3.5282578068234));
#58839=CARTESIAN_POINT('Ctrl Pts',(9.5879480776674,-36.2742356128,3.51019559573715));
#58840=CARTESIAN_POINT('Ctrl Pts',(9.60454635841574,-36.2742356128,3.49197510524274));
#58841=CARTESIAN_POINT('Ctrl Pts',(9.61854592084375,-36.2742356128,3.47660731516778));
#58842=CARTESIAN_POINT('Ctrl Pts',(9.63236114002549,-36.2742356128,3.46112352843253));
#58843=CARTESIAN_POINT('Ctrl Pts',(9.64601709274984,-36.2742356128,3.44551111050629));
#58844=CARTESIAN_POINT('Ctrl Pts',(9.68829875030944,-36.2742356128,3.39717183152965));
#58845=CARTESIAN_POINT('Ctrl Pts',(9.72900438532371,-36.2742356128,3.34764921013495));
#58846=CARTESIAN_POINT('Ctrl Pts',(9.76826941329833,-36.2742356128003,3.29726609260588));
#58847=CARTESIAN_POINT('Ctrl Pts',(9.81596491101616,-36.2742356128007,3.23606537555359));
#58848=CARTESIAN_POINT('Ctrl Pts',(9.86154147949212,-36.2742356128015,3.17359603058158));
#58849=CARTESIAN_POINT('Ctrl Pts',(9.90528177456204,-36.2742356128018,3.11040354515293));
#58850=CARTESIAN_POINT('Ctrl Pts',(9.93627439098575,-36.2742356128021,3.06562788786437));
#58851=CARTESIAN_POINT('Ctrl Pts',(9.96634647662424,-36.2742356128019,3.02048840177962));
#58852=CARTESIAN_POINT('Ctrl Pts',(9.99557085703759,-36.2742356128013,2.97516792500639));
#58853=CARTESIAN_POINT('Ctrl Pts',(10.0186995539105,-36.2742356128008,2.93930048985124));
#58854=CARTESIAN_POINT('Ctrl Pts',(10.0412970933275,-36.2742356128,2.90331950713817));
#58855=CARTESIAN_POINT('Ctrl Pts',(10.0633762714066,-36.2742356128,2.86731153433696));
#58856=CARTESIAN_POINT('Ctrl Pts',(10.0654960521548,-36.2742356128,2.86385447596031));
#58857=CARTESIAN_POINT('Ctrl Pts',(10.0676108788123,-36.2742356128,2.86039749820118));
#58858=CARTESIAN_POINT('Ctrl Pts',(10.0697211371,-36.2742356128,2.85693996784));
#58859=CARTESIAN_POINT('Ctrl Pts',(10.0697226446839,-36.2742356128,2.856937497759));
#58860=CARTESIAN_POINT('Ctrl Pts',(10.0868108449264,-36.2742356128,2.82893953241251));
#58861=CARTESIAN_POINT('Ctrl Pts',(10.1038408998495,-36.2742356128,2.80049888209122));
#58862=CARTESIAN_POINT('Ctrl Pts',(10.1206769338313,-36.2742356128,2.77172242081127));
#58863=CARTESIAN_POINT('Ctrl Pts',(10.1387077474632,-36.2742356128,2.74090382001234));
#58864=CARTESIAN_POINT('Ctrl Pts',(10.1565160503317,-36.2742356128,2.70970000356903));
#58865=CARTESIAN_POINT('Ctrl Pts',(10.1739861629327,-36.2742356128,2.67820448201693));
#58866=CARTESIAN_POINT('Ctrl Pts',(10.1914562755336,-36.2742356128,2.64670896046483));
#58867=CARTESIAN_POINT('Ctrl Pts',(10.2085888545462,-36.2742356128,2.61492121305597));
#58868=CARTESIAN_POINT('Ctrl Pts',(10.2253115688178,-36.2742356128,2.58290332614455));
#58869=CARTESIAN_POINT('Ctrl Pts',(10.2442752584305,-36.2742356128,2.54659479036591));
#58870=CARTESIAN_POINT('Ctrl Pts',(10.2627110130504,-36.2742356128,2.50999195948853));
#58871=CARTESIAN_POINT('Ctrl Pts',(10.2805666141344,-36.2742356128,2.47314559857214));
#58872=CARTESIAN_POINT('Ctrl Pts',(10.3020309699668,-36.2742356128,2.42885230381732));
#58873=CARTESIAN_POINT('Ctrl Pts',(10.3226574690849,-36.2742356128,2.38420646027191));
#58874=CARTESIAN_POINT('Ctrl Pts',(10.3424227968145,-36.2742356128,2.33925109872417));
#58875=CARTESIAN_POINT('Ctrl Pts',(10.3489984711218,-36.2742356128,2.32429501907034));
#58876=CARTESIAN_POINT('Ctrl Pts',(10.3554792490116,-36.2742356128,2.30930442405224));
#58877=CARTESIAN_POINT('Ctrl Pts',(10.361865220952,-36.2742356128,2.29428036879782));
#58878=CARTESIAN_POINT('Ctrl Pts',(10.3772600090511,-36.2742356128,2.25806158343659));
#58879=CARTESIAN_POINT('Ctrl Pts',(10.3921036880258,-36.2742356127998,2.22164740241346));
#58880=CARTESIAN_POINT('Ctrl Pts',(10.4064058460514,-36.2742356128045,2.18503336929683));
#58881=CARTESIAN_POINT('Ctrl Pts',(10.4113914515429,-36.2742356128061,2.17227004195534));
#58882=CARTESIAN_POINT('Ctrl Pts',(10.4163112030396,-36.2742356128083,2.15948291732981));
#58883=CARTESIAN_POINT('Ctrl Pts',(10.421165387575,-36.2742356128107,2.14667321556));
#58884=CARTESIAN_POINT('Ctrl Pts',(10.4378552303633,-36.2742356128188,2.10263040937052));
#58885=CARTESIAN_POINT('Ctrl Pts',(10.4537741614886,-36.2742356128187,2.05830255688421));
#58886=CARTESIAN_POINT('Ctrl Pts',(10.4689365032872,-36.2742356128129,2.0137770819743));
#58887=CARTESIAN_POINT('Ctrl Pts',(10.4708347607409,-36.2742356128122,2.00820269143803));
#58888=CARTESIAN_POINT('Ctrl Pts',(10.4727211655238,-36.2742356128114,2.00262526829492));
#58889=CARTESIAN_POINT('Ctrl Pts',(10.474595753097,-36.2742356128106,1.99704503209008));
#58890=CARTESIAN_POINT('Ctrl Pts',(10.4914316861822,-36.2742356128035,1.94692815054836));
#58891=CARTESIAN_POINT('Ctrl Pts',(10.5073119424348,-36.2742356128015,1.89658674680565));
#58892=CARTESIAN_POINT('Ctrl Pts',(10.5222742679554,-36.2742356128006,1.84619520383189));
#58893=CARTESIAN_POINT('Ctrl Pts',(10.5347506131046,-36.2742356127999,1.80417618199789));
#58894=CARTESIAN_POINT('Ctrl Pts',(10.5465886100346,-36.2742356128,1.7621246630014));
#58895=CARTESIAN_POINT('Ctrl Pts',(10.5578330012303,-36.2742356128,1.7201184927425));
#58896=CARTESIAN_POINT('Ctrl Pts',(10.5600735080027,-36.2742356128,1.71174853234975));
#58897=CARTESIAN_POINT('Ctrl Pts',(10.5622905328157,-36.2742356128,1.70338023330578));
#58898=CARTESIAN_POINT('Ctrl Pts',(10.5644845660067,-36.2742356128,1.69501397367632));
#58899=CARTESIAN_POINT('Ctrl Pts',(10.5723485254795,-36.2742356128,1.66502722282281));
#58900=CARTESIAN_POINT('Ctrl Pts',(10.5799204299038,-36.2742356128,1.63505503132499));
#58901=CARTESIAN_POINT('Ctrl Pts',(10.5872260308627,-36.2742356128,1.60511296430495));
#58902=CARTESIAN_POINT('Ctrl Pts',(10.5921494614707,-36.2742356128,1.58493424251863));
#58903=CARTESIAN_POINT('Ctrl Pts',(10.5969522070739,-36.2742356128,1.56476783804686));
#58904=CARTESIAN_POINT('Ctrl Pts',(10.6016441629848,-36.2742356128,1.54460836878356));
#58905=CARTESIAN_POINT('Ctrl Pts',(10.6120299146714,-36.2742356128,1.4999849226388));
#58906=CARTESIAN_POINT('Ctrl Pts',(10.6218649372005,-36.2742356128,1.45542433019419));
#58907=CARTESIAN_POINT('Ctrl Pts',(10.6312389216324,-36.2742356128,1.41097928305949));
#58908=CARTESIAN_POINT('Ctrl Pts',(10.6323836951226,-36.2742356128,1.40555154716935));
#58909=CARTESIAN_POINT('Ctrl Pts',(10.6335215933023,-36.2742356128,1.40012560768293));
#58910=CARTESIAN_POINT('Ctrl Pts',(10.6346527727281,-36.2742356128,1.39470165565607));
#58911=CARTESIAN_POINT('Ctrl Pts',(10.640718224484,-36.2742356128,1.36561810038896));
#58912=CARTESIAN_POINT('Ctrl Pts',(10.6465847391207,-36.2742356128,1.33662012121641));
#58913=CARTESIAN_POINT('Ctrl Pts',(10.6522905078878,-36.2742356128,1.30767149194298));
#58914=CARTESIAN_POINT('Ctrl Pts',(10.6573180094971,-36.2742356128,1.28216410000387));
#58915=CARTESIAN_POINT('Ctrl Pts',(10.6622206989433,-36.2742356128,1.25669466508444));
#58916=CARTESIAN_POINT('Ctrl Pts',(10.6670160317365,-36.2742356128,1.23127687061149));
#58917=CARTESIAN_POINT('Ctrl Pts',(10.6707148031908,-36.2742356128,1.21167142992987));
#58918=CARTESIAN_POINT('Ctrl Pts',(10.6743495673088,-36.2742356128,1.19209726647813));
#58919=CARTESIAN_POINT('Ctrl Pts',(10.6779240565849,-36.2742356128,1.17258170994967));
#58920=CARTESIAN_POINT('Ctrl Pts',(10.680203543542,-36.2742356128,1.16013644766692));
#58921=CARTESIAN_POINT('Ctrl Pts',(10.6824557997336,-36.2742356128,1.14772960431328));
#58922=CARTESIAN_POINT('Ctrl Pts',(10.6846973978384,-36.2742356128,1.13527354112906));
#58923=CARTESIAN_POINT('Ctrl Pts',(10.6868705679382,-36.2742356128,1.1231977171823));
#58924=CARTESIAN_POINT('Ctrl Pts',(10.6890335643841,-36.2742356128,1.11107657302086));
#58925=CARTESIAN_POINT('Ctrl Pts',(10.6911936071295,-36.2742356128,1.0988763009671));
#58926=CARTESIAN_POINT('Ctrl Pts',(10.6937914461701,-36.2742356128,1.08420328437349));
#58927=CARTESIAN_POINT('Ctrl Pts',(10.6963904005884,-36.2742356128,1.06938558364541));
#58928=CARTESIAN_POINT('Ctrl Pts',(10.6989919881183,-36.2742356128,1.05442681683859));
#58929=CARTESIAN_POINT('Ctrl Pts',(10.7019588055677,-36.2742356128,1.03736802874348));
#58930=CARTESIAN_POINT('Ctrl Pts',(10.7049289097575,-36.2742356128,1.02012674418216));
#58931=CARTESIAN_POINT('Ctrl Pts',(10.7078909939529,-36.2742356128,1.00278497532506));
#58932=CARTESIAN_POINT('Ctrl Pts',(10.7117733770868,-36.2742356128,0.980055239611377));
#58933=CARTESIAN_POINT('Ctrl Pts',(10.7156412504301,-36.2742356128,0.95715796020661));
#58934=CARTESIAN_POINT('Ctrl Pts',(10.7194527266718,-36.2742356128,0.934361636596206));
#58935=CARTESIAN_POINT('Ctrl Pts',(10.7221988944412,-36.2742356128,0.917936890595001));
#58936=CARTESIAN_POINT('Ctrl Pts',(10.7249152575914,-36.2742356128,0.901567378438556));
#58937=CARTESIAN_POINT('Ctrl Pts',(10.7275884500151,-36.2742356128,0.88533375000401));
#58938=CARTESIAN_POINT('Ctrl Pts',(10.7299953053386,-36.2742356128,0.870717520109329));
#58939=CARTESIAN_POINT('Ctrl Pts',(10.7323669962552,-36.2742356128,0.85621239808682));
#58940=CARTESIAN_POINT('Ctrl Pts',(10.734699590284,-36.2742356128,0.841838560557644));
#58941=CARTESIAN_POINT('Ctrl Pts',(10.7368184926509,-36.2742356128,0.828781527063753));
#58942=CARTESIAN_POINT('Ctrl Pts',(10.7389050773595,-36.2742356128,0.815833125356652));
#58943=CARTESIAN_POINT('Ctrl Pts',(10.7409628459172,-36.2742356128,0.802967107192119));
#58944=CARTESIAN_POINT('Ctrl Pts',(10.7427047093747,-36.2742356128,0.792076258073006));
#58945=CARTESIAN_POINT('Ctrl Pts',(10.7444259863495,-36.2742356128,0.781244030786989));
#58946=CARTESIAN_POINT('Ctrl Pts',(10.7461333960947,-36.2742356128,0.770425450444427));
#58947=CARTESIAN_POINT('Ctrl Pts',(10.746986856985,-36.2742356128,0.765017706206505));
#58948=CARTESIAN_POINT('Ctrl Pts',(10.7478357689667,-36.2742356128,0.759620335417667));
#58949=CARTESIAN_POINT('Ctrl Pts',(10.7486843238,-36.2742356128,0.754206356986));
#58950=CARTESIAN_POINT('',(9.7282927137,-36.2742356128,2.648549352));
#58951=CARTESIAN_POINT('',(10.3535102277,-36.2742356128,0.692259222377));
#58952=CARTESIAN_POINT('Ctrl Pts',(9.7282927137,-36.2742356128,2.648549352));
#58953=CARTESIAN_POINT('Ctrl Pts',(9.74639969517236,-36.2742356128,2.61888218325925));
#58954=CARTESIAN_POINT('Ctrl Pts',(9.76450481782315,-36.2742356127996,2.58857606374712));
#58955=CARTESIAN_POINT('Ctrl Pts',(9.78240917986035,-36.2742356128004,2.55776271394264));
#58956=CARTESIAN_POINT('Ctrl Pts',(9.80080208211504,-36.2742356128013,2.52610858798629));
#58957=CARTESIAN_POINT('Ctrl Pts',(9.81898317367036,-36.2742356127996,2.49391916838793));
#58958=CARTESIAN_POINT('Ctrl Pts',(9.83679025426058,-36.2742356128305,2.46132086015645));
#58959=CARTESIAN_POINT('Ctrl Pts',(9.84954651385432,-36.2742356128527,2.43796877388881));
#58960=CARTESIAN_POINT('Ctrl Pts',(9.86211199597106,-36.2742356128914,2.41440650413952));
#58961=CARTESIAN_POINT('Ctrl Pts',(9.87444269048559,-36.2742356129957,2.39067568122307));
#58962=CARTESIAN_POINT('Ctrl Pts',(9.89313929948119,-36.2742356131537,2.35469344869838));
#58963=CARTESIAN_POINT('Ctrl Pts',(9.91130525476423,-36.274235613575,2.31830080564483));
#58964=CARTESIAN_POINT('Ctrl Pts',(9.92886336081567,-36.2742356142595,2.28157258436356));
#58965=CARTESIAN_POINT('Ctrl Pts',(9.94780805475828,-36.2742356149981,2.24194388470814));
#58966=CARTESIAN_POINT('Ctrl Pts',(9.96604538607517,-36.2742356160186,2.20192435360085));
#58967=CARTESIAN_POINT('Ctrl Pts',(9.98353502301114,-36.274235616299,2.16158375789261));
#58968=CARTESIAN_POINT('Ctrl Pts',(9.99047178660671,-36.2742356164103,2.14558381594087));
#58969=CARTESIAN_POINT('Ctrl Pts',(9.99729149635977,-36.2742356163983,2.12953312949594));
#58970=CARTESIAN_POINT('Ctrl Pts',(10.0039936507053,-36.2742356162252,2.11343521377528));
#58971=CARTESIAN_POINT('Ctrl Pts',(10.0138233241821,-36.2742356159713,2.08982530462801));
#58972=CARTESIAN_POINT('Ctrl Pts',(10.0234041182003,-36.2742356155042,2.06610086022346));
#58973=CARTESIAN_POINT('Ctrl Pts',(10.0327214232002,-36.2742356149673,2.04231132471509));
#58974=CARTESIAN_POINT('Ctrl Pts',(10.0420387282002,-36.2742356144305,2.01852178920672));
#58975=CARTESIAN_POINT('Ctrl Pts',(10.0510920659195,-36.274235613744,1.99467139543396));
#58976=CARTESIAN_POINT('Ctrl Pts',(10.0598800359898,-36.2742356133125,1.97078707699407));
#58977=CARTESIAN_POINT('Ctrl Pts',(10.0774557575172,-36.2742356124497,1.9230190342708));
#58978=CARTESIAN_POINT('Ctrl Pts',(10.0939547323721,-36.2742356128,1.87511365332179));
#58979=CARTESIAN_POINT('Ctrl Pts',(10.1094721884702,-36.2742356128,1.82712935861783));
#58980=CARTESIAN_POINT('Ctrl Pts',(10.1249269578322,-36.2742356128,1.77933890875558));
#58981=CARTESIAN_POINT('Ctrl Pts',(10.1394203301501,-36.2742356128,1.73144552171482));
#58982=CARTESIAN_POINT('Ctrl Pts',(10.1530321403974,-36.2742356128,1.68352654520081));
#58983=CARTESIAN_POINT('Ctrl Pts',(10.1649940560187,-36.2742356128,1.64141585284596));
#58984=CARTESIAN_POINT('Ctrl Pts',(10.1762640081837,-36.2742356128,1.59931829911508));
#58985=CARTESIAN_POINT('Ctrl Pts',(10.186907836536,-36.2742356128,1.55738467788051));
#58986=CARTESIAN_POINT('Ctrl Pts',(10.1883759287505,-36.2742356128,1.55160081695896));
#58987=CARTESIAN_POINT('Ctrl Pts',(10.1898321493012,-36.2742356128,1.54582000429803));
#58988=CARTESIAN_POINT('Ctrl Pts',(10.1912767070894,-36.2742356128,1.540042567223));
#58989=CARTESIAN_POINT('Ctrl Pts',(10.2018224412741,-36.2742356128,1.4978654275073));
#58990=CARTESIAN_POINT('Ctrl Pts',(10.2117463179877,-36.2742356128,1.45586806131404));
#58991=CARTESIAN_POINT('Ctrl Pts',(10.2211403601895,-36.2742356128,1.41414635375179));
#58992=CARTESIAN_POINT('Ctrl Pts',(10.2304712937462,-36.2742356128,1.37270493026578));
#58993=CARTESIAN_POINT('Ctrl Pts',(10.239280159291,-36.2742356128,1.33153562152515));
#58994=CARTESIAN_POINT('Ctrl Pts',(10.2476672649487,-36.2742356128,1.29068235424995));
#58995=CARTESIAN_POINT('Ctrl Pts',(10.2559444639923,-36.2742356128,1.25036443784098));
#58996=CARTESIAN_POINT('Ctrl Pts',(10.2638115094769,-36.2742356128,1.21035441433096));
#58997=CARTESIAN_POINT('Ctrl Pts',(10.2713651096502,-36.2742356128,1.17064400636089));
#58998=CARTESIAN_POINT('Ctrl Pts',(10.2787081573781,-36.2742356128,1.13204050414655));
#58999=CARTESIAN_POINT('Ctrl Pts',(10.2857555068467,-36.2742356128,1.09372008741171));
#59000=CARTESIAN_POINT('Ctrl Pts',(10.2925879832386,-36.2742356128,1.05562716733571));
#59001=CARTESIAN_POINT('Ctrl Pts',(10.2993020847495,-36.2742356128,1.01819421951903));
#59002=CARTESIAN_POINT('Ctrl Pts',(10.305809150057,-36.2742356128,0.980980968471632));
#59003=CARTESIAN_POINT('Ctrl Pts',(10.312170914478,-36.2742356128,0.943887867072484));
#59004=CARTESIAN_POINT('Ctrl Pts',(10.3183609260776,-36.2742356128,0.907796193012892));
#59005=CARTESIAN_POINT('Ctrl Pts',(10.3244137257131,-36.2742356128,0.87181819850963));
#59006=CARTESIAN_POINT('Ctrl Pts',(10.3303660898792,-36.2742356128,0.835818017326376));
#59007=CARTESIAN_POINT('Ctrl Pts',(10.3363184540454,-36.2742356128,0.799817836143121));
#59008=CARTESIAN_POINT('Ctrl Pts',(10.3421708065341,-36.2742356128,0.763795596254962));
#59009=CARTESIAN_POINT('Ctrl Pts',(10.3479336927262,-36.2742356128,0.727569928829446));
#59010=CARTESIAN_POINT('Ctrl Pts',(10.3497066699331,-36.2742356128,0.716424943399226));
#59011=CARTESIAN_POINT('Ctrl Pts',(10.3514709231525,-36.2742356128,0.705260646778015));
#59012=CARTESIAN_POINT('Ctrl Pts',(10.3532261841132,-36.2742356128,0.694070745754275));
#59013=CARTESIAN_POINT('Ctrl Pts',(10.3533208886531,-36.2742356128,0.693466998247719));
#59014=CARTESIAN_POINT('Ctrl Pts',(10.3534155669269,-36.2742356128,0.692863176355315));
#59015=CARTESIAN_POINT('Ctrl Pts',(10.3535102277,-36.2742356128,0.692259222377));
#59016=CARTESIAN_POINT('',(6.27496287808,-36.2742356128,2.72284550202));
#59017=CARTESIAN_POINT('Ctrl Pts',(6.27496287808,-36.2742356128,2.72284550202));
#59018=CARTESIAN_POINT('Ctrl Pts',(6.3028237745312,-36.2742356128,2.77462456613411));
#59019=CARTESIAN_POINT('Ctrl Pts',(6.33266102473065,-36.2742356127999,2.82510898731958));
#59020=CARTESIAN_POINT('Ctrl Pts',(6.36432894986973,-36.2742356128001,2.87430077751781));
#59021=CARTESIAN_POINT('Ctrl Pts',(6.39573177399559,-36.2742356128004,2.92308076955223));
#59022=CARTESIAN_POINT('Ctrl Pts',(6.42893480005577,-36.2742356128,2.97058986708201));
#59023=CARTESIAN_POINT('Ctrl Pts',(6.46383563974238,-36.2742356128075,3.01679807520185));
#59024=CARTESIAN_POINT('Ctrl Pts',(6.49827611330993,-36.2742356128148,3.0623967652232));
#59025=CARTESIAN_POINT('Ctrl Pts',(6.53436997488869,-36.2742356128281,3.1067288077039));
#59026=CARTESIAN_POINT('Ctrl Pts',(6.57205669686505,-36.2742356128823,3.14973170076718));
#59027=CARTESIAN_POINT('Ctrl Pts',(6.58927927620085,-36.274235612907,3.16938373465635));
#59028=CARTESIAN_POINT('Ctrl Pts',(6.60683503228447,-36.2742356129409,3.18875770411654));
#59029=CARTESIAN_POINT('Ctrl Pts',(6.62472081865607,-36.2742356129908,3.20784512271744));
#59030=CARTESIAN_POINT('Ctrl Pts',(6.66420229257168,-36.274235613101,3.24997910575575));
#59031=CARTESIAN_POINT('Ctrl Pts',(6.70530692684205,-36.2742356131351,3.29074285237302));
#59032=CARTESIAN_POINT('Ctrl Pts',(6.74801769993325,-36.2742356130925,3.32999680629123));
#59033=CARTESIAN_POINT('Ctrl Pts',(6.79038833604411,-36.2742356130502,3.3689381523968));
#59034=CARTESIAN_POINT('Ctrl Pts',(6.83433964290682,-36.2742356129557,3.40639378325257));
#59035=CARTESIAN_POINT('Ctrl Pts',(6.87988888863763,-36.2742356128945,3.4421893332177));
#59036=CARTESIAN_POINT('Ctrl Pts',(6.92507555314669,-36.2742356128338,3.47769994335494));
#59037=CARTESIAN_POINT('Ctrl Pts',(6.97183486114045,-36.2742356128077,3.51157688320459));
#59038=CARTESIAN_POINT('Ctrl Pts',(7.02021674223042,-36.2742356128022,3.54361067505602));
#59039=CARTESIAN_POINT('Ctrl Pts',(7.04458018405629,-36.2742356127995,3.55974178460886));
#59040=CARTESIAN_POINT('Ctrl Pts',(7.06935559487873,-36.2742356128,3.57540488225698));
#59041=CARTESIAN_POINT('Ctrl Pts',(7.09455249876125,-36.2742356128,3.59056931505338));
#59042=CARTESIAN_POINT('Ctrl Pts',(7.13528363996614,-36.2742356128,3.61508282895183));
#59043=CARTESIAN_POINT('Ctrl Pts',(7.17711751931734,-36.2742356128,3.63829389976814));
#59044=CARTESIAN_POINT('Ctrl Pts',(7.22005071711028,-36.2742356128,3.6600252280536));
#59045=CARTESIAN_POINT('Ctrl Pts',(7.22426457543557,-36.2742356128,3.66215814018973));
#59046=CARTESIAN_POINT('Ctrl Pts',(7.22848898600892,-36.2742356128,3.66427678146597));
#59047=CARTESIAN_POINT('Ctrl Pts',(7.23272392142221,-36.2742356128,3.66638097422168));
#59048=CARTESIAN_POINT('Ctrl Pts',(7.27455512514582,-36.2742356128,3.68716545078337));
#59049=CARTESIAN_POINT('Ctrl Pts',(7.31741530957928,-36.2742356128,3.70653801486018));
#59050=CARTESIAN_POINT('Ctrl Pts',(7.36116658604512,-36.2742356128,3.72429188348139));
#59051=CARTESIAN_POINT('Ctrl Pts',(7.38747354611457,-36.2742356128,3.73496700774345));
#59052=CARTESIAN_POINT('Ctrl Pts',(7.41410383714687,-36.2742356128,3.74505817719987));
#59053=CARTESIAN_POINT('Ctrl Pts',(7.44102886118993,-36.2742356128,3.75452639334412));
#59054=CARTESIAN_POINT('Ctrl Pts',(7.47566119449322,-36.2742356128,3.76670489378932));
#59055=CARTESIAN_POINT('Ctrl Pts',(7.51077587512702,-36.2742356128,3.77785011506413));
#59056=CARTESIAN_POINT('Ctrl Pts',(7.54628534309336,-36.2742356128,3.78788183369851));
#59057=CARTESIAN_POINT('Ctrl Pts',(7.58124771398936,-36.2742356128,3.79775899288185));
#59058=CARTESIAN_POINT('Ctrl Pts',(7.61659277102232,-36.2742356128,3.8065576335011));
#59059=CARTESIAN_POINT('Ctrl Pts',(7.65227357737817,-36.2742356128,3.81421987407179));
#59060=CARTESIAN_POINT('Ctrl Pts',(7.68579079235983,-36.2742356128,3.82141749628604));
#59061=CARTESIAN_POINT('Ctrl Pts',(7.71960063055048,-36.2742356128,3.8276112329845));
#59062=CARTESIAN_POINT('Ctrl Pts',(7.7536458617549,-36.2742356128,3.83275416322896));
#59063=CARTESIAN_POINT('Ctrl Pts',(7.80194884419358,-36.2742356128,3.84005089350494));
#59064=CARTESIAN_POINT('Ctrl Pts',(7.85071830221758,-36.2742356128,3.84522820662984));
#59065=CARTESIAN_POINT('Ctrl Pts',(7.89972755275133,-36.2742356128,3.84817846111999));
#59066=CARTESIAN_POINT('Ctrl Pts',(7.94648093156463,-36.2742356128,3.85099291684563));
#59067=CARTESIAN_POINT('Ctrl Pts',(7.9934519414373,-36.2742356128,3.85178034557181));
#59068=CARTESIAN_POINT('Ctrl Pts',(8.04043402108122,-36.2742356128,3.8504930204742));
#59069=CARTESIAN_POINT('Ctrl Pts',(8.07113530574063,-36.2742356128,3.84965179474365));
#59070=CARTESIAN_POINT('Ctrl Pts',(8.10184114058114,-36.2742356128,3.84792554187736));
#59071=CARTESIAN_POINT('Ctrl Pts',(8.13249320763682,-36.2742356128,3.84531308289118));
#59072=CARTESIAN_POINT('Ctrl Pts',(8.17723382114091,-36.2742356128,3.84149986476192));
#59073=CARTESIAN_POINT('Ctrl Pts',(8.22185515513467,-36.2742356128046,3.83579376812364));
#59074=CARTESIAN_POINT('Ctrl Pts',(8.26614133198898,-36.2742356128544,3.82822139707751));
#59075=CARTESIAN_POINT('Ctrl Pts',(8.29571833031613,-36.2742356128876,3.82316410783576));
#59076=CARTESIAN_POINT('Ctrl Pts',(8.3251465213504,-36.2742356129346,3.81727535696549));
#59077=CARTESIAN_POINT('Ctrl Pts',(8.35436952870322,-36.2742356129424,3.81057315013535));
#59078=CARTESIAN_POINT('Ctrl Pts',(8.39085630599924,-36.2742356129521,3.80220502001613));
#59079=CARTESIAN_POINT('Ctrl Pts',(8.42702490644852,-36.2742356128792,3.79256699905163));
#59080=CARTESIAN_POINT('Ctrl Pts',(8.46274259986607,-36.274235612827,3.78172063018468));
#59081=CARTESIAN_POINT('Ctrl Pts',(8.49846029328184,-36.2742356127748,3.77087426131826));
#59082=CARTESIAN_POINT('Ctrl Pts',(8.53373640609619,-36.2742356128,3.75881047120901));
#59083=CARTESIAN_POINT('Ctrl Pts',(8.56844925695303,-36.2742356128,3.74561879250407));
#59084=CARTESIAN_POINT('Ctrl Pts',(8.61269289485571,-36.2742356128,3.72880519634176));
#59085=CARTESIAN_POINT('Ctrl Pts',(8.65603418238756,-36.2742356128,3.71015491345561));
#59086=CARTESIAN_POINT('Ctrl Pts',(8.69832444168997,-36.2742356128,3.6898583383386));
#59087=CARTESIAN_POINT('Ctrl Pts',(8.74129416914554,-36.2742356128,3.66923566268124));
#59088=CARTESIAN_POINT('Ctrl Pts',(8.78317866197519,-36.2742356128,3.64691408634317));
#59089=CARTESIAN_POINT('Ctrl Pts',(8.82386994827566,-36.2742356128,3.62311913239659));
#59090=CARTESIAN_POINT('Ctrl Pts',(8.86657743538069,-36.2742356128,3.59814516914229));
#59091=CARTESIAN_POINT('Ctrl Pts',(8.90796835167006,-36.2742356128,3.57155084765688));
#59092=CARTESIAN_POINT('Ctrl Pts',(8.94799791375628,-36.2742356128,3.54359600071795));
#59093=CARTESIAN_POINT('Ctrl Pts',(8.965002670958,-36.2742356128,3.53172064260677));
#59094=CARTESIAN_POINT('Ctrl Pts',(8.98176208440896,-36.2742356128,3.5196000334607));
#59095=CARTESIAN_POINT('Ctrl Pts',(8.99827512664272,-36.2742356128,3.50725452876548));
#59096=CARTESIAN_POINT('Ctrl Pts',(9.03434720067447,-36.2742356128,3.48028627221884));
#59097=CARTESIAN_POINT('Ctrl Pts',(9.06926218434382,-36.2742356128,3.45222818843661));
#59098=CARTESIAN_POINT('Ctrl Pts',(9.1030036175438,-36.2742356128,3.42331618990479));
#59099=CARTESIAN_POINT('Ctrl Pts',(9.10943887321986,-36.2742356128,3.41780201682401));
#59100=CARTESIAN_POINT('Ctrl Pts',(9.1158315930112,-36.2742356128,3.41225677682403));
#59101=CARTESIAN_POINT('Ctrl Pts',(9.12218187857283,-36.2742356128,3.40668208887777));
#59102=CARTESIAN_POINT('Ctrl Pts',(9.15591769209004,-36.2742356128,3.37706662810103));
#59103=CARTESIAN_POINT('Ctrl Pts',(9.18846346570522,-36.2742356126279,3.34660965236935));
#59104=CARTESIAN_POINT('Ctrl Pts',(9.21980647110474,-36.2742356130288,3.31558795797188));
#59105=CARTESIAN_POINT('Ctrl Pts',(9.22444834338276,-36.2742356130882,3.3109936715783));
#59106=CARTESIAN_POINT('Ctrl Pts',(9.22906391970104,-36.2742356131663,3.30638696037994));
#59107=CARTESIAN_POINT('Ctrl Pts',(9.2336532445861,-36.2742356132749,3.30176868004118));
#59108=CARTESIAN_POINT('Ctrl Pts',(9.25144261015871,-36.274235613696,3.28386707592281));
#59109=CARTESIAN_POINT('Ctrl Pts',(9.26883694920177,-36.2742356146205,3.26579252621011));
#59110=CARTESIAN_POINT('Ctrl Pts',(9.28584062583539,-36.2742356162734,3.24760004211036));
#59111=CARTESIAN_POINT('Ctrl Pts',(9.302844302469,-36.2742356179262,3.22940755801061));
#59112=CARTESIAN_POINT('Ctrl Pts',(9.31949202128959,-36.2742356204437,3.21105852851475));
#59113=CARTESIAN_POINT('Ctrl Pts',(9.33581316077557,-36.2742356244168,3.19257010082136));
#59114=CARTESIAN_POINT('Ctrl Pts',(9.36434739707762,-36.2742356313629,3.16024679612132));
#59115=CARTESIAN_POINT('Ctrl Pts',(9.39191683705234,-36.2742356357654,3.1274880628538));
#59116=CARTESIAN_POINT('Ctrl Pts',(9.41852620590725,-36.2742356356124,3.09454044363916));
#59117=CARTESIAN_POINT('Ctrl Pts',(9.44522459013014,-36.2742356354589,3.06148260593477));
#59118=CARTESIAN_POINT('Ctrl Pts',(9.47095736863029,-36.2742356315576,3.02823551422887));
#59119=CARTESIAN_POINT('Ctrl Pts',(9.49576670903768,-36.2742356276487,2.99501198544618));
#59120=CARTESIAN_POINT('Ctrl Pts',(9.50279286499792,-36.2742356265416,2.98560288020825));
#59121=CARTESIAN_POINT('Ctrl Pts',(9.50974513768581,-36.2742356254317,2.9761953997071));
#59122=CARTESIAN_POINT('Ctrl Pts',(9.51662486506729,-36.2742356243793,2.96679371865397));
#59123=CARTESIAN_POINT('Ctrl Pts',(9.52548491478471,-36.2742356230239,2.95468577353649));
#59124=CARTESIAN_POINT('Ctrl Pts',(9.53422639106844,-36.2742356219228,2.9425842244868));
#59125=CARTESIAN_POINT('Ctrl Pts',(9.54287330530364,-36.2742356208252,2.93046924908954));
#59126=CARTESIAN_POINT('Ctrl Pts',(9.56654480644426,-36.2742356178206,2.89730370053265));
#59127=CARTESIAN_POINT('Ctrl Pts',(9.58948819545112,-36.2742356158232,2.86405994531656));
#59128=CARTESIAN_POINT('Ctrl Pts',(9.61179276518404,-36.2742356146377,2.83081476039708));
#59129=CARTESIAN_POINT('Ctrl Pts',(9.63351607564837,-36.274235613483,2.79843594824792));
#59130=CARTESIAN_POINT('Ctrl Pts',(9.65463408372118,-36.2742356130699,2.76605589156097));
#59131=CARTESIAN_POINT('Ctrl Pts',(9.6752305983474,-36.2742356129102,2.73369667930163));
#59132=CARTESIAN_POINT('Ctrl Pts',(9.6928921026444,-36.2742356127732,2.70594866577907));
#59133=CARTESIAN_POINT('Ctrl Pts',(9.71017038222493,-36.2742356128,2.67821523964025));
#59134=CARTESIAN_POINT('Ctrl Pts',(9.72711381130454,-36.2742356128,2.65048002401181));
#59135=CARTESIAN_POINT('Ctrl Pts',(9.72750687873562,-36.2742356128,2.6498365999501));
#59136=CARTESIAN_POINT('Ctrl Pts',(9.72789975796667,-36.2742356128,2.64919318798333));
#59137=CARTESIAN_POINT('Ctrl Pts',(9.7282927137,-36.2742356128,2.648549352));
#59138=CARTESIAN_POINT('',(2.29653436395,-36.2742356128,-2.09683572989));
#59139=CARTESIAN_POINT('Ctrl Pts',(2.29653436395,-36.2742356128,-2.09683572989));
#59140=CARTESIAN_POINT('Ctrl Pts',(2.36844264581072,-36.2742356128,-2.06297361352936));
#59141=CARTESIAN_POINT('Ctrl Pts',(2.44020262706449,-36.2742356128,-2.02814938203184));
#59142=CARTESIAN_POINT('Ctrl Pts',(2.51175434855808,-36.2742356128,-1.99251485917145));
#59143=CARTESIAN_POINT('Ctrl Pts',(2.57619685221496,-36.2742356128,-1.96042090221547));
#59144=CARTESIAN_POINT('Ctrl Pts',(2.64046968487184,-36.2742356128,-1.9276691645241));
#59145=CARTESIAN_POINT('Ctrl Pts',(2.70449947469043,-36.2742356128,-1.89434968461788));
#59146=CARTESIAN_POINT('Ctrl Pts',(2.77206180084746,-36.2742356128,-1.85919196232666));
#59147=CARTESIAN_POINT('Ctrl Pts',(2.8393023230107,-36.2742356128,-1.82343113570922));
#59148=CARTESIAN_POINT('Ctrl Pts',(2.90642539048409,-36.2742356128,-1.78697407945998));
#59149=CARTESIAN_POINT('Ctrl Pts',(2.97354845795748,-36.2742356128,-1.75051702321074));
#59150=CARTESIAN_POINT('Ctrl Pts',(3.04052116237677,-36.2742356127993,-1.71337921672418));
#59151=CARTESIAN_POINT('Ctrl Pts',(3.10725339275564,-36.2742356128007,-1.67558113763683));
#59152=CARTESIAN_POINT('Ctrl Pts',(3.18601825695535,-36.2742356128024,-1.63096760457458));
#59153=CARTESIAN_POINT('Ctrl Pts',(3.2644395547577,-36.2742356128047,-1.58543858736672));
#59154=CARTESIAN_POINT('Ctrl Pts',(3.34237246387412,-36.2742356128046,-1.53896639731643));
#59155=CARTESIAN_POINT('Ctrl Pts',(3.42432560316084,-36.2742356128045,-1.49009690293556));
#59156=CARTESIAN_POINT('Ctrl Pts',(3.50573833803178,-36.2742356128027,-1.44018399272549));
#59157=CARTESIAN_POINT('Ctrl Pts',(3.58639477785833,-36.2742356128016,-1.3891592543171));
#59158=CARTESIAN_POINT('Ctrl Pts',(3.67575424130866,-36.2742356128003,-1.33262882405423));
#59159=CARTESIAN_POINT('Ctrl Pts',(3.76418511993075,-36.2742356128,-1.27473314069746));
#59160=CARTESIAN_POINT('Ctrl Pts',(3.85134110464983,-36.2742356128,-1.21534305390097));
#59161=CARTESIAN_POINT('Ctrl Pts',(3.86555391974856,-36.2742356128,-1.2056581157403));
#59162=CARTESIAN_POINT('Ctrl Pts',(3.87973273588502,-36.2742356128,-1.19593337885312));
#59163=CARTESIAN_POINT('Ctrl Pts',(3.89387594729535,-36.2742356128,-1.18616822317099));
#59164=CARTESIAN_POINT('Ctrl Pts',(4.00029785279444,-36.2742356128,-1.11268940389601));
#59165=CARTESIAN_POINT('Ctrl Pts',(4.10478398479914,-36.2742356128,-1.03687102559339));
#59166=CARTESIAN_POINT('Ctrl Pts',(4.20661656305114,-36.2742356128,-0.958414504056867));
#59167=CARTESIAN_POINT('Ctrl Pts',(4.30226608179997,-36.2742356128,-0.884721697133083));
#59168=CARTESIAN_POINT('Ctrl Pts',(4.39557138891166,-36.2742356128,-0.808698586640645));
#59169=CARTESIAN_POINT('Ctrl Pts',(4.48591276345593,-36.2742356128,-0.730108100871267));
#59170=CARTESIAN_POINT('Ctrl Pts',(4.52584144204364,-36.2742356128,-0.695373027797972));
#59171=CARTESIAN_POINT('Ctrl Pts',(4.56519106650209,-36.2742356128,-0.660136818345033));
#59172=CARTESIAN_POINT('Ctrl Pts',(4.60390869426853,-36.2742356128,-0.62438174071118));
#59173=CARTESIAN_POINT('Ctrl Pts',(4.6414702406575,-36.2742356128,-0.589694284772853));
#59174=CARTESIAN_POINT('Ctrl Pts',(4.67843073789759,-36.2742356128,-0.554524122905242));
#59175=CARTESIAN_POINT('Ctrl Pts',(4.71474137816731,-36.2742356128,-0.518860225151488));
#59176=CARTESIAN_POINT('Ctrl Pts',(4.78288652012131,-36.2742356128,-0.451928842035981));
#59177=CARTESIAN_POINT('Ctrl Pts',(4.84874492792749,-36.2742356128,-0.38325236142979));
#59178=CARTESIAN_POINT('Ctrl Pts',(4.91203343390612,-36.2742356128,-0.31276532051731));
#59179=CARTESIAN_POINT('Ctrl Pts',(4.97022521348273,-36.2742356128,-0.247954715742227));
#59180=CARTESIAN_POINT('Ctrl Pts',(5.02624407407463,-36.2742356128,-0.181613289617387));
#59181=CARTESIAN_POINT('Ctrl Pts',(5.07989426308131,-36.2742356128,-0.113725674955232));
#59182=CARTESIAN_POINT('Ctrl Pts',(5.12228748281073,-36.2742356128,-0.0600823492081344));
#59183=CARTESIAN_POINT('Ctrl Pts',(5.16320211219051,-36.2742356128,-0.00547418087444934));
#59184=CARTESIAN_POINT('Ctrl Pts',(5.20255537839219,-36.2742356128,0.050087718179765));
#59185=CARTESIAN_POINT('Ctrl Pts',(5.24837168523952,-36.2742356128,0.114774623786097));
#59186=CARTESIAN_POINT('Ctrl Pts',(5.29207438973777,-36.2742356128,0.180759277690909));
#59187=CARTESIAN_POINT('Ctrl Pts',(5.3336564943449,-36.2742356128,0.248044031897748));
#59188=CARTESIAN_POINT('Ctrl Pts',(5.37190124235283,-36.2742356128,0.309928549137294));
#59189=CARTESIAN_POINT('Ctrl Pts',(5.4083506840884,-36.2742356128,0.372912084581407));
#59190=CARTESIAN_POINT('Ctrl Pts',(5.44302947502448,-36.2742356128,0.436970376903849));
#59191=CARTESIAN_POINT('Ctrl Pts',(5.47645187793625,-36.2742356128,0.498707882683309));
#59192=CARTESIAN_POINT('Ctrl Pts',(5.50822844774793,-36.2742356128,0.561443272406974));
#59193=CARTESIAN_POINT('Ctrl Pts',(5.53842875337963,-36.2742356128,0.625137406042214));
#59194=CARTESIAN_POINT('Ctrl Pts',(5.56568797441512,-36.2742356128,0.682628627773582));
#59195=CARTESIAN_POINT('Ctrl Pts',(5.59166287037293,-36.2742356128,0.740900588750238));
#59196=CARTESIAN_POINT('Ctrl Pts',(5.61645139047291,-36.2742356128,0.799915459049706));
#59197=CARTESIAN_POINT('Ctrl Pts',(5.61912590323811,-36.2742356128,0.80628276227378));
#59198=CARTESIAN_POINT('Ctrl Pts',(5.62178665546896,-36.2742356128,0.812658706960601));
#59199=CARTESIAN_POINT('Ctrl Pts',(5.62443380765283,-36.2742356128,0.819043240976538));
#59200=CARTESIAN_POINT('Ctrl Pts',(5.63821488896908,-36.2742356128,0.852281142059808));
#59201=CARTESIAN_POINT('Ctrl Pts',(5.65162223151371,-36.2742356127983,0.885738848242016));
#59202=CARTESIAN_POINT('Ctrl Pts',(5.66468821373837,-36.2742356128112,0.919432993579274));
#59203=CARTESIAN_POINT('Ctrl Pts',(5.6830074126935,-36.2742356128293,0.966673969530669));
#59204=CARTESIAN_POINT('Ctrl Pts',(5.70065416799746,-36.27423561289,1.01437731418511));
#59205=CARTESIAN_POINT('Ctrl Pts',(5.71770208500406,-36.2742356129396,1.06248232003904));
#59206=CARTESIAN_POINT('Ctrl Pts',(5.73056789567574,-36.274235612977,1.09878645604799));
#59207=CARTESIAN_POINT('Ctrl Pts',(5.74309182301036,-36.2742356129966,1.13531530657873));
#59208=CARTESIAN_POINT('Ctrl Pts',(5.75531496840173,-36.2742356129631,1.17205239280299));
#59209=CARTESIAN_POINT('Ctrl Pts',(5.76290164272989,-36.2742356129423,1.19485440488948));
#59210=CARTESIAN_POINT('Ctrl Pts',(5.77037267378017,-36.2742356129007,1.21773704710012));
#59211=CARTESIAN_POINT('Ctrl Pts',(5.77774191173509,-36.2742356128602,1.24070637318723));
#59212=CARTESIAN_POINT('Ctrl Pts',(5.78763874363087,-36.2742356128057,1.27155400769627));
#59213=CARTESIAN_POINT('Ctrl Pts',(5.79735016193852,-36.2742356128004,1.30254774097663));
#59214=CARTESIAN_POINT('Ctrl Pts',(5.80690585556745,-36.2742356128,1.33367294521436));
#59215=CARTESIAN_POINT('Ctrl Pts',(5.80850125226195,-36.2742356128,1.3388695379354));
#59216=CARTESIAN_POINT('Ctrl Pts',(5.81009235283591,-36.2742356128,1.34406990458954));
#59217=CARTESIAN_POINT('Ctrl Pts',(5.81167935047957,-36.2742356128,1.34927411502766));
#59218=CARTESIAN_POINT('Ctrl Pts',(5.81722554825276,-36.2742356128,1.36746165327525));
#59219=CARTESIAN_POINT('Ctrl Pts',(5.8227208660317,-36.2742356128002,1.3856941788767));
#59220=CARTESIAN_POINT('Ctrl Pts',(5.82817327291951,-36.2742356128001,1.4039704504895));
#59221=CARTESIAN_POINT('Ctrl Pts',(5.83362567980732,-36.2742356127999,1.42224672210229));
#59222=CARTESIAN_POINT('Ctrl Pts',(5.83903086091247,-36.2742356128,1.44055010200303));
#59223=CARTESIAN_POINT('Ctrl Pts',(5.84436868428059,-36.2742356128,1.45878260789149));
#59224=CARTESIAN_POINT('Ctrl Pts',(5.85055639832583,-36.2742356128,1.47991810170344));
#59225=CARTESIAN_POINT('Ctrl Pts',(5.85665292951415,-36.2742356128,1.50095559806678));
#59226=CARTESIAN_POINT('Ctrl Pts',(5.86265812636259,-36.2742356128,1.52184723319947));
#59227=CARTESIAN_POINT('Ctrl Pts',(5.86821793006266,-36.2742356128,1.5411893785517));
#59228=CARTESIAN_POINT('Ctrl Pts',(5.873699232103,-36.2742356128,1.56040582099944));
#59229=CARTESIAN_POINT('Ctrl Pts',(5.87911331224062,-36.2742356128,1.57949901445499));
#59230=CARTESIAN_POINT('Ctrl Pts',(5.88408849546304,-36.2742356128,1.59704440228229));
#59231=CARTESIAN_POINT('Ctrl Pts',(5.88900683553615,-36.2742356128,1.61448547798691));
#59232=CARTESIAN_POINT('Ctrl Pts',(5.89388893987974,-36.2742356128,1.63186539882874));
#59233=CARTESIAN_POINT('Ctrl Pts',(5.89775638947452,-36.2742356128,1.64563322579158));
#59234=CARTESIAN_POINT('Ctrl Pts',(5.9016012789473,-36.2742356128,1.65936330446299));
#59235=CARTESIAN_POINT('Ctrl Pts',(5.90544038108676,-36.2742356128,1.67309959908521));
#59236=CARTESIAN_POINT('Ctrl Pts',(5.91404763889229,-36.2742356128,1.70389633874233));
#59237=CARTESIAN_POINT('Ctrl Pts',(5.92261916147267,-36.2742356128,1.73470121369864));
#59238=CARTESIAN_POINT('Ctrl Pts',(5.93129769863563,-36.2742356128,1.76582075309313));
#59239=CARTESIAN_POINT('Ctrl Pts',(5.93719226432172,-36.2742356128,1.78695751446628));
#59240=CARTESIAN_POINT('Ctrl Pts',(5.94313728997873,-36.2742356128,1.80824316276458));
#59241=CARTESIAN_POINT('Ctrl Pts',(5.94917528826636,-36.2742356128,1.82976108353145));
#59242=CARTESIAN_POINT('Ctrl Pts',(5.95444651401515,-36.2742356128,1.84854641810812));
#59243=CARTESIAN_POINT('Ctrl Pts',(5.9597888214508,-36.2742356128,1.86750955556035));
#59244=CARTESIAN_POINT('Ctrl Pts',(5.96522247846992,-36.2742356128,1.88667386362928));
#59245=CARTESIAN_POINT('Ctrl Pts',(5.97042798694682,-36.2742356128,1.90503350019741));
#59246=CARTESIAN_POINT('Ctrl Pts',(5.97571464628148,-36.2742356128,1.923568373342));
#59247=CARTESIAN_POINT('Ctrl Pts',(5.98109356255906,-36.2742356128,1.94227142362813));
#59248=CARTESIAN_POINT('Ctrl Pts',(5.98616571138456,-36.2742356128,1.95990781163764));
#59249=CARTESIAN_POINT('Ctrl Pts',(5.9913199976955,-36.2742356128,1.97769414502198));
#59250=CARTESIAN_POINT('Ctrl Pts',(5.99655425212487,-36.2742356128,1.99557925311492));
#59251=CARTESIAN_POINT('Ctrl Pts',(5.99687082384823,-36.2742356128,1.99666095817301));
#59252=CARTESIAN_POINT('Ctrl Pts',(5.99718768412742,-36.2742356128,1.99774300894027));
#59253=CARTESIAN_POINT('Ctrl Pts',(5.99750483090687,-36.2742356128,1.99882538789166));
#59254=CARTESIAN_POINT('Ctrl Pts',(6.00306576003192,-36.2742356128,2.01780408490275));
#59255=CARTESIAN_POINT('Ctrl Pts',(6.00871842800908,-36.2742356127999,2.03689599014484));
#59256=CARTESIAN_POINT('Ctrl Pts',(6.01445248808947,-36.2742356128001,2.0560106258512));
#59257=CARTESIAN_POINT('Ctrl Pts',(6.02403404969531,-36.2742356128006,2.08795100614474));
#59258=CARTESIAN_POINT('Ctrl Pts',(6.033867889391,-36.274235612802,2.12004423096413));
#59259=CARTESIAN_POINT('Ctrl Pts',(6.04400556249464,-36.2742356128029,2.15218869532583));
#59260=CARTESIAN_POINT('Ctrl Pts',(6.05513800463166,-36.274235612804,2.18748736651728));
#59261=CARTESIAN_POINT('Ctrl Pts',(6.06663691963859,-36.2742356128046,2.22284858676531));
#59262=CARTESIAN_POINT('Ctrl Pts',(6.07859889464087,-36.2742356128046,2.25819895240145));
#59263=CARTESIAN_POINT('Ctrl Pts',(6.09350733550585,-36.2742356128046,2.30225679699158));
#59264=CARTESIAN_POINT('Ctrl Pts',(6.10913487702226,-36.2742356128037,2.34629959452671));
#59265=CARTESIAN_POINT('Ctrl Pts',(6.12571299890265,-36.2742356128028,2.3902587946028));
#59266=CARTESIAN_POINT('Ctrl Pts',(6.14230562759224,-36.2742356128019,2.43425646150481));
#59267=CARTESIAN_POINT('Ctrl Pts',(6.15985227139991,-36.274235612801,2.47817620018358));
#59268=CARTESIAN_POINT('Ctrl Pts',(6.17860954326941,-36.2742356128006,2.52194911231665));
#59269=CARTESIAN_POINT('Ctrl Pts',(6.19307525815561,-36.2742356128002,2.55570703143523));
#59270=CARTESIAN_POINT('Ctrl Pts',(6.20826173241701,-36.2742356128001,2.58937838989207));
#59271=CARTESIAN_POINT('Ctrl Pts',(6.22428655479659,-36.2742356128,2.62289850029955));
#59272=CARTESIAN_POINT('Ctrl Pts',(6.23622615528486,-36.2742356128,2.64787329983915));
#59273=CARTESIAN_POINT('Ctrl Pts',(6.24863117121475,-36.2742356128,2.6727636320365));
#59274=CARTESIAN_POINT('Ctrl Pts',(6.26154754770469,-36.2742356128,2.69752366658337));
#59275=CARTESIAN_POINT('Ctrl Pts',(6.26508870643922,-36.2742356128,2.70431188715524));
#59276=CARTESIAN_POINT('Ctrl Pts',(6.26866844515828,-36.2742356128,2.71109052393618));
#59277=CARTESIAN_POINT('Ctrl Pts',(6.27228786163123,-36.2742356128,2.71785869834249));
#59278=CARTESIAN_POINT('Ctrl Pts',(6.27317711432132,-36.2742356128,2.71952156785276));
#59279=CARTESIAN_POINT('Ctrl Pts',(6.27406873921778,-36.2742356128,2.72118376295094));
#59280=CARTESIAN_POINT('Ctrl Pts',(6.27496287808,-36.2742356128,2.72284550202));
#59281=CARTESIAN_POINT('',(1.05996676265,-36.2742356128,-2.50526930112));
#59282=CARTESIAN_POINT('Origin',(0.442943622457021,-36.2742356127953,1.44025631334163));
#59283=CARTESIAN_POINT('',(0.417273426056,-36.2742356128,-3.28965091665));
#59284=CARTESIAN_POINT('Ctrl Pts',(0.417273426056,-36.2742356128,-3.28965091665));
#59285=CARTESIAN_POINT('Ctrl Pts',(0.417273426056,-36.2742356128,-3.24819118647009));
#59286=CARTESIAN_POINT('Ctrl Pts',(0.420519754893996,-36.2742356128,-3.20677004886387));
#59287=CARTESIAN_POINT('Ctrl Pts',(0.426943681519379,-36.2742356128,-3.16585830441977));
#59288=CARTESIAN_POINT('Ctrl Pts',(0.433369261721254,-36.2742356128,-3.12493602892469));
#59289=CARTESIAN_POINT('Ctrl Pts',(0.442974473167372,-36.2742356128,-3.08452446703945));
#59290=CARTESIAN_POINT('Ctrl Pts',(0.455636754962494,-36.2742356128,-3.0450968409));
#59291=CARTESIAN_POINT('Ctrl Pts',(0.467430703587185,-36.2742356128,-3.00837301776875));
#59292=CARTESIAN_POINT('Ctrl Pts',(0.481876462427866,-36.2742356128,-2.97250363953337));
#59293=CARTESIAN_POINT('Ctrl Pts',(0.498828968976865,-36.2742356128,-2.93785972150366));
#59294=CARTESIAN_POINT('Ctrl Pts',(0.515153014164737,-36.2742356128,-2.90450011879433));
#59295=CARTESIAN_POINT('Ctrl Pts',(0.53380145888552,-36.2742356128,-2.8722773944409));
#59296=CARTESIAN_POINT('Ctrl Pts',(0.554600533471897,-36.2742356128,-2.84150610599439));
#59297=CARTESIAN_POINT('Ctrl Pts',(0.574684449539934,-36.2742356128,-2.81179286217199));
#59298=CARTESIAN_POINT('Ctrl Pts',(0.596772989945446,-36.2742356128,-2.78343431295931));
#59299=CARTESIAN_POINT('Ctrl Pts',(0.620667862166697,-36.2742356128,-2.75668878505484));
#59300=CARTESIAN_POINT('Ctrl Pts',(0.629100264263006,-36.2742356128,-2.74725039829636));
#59301=CARTESIAN_POINT('Ctrl Pts',(0.637757237276887,-36.2742356128,-2.73801262565806));
#59302=CARTESIAN_POINT('Ctrl Pts',(0.646628795601126,-36.2742356128,-2.72898588795116));
#59303=CARTESIAN_POINT('Ctrl Pts',(0.673012364687384,-36.2742356128,-2.70214082317122));
#59304=CARTESIAN_POINT('Ctrl Pts',(0.701296621816972,-36.2742356127994,
-2.67716443387045));
#59305=CARTESIAN_POINT('Ctrl Pts',(0.731194309592696,-36.2742356128018,
-2.65430179476602));
#59306=CARTESIAN_POINT('Ctrl Pts',(0.742439371406182,-36.2742356128027,
-2.64570274216111));
#59307=CARTESIAN_POINT('Ctrl Pts',(0.753912541590767,-36.274235612804,-2.63740218614734));
#59308=CARTESIAN_POINT('Ctrl Pts',(0.765597959533844,-36.2742356128064,
-2.62941138371186));
#59309=CARTESIAN_POINT('Ctrl Pts',(0.797606714508346,-36.2742356128127,
-2.60752293791959));
#59310=CARTESIAN_POINT('Ctrl Pts',(0.83120590246872,-36.2742356128134,-2.58796315035183));
#59311=CARTESIAN_POINT('Ctrl Pts',(0.866047905424978,-36.2742356128085,
-2.5709319957786));
#59312=CARTESIAN_POINT('Ctrl Pts',(0.877736613138201,-36.2742356128068,
-2.56521842678329));
#59313=CARTESIAN_POINT('Ctrl Pts',(0.889564957491781,-36.2742356128049,
-2.55978907221658));
#59314=CARTESIAN_POINT('Ctrl Pts',(0.901519043131815,-36.2742356128032,
-2.55465043725105));
#59315=CARTESIAN_POINT('Ctrl Pts',(0.940012174823359,-36.274235612798,-2.53810361314431));
#59316=CARTESIAN_POINT('Ctrl Pts',(0.979809990161025,-36.2742356128,-2.52457520198315));
#59317=CARTESIAN_POINT('Ctrl Pts',(1.02045143135846,-36.2742356128,-2.51424729380737));
#59318=CARTESIAN_POINT('Ctrl Pts',(1.03008167823426,-36.2742356128,-2.51180003055801));
#59319=CARTESIAN_POINT('Ctrl Pts',(1.03975907726387,-36.2742356128,-2.50953240002355));
#59320=CARTESIAN_POINT('Ctrl Pts',(1.04947705709931,-36.2742356128,-2.50744672775021));
#59321=CARTESIAN_POINT('Ctrl Pts',(1.05296820937862,-36.2742356128,-2.50669745684882));
#59322=CARTESIAN_POINT('Ctrl Pts',(1.05646717145,-36.2742356128,-2.50597114875333));
#59323=CARTESIAN_POINT('Ctrl Pts',(1.05996676265,-36.2742356128,-2.50526930112));
#59324=CARTESIAN_POINT('',(0.417273580719025,-36.2742356128,-7.9503178894794));
#59325=CARTESIAN_POINT('',(0.417273426056,-36.2742356128,0.915007091638));
#59326=CARTESIAN_POINT('',(2.08574076971679,-36.2742356128,-9.317281773533));
#59327=CARTESIAN_POINT('Ctrl Pts',(2.08574076953038,-36.2742356128,-9.31728177257901));
#59328=CARTESIAN_POINT('Ctrl Pts',(2.03330044437365,-36.2742356128,-9.32752871414683));
#59329=CARTESIAN_POINT('Ctrl Pts',(1.98026066869069,-36.2742356128,-9.3347827687861));
#59330=CARTESIAN_POINT('Ctrl Pts',(1.92697417280592,-36.2742356128,-9.33898117872619));
#59331=CARTESIAN_POINT('Ctrl Pts',(1.87250923120824,-36.2742356128,-9.34327243767263));
#59332=CARTESIAN_POINT('Ctrl Pts',(1.81778687287914,-36.2742356128,-9.34437149963258));
#59333=CARTESIAN_POINT('Ctrl Pts',(1.76318602342788,-36.2742356128,-9.34226540624991));
#59334=CARTESIAN_POINT('Ctrl Pts',(1.75574898470314,-36.2742356128,-9.34197854078531));
#59335=CARTESIAN_POINT('Ctrl Pts',(1.74831419900645,-36.2742356128,-9.34163229076523));
#59336=CARTESIAN_POINT('Ctrl Pts',(1.74088262153701,-36.2742356128,-9.34122669715811));
#59337=CARTESIAN_POINT('Ctrl Pts',(1.68259407240854,-36.2742356128,-9.33804547984701));
#59338=CARTESIAN_POINT('Ctrl Pts',(1.62450457226369,-36.2742356128,-9.33120851843907));
#59339=CARTESIAN_POINT('Ctrl Pts',(1.56707106712167,-36.2742356128,-9.32077143204654));
#59340=CARTESIAN_POINT('Ctrl Pts',(1.51078881778076,-36.2742356128,-9.3105435572671));
#59341=CARTESIAN_POINT('Ctrl Pts',(1.45513695060325,-36.2742356128,-9.29685901434515));
#59342=CARTESIAN_POINT('Ctrl Pts',(1.40053396527419,-36.2742356128,-9.27982447959625));
#59343=CARTESIAN_POINT('Ctrl Pts',(1.3442556203685,-36.2742356128,-9.26226728164948));
#59344=CARTESIAN_POINT('Ctrl Pts',(1.28909210804698,-36.2742356128,-9.24115151949635));
#59345=CARTESIAN_POINT('Ctrl Pts',(1.23548138966384,-36.2742356128,-9.21664740185734));
#59346=CARTESIAN_POINT('Ctrl Pts',(1.1818706712807,-36.2742356128,-9.19214328421834));
#59347=CARTESIAN_POINT('Ctrl Pts',(1.12981326798746,-36.2742356128,-9.1642512489844));
#59348=CARTESIAN_POINT('Ctrl Pts',(1.07971883490905,-36.2742356128,-9.13318920782522));
#59349=CARTESIAN_POINT('Ctrl Pts',(1.02860460246243,-36.2742356128,-9.10149481995598));
#59350=CARTESIAN_POINT('Ctrl Pts',(0.979533727061269,-36.2742356127831,
-9.06649723223452));
#59351=CARTESIAN_POINT('Ctrl Pts',(0.932909924660566,-36.2742356128878,
-9.02849863344844));
#59352=CARTESIAN_POINT('Ctrl Pts',(0.887156901283107,-36.2742356129905,
-8.99120972329846));
#59353=CARTESIAN_POINT('Ctrl Pts',(0.843760705446356,-36.2742356132368,
-8.95103091589256));
#59354=CARTESIAN_POINT('Ctrl Pts',(0.803067537737909,-36.2742356136497,
-8.90828164242417));
#59355=CARTESIAN_POINT('Ctrl Pts',(0.763525064799684,-36.2742356140509,
-8.86674120493933));
#59356=CARTESIAN_POINT('Ctrl Pts',(0.726535097662597,-36.2742356146066,
-8.82277372740761));
#59357=CARTESIAN_POINT('Ctrl Pts',(0.692378156264808,-36.2742356150751,
-8.77670324089393));
#59358=CARTESIAN_POINT('Ctrl Pts',(0.658532619600355,-36.2742356155394,
-8.73105277347389));
#59359=CARTESIAN_POINT('Ctrl Pts',(0.627468960880158,-36.2742356158936,
-8.6833374757917));
#59360=CARTESIAN_POINT('Ctrl Pts',(0.599419561563431,-36.2742356158468,
-8.63390270394093));
#59361=CARTESIAN_POINT('Ctrl Pts',(0.570615857250581,-36.2742356157988,
-8.58313853123675));
#59362=CARTESIAN_POINT('Ctrl Pts',(0.544992286373528,-36.2742356148864,
-8.53056909660664));
#59363=CARTESIAN_POINT('Ctrl Pts',(0.522753564674736,-36.2742356141856,
-8.4765995297206));
#59364=CARTESIAN_POINT('Ctrl Pts',(0.502029446455075,-36.2742356135326,
-8.42630564594621));
#59365=CARTESIAN_POINT('Ctrl Pts',(0.484244625968573,-36.2742356131106,
-8.37479614579619));
#59366=CARTESIAN_POINT('Ctrl Pts',(0.469521955598608,-36.2742356129622,
-8.32242775617462));
#59367=CARTESIAN_POINT('Ctrl Pts',(0.468445962520008,-36.2742356129513,
-8.31860045967512));
#59368=CARTESIAN_POINT('Ctrl Pts',(0.467386305746146,-36.2742356129416,
-8.31476858813491));
#59369=CARTESIAN_POINT('Ctrl Pts',(0.466343023886594,-36.2742356129328,
-8.31093228675359));
#59370=CARTESIAN_POINT('Ctrl Pts',(0.450543397904615,-36.2742356128,-8.25283473006365));
#59371=CARTESIAN_POINT('Ctrl Pts',(0.438503293447399,-36.2742356128062,
-8.19372526762956));
#59372=CARTESIAN_POINT('Ctrl Pts',(0.430309059876441,-36.2742356128021,
-8.13408616006745));
#59373=CARTESIAN_POINT('Ctrl Pts',(0.422791149948173,-36.2742356127983,
-8.07936945777046));
#59374=CARTESIAN_POINT('Ctrl Pts',(0.41851018184678,-36.2742356128,-8.0242069294277));
#59375=CARTESIAN_POINT('Ctrl Pts',(0.417493303474974,-36.2742356128,-7.9690017292704));
#59376=CARTESIAN_POINT('Ctrl Pts',(0.417401823410547,-36.2742356128,-7.96403537792779));
#59377=CARTESIAN_POINT('Ctrl Pts',(0.417336732786752,-36.2742356128,-7.95906870352496));
#59378=CARTESIAN_POINT('Ctrl Pts',(0.417298034990758,-36.2742356128,-7.95410201315234));
#59379=CARTESIAN_POINT('Ctrl Pts',(0.417288206348154,-36.2742356128,-7.95284055049421));
#59380=CARTESIAN_POINT('Ctrl Pts',(0.417280080432586,-36.2742356128,-7.9515790775042));
#59381=CARTESIAN_POINT('Ctrl Pts',(0.417273658050834,-36.2742356128,-7.95031788947841));
#59382=CARTESIAN_POINT('',(2.11953888391737,-36.2742356128,-9.31090074964532));
#59383=CARTESIAN_POINT('Origin',(2.09997707267667,-36.2742356127977,-9.34384840219991));
#59384=CARTESIAN_POINT('Ctrl Pts',(10.3535102269266,-36.2742356128,0.692259222255781));
#59385=CARTESIAN_POINT('Ctrl Pts',(10.3562093920332,-36.2742356128,0.675037953476251));
#59386=CARTESIAN_POINT('Ctrl Pts',(10.3588778370901,-36.2742356128,0.657806411951718));
#59387=CARTESIAN_POINT('Ctrl Pts',(10.3615152739502,-36.2742356128,0.640566949063097));
#59388=CARTESIAN_POINT('Ctrl Pts',(10.3727685745492,-36.2742356128,0.56701036047497));
#59389=CARTESIAN_POINT('Ctrl Pts',(10.3834624844301,-36.2742356128,0.493289697396397));
#59390=CARTESIAN_POINT('Ctrl Pts',(10.3935931754126,-36.2742356128,0.419366129654924));
#59391=CARTESIAN_POINT('Ctrl Pts',(10.4061289190632,-36.2742356128,0.327892912621584));
#59392=CARTESIAN_POINT('Ctrl Pts',(10.4178057955057,-36.2742356127957,0.236089364064904));
#59393=CARTESIAN_POINT('Ctrl Pts',(10.428558083588,-36.2742356128043,0.143938604015692));
#59394=CARTESIAN_POINT('Ctrl Pts',(10.4400001246915,-36.2742356128135,0.0458764263548748));
#59395=CARTESIAN_POINT('Ctrl Pts',(10.4503948687392,-36.2742356127897,-0.0525792420430679));
#59396=CARTESIAN_POINT('Ctrl Pts',(10.4596079894754,-36.2742356131329,-0.151426466320893));
#59397=CARTESIAN_POINT('Ctrl Pts',(10.4695724147274,-36.2742356135041,-0.25833440836185));
#59398=CARTESIAN_POINT('Ctrl Pts',(10.4781541249895,-36.2742356141501,-0.365700880393748));
#59399=CARTESIAN_POINT('Ctrl Pts',(10.4851266846754,-36.2742356175533,-0.473491504220951));
#59400=CARTESIAN_POINT('Ctrl Pts',(10.4918461373707,-36.2742356208329,-0.577369280882969));
#59401=CARTESIAN_POINT('Ctrl Pts',(10.4970697073588,-36.2742356265035,-0.681640880070512));
#59402=CARTESIAN_POINT('Ctrl Pts',(10.5005608005868,-36.2742356409383,-0.786244887940372));
#59403=CARTESIAN_POINT('Ctrl Pts',(10.5045127180508,-36.2742356572785,-0.904656622749569));
#59404=CARTESIAN_POINT('Ctrl Pts',(10.5062623540639,-36.2742356782692,-1.02352896187271));
#59405=CARTESIAN_POINT('Ctrl Pts',(10.5054484661738,-36.2742356903982,-1.14275590241697));
#59406=CARTESIAN_POINT('Ctrl Pts',(10.5046492533298,-36.2742357023086,-1.2598330863741));
#59407=CARTESIAN_POINT('Ctrl Pts',(10.501376236877,-36.2742357042772,-1.37725221277007));
#59408=CARTESIAN_POINT('Ctrl Pts',(10.4952861980909,-36.2742356908098,-1.4948647931778));
#59409=CARTESIAN_POINT('Ctrl Pts',(10.4934120668053,-36.2742356866653,-1.53105855552529));
#59410=CARTESIAN_POINT('Ctrl Pts',(10.4912712575296,-36.2742356811994,-1.56727028837258));
#59411=CARTESIAN_POINT('Ctrl Pts',(10.4888541645596,-36.2742356747649,-1.60349471863259));
#59412=CARTESIAN_POINT('Ctrl Pts',(10.4818861663663,-36.2742356562156,-1.70792254484433));
#59413=CARTESIAN_POINT('Ctrl Pts',(10.4726172291219,-36.2742356337617,-1.81245827726364));
#59414=CARTESIAN_POINT('Ctrl Pts',(10.4608100921849,-36.2742356232957,-1.91693269295077));
#59415=CARTESIAN_POINT('Ctrl Pts',(10.4571364571787,-36.2742356200393,-1.94943853012084));
#59416=CARTESIAN_POINT('Ctrl Pts',(10.4532173571464,-36.2742356177031,-1.98193815780485));
#59417=CARTESIAN_POINT('Ctrl Pts',(10.449046400631,-36.274235616125,-2.01442572802847));
#59418=CARTESIAN_POINT('Ctrl Pts',(10.4365783728994,-36.2742356114077,-2.11153916591473));
#59419=CARTESIAN_POINT('Ctrl Pts',(10.421841819238,-36.2742356128118,-2.20856774744078));
#59420=CARTESIAN_POINT('Ctrl Pts',(10.4047260362417,-36.274235612802,-2.3053166118921));
#59421=CARTESIAN_POINT('Ctrl Pts',(10.397713265999,-36.274235612798,-2.34495707460304));
#59422=CARTESIAN_POINT('Ctrl Pts',(10.3903015981004,-36.2742356128,-2.38455030881704));
#59423=CARTESIAN_POINT('Ctrl Pts',(10.3824857480538,-36.2742356128,-2.42408179319258));
#59424=CARTESIAN_POINT('Ctrl Pts',(10.3633959928289,-36.2742356128,-2.52063512467945));
#59425=CARTESIAN_POINT('Ctrl Pts',(10.3418892837525,-36.2742356128,-2.61683237280929));
#59426=CARTESIAN_POINT('Ctrl Pts',(10.3179031203684,-36.2742356128,-2.71246883714195));
#59427=CARTESIAN_POINT('Ctrl Pts',(10.2957385119174,-36.2742356128,-2.80084248621773));
#59428=CARTESIAN_POINT('Ctrl Pts',(10.271456816493,-36.2742356128,-2.88873703944073));
#59429=CARTESIAN_POINT('Ctrl Pts',(10.2450543902945,-36.2742356128,-2.97597002930809));
#59430=CARTESIAN_POINT('Ctrl Pts',(10.2428845586102,-36.2742356128,-2.98313910172208));
#59431=CARTESIAN_POINT('Ctrl Pts',(10.2407004304474,-36.2742356128,-2.99030369449288));
#59432=CARTESIAN_POINT('Ctrl Pts',(10.2385020185913,-36.2742356128,-2.99746370019166));
#59433=CARTESIAN_POINT('Ctrl Pts',(10.2115899242788,-36.2742356128,-3.08511367720213));
#59434=CARTESIAN_POINT('Ctrl Pts',(10.1825218137777,-36.2742356128,-3.17211436346743));
#59435=CARTESIAN_POINT('Ctrl Pts',(10.1513609907264,-36.2742356128,-3.25830680597497));
#59436=CARTESIAN_POINT('Ctrl Pts',(10.1191814800406,-36.2742356128,-3.34731699098008));
#59437=CARTESIAN_POINT('Ctrl Pts',(10.0847703883543,-36.2742356128,-3.43546527477735));
#59438=CARTESIAN_POINT('Ctrl Pts',(10.0482313430007,-36.2742356128,-3.52262013151324));
#59439=CARTESIAN_POINT('Ctrl Pts',(10.0440330941911,-36.2742356128,-3.53263401583891));
#59440=CARTESIAN_POINT('Ctrl Pts',(10.0398067869187,-36.2742356128,-3.5426348306343));
#59441=CARTESIAN_POINT('Ctrl Pts',(10.0355526038407,-36.2742356128,-3.55262241101358));
#59442=CARTESIAN_POINT('Ctrl Pts',(9.99574377590588,-36.2742356128,-3.64608192169306));
#59443=CARTESIAN_POINT('Ctrl Pts',(9.95348996234073,-36.2742356127974,-3.7383821453158));
#59444=CARTESIAN_POINT('Ctrl Pts',(9.90894409633191,-36.274235612804,-3.82944201792403));
#59445=CARTESIAN_POINT('Ctrl Pts',(9.86082512674903,-36.2742356128112,-3.9278059657568));
#59446=CARTESIAN_POINT('Ctrl Pts',(9.81003197512694,-36.274235612815,-4.02472257560848));
#59447=CARTESIAN_POINT('Ctrl Pts',(9.75678784892353,-36.2742356129677,-4.12014431547425));
#59448=CARTESIAN_POINT('Ctrl Pts',(9.70038315635778,-36.2742356131295,-4.22123028091305));
#59449=CARTESIAN_POINT('Ctrl Pts',(9.64122859138951,-36.2742356134239,-4.32063899789456));
#59450=CARTESIAN_POINT('Ctrl Pts',(9.57961405954658,-36.2742356145569,-4.418370168869));
#59451=CARTESIAN_POINT('Ctrl Pts',(9.51096163102881,-36.2742356158192,-4.52726464600931));
#59452=CARTESIAN_POINT('Ctrl Pts',(9.43925643293375,-36.2742356180243,-4.63407677905874));
#59453=CARTESIAN_POINT('Ctrl Pts',(9.36491343540478,-36.2742356238331,-4.73886931201533));
#59454=CARTESIAN_POINT('Ctrl Pts',(9.34738694186789,-36.2742356252025,-4.76357433754059));
#59455=CARTESIAN_POINT('Ctrl Pts',(9.32971384400554,-36.2742356267831,-4.78816734894402));
#59456=CARTESIAN_POINT('Ctrl Pts',(9.31189953928727,-36.2742356286321,-4.81264955991275));
#59457=CARTESIAN_POINT('Ctrl Pts',(9.23439860673501,-36.2742356366765,-4.91915914370095));
#59458=CARTESIAN_POINT('Ctrl Pts',(9.15429593033449,-36.2742356347254,-5.02353989346411));
#59459=CARTESIAN_POINT('Ctrl Pts',(9.07199160966919,-36.2742356291196,-5.12593022601556));
#59460=CARTESIAN_POINT('Ctrl Pts',(8.99453182595689,-36.2742356238438,-5.2222937334178));
#59461=CARTESIAN_POINT('Ctrl Pts',(8.91512306183019,-36.2742356177619,-5.31689571089193));
#59462=CARTESIAN_POINT('Ctrl Pts',(8.83405735451404,-36.2742356153905,-5.40985684740955));
#59463=CARTESIAN_POINT('Ctrl Pts',(8.82923042275601,-36.2742356152493,-5.41539207404207));
#59464=CARTESIAN_POINT('Ctrl Pts',(8.82439760074115,-36.2742356151174,-5.42092148120503));
#59465=CARTESIAN_POINT('Ctrl Pts',(8.81955894387271,-36.2742356149942,-5.42644509335966));
#59466=CARTESIAN_POINT('Ctrl Pts',(8.74513530805297,-36.2742356131003,-5.51140406246664));
#59467=CARTESIAN_POINT('Ctrl Pts',(8.66932164913453,-36.2742356129864,-5.59500897384072));
#59468=CARTESIAN_POINT('Ctrl Pts',(8.59233223129399,-36.274235612874,-5.67732225807105));
#59469=CARTESIAN_POINT('Ctrl Pts',(8.52142141683534,-36.2742356127705,-5.75313659969431));
#59470=CARTESIAN_POINT('Ctrl Pts',(8.44951333249385,-36.2742356128003,-5.82785570799169));
#59471=CARTESIAN_POINT('Ctrl Pts',(8.37673301404561,-36.2742356128001,-5.90151430451527));
#59472=CARTESIAN_POINT('Ctrl Pts',(8.34543794122704,-36.2742356127999,-5.93318703130553));
#59473=CARTESIAN_POINT('Ctrl Pts',(8.31398102395895,-36.2742356128,-5.96466344924576));
#59474=CARTESIAN_POINT('Ctrl Pts',(8.28236940694129,-36.2742356128,-5.99594511180429));
#59475=CARTESIAN_POINT('Ctrl Pts',(8.20001179535807,-36.2742356128,-6.07744309443625));
#59476=CARTESIAN_POINT('Ctrl Pts',(8.11660321287264,-36.2742356128,-6.15762467605));
#59477=CARTESIAN_POINT('Ctrl Pts',(8.0323151898841,-36.2742356128,-6.23653007960427));
#59478=CARTESIAN_POINT('Ctrl Pts',(7.94850474427214,-36.2742356128,-6.31498840379551));
#59479=CARTESIAN_POINT('Ctrl Pts',(7.86382513325578,-36.2742356128,-6.39218413842518));
#59480=CARTESIAN_POINT('Ctrl Pts',(7.77839945421262,-36.2742356128,-6.46813409547328));
#59481=CARTESIAN_POINT('Ctrl Pts',(7.69733765843861,-36.2742356128,-6.54020422679956));
#59482=CARTESIAN_POINT('Ctrl Pts',(7.61560400991131,-36.2742356128,-6.6111518590271));
#59483=CARTESIAN_POINT('Ctrl Pts',(7.53326120006503,-36.2742356128,-6.68098237572902));
#59484=CARTESIAN_POINT('Ctrl Pts',(7.44973420875221,-36.2742356128,-6.75181713316343));
#59485=CARTESIAN_POINT('Ctrl Pts',(7.36558032122966,-36.2742356128,-6.8215019053945));
#59486=CARTESIAN_POINT('Ctrl Pts',(7.28083955628857,-36.2742356128,-6.89002539244422));
#59487=CARTESIAN_POINT('Ctrl Pts',(7.23551914769524,-36.2742356128,-6.92667260035523));
#59488=CARTESIAN_POINT('Ctrl Pts',(7.1900300427837,-36.2742356128,-6.96298776645332));
#59489=CARTESIAN_POINT('Ctrl Pts',(7.14437232377622,-36.2742356128,-6.99897053618122));
#59490=CARTESIAN_POINT('Ctrl Pts',(7.06326365371102,-36.2742356128,-7.06289213939169));
#59491=CARTESIAN_POINT('Ctrl Pts',(6.98159496509443,-36.2742356128,-7.12578783863602));
#59492=CARTESIAN_POINT('Ctrl Pts',(6.89932083587377,-36.2742356128,-7.18767259991881));
#59493=CARTESIAN_POINT('Ctrl Pts',(6.84868300071105,-36.2742356128,-7.22576124784017));
#59494=CARTESIAN_POINT('Ctrl Pts',(6.79781491836607,-36.2742356128,-7.26346724760522));
#59495=CARTESIAN_POINT('Ctrl Pts',(6.74669690171385,-36.2742356128,-7.30079801871496));
#59496=CARTESIAN_POINT('Ctrl Pts',(6.63653183176793,-36.2742356128,-7.38125002526323));
#59497=CARTESIAN_POINT('Ctrl Pts',(6.52520299962451,-36.2742356128,-7.45996077864774));
#59498=CARTESIAN_POINT('Ctrl Pts',(6.41266159909594,-36.2742356128,-7.53683581128796));
#59499=CARTESIAN_POINT('Ctrl Pts',(6.29028365174599,-36.2742356128,-7.62043001442375));
#59500=CARTESIAN_POINT('Ctrl Pts',(6.16647232408381,-36.2742356128,-7.70185249404446));
#59501=CARTESIAN_POINT('Ctrl Pts',(6.04121534251757,-36.2742356128,-7.78095113049375));
#59502=CARTESIAN_POINT('Ctrl Pts',(5.89675184985328,-36.2742356128,-7.87217850276126));
#59503=CARTESIAN_POINT('Ctrl Pts',(5.75036379756427,-36.2742356128,-7.9603131905575));
#59504=CARTESIAN_POINT('Ctrl Pts',(5.60211169574243,-36.2742356128,-8.04509917799797));
#59505=CARTESIAN_POINT('Ctrl Pts',(5.4664708448076,-36.2742356128,-8.12267273913099));
#59506=CARTESIAN_POINT('Ctrl Pts',(5.3292712661405,-36.2742356128,-8.19744131634106));
#59507=CARTESIAN_POINT('Ctrl Pts',(5.19057678671885,-36.2742356128,-8.26924053097918));
#59508=CARTESIAN_POINT('Ctrl Pts',(5.14691539854509,-36.2742356128,-8.29184311324459));
#59509=CARTESIAN_POINT('Ctrl Pts',(5.10310589926147,-36.2742356128,-8.31415178850976));
#59510=CARTESIAN_POINT('Ctrl Pts',(5.05915024981415,-36.2742356128,-8.33616259114357));
#59511=CARTESIAN_POINT('Ctrl Pts',(4.9149063727951,-36.2742356128,-8.40839274922615));
#59512=CARTESIAN_POINT('Ctrl Pts',(4.76907703785031,-36.2742356128,-8.4774166113732));
#59513=CARTESIAN_POINT('Ctrl Pts',(4.62172660701796,-36.2742356128,-8.54311658750294));
#59514=CARTESIAN_POINT('Ctrl Pts',(4.47177917813589,-36.2742356128,-8.6099745019496));
#59515=CARTESIAN_POINT('Ctrl Pts',(4.32025603921681,-36.2742356128001,-8.67339068051086));
#59516=CARTESIAN_POINT('Ctrl Pts',(4.16724319798237,-36.2742356128002,-8.73329245421995));
#59517=CARTESIAN_POINT('Ctrl Pts',(4.00592103591442,-36.2742356128003,-8.79644717750001));
#59518=CARTESIAN_POINT('Ctrl Pts',(3.84294213456988,-36.2742356128004,-8.855695593392));
#59519=CARTESIAN_POINT('Ctrl Pts',(3.67843820111028,-36.2742356128005,-8.91100547987655));
#59520=CARTESIAN_POINT('Ctrl Pts',(3.52009056743237,-36.2742356128007,-8.96424548125302));
#59521=CARTESIAN_POINT('Ctrl Pts',(3.36032959080013,-36.2742356128008,-9.01383705874524));
#59522=CARTESIAN_POINT('Ctrl Pts',(3.19930855420316,-36.2742356128008,-9.05979054692544));
#59523=CARTESIAN_POINT('Ctrl Pts',(3.03944143838186,-36.2742356128008,-9.10541471984443));
#59524=CARTESIAN_POINT('Ctrl Pts',(2.87833180211124,-36.2742356128008,-9.14745333097509));
#59525=CARTESIAN_POINT('Ctrl Pts',(2.71617158796638,-36.2742356128006,-9.18594575578493));
#59526=CARTESIAN_POINT('Ctrl Pts',(2.5569407515265,-36.2742356128005,-9.2237428259935));
#59527=CARTESIAN_POINT('Ctrl Pts',(2.39669662428977,-36.2742356128002,-9.2581212331758));
#59528=CARTESIAN_POINT('Ctrl Pts',(2.23566714738507,-36.2742356128001,-9.28913817160275));
#59529=CARTESIAN_POINT('Ctrl Pts',(2.21107200779576,-36.2742356128001,-9.29387560194722));
#59530=CARTESIAN_POINT('Ctrl Pts',(2.18645864179448,-36.2742356128,-9.29853464335292));
#59531=CARTESIAN_POINT('Ctrl Pts',(2.16182796614964,-36.2742356128,-9.30311552892602));
#59532=CARTESIAN_POINT('Ctrl Pts',(2.14773674018185,-36.2742356128,-9.30573625661834));
#59533=CARTESIAN_POINT('Ctrl Pts',(2.13364445853742,-36.2742356128,-9.30833065550249));
#59534=CARTESIAN_POINT('Ctrl Pts',(2.11954062634,-36.2742356128,-9.3109005156));
#59535=CARTESIAN_POINT('',(-2.08574139433879,-36.2742356128,-9.31728165005513));
#59536=CARTESIAN_POINT('',(-2.11953809613257,-36.2742356128,-9.31090088400518));
#59537=CARTESIAN_POINT('Origin',(-2.11596805996584,-36.2742356128,-9.34083853594215));
#59538=CARTESIAN_POINT('',(-0.417295449791195,-36.2742356130695,-7.95031783857217));
#59539=CARTESIAN_POINT('Ctrl Pts',(-0.417317472604425,-36.2742356128,-7.95031777923111));
#59540=CARTESIAN_POINT('Ctrl Pts',(-0.417546231264646,-36.2742356128,-7.98699548713484));
#59541=CARTESIAN_POINT('Ctrl Pts',(-0.419189898479267,-36.2742356128,-8.02382064895258));
#59542=CARTESIAN_POINT('Ctrl Pts',(-0.422268169047606,-36.2742356128,-8.06057389439151));
#59543=CARTESIAN_POINT('Ctrl Pts',(-0.425579935577801,-36.2742356128,-8.10011498261571));
#59544=CARTESIAN_POINT('Ctrl Pts',(-0.430552260190847,-36.2742356128,-8.13957291541615));
#59545=CARTESIAN_POINT('Ctrl Pts',(-0.437183115066485,-36.2742356128,-8.17873091302802));
#59546=CARTESIAN_POINT('Ctrl Pts',(-0.444221005381981,-36.2742356128,-8.22029262676411));
#59547=CARTESIAN_POINT('Ctrl Pts',(-0.453127236965292,-36.2742356128,-8.26151691063071));
#59548=CARTESIAN_POINT('Ctrl Pts',(-0.463870525352078,-36.2742356128,-8.30220140912958));
#59549=CARTESIAN_POINT('Ctrl Pts',(-0.475525438127585,-36.2742356128,-8.34633820079412));
#59550=CARTESIAN_POINT('Ctrl Pts',(-0.489342347521156,-36.2742356128,-8.38984042100709));
#59551=CARTESIAN_POINT('Ctrl Pts',(-0.50524902702277,-36.2742356128,-8.43250571146025));
#59552=CARTESIAN_POINT('Ctrl Pts',(-0.523707995997356,-36.2742356128,-8.48201681606801));
#59553=CARTESIAN_POINT('Ctrl Pts',(-0.544981258452666,-36.2742356128,-8.53040226246549));
#59554=CARTESIAN_POINT('Ctrl Pts',(-0.568913005101385,-36.2742356128,-8.57740254193819));
#59555=CARTESIAN_POINT('Ctrl Pts',(-0.597130208862658,-36.2742356128,-8.63281915996381));
#59556=CARTESIAN_POINT('Ctrl Pts',(-0.629042639893959,-36.2742356128,-8.68631556893906));
#59557=CARTESIAN_POINT('Ctrl Pts',(-0.664342184627549,-36.2742356128,-8.73748510336353));
#59558=CARTESIAN_POINT('Ctrl Pts',(-0.691469202170332,-36.2742356128,-8.77680790110681));
#59559=CARTESIAN_POINT('Ctrl Pts',(-0.720595035674572,-36.2742356128,-8.81475797815996));
#59560=CARTESIAN_POINT('Ctrl Pts',(-0.751569999107162,-36.2742356128,-8.8511190844982));
#59561=CARTESIAN_POINT('Ctrl Pts',(-0.766075428722424,-36.2742356128,-8.86814681949038));
#59562=CARTESIAN_POINT('Ctrl Pts',(-0.780986324397503,-36.2742356128,-8.88482547557127));
#59563=CARTESIAN_POINT('Ctrl Pts',(-0.796287350366606,-36.2742356128,-8.90112867589867));
#59564=CARTESIAN_POINT('Ctrl Pts',(-0.841225815081245,-36.2742356128,-8.94901048422498));
#59565=CARTESIAN_POINT('Ctrl Pts',(-0.889533606854501,-36.2742356128,-8.99364989843403));
#59566=CARTESIAN_POINT('Ctrl Pts',(-0.940722367446665,-36.2742356128,-9.03468164511675));
#59567=CARTESIAN_POINT('Ctrl Pts',(-0.990589460005256,-36.2742356128,-9.07465397275269));
#59568=CARTESIAN_POINT('Ctrl Pts',(-1.04319010310048,-36.2742356128,-9.11120153033691));
#59569=CARTESIAN_POINT('Ctrl Pts',(-1.09803239553826,-36.2742356128,-9.14401237848499));
#59570=CARTESIAN_POINT('Ctrl Pts',(-1.15083837102938,-36.2742356128,-9.17560494630327));
#59571=CARTESIAN_POINT('Ctrl Pts',(-1.20572210860661,-36.2742356128,-9.20373244016034));
#59572=CARTESIAN_POINT('Ctrl Pts',(-1.26221438398181,-36.2742356128,-9.22815264079006));
#59573=CARTESIAN_POINT('Ctrl Pts',(-1.31652092227226,-36.2742356128,-9.2516280018328));
#59574=CARTESIAN_POINT('Ctrl Pts',(-1.37231353359154,-36.2742356128,-9.27167690323985));
#59575=CARTESIAN_POINT('Ctrl Pts',(-1.42915351048309,-36.2742356128,-9.28812676549147));
#59576=CARTESIAN_POINT('Ctrl Pts',(-1.48289927719425,-36.2742356128,-9.30368114301511));
#59577=CARTESIAN_POINT('Ctrl Pts',(-1.53758114708514,-36.2742356128,-9.31601746172819));
#59578=CARTESIAN_POINT('Ctrl Pts',(-1.59281351672207,-36.2742356128,-9.32503325122765));
#59579=CARTESIAN_POINT('Ctrl Pts',(-1.64655555550598,-36.2742356128,-9.33380576836086));
#59580=CARTESIAN_POINT('Ctrl Pts',(-1.70081857799357,-36.2742356128,-9.33943422361108));
#59581=CARTESIAN_POINT('Ctrl Pts',(-1.75523679570936,-36.2742356128,-9.3418704259924));
#59582=CARTESIAN_POINT('Ctrl Pts',(-1.81052478073578,-36.2742356128,-9.34434556623831));
#59583=CARTESIAN_POINT('Ctrl Pts',(-1.86597282268321,-36.2742356128,-9.3435249016013));
#59584=CARTESIAN_POINT('Ctrl Pts',(-1.92118875397118,-36.2742356128,-9.33941424583912));
#59585=CARTESIAN_POINT('Ctrl Pts',(-1.97252446862824,-36.2742356128,-9.33559246023598));
#59586=CARTESIAN_POINT('Ctrl Pts',(-2.02365935968099,-36.2742356128,-9.32892702411511));
#59587=CARTESIAN_POINT('Ctrl Pts',(-2.07427344695003,-36.2742356128,-9.31947306843533));
#59588=CARTESIAN_POINT('Ctrl Pts',(-2.07809911928149,-36.2742356128,-9.31875848997272));
#59589=CARTESIAN_POINT('Ctrl Pts',(-2.08192181451298,-36.2742356128,-9.31802800517262));
#59590=CARTESIAN_POINT('Ctrl Pts',(-2.08574139369,-36.2742356128,-9.31728165018));
#59591=CARTESIAN_POINT('',(-0.417273456068905,-36.2742356128057,-3.28965270484013));
#59592=CARTESIAN_POINT('',(-0.417273426056,-36.2742356128,0.915007091638));
#59593=CARTESIAN_POINT('',(-1.05996478409,-36.2742356128,-2.50526963826));
#59594=CARTESIAN_POINT('Ctrl Pts',(-1.05996478409,-36.2742356128,-2.50526963826));
#59595=CARTESIAN_POINT('Ctrl Pts',(-1.01931967505232,-36.2742356128,-2.51342106522695));
#59596=CARTESIAN_POINT('Ctrl Pts',(-0.9793504971128,-36.2742356128,-2.52474706012613));
#59597=CARTESIAN_POINT('Ctrl Pts',(-0.940505223089573,-36.2742356128,-2.53908773691866));
#59598=CARTESIAN_POINT('Ctrl Pts',(-0.902843959426671,-36.2742356128,-2.55299130751685));
#59599=CARTESIAN_POINT('Ctrl Pts',(-0.86624009095651,-36.2742356128,-2.56972849573662));
#59600=CARTESIAN_POINT('Ctrl Pts',(-0.831094331796187,-36.2742356128,-2.58910597838381));
#59601=CARTESIAN_POINT('Ctrl Pts',(-0.811886969644185,-36.2742356128,-2.59969588555015));
#59602=CARTESIAN_POINT('Ctrl Pts',(-0.793114883117866,-36.2742356128,-2.61107353370296));
#59603=CARTESIAN_POINT('Ctrl Pts',(-0.774840964085916,-36.2742356128,-2.62320119611295));
#59604=CARTESIAN_POINT('Ctrl Pts',(-0.743411052499667,-36.2742356128,-2.64405995972176));
#59605=CARTESIAN_POINT('Ctrl Pts',(-0.713455797872463,-36.2742356128,-2.66714014311122));
#59606=CARTESIAN_POINT('Ctrl Pts',(-0.685276497880166,-36.2742356128,-2.69221820140988));
#59607=CARTESIAN_POINT('Ctrl Pts',(-0.658305885066703,-36.2742356128,-2.71622059326032));
#59608=CARTESIAN_POINT('Ctrl Pts',(-0.632962377549237,-36.2742356128,-2.74205330272653));
#59609=CARTESIAN_POINT('Ctrl Pts',(-0.609482897196851,-36.2742356128,-2.76948226806354));
#59610=CARTESIAN_POINT('Ctrl Pts',(-0.590134228562073,-36.2742356128,-2.79208557756339));
#59611=CARTESIAN_POINT('Ctrl Pts',(-0.57205081595477,-36.2742356128,-2.81577241456369));
#59612=CARTESIAN_POINT('Ctrl Pts',(-0.555345443066818,-36.2742356128,-2.8403938476929));
#59613=CARTESIAN_POINT('Ctrl Pts',(-0.534212430985569,-36.2742356128,-2.87154101497058));
#59614=CARTESIAN_POINT('Ctrl Pts',(-0.515285354405834,-36.2742356127994,
-2.90418431450337));
#59615=CARTESIAN_POINT('Ctrl Pts',(-0.498748018357097,-36.2742356128018,
-2.9379939067206));
#59616=CARTESIAN_POINT('Ctrl Pts',(-0.492528026848015,-36.2742356128027,
-2.9507103065021));
#59617=CARTESIAN_POINT('Ctrl Pts',(-0.486645558484015,-36.274235612804,
-2.96359166617615));
#59618=CARTESIAN_POINT('Ctrl Pts',(-0.481108531718049,-36.2742356128064,
-2.97662022125917));
#59619=CARTESIAN_POINT('Ctrl Pts',(-0.465941480447615,-36.2742356128127,
-3.01230810417467));
#59620=CARTESIAN_POINT('Ctrl Pts',(-0.453370359796223,-36.2742356128134,
-3.04909747252491));
#59621=CARTESIAN_POINT('Ctrl Pts',(-0.44352288631122,-36.2742356128085,
-3.08660817285071));
#59622=CARTESIAN_POINT('Ctrl Pts',(-0.440219280518529,-36.2742356128068,
-3.0991921688445));
#59623=CARTESIAN_POINT('Ctrl Pts',(-0.437221797877176,-36.2742356128049,
-3.11185718865161));
#59624=CARTESIAN_POINT('Ctrl Pts',(-0.434534084237162,-36.2742356128032,
-3.12458832905277));
#59625=CARTESIAN_POINT('Ctrl Pts',(-0.425879427376572,-36.274235612798,
-3.16558363821654));
#59626=CARTESIAN_POINT('Ctrl Pts',(-0.420440800887583,-36.2742356128,-3.20726463195048));
#59627=CARTESIAN_POINT('Ctrl Pts',(-0.418306079453427,-36.2742356128,-3.24914344852297));
#59628=CARTESIAN_POINT('Ctrl Pts',(-0.417800243602732,-36.2742356128,-3.25906690104849));
#59629=CARTESIAN_POINT('Ctrl Pts',(-0.417479805275784,-36.2742356128,-3.26900126298853));
#59630=CARTESIAN_POINT('Ctrl Pts',(-0.41734575245625,-36.2742356128,-3.2789396340017));
#59631=CARTESIAN_POINT('Ctrl Pts',(-0.417297594428668,-36.2742356128,-3.28250996058665));
#59632=CARTESIAN_POINT('Ctrl Pts',(-0.41727348657,-36.2742356128,-3.28608342917333));
#59633=CARTESIAN_POINT('Ctrl Pts',(-0.41727348535,-36.2742356128,-3.28965270484));
#59634=CARTESIAN_POINT('',(-2.29653265536,-36.2742356128,-2.09683653367));
#59635=CARTESIAN_POINT('Origin',(-0.442148072512747,-36.2742356127947,1.43999152964127));
#59636=CARTESIAN_POINT('',(-6.27496294130418,-36.2742356128,2.72284562885154));
#59637=CARTESIAN_POINT('Ctrl Pts',(-6.2749628032,-36.2742356128,2.72284536858));
#59638=CARTESIAN_POINT('Ctrl Pts',(-6.24453537274772,-36.2742356128,2.66629639399008));
#59639=CARTESIAN_POINT('Ctrl Pts',(-6.2168833111465,-36.2742356128,2.6090079890714));
#59640=CARTESIAN_POINT('Ctrl Pts',(-6.19141504098666,-36.2742356128,2.551348392481));
#59641=CARTESIAN_POINT('Ctrl Pts',(-6.17072302935005,-36.2742356128,2.50450213884372));
#59642=CARTESIAN_POINT('Ctrl Pts',(-6.1514737587113,-36.2742356128,2.45741434061633));
#59643=CARTESIAN_POINT('Ctrl Pts',(-6.1333727111274,-36.2742356128,2.41026966734787));
#59644=CARTESIAN_POINT('Ctrl Pts',(-6.11724305155994,-36.2742356128,2.36825952806092));
#59645=CARTESIAN_POINT('Ctrl Pts',(-6.10202552397655,-36.2742356128,2.32620538526914));
#59646=CARTESIAN_POINT('Ctrl Pts',(-6.08752271510141,-36.2742356128,2.28420045422166));
#59647=CARTESIAN_POINT('Ctrl Pts',(-6.07444612368462,-36.2742356128,2.24632632062948));
#59648=CARTESIAN_POINT('Ctrl Pts',(-6.06195079512164,-36.2742356128,2.208492564208));
#59649=CARTESIAN_POINT('Ctrl Pts',(-6.04989771094152,-36.2742356128,2.17072599038824));
#59650=CARTESIAN_POINT('Ctrl Pts',(-6.04164302161129,-36.2742356128,2.14486113046605));
#59651=CARTESIAN_POINT('Ctrl Pts',(-6.03359587134105,-36.2742356128,2.11902695315767));
#59652=CARTESIAN_POINT('Ctrl Pts',(-6.0257127381864,-36.2742356128,2.09321776497177));
#59653=CARTESIAN_POINT('Ctrl Pts',(-6.01988428400105,-36.2742356128,2.07413554627123));
#59654=CARTESIAN_POINT('Ctrl Pts',(-6.01414698874104,-36.2742356127997,
2.05507173915977));
#59655=CARTESIAN_POINT('Ctrl Pts',(-6.00849032434624,-36.2742356128003,
2.03604835176757));
#59656=CARTESIAN_POINT('Ctrl Pts',(-6.00026038362399,-36.274235612801,2.00837102469864));
#59657=CARTESIAN_POINT('Ctrl Pts',(-5.9922193766253,-36.2742356128019,1.98084599545624));
#59658=CARTESIAN_POINT('Ctrl Pts',(-5.98436613823573,-36.2742356128016,
1.95363294374715));
#59659=CARTESIAN_POINT('Ctrl Pts',(-5.97824034356331,-36.2742356128013,
1.93240583221554));
#59660=CARTESIAN_POINT('Ctrl Pts',(-5.97222942790735,-36.2742356128007,
1.91137021894081));
#59661=CARTESIAN_POINT('Ctrl Pts',(-5.9663261063212,-36.2742356128004,1.8905682486979));
#59662=CARTESIAN_POINT('Ctrl Pts',(-5.96115895320338,-36.2742356128001,
1.8723603696541));
#59663=CARTESIAN_POINT('Ctrl Pts',(-5.95607439962134,-36.2742356128,1.85433193430266));
#59664=CARTESIAN_POINT('Ctrl Pts',(-5.95105754275361,-36.2742356128,1.83647095674252));
#59665=CARTESIAN_POINT('Ctrl Pts',(-5.94895269411707,-36.2742356128,1.82897728983993));
#59666=CARTESIAN_POINT('Ctrl Pts',(-5.9468596177166,-36.2742356128,1.82151253845821));
#59667=CARTESIAN_POINT('Ctrl Pts',(-5.94477649645998,-36.2742356128,1.81407306760198));
#59668=CARTESIAN_POINT('Ctrl Pts',(-5.93757006918152,-36.2742356128,1.78833668497644));
#59669=CARTESIAN_POINT('Ctrl Pts',(-5.93048994125108,-36.2742356128,1.76293068499097));
#59670=CARTESIAN_POINT('Ctrl Pts',(-5.92345520647712,-36.2742356128,1.73768612585181));
#59671=CARTESIAN_POINT('Ctrl Pts',(-5.91531260482293,-36.2742356128,1.70846592130808));
#59672=CARTESIAN_POINT('Ctrl Pts',(-5.90722899374801,-36.2742356128,1.6794554850506));
#59673=CARTESIAN_POINT('Ctrl Pts',(-5.89907507031516,-36.2742356128,1.65035466102641));
#59674=CARTESIAN_POINT('Ctrl Pts',(-5.89290045814991,-36.2742356128,1.62831787057597));
#59675=CARTESIAN_POINT('Ctrl Pts',(-5.886685159316,-36.2742356128,1.6062273279421));
#59676=CARTESIAN_POINT('Ctrl Pts',(-5.88038345128574,-36.2742356128,1.5839833454214));
#59677=CARTESIAN_POINT('Ctrl Pts',(-5.87491371948055,-36.2742356128,1.56467610076913));
#59678=CARTESIAN_POINT('Ctrl Pts',(-5.86937880076088,-36.2742356128,1.54525279633991));
#59679=CARTESIAN_POINT('Ctrl Pts',(-5.86376008203665,-36.2742356128,1.52568667108676));
#59680=CARTESIAN_POINT('Ctrl Pts',(-5.86063563574475,-36.2742356128,1.51480637782159));
#59681=CARTESIAN_POINT('Ctrl Pts',(-5.85748549226303,-36.2742356128,1.50388266814331));
#59682=CARTESIAN_POINT('Ctrl Pts',(-5.85430841249731,-36.2742356128,1.4929178587057));
#59683=CARTESIAN_POINT('Ctrl Pts',(-5.84903277585167,-36.2742356128,1.47471046237093));
#59684=CARTESIAN_POINT('Ctrl Pts',(-5.84368586733359,-36.2742356128,1.45639984537539));
#59685=CARTESIAN_POINT('Ctrl Pts',(-5.83827687493929,-36.2742356128,1.438048312437));
#59686=CARTESIAN_POINT('Ctrl Pts',(-5.83316400341666,-36.2742356128,1.42070145311135));
#59687=CARTESIAN_POINT('Ctrl Pts',(-5.82799788376965,-36.2742356128,1.40332542183888));
#59688=CARTESIAN_POINT('Ctrl Pts',(-5.82279354468847,-36.2742356128,1.38599962836736));
#59689=CARTESIAN_POINT('Ctrl Pts',(-5.82249212631315,-36.2742356128,1.38499617481874));
#59690=CARTESIAN_POINT('Ctrl Pts',(-5.8221905835966,-36.2742356128,1.38399290398093));
#59691=CARTESIAN_POINT('Ctrl Pts',(-5.82188892091261,-36.2742356128,1.38298983663647));
#59692=CARTESIAN_POINT('Ctrl Pts',(-5.81355730601708,-36.2742356128,1.35528614217218));
#59693=CARTESIAN_POINT('Ctrl Pts',(-5.80513063484038,-36.2742356128,1.32772641991473));
#59694=CARTESIAN_POINT('Ctrl Pts',(-5.79657009907114,-36.2742356128,1.30026398785058));
#59695=CARTESIAN_POINT('Ctrl Pts',(-5.78691018700546,-36.2742356128,1.26927472666409));
#59696=CARTESIAN_POINT('Ctrl Pts',(-5.77708000240597,-36.2742356128,1.23841018151499));
#59697=CARTESIAN_POINT('Ctrl Pts',(-5.76704602152116,-36.2742356128,1.20766721886827));
#59698=CARTESIAN_POINT('Ctrl Pts',(-5.7529866774042,-36.2742356128,1.16459100654669));
#59699=CARTESIAN_POINT('Ctrl Pts',(-5.73852780525219,-36.2742356128,1.12175735602248));
#59700=CARTESIAN_POINT('Ctrl Pts',(-5.72361628682829,-36.2742356128,1.0792503575753));
#59701=CARTESIAN_POINT('Ctrl Pts',(-5.71260137263102,-36.2742356128,1.04785107767843));
#59702=CARTESIAN_POINT('Ctrl Pts',(-5.7013407996525,-36.2742356128,1.01663358324319));
#59703=CARTESIAN_POINT('Ctrl Pts',(-5.68981205327961,-36.2742356128,0.985611834769589));
#59704=CARTESIAN_POINT('Ctrl Pts',(-5.68573367726689,-36.2742356128,0.974637670644965));
#59705=CARTESIAN_POINT('Ctrl Pts',(-5.68162165873323,-36.2742356128,0.963687599243863));
#59706=CARTESIAN_POINT('Ctrl Pts',(-5.67747462183944,-36.2742356128,0.952760543386742));
#59707=CARTESIAN_POINT('Ctrl Pts',(-5.65389160120622,-36.2742356128,0.890621481126485));
#59708=CARTESIAN_POINT('Ctrl Pts',(-5.62917129836967,-36.2742356128,0.829225266724225));
#59709=CARTESIAN_POINT('Ctrl Pts',(-5.60316923875744,-36.2742356128,0.768629253667028));
#59710=CARTESIAN_POINT('Ctrl Pts',(-5.57625830207163,-36.2742356128,0.705915165048141));
#59711=CARTESIAN_POINT('Ctrl Pts',(-5.54797443819125,-36.2742356128,0.644058001660994));
#59712=CARTESIAN_POINT('Ctrl Pts',(-5.51820998035682,-36.2742356128,0.583101326837146));
#59713=CARTESIAN_POINT('Ctrl Pts',(-5.48778020704284,-36.2742356128,0.520782106806925));
#59714=CARTESIAN_POINT('Ctrl Pts',(-5.45580305455407,-36.2742356128,0.459403793931162));
#59715=CARTESIAN_POINT('Ctrl Pts',(-5.42221613166309,-36.2742356128,0.398996157173145));
#59716=CARTESIAN_POINT('Ctrl Pts',(-5.38743512568233,-36.2742356128,0.336440906661415));
#59717=CARTESIAN_POINT('Ctrl Pts',(-5.35092793674563,-36.2742356128,0.274926244750017));
#59718=CARTESIAN_POINT('Ctrl Pts',(-5.3126795256956,-36.2742356128,0.214472196036214));
#59719=CARTESIAN_POINT('Ctrl Pts',(-5.30231556565285,-36.2742356128,0.198091297376847));
#59720=CARTESIAN_POINT('Ctrl Pts',(-5.2918240555852,-36.2742356128,0.181788215678701));
#59721=CARTESIAN_POINT('Ctrl Pts',(-5.28120533345534,-36.2742356128,0.165563244497791));
#59722=CARTESIAN_POINT('Ctrl Pts',(-5.23908934623629,-36.2742356128,0.101211746216937));
#59723=CARTESIAN_POINT('Ctrl Pts',(-5.19496806917432,-36.2742356128,0.0380905722805007));
#59724=CARTESIAN_POINT('Ctrl Pts',(-5.14890045052453,-36.2742356128,-0.0237928430699731));
#59725=CARTESIAN_POINT('Ctrl Pts',(-5.10113638619278,-36.2742356128,-0.0879551227471305));
#59726=CARTESIAN_POINT('Ctrl Pts',(-5.05128029700902,-36.2742356128,-0.150787036013723));
#59727=CARTESIAN_POINT('Ctrl Pts',(-4.99945322518508,-36.2742356128,-0.212299321910926));
#59728=CARTESIAN_POINT('Ctrl Pts',(-4.94375172282346,-36.2742356128,-0.278410074797206));
#59729=CARTESIAN_POINT('Ctrl Pts',(-4.88577370413207,-36.2742356128,-0.34299678500102));
#59730=CARTESIAN_POINT('Ctrl Pts',(-4.82572895436385,-36.2742356128,-0.406090623479409));
#59731=CARTESIAN_POINT('Ctrl Pts',(-4.79084535329308,-36.2742356128,-0.442745623292039));
#59732=CARTESIAN_POINT('Ctrl Pts',(-4.75526528057978,-36.2742356128,-0.478897064056129));
#59733=CARTESIAN_POINT('Ctrl Pts',(-4.71903753054964,-36.2742356128,-0.514552888056171));
#59734=CARTESIAN_POINT('Ctrl Pts',(-4.64444432098229,-36.2742356128,-0.587968497629466));
#59735=CARTESIAN_POINT('Ctrl Pts',(-4.56710094042078,-36.2742356127999,
-0.659284698548609));
#59736=CARTESIAN_POINT('Ctrl Pts',(-4.48745667359651,-36.2742356128001,
-0.728608343046159));
#59737=CARTESIAN_POINT('Ctrl Pts',(-4.39811945811274,-36.2742356128004,
-0.806368885186153));
#59738=CARTESIAN_POINT('Ctrl Pts',(-4.3058889383997,-36.2742356127994,-0.881623702287833));
#59739=CARTESIAN_POINT('Ctrl Pts',(-4.21137879892378,-36.2742356128104,
-0.954588341667663));
#59740=CARTESIAN_POINT('Ctrl Pts',(-4.1488246595336,-36.2742356128176,-1.00288199828091));
#59741=CARTESIAN_POINT('Ctrl Pts',(-4.0852713916205,-36.2742356128302,-1.05017372938662));
#59742=CARTESIAN_POINT('Ctrl Pts',(-4.02088678663867,-36.2742356128628,
-1.09653320575464));
#59743=CARTESIAN_POINT('Ctrl Pts',(-3.93246496197258,-36.2742356129075,
-1.1602004363322));
#59744=CARTESIAN_POINT('Ctrl Pts',(-3.84242717112692,-36.2742356129842,
-1.22214574970036));
#59745=CARTESIAN_POINT('Ctrl Pts',(-3.75117549355878,-36.2742356130422,
-1.28253353257367));
#59746=CARTESIAN_POINT('Ctrl Pts',(-3.66800942582536,-36.2742356130951,
-1.33757048723089));
#59747=CARTESIAN_POINT('Ctrl Pts',(-3.58383519756554,-36.2742356131249,
-1.39131473192463));
#59748=CARTESIAN_POINT('Ctrl Pts',(-3.498919466185,-36.2742356130898,-1.44387055986142));
#59749=CARTESIAN_POINT('Ctrl Pts',(-3.41958194559884,-36.2742356130569,
-1.4929739357974));
#59750=CARTESIAN_POINT('Ctrl Pts',(-3.33959721867197,-36.274235612958,-1.54104048394551));
#59751=CARTESIAN_POINT('Ctrl Pts',(-3.25914673123784,-36.2742356128737,
-1.58812608964871));
#59752=CARTESIAN_POINT('Ctrl Pts',(-3.25349026788856,-36.2742356128678,
-1.59143667248585));
#59753=CARTESIAN_POINT('Ctrl Pts',(-3.24783148609435,-36.274235612862,-1.59474239134763));
#59754=CARTESIAN_POINT('Ctrl Pts',(-3.24217044152485,-36.2742356128564,
-1.59804325870171));
#59755=CARTESIAN_POINT('Ctrl Pts',(-3.17540989463343,-36.2742356127911,
-1.6369702989447));
#59756=CARTESIAN_POINT('Ctrl Pts',(-3.10833928979081,-36.2742356128,-1.67522511318535));
#59757=CARTESIAN_POINT('Ctrl Pts',(-3.04105812388561,-36.2742356128,-1.71280864441373));
#59758=CARTESIAN_POINT('Ctrl Pts',(-3.00580358073116,-36.2742356128,-1.73250197472039));
#59759=CARTESIAN_POINT('Ctrl Pts',(-2.9704911135997,-36.2742356128,-1.75200976423252));
#59760=CARTESIAN_POINT('Ctrl Pts',(-2.93513275915533,-36.2742356128,-1.77132942170696));
#59761=CARTESIAN_POINT('Ctrl Pts',(-2.90681919636723,-36.2742356128,-1.78679983438716));
#59762=CARTESIAN_POINT('Ctrl Pts',(-2.87847617925005,-36.2742356128,-1.80214958270991));
#59763=CARTESIAN_POINT('Ctrl Pts',(-2.85010907686803,-36.2742356128,-1.81737646356693));
#59764=CARTESIAN_POINT('Ctrl Pts',(-2.83489978685648,-36.2742356128,-1.82554049963262));
#59765=CARTESIAN_POINT('Ctrl Pts',(-2.81968183312169,-36.2742356128,-1.83367014577044));
#59766=CARTESIAN_POINT('Ctrl Pts',(-2.80444614119178,-36.2742356128,-1.84177010461572));
#59767=CARTESIAN_POINT('Ctrl Pts',(-2.7312492107695,-36.2742356128,-1.88068478776555));
#59768=CARTESIAN_POINT('Ctrl Pts',(-2.65771102048995,-36.2742356128,-1.91888207960992));
#59769=CARTESIAN_POINT('Ctrl Pts',(-2.58393848667699,-36.2742356128,-1.95625204730452));
#59770=CARTESIAN_POINT('Ctrl Pts',(-2.53620979668164,-36.2742356128,-1.98042933268493));
#59771=CARTESIAN_POINT('Ctrl Pts',(-2.48838235857969,-36.2742356128,-2.00425958104195));
#59772=CARTESIAN_POINT('Ctrl Pts',(-2.44047714007376,-36.2742356128,-2.02770384416305));
#59773=CARTESIAN_POINT('Ctrl Pts',(-2.41652453082079,-36.2742356128,-2.0394259757236));
#59774=CARTESIAN_POINT('Ctrl Pts',(-2.39255237409675,-36.2742356128,-2.05105149240143));
#59775=CARTESIAN_POINT('Ctrl Pts',(-2.36856266117483,-36.2742356128,-2.06257479271213));
#59776=CARTESIAN_POINT('Ctrl Pts',(-2.35274440118297,-36.2742356128,-2.07017298952559));
#59777=CARTESIAN_POINT('Ctrl Pts',(-2.33692076087942,-36.2742356128,-2.07772567107306));
#59778=CARTESIAN_POINT('Ctrl Pts',(-2.32108130896673,-36.2742356128,-2.0852362535285));
#59779=CARTESIAN_POINT('Ctrl Pts',(-2.31289890863895,-36.2742356128,-2.08911609688949));
#59780=CARTESIAN_POINT('Ctrl Pts',(-2.30471404262477,-36.2742356128,-2.09298385940345));
#59781=CARTESIAN_POINT('Ctrl Pts',(-2.29653265536,-36.2742356128,-2.09683653367));
#59782=CARTESIAN_POINT('',(-9.72829200583979,-36.2742356128,2.64855052067506));
#59783=CARTESIAN_POINT('Ctrl Pts',(-9.72829200283952,-36.2742356128,2.64855051884389));
#59784=CARTESIAN_POINT('Ctrl Pts',(-9.70881714164152,-36.2742356128,2.68045885667498));
#59785=CARTESIAN_POINT('Ctrl Pts',(-9.68889475699523,-36.2742356127939,
2.71236488661939));
#59786=CARTESIAN_POINT('Ctrl Pts',(-9.66845938327075,-36.2742356128061,
2.74429101374004));
#59787=CARTESIAN_POINT('Ctrl Pts',(-9.64722469389298,-36.2742356128187,
2.7774659094666));
#59788=CARTESIAN_POINT('Ctrl Pts',(-9.62543546500888,-36.2742356127916,
2.81066258335515));
#59789=CARTESIAN_POINT('Ctrl Pts',(-9.60300164534709,-36.2742356132359,
2.84385119710766));
#59790=CARTESIAN_POINT('Ctrl Pts',(-9.58651192372458,-36.2742356135625,
2.86824610667128));
#59791=CARTESIAN_POINT('Ctrl Pts',(-9.56967353061277,-36.2742356141378,
2.89263545845183));
#59792=CARTESIAN_POINT('Ctrl Pts',(-9.55244862998868,-36.2742356157403,
2.91698968329831));
#59793=CARTESIAN_POINT('Ctrl Pts',(-9.53980531242101,-36.2742356169165,
2.93486602439127));
#59794=CARTESIAN_POINT('Ctrl Pts',(-9.52696074018631,-36.2742356188376,
2.95271192605641));
#59795=CARTESIAN_POINT('Ctrl Pts',(-9.51385958563359,-36.2742356221257,
2.97056761705111));
#59796=CARTESIAN_POINT('Ctrl Pts',(-9.48902877144369,-36.2742356283578,
3.0044097752775));
#59797=CARTESIAN_POINT('Ctrl Pts',(-9.46324980492634,-36.2742356393454,
3.03832837506574));
#59798=CARTESIAN_POINT('Ctrl Pts',(-9.43647539801905,-36.2742356478859,
3.072103909518));
#59799=CARTESIAN_POINT('Ctrl Pts',(-9.4100087918541,-36.2742356563283,3.10549115770071));
#59800=CARTESIAN_POINT('Ctrl Pts',(-9.38256837684105,-36.2742356607735,
3.13873761718217));
#59801=CARTESIAN_POINT('Ctrl Pts',(-9.35414272876498,-36.2742356533727,
3.17159442011749));
#59802=CARTESIAN_POINT('Ctrl Pts',(-9.34981362475727,-36.2742356522455,
3.17659836996191));
#59803=CARTESIAN_POINT('Ctrl Pts',(-9.34546175267801,-36.2742356508755,
3.18159322937679));
#59804=CARTESIAN_POINT('Ctrl Pts',(-9.34108716705853,-36.2742356492836,
3.18657806784048));
#59805=CARTESIAN_POINT('Ctrl Pts',(-9.32533707496848,-36.2742356435521,
3.20452529111746));
#59806=CARTESIAN_POINT('Ctrl Pts',(-9.30928255086254,-36.2742356380445,
3.2223449918369));
#59807=CARTESIAN_POINT('Ctrl Pts',(-9.29289822512316,-36.2742356335668,
3.24001817562276));
#59808=CARTESIAN_POINT('Ctrl Pts',(-9.27651389938378,-36.2742356290892,
3.25769135940861));
#59809=CARTESIAN_POINT('Ctrl Pts',(-9.25978052146042,-36.2742356248894,
3.27524193625796));
#59810=CARTESIAN_POINT('Ctrl Pts',(-9.24266879473122,-36.2742356217968,
3.29264736551428));
#59811=CARTESIAN_POINT('Ctrl Pts',(-9.21166804126147,-36.2742356161942,
3.32418021020898));
#59812=CARTESIAN_POINT('Ctrl Pts',(-9.17946812786415,-36.274235614416,3.35518678266736));
#59813=CARTESIAN_POINT('Ctrl Pts',(-9.14603905518141,-36.2742356135611,
3.38542077511821));
#59814=CARTESIAN_POINT('Ctrl Pts',(-9.11365966829153,-36.2742356127332,
3.41470540852945));
#59815=CARTESIAN_POINT('Ctrl Pts',(-9.08012671258212,-36.2742356128071,
3.44326464800626));
#59816=CARTESIAN_POINT('Ctrl Pts',(-9.04545810927638,-36.2742356128011,
3.47085541290006));
#59817=CARTESIAN_POINT('Ctrl Pts',(-9.03688320628073,-36.2742356127996,
3.4776796893341));
#59818=CARTESIAN_POINT('Ctrl Pts',(-9.02823906549762,-36.2742356128,3.48444464576843));
#59819=CARTESIAN_POINT('Ctrl Pts',(-9.0195264422119,-36.2742356128,3.49114647591936));
#59820=CARTESIAN_POINT('Ctrl Pts',(-8.98770603560951,-36.2742356128,3.51562302602248));
#59821=CARTESIAN_POINT('Ctrl Pts',(-8.95495184342817,-36.2742356128,3.53927487380998));
#59822=CARTESIAN_POINT('Ctrl Pts',(-8.92126202698245,-36.2742356128,3.56194807661424));
#59823=CARTESIAN_POINT('Ctrl Pts',(-8.91092880879014,-36.2742356128,3.56890231906528));
#59824=CARTESIAN_POINT('Ctrl Pts',(-8.90050794619933,-36.2742356128,3.57576445922664));
#59825=CARTESIAN_POINT('Ctrl Pts',(-8.89000034786166,-36.2742356128,3.58252999939621));
#59826=CARTESIAN_POINT('Ctrl Pts',(-8.85417163483683,-36.2742356128,3.60559907659196));
#59827=CARTESIAN_POINT('Ctrl Pts',(-8.81731612594884,-36.2742356128,3.6275536106033));
#59828=CARTESIAN_POINT('Ctrl Pts',(-8.77950365203068,-36.2742356128,3.64821448776519));
#59829=CARTESIAN_POINT('Ctrl Pts',(-8.77007157519482,-36.2742356128,3.65336820982287));
#59830=CARTESIAN_POINT('Ctrl Pts',(-8.76058020706037,-36.2742356128,3.65844147391791));
#59831=CARTESIAN_POINT('Ctrl Pts',(-8.75103111774342,-36.2742356128,3.66343159406543));
#59832=CARTESIAN_POINT('Ctrl Pts',(-8.71119259904518,-36.2742356128,3.68425022799007));
#59833=CARTESIAN_POINT('Ctrl Pts',(-8.67032239058182,-36.2742356128,3.70363224949672));
#59834=CARTESIAN_POINT('Ctrl Pts',(-8.62855784922379,-36.2742356128,3.72139135357447));
#59835=CARTESIAN_POINT('Ctrl Pts',(-8.62017492022797,-36.2742356128,3.72495593979216));
#59836=CARTESIAN_POINT('Ctrl Pts',(-8.6117561124818,-36.2742356128,3.72845521369156));
#59837=CARTESIAN_POINT('Ctrl Pts',(-8.60330275640969,-36.2742356128,3.7318877882704));
#59838=CARTESIAN_POINT('Ctrl Pts',(-8.56260230061348,-36.2742356128,3.74841463852037));
#59839=CARTESIAN_POINT('Ctrl Pts',(-8.52106780561381,-36.2742356127477,
3.76340465617139));
#59840=CARTESIAN_POINT('Ctrl Pts',(-8.47888591381473,-36.2742356128523,
3.77670246412333));
#59841=CARTESIAN_POINT('Ctrl Pts',(-8.46865840584675,-36.2742356128777,
3.77992667790285));
#59842=CARTESIAN_POINT('Ctrl Pts',(-8.4583930024119,-36.2742356129174,3.78305158595824));
#59843=CARTESIAN_POINT('Ctrl Pts',(-8.44809265827065,-36.2742356129926,
3.78607533346085));
#59844=CARTESIAN_POINT('Ctrl Pts',(-8.40414425667525,-36.2742356133133,
3.79897673439904));
#59845=CARTESIAN_POINT('Ctrl Pts',(-8.35956591318086,-36.2742356136175,
3.81004533329349));
#59846=CARTESIAN_POINT('Ctrl Pts',(-8.31455927271245,-36.2742356135546,
3.81918158877721));
#59847=CARTESIAN_POINT('Ctrl Pts',(-8.2708985149816,-36.2742356134935,3.82804463283228));
#59848=CARTESIAN_POINT('Ctrl Pts',(-8.22683534940045,-36.2742356132172,
3.83508870122784));
#59849=CARTESIAN_POINT('Ctrl Pts',(-8.18256835517632,-36.2742356130434,
3.84026882783139));
#59850=CARTESIAN_POINT('Ctrl Pts',(-8.14029162176882,-36.2742356128773,
3.84521605398202));
#59851=CARTESIAN_POINT('Ctrl Pts',(-8.0978294896405,-36.2742356128133,3.84846295530726));
#59852=CARTESIAN_POINT('Ctrl Pts',(-8.05536002370458,-36.2742356128032,
3.85001759540461));
#59853=CARTESIAN_POINT('Ctrl Pts',(-8.03833269714543,-36.2742356127992,
3.85064089885419));
#59854=CARTESIAN_POINT('Ctrl Pts',(-8.02130420979561,-36.2742356128,3.85099274476445));
#59855=CARTESIAN_POINT('Ctrl Pts',(-8.0042860115659,-36.2742356128,3.85107605173954));
#59856=CARTESIAN_POINT('Ctrl Pts',(-7.9599310512507,-36.2742356128,3.85129317681496));
#59857=CARTESIAN_POINT('Ctrl Pts',(-7.91563944625556,-36.2742356129104,
3.84967518465513));
#59858=CARTESIAN_POINT('Ctrl Pts',(-7.87158021912379,-36.2742356132959,
3.84626457629435));
#59859=CARTESIAN_POINT('Ctrl Pts',(-7.84149821150494,-36.2742356135591,
3.84393593928973));
#59860=CARTESIAN_POINT('Ctrl Pts',(-7.81152457443802,-36.2742356137885,
3.84077293715099));
#59861=CARTESIAN_POINT('Ctrl Pts',(-7.78171169682192,-36.2742356135375,
3.83680279283792));
#59862=CARTESIAN_POINT('Ctrl Pts',(-7.74497551896622,-36.2742356132282,
3.83191068113117));
#59863=CARTESIAN_POINT('Ctrl Pts',(-7.70847517960959,-36.2742356128376,
3.82578856669653));
#59864=CARTESIAN_POINT('Ctrl Pts',(-7.67230948527672,-36.2742356128125,
3.81848117117423));
#59865=CARTESIAN_POINT('Ctrl Pts',(-7.63614379094206,-36.2742356127875,
3.81117377565156));
#59866=CARTESIAN_POINT('Ctrl Pts',(-7.60030599244742,-36.2742356128,3.8026864810845));
#59867=CARTESIAN_POINT('Ctrl Pts',(-7.56485464772436,-36.2742356128,3.79308618073687));
#59868=CARTESIAN_POINT('Ctrl Pts',(-7.51614449460733,-36.2742356128,3.77989536657861));
#59869=CARTESIAN_POINT('Ctrl Pts',(-7.46815457775148,-36.2742356128,3.76459822919188));
#59870=CARTESIAN_POINT('Ctrl Pts',(-7.42109393627412,-36.2742356128,3.74740524786678));
#59871=CARTESIAN_POINT('Ctrl Pts',(-7.37554524515301,-36.2742356128,3.7307646375554));
#59872=CARTESIAN_POINT('Ctrl Pts',(-7.33086784647416,-36.2742356128,3.71234961793179));
#59873=CARTESIAN_POINT('Ctrl Pts',(-7.28720664579929,-36.2742356128,3.69236808034837));
#59874=CARTESIAN_POINT('Ctrl Pts',(-7.25324153041755,-36.2742356128,3.67682395377753));
#59875=CARTESIAN_POINT('Ctrl Pts',(-7.2198880141248,-36.2742356128,3.66033091549968));
#59876=CARTESIAN_POINT('Ctrl Pts',(-7.18720047173584,-36.2742356128,3.64299101963176));
#59877=CARTESIAN_POINT('Ctrl Pts',(-7.16357818122735,-36.2742356128,3.63046000543972));
#59878=CARTESIAN_POINT('Ctrl Pts',(-7.14030418161754,-36.2742356127951,
3.61748764102144));
#59879=CARTESIAN_POINT('Ctrl Pts',(-7.11736987557029,-36.2742356128049,
3.60409577182642));
#59880=CARTESIAN_POINT('Ctrl Pts',(-7.08175075284689,-36.27423561282,3.58329694619941));
#59881=CARTESIAN_POINT('Ctrl Pts',(-7.04694106975427,-36.2742356128032,
3.56149027437102));
#59882=CARTESIAN_POINT('Ctrl Pts',(-7.0129444202984,-36.2742356128006,3.53877467325613));
#59883=CARTESIAN_POINT('Ctrl Pts',(-7.00316458010594,-36.2742356127999,
3.53224006021823));
#59884=CARTESIAN_POINT('Ctrl Pts',(-6.99345173196612,-36.2742356128,3.5256300856373));
#59885=CARTESIAN_POINT('Ctrl Pts',(-6.98380523431276,-36.2742356128,3.51894671931244));
#59886=CARTESIAN_POINT('Ctrl Pts',(-6.93692149920594,-36.2742356128,3.48646434201277));
#59887=CARTESIAN_POINT('Ctrl Pts',(-6.89160109645423,-36.2742356127441,
3.45225020263866));
#59888=CARTESIAN_POINT('Ctrl Pts',(-6.84780885039552,-36.2742356131978,
3.41649930066148));
#59889=CARTESIAN_POINT('Ctrl Pts',(-6.80350698393218,-36.2742356136568,
3.38033235724384));
#59890=CARTESIAN_POINT('Ctrl Pts',(-6.76076867429983,-36.274235614773,3.34259238553588));
#59891=CARTESIAN_POINT('Ctrl Pts',(-6.71957759739078,-36.2742356160617,
3.30343121875042));
#59892=CARTESIAN_POINT('Ctrl Pts',(-6.67781355062949,-36.2742356173683,
3.26372531825973));
#59893=CARTESIAN_POINT('Ctrl Pts',(-6.6376396712846,-36.2742356186979,3.22255810360343));
#59894=CARTESIAN_POINT('Ctrl Pts',(-6.5990654582959,-36.2742356185244,3.18004119693173));
#59895=CARTESIAN_POINT('Ctrl Pts',(-6.57718261135267,-36.274235618426,3.15592169094288));
#59896=CARTESIAN_POINT('Ctrl Pts',(-6.55581508439785,-36.2742356178269,
3.1313670070968));
#59897=CARTESIAN_POINT('Ctrl Pts',(-6.53496908430346,-36.2742356168316,
3.10639158569407));
#59898=CARTESIAN_POINT('Ctrl Pts',(-6.49664188907379,-36.2742356150015,
3.06047208805849));
#59899=CARTESIAN_POINT('Ctrl Pts',(-6.46006641236599,-36.2742356135502,
3.01310950800297));
#59900=CARTESIAN_POINT('Ctrl Pts',(-6.42534220694393,-36.2742356130965,
2.96437182473463));
#59901=CARTESIAN_POINT('Ctrl Pts',(-6.40199804386673,-36.2742356127915,
2.93160677187331));
#59902=CARTESIAN_POINT('Ctrl Pts',(-6.37949136823164,-36.2742356128032,
2.89821949802322));
#59903=CARTESIAN_POINT('Ctrl Pts',(-6.35786343822196,-36.2742356128012,
2.86422329401434));
#59904=CARTESIAN_POINT('Ctrl Pts',(-6.33095671764626,-36.2742356127988,
2.82192953952689));
#59905=CARTESIAN_POINT('Ctrl Pts',(-6.30539306828795,-36.2742356128,2.77867851495301));
#59906=CARTESIAN_POINT('Ctrl Pts',(-6.28127323414043,-36.2742356128,2.73448936390555));
#59907=CARTESIAN_POINT('Ctrl Pts',(-6.27915867338878,-36.2742356128,2.73061534703287));
#59908=CARTESIAN_POINT('Ctrl Pts',(-6.27705587738,-36.2742356128,2.72673532671));
#59909=CARTESIAN_POINT('Ctrl Pts',(-6.27496307903,-36.2742356128,2.72284588841));
#59910=CARTESIAN_POINT('',(-10.3535103411566,-36.2742356128,0.692258559169219));
#59911=CARTESIAN_POINT('Ctrl Pts',(-10.3535102174,-36.2742356128,0.692259289483));
#59912=CARTESIAN_POINT('Ctrl Pts',(-10.3480579903016,-36.2742356128,0.727045462316002));
#59913=CARTESIAN_POINT('Ctrl Pts',(-10.3425213376762,-36.2742356128,0.761582529081522));
#59914=CARTESIAN_POINT('Ctrl Pts',(-10.3368982634255,-36.2742356128,0.796052242175564));
#59915=CARTESIAN_POINT('Ctrl Pts',(-10.3310793079616,-36.2742356128,0.831722716439654));
#59916=CARTESIAN_POINT('Ctrl Pts',(-10.3251675908898,-36.2742356128,0.867321117622198));
#59917=CARTESIAN_POINT('Ctrl Pts',(-10.3191354058366,-36.2742356128,0.902998219346001));
#59918=CARTESIAN_POINT('Ctrl Pts',(-10.3129769350349,-36.2742356128,0.939422232753249));
#59919=CARTESIAN_POINT('Ctrl Pts',(-10.3066925671242,-36.2742356128,0.975928187824864));
#59920=CARTESIAN_POINT('Ctrl Pts',(-10.3002309954935,-36.2742356128,1.01262505579727));
#59921=CARTESIAN_POINT('Ctrl Pts',(-10.293530416437,-36.2742356128,1.05067930622249));
#59922=CARTESIAN_POINT('Ctrl Pts',(-10.2866389091829,-36.2742356128,1.08893886185183));
#59923=CARTESIAN_POINT('Ctrl Pts',(-10.2794814194908,-36.2742356128,1.1274708876644));
#59924=CARTESIAN_POINT('Ctrl Pts',(-10.2737499087197,-36.2742356128,1.15832621969877));
#59925=CARTESIAN_POINT('Ctrl Pts',(-10.2678473908321,-36.2742356128,1.18935513968225));
#59926=CARTESIAN_POINT('Ctrl Pts',(-10.2617301906119,-36.2742356128,1.22056871200232));
#59927=CARTESIAN_POINT('Ctrl Pts',(-10.2537209481499,-36.2742356128,1.26143660251052));
#59928=CARTESIAN_POINT('Ctrl Pts',(-10.2453441318077,-36.2742356128,1.30261904015665));
#59929=CARTESIAN_POINT('Ctrl Pts',(-10.2364970665051,-36.2742356128,1.34409448776794));
#59930=CARTESIAN_POINT('Ctrl Pts',(-10.2273826990709,-36.2742356128,1.38682306002305));
#59931=CARTESIAN_POINT('Ctrl Pts',(-10.217768515935,-36.2742356128,1.42986240026419));
#59932=CARTESIAN_POINT('Ctrl Pts',(-10.207546645515,-36.2742356128,1.47313438920396));
#59933=CARTESIAN_POINT('Ctrl Pts',(-10.2056609342062,-36.2742356128,1.48111712382525));
#59934=CARTESIAN_POINT('Ctrl Pts',(-10.2037545714597,-36.2742356128,1.4891076361342));
#59935=CARTESIAN_POINT('Ctrl Pts',(-10.2018269270533,-36.2742356128,1.49710525066367));
#59936=CARTESIAN_POINT('Ctrl Pts',(-10.191131512178,-36.2742356128,1.54147951654082));
#59937=CARTESIAN_POINT('Ctrl Pts',(-10.179777778705,-36.2742356128,1.58608219549579));
#59938=CARTESIAN_POINT('Ctrl Pts',(-10.16766492246,-36.2742356128,1.6307873871189));
#59939=CARTESIAN_POINT('Ctrl Pts',(-10.1669020529659,-36.2742356128,1.63360292675943));
#59940=CARTESIAN_POINT('Ctrl Pts',(-10.1661361802017,-36.2742356128,1.63641885774768));
#59941=CARTESIAN_POINT('Ctrl Pts',(-10.1653672823159,-36.2742356128,1.63923514258223));
#59942=CARTESIAN_POINT('Ctrl Pts',(-10.1523898092668,-36.2742356128,1.68676845124615));
#59943=CARTESIAN_POINT('Ctrl Pts',(-10.1385595407206,-36.2742356128,1.73436882358064));
#59944=CARTESIAN_POINT('Ctrl Pts',(-10.123819450048,-36.2742356128,1.78185933117367));
#59945=CARTESIAN_POINT('Ctrl Pts',(-10.1070954365052,-36.2742356128,1.8357417603786));
#59946=CARTESIAN_POINT('Ctrl Pts',(-10.0891534135,-36.2742356127716,1.88957161512486));
#59947=CARTESIAN_POINT('Ctrl Pts',(-10.069899218258,-36.274235614767,1.94320888333938));
#59948=CARTESIAN_POINT('Ctrl Pts',(-10.0549879588562,-36.2742356163123,
1.98474784198701));
#59949=CARTESIAN_POINT('Ctrl Pts',(-10.0392893023929,-36.2742356190629,
2.02617198779279));
#59950=CARTESIAN_POINT('Ctrl Pts',(-10.0227819439559,-36.2742356205281,
2.06741497935644));
#59951=CARTESIAN_POINT('Ctrl Pts',(-10.0055355624289,-36.2742356220589,
2.11050439130175));
#59952=CARTESIAN_POINT('Ctrl Pts',(-9.98745291704985,-36.2742356220055,
2.15327460749465));
#59953=CARTESIAN_POINT('Ctrl Pts',(-9.96854770915045,-36.2742356203452,
2.19566393769648));
#59954=CARTESIAN_POINT('Ctrl Pts',(-9.96662228141052,-36.2742356201761,
2.19998113921482));
#59955=CARTESIAN_POINT('Ctrl Pts',(-9.96468836454892,-36.274235619993,2.20429437570766));
#59956=CARTESIAN_POINT('Ctrl Pts',(-9.96274600376888,-36.2742356197975,
2.20860357150312));
#59957=CARTESIAN_POINT('Ctrl Pts',(-9.94548075860643,-36.2742356180606,
2.24690712593345));
#59958=CARTESIAN_POINT('Ctrl Pts',(-9.92754090731581,-36.2742356158519,
2.28489765236143));
#59959=CARTESIAN_POINT('Ctrl Pts',(-9.90897813049164,-36.2742356146521,
2.32250503559895));
#59960=CARTESIAN_POINT('Ctrl Pts',(-9.90494782982202,-36.2742356143916,
2.33067025049546));
#59961=CARTESIAN_POINT('Ctrl Pts',(-9.90088834402933,-36.2742356141686,
2.33881733230838));
#59962=CARTESIAN_POINT('Ctrl Pts',(-9.89680051537798,-36.2742356139816,
2.34694543639459));
#59963=CARTESIAN_POINT('Ctrl Pts',(-9.87951639572504,-36.2742356131909,
2.38131261162618));
#59964=CARTESIAN_POINT('Ctrl Pts',(-9.86170905446685,-36.2742356130057,
2.41536635168401));
#59965=CARTESIAN_POINT('Ctrl Pts',(-9.84349333770681,-36.2742356129026,
2.44899524721528));
#59966=CARTESIAN_POINT('Ctrl Pts',(-9.82538061717865,-36.2742356128,2.48243399653557));
#59967=CARTESIAN_POINT('Ctrl Pts',(-9.80686377000502,-36.2742356128048,
2.51545283764242));
#59968=CARTESIAN_POINT('Ctrl Pts',(-9.78810607413667,-36.2742356128016,
2.54792653892519));
#59969=CARTESIAN_POINT('Ctrl Pts',(-9.76934837826831,-36.2742356127984,
2.58040024020796));
#59970=CARTESIAN_POINT('Ctrl Pts',(-9.75034951548812,-36.2742356128,2.61232893171438));
#59971=CARTESIAN_POINT('Ctrl Pts',(-9.73132840842276,-36.2742356128,2.64356954426823));
#59972=CARTESIAN_POINT('Ctrl Pts',(-9.73031636916408,-36.2742356128,2.64523173597248));
#59973=CARTESIAN_POINT('Ctrl Pts',(-9.72930457700097,-36.2742356128,2.64689149083652));
#59974=CARTESIAN_POINT('Ctrl Pts',(-9.72829200824,-36.2742356128,2.64855052214));
#59975=CARTESIAN_POINT('Ctrl Pts',(-2.11953809549828,-36.2742356128,-9.31090088052415));
#59976=CARTESIAN_POINT('Ctrl Pts',(-2.1432042809605,-36.2742356128,-9.30658861277567));
#59977=CARTESIAN_POINT('Ctrl Pts',(-2.16685412882638,-36.2742356128,-9.30220459811138));
#59978=CARTESIAN_POINT('Ctrl Pts',(-2.19048902654178,-36.2742356128,-9.29774821966819));
#59979=CARTESIAN_POINT('Ctrl Pts',(-2.35462317202845,-36.2742356128,-9.26680059820831));
#59980=CARTESIAN_POINT('Ctrl Pts',(-2.51797534469943,-36.2742356128001,
-9.23237423419211));
#59981=CARTESIAN_POINT('Ctrl Pts',(-2.68029691391768,-36.2742356128001,
-9.19440935897591));
#59982=CARTESIAN_POINT('Ctrl Pts',(-2.84229564204318,-36.2742356128001,
-9.1565199920354));
#59983=CARTESIAN_POINT('Ctrl Pts',(-3.00326827555196,-36.2742356128001,
-9.11510506553852));
#59984=CARTESIAN_POINT('Ctrl Pts',(-3.16301674313939,-36.2742356128001,
-9.07011799870195));
#59985=CARTESIAN_POINT('Ctrl Pts',(-3.31930702526653,-36.2742356128001,
-9.0261047979862));
#59986=CARTESIAN_POINT('Ctrl Pts',(-3.47442608318702,-36.2742356128,-8.97867151143555));
#59987=CARTESIAN_POINT('Ctrl Pts',(-3.62822837685435,-36.2742356128,-8.9278017362869));
#59988=CARTESIAN_POINT('Ctrl Pts',(-3.78139308336189,-36.2742356128,-8.8771428417089));
#59989=CARTESIAN_POINT('Ctrl Pts',(-3.93325229434668,-36.2742356128,-8.82307493906309));
#59990=CARTESIAN_POINT('Ctrl Pts',(-4.08369592329912,-36.2742356128,-8.7656231571103));
#59991=CARTESIAN_POINT('Ctrl Pts',(-4.22435201933401,-36.2742356128,-8.71190906222974));
#59992=CARTESIAN_POINT('Ctrl Pts',(-4.36377126817408,-36.2742356128,-8.65523679979434));
#59993=CARTESIAN_POINT('Ctrl Pts',(-4.50188619308555,-36.2742356128,-8.59567086336398));
#59994=CARTESIAN_POINT('Ctrl Pts',(-4.51149689899936,-36.2742356128,-8.59152597679303));
#59995=CARTESIAN_POINT('Ctrl Pts',(-4.52110129710902,-36.2742356128,-8.58736709855662));
#59996=CARTESIAN_POINT('Ctrl Pts',(-4.53069936809608,-36.2742356128,-8.58319425943421));
#59997=CARTESIAN_POINT('Ctrl Pts',(-4.653905380685,-36.2742356128,-8.52962944728182));
#59998=CARTESIAN_POINT('Ctrl Pts',(-4.77607707362801,-36.2742356128,-8.47375564208602));
#59999=CARTESIAN_POINT('Ctrl Pts',(-4.89716285107826,-36.2742356128,-8.41561384004806));
#60000=CARTESIAN_POINT('Ctrl Pts',(-5.02947170663252,-36.2742356128,-8.35208304849275));
#60001=CARTESIAN_POINT('Ctrl Pts',(-5.1604834473911,-36.2742356128,-8.28584521369305));
#60002=CARTESIAN_POINT('Ctrl Pts',(-5.29014337296856,-36.2742356128,-8.21701574955886));
#60003=CARTESIAN_POINT('Ctrl Pts',(-5.37098118845278,-36.2742356128,-8.174103311527));
#60004=CARTESIAN_POINT('Ctrl Pts',(-5.45129383189978,-36.2742356128,-8.13018468581161));
#60005=CARTESIAN_POINT('Ctrl Pts',(-5.53107177181599,-36.2742356128,-8.08529551782231));
#60006=CARTESIAN_POINT('Ctrl Pts',(-5.60994290563681,-36.2742356128,-8.04091658826725));
#60007=CARTESIAN_POINT('Ctrl Pts',(-5.68829912285867,-36.2742356128,-7.99558484614536));
#60008=CARTESIAN_POINT('Ctrl Pts',(-5.76613073017276,-36.2742356128,-7.94933895772168));
#60009=CARTESIAN_POINT('Ctrl Pts',(-5.89632002798005,-36.2742356128,-7.87198324134728));
#60010=CARTESIAN_POINT('Ctrl Pts',(-6.02503595167037,-36.2742356128,-7.79207291887174));
#60011=CARTESIAN_POINT('Ctrl Pts',(-6.1522441308659,-36.2742356128,-7.70979855315438));
#60012=CARTESIAN_POINT('Ctrl Pts',(-6.27232259158325,-36.2742356128,-7.63213547162681));
#60013=CARTESIAN_POINT('Ctrl Pts',(-6.39105751633973,-36.2742356128,-7.55236760087967));
#60014=CARTESIAN_POINT('Ctrl Pts',(-6.50845458459874,-36.2742356128,-7.47062987547745));
#60015=CARTESIAN_POINT('Ctrl Pts',(-6.61234621683071,-36.2742356128,-7.39829531182181));
#60016=CARTESIAN_POINT('Ctrl Pts',(-6.71520102544753,-36.2742356127886,
-7.32441168797259));
#60017=CARTESIAN_POINT('Ctrl Pts',(-6.81708760544559,-36.2742356128114,
-7.24900408693246));
#60018=CARTESIAN_POINT('Ctrl Pts',(-6.86842159421278,-36.2742356128229,
-7.21101112510345));
#60019=CARTESIAN_POINT('Ctrl Pts',(-6.919510141846,-36.2742356128435,-7.17263064176347));
#60020=CARTESIAN_POINT('Ctrl Pts',(-6.97036425874489,-36.2742356129319,
-7.13386121169139));
#60021=CARTESIAN_POINT('Ctrl Pts',(-7.06478009632977,-36.274235613096,-7.0618818236662));
#60022=CARTESIAN_POINT('Ctrl Pts',(-7.15843501790257,-36.2742356129223,
-6.98854451497165));
#60023=CARTESIAN_POINT('Ctrl Pts',(-7.25136378947047,-36.2742356128455,
-6.91383222628363));
#60024=CARTESIAN_POINT('Ctrl Pts',(-7.30783258389914,-36.2742356127988,
-6.86843280046494));
#60025=CARTESIAN_POINT('Ctrl Pts',(-7.36403369072445,-36.2742356128,-6.8225248802803));
#60026=CARTESIAN_POINT('Ctrl Pts',(-7.41997923973695,-36.2742356128,-6.7760961334252));
#60027=CARTESIAN_POINT('Ctrl Pts',(-7.52440937719628,-36.2742356128,-6.68943042897284));
#60028=CARTESIAN_POINT('Ctrl Pts',(-7.62796140085615,-36.2742356128,-6.60095511075596));
#60029=CARTESIAN_POINT('Ctrl Pts',(-7.73046643660877,-36.2742356128,-6.51068806246407));
#60030=CARTESIAN_POINT('Ctrl Pts',(-7.83073696140362,-36.2742356128,-6.42238874880153));
#60031=CARTESIAN_POINT('Ctrl Pts',(-7.93000558009221,-36.2742356128,-6.33237534185209));
#60032=CARTESIAN_POINT('Ctrl Pts',(-8.02807297507958,-36.2742356128,-6.2406374376305));
#60033=CARTESIAN_POINT('Ctrl Pts',(-8.12407285064597,-36.2742356128,-6.15083361046521));
#60034=CARTESIAN_POINT('Ctrl Pts',(-8.21892155557018,-36.2742356128,-6.05937754589244));
#60035=CARTESIAN_POINT('Ctrl Pts',(-8.31239309349182,-36.2742356128,-5.96622819442902));
#60036=CARTESIAN_POINT('Ctrl Pts',(-8.4031368230666,-36.2742356128,-5.87579724884696));
#60037=CARTESIAN_POINT('Ctrl Pts',(-8.4925824812243,-36.2742356128,-5.7837706089873));
#60038=CARTESIAN_POINT('Ctrl Pts',(-8.58048747027233,-36.2742356128,-5.6900772537884));
#60039=CARTESIAN_POINT('Ctrl Pts',(-8.66700528995599,-36.2742356128,-5.59786241025743));
#60040=CARTESIAN_POINT('Ctrl Pts',(-8.75203065067016,-36.2742356128,-5.50403327768024));
#60041=CARTESIAN_POINT('Ctrl Pts',(-8.83529796619582,-36.2742356128,-5.4084859080225));
#60042=CARTESIAN_POINT('Ctrl Pts',(-8.91673430633736,-36.2742356128,-5.31503954139046));
#60043=CARTESIAN_POINT('Ctrl Pts',(-8.99648900098376,-36.2742356128,-5.21994983342886));
#60044=CARTESIAN_POINT('Ctrl Pts',(-9.07428130247451,-36.2742356128,-5.12308174646508));
#60045=CARTESIAN_POINT('Ctrl Pts',(-9.11371256086522,-36.2742356128,-5.07398137928625));
#60046=CARTESIAN_POINT('Ctrl Pts',(-9.15263911624697,-36.2742356128,-5.02442347780941));
#60047=CARTESIAN_POINT('Ctrl Pts',(-9.19102120553304,-36.2742356128,-4.97438641806384));
#60048=CARTESIAN_POINT('Ctrl Pts',(-9.27135473353872,-36.2742356128,-4.86965909302337));
#60049=CARTESIAN_POINT('Ctrl Pts',(-9.34931008261837,-36.2742356128,-4.76281768826537));
#60050=CARTESIAN_POINT('Ctrl Pts',(-9.4243664421214,-36.2742356128,-4.65380960606161));
#60051=CARTESIAN_POINT('Ctrl Pts',(-9.47733401721219,-36.2742356128,-4.57688216356558));
#60052=CARTESIAN_POINT('Ctrl Pts',(-9.52885782823991,-36.2742356128,-4.49887605020695));
#60053=CARTESIAN_POINT('Ctrl Pts',(-9.57876242917955,-36.2742356128,-4.41978698025841));
#60054=CARTESIAN_POINT('Ctrl Pts',(-9.61242567371991,-36.2742356128,-4.36643729602053));
#60055=CARTESIAN_POINT('Ctrl Pts',(-9.64535662293559,-36.2742356128,-4.31258838992345));
#60056=CARTESIAN_POINT('Ctrl Pts',(-9.6775073418473,-36.2742356128,-4.25823628901775));
#60057=CARTESIAN_POINT('Ctrl Pts',(-9.73227334817142,-36.2742356128,-4.1656521228563));
#60058=CARTESIAN_POINT('Ctrl Pts',(-9.78477154511798,-36.2742356128,-4.07160923888473));
#60059=CARTESIAN_POINT('Ctrl Pts',(-9.83477068606681,-36.2742356128,-3.97613665347847));
#60060=CARTESIAN_POINT('Ctrl Pts',(-9.86501146635147,-36.2742356128,-3.91839235180268));
#60061=CARTESIAN_POINT('Ctrl Pts',(-9.89433851557226,-36.2742356128,-3.86012577086578));
#60062=CARTESIAN_POINT('Ctrl Pts',(-9.92270588308633,-36.2742356128,-3.80135120370847));
#60063=CARTESIAN_POINT('Ctrl Pts',(-9.96655495577847,-36.2742356128,-3.71049997239656));
#60064=CARTESIAN_POINT('Ctrl Pts',(-10.0081226102412,-36.2742356128,-3.61840409165624));
#60065=CARTESIAN_POINT('Ctrl Pts',(-10.0472459446408,-36.2742356128,-3.52517965095815));
#60066=CARTESIAN_POINT('Ctrl Pts',(-10.0837578615216,-36.2742356128,-3.43817778666758));
#60067=CARTESIAN_POINT('Ctrl Pts',(-10.1181408830724,-36.2742356128,-3.3501931104458));
#60068=CARTESIAN_POINT('Ctrl Pts',(-10.1502938375145,-36.2742356128,-3.26135920624506));
#60069=CARTESIAN_POINT('Ctrl Pts',(-10.1525934918653,-36.2742356128,-3.25500559806695));
#60070=CARTESIAN_POINT('Ctrl Pts',(-10.1548817525012,-36.2742356128,-3.24864766298652));
#60071=CARTESIAN_POINT('Ctrl Pts',(-10.1571585890232,-36.2742356128,-3.24228545796934));
#60072=CARTESIAN_POINT('Ctrl Pts',(-10.1873913807981,-36.2742356128,-3.1578054271638));
#60073=CARTESIAN_POINT('Ctrl Pts',(-10.2156163880341,-36.2742356128,-3.07254357398699));
#60074=CARTESIAN_POINT('Ctrl Pts',(-10.2417876145186,-36.2742356128,-2.98665974253318));
#60075=CARTESIAN_POINT('Ctrl Pts',(-10.2689167782626,-36.2742356128,-2.89763233192031));
#60076=CARTESIAN_POINT('Ctrl Pts',(-10.2938392644185,-36.2742356128,-2.80793667316511));
#60077=CARTESIAN_POINT('Ctrl Pts',(-10.3165575839241,-36.2742356128,-2.7177359139567));
#60078=CARTESIAN_POINT('Ctrl Pts',(-10.3213777705173,-36.2742356128,-2.69859785710684));
#60079=CARTESIAN_POINT('Ctrl Pts',(-10.326098911838,-36.2742356128,-2.67943700760276));
#60080=CARTESIAN_POINT('Ctrl Pts',(-10.330721313039,-36.2742356128,-2.66025483528842));
#60081=CARTESIAN_POINT('Ctrl Pts',(-10.3528699418875,-36.2742356128,-2.56834182371183));
#60082=CARTESIAN_POINT('Ctrl Pts',(-10.3727493785979,-36.2742356128,-2.47593200036486));
#60083=CARTESIAN_POINT('Ctrl Pts',(-10.3904135773074,-36.2742356128,-2.38322042713068));
#60084=CARTESIAN_POINT('Ctrl Pts',(-10.398691197646,-36.2742356128,-2.33977485584547));
#60085=CARTESIAN_POINT('Ctrl Pts',(-10.4064831129282,-36.2742356128,-2.29626280366837));
#60086=CARTESIAN_POINT('Ctrl Pts',(-10.4137985541644,-36.2742356128,-2.25270313971161));
#60087=CARTESIAN_POINT('Ctrl Pts',(-10.430672018222,-36.2742356128,-2.15223039987303));
#60088=CARTESIAN_POINT('Ctrl Pts',(-10.4449859145385,-36.2742356121164,
-2.05149538873562));
#60089=CARTESIAN_POINT('Ctrl Pts',(-10.4569090914569,-36.2742356176125,
-1.95069270481178));
#60090=CARTESIAN_POINT('Ctrl Pts',(-10.4611862193506,-36.2742356195841,
-1.91453237823736));
#60091=CARTESIAN_POINT('Ctrl Pts',(-10.465156138689,-36.2742356223624,-1.87836308786589));
#60092=CARTESIAN_POINT('Ctrl Pts',(-10.4688279745932,-36.2742356259991,
-1.84219295236756));
#60093=CARTESIAN_POINT('Ctrl Pts',(-10.48024327157,-36.2742356373051,-1.7297443437734));
#60094=CARTESIAN_POINT('Ctrl Pts',(-10.4887947228398,-36.2742356503102,
-1.61726739875892));
#60095=CARTESIAN_POINT('Ctrl Pts',(-10.4947633362093,-36.2742356548179,
-1.50495659874232));
#60096=CARTESIAN_POINT('Ctrl Pts',(-10.5011033567854,-36.274235659606,-1.38565706651662));
#60097=CARTESIAN_POINT('Ctrl Pts',(-10.5045307178127,-36.2742356547264,
-1.26654556817452));
#60098=CARTESIAN_POINT('Ctrl Pts',(-10.5054136103061,-36.2742356439644,
-1.14780685036128));
#60099=CARTESIAN_POINT('Ctrl Pts',(-10.5057246075479,-36.2742356401736,
-1.10598135743335));
#60100=CARTESIAN_POINT('Ctrl Pts',(-10.5057200383727,-36.2742356357964,
-1.06420166036534));
#60101=CARTESIAN_POINT('Ctrl Pts',(-10.5054162157459,-36.2742356314567,
-1.02247432570434));
#60102=CARTESIAN_POINT('Ctrl Pts',(-10.5045830083842,-36.2742356195555,
-0.908040707645507));
#60103=CARTESIAN_POINT('Ctrl Pts',(-10.5014747563221,-36.2742356163105,
-0.79393675611565));
#60104=CARTESIAN_POINT('Ctrl Pts',(-10.496415029551,-36.2742356145671,-0.680268028397453));
#60105=CARTESIAN_POINT('Ctrl Pts',(-10.4917546355556,-36.2742356129613,
-0.575570466636018));
#60106=CARTESIAN_POINT('Ctrl Pts',(-10.4854396323409,-36.2742356129067,
-0.4712417088829));
#60107=CARTESIAN_POINT('Ctrl Pts',(-10.4776986870203,-36.2742356128358,
-0.367328990181301));
#60108=CARTESIAN_POINT('Ctrl Pts',(-10.4719656657543,-36.2742356127833,
-0.290370194909717));
#60109=CARTESIAN_POINT('Ctrl Pts',(-10.4654501123239,-36.2742356128,-0.21363890449008));
#60110=CARTESIAN_POINT('Ctrl Pts',(-10.4582308198287,-36.2742356128,-0.137142046369777));
#60111=CARTESIAN_POINT('Ctrl Pts',(-10.4493364654897,-36.2742356128,-0.0428959464369612));
#60112=CARTESIAN_POINT('Ctrl Pts',(-10.4393783264163,-36.2742356128,0.0509843559394398));
#60113=CARTESIAN_POINT('Ctrl Pts',(-10.4284676904419,-36.2742356128,0.14450999181293));
#60114=CARTESIAN_POINT('Ctrl Pts',(-10.4180812512127,-36.2742356128,0.233542229314824));
#60115=CARTESIAN_POINT('Ctrl Pts',(-10.4068319117135,-36.2742356128,0.322253206188292));
#60116=CARTESIAN_POINT('Ctrl Pts',(-10.3947746327428,-36.2742356128,0.41067344725918));
#60117=CARTESIAN_POINT('Ctrl Pts',(-10.3853531073324,-36.2742356128,0.479764786197444));
#60118=CARTESIAN_POINT('Ctrl Pts',(-10.3754375603691,-36.2742356128,0.548679007393723));
#60119=CARTESIAN_POINT('Ctrl Pts',(-10.3650337459782,-36.2742356128,0.617439519286842));
#60120=CARTESIAN_POINT('Ctrl Pts',(-10.3621231885442,-36.2742356128,0.636675869680322));
#60121=CARTESIAN_POINT('Ctrl Pts',(-10.3591742392757,-36.2742356128,0.655900638740825));
#60122=CARTESIAN_POINT('Ctrl Pts',(-10.3561866610074,-36.2742356128,0.675114926906024));
#60123=CARTESIAN_POINT('Ctrl Pts',(-10.3552979558047,-36.2742356128,0.680830538791121));
#60124=CARTESIAN_POINT('Ctrl Pts',(-10.3544061621333,-36.2742356128,0.686543110974668));
#60125=CARTESIAN_POINT('Ctrl Pts',(-10.3535104648,-36.2742356128,0.692257829523));
#60126=CARTESIAN_POINT('',(-5.5398869008,-36.2742356128,5.60697988192));
#60127=CARTESIAN_POINT('',(-2.46701990945003E-5,-36.2742356128,10.9643459861));
#60128=CARTESIAN_POINT('Ctrl Pts',(-5.5398869008,-36.2742356128,5.60697988192));
#60129=CARTESIAN_POINT('Ctrl Pts',(-5.5346953901423,-36.2742356128,5.76156714385257));
#60130=CARTESIAN_POINT('Ctrl Pts',(-5.52304547085452,-36.2742356128,5.91594818570587));
#60131=CARTESIAN_POINT('Ctrl Pts',(-5.50496486738705,-36.2742356128,6.06957376603556));
#60132=CARTESIAN_POINT('Ctrl Pts',(-5.48674534930841,-36.2742356128,6.22437966303974));
#60133=CARTESIAN_POINT('Ctrl Pts',(-5.46199605025368,-36.2742356128,6.37841824757372));
#60134=CARTESIAN_POINT('Ctrl Pts',(-5.43079794581926,-36.2742356128,6.53113717557828));
#60135=CARTESIAN_POINT('Ctrl Pts',(-5.3993756059117,-36.2742356128,6.68495376646011));
#60136=CARTESIAN_POINT('Ctrl Pts',(-5.36141153554192,-36.2742356128,6.83743145494455));
#60137=CARTESIAN_POINT('Ctrl Pts',(-5.31704005924504,-36.2742356128,6.98801872521846));
#60138=CARTESIAN_POINT('Ctrl Pts',(-5.27237815171884,-36.2742356128,7.13959165677023));
#60139=CARTESIAN_POINT('Ctrl Pts',(-5.22122480697047,-36.2742356128,7.28924912531629));
#60140=CARTESIAN_POINT('Ctrl Pts',(-5.16376732938617,-36.2742356128,7.43644486626614));
#60141=CARTESIAN_POINT('Ctrl Pts',(-5.10582843211048,-36.2742356128,7.58487391802533));
#60142=CARTESIAN_POINT('Ctrl Pts',(-5.04147943369501,-36.2742356128,7.73079958280341));
#60143=CARTESIAN_POINT('Ctrl Pts',(-4.97096161827184,-36.2742356128,7.87368154053936));
#60144=CARTESIAN_POINT('Ctrl Pts',(-4.90018282130001,-36.2742356128,8.01709229450049));
#60145=CARTESIAN_POINT('Ctrl Pts',(-4.82318962125999,-36.2742356128,8.15743654403781));
#60146=CARTESIAN_POINT('Ctrl Pts',(-4.7402732528861,-36.2742356128,8.29419125952485));
#60147=CARTESIAN_POINT('Ctrl Pts',(-4.6570241839819,-36.2742356128,8.43149470100239));
#60148=CARTESIAN_POINT('Ctrl Pts',(-4.56780448001639,-36.2742356128,8.56517951035103));
#60149=CARTESIAN_POINT('Ctrl Pts',(-4.47295403381865,-36.2742356128,8.69474326837329));
#60150=CARTESIAN_POINT('Ctrl Pts',(-4.41538891090186,-36.2742356128,8.77337604191411));
#60151=CARTESIAN_POINT('Ctrl Pts',(-4.35575066660558,-36.2742356128,8.85049143545389));
#60152=CARTESIAN_POINT('Ctrl Pts',(-4.29412294654456,-36.2742356128,8.92598250047464));
#60153=CARTESIAN_POINT('Ctrl Pts',(-4.19173460457658,-36.2742356128,9.05140341452465));
#60154=CARTESIAN_POINT('Ctrl Pts',(-4.0838526562137,-36.2742356128,9.17233904229695));
#60155=CARTESIAN_POINT('Ctrl Pts',(-3.97089095617117,-36.2742356128,9.28832809052255));
#60156=CARTESIAN_POINT('Ctrl Pts',(-3.85796902574901,-36.2742356128,9.40427630331089));
#60157=CARTESIAN_POINT('Ctrl Pts',(-3.73997114015286,-36.2742356128,9.51528119940368));
#60158=CARTESIAN_POINT('Ctrl Pts',(-3.61734836254789,-36.2742356128001,
9.62091792946744));
#60159=CARTESIAN_POINT('Ctrl Pts',(-3.49495417070753,-36.2742356128001,
9.72635773810123));
#60160=CARTESIAN_POINT('Ctrl Pts',(-3.36795254093104,-36.2742356128002,
9.8264491681409));
#60161=CARTESIAN_POINT('Ctrl Pts',(-3.23682616443467,-36.2742356128003,
9.92080875803141));
#60162=CARTESIAN_POINT('Ctrl Pts',(-3.10613251965052,-36.2742356128004,
10.0148569507188));
#60163=CARTESIAN_POINT('Ctrl Pts',(-2.9713415378996,-36.2742356128006,10.1032108784461));
#60164=CARTESIAN_POINT('Ctrl Pts',(-2.83296166688316,-36.2742356128007,
10.1855326471265));
#60165=CARTESIAN_POINT('Ctrl Pts',(-2.69559582751787,-36.2742356128008,
10.2672511714303));
#60166=CARTESIAN_POINT('Ctrl Pts',(-2.55469374396532,-36.2742356128009,
10.3430254623245));
#60167=CARTESIAN_POINT('Ctrl Pts',(-2.41077935977487,-36.2742356128009,
10.412568804815));
#60168=CARTESIAN_POINT('Ctrl Pts',(-2.26762762952295,-36.274235612801,10.481743612191));
#60169=CARTESIAN_POINT('Ctrl Pts',(-2.12149566208515,-36.274235612801,10.5447531729252));
#60170=CARTESIAN_POINT('Ctrl Pts',(-1.97292210274691,-36.2742356128009,
10.6013612096786));
#60171=CARTESIAN_POINT('Ctrl Pts',(-1.82570947854556,-36.2742356128008,
10.6574507163074));
#60172=CARTESIAN_POINT('Ctrl Pts',(-1.67610001053631,-36.2742356128007,
10.707255314709));
#60173=CARTESIAN_POINT('Ctrl Pts',(-1.52463698246422,-36.2742356128005,
10.7505924289492));
#60174=CARTESIAN_POINT('Ctrl Pts',(-1.44518898427323,-36.2742356128004,
10.7733243590946));
#60175=CARTESIAN_POINT('Ctrl Pts',(-1.36523130057623,-36.2742356128003,
10.7942776299538));
#60176=CARTESIAN_POINT('Ctrl Pts',(-1.28484418209153,-36.2742356128002,
10.8134313424015));
#60177=CARTESIAN_POINT('Ctrl Pts',(-1.13262152986081,-36.2742356128,10.8497011946341));
#60178=CARTESIAN_POINT('Ctrl Pts',(-0.978861102002178,-36.2742356128,10.8795144100532));
#60179=CARTESIAN_POINT('Ctrl Pts',(-0.82411483131256,-36.2742356128,10.9027686625403));
#60180=CARTESIAN_POINT('Ctrl Pts',(-0.671184727618257,-36.2742356128,10.9257499933881));
#60181=CARTESIAN_POINT('Ctrl Pts',(-0.517291966768855,-36.2742356128,10.9423253362505));
#60182=CARTESIAN_POINT('Ctrl Pts',(-0.362980351578935,-36.2742356128,10.9524454430755));
#60183=CARTESIAN_POINT('Ctrl Pts',(-0.272471115856985,-36.2742356128,10.9583812446873));
#60184=CARTESIAN_POINT('Ctrl Pts',(-0.181817979358742,-36.2742356128,10.9620972299496));
#60185=CARTESIAN_POINT('Ctrl Pts',(-0.0911321048928935,-36.2742356128,10.9635917110187));
#60186=CARTESIAN_POINT('Ctrl Pts',(-0.0660653661594743,-36.2742356128,10.9640048047526));
#60187=CARTESIAN_POINT('Ctrl Pts',(-0.0409957765907243,-36.2742356128,10.9642482065052));
#60188=CARTESIAN_POINT('Ctrl Pts',(-0.0159262763392949,-36.2742356128,10.9643219569687));
#60189=CARTESIAN_POINT('Ctrl Pts',(-0.0106256139653286,-36.2742356128,10.9643375506703));
#60190=CARTESIAN_POINT('Ctrl Pts',(-0.00532495008970526,-36.2742356128,
10.9643455597667));
#60191=CARTESIAN_POINT('Ctrl Pts',(-2.46701990951337E-5,-36.2742356128,
10.9643459861));
#60192=CARTESIAN_POINT('',(-4.67790704727252,-36.2742356128007,1.76602464761587));
#60193=CARTESIAN_POINT('Ctrl Pts',(-4.67800175527594,-36.2742356128,1.76632657424107));
#60194=CARTESIAN_POINT('Ctrl Pts',(-4.69198401483433,-36.2742356128,1.81130696346438));
#60195=CARTESIAN_POINT('Ctrl Pts',(-4.705344244229,-36.2742356128112,1.85562502943862));
#60196=CARTESIAN_POINT('Ctrl Pts',(-4.71832385294181,-36.2742356128199,
1.89944120814255));
#60197=CARTESIAN_POINT('Ctrl Pts',(-4.73151535902486,-36.2742356128287,
1.94397270371365));
#60198=CARTESIAN_POINT('Ctrl Pts',(-4.74431347042368,-36.2742356128363,
1.98798562464597));
#60199=CARTESIAN_POINT('Ctrl Pts',(-4.75692050655433,-36.2742356128616,
2.03162435033008));
#60200=CARTESIAN_POINT('Ctrl Pts',(-4.77000908213447,-36.2742356128878,
2.07692990457919));
#60201=CARTESIAN_POINT('Ctrl Pts',(-4.78289163080876,-36.2742356129249,
2.12183203129925));
#60202=CARTESIAN_POINT('Ctrl Pts',(-4.79574215657131,-36.2742356130778,
2.16646854508074));
#60203=CARTESIAN_POINT('Ctrl Pts',(-4.80705064219312,-36.2742356132124,
2.20574875692834));
#60204=CARTESIAN_POINT('Ctrl Pts',(-4.81833339247835,-36.2742356134291,
2.24482282251678));
#60205=CARTESIAN_POINT('Ctrl Pts',(-4.82967844196943,-36.2742356139743,
2.28377145245306));
#60206=CARTESIAN_POINT('Ctrl Pts',(-4.84309399664076,-36.2742356146189,
2.32982832286991));
#60207=CARTESIAN_POINT('Ctrl Pts',(-4.85663254045109,-36.2742356167299,
2.3758619561797));
#60208=CARTESIAN_POINT('Ctrl Pts',(-4.87035410558333,-36.2742356218589,
2.42180875135198));
#60209=CARTESIAN_POINT('Ctrl Pts',(-4.88114209308927,-36.2742356258913,
2.45793243312445));
#60210=CARTESIAN_POINT('Ctrl Pts',(-4.8920422151928,-36.274235631805,2.4940022482321));
#60211=CARTESIAN_POINT('Ctrl Pts',(-4.90306179734455,-36.2742356374317,
2.52998105296957));
#60212=CARTESIAN_POINT('Ctrl Pts',(-4.91857234662679,-36.2742356453514,
2.58062281200475));
#60213=CARTESIAN_POINT('Ctrl Pts',(-4.93433974729081,-36.274235650124,2.63113356670393));
#60214=CARTESIAN_POINT('Ctrl Pts',(-4.95040944020017,-36.2742356495911,
2.68169254618777));
#60215=CARTESIAN_POINT('Ctrl Pts',(-4.96027798559937,-36.2742356492639,
2.71274127793313));
#60216=CARTESIAN_POINT('Ctrl Pts',(-4.97025944992807,-36.2742356470856,
2.74380776889054));
#60217=CARTESIAN_POINT('Ctrl Pts',(-4.98035527463554,-36.2742356436435,
2.77493058470113));
#60218=CARTESIAN_POINT('Ctrl Pts',(-4.99775694492439,-36.2742356377105,
2.82857543243661));
#60219=CARTESIAN_POINT('Ctrl Pts',(-5.01549138037413,-36.2742356323325,
2.88238703379159));
#60220=CARTESIAN_POINT('Ctrl Pts',(-5.03348596356622,-36.27423562799,2.9364371383734));
#60221=CARTESIAN_POINT('Ctrl Pts',(-5.05350905181838,-36.2742356231581,
2.9965802382456));
#60222=CARTESIAN_POINT('Ctrl Pts',(-5.07385411249554,-36.2742356196165,
3.05701811984453));
#60223=CARTESIAN_POINT('Ctrl Pts',(-5.09435518995256,-36.2742356172974,
3.11783961754101));
#60224=CARTESIAN_POINT('Ctrl Pts',(-5.11697946350513,-36.2742356147382,
3.18496009960577));
#60225=CARTESIAN_POINT('Ctrl Pts',(-5.13979261948919,-36.2742356136397,
3.25254656888927));
#60226=CARTESIAN_POINT('Ctrl Pts',(-5.16250518657835,-36.2742356131765,
3.32072084496247));
#60227=CARTESIAN_POINT('Ctrl Pts',(-5.18560887764447,-36.2742356127054,
3.39006912280654));
#60228=CARTESIAN_POINT('Ctrl Pts',(-5.20860586975898,-36.2742356128,3.46002414789234));
#60229=CARTESIAN_POINT('Ctrl Pts',(-5.23115686865635,-36.2742356128,3.53073768416982));
#60230=CARTESIAN_POINT('Ctrl Pts',(-5.25137840927041,-36.2742356128,3.59414669998799));
#60231=CARTESIAN_POINT('Ctrl Pts',(-5.27126682535185,-36.2742356128,3.65823688138688));
#60232=CARTESIAN_POINT('Ctrl Pts',(-5.29057772872032,-36.2742356128,3.72303682547084));
#60233=CARTESIAN_POINT('Ctrl Pts',(-5.31043088538772,-36.2742356128,3.78965636249563));
#60234=CARTESIAN_POINT('Ctrl Pts',(-5.32967208410964,-36.2742356128,3.85702515017592));
#60235=CARTESIAN_POINT('Ctrl Pts',(-5.34803592730172,-36.2742356128,3.92511801119792));
#60236=CARTESIAN_POINT('Ctrl Pts',(-5.3656885232509,-36.2742356128,3.99057357788252));
#60237=CARTESIAN_POINT('Ctrl Pts',(-5.38252963521041,-36.2742356128,4.05669852810358));
#60238=CARTESIAN_POINT('Ctrl Pts',(-5.39834060086143,-36.2742356128,4.12342537331533));
#60239=CARTESIAN_POINT('Ctrl Pts',(-5.4140940065713,-36.2742356128,4.18990929893772));
#60240=CARTESIAN_POINT('Ctrl Pts',(-5.42882371242491,-36.2742356128,4.25699046577942));
#60241=CARTESIAN_POINT('Ctrl Pts',(-5.44234517887241,-36.2742356128,4.32455897862455));
#60242=CARTESIAN_POINT('Ctrl Pts',(-5.45153207351824,-36.2742356128,4.37046707678046));
#60243=CARTESIAN_POINT('Ctrl Pts',(-5.46016234726271,-36.2742356128,4.41660102851775));
#60244=CARTESIAN_POINT('Ctrl Pts',(-5.46819181711895,-36.2742356128,4.46292801882197));
#60245=CARTESIAN_POINT('Ctrl Pts',(-5.47904486691391,-36.2742356128,4.52554599256428));
#60246=CARTESIAN_POINT('Ctrl Pts',(-5.48879737839669,-36.2742356128,4.58851297281068));
#60247=CARTESIAN_POINT('Ctrl Pts',(-5.49737103594156,-36.2742356128,4.65170380600931));
#60248=CARTESIAN_POINT('Ctrl Pts',(-5.50560634546158,-36.2742356128,4.71240089677772));
#60249=CARTESIAN_POINT('Ctrl Pts',(-5.5127537305799,-36.2742356128,4.77330424861653));
#60250=CARTESIAN_POINT('Ctrl Pts',(-5.51878676668022,-36.2742356128,4.83428226178526));
#60251=CARTESIAN_POINT('Ctrl Pts',(-5.52234392131188,-36.2742356128,4.87023567203606));
#60252=CARTESIAN_POINT('Ctrl Pts',(-5.52551451797872,-36.2742356128,4.90621466424306));
#60253=CARTESIAN_POINT('Ctrl Pts',(-5.52830117031403,-36.2742356128,4.94218922880154));
#60254=CARTESIAN_POINT('Ctrl Pts',(-5.53276441084929,-36.2742356128,4.99980787492446));
#60255=CARTESIAN_POINT('Ctrl Pts',(-5.536241669784,-36.2742356128,5.05743511975529));
#60256=CARTESIAN_POINT('Ctrl Pts',(-5.53877783630915,-36.2742356128,5.11493113448532));
#60257=CARTESIAN_POINT('Ctrl Pts',(-5.54126560210858,-36.2742356128,5.17132988339643));
#60258=CARTESIAN_POINT('Ctrl Pts',(-5.542847624125,-36.2742356128,5.22760222608721));
#60259=CARTESIAN_POINT('Ctrl Pts',(-5.5436136967884,-36.2742356128,5.28360428844439));
#60260=CARTESIAN_POINT('Ctrl Pts',(-5.54435882909874,-36.2742356128,5.338075552206));
#60261=CARTESIAN_POINT('Ctrl Pts',(-5.54433190551395,-36.2742356128,5.39229097618915));
#60262=CARTESIAN_POINT('Ctrl Pts',(-5.54366316138914,-36.2742356128,5.4461087902728));
#60263=CARTESIAN_POINT('Ctrl Pts',(-5.54301952581734,-36.2742356128,5.49790596987407));
#60264=CARTESIAN_POINT('Ctrl Pts',(-5.54178138873351,-36.2742356128,5.54933471403915));
#60265=CARTESIAN_POINT('Ctrl Pts',(-5.54010996325318,-36.2742356128,5.60026168051131));
#60266=CARTESIAN_POINT('Ctrl Pts',(-5.54003643972157,-36.2742356128,5.60250188234686));
#60267=CARTESIAN_POINT('Ctrl Pts',(-5.53996208891191,-36.2742356128,5.60474108660317));
#60268=CARTESIAN_POINT('Ctrl Pts',(-5.5398869008,-36.2742356128,5.60697988192));
#60269=CARTESIAN_POINT('',(-0.665818988042834,-36.2742356128,-2.24488955640065));
#60270=CARTESIAN_POINT('Ctrl Pts',(-0.665819092629,-36.2742356128,-2.2448895341));
#60271=CARTESIAN_POINT('Ctrl Pts',(-0.737228677932033,-36.2742356128,-2.23017916472095));
#60272=CARTESIAN_POINT('Ctrl Pts',(-0.808566626719662,-36.2742356127611,
-2.21435533917569));
#60273=CARTESIAN_POINT('Ctrl Pts',(-0.879795665857112,-36.2742356129554,
-2.19738461926913));
#60274=CARTESIAN_POINT('Ctrl Pts',(-0.954705463597933,-36.2742356131597,
-2.17953693788649));
#60275=CARTESIAN_POINT('Ctrl Pts',(-1.02949530188753,-36.2742356136668,
-2.16041996465169));
#60276=CARTESIAN_POINT('Ctrl Pts',(-1.10409917953572,-36.2742356148821,
-2.1399379701008));
#60277=CARTESIAN_POINT('Ctrl Pts',(-1.18453540429552,-36.2742356161925,
-2.11785474374367));
#60278=CARTESIAN_POINT('Ctrl Pts',(-1.26475633734396,-36.2742356183635,
-2.09418353794173));
#60279=CARTESIAN_POINT('Ctrl Pts',(-1.34464241851358,-36.2742356213129,
-2.06875540131051));
#60280=CARTESIAN_POINT('Ctrl Pts',(-1.38843799632301,-36.2742356229299,
-2.05481505125108));
#60281=CARTESIAN_POINT('Ctrl Pts',(-1.43213222438249,-36.2742356247662,
-2.0403459268008));
#60282=CARTESIAN_POINT('Ctrl Pts',(-1.47569974337329,-36.2742356267012,
-2.02531691033586));
#60283=CARTESIAN_POINT('Ctrl Pts',(-1.54285372709818,-36.2742356296839,
-2.0021515258828));
#60284=CARTESIAN_POINT('Ctrl Pts',(-1.60972379741354,-36.2742356283408,
-1.97766308160781));
#60285=CARTESIAN_POINT('Ctrl Pts',(-1.67619838733452,-36.2742356240296,
-1.95173199462251));
#60286=CARTESIAN_POINT('Ctrl Pts',(-1.742672977254,-36.2742356197183,-1.9258009076378));
#60287=CARTESIAN_POINT('Ctrl Pts',(-1.80876937761299,-36.2742356150089,
-1.89841859520787));
#60288=CARTESIAN_POINT('Ctrl Pts',(-1.87430531806608,-36.2742356139044,
-1.86946353977244));
#60289=CARTESIAN_POINT('Ctrl Pts',(-1.94075639204582,-36.2742356127845,
-1.84010416051391));
#60290=CARTESIAN_POINT('Ctrl Pts',(-2.00662329644622,-36.2742356128485,
-1.80914041603183));
#60291=CARTESIAN_POINT('Ctrl Pts',(-2.07172628696219,-36.2742356128159,
-1.77648961183462));
#60292=CARTESIAN_POINT('Ctrl Pts',(-2.13502947445721,-36.2742356127841,
-1.74474145459058));
#60293=CARTESIAN_POINT('Ctrl Pts',(-2.19761044716111,-36.2742356128,-1.7113975703382));
#60294=CARTESIAN_POINT('Ctrl Pts',(-2.25927107931469,-36.2742356128,-1.67641596621023));
#60295=CARTESIAN_POINT('Ctrl Pts',(-2.32014698221066,-36.2742356128,-1.64187955843005));
#60296=CARTESIAN_POINT('Ctrl Pts',(-2.3801290898588,-36.2742356128,-1.60574174956389));
#60297=CARTESIAN_POINT('Ctrl Pts',(-2.43909548117802,-36.2742356128,-1.56799290777033));
#60298=CARTESIAN_POINT('Ctrl Pts',(-2.49915480898836,-36.2742356128,-1.52954439476116));
#60299=CARTESIAN_POINT('Ctrl Pts',(-2.55816012613216,-36.2742356128,-1.48942481668619));
#60300=CARTESIAN_POINT('Ctrl Pts',(-2.6159991563388,-36.2742356128,-1.44767594041806));
#60301=CARTESIAN_POINT('Ctrl Pts',(-2.67546098795818,-36.2742356128,-1.40475570745278));
#60302=CARTESIAN_POINT('Ctrl Pts',(-2.73368979290356,-36.2742356128,-1.36011369078322));
#60303=CARTESIAN_POINT('Ctrl Pts',(-2.79058610628415,-36.2742356128,-1.31384619761134));
#60304=CARTESIAN_POINT('Ctrl Pts',(-2.83586651357112,-36.2742356128,-1.2770246390517));
#60305=CARTESIAN_POINT('Ctrl Pts',(-2.88030335942422,-36.2742356128,-1.23917465391729));
#60306=CARTESIAN_POINT('Ctrl Pts',(-2.92385864229918,-36.2742356128,-1.20036514515414));
#60307=CARTESIAN_POINT('Ctrl Pts',(-2.95967700329097,-36.2742356128,-1.16844954495513));
#60308=CARTESIAN_POINT('Ctrl Pts',(-2.99489972169506,-36.2742356128,-1.13588523359943));
#60309=CARTESIAN_POINT('Ctrl Pts',(-3.02951901097885,-36.2742356128,-1.10271102209015));
#60310=CARTESIAN_POINT('Ctrl Pts',(-3.08321457923609,-36.2742356128,-1.05125681331438));
#60311=CARTESIAN_POINT('Ctrl Pts',(-3.13545017609485,-36.2742356128,-0.998339298681614));
#60312=CARTESIAN_POINT('Ctrl Pts',(-3.1861888002707,-36.2742356128,-0.944168555886378));
#60313=CARTESIAN_POINT('Ctrl Pts',(-3.21255606226399,-36.2742356128,-0.916017730142606));
#60314=CARTESIAN_POINT('Ctrl Pts',(-3.23851969999428,-36.2742356128,-0.887529050260996));
#60315=CARTESIAN_POINT('Ctrl Pts',(-3.26407891862252,-36.2742356128,-0.858735372798419));
#60316=CARTESIAN_POINT('Ctrl Pts',(-3.30671952622392,-36.2742356128,-0.810698696875676));
#60317=CARTESIAN_POINT('Ctrl Pts',(-3.3482422594108,-36.2742356127889,-0.761808566534635));
#60318=CARTESIAN_POINT('Ctrl Pts',(-3.38869992815495,-36.2742356128111,
-0.712264459872021));
#60319=CARTESIAN_POINT('Ctrl Pts',(-3.39362145153746,-36.2742356128137,
-0.706237605459142));
#60320=CARTESIAN_POINT('Ctrl Pts',(-3.39852723137462,-36.2742356128172,
-0.700201012931191));
#60321=CARTESIAN_POINT('Ctrl Pts',(-3.40341737611036,-36.274235612822,-0.694154991753613));
#60322=CARTESIAN_POINT('Ctrl Pts',(-3.44454477977108,-36.2742356128622,
-0.643306363144609));
#60323=CARTESIAN_POINT('Ctrl Pts',(-3.48454420070821,-36.2742356122796,
-0.591773595290768));
#60324=CARTESIAN_POINT('Ctrl Pts',(-3.52350036363258,-36.2742356262016,
-0.539735571971687));
#60325=CARTESIAN_POINT('Ctrl Pts',(-3.52725363315677,-36.2742356275429,
-0.534721917844568));
#60326=CARTESIAN_POINT('Ctrl Pts',(-3.5309972277434,-36.2742356290141,-0.529703535081257));
#60327=CARTESIAN_POINT('Ctrl Pts',(-3.53473122853353,-36.2742356306207,
-0.524680559427204));
#60328=CARTESIAN_POINT('Ctrl Pts',(-3.57694501547953,-36.2742356487836,
-0.467894598198846));
#60329=CARTESIAN_POINT('Ctrl Pts',(-3.61794060915933,-36.2742356874614,
-0.410522390412449));
#60330=CARTESIAN_POINT('Ctrl Pts',(-3.65782801944055,-36.2742357136805,
-0.352746823971276));
#60331=CARTESIAN_POINT('Ctrl Pts',(-3.69771542972177,-36.2742357398996,
-0.294971257530103));
#60332=CARTESIAN_POINT('Ctrl Pts',(-3.73649023726764,-36.2742357474187,
-0.236799307450452));
#60333=CARTESIAN_POINT('Ctrl Pts',(-3.77426745301402,-36.274235735014,-0.178287757725677));
#60334=CARTESIAN_POINT('Ctrl Pts',(-3.81489213576152,-36.2742357216743,
-0.115365885436529));
#60335=CARTESIAN_POINT('Ctrl Pts',(-3.85436208782408,-36.2742356989606,
-0.0520319711964369));
#60336=CARTESIAN_POINT('Ctrl Pts',(-3.89277713141461,-36.2742356785138,
0.0116646972747143));
#60337=CARTESIAN_POINT('Ctrl Pts',(-3.93133559414501,-36.2742356579906,
0.0755991715779432));
#60338=CARTESIAN_POINT('Ctrl Pts',(-3.96883222655404,-36.2742356401906,
0.139900037745291));
#60339=CARTESIAN_POINT('Ctrl Pts',(-4.00533748203647,-36.2742356294551,
0.204560244972189));
#60340=CARTESIAN_POINT('Ctrl Pts',(-4.04068199553069,-36.2742356190609,
0.2671644792576));
#60341=CARTESIAN_POINT('Ctrl Pts',(-4.07509781584091,-36.274235614972,0.330106576768051));
#60342=CARTESIAN_POINT('Ctrl Pts',(-4.10860887549533,-36.2742356136137,
0.393405625592747));
#60343=CARTESIAN_POINT('Ctrl Pts',(-4.1336476948815,-36.2742356125987,0.440701457690656));
#60344=CARTESIAN_POINT('Ctrl Pts',(-4.15818066405112,-36.2742356128,0.488197154084093));
#60345=CARTESIAN_POINT('Ctrl Pts',(-4.18219924647829,-36.2742356128,0.535905566233154));
#60346=CARTESIAN_POINT('Ctrl Pts',(-4.21266801474939,-36.2742356128,0.596426063592234));
#60347=CARTESIAN_POINT('Ctrl Pts',(-4.24232577357362,-36.2742356128,0.657296560446234));
#60348=CARTESIAN_POINT('Ctrl Pts',(-4.27120625360895,-36.2742356128,0.718566923232716));
#60349=CARTESIAN_POINT('Ctrl Pts',(-4.30008673365087,-36.2742356128,0.779837286033185));
#60350=CARTESIAN_POINT('Ctrl Pts',(-4.32819338159656,-36.2742356128,0.841515222100351));
#60351=CARTESIAN_POINT('Ctrl Pts',(-4.35553865680325,-36.2742356128,0.903617154925355));
#60352=CARTESIAN_POINT('Ctrl Pts',(-4.38898012358046,-36.2742356128,0.979563720014614));
#60353=CARTESIAN_POINT('Ctrl Pts',(-4.42129069411876,-36.2742356128,1.05616247724551));
#60354=CARTESIAN_POINT('Ctrl Pts',(-4.45246773012636,-36.2742356128001,
1.13340427103704));
#60355=CARTESIAN_POINT('Ctrl Pts',(-4.48679159733215,-36.2742356128001,
1.21844240847226));
#60356=CARTESIAN_POINT('Ctrl Pts',(-4.51974041626447,-36.2742356128003,
1.30425926912065));
#60357=CARTESIAN_POINT('Ctrl Pts',(-4.5512834584953,-36.2742356128004,1.39077904393112));
#60358=CARTESIAN_POINT('Ctrl Pts',(-4.58913299486063,-36.2742356128005,
1.49459697433378));
#60359=CARTESIAN_POINT('Ctrl Pts',(-4.62495504282474,-36.2742356128003,
1.59942531003409));
#60360=CARTESIAN_POINT('Ctrl Pts',(-4.6586950898368,-36.2742356128001,1.70506228796727));
#60361=CARTESIAN_POINT('Ctrl Pts',(-4.664047403989,-36.2742356128,1.72181989034363));
#60362=CARTESIAN_POINT('Ctrl Pts',(-4.66934739557618,-36.2742356128,1.73859776216507));
#60363=CARTESIAN_POINT('Ctrl Pts',(-4.67459495121429,-36.2742356128,1.7553950339094));
#60364=CARTESIAN_POINT('Ctrl Pts',(-4.67570152189309,-36.2742356128,1.75893713420865));
#60365=CARTESIAN_POINT('Ctrl Pts',(-4.67680559494956,-36.2742356128,1.76247955985014));
#60366=CARTESIAN_POINT('Ctrl Pts',(-4.67790780735,-36.2742356128,1.7660244085));
#60367=CARTESIAN_POINT('',(0.665819005986112,-36.2742356128,-2.24488955701597));
#60368=CARTESIAN_POINT('Origin',(0.000212348057480882,-36.2742356128,0.227537950203741));
#60369=CARTESIAN_POINT('',(4.67794129913,-36.2742356128,1.76613211329));
#60370=CARTESIAN_POINT('Ctrl Pts',(4.67793839402,-36.2742356128,1.76612278889));
#60371=CARTESIAN_POINT('Ctrl Pts',(4.6548471491261,-36.2742356128,1.69186544974786));
#60372=CARTESIAN_POINT('Ctrl Pts',(4.6307323914171,-36.2742356128003,1.61797566847106));
#60373=CARTESIAN_POINT('Ctrl Pts',(4.6056194961289,-36.2742356128003,1.54456189260851));
#60374=CARTESIAN_POINT('Ctrl Pts',(4.57962597242507,-36.2742356128003,1.46857373189777));
#60375=CARTESIAN_POINT('Ctrl Pts',(4.55256322090791,-36.2742356128002,1.39309516362647));
#60376=CARTESIAN_POINT('Ctrl Pts',(4.52444922260764,-36.2742356128002,1.31818980649636));
#60377=CARTESIAN_POINT('Ctrl Pts',(4.49451631237348,-36.2742356128001,1.23843824262817));
#60378=CARTESIAN_POINT('Ctrl Pts',(4.46339198392542,-36.2742356128,1.15933612320618));
#60379=CARTESIAN_POINT('Ctrl Pts',(4.43108342262081,-36.2742356128,1.0809023888135));
#60380=CARTESIAN_POINT('Ctrl Pts',(4.41927317708614,-36.2742356128,1.05223129904735));
#60381=CARTESIAN_POINT('Ctrl Pts',(4.40730453730176,-36.2742356128,1.02364901856025));
#60382=CARTESIAN_POINT('Ctrl Pts',(4.39517730788851,-36.2742356128,0.995154883908435));
#60383=CARTESIAN_POINT('Ctrl Pts',(4.35794106844874,-36.2742356128,0.907664626705557));
#60384=CARTESIAN_POINT('Ctrl Pts',(4.31921781659372,-36.2742356128,0.821022734370667));
#60385=CARTESIAN_POINT('Ctrl Pts',(4.27898363757762,-36.2742356128,0.735169479465547));
#60386=CARTESIAN_POINT('Ctrl Pts',(4.2608748946734,-36.2742356128,0.696528340051589));
#60387=CARTESIAN_POINT('Ctrl Pts',(4.24246006787135,-36.2742356128,0.658047080571516));
#60388=CARTESIAN_POINT('Ctrl Pts',(4.22373377331199,-36.2742356128,0.619715222891086));
#60389=CARTESIAN_POINT('Ctrl Pts',(4.17632752669855,-36.2742356128,0.522676831628486));
#60390=CARTESIAN_POINT('Ctrl Pts',(4.12690751722882,-36.2742356128,0.426554009358753));
#60391=CARTESIAN_POINT('Ctrl Pts',(4.07538515541344,-36.2742356128,0.331241273540381));
#60392=CARTESIAN_POINT('Ctrl Pts',(4.06339888726419,-36.2742356128,0.309067522778492));
#60393=CARTESIAN_POINT('Ctrl Pts',(4.05129861740903,-36.2742356128,0.286937563794092));
#60394=CARTESIAN_POINT('Ctrl Pts',(4.03908282686399,-36.2742356128,0.264850055636609));
#60395=CARTESIAN_POINT('Ctrl Pts',(4.00554454927516,-36.2742356128,0.204209119047194));
#60396=CARTESIAN_POINT('Ctrl Pts',(3.97113537519678,-36.2742356126953,0.143887166400186));
#60397=CARTESIAN_POINT('Ctrl Pts',(3.93582787419494,-36.2742356130921,0.0838826972028474));
#60398=CARTESIAN_POINT('Ctrl Pts',(3.90185603841753,-36.2742356134739,0.0261481672689329));
#60399=CARTESIAN_POINT('Ctrl Pts',(3.86705131020918,-36.2742356143011,-0.0312931655954265));
#60400=CARTESIAN_POINT('Ctrl Pts',(3.83134932336719,-36.2742356174484,-0.0884208183885626));
#60401=CARTESIAN_POINT('Ctrl Pts',(3.79481499520452,-36.2742356206691,-0.146880321596174));
#60402=CARTESIAN_POINT('Ctrl Pts',(3.75734127373668,-36.2742356252224,-0.20502580031905));
#60403=CARTESIAN_POINT('Ctrl Pts',(3.71883255615869,-36.274235626969,-0.262808961349773));
#60404=CARTESIAN_POINT('Ctrl Pts',(3.68059893653406,-36.2742356287032,-0.320179331969947));
#60405=CARTESIAN_POINT('Ctrl Pts',(3.64134406340379,-36.2742356268112,-0.377193377062157));
#60406=CARTESIAN_POINT('Ctrl Pts',(3.60096083749056,-36.2742356218413,-0.433754819684179));
#60407=CARTESIAN_POINT('Ctrl Pts',(3.563485510393,-36.2742356172293,-0.486243409078299));
#60408=CARTESIAN_POINT('Ctrl Pts',(3.52503334401459,-36.2742356149048,-0.538321086354601));
#60409=CARTESIAN_POINT('Ctrl Pts',(3.48552085288005,-36.2742356138311,-0.589851613583241));
#60410=CARTESIAN_POINT('Ctrl Pts',(3.44795857840759,-36.2742356128104,-0.638838750356814));
#60411=CARTESIAN_POINT('Ctrl Pts',(3.40943757352298,-36.2742356128121,-0.687331515184078));
#60412=CARTESIAN_POINT('Ctrl Pts',(3.36989713281383,-36.2742356128019,-0.735166458595873));
#60413=CARTESIAN_POINT('Ctrl Pts',(3.36032902804291,-36.2742356127994,-0.746741689980915));
#60414=CARTESIAN_POINT('Ctrl Pts',(3.35070130074832,-36.2742356128,-0.75827817578659));
#60415=CARTESIAN_POINT('Ctrl Pts',(3.34101324167528,-36.2742356128,-0.769773154095528));
#60416=CARTESIAN_POINT('Ctrl Pts',(3.29526352088457,-36.2742356128,-0.824055652185619));
#60417=CARTESIAN_POINT('Ctrl Pts',(3.24815560232718,-36.2742356128,-0.877433457315812));
#60418=CARTESIAN_POINT('Ctrl Pts',(3.19967614454946,-36.2742356128,-0.929673275944785));
#60419=CARTESIAN_POINT('Ctrl Pts',(3.15240628788772,-36.2742356128,-0.980609669457032));
#60420=CARTESIAN_POINT('Ctrl Pts',(3.10383269162824,-36.2742356128,-1.03046421061228));
#60421=CARTESIAN_POINT('Ctrl Pts',(3.05397476891398,-36.2742356128,-1.07905634490027));
#60422=CARTESIAN_POINT('Ctrl Pts',(3.00183115446817,-36.2742356128,-1.12987614198513));
#60423=CARTESIAN_POINT('Ctrl Pts',(2.94827976440738,-36.2742356128,-1.17931792987394));
#60424=CARTESIAN_POINT('Ctrl Pts',(2.89336456309009,-36.2742356128,-1.22722756870653));
#60425=CARTESIAN_POINT('Ctrl Pts',(2.83863179705281,-36.2742356128,-1.27497804562829));
#60426=CARTESIAN_POINT('Ctrl Pts',(2.78254459846684,-36.2742356128,-1.32120629344724));
#60427=CARTESIAN_POINT('Ctrl Pts',(2.72517907321423,-36.2742356128,-1.36580058859031));
#60428=CARTESIAN_POINT('Ctrl Pts',(2.66752673177032,-36.2742356128,-1.4106178463199));
#60429=CARTESIAN_POINT('Ctrl Pts',(2.60858331698472,-36.2742356128,-1.45378468187809));
#60430=CARTESIAN_POINT('Ctrl Pts',(2.54845707550452,-36.2742356128,-1.49523068468984));
#60431=CARTESIAN_POINT('Ctrl Pts',(2.48833083402433,-36.2742356128,-1.5366766875016));
#60432=CARTESIAN_POINT('Ctrl Pts',(2.42702185855343,-36.2742356128,-1.57640180073771));
#60433=CARTESIAN_POINT('Ctrl Pts',(2.36466806519104,-36.2742356128,-1.61437955209257));
#60434=CARTESIAN_POINT('Ctrl Pts',(2.30285964294221,-36.2742356128,-1.65202513490675));
#60435=CARTESIAN_POINT('Ctrl Pts',(2.24001695357672,-36.2742356128,-1.68795837080037));
#60436=CARTESIAN_POINT('Ctrl Pts',(2.17630747177397,-36.2742356128,-1.72219266457153));
#60437=CARTESIAN_POINT('Ctrl Pts',(2.11259798997122,-36.2742356128,-1.75642695834268));
#60438=CARTESIAN_POINT('Ctrl Pts',(2.04802182342419,-36.2742356128,-1.78896225437204));
#60439=CARTESIAN_POINT('Ctrl Pts',(1.98277319980503,-36.2742356128,-1.81985743232702));
#60440=CARTESIAN_POINT('Ctrl Pts',(1.91752074047581,-36.2742356128,-1.85075442648805));
#60441=CARTESIAN_POINT('Ctrl Pts',(1.85157764819585,-36.2742356126615,-1.88002487306571));
#60442=CARTESIAN_POINT('Ctrl Pts',(1.78516561446401,-36.2742356129385,-1.90775210033866));
#60443=CARTESIAN_POINT('Ctrl Pts',(1.71875358073217,-36.2742356132154,-1.93547932761161));
#60444=CARTESIAN_POINT('Ctrl Pts',(1.6518693341746,-36.2742356144321,-1.96167041142089));
#60445=CARTESIAN_POINT('Ctrl Pts',(1.58464405915673,-36.2742356155218,-1.98645717948924));
#60446=CARTESIAN_POINT('Ctrl Pts',(1.50771176789187,-36.274235616769,-2.01482304128813));
#60447=CARTESIAN_POINT('Ctrl Pts',(1.43032073812522,-36.2742356171986,-2.04135449475494));
#60448=CARTESIAN_POINT('Ctrl Pts',(1.35262135824679,-36.2742356167949,-2.06621671682666));
#60449=CARTESIAN_POINT('Ctrl Pts',(1.27282710612553,-36.2742356163803,-2.09174925543107));
#60450=CARTESIAN_POINT('Ctrl Pts',(1.19270675788403,-36.2742356152832,-2.11552252631164));
#60451=CARTESIAN_POINT('Ctrl Pts',(1.11236951057882,-36.2742356144497,-2.13769695919322));
#60452=CARTESIAN_POINT('Ctrl Pts',(1.03319649335471,-36.2742356136283,-2.15955004497047));
#60453=CARTESIAN_POINT('Ctrl Pts',(0.953811601705358,-36.2742356131035,
-2.17985130581748));
#60454=CARTESIAN_POINT('Ctrl Pts',(0.874284313879753,-36.2742356129234,
-2.19872032066919));
#60455=CARTESIAN_POINT('Ctrl Pts',(0.809363582982145,-36.2742356127764,
-2.2141237157677));
#60456=CARTESIAN_POINT('Ctrl Pts',(0.74434705187334,-36.2742356128,-2.22857228708359));
#60457=CARTESIAN_POINT('Ctrl Pts',(0.679263141868309,-36.2742356128,-2.24210692825591));
#60458=CARTESIAN_POINT('Ctrl Pts',(0.674782103646385,-36.2742356128,-2.24303879059191));
#60459=CARTESIAN_POINT('Ctrl Pts',(0.670301885654333,-36.2742356128,-2.24396609231333));
#60460=CARTESIAN_POINT('Ctrl Pts',(0.665819006916,-36.2742356128,-2.24488956153));
#60461=CARTESIAN_POINT('',(5.53988691730504,-36.2742356128,5.60697933185575));
#60462=CARTESIAN_POINT('Ctrl Pts',(5.53988692237398,-36.2742356128,5.60697918091797));
#60463=CARTESIAN_POINT('Ctrl Pts',(5.54165830493023,-36.2742356128,5.55423263886826));
#60464=CARTESIAN_POINT('Ctrl Pts',(5.5429724375768,-36.2742356128,5.50093679546234));
#60465=CARTESIAN_POINT('Ctrl Pts',(5.54364945845749,-36.2742356128,5.44724531226854));
#60466=CARTESIAN_POINT('Ctrl Pts',(5.54433722472412,-36.2742356128,5.39270166081026));
#60467=CARTESIAN_POINT('Ctrl Pts',(5.54436767013136,-36.2742356128,5.337749782334));
#60468=CARTESIAN_POINT('Ctrl Pts',(5.54360552907939,-36.2742356128,5.282539087133));
#60469=CARTESIAN_POINT('Ctrl Pts',(5.54282290024159,-36.2742356128,5.22584422453863));
#60470=CARTESIAN_POINT('Ctrl Pts',(5.54120462781002,-36.2742356128,5.16887654624831));
#60471=CARTESIAN_POINT('Ctrl Pts',(5.53865781012939,-36.2742356128,5.11178424092544));
#60472=CARTESIAN_POINT('Ctrl Pts',(5.53745660746727,-36.2742356128,5.08485674247821));
#60473=CARTESIAN_POINT('Ctrl Pts',(5.53604959570276,-36.2742356128,5.05790131769372));
#60474=CARTESIAN_POINT('Ctrl Pts',(5.53443085180288,-36.2742356128,5.03093240776099));
#60475=CARTESIAN_POINT('Ctrl Pts',(5.5308382665806,-36.2742356128,4.97107852519674));
#60476=CARTESIAN_POINT('Ctrl Pts',(5.52619836949679,-36.2742356128,4.9111422095337));
#60477=CARTESIAN_POINT('Ctrl Pts',(5.52048353574769,-36.2742356128,4.85126756067043));
#60478=CARTESIAN_POINT('Ctrl Pts',(5.51460523213774,-36.2742356128,4.78968022847327));
#60479=CARTESIAN_POINT('Ctrl Pts',(5.50758989745033,-36.2742356128,4.72815829258806));
#60480=CARTESIAN_POINT('Ctrl Pts',(5.49946006720242,-36.2742356128,4.66683869085727));
#60481=CARTESIAN_POINT('Ctrl Pts',(5.49106651547459,-36.2742356128,4.60352995828077));
#60482=CARTESIAN_POINT('Ctrl Pts',(5.48148534744977,-36.2742356128,4.5404370884034));
#60483=CARTESIAN_POINT('Ctrl Pts',(5.47079175011765,-36.2742356128,4.47768722295259));
#60484=CARTESIAN_POINT('Ctrl Pts',(5.46138568923118,-36.2742356128,4.42249260165565));
#60485=CARTESIAN_POINT('Ctrl Pts',(5.45111955899517,-36.2742356128,4.36755995871729));
#60486=CARTESIAN_POINT('Ctrl Pts',(5.44006866845322,-36.2742356128,4.31295000014857));
#60487=CARTESIAN_POINT('Ctrl Pts',(5.42645679487174,-36.2742356128,4.245684484351));
#60488=CARTESIAN_POINT('Ctrl Pts',(5.41165453195185,-36.2742356128,4.17891441274785));
#60489=CARTESIAN_POINT('Ctrl Pts',(5.39584673414317,-36.2742356128,4.11274168517014));
#60490=CARTESIAN_POINT('Ctrl Pts',(5.37930929780952,-36.2742356128,4.04351463137146));
#60491=CARTESIAN_POINT('Ctrl Pts',(5.36167225848251,-36.2742356128,3.97494176650156));
#60492=CARTESIAN_POINT('Ctrl Pts',(5.34318328727252,-36.2742356128,3.907096637803));
#60493=CARTESIAN_POINT('Ctrl Pts',(5.34002882901784,-36.2742356128,3.89552137902669));
#60494=CARTESIAN_POINT('Ctrl Pts',(5.33684963359364,-36.2742356128,3.8839671975358));
#60495=CARTESIAN_POINT('Ctrl Pts',(5.33364699796188,-36.2742356128,3.87243432667238));
#60496=CARTESIAN_POINT('Ctrl Pts',(5.31440651792086,-36.2742356128,3.80314827693791));
#60497=CARTESIAN_POINT('Ctrl Pts',(5.29431680957279,-36.2742356128,3.73462645497715));
#60498=CARTESIAN_POINT('Ctrl Pts',(5.27366540454653,-36.2742356128,3.66689041569989));
#60499=CARTESIAN_POINT('Ctrl Pts',(5.26699976162205,-36.2742356128,3.64502729063082));
#60500=CARTESIAN_POINT('Ctrl Pts',(5.2602756459931,-36.2742356128,3.62324562548497));
#60501=CARTESIAN_POINT('Ctrl Pts',(5.25350273274586,-36.2742356128,3.60154498249611));
#60502=CARTESIAN_POINT('Ctrl Pts',(5.23084294007848,-36.2742356128,3.52894224082113));
#60503=CARTESIAN_POINT('Ctrl Pts',(5.20764098851541,-36.2742356128,3.45725487651199));
#60504=CARTESIAN_POINT('Ctrl Pts',(5.18422503958467,-36.2742356128,3.38623266017563));
#60505=CARTESIAN_POINT('Ctrl Pts',(5.17895808821716,-36.2742356128,3.37025762706625));
#60506=CARTESIAN_POINT('Ctrl Pts',(5.17368029169311,-36.2742356128,3.35431645791937));
#60507=CARTESIAN_POINT('Ctrl Pts',(5.16839529949842,-36.2742356128,3.33840663348512));
#60508=CARTESIAN_POINT('Ctrl Pts',(5.14673287022256,-36.2742356128,3.27319453214193));
#60509=CARTESIAN_POINT('Ctrl Pts',(5.12495264363142,-36.2742356125143,3.20855115611014));
#60510=CARTESIAN_POINT('Ctrl Pts',(5.10330747750946,-36.2742356145159,3.1443462134388));
#60511=CARTESIAN_POINT('Ctrl Pts',(5.08348665088416,-36.2742356163488,3.08555271515814));
#60512=CARTESIAN_POINT('Ctrl Pts',(5.06377991216152,-36.2742356205018,3.02712777923992));
#60513=CARTESIAN_POINT('Ctrl Pts',(5.04434337184934,-36.2742356265321,2.96897470189817));
#60514=CARTESIAN_POINT('Ctrl Pts',(5.02611549217322,-36.2742356321874,2.91443787180618));
#60515=CARTESIAN_POINT('Ctrl Pts',(5.0081257568683,-36.2742356393532,2.86014068095253));
#60516=CARTESIAN_POINT('Ctrl Pts',(4.99045886252433,-36.2742356442228,2.80599669724385));
#60517=CARTESIAN_POINT('Ctrl Pts',(4.97397667379101,-36.2742356487659,2.75548349775978));
#60518=CARTESIAN_POINT('Ctrl Pts',(4.95777566188676,-36.2742356509722,2.70510395407236));
#60519=CARTESIAN_POINT('Ctrl Pts',(4.94188051554086,-36.274235648232,2.65477619342767));
#60520=CARTESIAN_POINT('Ctrl Pts',(4.93489101734184,-36.274235647027,2.63264580313543));
#60521=CARTESIAN_POINT('Ctrl Pts',(4.92796004742607,-36.2742356449018,2.610525240921));
#60522=CARTESIAN_POINT('Ctrl Pts',(4.92108659841074,-36.2742356419742,2.58840653662621));
#60523=CARTESIAN_POINT('Ctrl Pts',(4.90838833654212,-36.2742356365656,2.54754363087059));
#60524=CARTESIAN_POINT('Ctrl Pts',(4.89587110254343,-36.2742356286996,2.50663414959663));
#60525=CARTESIAN_POINT('Ctrl Pts',(4.88349086308502,-36.2742356228979,2.46557954036258));
#60526=CARTESIAN_POINT('Ctrl Pts',(4.87111062362242,-36.2742356170962,2.42452493111463));
#60527=CARTESIAN_POINT('Ctrl Pts',(4.85888611536352,-36.2742356144804,2.38339106874945));
#60528=CARTESIAN_POINT('Ctrl Pts',(4.84678270416545,-36.2742356139505,2.34224859775519));
#60529=CARTESIAN_POINT('Ctrl Pts',(4.83364239888552,-36.2742356133753,2.29758146879557));
#60530=CARTESIAN_POINT('Ctrl Pts',(4.82064635349563,-36.2742356131413,2.25284307171249));
#60531=CARTESIAN_POINT('Ctrl Pts',(4.80767077257532,-36.2742356130048,2.20789713737373));
#60532=CARTESIAN_POINT('Ctrl Pts',(4.79507702413614,-36.2742356128723,2.16427382725746));
#60533=CARTESIAN_POINT('Ctrl Pts',(4.78250272372987,-36.2742356128384,2.1204551903821));
#60534=CARTESIAN_POINT('Ctrl Pts',(4.76979178214926,-36.2742356128196,2.07629693005267));
#60535=CARTESIAN_POINT('Ctrl Pts',(4.75743128237245,-36.2742356128014,2.03335611693627));
#60536=CARTESIAN_POINT('Ctrl Pts',(4.74494177342037,-36.2742356128013,1.99009431956366));
#60537=CARTESIAN_POINT('Ctrl Pts',(4.73213582539401,-36.2742356128005,1.94635742420483));
#60538=CARTESIAN_POINT('Ctrl Pts',(4.71981950552344,-36.2742356127997,1.90429278422065));
#60539=CARTESIAN_POINT('Ctrl Pts',(4.70721060716778,-36.2742356128,1.86178879696953));
#60540=CARTESIAN_POINT('Ctrl Pts',(4.69409898682122,-36.2742356128,1.81868627934494));
#60541=CARTESIAN_POINT('Ctrl Pts',(4.69152954119736,-36.2742356128,1.81023960590866));
#60542=CARTESIAN_POINT('Ctrl Pts',(4.68894064748119,-36.2742356128,1.80176987349512));
#60543=CARTESIAN_POINT('Ctrl Pts',(4.68633051117043,-36.2742356128,1.79327577326918));
#60544=CARTESIAN_POINT('Ctrl Pts',(4.68355698486512,-36.2742356128,1.78424995713865));
#60545=CARTESIAN_POINT('Ctrl Pts',(4.68076549196667,-36.2742356128,1.77521613159));
#60546=CARTESIAN_POINT('Ctrl Pts',(4.67794710935,-36.2742356128,1.76615076209));
#60547=CARTESIAN_POINT('Ctrl Pts',(2.32481332798E-5,-36.2742356128,10.9643459795));
#60548=CARTESIAN_POINT('Ctrl Pts',(0.012267597991931,-36.2742356128,10.9643448993192));
#60549=CARTESIAN_POINT('Ctrl Pts',(0.0244497673928545,-36.2742356128,10.9643037788664));
#60550=CARTESIAN_POINT('Ctrl Pts',(0.0366626829731096,-36.2742356128,10.9642222827207));
#60551=CARTESIAN_POINT('Ctrl Pts',(0.190945660670054,-36.2742356128,10.9631927604951));
#60552=CARTESIAN_POINT('Ctrl Pts',(0.345196887448164,-36.2742356128,10.955732938611));
#60553=CARTESIAN_POINT('Ctrl Pts',(0.498871345331836,-36.2742356128,10.9418556346228));
#60554=CARTESIAN_POINT('Ctrl Pts',(0.654951435072277,-36.2742356128,10.927761094244));
#60555=CARTESIAN_POINT('Ctrl Pts',(0.810436383027939,-36.2742356128,10.9070466255314));
#60556=CARTESIAN_POINT('Ctrl Pts',(0.964764670252676,-36.2742356128,10.8797788422672));
#60557=CARTESIAN_POINT('Ctrl Pts',(1.11914274361821,-36.2742356128,10.8525022624451));
#60558=CARTESIAN_POINT('Ctrl Pts',(1.27236128250835,-36.2742356128,10.8186685334414));
#60559=CARTESIAN_POINT('Ctrl Pts',(1.42386599695573,-36.2742356128,10.7783972802877));
#60560=CARTESIAN_POINT('Ctrl Pts',(1.57654467229091,-36.2742356128,10.7378139782563));
#60561=CARTESIAN_POINT('Ctrl Pts',(1.72748264701554,-36.2742356128,10.6906931305989));
#60562=CARTESIAN_POINT('Ctrl Pts',(1.87612834575455,-36.2742356128,10.6372081072336));
#60563=CARTESIAN_POINT('Ctrl Pts',(2.02581869224373,-36.2742356128,10.5833472034372));
#60564=CARTESIAN_POINT('Ctrl Pts',(2.17318420757732,-36.2742356128,10.5230325024168));
#60565=CARTESIAN_POINT('Ctrl Pts',(2.31768076387948,-36.2742356128,10.4564904323508));
#60566=CARTESIAN_POINT('Ctrl Pts',(2.46348798666278,-36.2742356128,10.389344787618));
#60567=CARTESIAN_POINT('Ctrl Pts',(2.60637372464546,-36.2742356128,10.3158584289551));
#60568=CARTESIAN_POINT('Ctrl Pts',(2.74580189015219,-36.2742356128,10.2363119782628));
#60569=CARTESIAN_POINT('Ctrl Pts',(2.88575737001097,-36.2742356128,10.1564646845884));
#60570=CARTESIAN_POINT('Ctrl Pts',(3.02222884358078,-36.2742356128,10.0705115620573));
#60571=CARTESIAN_POINT('Ctrl Pts',(3.1547007261638,-36.2742356128,9.97878201671825));
#60572=CARTESIAN_POINT('Ctrl Pts',(3.28770166123135,-36.2742356128,9.8866861314215));
#60573=CARTESIAN_POINT('Ctrl Pts',(3.41667075619548,-36.2742356128,9.78876778525046));
#60574=CARTESIAN_POINT('Ctrl Pts',(3.54111654199492,-36.2742356128,9.68540334602765));
#60575=CARTESIAN_POINT('Ctrl Pts',(3.64858270370976,-36.2742356128,9.59614215112479));
#60576=CARTESIAN_POINT('Ctrl Pts',(3.75267608382533,-36.2742356128,9.50282039201421));
#60577=CARTESIAN_POINT('Ctrl Pts',(3.85310031130201,-36.2742356128,9.40570437827657));
#60578=CARTESIAN_POINT('Ctrl Pts',(3.96951110904278,-36.2742356128,9.29312843005505));
#60579=CARTESIAN_POINT('Ctrl Pts',(4.080990284725,-36.2742356128,9.17545378429104));
#60580=CARTESIAN_POINT('Ctrl Pts',(4.18710961345993,-36.2742356128,9.05313210221856));
#60581=CARTESIAN_POINT('Ctrl Pts',(4.29281661966718,-36.2742356128,8.93128569628798));
#60582=CARTESIAN_POINT('Ctrl Pts',(4.39320516825513,-36.2742356128,8.80482851427014));
#60583=CARTESIAN_POINT('Ctrl Pts',(4.48789158020286,-36.2742356128,8.67424009053965));
#60584=CARTESIAN_POINT('Ctrl Pts',(4.58220205051933,-36.2742356128,8.54417015329556));
#60585=CARTESIAN_POINT('Ctrl Pts',(4.67085539903292,-36.2742356128,8.41000192729587));
#60586=CARTESIAN_POINT('Ctrl Pts',(4.75351448617961,-36.2742356128,8.27223895635978));
#60587=CARTESIAN_POINT('Ctrl Pts',(4.8357582380376,-36.2742356128,8.13516819997965));
#60588=CARTESIAN_POINT('Ctrl Pts',(4.91206765482947,-36.2742356128,7.99453894339549));
#60589=CARTESIAN_POINT('Ctrl Pts',(4.98215479283938,-36.2742356128,7.85087347247978));
#60590=CARTESIAN_POINT('Ctrl Pts',(5.05182619136561,-36.2742356128,7.70806018943188));
#60591=CARTESIAN_POINT('Ctrl Pts',(5.11534876334311,-36.2742356128,7.56224681130156));
#60592=CARTESIAN_POINT('Ctrl Pts',(5.1724856667926,-36.2742356128,7.41396932577449));
#60593=CARTESIAN_POINT('Ctrl Pts',(5.22901464574304,-36.2742356128,7.26726948115318));
#60594=CARTESIAN_POINT('Ctrl Pts',(5.27929301765054,-36.2742356128,7.11815789491069));
#60595=CARTESIAN_POINT('Ctrl Pts',(5.32313836217568,-36.2742356128,6.9671730420275));
#60596=CARTESIAN_POINT('Ctrl Pts',(5.36670086892032,-36.2742356128,6.8171621630323));
#60597=CARTESIAN_POINT('Ctrl Pts',(5.40391295200194,-36.2742356128,6.66530229338273));
#60598=CARTESIAN_POINT('Ctrl Pts',(5.43464400506635,-36.2742356128,6.51213790757587));
#60599=CARTESIAN_POINT('Ctrl Pts',(5.46503102108015,-36.2742356128,6.36068821157939));
#60600=CARTESIAN_POINT('Ctrl Pts',(5.48908122944364,-36.2742356128,6.20796322934857));
#60601=CARTESIAN_POINT('Ctrl Pts',(5.50671718129312,-36.2742356128,6.05450262692307));
#60602=CARTESIAN_POINT('Ctrl Pts',(5.52334991985196,-36.2742356128,5.90977156273051));
#60603=CARTESIAN_POINT('Ctrl Pts',(5.53427767276785,-36.2742356128,5.7643864062297));
#60604=CARTESIAN_POINT('Ctrl Pts',(5.53947703985376,-36.2742356128,5.61880872757919));
#60605=CARTESIAN_POINT('Ctrl Pts',(5.53961786526957,-36.2742356128,5.61486574052124));
#60606=CARTESIAN_POINT('Ctrl Pts',(5.53975449137418,-36.2742356128,5.61092259462969));
#60607=CARTESIAN_POINT('Ctrl Pts',(5.53988691225,-36.2742356128,5.60697948238));
#60608=CARTESIAN_POINT('Origin',(-3.35265884719E-30,-38.2742356128,3.15283103411E-22));
#60609=CARTESIAN_POINT('',(10.0697226343,-38.2742356128,2.85693747561));
#60610=CARTESIAN_POINT('',(10.7486858853,-38.2742356128,0.75419629452));
#60611=CARTESIAN_POINT('Ctrl Pts',(10.0697226344311,-38.2742356128,2.85693747569001));
#60612=CARTESIAN_POINT('Ctrl Pts',(10.0776188393002,-38.2742356128,2.84400003564299));
#60613=CARTESIAN_POINT('Ctrl Pts',(10.0855029430265,-38.2742356128062,2.8309683272098));
#60614=CARTESIAN_POINT('Ctrl Pts',(10.0933605009977,-38.2742356127531,2.81785320039552));
#60615=CARTESIAN_POINT('Ctrl Pts',(10.1109731368737,-38.2742356126341,2.78845577769836));
#60616=CARTESIAN_POINT('Ctrl Pts',(10.1284465935078,-38.2742356123565,2.75863590433942));
#60617=CARTESIAN_POINT('Ctrl Pts',(10.1456594638731,-38.2742356122038,2.72850124510115));
#60618=CARTESIAN_POINT('Ctrl Pts',(10.1640041649347,-38.2742356120411,2.69638508413648));
#60619=CARTESIAN_POINT('Ctrl Pts',(10.1820528841507,-38.2742356120154,2.66391120473192));
#60620=CARTESIAN_POINT('Ctrl Pts',(10.1997035416477,-38.2742356121317,2.63116652928536));
#60621=CARTESIAN_POINT('Ctrl Pts',(10.2172099443932,-38.274235612247,2.59868946851639));
#60622=CARTESIAN_POINT('Ctrl Pts',(10.2343253141801,-38.2742356124941,2.56594530790568));
#60623=CARTESIAN_POINT('Ctrl Pts',(10.250987782861,-38.2742356126595,2.53298508626117));
#60624=CARTESIAN_POINT('Ctrl Pts',(10.2704216371138,-38.2742356128525,2.49454275482485));
#60625=CARTESIAN_POINT('Ctrl Pts',(10.2892457459371,-38.2742356127993,2.45580776597392));
#60626=CARTESIAN_POINT('Ctrl Pts',(10.3074100253296,-38.2742356127999,2.41681942324682));
#60627=CARTESIAN_POINT('Ctrl Pts',(10.3156933625564,-38.2742356128001,2.39903982496235));
#60628=CARTESIAN_POINT('Ctrl Pts',(10.3238401489906,-38.2742356128,2.3812070736748));
#60629=CARTESIAN_POINT('Ctrl Pts',(10.3318485530151,-38.2742356128,2.3633231281257));
#60630=CARTESIAN_POINT('Ctrl Pts',(10.3539275416858,-38.2742356128,2.31401749494804));
#60631=CARTESIAN_POINT('Ctrl Pts',(10.3749527959892,-38.2742356128,2.26431782944173));
#60632=CARTESIAN_POINT('Ctrl Pts',(10.394940586342,-38.2742356128,2.21425144102859));
#60633=CARTESIAN_POINT('Ctrl Pts',(10.3981007591477,-38.2742356128,2.20633568664295));
#60634=CARTESIAN_POINT('Ctrl Pts',(10.4012351022165,-38.2742356128,2.19841078058856));
#60635=CARTESIAN_POINT('Ctrl Pts',(10.4043437787341,-38.2742356128,2.19047687263431));
#60636=CARTESIAN_POINT('Ctrl Pts',(10.4217205779389,-38.2742356128,2.1461281201514));
#60637=CARTESIAN_POINT('Ctrl Pts',(10.438297812734,-38.2742356128,2.10148777201649));
#60638=CARTESIAN_POINT('Ctrl Pts',(10.4541056780973,-38.2742356128,2.05660920251616));
#60639=CARTESIAN_POINT('Ctrl Pts',(10.4675450264758,-38.2742356128,2.01845485868911));
#60640=CARTESIAN_POINT('Ctrl Pts',(10.4804291335677,-38.2742356128,1.98012800337298));
#60641=CARTESIAN_POINT('Ctrl Pts',(10.4927701214951,-38.2742356128,1.94169718949288));
#60642=CARTESIAN_POINT('Ctrl Pts',(10.5039195447129,-38.2742356128,1.90697700249726));
#60643=CARTESIAN_POINT('Ctrl Pts',(10.514626001726,-38.2742356128,1.87217183244256));
#60644=CARTESIAN_POINT('Ctrl Pts',(10.5248856152871,-38.2742356128,1.83736677743975));
#60645=CARTESIAN_POINT('Ctrl Pts',(10.5346062277631,-38.2742356128,1.80439024768327));
#60646=CARTESIAN_POINT('Ctrl Pts',(10.5439352285554,-38.2742356127913,1.77139355586021));
#60647=CARTESIAN_POINT('Ctrl Pts',(10.5528945995153,-38.2742356127464,1.73842376238139));
#60648=CARTESIAN_POINT('Ctrl Pts',(10.560024647317,-38.2742356127106,1.71218573690282));
#60649=CARTESIAN_POINT('Ctrl Pts',(10.5669209610923,-38.2742356126719,1.6859628905476));
#60650=CARTESIAN_POINT('Ctrl Pts',(10.57359934485,-38.2742356127066,1.659756377355));
#60651=CARTESIAN_POINT('Ctrl Pts',(10.5886695541833,-38.2742356127848,1.60061966793));
#60652=CARTESIAN_POINT('Ctrl Pts',(10.6026459235773,-38.2742356128,1.54154272041369));
#60653=CARTESIAN_POINT('Ctrl Pts',(10.6157344632958,-38.2742356128,1.48260713307673));
#60654=CARTESIAN_POINT('Ctrl Pts',(10.6229873571614,-38.2742356128,1.44994851958333));
#60655=CARTESIAN_POINT('Ctrl Pts',(10.6299550378573,-38.2742356128,1.4173888281794));
#60656=CARTESIAN_POINT('Ctrl Pts',(10.6366903508906,-38.2742356128,1.38487935873198));
#60657=CARTESIAN_POINT('Ctrl Pts',(10.6428618776733,-38.2742356128,1.35509112759876));
#60658=CARTESIAN_POINT('Ctrl Pts',(10.648838346926,-38.2742356128,1.32534429110625));
#60659=CARTESIAN_POINT('Ctrl Pts',(10.6546508806194,-38.2742356128,1.2956426679367));
#60660=CARTESIAN_POINT('Ctrl Pts',(10.6599433244144,-38.2742356128,1.26859866620975));
#60661=CARTESIAN_POINT('Ctrl Pts',(10.6650998558584,-38.2742356128,1.24159183508873));
#60662=CARTESIAN_POINT('Ctrl Pts',(10.6701355237829,-38.2742356128,1.21466761412695));
#60663=CARTESIAN_POINT('Ctrl Pts',(10.6725084893088,-38.2742356128,1.20198007215385));
#60664=CARTESIAN_POINT('Ctrl Pts',(10.6748544884253,-38.2742356128,1.18931154490809));
#60665=CARTESIAN_POINT('Ctrl Pts',(10.6771743463304,-38.2742356128,1.17667085189563));
#60666=CARTESIAN_POINT('Ctrl Pts',(10.6794225509139,-38.2742356128,1.16442059126226));
#60667=CARTESIAN_POINT('Ctrl Pts',(10.681645032157,-38.2742356128,1.15220289282337));
#60668=CARTESIAN_POINT('Ctrl Pts',(10.68385417031,-38.2742356127999,1.1399539012589));
#60669=CARTESIAN_POINT('Ctrl Pts',(10.684249048922,-38.2742356127998,1.13776442081368));
#60670=CARTESIAN_POINT('Ctrl Pts',(10.6846434790834,-38.2742356127998,1.13557407331553));
#60671=CARTESIAN_POINT('Ctrl Pts',(10.6850375033588,-38.2742356127997,1.13338266268583));
#60672=CARTESIAN_POINT('Ctrl Pts',(10.6874088318044,-38.2742356127994,1.12019425098996));
#60673=CARTESIAN_POINT('Ctrl Pts',(10.6897723350178,-38.2742356127989,1.10692783802663));
#60674=CARTESIAN_POINT('Ctrl Pts',(10.6921362766321,-38.2742356127984,1.093545659875));
#60675=CARTESIAN_POINT('Ctrl Pts',(10.6948056682513,-38.2742356127979,1.078434341563));
#60676=CARTESIAN_POINT('Ctrl Pts',(10.6974756107928,-38.2742356127975,1.06317553188));
#60677=CARTESIAN_POINT('Ctrl Pts',(10.7001461013002,-38.2742356127972,1.04778309134131));
#60678=CARTESIAN_POINT('Ctrl Pts',(10.7032679269097,-38.274235612797,1.0297892003566));
#60679=CARTESIAN_POINT('Ctrl Pts',(10.7063903477994,-38.274235612797,1.0116137923099));
#60680=CARTESIAN_POINT('Ctrl Pts',(10.7094989857158,-38.2742356127972,0.993358985853085));
#60681=CARTESIAN_POINT('Ctrl Pts',(10.7131804317752,-38.2742356127974,0.97174048697887));
#60682=CARTESIAN_POINT('Ctrl Pts',(10.7168416621835,-38.2742356127979,0.950016346973492));
#60683=CARTESIAN_POINT('Ctrl Pts',(10.7204480893748,-38.2742356127984,0.928407232902512));
#60684=CARTESIAN_POINT('Ctrl Pts',(10.7231942485053,-38.2742356127987,0.911952702487821));
#60685=CARTESIAN_POINT('Ctrl Pts',(10.7259082038139,-38.2742356127991,0.89556715018462));
#60686=CARTESIAN_POINT('Ctrl Pts',(10.7285778286188,-38.2742356127993,0.879323202461527));
#60687=CARTESIAN_POINT('Ctrl Pts',(10.730988497373,-38.2742356127995,0.864654932542631));
#60688=CARTESIAN_POINT('Ctrl Pts',(10.7333628612606,-38.2742356127997,0.850103016441976));
#60689=CARTESIAN_POINT('Ctrl Pts',(10.7356981739405,-38.2742356127998,0.835680045130879));
#60690=CARTESIAN_POINT('Ctrl Pts',(10.7378330625263,-38.2742356127999,0.822494899908279));
#60691=CARTESIAN_POINT('Ctrl Pts',(10.7399352552987,-38.2742356128,0.809417839967112));
#60692=CARTESIAN_POINT('Ctrl Pts',(10.7420094653683,-38.2742356128,0.796414883560318));
#60693=CARTESIAN_POINT('Ctrl Pts',(10.7429375365281,-38.2742356128,0.790596924709413));
#60694=CARTESIAN_POINT('Ctrl Pts',(10.7438601064876,-38.2742356128,0.784793160677161));
#60695=CARTESIAN_POINT('Ctrl Pts',(10.7447781403271,-38.2742356128,0.778997116234539));
#60696=CARTESIAN_POINT('Ctrl Pts',(10.7460880302118,-38.2742356128,0.770727072518073));
#60697=CARTESIAN_POINT('Ctrl Pts',(10.7473907134667,-38.2742356128,0.762459686238333));
#60698=CARTESIAN_POINT('Ctrl Pts',(10.7486858853,-38.2742356128,0.75419629452));
#60699=CARTESIAN_POINT('',(6.79137814506709,-38.2742356128,3.87179982043696));
#60700=CARTESIAN_POINT('Ctrl Pts',(6.79137821743737,-38.2742356128,3.87179986876002));
#60701=CARTESIAN_POINT('Ctrl Pts',(6.80226365184488,-38.2742356128,3.87906825465593));
#60702=CARTESIAN_POINT('Ctrl Pts',(6.81320993266797,-38.2742356128,3.88625408753819));
#60703=CARTESIAN_POINT('Ctrl Pts',(6.82421601895544,-38.2742356128,3.89335477754412));
#60704=CARTESIAN_POINT('Ctrl Pts',(6.87563019015907,-38.2742356128,3.9265251600119));
#60705=CARTESIAN_POINT('Ctrl Pts',(6.92832455620214,-38.2742356128001,3.95781726483387));
#60706=CARTESIAN_POINT('Ctrl Pts',(6.98218879584778,-38.2742356127999,3.98701052943907));
#60707=CARTESIAN_POINT('Ctrl Pts',(7.03678152742978,-38.2742356127997,4.01659862107609));
#60708=CARTESIAN_POINT('Ctrl Pts',(7.09257560090438,-38.2742356128,4.04403030945431));
#60709=CARTESIAN_POINT('Ctrl Pts',(7.14940901416357,-38.2742356127945,4.06910193455759));
#60710=CARTESIAN_POINT('Ctrl Pts',(7.20715367516088,-38.2742356127889,4.09457554962341));
#60711=CARTESIAN_POINT('Ctrl Pts',(7.26597081847314,-38.2742356127788,4.11761237182838));
#60712=CARTESIAN_POINT('Ctrl Pts',(7.32564859213579,-38.2742356127345,4.13803193031878));
#60713=CARTESIAN_POINT('Ctrl Pts',(7.33536951733907,-38.2742356127273,4.14135807653012));
#60714=CARTESIAN_POINT('Ctrl Pts',(7.34511319782085,-38.2742356127191,4.14461485693852));
#60715=CARTESIAN_POINT('Ctrl Pts',(7.3548786281491,-38.2742356127097,4.14780158544441));
#60716=CARTESIAN_POINT('Ctrl Pts',(7.40494059735844,-38.2742356126613,4.16413818290895));
#60717=CARTESIAN_POINT('Ctrl Pts',(7.45560498502167,-38.2742356122277,4.17865129560831));
#60718=CARTESIAN_POINT('Ctrl Pts',(7.50678821535502,-38.2742356117529,4.19125010342492));
#60719=CARTESIAN_POINT('Ctrl Pts',(7.55797144568837,-38.2742356112782,4.20384891124152));
#60720=CARTESIAN_POINT('Ctrl Pts',(7.60968799204104,-38.2742356112205,4.21453391209546));
#60721=CARTESIAN_POINT('Ctrl Pts',(7.66177351399378,-38.2742356112926,4.2232251536338));
#60722=CARTESIAN_POINT('Ctrl Pts',(7.71385951973192,-38.2742356113647,4.23191647589892));
#60723=CARTESIAN_POINT('Ctrl Pts',(7.76630497190309,-38.2742356112526,4.23861290835011));
#60724=CARTESIAN_POINT('Ctrl Pts',(7.81885823355599,-38.2742356112199,4.24325350235059));
#60725=CARTESIAN_POINT('Ctrl Pts',(7.87141149519477,-38.2742356111873,4.24789409634982));
#60726=CARTESIAN_POINT('Ctrl Pts',(7.92410320133167,-38.2742356114824,4.25048261299401));
#60727=CARTESIAN_POINT('Ctrl Pts',(7.97680547469087,-38.2742356117947,4.25099795223007));
#60728=CARTESIAN_POINT('Ctrl Pts',(8.04056423400334,-38.2742356121725,4.25162140522785));
#60729=CARTESIAN_POINT('Ctrl Pts',(8.10433843773227,-38.2742356123995,4.24920992909844));
#60730=CARTESIAN_POINT('Ctrl Pts',(8.16783744970057,-38.2742356125418,4.2437573156433));
#60731=CARTESIAN_POINT('Ctrl Pts',(8.23026340554995,-38.2742356126817,4.23839684472787));
#60732=CARTESIAN_POINT('Ctrl Pts',(8.29242292091689,-38.2742356127405,4.23009699484735));
#60733=CARTESIAN_POINT('Ctrl Pts',(8.35403932933331,-38.2742356127697,4.21890169877675));
#60734=CARTESIAN_POINT('Ctrl Pts',(8.4140575137154,-38.2742356127981,4.2079967894994));
#60735=CARTESIAN_POINT('Ctrl Pts',(8.47356000826017,-38.2742356127991,4.19434463963401));
#60736=CARTESIAN_POINT('Ctrl Pts',(8.53229689916312,-38.2742356127998,4.17803492716954));
#60737=CARTESIAN_POINT('Ctrl Pts',(8.55498221166293,-38.2742356128001,4.17173580376769));
#60738=CARTESIAN_POINT('Ctrl Pts',(8.57755341554526,-38.2742356128,4.16504079768994));
#60739=CARTESIAN_POINT('Ctrl Pts',(8.59999653905443,-38.2742356128,4.15795713803855));
#60740=CARTESIAN_POINT('Ctrl Pts',(8.65275187384972,-38.2742356128,4.1413061207979));
#60741=CARTESIAN_POINT('Ctrl Pts',(8.70480164426777,-38.2742356128066,4.12250510557686));
#60742=CARTESIAN_POINT('Ctrl Pts',(8.75602778748263,-38.2742356127783,4.10163626378869));
#60743=CARTESIAN_POINT('Ctrl Pts',(8.80228054147308,-38.2742356127528,4.08279351388176));
#60744=CARTESIAN_POINT('Ctrl Pts',(8.84786037356255,-38.2742356126966,4.06226581784222));
#60745=CARTESIAN_POINT('Ctrl Pts',(8.8926632647348,-38.2742356125373,4.04014566152166));
#60746=CARTESIAN_POINT('Ctrl Pts',(8.94857266920348,-38.2742356123387,4.01254197938691));
#60747=CARTESIAN_POINT('Ctrl Pts',(9.00330501446036,-38.2742356122495,3.98243553233308));
#60748=CARTESIAN_POINT('Ctrl Pts',(9.05668746409715,-38.2742356123646,3.95003024395078));
#60749=CARTESIAN_POINT('Ctrl Pts',(9.09347531147182,-38.274235612444,3.92769854483896));
#60750=CARTESIAN_POINT('Ctrl Pts',(9.12962185589216,-38.2742356126008,3.90427618224411));
#60751=CARTESIAN_POINT('Ctrl Pts',(9.16507828894361,-38.2742356127068,3.87984233486085));
#60752=CARTESIAN_POINT('Ctrl Pts',(9.20849780261757,-38.2742356128365,3.8499209446007));
#60753=CARTESIAN_POINT('Ctrl Pts',(9.25088407878093,-38.2742356128,3.81848432781475));
#60754=CARTESIAN_POINT('Ctrl Pts',(9.29213478581693,-38.2742356128,3.7857321116292));
#60755=CARTESIAN_POINT('Ctrl Pts',(9.31268689240908,-38.2742356128,3.76941416009476));
#60756=CARTESIAN_POINT('Ctrl Pts',(9.33295849535396,-38.2742356128,3.75276882613797));
#60757=CARTESIAN_POINT('Ctrl Pts',(9.35293864601996,-38.2742356128,3.73582645507306));
#60758=CARTESIAN_POINT('Ctrl Pts',(9.36914328585316,-38.2742356128,3.72208556664751));
#60759=CARTESIAN_POINT('Ctrl Pts',(9.38514901708334,-38.2742356128,3.70815579621019));
#60760=CARTESIAN_POINT('Ctrl Pts',(9.40097242007251,-38.2742356128,3.69403625763351));
#60761=CARTESIAN_POINT('Ctrl Pts',(9.40479906360245,-38.2742356128,3.69062166717043));
#60762=CARTESIAN_POINT('Ctrl Pts',(9.40861504872694,-38.2742356128,3.68719596937193));
#60763=CARTESIAN_POINT('Ctrl Pts',(9.41242061503587,-38.2742356128,3.68375913884913));
#60764=CARTESIAN_POINT('Ctrl Pts',(9.44710216596526,-38.2742356128,3.65243801522751));
#60765=CARTESIAN_POINT('Ctrl Pts',(9.48095984392308,-38.2742356128367,3.62015512214142));
#60766=CARTESIAN_POINT('Ctrl Pts',(9.51391146087876,-38.2742356126435,3.58711756919405));
#60767=CARTESIAN_POINT('Ctrl Pts',(9.54924040229739,-38.2742356124364,3.55169649185321));
#60768=CARTESIAN_POINT('Ctrl Pts',(9.58352812796506,-38.2742356119099,3.51540827645441));
#60769=CARTESIAN_POINT('Ctrl Pts',(9.61673281222635,-38.2742356107591,3.47851494924075));
#60770=CARTESIAN_POINT('Ctrl Pts',(9.62208609212353,-38.2742356105735,3.47256698402722));
#60771=CARTESIAN_POINT('Ctrl Pts',(9.62741133109786,-38.2742356103727,3.4666032974567));
#60772=CARTESIAN_POINT('Ctrl Pts',(9.63270847298428,-38.2742356101568,3.46062499292125));
#60773=CARTESIAN_POINT('Ctrl Pts',(9.64981262109995,-38.2742356094594,3.4413214121512));
#60774=CARTESIAN_POINT('Ctrl Pts',(9.6666629516528,-38.2742356085896,3.42182106045621));
#60775=CARTESIAN_POINT('Ctrl Pts',(9.6832637335943,-38.2742356078081,3.40214758502691));
#60776=CARTESIAN_POINT('Ctrl Pts',(9.6998645155358,-38.2742356070266,3.38247410959761));
#60777=CARTESIAN_POINT('Ctrl Pts',(9.71621862624953,-38.274235606372,3.3626240804197));
#60778=CARTESIAN_POINT('Ctrl Pts',(9.73233640212346,-38.2742356060233,3.34261606036647));
#60779=CARTESIAN_POINT('Ctrl Pts',(9.78137505758533,-38.2742356049622,3.28174125918181));
#60780=CARTESIAN_POINT('Ctrl Pts',(9.82817652284925,-38.2742356070341,3.219469380873));
#60781=CARTESIAN_POINT('Ctrl Pts',(9.87305796788631,-38.2742356090049,3.15633700294021));
#60782=CARTESIAN_POINT('Ctrl Pts',(9.90790930677723,-38.2742356105353,3.10731344996618));
#60783=CARTESIAN_POINT('Ctrl Pts',(9.94160538607107,-38.2742356118045,3.05776986132032));
#60784=CARTESIAN_POINT('Ctrl Pts',(9.97426184086033,-38.274235612334,3.00794438327731));
#60785=CARTESIAN_POINT('Ctrl Pts',(10.0025204308224,-38.2742356127921,2.96482893296992));
#60786=CARTESIAN_POINT('Ctrl Pts',(10.0300010756658,-38.2742356127974,2.92150209599565));
#60787=CARTESIAN_POINT('Ctrl Pts',(10.0567356987662,-38.2742356127997,2.87811469479087));
#60788=CARTESIAN_POINT('Ctrl Pts',(10.0608963896839,-38.2742356128001,2.87136234352503));
#60789=CARTESIAN_POINT('Ctrl Pts',(10.065038908559,-38.2742356128,2.86460852225224));
#60790=CARTESIAN_POINT('Ctrl Pts',(10.0691632550904,-38.2742356128,2.85785379691802));
#60791=CARTESIAN_POINT('Ctrl Pts',(10.069349746965,-38.2742356128,2.85754836637758));
#60792=CARTESIAN_POINT('Ctrl Pts',(10.0695362045312,-38.2742356128,2.8572429295994));
#60793=CARTESIAN_POINT('Ctrl Pts',(10.0697226343,-38.2742356128,2.85693747561));
#60794=CARTESIAN_POINT('',(5.86597170597801,-38.2742356128,4.46707956737663));
#60795=CARTESIAN_POINT('Ctrl Pts',(5.86597168188,-38.2742356128,4.46707937639));
#60796=CARTESIAN_POINT('Ctrl Pts',(5.86521847952036,-38.2742356128,4.46244689300994));
#60797=CARTESIAN_POINT('Ctrl Pts',(5.86451251383266,-38.2742356128,4.45775891558074));
#60798=CARTESIAN_POINT('Ctrl Pts',(5.86386803963271,-38.2742356127999,4.45310957470034));
#60799=CARTESIAN_POINT('Ctrl Pts',(5.86322141073989,-38.2742356127999,4.4484446895179));
#60800=CARTESIAN_POINT('Ctrl Pts',(5.86262940399853,-38.2742356127997,4.44377160748202));
#60801=CARTESIAN_POINT('Ctrl Pts',(5.8620923017773,-38.2742356127993,4.43909214018255));
#60802=CARTESIAN_POINT('Ctrl Pts',(5.85880657218188,-38.2742356127967,4.41046544010783));
#60803=CARTESIAN_POINT('Ctrl Pts',(5.85757720777026,-38.2742356127862,4.38158802376726));
#60804=CARTESIAN_POINT('Ctrl Pts',(5.8584296426603,-38.2742356127781,4.35276644081144));
#60805=CARTESIAN_POINT('Ctrl Pts',(5.85930076534106,-38.2742356127698,4.32331300700491));
#60806=CARTESIAN_POINT('Ctrl Pts',(5.86234582254843,-38.2742356127665,4.29391819633034));
#60807=CARTESIAN_POINT('Ctrl Pts',(5.8675381376056,-38.2742356127753,4.26490239478237));
#60808=CARTESIAN_POINT('Ctrl Pts',(5.86889338350707,-38.2742356127776,4.25732898182635));
#60809=CARTESIAN_POINT('Ctrl Pts',(5.87039464119523,-38.2742356127806,4.24978133983799));
#60810=CARTESIAN_POINT('Ctrl Pts',(5.87204087021659,-38.2742356127838,4.24226504999152));
#60811=CARTESIAN_POINT('Ctrl Pts',(5.87836316827691,-38.2742356127961,4.21339894199529));
#60812=CARTESIAN_POINT('Ctrl Pts',(5.88682789242818,-38.2742356127977,4.18500208544504));
#60813=CARTESIAN_POINT('Ctrl Pts',(5.89734093285122,-38.2742356127986,4.15738756121468));
#60814=CARTESIAN_POINT('Ctrl Pts',(5.90798936103777,-38.2742356127994,4.12941741496392));
#60815=CARTESIAN_POINT('Ctrl Pts',(5.92073893937052,-38.2742356127996,4.10225034381996));
#60816=CARTESIAN_POINT('Ctrl Pts',(5.93544258166133,-38.2742356127962,4.07619079382842));
#60817=CARTESIAN_POINT('Ctrl Pts',(5.94424329501613,-38.2742356127942,4.06059311910984));
#60818=CARTESIAN_POINT('Ctrl Pts',(5.9537431263084,-38.2742356127907,4.04539178133931));
#60819=CARTESIAN_POINT('Ctrl Pts',(5.96390288113939,-38.2742356127826,4.03064749997891));
#60820=CARTESIAN_POINT('Ctrl Pts',(5.9810490467527,-38.2742356127691,4.00576423318162));
#60821=CARTESIAN_POINT('Ctrl Pts',(6.00007557603257,-38.2742356127705,3.98218298150727));
#60822=CARTESIAN_POINT('Ctrl Pts',(6.0207634836268,-38.2742356127792,3.96016862488714));
#60823=CARTESIAN_POINT('Ctrl Pts',(6.04132264280314,-38.2742356127878,3.93829127166248));
#60824=CARTESIAN_POINT('Ctrl Pts',(6.06352216120708,-38.274235612797,3.91796176161847));
#60825=CARTESIAN_POINT('Ctrl Pts',(6.08711174806247,-38.274235612799,3.89940302051962));
#60826=CARTESIAN_POINT('Ctrl Pts',(6.10047468249298,-38.2742356128002,3.88888993939034));
#60827=CARTESIAN_POINT('Ctrl Pts',(6.11428307295518,-38.2742356128,3.87894438340428));
#60828=CARTESIAN_POINT('Ctrl Pts',(6.12848708214859,-38.2742356128,3.86960082529007));
#60829=CARTESIAN_POINT('Ctrl Pts',(6.15338993303026,-38.2742356128,3.85321944794413));
#60830=CARTESIAN_POINT('Ctrl Pts',(6.17951083601368,-38.2742356128,3.8386899453089));
#60831=CARTESIAN_POINT('Ctrl Pts',(6.20656832160519,-38.2742356127994,3.82617616464038));
#60832=CARTESIAN_POINT('Ctrl Pts',(6.23388644440146,-38.2742356127989,3.81354184221628));
#60833=CARTESIAN_POINT('Ctrl Pts',(6.26215874205547,-38.2742356127977,3.80296251155965));
#60834=CARTESIAN_POINT('Ctrl Pts',(6.29106888820992,-38.2742356127976,3.79456090317743));
#60835=CARTESIAN_POINT('Ctrl Pts',(6.3074976151048,-38.2742356127975,3.78978653334714));
#60836=CARTESIAN_POINT('Ctrl Pts',(6.32413188205186,-38.2742356127978,3.78571455856394));
#60837=CARTESIAN_POINT('Ctrl Pts',(6.34091089081714,-38.2742356127985,3.78236053332006));
#60838=CARTESIAN_POINT('Ctrl Pts',(6.37044752808834,-38.2742356127997,3.77645633311296));
#60839=CARTESIAN_POINT('Ctrl Pts',(6.40043493735285,-38.2742356127998,3.77278002228652));
#60840=CARTESIAN_POINT('Ctrl Pts',(6.43053277796928,-38.2742356127999,3.77137787478142));
#60841=CARTESIAN_POINT('Ctrl Pts',(6.46027533040864,-38.2742356128,3.76999227884349));
#60842=CARTESIAN_POINT('Ctrl Pts',(6.49012515981829,-38.2742356128,3.77082754411741));
#60843=CARTESIAN_POINT('Ctrl Pts',(6.5197493946603,-38.2742356127999,3.7738779521685));
#60844=CARTESIAN_POINT('Ctrl Pts',(6.53700806446756,-38.2742356127999,3.77565507774194));
#60845=CARTESIAN_POINT('Ctrl Pts',(6.55419012590196,-38.2742356127999,3.77818308879307));
#60846=CARTESIAN_POINT('Ctrl Pts',(6.57123018973728,-38.2742356127998,3.78145267165003));
#60847=CARTESIAN_POINT('Ctrl Pts',(6.59976050908503,-38.2742356127997,3.78692696117996));
#60848=CARTESIAN_POINT('Ctrl Pts',(6.62788960711445,-38.2742356127906,3.79448443707445));
#60849=CARTESIAN_POINT('Ctrl Pts',(6.65531799034395,-38.2742356127749,3.80403807813415));
#60850=CARTESIAN_POINT('Ctrl Pts',(6.66446340893655,-38.2742356127697,3.80722353918898));
#60851=CARTESIAN_POINT('Ctrl Pts',(6.67353103771832,-38.2742356127651,3.81063051321018));
#60852=CARTESIAN_POINT('Ctrl Pts',(6.68251015765301,-38.2742356127641,3.81425453223265));
#60853=CARTESIAN_POINT('Ctrl Pts',(6.70935764852629,-38.2742356127609,3.82509031773702));
#60854=CARTESIAN_POINT('Ctrl Pts',(6.73541115755773,-38.2742356127925,3.83786890772086));
#60855=CARTESIAN_POINT('Ctrl Pts',(6.76040182236934,-38.2742356127979,3.85244737074258));
#60856=CARTESIAN_POINT('Ctrl Pts',(6.76883599265748,-38.2742356127998,3.85736749754158));
#60857=CARTESIAN_POINT('Ctrl Pts',(6.77714924361623,-38.2742356128,3.86249222401201));
#60858=CARTESIAN_POINT('Ctrl Pts',(6.78533170849366,-38.2742356128,3.86781477988002));
#60859=CARTESIAN_POINT('Ctrl Pts',(6.78735517139677,-38.2742356128,3.86913100848716));
#60860=CARTESIAN_POINT('Ctrl Pts',(6.7893712469383,-38.2742356128,3.87045977491255));
#60861=CARTESIAN_POINT('Ctrl Pts',(6.79137807329,-38.2742356128,3.87179977251));
#60862=CARTESIAN_POINT('',(1.96099433484507E-5,-38.2742356128,11.3643459819103));
#60863=CARTESIAN_POINT('Ctrl Pts',(1.96099437674846E-5,-38.2742356128,11.3643459876291));
#60864=CARTESIAN_POINT('Ctrl Pts',(0.0472697587385178,-38.2742356128,11.3643425323295));
#60865=CARTESIAN_POINT('Ctrl Pts',(0.0945221110592471,-38.2742356128,11.363777913887));
#60866=CARTESIAN_POINT('Ctrl Pts',(0.141759781888426,-38.2742356128,11.3626518420063));
#60867=CARTESIAN_POINT('Ctrl Pts',(0.245241952691282,-38.2742356128,11.3601849895844));
#60868=CARTESIAN_POINT('Ctrl Pts',(0.348663149583877,-38.2742356128,11.3550229294214));
#60869=CARTESIAN_POINT('Ctrl Pts',(0.451876489369207,-38.2742356128,11.3471684549389));
#60870=CARTESIAN_POINT('Ctrl Pts',(0.614063148796439,-38.2742356128,11.3348261454999));
#60871=CARTESIAN_POINT('Ctrl Pts',(0.775739638000677,-38.2742356128,11.315833030005));
#60872=CARTESIAN_POINT('Ctrl Pts',(0.93635482831518,-38.2742356128,11.290242195175));
#60873=CARTESIAN_POINT('Ctrl Pts',(1.09834028128939,-38.2742356128,11.2644330362542));
#60874=CARTESIAN_POINT('Ctrl Pts',(1.25924606969199,-38.2742356128,11.2319132010809));
#60875=CARTESIAN_POINT('Ctrl Pts',(1.41851896539168,-38.2742356128,11.1927887894903));
#60876=CARTESIAN_POINT('Ctrl Pts',(1.57908539079494,-38.2742356128,11.1533466302484));
#60877=CARTESIAN_POINT('Ctrl Pts',(1.73799210302976,-38.2742356128,11.1071922912551));
#60878=CARTESIAN_POINT('Ctrl Pts',(1.8946873563024,-38.2742356128,11.0544851600217));
#60879=CARTESIAN_POINT('Ctrl Pts',(2.05312041979911,-38.2742356128,11.0011934865662));
#60880=CARTESIAN_POINT('Ctrl Pts',(2.20929248845345,-38.2742356128,10.9412029647644));
#60881=CARTESIAN_POINT('Ctrl Pts',(2.36265166093631,-38.2742356128,10.8747284217424));
#60882=CARTESIAN_POINT('Ctrl Pts',(2.51692692416807,-38.2742356128,10.8078567931537));
#60883=CARTESIAN_POINT('Ctrl Pts',(2.66835537858543,-38.2742356128,10.7344235939096));
#60884=CARTESIAN_POINT('Ctrl Pts',(2.81639684408017,-38.2742356128,10.6546960255344));
#60885=CARTESIAN_POINT('Ctrl Pts',(2.9651921921399,-38.2742356128,10.5745624545331));
#60886=CARTESIAN_POINT('Ctrl Pts',(3.11056575655573,-38.2742356128,10.4880704051236));
#60887=CARTESIAN_POINT('Ctrl Pts',(3.25199403978543,-38.2742356128,10.3955377043536));
#60888=CARTESIAN_POINT('Ctrl Pts',(3.39399708912114,-38.2742356128,10.302628949665));
#60889=CARTESIAN_POINT('Ctrl Pts',(3.53202251132963,-38.2742356128,10.2036305196863));
#60890=CARTESIAN_POINT('Ctrl Pts',(3.66556871335094,-38.2742356128,10.0989083774764));
#60891=CARTESIAN_POINT('Ctrl Pts',(3.79963116547533,-38.2742356128,9.99378141045011));
#60892=CARTESIAN_POINT('Ctrl Pts',(3.9291794812562,-38.2742356128,9.88288657476412));
#60893=CARTESIAN_POINT('Ctrl Pts',(4.05373795681475,-38.2742356128,9.76663590776425));
#60894=CARTESIAN_POINT('Ctrl Pts',(4.17841478767598,-38.2742356128,9.65027477953067));
#60895=CARTESIAN_POINT('Ctrl Pts',(4.2980920856376,-38.2742356128,9.52854784101018));
#60896=CARTESIAN_POINT('Ctrl Pts',(4.41232768238676,-38.2742356128,9.40190718867832));
#60897=CARTESIAN_POINT('Ctrl Pts',(4.52652134987461,-38.2742356128,9.27531301878411));
#60898=CARTESIAN_POINT('Ctrl Pts',(4.63527711242045,-38.2742356128,9.14380895394925));
#60899=CARTESIAN_POINT('Ctrl Pts',(4.73819115171614,-38.2742356128,9.00788229232382));
#60900=CARTESIAN_POINT('Ctrl Pts',(4.77683663195496,-38.2742356128,8.95684016870565));
#60901=CARTESIAN_POINT('Ctrl Pts',(4.81465877164806,-38.2742356128,8.90517476127336));
#60902=CARTESIAN_POINT('Ctrl Pts',(4.85163765566323,-38.2742356128,8.85291307936199));
#60903=CARTESIAN_POINT('Ctrl Pts',(4.94954299698168,-38.2742356128,8.71454498249593));
#60904=CARTESIAN_POINT('Ctrl Pts',(5.04153458224144,-38.2742356128,8.57199450810618));
#60905=CARTESIAN_POINT('Ctrl Pts',(5.12727126160882,-38.2742356128,8.42578326478887));
#60906=CARTESIAN_POINT('Ctrl Pts',(5.21317959608459,-38.2742356128,8.27927928903775));
#60907=CARTESIAN_POINT('Ctrl Pts',(5.29280778803326,-38.2742356128,8.12910009662651));
#60908=CARTESIAN_POINT('Ctrl Pts',(5.3658589507314,-38.2742356128,7.97579537182009));
#60909=CARTESIAN_POINT('Ctrl Pts',(5.438330036196,-38.2742356128,7.82370799356053));
#60910=CARTESIAN_POINT('Ctrl Pts',(5.50432804704475,-38.2742356128,7.66854477968326));
#60911=CARTESIAN_POINT('Ctrl Pts',(5.56361038688553,-38.2742356128,7.51086328617028));
#60912=CARTESIAN_POINT('Ctrl Pts',(5.62264547171644,-38.2742356128,7.35383945123388));
#60913=CARTESIAN_POINT('Ctrl Pts',(5.67502067999286,-38.2742356128,7.19431853361871));
#60914=CARTESIAN_POINT('Ctrl Pts',(5.72054497528076,-38.2742356128,7.03286828206397));
#60915=CARTESIAN_POINT('Ctrl Pts',(5.76583911502499,-38.2742356128,6.87223426874395));
#60916=CARTESIAN_POINT('Ctrl Pts',(5.80435134203715,-38.2742356128,6.70969060885712));
#60917=CARTESIAN_POINT('Ctrl Pts',(5.83594316574969,-38.2742356128,6.545810032148));
#60918=CARTESIAN_POINT('Ctrl Pts',(5.86838176458437,-38.2742356128,6.37753686333587));
#60919=CARTESIAN_POINT('Ctrl Pts',(5.89352360761337,-38.2742356128,6.20785433630628));
#60920=CARTESIAN_POINT('Ctrl Pts',(5.91127539609655,-38.2742356128,6.03739372678238));
#60921=CARTESIAN_POINT('Ctrl Pts',(5.92829692245465,-38.2742356128,5.87394542067063));
#60922=CARTESIAN_POINT('Ctrl Pts',(5.9385241365587,-38.2742356128,5.70978199238531));
#60923=CARTESIAN_POINT('Ctrl Pts',(5.94192631696286,-38.2742356128,5.54546668994573));
#60924=CARTESIAN_POINT('Ctrl Pts',(5.94530777257515,-38.2742356128,5.38215233397002));
#60925=CARTESIAN_POINT('Ctrl Pts',(5.94194702074655,-38.2742356128,5.2186881472073));
#60926=CARTESIAN_POINT('Ctrl Pts',(5.93186515922344,-38.2742356128,5.05563062583815));
#60927=CARTESIAN_POINT('Ctrl Pts',(5.92187214024643,-38.2742356128,4.89400998647002));
#60928=CARTESIAN_POINT('Ctrl Pts',(5.90527590134661,-38.2742356128,4.73278906515281));
#60929=CARTESIAN_POINT('Ctrl Pts',(5.88214831546199,-38.2742356128,4.57251032877608));
#60930=CARTESIAN_POINT('Ctrl Pts',(5.87863513626286,-38.2742356128,4.54816330330133));
#60931=CARTESIAN_POINT('Ctrl Pts',(5.87497134477382,-38.2742356128,4.52383801660917));
#60932=CARTESIAN_POINT('Ctrl Pts',(5.87115729873963,-38.2742356128,4.49953636706381));
#60933=CARTESIAN_POINT('Ctrl Pts',(5.86945856588079,-38.2742356128,4.48871268789568));
#60934=CARTESIAN_POINT('Ctrl Pts',(5.86773011656,-38.2742356128,4.47789435759));
#60935=CARTESIAN_POINT('Ctrl Pts',(5.86597173001,-38.2742356128,4.46707975784));
#60936=CARTESIAN_POINT('',(-5.86597169341063,-38.2742356128,4.46707928635527));
#60937=CARTESIAN_POINT('Ctrl Pts',(-5.86597170737572,-38.2742356128,4.46707937224455));
#60938=CARTESIAN_POINT('Ctrl Pts',(-5.87355683913933,-38.2742356128,4.51373024197535));
#60939=CARTESIAN_POINT('Ctrl Pts',(-5.88058812630781,-38.2742356128,4.56047314614868));
#60940=CARTESIAN_POINT('Ctrl Pts',(-5.88706259142912,-38.2742356128,4.6072918885805));
#60941=CARTESIAN_POINT('Ctrl Pts',(-5.90124205880004,-38.2742356128,4.70982774570868));
#60942=CARTESIAN_POINT('Ctrl Pts',(-5.91275148943592,-38.2742356128,4.81273614246136));
#60943=CARTESIAN_POINT('Ctrl Pts',(-5.92157005802919,-38.2742356128,4.91587165229804));
#60944=CARTESIAN_POINT('Ctrl Pts',(-5.93542730978309,-38.2742356128,5.07793590450159));
#60945=CARTESIAN_POINT('Ctrl Pts',(-5.94263812513509,-38.2742356128,5.24056440725797));
#60946=CARTESIAN_POINT('Ctrl Pts',(-5.94316641713255,-38.2742356128,5.40320465831166));
#60947=CARTESIAN_POINT('Ctrl Pts',(-5.9436992161682,-38.2742356128,5.56723244850165));
#60948=CARTESIAN_POINT('Ctrl Pts',(-5.93743505163129,-38.2742356128,5.7312719950569));
#60949=CARTESIAN_POINT('Ctrl Pts',(-5.92438982488806,-38.2742356128,5.89476021211246));
#60950=CARTESIAN_POINT('Ctrl Pts',(-5.91123865175597,-38.2742356128,6.05957619345761));
#60951=CARTESIAN_POINT('Ctrl Pts',(-5.89119590289791,-38.2742356128,6.22383164873817));
#60952=CARTESIAN_POINT('Ctrl Pts',(-5.86433031406539,-38.2742356128,6.38695639973516));
#60953=CARTESIAN_POINT('Ctrl Pts',(-5.83716677560075,-38.2742356128,6.5518902664695));
#60954=CARTESIAN_POINT('Ctrl Pts',(-5.803028282697,-38.2742356128,6.71566798530386));
#60955=CARTESIAN_POINT('Ctrl Pts',(-5.76203826654907,-38.2742356128,6.87771032354166));
#60956=CARTESIAN_POINT('Ctrl Pts',(-5.72080339661986,-38.2742356128,7.04072062137001));
#60957=CARTESIAN_POINT('Ctrl Pts',(-5.67263501528278,-38.2742356128,7.20197451664067));
#60958=CARTESIAN_POINT('Ctrl Pts',(-5.6177101305643,-38.2742356128,7.36089593699001));
#60959=CARTESIAN_POINT('Ctrl Pts',(-5.56250554778591,-38.2742356128,7.52062664466291));
#60960=CARTESIAN_POINT('Ctrl Pts',(-5.50047559764723,-38.2742356128,7.67800082696959));
#60961=CARTESIAN_POINT('Ctrl Pts',(-5.43184993537474,-38.2742356128,7.8324507496487));
#60962=CARTESIAN_POINT('Ctrl Pts',(-5.36294537767596,-38.2742356128,7.98752835846738));
#60963=CARTESIAN_POINT('Ctrl Pts',(-5.28739152667286,-38.2742356128,8.13965765223937));
#60964=CARTESIAN_POINT('Ctrl Pts',(-5.20546906596608,-38.2742356128,8.288284788677));
#60965=CARTESIAN_POINT('Ctrl Pts',(-5.12322991732637,-38.2742356128,8.43748647353773));
#60966=CARTESIAN_POINT('Ctrl Pts',(-5.03457296952003,-38.2742356128,8.58315862728677));
#60967=CARTESIAN_POINT('Ctrl Pts',(-4.939828539296,-38.2742356128,8.72476556363208));
#60968=CARTESIAN_POINT('Ctrl Pts',(-4.84499408306954,-38.2742356128,8.86650705465637));
#60969=CARTESIAN_POINT('Ctrl Pts',(-4.74406073872847,-38.2742356128,9.00417536348988));
#60970=CARTESIAN_POINT('Ctrl Pts',(-4.63740374669067,-38.2742356128,9.13726147277406));
#60971=CARTESIAN_POINT('Ctrl Pts',(-4.53078590229245,-38.2742356128,9.27029873381173));
#60972=CARTESIAN_POINT('Ctrl Pts',(-4.41844878903217,-38.2742356128,9.39875692919792));
#60973=CARTESIAN_POINT('Ctrl Pts',(-4.30080854952501,-38.2742356128,9.52215924236615));
#60974=CARTESIAN_POINT('Ctrl Pts',(-4.25663325102553,-38.2742356128,9.56849826753789));
#60975=CARTESIAN_POINT('Ctrl Pts',(-4.21171056680681,-38.2742356128,9.61412470438002));
#60976=CARTESIAN_POINT('Ctrl Pts',(-4.16606395831939,-38.2742356128,9.65901455978178));
#60977=CARTESIAN_POINT('Ctrl Pts',(-4.04520980158801,-38.2742356128,9.77786513379252));
#60978=CARTESIAN_POINT('Ctrl Pts',(-3.91927805635973,-38.2742356128,9.8915501596496));
#60979=CARTESIAN_POINT('Ctrl Pts',(-3.78872879215426,-38.2742356128,9.99964916764474));
#60980=CARTESIAN_POINT('Ctrl Pts',(-3.65791815280783,-38.2742356128,10.1079646027));
#60981=CARTESIAN_POINT('Ctrl Pts',(-3.52247168238513,-38.2742356128,10.2106714302746));
#60982=CARTESIAN_POINT('Ctrl Pts',(-3.38288426840432,-38.2742356128,10.3073883619451));
#60983=CARTESIAN_POINT('Ctrl Pts',(-3.24440527586281,-38.2742356128,10.403337293711));
#60984=CARTESIAN_POINT('Ctrl Pts',(-3.10185108199932,-38.2742356128,10.4933909566946));
#60985=CARTESIAN_POINT('Ctrl Pts',(-2.95573306037451,-38.2742356128,10.5772203846891));
#60986=CARTESIAN_POINT('Ctrl Pts',(-2.81022446838551,-38.2742356128,10.6607001765661));
#60987=CARTESIAN_POINT('Ctrl Pts',(-2.66118192854463,-38.2742356128,10.7380074008848));
#60988=CARTESIAN_POINT('Ctrl Pts',(-2.50913515301595,-38.2742356128,10.8088623460546));
#60989=CARTESIAN_POINT('Ctrl Pts',(-2.35785707494213,-38.2742356128,10.8793590724076));
#60990=CARTESIAN_POINT('Ctrl Pts',(-2.20360527131204,-38.2742356128,10.9434684638986));
#60991=CARTESIAN_POINT('Ctrl Pts',(-2.04692280704148,-38.2742356128,11.0009618734306));
#60992=CARTESIAN_POINT('Ctrl Pts',(-1.8860406861784,-38.2742356128,11.0599963142292));
#60993=CARTESIAN_POINT('Ctrl Pts',(-1.72259597875071,-38.2742356128,11.1120549335068));
#60994=CARTESIAN_POINT('Ctrl Pts',(-1.55719679180931,-38.2742356128,11.156944290039));
#60995=CARTESIAN_POINT('Ctrl Pts',(-1.3986016946317,-38.2742356128,11.1999870159019));
#60996=CARTESIAN_POINT('Ctrl Pts',(-1.23820990933965,-38.2742356128,11.236438384511));
#60997=CARTESIAN_POINT('Ctrl Pts',(-1.07657244471484,-38.2742356128,11.266177642151));
#60998=CARTESIAN_POINT('Ctrl Pts',(-0.915919614215123,-38.2742356128,11.2957357395136));
#60999=CARTESIAN_POINT('Ctrl Pts',(-0.754036419195308,-38.2742356128,11.3186631496228));
#61000=CARTESIAN_POINT('Ctrl Pts',(-0.591475523881897,-38.2742356128,11.3348913497454));
#61001=CARTESIAN_POINT('Ctrl Pts',(-0.430347134286956,-38.2742356128,11.3509765450609));
#61002=CARTESIAN_POINT('Ctrl Pts',(-0.268553114665031,-38.2742356128,11.3604800062314));
#61003=CARTESIAN_POINT('Ctrl Pts',(-0.106640434026326,-38.2742356128,11.3633855794612));
#61004=CARTESIAN_POINT('Ctrl Pts',(-0.0820452052041727,-38.2742356128,11.3638269484643));
#61005=CARTESIAN_POINT('Ctrl Pts',(-0.0574472519929075,-38.2742356128,11.3641161688066));
#61006=CARTESIAN_POINT('Ctrl Pts',(-0.0328485055666778,-38.2742356128,11.364253288805));
#61007=CARTESIAN_POINT('Ctrl Pts',(-0.0218925028918889,-38.2742356128,11.3643143604971));
#61008=CARTESIAN_POINT('Ctrl Pts',(-0.0109370086389902,-38.2742356128,11.3643452424498));
#61009=CARTESIAN_POINT('Ctrl Pts',(1.96099429597E-5,-38.2742356128,11.3643459766));
#61010=CARTESIAN_POINT('',(-6.79137866102648,-38.2742356128,3.871800145837));
#61011=CARTESIAN_POINT('Ctrl Pts',(-6.79137822626605,-38.2742356128,3.87179985553789));
#61012=CARTESIAN_POINT('Ctrl Pts',(-6.7874746870692,-38.2742356128,3.86919337612066));
#61013=CARTESIAN_POINT('Ctrl Pts',(-6.78350177861248,-38.2742356128,3.86660738669588));
#61014=CARTESIAN_POINT('Ctrl Pts',(-6.77953817139297,-38.2742356127999,
3.86409312034724));
#61015=CARTESIAN_POINT('Ctrl Pts',(-6.77556131249333,-38.2742356127999,
3.86157044795541));
#61016=CARTESIAN_POINT('Ctrl Pts',(-6.77155434602956,-38.2742356127997,
3.85909408218151));
#61017=CARTESIAN_POINT('Ctrl Pts',(-6.76751880344076,-38.2742356127993,
3.8566650311283));
#61018=CARTESIAN_POINT('Ctrl Pts',(-6.74283132067483,-38.2742356127967,
3.84180528062534));
#61019=CARTESIAN_POINT('Ctrl Pts',(-6.71706303780477,-38.2742356127862,
3.82871283533343));
#61020=CARTESIAN_POINT('Ctrl Pts',(-6.69048236453115,-38.2742356127781,
3.81753794777997));
#61021=CARTESIAN_POINT('Ctrl Pts',(-6.66331896745911,-38.2742356127698,
3.8061180749752));
#61022=CARTESIAN_POINT('Ctrl Pts',(-6.63530751562895,-38.2742356127665,
3.79670075836635));
#61023=CARTESIAN_POINT('Ctrl Pts',(-6.60675061684617,-38.2742356127753,
3.78939456752495));
#61024=CARTESIAN_POINT('Ctrl Pts',(-6.59929698268323,-38.2742356127776,
3.78748757916214));
#61025=CARTESIAN_POINT('Ctrl Pts',(-6.59180625735376,-38.2742356127806,
3.78572414505303));
#61026=CARTESIAN_POINT('Ctrl Pts',(-6.58428395105746,-38.2742356127838,
3.78410563257977));
#61027=CARTESIAN_POINT('Ctrl Pts',(-6.55539473516567,-38.2742356127961,
3.77788977876823));
#61028=CARTESIAN_POINT('Ctrl Pts',(-6.52604419496571,-38.2742356127977,
3.773818071927));
#61029=CARTESIAN_POINT('Ctrl Pts',(-6.49655625119644,-38.2742356127986,
3.77193468945706));
#61030=CARTESIAN_POINT('Ctrl Pts',(-6.46668855933259,-38.2742356127994,
3.77002705263727));
#61031=CARTESIAN_POINT('Ctrl Pts',(-6.43668043247659,-38.2742356127996,
3.770364419042));
#61032=CARTESIAN_POINT('Ctrl Pts',(-6.40686989994023,-38.2742356127962,
3.77293917800287));
#61033=CARTESIAN_POINT('Ctrl Pts',(-6.38902711292706,-38.2742356127942,
3.77448027344265));
#61034=CARTESIAN_POINT('Ctrl Pts',(-6.37125510424854,-38.2742356127907,
3.7768218932986));
#61035=CARTESIAN_POINT('Ctrl Pts',(-6.35362537931003,-38.2742356127826,
3.77995354797865));
#61036=CARTESIAN_POINT('Ctrl Pts',(-6.32387247818031,-38.2742356127691,
3.78523870202347));
#61037=CARTESIAN_POINT('Ctrl Pts',(-6.29452471716957,-38.2742356127705,
3.79277482754427));
#61038=CARTESIAN_POINT('Ctrl Pts',(-6.26591393330974,-38.2742356127792,
3.80247248097018));
#61039=CARTESIAN_POINT('Ctrl Pts',(-6.23748120457973,-38.2742356127878,
3.8121097824341));
#61040=CARTESIAN_POINT('Ctrl Pts',(-6.20977683144767,-38.274235612797,3.82388158510264));
#61041=CARTESIAN_POINT('Ctrl Pts',(-6.1831074537671,-38.274235612799,3.83765256203365));
#61042=CARTESIAN_POINT('Ctrl Pts',(-6.1679998927991,-38.2742356128002,3.84545348922686));
#61043=CARTESIAN_POINT('Ctrl Pts',(-6.15322406734753,-38.2742356128,3.85389509364796));
#61044=CARTESIAN_POINT('Ctrl Pts',(-6.13883201163921,-38.2742356128,3.86294631787056));
#61045=CARTESIAN_POINT('Ctrl Pts',(-6.11359947122505,-38.2742356128,3.87881516841026));
#61046=CARTESIAN_POINT('Ctrl Pts',(-6.08954705620527,-38.2742356128,3.8965602905199));
#61047=CARTESIAN_POINT('Ctrl Pts',(-6.0669405737948,-38.2742356127994,3.91599348875386));
#61048=CARTESIAN_POINT('Ctrl Pts',(-6.0441163294935,-38.2742356127989,3.93561388152413));
#61049=CARTESIAN_POINT('Ctrl Pts',(-6.02276645828458,-38.2742356127977,
3.95695464194579));
#61050=CARTESIAN_POINT('Ctrl Pts',(-6.00313380480363,-38.2742356127976,
3.97977880667488));
#61051=CARTESIAN_POINT('Ctrl Pts',(-5.99197718539001,-38.2742356127975,
3.99274906153947));
#61052=CARTESIAN_POINT('Ctrl Pts',(-5.98137450999299,-38.2742356127978,
4.00619759615233));
#61053=CARTESIAN_POINT('Ctrl Pts',(-5.97136514237198,-38.2742356127985,
4.02007553453086));
#61054=CARTESIAN_POINT('Ctrl Pts',(-5.95374532527902,-38.2742356127997,
4.04450532321639));
#61055=CARTESIAN_POINT('Ctrl Pts',(-5.93796594671887,-38.2742356127998,
4.07026908063358));
#61056=CARTESIAN_POINT('Ctrl Pts',(-5.92421023426017,-38.2742356127999,
4.09707628881351));
#61057=CARTESIAN_POINT('Ctrl Pts',(-5.91061690032008,-38.2742356128,4.1235670528423));
#61058=CARTESIAN_POINT('Ctrl Pts',(-5.89900003626705,-38.2742356128,4.15107629598417));
#61059=CARTESIAN_POINT('Ctrl Pts',(-5.88949246037583,-38.2742356127999,
4.17929873891104));
#61060=CARTESIAN_POINT('Ctrl Pts',(-5.88395347814263,-38.2742356127999,
4.19574074386982));
#61061=CARTESIAN_POINT('Ctrl Pts',(-5.87912955562004,-38.2742356127999,
4.21242438372798));
#61062=CARTESIAN_POINT('Ctrl Pts',(-5.87503933051281,-38.2742356127998,
4.22928629342425));
#61063=CARTESIAN_POINT('Ctrl Pts',(-5.8681910328462,-38.2742356127997,4.25751832804343));
#61064=CARTESIAN_POINT('Ctrl Pts',(-5.86340476684082,-38.2742356127906,
4.28624903021261));
#61065=CARTESIAN_POINT('Ctrl Pts',(-5.86072552655069,-38.2742356127749,
4.31516978274542));
#61066=CARTESIAN_POINT('Ctrl Pts',(-5.85983219010252,-38.2742356127697,
4.32481280074619));
#61067=CARTESIAN_POINT('Ctrl Pts',(-5.85917268201552,-38.2742356127651,
4.33447687936722));
#61068=CARTESIAN_POINT('Ctrl Pts',(-5.8587473810514,-38.2742356127641,4.3441504118431));
#61069=CARTESIAN_POINT('Ctrl Pts',(-5.85747573494016,-38.2742356127609,
4.37307418816316));
#61070=CARTESIAN_POINT('Ctrl Pts',(-5.85830122916367,-38.2742356127925,
4.40208101771261));
#61071=CARTESIAN_POINT('Ctrl Pts',(-5.86120527939883,-38.2742356127979,
4.43086697454951));
#61072=CARTESIAN_POINT('Ctrl Pts',(-5.86218537575815,-38.2742356127998,
4.44058203083669));
#61073=CARTESIAN_POINT('Ctrl Pts',(-5.86340179293723,-38.2742356128,4.45027188757047));
#61074=CARTESIAN_POINT('Ctrl Pts',(-5.8648524612382,-38.2742356128,4.45992475891561));
#61075=CARTESIAN_POINT('Ctrl Pts',(-5.86521120069541,-38.2742356128,4.4623118420445));
#61076=CARTESIAN_POINT('Ctrl Pts',(-5.86558441248322,-38.2742356128,4.46469740146893));
#61077=CARTESIAN_POINT('Ctrl Pts',(-5.86597167956,-38.2742356128,4.46707920117));
#61078=CARTESIAN_POINT('',(-10.0697223221,-38.2742356128,2.85693798735));
#61079=CARTESIAN_POINT('Ctrl Pts',(-10.0697223221334,-38.2742356128,2.85693798737036));
#61080=CARTESIAN_POINT('Ctrl Pts',(-10.0633104414333,-38.2742356128,2.8674434550834));
#61081=CARTESIAN_POINT('Ctrl Pts',(-10.0568574951365,-38.2742356128007,
2.87794244256903));
#61082=CARTESIAN_POINT('Ctrl Pts',(-10.0503628618,-38.2742356127971,2.88843372499632));
#61083=CARTESIAN_POINT('Ctrl Pts',(-10.0215331036382,-38.2742356127809,
2.93500465818227));
#61084=CARTESIAN_POINT('Ctrl Pts',(-9.99182828957869,-38.2742356126542,
2.9815154431619));
#61085=CARTESIAN_POINT('Ctrl Pts',(-9.96120627016625,-38.274235611881,3.02776802419006));
#61086=CARTESIAN_POINT('Ctrl Pts',(-9.92616571750551,-38.2742356109961,
3.0806945140921));
#61087=CARTESIAN_POINT('Ctrl Pts',(-9.88992281642545,-38.2742356091384,
3.13328334536304));
#61088=CARTESIAN_POINT('Ctrl Pts',(-9.85233972844716,-38.2742356074002,
3.18522873807128));
#61089=CARTESIAN_POINT('Ctrl Pts',(-9.81179508152477,-38.2742356055251,
3.24126744377361));
#61090=CARTESIAN_POINT('Ctrl Pts',(-9.76968638910866,-38.2742356041571,
3.29655790872663));
#61091=CARTESIAN_POINT('Ctrl Pts',(-9.72580603199727,-38.274235605455,3.35069795220807));
#61092=CARTESIAN_POINT('Ctrl Pts',(-9.70965791715154,-38.2742356059326,
3.37062166517313));
#61093=CARTESIAN_POINT('Ctrl Pts',(-9.69327312413074,-38.2742356067395,
3.39038536076922));
#61094=CARTESIAN_POINT('Ctrl Pts',(-9.67664111106427,-38.274235607639,3.40997117451938));
#61095=CARTESIAN_POINT('Ctrl Pts',(-9.6600090979978,-38.2742356085385,3.42955698826954));
#61096=CARTESIAN_POINT('Ctrl Pts',(-9.64312794404234,-38.2742356094539,
3.44896763473112));
#61097=CARTESIAN_POINT('Ctrl Pts',(-9.62599170539255,-38.2742356102203,
3.46818060849546));
#61098=CARTESIAN_POINT('Ctrl Pts',(-9.59172981984717,-38.2742356117526,
3.50659468065872));
#61099=CARTESIAN_POINT('Ctrl Pts',(-9.55628350961246,-38.2742356123503,
3.54440198554242));
#61100=CARTESIAN_POINT('Ctrl Pts',(-9.51970351119237,-38.2742356126017,
3.58129418363479));
#61101=CARTESIAN_POINT('Ctrl Pts',(-9.4871353878986,-38.2742356128255,3.61414026641076));
#61102=CARTESIAN_POINT('Ctrl Pts',(-9.4536687089984,-38.2742356127996,3.64626067650308));
#61103=CARTESIAN_POINT('Ctrl Pts',(-9.41938694957581,-38.2742356128,3.67744527399227));
#61104=CARTESIAN_POINT('Ctrl Pts',(-9.41516398171632,-38.2742356128,3.68128672073031));
#61105=CARTESIAN_POINT('Ctrl Pts',(-9.41092870958514,-38.2742356128,3.68511398034174));
#61106=CARTESIAN_POINT('Ctrl Pts',(-9.40668134445996,-38.2742356128,3.68892667205413));
#61107=CARTESIAN_POINT('Ctrl Pts',(-9.38731105321667,-38.2742356128,3.70631461651221));
#61108=CARTESIAN_POINT('Ctrl Pts',(-9.3676655441854,-38.2742356128,3.72341953810915));
#61109=CARTESIAN_POINT('Ctrl Pts',(-9.34772272761063,-38.2742356128,3.74023552570305));
#61110=CARTESIAN_POINT('Ctrl Pts',(-9.32777991104666,-38.2742356128,3.75705151328784));
#61111=CARTESIAN_POINT('Ctrl Pts',(-9.30754898442837,-38.2742356128008,
3.77357031050439));
#61112=CARTESIAN_POINT('Ctrl Pts',(-9.2870412695087,-38.2742356127992,3.78976284024232));
#61113=CARTESIAN_POINT('Ctrl Pts',(-9.24453342509635,-38.2742356127959,
3.82332628392381));
#61114=CARTESIAN_POINT('Ctrl Pts',(-9.20083288838149,-38.2742356127424,
3.85548921994169));
#61115=CARTESIAN_POINT('Ctrl Pts',(-9.15603215791692,-38.2742356124498,
3.88604394693062));
#61116=CARTESIAN_POINT('Ctrl Pts',(-9.11383041795814,-38.2742356121741,
3.9148261259158));
#61117=CARTESIAN_POINT('Ctrl Pts',(-9.07065408929891,-38.2742356117035,
3.94218116564615));
#61118=CARTESIAN_POINT('Ctrl Pts',(-9.02661495058258,-38.2742356116231,
3.96795976616807));
#61119=CARTESIAN_POINT('Ctrl Pts',(-8.97306006550268,-38.2742356115254,
3.99930847163129));
#61120=CARTESIAN_POINT('Ctrl Pts',(-8.91820571108124,-38.2742356120678,
4.02834059887391));
#61121=CARTESIAN_POINT('Ctrl Pts',(-8.86221555378884,-38.2742356123975,
4.05487553259682));
#61122=CARTESIAN_POINT('Ctrl Pts',(-8.82327077478763,-38.2742356126268,
4.07333229677867));
#61123=CARTESIAN_POINT('Ctrl Pts',(-8.7837768881238,-38.2742356127455,4.09058175925433));
#61124=CARTESIAN_POINT('Ctrl Pts',(-8.74378271581823,-38.2742356127794,
4.10657708416326));
#61125=CARTESIAN_POINT('Ctrl Pts',(-8.69495943512302,-38.2742356128206,
4.12610353496397));
#61126=CARTESIAN_POINT('Ctrl Pts',(-8.64537775540928,-38.2742356128,4.14376462596244));
#61127=CARTESIAN_POINT('Ctrl Pts',(-8.5951696327512,-38.2742356128,4.1594740219235));
#61128=CARTESIAN_POINT('Ctrl Pts',(-8.54496151009177,-38.2742356128,4.17518341788498));
#61129=CARTESIAN_POINT('Ctrl Pts',(-8.4941169724322,-38.2742356128,4.18894526362599));
#61130=CARTESIAN_POINT('Ctrl Pts',(-8.44279988453127,-38.2742356128,4.2006885559872));
#61131=CARTESIAN_POINT('Ctrl Pts',(-8.38210007741659,-38.2742356128,4.21457896969487));
#61132=CARTESIAN_POINT('Ctrl Pts',(-8.32072862449063,-38.2742356128,4.22564662450852));
#61133=CARTESIAN_POINT('Ctrl Pts',(-8.25895938697734,-38.2742356128,4.23382180321406));
#61134=CARTESIAN_POINT('Ctrl Pts',(-8.19517547597314,-38.2742356128,4.24226362461239));
#61135=CARTESIAN_POINT('Ctrl Pts',(-8.13096964626072,-38.2742356128,4.24762123684602));
#61136=CARTESIAN_POINT('Ctrl Pts',(-8.06663542917861,-38.2742356128,4.24987419949773));
#61137=CARTESIAN_POINT('Ctrl Pts',(-8.0228271688435,-38.2742356128,4.25140835004541));
#61138=CARTESIAN_POINT('Ctrl Pts',(-7.97896315899794,-38.2742356128,4.25150389571578));
#61139=CARTESIAN_POINT('Ctrl Pts',(-7.93513432458635,-38.2742356128,4.25016834652164));
#61140=CARTESIAN_POINT('Ctrl Pts',(-7.8842940518043,-38.2742356128,4.24861914526508));
#61141=CARTESIAN_POINT('Ctrl Pts',(-7.83349885095115,-38.2742356128,4.24514493423103));
#61142=CARTESIAN_POINT('Ctrl Pts',(-7.78284834806656,-38.2742356128,4.23976656890104));
#61143=CARTESIAN_POINT('Ctrl Pts',(-7.73716457234106,-38.2742356128,4.23491559958164));
#61144=CARTESIAN_POINT('Ctrl Pts',(-7.69160498203115,-38.2742356128,4.22851414021581));
#61145=CARTESIAN_POINT('Ctrl Pts',(-7.64633824031241,-38.2742356128,4.22060655270573));
#61146=CARTESIAN_POINT('Ctrl Pts',(-7.5986399936733,-38.2742356128,4.21227420880257));
#61147=CARTESIAN_POINT('Ctrl Pts',(-7.55126746264243,-38.2742356128,4.20227103909697));
#61148=CARTESIAN_POINT('Ctrl Pts',(-7.50434329892817,-38.2742356128,4.19066324261345));
#61149=CARTESIAN_POINT('Ctrl Pts',(-7.48263553697715,-38.2742356128,4.18529331669693));
#61150=CARTESIAN_POINT('Ctrl Pts',(-7.46101470252345,-38.2742356128,4.17957805554725));
#61151=CARTESIAN_POINT('Ctrl Pts',(-7.43948853881381,-38.2742356128,4.17352310085893));
#61152=CARTESIAN_POINT('Ctrl Pts',(-7.37616575706325,-38.2742356128,4.15571144712398));
#61153=CARTESIAN_POINT('Ctrl Pts',(-7.31367164510924,-38.2742356128,4.13495923978566));
#61154=CARTESIAN_POINT('Ctrl Pts',(-7.2522425471246,-38.2742356128,4.11145109233569));
#61155=CARTESIAN_POINT('Ctrl Pts',(-7.19141311353757,-38.2742356128,4.08817242895015));
#61156=CARTESIAN_POINT('Ctrl Pts',(-7.13162842509448,-38.2742356128,4.06219174970784));
#61157=CARTESIAN_POINT('Ctrl Pts',(-7.07307992195391,-38.2742356128,4.03372160610396));
#61158=CARTESIAN_POINT('Ctrl Pts',(-7.02430271531214,-38.2742356128,4.01000291129202));
#61159=CARTESIAN_POINT('Ctrl Pts',(-6.9763829736138,-38.2742356128,3.98455703310644));
#61160=CARTESIAN_POINT('Ctrl Pts',(-6.9294076769401,-38.2742356128,3.95752201570169));
#61161=CARTESIAN_POINT('Ctrl Pts',(-6.90592002860325,-38.2742356128,3.94400450699932));
#61162=CARTESIAN_POINT('Ctrl Pts',(-6.88266813368041,-38.2742356128,3.93008991477376));
#61163=CARTESIAN_POINT('Ctrl Pts',(-6.85966059236408,-38.2742356128,3.91579662211982));
#61164=CARTESIAN_POINT('Ctrl Pts',(-6.84686917138494,-38.2742356128,3.90785003099994));
#61165=CARTESIAN_POINT('Ctrl Pts',(-6.83415325180026,-38.2742356128,3.89978639679546));
#61166=CARTESIAN_POINT('Ctrl Pts',(-6.82151409446459,-38.2742356128,3.89160896986944));
#61167=CARTESIAN_POINT('Ctrl Pts',(-6.81272250047702,-38.2742356128,3.88592088359223));
#61168=CARTESIAN_POINT('Ctrl Pts',(-6.80396727363108,-38.2742356128,3.8801772286737));
#61169=CARTESIAN_POINT('Ctrl Pts',(-6.79525123070431,-38.2742356128,3.87438074050389));
#61170=CARTESIAN_POINT('Ctrl Pts',(-6.79395950941247,-38.2742356128,3.87352169847648));
#61171=CARTESIAN_POINT('Ctrl Pts',(-6.79266874994473,-38.2742356128,3.87266156363026));
#61172=CARTESIAN_POINT('Ctrl Pts',(-6.79137909539,-38.2742356128,3.87180043587));
#61173=CARTESIAN_POINT('',(-10.7486857339,-38.2742356128,0.754197251045));
#61174=CARTESIAN_POINT('Ctrl Pts',(-10.748685733951,-38.2742356128,0.754197251052992));
#61175=CARTESIAN_POINT('Ctrl Pts',(-10.7467233592932,-38.2742356128,0.76671756222468));
#61176=CARTESIAN_POINT('Ctrl Pts',(-10.7447502486204,-38.2742356128,0.779205465261789));
#61177=CARTESIAN_POINT('Ctrl Pts',(-10.742753142554,-38.2742356128,0.791748410472544));
#61178=CARTESIAN_POINT('Ctrl Pts',(-10.7424571718059,-38.2742356128,0.793607272623299));
#61179=CARTESIAN_POINT('Ctrl Pts',(-10.7421606885948,-38.2742356128,0.795467251786625));
#61180=CARTESIAN_POINT('Ctrl Pts',(-10.7418636644767,-38.2742356128,0.797328539574165));
#61181=CARTESIAN_POINT('Ctrl Pts',(-10.7397289995216,-38.2742356128,0.810705317986936));
#61182=CARTESIAN_POINT('Ctrl Pts',(-10.7375655067097,-38.2742356128,0.824156020876981));
#61183=CARTESIAN_POINT('Ctrl Pts',(-10.7353677682444,-38.2742356127999,
0.83771928337193));
#61184=CARTESIAN_POINT('Ctrl Pts',(-10.7328906315049,-38.2742356127998,
0.85300684208891));
#61185=CARTESIAN_POINT('Ctrl Pts',(-10.7303700221984,-38.2742356127996,
0.868437268995491));
#61186=CARTESIAN_POINT('Ctrl Pts',(-10.7278087378651,-38.2742356127991,
0.883997963310959));
#61187=CARTESIAN_POINT('Ctrl Pts',(-10.7248377347222,-38.2742356127985,
0.90204784208249));
#61188=CARTESIAN_POINT('Ctrl Pts',(-10.72181220956,-38.2742356127974,0.920271904703645));
#61189=CARTESIAN_POINT('Ctrl Pts',(-10.7187482319499,-38.2742356127961,
0.938572490763118));
#61190=CARTESIAN_POINT('Ctrl Pts',(-10.7149229765464,-38.2742356127944,
0.961420051880341));
#61191=CARTESIAN_POINT('Ctrl Pts',(-10.7110388540621,-38.2742356127923,
0.984380955081967));
#61192=CARTESIAN_POINT('Ctrl Pts',(-10.7071345609069,-38.2742356127909,
1.00720366640169));
#61193=CARTESIAN_POINT('Ctrl Pts',(-10.7042498808607,-38.27423561279,1.02406618602461));
#61194=CARTESIAN_POINT('Ctrl Pts',(-10.7013545207682,-38.2742356127895,
1.0408508782088));
#61195=CARTESIAN_POINT('Ctrl Pts',(-10.6984588552136,-38.27423561279,1.05748168729192));
#61196=CARTESIAN_POINT('Ctrl Pts',(-10.6958462069106,-38.2742356127904,
1.07248703038407));
#61197=CARTESIAN_POINT('Ctrl Pts',(-10.6932334434059,-38.2742356127916,
1.08736621956575));
#61198=CARTESIAN_POINT('Ctrl Pts',(-10.6906206945055,-38.2742356127934,
1.10210512196072));
#61199=CARTESIAN_POINT('Ctrl Pts',(-10.6882215637706,-38.274235612795,1.11563897273773));
#61200=CARTESIAN_POINT('Ctrl Pts',(-10.6858224949344,-38.2742356127971,
1.12905419587582));
#61201=CARTESIAN_POINT('Ctrl Pts',(-10.6834157727329,-38.2742356127986,
1.1423847022234));
#61202=CARTESIAN_POINT('Ctrl Pts',(-10.6828674279457,-38.2742356127989,
1.14542190928546));
#61203=CARTESIAN_POINT('Ctrl Pts',(-10.6823186498546,-38.2742356127992,
1.14845492720555));
#61204=CARTESIAN_POINT('Ctrl Pts',(-10.6817692804452,-38.2742356127994,
1.15148454459705));
#61205=CARTESIAN_POINT('Ctrl Pts',(-10.6795353563807,-38.2742356128004,
1.16380400593097));
#61206=CARTESIAN_POINT('Ctrl Pts',(-10.6772801001843,-38.2742356128,1.17613331617475));
#61207=CARTESIAN_POINT('Ctrl Pts',(-10.6750013200392,-38.2742356128,1.18847758722424));
#61208=CARTESIAN_POINT('Ctrl Pts',(-10.6746215084719,-38.2742356128,1.19053504631933));
#61209=CARTESIAN_POINT('Ctrl Pts',(-10.6742410257375,-38.2742356128,1.19259303749411));
#61210=CARTESIAN_POINT('Ctrl Pts',(-10.6738598407567,-38.2742356128,1.19465172326413));
#61211=CARTESIAN_POINT('Ctrl Pts',(-10.6710364362196,-38.2742356128,1.20990023261282));
#61212=CARTESIAN_POINT('Ctrl Pts',(-10.6681670600522,-38.2742356128,1.22522670900423));
#61213=CARTESIAN_POINT('Ctrl Pts',(-10.6652585665919,-38.2742356128,1.24056634443058));
#61214=CARTESIAN_POINT('Ctrl Pts',(-10.6620395305332,-38.2742356128,1.25754380724367));
#61215=CARTESIAN_POINT('Ctrl Pts',(-10.6587724492008,-38.2742356128,1.27453816301365));
#61216=CARTESIAN_POINT('Ctrl Pts',(-10.6554555858017,-38.2742356128,1.29152616786436));
#61217=CARTESIAN_POINT('Ctrl Pts',(-10.6511604363153,-38.2742356128,1.31352466811263));
#61218=CARTESIAN_POINT('Ctrl Pts',(-10.646781470819,-38.2742356128,1.33551458505531));
#61219=CARTESIAN_POINT('Ctrl Pts',(-10.6423001074962,-38.2742356128,1.3575313458063));
#61220=CARTESIAN_POINT('Ctrl Pts',(-10.6384602262308,-38.2742356128,1.37639653058204));
#61221=CARTESIAN_POINT('Ctrl Pts',(-10.6345444130273,-38.2742356128,1.39528583945895));
#61222=CARTESIAN_POINT('Ctrl Pts',(-10.6305412850362,-38.2742356128,1.41421856465516));
#61223=CARTESIAN_POINT('Ctrl Pts',(-10.6276006111313,-38.2742356128,1.42812643146691));
#61224=CARTESIAN_POINT('Ctrl Pts',(-10.6246127952894,-38.2742356128,1.44205784892357));
#61225=CARTESIAN_POINT('Ctrl Pts',(-10.6215764121983,-38.2742356128,1.45600181465977));
#61226=CARTESIAN_POINT('Ctrl Pts',(-10.6122522885066,-38.2742356128,1.49882093773288));
#61227=CARTESIAN_POINT('Ctrl Pts',(-10.6024753861189,-38.2742356127986,
1.54173415070471));
#61228=CARTESIAN_POINT('Ctrl Pts',(-10.5921655850875,-38.2742356127461,
1.58468657520376));
#61229=CARTESIAN_POINT('Ctrl Pts',(-10.588366873773,-38.2742356127268,1.60051266733034));
#61230=CARTESIAN_POINT('Ctrl Pts',(-10.5844959048361,-38.2742356127021,
1.61634467614605));
#61231=CARTESIAN_POINT('Ctrl Pts',(-10.5805488316998,-38.2742356126787,
1.63218139868328));
#61232=CARTESIAN_POINT('Ctrl Pts',(-10.5673420237974,-38.2742356126001,
1.68517067583315));
#61233=CARTESIAN_POINT('Ctrl Pts',(-10.5532662440154,-38.2742356127979,
1.73824876968933));
#61234=CARTESIAN_POINT('Ctrl Pts',(-10.5381979081127,-38.2742356127998,
1.79134448248764));
#61235=CARTESIAN_POINT('Ctrl Pts',(-10.5365404194269,-38.2742356128,1.79718491130464));
#61236=CARTESIAN_POINT('Ctrl Pts',(-10.534870891996,-38.2742356128,1.80302550347159));
#61237=CARTESIAN_POINT('Ctrl Pts',(-10.5331891355497,-38.2742356128,1.8088661121043));
#61238=CARTESIAN_POINT('Ctrl Pts',(-10.5223070013948,-38.2742356128,1.84665891309219));
#61239=CARTESIAN_POINT('Ctrl Pts',(-10.5109029235634,-38.2742356128,1.88447164217536));
#61240=CARTESIAN_POINT('Ctrl Pts',(-10.4989800247135,-38.2742356128,1.9221950930079));
#61241=CARTESIAN_POINT('Ctrl Pts',(-10.4853933388155,-38.2742356128,1.96518268217577));
#61242=CARTESIAN_POINT('Ctrl Pts',(-10.4711323192743,-38.2742356128,2.00805437618363));
#61243=CARTESIAN_POINT('Ctrl Pts',(-10.456177188935,-38.2742356128,2.05071523903541));
#61244=CARTESIAN_POINT('Ctrl Pts',(-10.4401159541856,-38.2742356128,2.09653136482825));
#61245=CARTESIAN_POINT('Ctrl Pts',(-10.4232523167762,-38.2742356128,2.142106292031));
#61246=CARTESIAN_POINT('Ctrl Pts',(-10.405554623622,-38.2742356128,2.18737956628733));
#61247=CARTESIAN_POINT('Ctrl Pts',(-10.386182665736,-38.2742356128,2.23693585334798));
#61248=CARTESIAN_POINT('Ctrl Pts',(-10.3658081590339,-38.2742356128,2.2861351960916));
#61249=CARTESIAN_POINT('Ctrl Pts',(-10.3444057568216,-38.2742356128,2.33495675618703));
#61250=CARTESIAN_POINT('Ctrl Pts',(-10.3267437697895,-38.2742356128,2.37524596076966));
#61251=CARTESIAN_POINT('Ctrl Pts',(-10.308380690975,-38.2742356128292,2.4152812514512));
#61252=CARTESIAN_POINT('Ctrl Pts',(-10.2893404343762,-38.2742356127708,
2.45504116755052));
#61253=CARTESIAN_POINT('Ctrl Pts',(-10.281341785723,-38.2742356127462,2.47174396762627));
#61254=CARTESIAN_POINT('Ctrl Pts',(-10.2732241195849,-38.2742356127022,
2.48839790173856));
#61255=CARTESIAN_POINT('Ctrl Pts',(-10.2649916475408,-38.2742356125604,
2.50499979826043));
#61256=CARTESIAN_POINT('Ctrl Pts',(-10.2479974939845,-38.2742356122679,
2.53927081397805));
#61257=CARTESIAN_POINT('Ctrl Pts',(-10.2305030891973,-38.2742356119712,
2.5733197530435));
#61258=CARTESIAN_POINT('Ctrl Pts',(-10.2125691285345,-38.274235611949,2.60709854992017));
#61259=CARTESIAN_POINT('Ctrl Pts',(-10.1954390335978,-38.2742356119277,
2.63936325754504));
#61260=CARTESIAN_POINT('Ctrl Pts',(-10.1779076823657,-38.2742356121028,
2.67138189744662));
#61261=CARTESIAN_POINT('Ctrl Pts',(-10.1600624624965,-38.27423561229,2.703082197551));
#61262=CARTESIAN_POINT('Ctrl Pts',(-10.1431808811642,-38.2742356124672,
2.73307068737573));
#61263=CARTESIAN_POINT('Ctrl Pts',(-10.1260183450808,-38.2742356126392,
2.7627744857011));
#61264=CARTESIAN_POINT('Ctrl Pts',(-10.1086823197939,-38.2742356127228,
2.79210055954277));
#61265=CARTESIAN_POINT('Ctrl Pts',(-10.0979357011284,-38.2742356127746,
2.8102798207816));
#61266=CARTESIAN_POINT('Ctrl Pts',(-10.0871230781097,-38.2742356127961,
2.82831329245778));
#61267=CARTESIAN_POINT('Ctrl Pts',(-10.0762772719591,-38.2742356127995,
2.846171629031));
#61268=CARTESIAN_POINT('Ctrl Pts',(-10.0740935067996,-38.2742356128001,
2.84976734268047));
#61269=CARTESIAN_POINT('Ctrl Pts',(-10.0719070834333,-38.2742356128,2.85335838651667));
#61270=CARTESIAN_POINT('Ctrl Pts',(-10.0697223221,-38.2742356128,2.85693798735));
#61271=CARTESIAN_POINT('',(-1.34538288120071,-38.2742356128,-9.83573535821205));
#61272=CARTESIAN_POINT('Ctrl Pts',(-1.34538313247,-38.2742356128,-9.83573533307));
#61273=CARTESIAN_POINT('Ctrl Pts',(-1.36959257784029,-38.2742356128,-9.83234472937659));
#61274=CARTESIAN_POINT('Ctrl Pts',(-1.39358213876267,-38.2742356128,-9.82897090867581));
#61275=CARTESIAN_POINT('Ctrl Pts',(-1.41743559841733,-38.2742356128,-9.82559963885233));
#61276=CARTESIAN_POINT('Ctrl Pts',(-1.44325409530112,-38.2742356128,-9.82195064534396));
#61277=CARTESIAN_POINT('Ctrl Pts',(-1.46891304898785,-38.2742356128,-9.81830465474449));
#61278=CARTESIAN_POINT('Ctrl Pts',(-1.49445697405912,-38.2742356128,-9.81465207203634));
#61279=CARTESIAN_POINT('Ctrl Pts',(-1.52191069053112,-38.2742356128,-9.81072640400451));
#61280=CARTESIAN_POINT('Ctrl Pts',(-1.54923100158245,-38.2742356128,-9.80679319694156));
#61281=CARTESIAN_POINT('Ctrl Pts',(-1.57640956213349,-38.2742356128,-9.80284921566262));
#61282=CARTESIAN_POINT('Ctrl Pts',(-1.6070765377458,-38.2742356128,-9.79839901759309));
#61283=CARTESIAN_POINT('Ctrl Pts',(-1.63756215570723,-38.2742356128,-9.79393522891224));
#61284=CARTESIAN_POINT('Ctrl Pts',(-1.6677866639062,-38.2742356128,-9.78946237139186));
#61285=CARTESIAN_POINT('Ctrl Pts',(-1.71351404398834,-38.2742356128,-9.78269527845716));
#61286=CARTESIAN_POINT('Ctrl Pts',(-1.75863901101848,-38.2742356128,-9.77590814500956));
#61287=CARTESIAN_POINT('Ctrl Pts',(-1.8027616949637,-38.2742356128,-9.76913273533593));
#61288=CARTESIAN_POINT('Ctrl Pts',(-1.83164853545357,-38.2742356128,-9.76469691772478));
#61289=CARTESIAN_POINT('Ctrl Pts',(-1.86010274514465,-38.2742356128,-9.76026651943909));
#61290=CARTESIAN_POINT('Ctrl Pts',(-1.88803424909477,-38.2742356128,-9.75584709271156));
#61291=CARTESIAN_POINT('Ctrl Pts',(-1.90276621750807,-38.2742356128,-9.75351614572527));
#61292=CARTESIAN_POINT('Ctrl Pts',(-1.91735339380267,-38.2742356128,-9.75118816150423));
#61293=CARTESIAN_POINT('Ctrl Pts',(-1.93178873575302,-38.2742356128,-9.74886307273491));
#61294=CARTESIAN_POINT('Ctrl Pts',(-1.9542416630588,-38.2742356128,-9.74524659802329));
#61295=CARTESIAN_POINT('Ctrl Pts',(-1.97633365589926,-38.2742356128,-9.74163600882343));
#61296=CARTESIAN_POINT('Ctrl Pts',(-1.99822346015992,-38.2742356128,-9.73800258624781));
#61297=CARTESIAN_POINT('Ctrl Pts',(-2.02071725826659,-38.2742356128,-9.73426890855571));
#61298=CARTESIAN_POINT('Ctrl Pts',(-2.04299696927202,-38.2742356128,-9.73051122797212));
#61299=CARTESIAN_POINT('Ctrl Pts',(-2.06517301875635,-38.2742356128,-9.72670961912013));
#61300=CARTESIAN_POINT('Ctrl Pts',(-2.08884787124812,-38.2742356128,-9.72265107258477));
#61301=CARTESIAN_POINT('Ctrl Pts',(-2.1124040946237,-38.2742356128,-9.71854254870478));
#61302=CARTESIAN_POINT('Ctrl Pts',(-2.13591439660367,-38.2742356128,-9.71437098329188));
#61303=CARTESIAN_POINT('Ctrl Pts',(-2.1619581216413,-38.2742356128,-9.70974989834442));
#61304=CARTESIAN_POINT('Ctrl Pts',(-2.1879447425657,-38.2742356128,-9.70505159407837));
#61305=CARTESIAN_POINT('Ctrl Pts',(-2.21390903684172,-38.2742356128,-9.70026987667837));
#61306=CARTESIAN_POINT('Ctrl Pts',(-2.25014620370348,-38.2742356128,-9.69359625445443));
#61307=CARTESIAN_POINT('Ctrl Pts',(-2.28633804663903,-38.2742356128,-9.68676051999743));
#61308=CARTESIAN_POINT('Ctrl Pts',(-2.32247055514705,-38.2742356128,-9.67976513651878));
#61309=CARTESIAN_POINT('Ctrl Pts',(-2.35165394779118,-38.2742356128,-9.67411512684098));
#61310=CARTESIAN_POINT('Ctrl Pts',(-2.38079361486408,-38.2742356128,-9.66836187808848));
#61311=CARTESIAN_POINT('Ctrl Pts',(-2.40988939653965,-38.2742356128,-9.66250503837571));
#61312=CARTESIAN_POINT('Ctrl Pts',(-2.4225086275498,-38.2742356128,-9.65996484838703));
#61313=CARTESIAN_POINT('Ctrl Pts',(-2.43512007479769,-38.2742356128,-9.65740508209448));
#61314=CARTESIAN_POINT('Ctrl Pts',(-2.44772709713684,-38.2742356128,-9.65482507591868));
#61315=CARTESIAN_POINT('Ctrl Pts',(-2.56020547209503,-38.2742356128,-9.63180656336037));
#61316=CARTESIAN_POINT('Ctrl Pts',(-2.67234639159194,-38.2742356128,-9.6071728357461));
#61317=CARTESIAN_POINT('Ctrl Pts',(-2.78403077108086,-38.2742356128,-9.58090883358199));
#61318=CARTESIAN_POINT('Ctrl Pts',(-2.9120337603626,-38.2742356128,-9.55080730279592));
#61319=CARTESIAN_POINT('Ctrl Pts',(-3.03943743362999,-38.2742356128,-9.51856418783258));
#61320=CARTESIAN_POINT('Ctrl Pts',(-3.16613185998554,-38.2742356128,-9.48416597085791));
#61321=CARTESIAN_POINT('Ctrl Pts',(-3.33071450491481,-38.2742356128,-9.43948089911959));
#61322=CARTESIAN_POINT('Ctrl Pts',(-3.49410236255372,-38.2742356128,-9.39115857075402));
#61323=CARTESIAN_POINT('Ctrl Pts',(-3.65615113873269,-38.2742356128,-9.33918912043045));
#61324=CARTESIAN_POINT('Ctrl Pts',(-3.7213143204076,-38.2742356128,-9.31829112408125));
#61325=CARTESIAN_POINT('Ctrl Pts',(-3.78626160561947,-38.2742356128,-9.29680360387223));
#61326=CARTESIAN_POINT('Ctrl Pts',(-3.85098428964021,-38.2742356128,-9.27472670369517));
#61327=CARTESIAN_POINT('Ctrl Pts',(-3.95865102485678,-38.2742356128,-9.23800159252698));
#61328=CARTESIAN_POINT('Ctrl Pts',(-4.06569998469652,-38.2742356128,-9.1996429145904));
#61329=CARTESIAN_POINT('Ctrl Pts',(-4.17210492639527,-38.2742356128,-9.15965461239092));
#61330=CARTESIAN_POINT('Ctrl Pts',(-4.31210622633393,-38.2742356128,-9.10704038037415));
#61331=CARTESIAN_POINT('Ctrl Pts',(-4.45098794296568,-38.2742356128,-9.05160623665064));
#61332=CARTESIAN_POINT('Ctrl Pts',(-4.58863476770087,-38.2742356128,-8.99341240511538));
#61333=CARTESIAN_POINT('Ctrl Pts',(-4.6795968534866,-38.2742356128,-8.95495578029679));
#61334=CARTESIAN_POINT('Ctrl Pts',(-4.77001840222156,-38.2742356128,-8.91529515967408));
#61335=CARTESIAN_POINT('Ctrl Pts',(-4.85988107462834,-38.2742356128,-8.87444749686709));
#61336=CARTESIAN_POINT('Ctrl Pts',(-5.02694237423458,-38.2742356128,-8.79850869545327));
#61337=CARTESIAN_POINT('Ctrl Pts',(-5.19207696240372,-38.2742356128,-8.71846212306564));
#61338=CARTESIAN_POINT('Ctrl Pts',(-5.35517439119676,-38.2742356128,-8.6344774086833));
#61339=CARTESIAN_POINT('Ctrl Pts',(-5.49157233846693,-38.2742356128,-8.56424121471878));
#61340=CARTESIAN_POINT('Ctrl Pts',(-5.62654463760369,-38.2742356128,-8.49125208831812));
#61341=CARTESIAN_POINT('Ctrl Pts',(-5.76006044505498,-38.2742356128,-8.41562097191507));
#61342=CARTESIAN_POINT('Ctrl Pts',(-5.88434039844082,-38.2742356128,-8.34522158025862));
#61343=CARTESIAN_POINT('Ctrl Pts',(-6.00735775169599,-38.2742356128,-8.27253364803918));
#61344=CARTESIAN_POINT('Ctrl Pts',(-6.12912965309513,-38.2742356128,-8.19764585212784));
#61345=CARTESIAN_POINT('Ctrl Pts',(-6.24138886497924,-38.2742356128,-8.12860821001047));
#61346=CARTESIAN_POINT('Ctrl Pts',(-6.35258942208878,-38.2742356128,-8.05770128566654));
#61347=CARTESIAN_POINT('Ctrl Pts',(-6.46278702258669,-38.2742356128,-7.98498804904817));
#61348=CARTESIAN_POINT('Ctrl Pts',(-6.56530437260463,-38.2742356128,-7.91734258040219));
#61349=CARTESIAN_POINT('Ctrl Pts',(-6.66695365169245,-38.2742356128,-7.84813396875634));
#61350=CARTESIAN_POINT('Ctrl Pts',(-6.76781933890444,-38.2742356128,-7.7774039677487));
#61351=CARTESIAN_POINT('Ctrl Pts',(-6.85248887582691,-38.2742356128,-7.71803118600919));
#61352=CARTESIAN_POINT('Ctrl Pts',(-6.93661315853148,-38.2742356128,-7.65758405631927));
#61353=CARTESIAN_POINT('Ctrl Pts',(-7.02025404496547,-38.2742356128,-7.59605079899767));
#61354=CARTESIAN_POINT('Ctrl Pts',(-7.10707098904692,-38.2742356128,-7.53218096705544));
#61355=CARTESIAN_POINT('Ctrl Pts',(-7.19336693513277,-38.2742356128,-7.46714123578346));
#61356=CARTESIAN_POINT('Ctrl Pts',(-7.2791559123188,-38.2742356128,-7.40093769788929));
#61357=CARTESIAN_POINT('Ctrl Pts',(-7.36884947222418,-38.2742356128,-7.33172098512697));
#61358=CARTESIAN_POINT('Ctrl Pts',(-7.45798861557288,-38.2742356128,-7.26123249546362));
#61359=CARTESIAN_POINT('Ctrl Pts',(-7.5465335522818,-38.2742356128,-7.18949473649223));
#61360=CARTESIAN_POINT('Ctrl Pts',(-7.64317344207319,-38.2742356128,-7.11119856983884));
#61361=CARTESIAN_POINT('Ctrl Pts',(-7.73910544090864,-38.2742356128,-7.03141483703542));
#61362=CARTESIAN_POINT('Ctrl Pts',(-7.83421469437285,-38.2742356128,-6.95018353462036));
#61363=CARTESIAN_POINT('Ctrl Pts',(-7.93533493965101,-38.2742356128,-6.86381833959162));
#61364=CARTESIAN_POINT('Ctrl Pts',(-8.03552442437534,-38.2742356128,-6.77581783862214));
#61365=CARTESIAN_POINT('Ctrl Pts',(-8.13458343720895,-38.2742356128,-6.68622895146722));
#61366=CARTESIAN_POINT('Ctrl Pts',(-8.24082633690025,-38.2742356128,-6.59014296313374));
#61367=CARTESIAN_POINT('Ctrl Pts',(-8.34576756691707,-38.2742356128,-6.4922315231506));
#61368=CARTESIAN_POINT('Ctrl Pts',(-8.44910778731491,-38.2742356128,-6.39252971936197));
#61369=CARTESIAN_POINT('Ctrl Pts',(-8.47511576604178,-38.2742356128,-6.36743743310612));
#61370=CARTESIAN_POINT('Ctrl Pts',(-8.50102215119995,-38.2742356128,-6.34223156598619));
#61371=CARTESIAN_POINT('Ctrl Pts',(-8.52682186017411,-38.2742356128,-6.31691226462336));
#61372=CARTESIAN_POINT('Ctrl Pts',(-8.60961626803044,-38.2742356128,-6.23565954329336));
#61373=CARTESIAN_POINT('Ctrl Pts',(-8.69131691175532,-38.2742356128,-6.15323856599964));
#61374=CARTESIAN_POINT('Ctrl Pts',(-8.77180401686034,-38.2742356128,-6.06959560014329));
#61375=CARTESIAN_POINT('Ctrl Pts',(-8.85668253824117,-38.2742356128,-5.98138903268718));
#61376=CARTESIAN_POINT('Ctrl Pts',(-8.94021107931082,-38.2742356128,-5.89182312662737));
#61377=CARTESIAN_POINT('Ctrl Pts',(-9.02218699302706,-38.2742356128,-5.80083647024894));
#61378=CARTESIAN_POINT('Ctrl Pts',(-9.10978693087572,-38.2742356128,-5.70360760042021));
#61379=CARTESIAN_POINT('Ctrl Pts',(-9.19561326069119,-38.2742356128,-5.60475576571228));
#61380=CARTESIAN_POINT('Ctrl Pts',(-9.27935754613207,-38.2742356128,-5.50421539201818));
#61381=CARTESIAN_POINT('Ctrl Pts',(-9.37333346090317,-38.2742356128,-5.39139129256366));
#61382=CARTESIAN_POINT('Ctrl Pts',(-9.46468648696409,-38.2742356128,-5.27643956006855));
#61383=CARTESIAN_POINT('Ctrl Pts',(-9.55291854354469,-38.2742356128,-5.15929424499621));
#61384=CARTESIAN_POINT('Ctrl Pts',(-9.64137851939688,-38.2742356128,-5.04184632250526));
#61385=CARTESIAN_POINT('Ctrl Pts',(-9.72669884147059,-38.2742356128,-4.92219249370742));
#61386=CARTESIAN_POINT('Ctrl Pts',(-9.80834822171838,-38.2742356128,-4.80030871896846));
#61387=CARTESIAN_POINT('Ctrl Pts',(-9.88177596113607,-38.2742356128,-4.69069796597051));
#61388=CARTESIAN_POINT('Ctrl Pts',(-9.95223315159215,-38.2742356128,-4.57928380474877));
#61389=CARTESIAN_POINT('Ctrl Pts',(-10.0193388107923,-38.2742356128,-4.4660877450883));
#61390=CARTESIAN_POINT('Ctrl Pts',(-10.0741971857383,-38.2742356128,-4.37355081217879));
#61391=CARTESIAN_POINT('Ctrl Pts',(-10.1268155003064,-38.2742356128,-4.27982359904656));
#61392=CARTESIAN_POINT('Ctrl Pts',(-10.1769991523961,-38.2742356128,-4.18494031390587));
#61393=CARTESIAN_POINT('Ctrl Pts',(-10.2227626539552,-38.2742356128,-4.0984143002212));
#61394=CARTESIAN_POINT('Ctrl Pts',(-10.2665046430741,-38.2742356128,-4.01092417744194));
#61395=CARTESIAN_POINT('Ctrl Pts',(-10.30814198582,-38.2742356128,-3.92251508690199));
#61396=CARTESIAN_POINT('Ctrl Pts',(-10.35470936117,-38.2742356128,-3.82363799648239));
#61397=CARTESIAN_POINT('Ctrl Pts',(-10.3986412352236,-38.2742356128,-3.72361213751219));
#61398=CARTESIAN_POINT('Ctrl Pts',(-10.4398160136821,-38.2742356128,-3.62255987753841));
#61399=CARTESIAN_POINT('Ctrl Pts',(-10.477385766401,-38.2742356128,-3.53035516968021));
#61400=CARTESIAN_POINT('Ctrl Pts',(-10.5126579933682,-38.2742356128,-3.43729780988155));
#61401=CARTESIAN_POINT('Ctrl Pts',(-10.5455730499076,-38.2742356128,-3.34350507155265));
#61402=CARTESIAN_POINT('Ctrl Pts',(-10.5745613901557,-38.2742356128,-3.26090166456049));
#61403=CARTESIAN_POINT('Ctrl Pts',(-10.6017209066368,-38.2742356128,-3.17772876645298));
#61404=CARTESIAN_POINT('Ctrl Pts',(-10.6270526045767,-38.2742356128,-3.09406894779799));
#61405=CARTESIAN_POINT('Ctrl Pts',(-10.6356138257324,-38.2742356128,-3.06579487745959));
#61406=CARTESIAN_POINT('Ctrl Pts',(-10.6439666896209,-38.2742356128,-3.03746516058653));
#61407=CARTESIAN_POINT('Ctrl Pts',(-10.652112636549,-38.2742356128,-3.00908281936168));
#61408=CARTESIAN_POINT('Ctrl Pts',(-10.6798118244882,-38.2742356128,-2.91257251666922));
#61409=CARTESIAN_POINT('Ctrl Pts',(-10.7051257417243,-38.2742356131574,
-2.81545484897836));
#61410=CARTESIAN_POINT('Ctrl Pts',(-10.7280634120543,-38.2742356113512,
-2.71781791747719));
#61411=CARTESIAN_POINT('Ctrl Pts',(-10.7519843914305,-38.2742356094676,
-2.61599541365775));
#61412=CARTESIAN_POINT('Ctrl Pts',(-10.7733212964808,-38.2742356048073,
-2.51360839689941));
#61413=CARTESIAN_POINT('Ctrl Pts',(-10.7921397632951,-38.2742355939441,
-2.41077097878834));
#61414=CARTESIAN_POINT('Ctrl Pts',(-10.8125905501039,-38.2742355821387,
-2.29901340924145));
#61415=CARTESIAN_POINT('Ctrl Pts',(-10.8300671649845,-38.2742355626624,
-2.18672421827063));
#61416=CARTESIAN_POINT('Ctrl Pts',(-10.8447154334301,-38.2742355369699,
-2.07406220155496));
#61417=CARTESIAN_POINT('Ctrl Pts',(-10.860404624582,-38.2742355094516,-1.95339429310082));
#61418=CARTESIAN_POINT('Ctrl Pts',(-10.8728498863203,-38.2742354748395,
-1.83229930406024));
#61419=CARTESIAN_POINT('Ctrl Pts',(-10.8822918719481,-38.2742354444275,
-1.71097854711714));
#61420=CARTESIAN_POINT('Ctrl Pts',(-10.8925246339109,-38.2742354114683,
-1.57949704779296));
#61421=CARTESIAN_POINT('Ctrl Pts',(-10.8992312908214,-38.2742353844433,
-1.4477514764851));
#61422=CARTESIAN_POINT('Ctrl Pts',(-10.902772559254,-38.2742353812247,-1.31599141604773));
#61423=CARTESIAN_POINT('Ctrl Pts',(-10.9065651862778,-38.2742353777777,
-1.1748790504173));
#61424=CARTESIAN_POINT('Ctrl Pts',(-10.9066994914357,-38.2742354430818,
-1.03372140575963));
#61425=CARTESIAN_POINT('Ctrl Pts',(-10.9036908051778,-38.2742354987534,
-0.892752944805049));
#61426=CARTESIAN_POINT('Ctrl Pts',(-10.9010418512978,-38.2742355477687,
-0.76863932192075));
#61427=CARTESIAN_POINT('Ctrl Pts',(-10.8959582328936,-38.274235585137,-0.644672308720675));
#61428=CARTESIAN_POINT('Ctrl Pts',(-10.8887788880352,-38.2742355999926,
-0.520973121180266));
#61429=CARTESIAN_POINT('Ctrl Pts',(-10.8866544720092,-38.2742356043884,
-0.484369706578729));
#61430=CARTESIAN_POINT('Ctrl Pts',(-10.8843463777221,-38.2742356072249,
-0.447789460145407));
#61431=CARTESIAN_POINT('Ctrl Pts',(-10.8818628486602,-38.2742356090502,
-0.411234766122649));
#61432=CARTESIAN_POINT('Ctrl Pts',(-10.874153398296,-38.2742356147162,-0.297760515520062));
#61433=CARTESIAN_POINT('Ctrl Pts',(-10.8647666322912,-38.2742356127942,
-0.184597665520344));
#61434=CARTESIAN_POINT('Ctrl Pts',(-10.8539025069105,-38.2742356127992,
-0.0718960390738849));
#61435=CARTESIAN_POINT('Ctrl Pts',(-10.8503866394393,-38.2742356128008,
-0.0354233393866784));
#61436=CARTESIAN_POINT('Ctrl Pts',(-10.8467158042603,-38.2742356128,0.00100136055282495));
#61437=CARTESIAN_POINT('Ctrl Pts',(-10.8428959742023,-38.2742356128,0.0373739107865892));
#61438=CARTESIAN_POINT('Ctrl Pts',(-10.8325161134709,-38.2742356128,0.136211293637533));
#61439=CARTESIAN_POINT('Ctrl Pts',(-10.8210390244351,-38.2742356127994,
0.23467135316527));
#61440=CARTESIAN_POINT('Ctrl Pts',(-10.8085583220161,-38.2742356127967,
0.332816547392836));
#61441=CARTESIAN_POINT('Ctrl Pts',(-10.8022537424958,-38.2742356127953,
0.38239422024847));
#61442=CARTESIAN_POINT('Ctrl Pts',(-10.7956924176571,-38.2742356127937,
0.431891974651008));
#61443=CARTESIAN_POINT('Ctrl Pts',(-10.7888821093176,-38.2742356127936,
0.481320658221345));
#61444=CARTESIAN_POINT('Ctrl Pts',(-10.776316920979,-38.2742356127932,0.572517809279948));
#61445=CARTESIAN_POINT('Ctrl Pts',(-10.7629084439009,-38.2742356128,0.663453825543477));
#61446=CARTESIAN_POINT('Ctrl Pts',(-10.7486857339,-38.2742356128,0.754197251045));
#61447=CARTESIAN_POINT('',(1.34539004473266,-38.2742356128,-9.83573437512944));
#61448=CARTESIAN_POINT('Origin',(-0.000586909216232778,-38.2742356128,-2.71382866332907));
#61449=CARTESIAN_POINT('Ctrl Pts',(10.7486858853,-38.2742356128,0.754196294519999));
#61450=CARTESIAN_POINT('Ctrl Pts',(10.7487507681651,-38.2742356128,0.75378232052338));
#61451=CARTESIAN_POINT('Ctrl Pts',(10.7488160123459,-38.2742356128,0.753365938766182));
#61452=CARTESIAN_POINT('Ctrl Pts',(10.7488811261052,-38.2742356128,0.752950275000361));
#61453=CARTESIAN_POINT('Ctrl Pts',(10.7635805210417,-38.2742356128,0.659114411071533));
#61454=CARTESIAN_POINT('Ctrl Pts',(10.7774074937196,-38.2742356128009,0.565058978147053));
#61455=CARTESIAN_POINT('Ctrl Pts',(10.7903335869119,-38.2742356127991,0.47072184452806));
#61456=CARTESIAN_POINT('Ctrl Pts',(10.8036736449597,-38.2742356127974,0.373363515154428));
#61457=CARTESIAN_POINT('Ctrl Pts',(10.816053894268,-38.2742356128009,0.275705290202299));
#61458=CARTESIAN_POINT('Ctrl Pts',(10.8273976278922,-38.2742356127401,0.177714287921341));
#61459=CARTESIAN_POINT('Ctrl Pts',(10.839417545248,-38.2742356126756,0.0738821821922056));
#61460=CARTESIAN_POINT('Ctrl Pts',(10.8502734645611,-38.2742356125617,-0.0303235245117267));
#61461=CARTESIAN_POINT('Ctrl Pts',(10.8598278196961,-38.2742356120064,-0.134903919694318));
#61462=CARTESIAN_POINT('Ctrl Pts',(10.865531383808,-38.274235611675,-0.197334191580115));
#61463=CARTESIAN_POINT('Ctrl Pts',(10.8707702592039,-38.2742356111793,-0.2598972685949));
#61464=CARTESIAN_POINT('Ctrl Pts',(10.8755086549781,-38.2742356103235,-0.322587644605349));
#61465=CARTESIAN_POINT('Ctrl Pts',(10.8846876179272,-38.2742356086658,-0.444028036264462));
#61466=CARTESIAN_POINT('Ctrl Pts',(10.8920102665268,-38.2742356018392,-0.565865217904973));
#61467=CARTESIAN_POINT('Ctrl Pts',(10.8971588132929,-38.2742355766501,-0.687882711279094));
#61468=CARTESIAN_POINT('Ctrl Pts',(10.8984152249802,-38.2742355705032,-0.717658920314688));
#61469=CARTESIAN_POINT('Ctrl Pts',(10.8995420735683,-38.2742355633587,-0.74744563510997));
#61470=CARTESIAN_POINT('Ctrl Pts',(10.9005346180392,-38.2742355553307,-0.777239287853531));
#61471=CARTESIAN_POINT('Ctrl Pts',(10.9050918295056,-38.2742355184706,-0.914035149284712));
#61472=CARTESIAN_POINT('Ctrl Pts',(10.9068104832314,-38.2742354680899,-1.05102520549406));
#61473=CARTESIAN_POINT('Ctrl Pts',(10.9052251807396,-38.2742354568179,-1.18807097906776));
#61474=CARTESIAN_POINT('Ctrl Pts',(10.9050503429394,-38.2742354555748,-1.20318530690122));
#61475=CARTESIAN_POINT('Ctrl Pts',(10.9048352995357,-38.2742354548037,-1.21830026518269));
#61476=CARTESIAN_POINT('Ctrl Pts',(10.9045794158392,-38.2742354545548,-1.23341563491137));
#61477=CARTESIAN_POINT('Ctrl Pts',(10.902164660392,-38.2742354522063,-1.37605825686335));
#61478=CARTESIAN_POINT('Ctrl Pts',(10.8961336835133,-38.2742354717451,-1.51874802165549));
#61479=CARTESIAN_POINT('Ctrl Pts',(10.8860165731785,-38.2742354967745,-1.66116169724552));
#61480=CARTESIAN_POINT('Ctrl Pts',(10.8777741390387,-38.274235517166,-1.77718646151313));
#61481=CARTESIAN_POINT('Ctrl Pts',(10.8668192226381,-38.2742355405236,-1.89302685111375));
#61482=CARTESIAN_POINT('Ctrl Pts',(10.8529343365985,-38.2742355593193,-2.00850492848472));
#61483=CARTESIAN_POINT('Ctrl Pts',(10.8399197629638,-38.2742355769368,-2.11674477552758));
#61484=CARTESIAN_POINT('Ctrl Pts',(10.8243304799624,-38.2742355905135,-2.22466580464906));
#61485=CARTESIAN_POINT('Ctrl Pts',(10.8060293952058,-38.274235598896,-2.33212834528309));
#61486=CARTESIAN_POINT('Ctrl Pts',(10.7889938389441,-38.2742356066989,-2.43215980141552));
#61487=CARTESIAN_POINT('Ctrl Pts',(10.7696083786317,-38.2742356101862,-2.53179372082084));
#61488=CARTESIAN_POINT('Ctrl Pts',(10.7478046429435,-38.2742356116343,-2.63092871096361));
#61489=CARTESIAN_POINT('Ctrl Pts',(10.7260009072553,-38.2742356130824,-2.73006370110638));
#61490=CARTESIAN_POINT('Ctrl Pts',(10.701778271492,-38.2742356128,-2.82869940493948));
#61491=CARTESIAN_POINT('Ctrl Pts',(10.6751186719673,-38.2742356128,-2.92675080812293));
#61492=CARTESIAN_POINT('Ctrl Pts',(10.649771284584,-38.2742356128,-3.01997602321491));
#61493=CARTESIAN_POINT('Ctrl Pts',(10.6222091430034,-38.2742356128002,-3.11268297971948));
#61494=CARTESIAN_POINT('Ctrl Pts',(10.5924125813341,-38.2742356127998,-3.20473440645213));
#61495=CARTESIAN_POINT('Ctrl Pts',(10.5615425589387,-38.2742356127993,-3.30010210814564));
#61496=CARTESIAN_POINT('Ctrl Pts',(10.5282742733662,-38.2742356128003,-3.394766254745));
#61497=CARTESIAN_POINT('Ctrl Pts',(10.492632290442,-38.2742356127837,-3.48860580498373));
#61498=CARTESIAN_POINT('Ctrl Pts',(10.4561089049894,-38.2742356127667,-3.58476594487729));
#61499=CARTESIAN_POINT('Ctrl Pts',(10.4170931618951,-38.2742356127363,-3.68006035850158));
#61500=CARTESIAN_POINT('Ctrl Pts',(10.3756573972349,-38.2742356125976,-3.77438966006884));
#61501=CARTESIAN_POINT('Ctrl Pts',(10.3325447200932,-38.2742356124533,-3.87253648460131));
#61502=CARTESIAN_POINT('Ctrl Pts',(10.2868123323073,-38.2742356122017,-3.96963864096929));
#61503=CARTESIAN_POINT('Ctrl Pts',(10.2385883089484,-38.2742356115385,-4.06561497714332));
#61504=CARTESIAN_POINT('Ctrl Pts',(10.2340891761824,-38.2742356114766,-4.07456923373088));
#61505=CARTESIAN_POINT('Ctrl Pts',(10.229568386755,-38.2742356114109,-4.08351371121035));
#61506=CARTESIAN_POINT('Ctrl Pts',(10.225026063464,-38.2742356113411,-4.09244835589245));
#61507=CARTESIAN_POINT('Ctrl Pts',(10.1732446638246,-38.2742356105449,-4.19430116937208));
#61508=CARTESIAN_POINT('Ctrl Pts',(10.1186492306826,-38.2742356100661,-4.29488069311728));
#61509=CARTESIAN_POINT('Ctrl Pts',(10.0614431398963,-38.2742356101221,-4.39413041658256));
#61510=CARTESIAN_POINT('Ctrl Pts',(9.99888850242757,-38.2742356101833,-4.50265960263433));
#61511=CARTESIAN_POINT('Ctrl Pts',(9.93321232209925,-38.2742356107809,-4.60959891059151));
#61512=CARTESIAN_POINT('Ctrl Pts',(9.86473431993858,-38.2742356113417,-4.71490795461342));
#61513=CARTESIAN_POINT('Ctrl Pts',(9.79013485868931,-38.2742356119526,-4.82963089776058));
#61514=CARTESIAN_POINT('Ctrl Pts',(9.71221083835581,-38.2742356124542,-4.94241971263403));
#61515=CARTESIAN_POINT('Ctrl Pts',(9.63143135527856,-38.2742356126467,-5.05325356687146));
#61516=CARTESIAN_POINT('Ctrl Pts',(9.5572130696955,-38.2742356128236,-5.15508510048252));
#61517=CARTESIAN_POINT('Ctrl Pts',(9.48058587434832,-38.2742356128,-5.25526742056234));
#61518=CARTESIAN_POINT('Ctrl Pts',(9.40194072919181,-38.2742356128,-5.35379594985318));
#61519=CARTESIAN_POINT('Ctrl Pts',(9.32883368845949,-38.2742356128,-5.44538620872836));
#61520=CARTESIAN_POINT('Ctrl Pts',(9.25398927525911,-38.2742356128027,-5.53553487524453));
#61521=CARTESIAN_POINT('Ctrl Pts',(9.17757104467065,-38.2742356127973,-5.62435381279997));
#61522=CARTESIAN_POINT('Ctrl Pts',(9.0897197837434,-38.274235612791,-5.72646106650603));
#61523=CARTESIAN_POINT('Ctrl Pts',(8.99979124685434,-38.2742356128188,-5.82681131345604));
#61524=CARTESIAN_POINT('Ctrl Pts',(8.90806463915596,-38.2742356125302,-5.92551716111057));
#61525=CARTESIAN_POINT('Ctrl Pts',(8.82230671692448,-38.2742356122604,-6.0178001814833));
#61526=CARTESIAN_POINT('Ctrl Pts',(8.7349530547604,-38.2742356124164,-6.10865432231495));
#61527=CARTESIAN_POINT('Ctrl Pts',(8.64624659176705,-38.2742356125934,-6.19810755671757));
#61528=CARTESIAN_POINT('Ctrl Pts',(8.56780722406295,-38.27423561275,-6.27720726274637));
#61529=CARTESIAN_POINT('Ctrl Pts',(8.48831121256558,-38.2742356127989,-6.355210827178));
#61530=CARTESIAN_POINT('Ctrl Pts',(8.40788750264759,-38.2742356127999,-6.43212465908309));
#61531=CARTESIAN_POINT('Ctrl Pts',(8.39736067259514,-38.2742356128,-6.44219207375438));
#61532=CARTESIAN_POINT('Ctrl Pts',(8.38681787544318,-38.2742356128,-6.45224080652579));
#61533=CARTESIAN_POINT('Ctrl Pts',(8.37625932979455,-38.2742356128,-6.46227086223487));
#61534=CARTESIAN_POINT('Ctrl Pts',(8.29902949041214,-38.2742356128,-6.5356350941269));
#61535=CARTESIAN_POINT('Ctrl Pts',(8.22093580705538,-38.2742356128,-6.60801769618829));
#61536=CARTESIAN_POINT('Ctrl Pts',(8.14213077435888,-38.2742356128,-6.67939428797839));
#61537=CARTESIAN_POINT('Ctrl Pts',(8.06062371227756,-38.2742356128,-6.75321820631358));
#61538=CARTESIAN_POINT('Ctrl Pts',(7.97835543517539,-38.2742356128,-6.8259660231991));
#61539=CARTESIAN_POINT('Ctrl Pts',(7.89543908612086,-38.2742356128,-6.89761648202541));
#61540=CARTESIAN_POINT('Ctrl Pts',(7.80430769103316,-38.2742356128,-6.97636580403453));
#61541=CARTESIAN_POINT('Ctrl Pts',(7.71239362383212,-38.2742356128,-7.05378962970782));
#61542=CARTESIAN_POINT('Ctrl Pts',(7.61978080920412,-38.2742356128,-7.12986536475923));
#61543=CARTESIAN_POINT('Ctrl Pts',(7.53858314384994,-38.2742356128,-7.19656425627969));
#61544=CARTESIAN_POINT('Ctrl Pts',(7.45683925660418,-38.2742356128,-7.26223284344318));
#61545=CARTESIAN_POINT('Ctrl Pts',(7.37461477413073,-38.2742356128,-7.32682367825847));
#61546=CARTESIAN_POINT('Ctrl Pts',(7.26936526560721,-38.2742356128,-7.40950165220167));
#61547=CARTESIAN_POINT('Ctrl Pts',(7.16332488578667,-38.2742356128,-7.49041743571964));
#61548=CARTESIAN_POINT('Ctrl Pts',(7.05653747020417,-38.2742356128,-7.5695101875824));
#61549=CARTESIAN_POINT('Ctrl Pts',(6.93682525271323,-38.2742356128,-7.65817577295409));
#61550=CARTESIAN_POINT('Ctrl Pts',(6.8161179135486,-38.274235612803,-7.7445940920218));
#61551=CARTESIAN_POINT('Ctrl Pts',(6.69424703684613,-38.274235612797,-7.82878929709039));
#61552=CARTESIAN_POINT('Ctrl Pts',(6.66149200838404,-38.2742356127954,-7.85141829930169));
#61553=CARTESIAN_POINT('Ctrl Pts',(6.62865265483242,-38.2742356127928,-7.87388658008447));
#61554=CARTESIAN_POINT('Ctrl Pts',(6.59572521641468,-38.2742356127876,-7.89619429227605));
#61555=CARTESIAN_POINT('Ctrl Pts',(6.45082872454463,-38.2742356127644,-7.99435890493734));
#61556=CARTESIAN_POINT('Ctrl Pts',(6.30423053627507,-38.2742356127633,-8.08940636380272));
#61557=CARTESIAN_POINT('Ctrl Pts',(6.15579746382474,-38.2742356127777,-8.18120196847487));
#61558=CARTESIAN_POINT('Ctrl Pts',(6.04282160604217,-38.2742356127887,-8.25106973451452));
#61559=CARTESIAN_POINT('Ctrl Pts',(5.92878159477683,-38.2742356127977,-8.31905327369613));
#61560=CARTESIAN_POINT('Ctrl Pts',(5.81364866406122,-38.2742356127993,-8.38507547572244));
#61561=CARTESIAN_POINT('Ctrl Pts',(5.75685723795896,-38.2742356128001,-8.41764213570564));
#61562=CARTESIAN_POINT('Ctrl Pts',(5.69980049290472,-38.2742356128,-8.44973130130719));
#61563=CARTESIAN_POINT('Ctrl Pts',(5.64247954756403,-38.2742356128,-8.48133191784778));
#61564=CARTESIAN_POINT('Ctrl Pts',(5.47394056080791,-38.2742356128,-8.57424622449373));
#61565=CARTESIAN_POINT('Ctrl Pts',(5.30310577360258,-38.2742356127314,-8.66295141982281));
#61566=CARTESIAN_POINT('Ctrl Pts',(5.13008046296484,-38.2742356120248,-8.74723786088109));
#61567=CARTESIAN_POINT('Ctrl Pts',(4.96821764570703,-38.2742356113638,-8.82608667644479));
#61568=CARTESIAN_POINT('Ctrl Pts',(4.80443919432874,-38.2742356104042,-8.90106705839819));
#61569=CARTESIAN_POINT('Ctrl Pts',(4.63886472540473,-38.2742356109888,-8.9720316944694));
#61570=CARTESIAN_POINT('Ctrl Pts',(4.48111130549067,-38.2742356115458,-9.0396442563936));
#61571=CARTESIAN_POINT('Ctrl Pts',(4.32172857521236,-38.2742356121698,-9.10362042101943));
#61572=CARTESIAN_POINT('Ctrl Pts',(4.16084936519698,-38.2742356124732,-9.16388103868563));
#61573=CARTESIAN_POINT('Ctrl Pts',(4.01162006782644,-38.2742356127547,-9.21977794191249));
#61574=CARTESIAN_POINT('Ctrl Pts',(3.86110376548713,-38.2742356127939,-9.27247759567066));
#61575=CARTESIAN_POINT('Ctrl Pts',(3.70940907605795,-38.274235612799,-9.32196250357574));
#61576=CARTESIAN_POINT('Ctrl Pts',(3.66957825401608,-38.2742356128003,-9.33495586918361));
#61577=CARTESIAN_POINT('Ctrl Pts',(3.62966617913399,-38.2742356128,-9.34772787071446));
#61578=CARTESIAN_POINT('Ctrl Pts',(3.5896747782925,-38.2742356128,-9.3602788074025));
#61579=CARTESIAN_POINT('Ctrl Pts',(3.52881041758992,-38.2742356128,-9.37938053231491));
#61580=CARTESIAN_POINT('Ctrl Pts',(3.46776633660297,-38.2742356128,-9.39796892242277));
#61581=CARTESIAN_POINT('Ctrl Pts',(3.4065727323248,-38.2742356128,-9.41604021540843));
#61582=CARTESIAN_POINT('Ctrl Pts',(3.32968048064773,-38.2742356128,-9.43874752975565));
#61583=CARTESIAN_POINT('Ctrl Pts',(3.25255020799119,-38.2742356128,-9.4606387062831));
#61584=CARTESIAN_POINT('Ctrl Pts',(3.17515279442903,-38.2742356128,-9.48172455098315));
#61585=CARTESIAN_POINT('Ctrl Pts',(3.10379770456818,-38.2742356128,-9.50116424895388));
#61586=CARTESIAN_POINT('Ctrl Pts',(3.0322103272402,-38.2742356128,-9.51992044345575));
#61587=CARTESIAN_POINT('Ctrl Pts',(2.96036414388182,-38.2742356128,-9.53800370488677));
#61588=CARTESIAN_POINT('Ctrl Pts',(2.89997433382167,-38.2742356128,-9.55320346459621));
#61589=CARTESIAN_POINT('Ctrl Pts',(2.83940025379948,-38.2742356128,-9.56792807659975));
#61590=CARTESIAN_POINT('Ctrl Pts',(2.77866084909843,-38.2742356128,-9.5821780964647));
#61591=CARTESIAN_POINT('Ctrl Pts',(2.7249273018283,-38.2742356128,-9.59478447810084));
#61592=CARTESIAN_POINT('Ctrl Pts',(2.67106397863643,-38.2742356128,-9.60701951748907));
#61593=CARTESIAN_POINT('Ctrl Pts',(2.61712385866369,-38.2742356128,-9.6188766151844));
#61594=CARTESIAN_POINT('Ctrl Pts',(2.5791100250399,-38.2742356128,-9.62723280236529));
#61595=CARTESIAN_POINT('Ctrl Pts',(2.54105881814865,-38.2742356128,-9.63540114632831));
#61596=CARTESIAN_POINT('Ctrl Pts',(2.50300436723069,-38.2742356128,-9.64337655749628));
#61597=CARTESIAN_POINT('Ctrl Pts',(2.47884007178717,-38.2742356128,-9.64844088471945));
#61598=CARTESIAN_POINT('Ctrl Pts',(2.45468813957632,-38.2742356128003,-9.65342485999044));
#61599=CARTESIAN_POINT('Ctrl Pts',(2.4304966052416,-38.2742356127983,-9.65833864391884));
#61600=CARTESIAN_POINT('Ctrl Pts',(2.40173189730255,-38.2742356127959,-9.66418133077037));
#61601=CARTESIAN_POINT('Ctrl Pts',(2.37291265402142,-38.2742356127891,-9.66992453918787));
#61602=CARTESIAN_POINT('Ctrl Pts',(2.34403422863427,-38.2742356127787,-9.67556977277591));
#61603=CARTESIAN_POINT('Ctrl Pts',(2.31516852578334,-38.2742356127683,-9.68121251932776));
#61604=CARTESIAN_POINT('Ctrl Pts',(2.28624826799992,-38.274235612755,-9.68675655791408));
#61605=CARTESIAN_POINT('Ctrl Pts',(2.25729271764595,-38.2742356127499,-9.69219828457188));
#61606=CARTESIAN_POINT('Ctrl Pts',(2.23247417729856,-38.2742356127456,-9.69686252721156));
#61607=CARTESIAN_POINT('Ctrl Pts',(2.20763015646299,-38.2742356127488,-9.70145144234736));
#61608=CARTESIAN_POINT('Ctrl Pts',(2.18277308169882,-38.2742356127574,-9.70596255728258));
#61609=CARTESIAN_POINT('Ctrl Pts',(2.16642284667288,-38.2742356127631,-9.70892983280151));
#61610=CARTESIAN_POINT('Ctrl Pts',(2.15006640220555,-38.2742356127709,-9.71186355167236));
#61611=CARTESIAN_POINT('Ctrl Pts',(2.133694660445,-38.2742356127786,-9.714765315785));
#61612=CARTESIAN_POINT('Ctrl Pts',(2.11282185420172,-38.2742356127884,-9.71846485862978));
#61613=CARTESIAN_POINT('Ctrl Pts',(2.09193075869325,-38.2742356127951,-9.7221114546842));
#61614=CARTESIAN_POINT('Ctrl Pts',(2.07096182677399,-38.2742356127978,-9.72571609201187));
#61615=CARTESIAN_POINT('Ctrl Pts',(2.05047922380141,-38.2742356128004,-9.72923712758617));
#61616=CARTESIAN_POINT('Ctrl Pts',(2.02992295383359,-38.2742356128,-9.73271802045324));
#61617=CARTESIAN_POINT('Ctrl Pts',(2.00919017821102,-38.2742356128,-9.73617746265811));
#61618=CARTESIAN_POINT('Ctrl Pts',(1.99020952480306,-38.2742356128,-9.73934454817869));
#61619=CARTESIAN_POINT('Ctrl Pts',(1.97105595139246,-38.2742356128,-9.74249735848642));
#61620=CARTESIAN_POINT('Ctrl Pts',(1.95166188100995,-38.2742356128,-9.74564856373225));
#61621=CARTESIAN_POINT('Ctrl Pts',(1.93060030650991,-38.2742356128,-9.74907070992131));
#61622=CARTESIAN_POINT('Ctrl Pts',(1.90925526880756,-38.2742356128,-9.75249094179596));
#61623=CARTESIAN_POINT('Ctrl Pts',(1.88760220884021,-38.2742356128,-9.75591654570863));
#61624=CARTESIAN_POINT('Ctrl Pts',(1.86420953953537,-38.2742356128,-9.75961736303512));
#61625=CARTESIAN_POINT('Ctrl Pts',(1.84045811266083,-38.2742356128,-9.76332434748164));
#61626=CARTESIAN_POINT('Ctrl Pts',(1.81637926323375,-38.2742356128,-9.76703763917552));
#61627=CARTESIAN_POINT('Ctrl Pts',(1.79251866984357,-38.2742356128,-9.77071727276912));
#61628=CARTESIAN_POINT('Ctrl Pts',(1.76833830132548,-38.2742356128,-9.77440285307543));
#61629=CARTESIAN_POINT('Ctrl Pts',(1.74390696076956,-38.2742356128,-9.77808886554085));
#61630=CARTESIAN_POINT('Ctrl Pts',(1.7075926768814,-38.2742356128,-9.78356768496044));
#61631=CARTESIAN_POINT('Ctrl Pts',(1.67072328673315,-38.2742356128,-9.78904774830279));
#61632=CARTESIAN_POINT('Ctrl Pts',(1.63351884074209,-38.2742356128,-9.79451085705819));
#61633=CARTESIAN_POINT('Ctrl Pts',(1.60635470047306,-38.2742356128,-9.79849964518776));
#61634=CARTESIAN_POINT('Ctrl Pts',(1.57901385029371,-38.2742356127999,-9.80247908710984));
#61635=CARTESIAN_POINT('Ctrl Pts',(1.5515482103417,-38.2742356127999,-9.80644638056753));
#61636=CARTESIAN_POINT('Ctrl Pts',(1.52760933636065,-38.2742356127999,-9.80990424786265));
#61637=CARTESIAN_POINT('Ctrl Pts',(1.50357615349941,-38.2742356127999,-9.81335280883629));
#61638=CARTESIAN_POINT('Ctrl Pts',(1.47944139357322,-38.2742356127999,-9.81679588996537));
#61639=CARTESIAN_POINT('Ctrl Pts',(1.47214765940106,-38.2742356127999,-9.81783641900173));
#61640=CARTESIAN_POINT('Ctrl Pts',(1.46484430455737,-38.2742356127999,-9.81887649496593));
#61641=CARTESIAN_POINT('Ctrl Pts',(1.45753015363098,-38.2742356127999,-9.81991635837771));
#61642=CARTESIAN_POINT('Ctrl Pts',(1.43544665144904,-38.2742356127999,-9.82305600181057));
#61643=CARTESIAN_POINT('Ctrl Pts',(1.41326877283713,-38.2742356128,-9.8261930691028));
#61644=CARTESIAN_POINT('Ctrl Pts',(1.39094458750546,-38.2742356128,-9.8293370211813));
#61645=CARTESIAN_POINT('Ctrl Pts',(1.38335731497305,-38.2742356128,-9.83040554936694));
#61646=CARTESIAN_POINT('Ctrl Pts',(1.37575271635051,-38.2742356128,-9.83147493276944));
#61647=CARTESIAN_POINT('Ctrl Pts',(1.36812735591189,-38.2742356128,-9.83254573941051));
#61648=CARTESIAN_POINT('Ctrl Pts',(1.36056853098454,-38.2742356128,-9.83360720266801));
#61649=CARTESIAN_POINT('Ctrl Pts',(1.3530001371342,-38.2742356128,-9.83466855937952));
#61650=CARTESIAN_POINT('Ctrl Pts',(1.3453969549,-38.2742356128,-9.83573340734));
#61651=CARTESIAN_POINT('',(10.3535098587966,-38.2742356128,0.692261636805038));
#61652=CARTESIAN_POINT('',(2.11953732489483,-38.2742356128,-9.3109010209371));
#61653=CARTESIAN_POINT('Ctrl Pts',(10.3535104557559,-38.2742356128,0.692257828105415));
#61654=CARTESIAN_POINT('Ctrl Pts',(10.3544069581266,-38.2742356128,0.686538032597277));
#61655=CARTESIAN_POINT('Ctrl Pts',(10.3552979558028,-38.2742356128,0.680830538803156));
#61656=CARTESIAN_POINT('Ctrl Pts',(10.3561866610052,-38.2742356128,0.675114926919618));
#61657=CARTESIAN_POINT('Ctrl Pts',(10.366268957202,-38.2742356128,0.610271723800219));
#61658=CARTESIAN_POINT('Ctrl Pts',(10.3759130539615,-38.2742356128,0.54530562811968));
#61659=CARTESIAN_POINT('Ctrl Pts',(10.3851207453064,-38.2742356128,0.480185305521681));
#61660=CARTESIAN_POINT('Ctrl Pts',(10.3977033092524,-38.2742356128,0.391196590262687));
#61661=CARTESIAN_POINT('Ctrl Pts',(10.4094717744052,-38.2742356128,0.301923984939355));
#61662=CARTESIAN_POINT('Ctrl Pts',(10.4203818846726,-38.2742356128,0.212330742444658));
#61663=CARTESIAN_POINT('Ctrl Pts',(10.4318076654474,-38.2742356128,0.118502841300599));
#61664=CARTESIAN_POINT('Ctrl Pts',(10.4422917188659,-38.2742356128,0.0243231242626569));
#61665=CARTESIAN_POINT('Ctrl Pts',(10.4517319391243,-38.2742356128,-0.0702256999872293));
#61666=CARTESIAN_POINT('Ctrl Pts',(10.4539569878336,-38.2742356128,-0.0925107456319238));
#61667=CARTESIAN_POINT('Ctrl Pts',(10.4561238455536,-38.2742356128,-0.114816186554481));
#61668=CARTESIAN_POINT('Ctrl Pts',(10.4582308198332,-38.2742356128,-0.137142046414437));
#61669=CARTESIAN_POINT('Ctrl Pts',(10.46787464667,-38.2742356128,-0.239329685132882));
#61670=CARTESIAN_POINT('Ctrl Pts',(10.4762642537817,-38.2742356128652,-0.34193688806554));
#61671=CARTESIAN_POINT('Ctrl Pts',(10.4832063794709,-38.2742356126705,-0.444942932774762));
#61672=CARTESIAN_POINT('Ctrl Pts',(10.4907263606177,-38.2742356124595,-0.556523095523347));
#61673=CARTESIAN_POINT('Ctrl Pts',(10.4965469735829,-38.2742356121524,-0.668571745847588));
#61674=CARTESIAN_POINT('Ctrl Pts',(10.5003763583156,-38.2742356088356,-0.781018782404027));
#61675=CARTESIAN_POINT('Ctrl Pts',(10.5031108430682,-38.2742356064671,-0.861314894808877));
#61676=CARTESIAN_POINT('Ctrl Pts',(10.5048289106488,-38.2742356025357,-0.941813195868945));
#61677=CARTESIAN_POINT('Ctrl Pts',(10.5054162157459,-38.2742355941479,-1.02247432568956));
#61678=CARTESIAN_POINT('Ctrl Pts',(10.506280668347,-38.2742355818018,-1.14119919937776));
#61679=CARTESIAN_POINT('Ctrl Pts',(10.5047222260127,-38.2742355702844,-1.26035174466673));
#61680=CARTESIAN_POINT('Ctrl Pts',(10.5003661398209,-38.2742355689454,-1.37976394248105));
#61681=CARTESIAN_POINT('Ctrl Pts',(10.4962520805443,-38.2742355676808,-1.49254152274945));
#61682=CARTESIAN_POINT('Ctrl Pts',(10.4896410471889,-38.2742355754336,-1.60555021006541));
#61683=CARTESIAN_POINT('Ctrl Pts',(10.480234955494,-38.274235586815,-1.71860685456706));
#61684=CARTESIAN_POINT('Ctrl Pts',(10.4768077977861,-38.2742355909618,-1.75979962231792));
#61685=CARTESIAN_POINT('Ctrl Pts',(10.4730098701887,-38.2742355954618,-1.80099837490319));
#61686=CARTESIAN_POINT('Ctrl Pts',(10.4688279746376,-38.2742355996032,-1.84219295234867));
#61687=CARTESIAN_POINT('Ctrl Pts',(10.4585921454847,-38.2742356097399,-1.94302298303868));
#61688=CARTESIAN_POINT('Ctrl Pts',(10.4460369350901,-38.2742356122915,-2.04384845382126));
#61689=CARTESIAN_POINT('Ctrl Pts',(10.4309775984689,-38.2742356126884,-2.14448461737793));
#61690=CARTESIAN_POINT('Ctrl Pts',(10.425575455875,-38.2742356128308,-2.18058520529327));
#61691=CARTESIAN_POINT('Ctrl Pts',(10.4198514676322,-38.2742356128,-2.21666117475377));
#61692=CARTESIAN_POINT('Ctrl Pts',(10.4137985541642,-38.2742356128,-2.25270313970304));
#61693=CARTESIAN_POINT('Ctrl Pts',(10.3981876175369,-38.2742356128,-2.34565818254684));
#61694=CARTESIAN_POINT('Ctrl Pts',(10.3804038373573,-38.2742356128,-2.4383974632595));
#61695=CARTESIAN_POINT('Ctrl Pts',(10.360369967161,-38.2742356128,-2.53073330308211));
#61696=CARTESIAN_POINT('Ctrl Pts',(10.3509818947903,-38.2742356128,-2.57400280309234));
#61697=CARTESIAN_POINT('Ctrl Pts',(10.3411003824232,-38.2742356128,-2.61718347718347));
#61698=CARTESIAN_POINT('Ctrl Pts',(10.3307213130425,-38.2742356128,-2.66025483526559));
#61699=CARTESIAN_POINT('Ctrl Pts',(10.3088850088353,-38.2742356128,-2.75087175314097));
#61700=CARTESIAN_POINT('Ctrl Pts',(10.2848413058874,-38.2742356128,-2.84101405148704));
#61701=CARTESIAN_POINT('Ctrl Pts',(10.2585770843906,-38.2742356128,-2.93052069295465));
#61702=CARTESIAN_POINT('Ctrl Pts',(10.2332623103076,-38.2742356128,-3.01679168362346));
#61703=CARTESIAN_POINT('Ctrl Pts',(10.2058844678468,-38.2742356128,-3.1024720520646));
#61704=CARTESIAN_POINT('Ctrl Pts',(10.17647883038,-38.2742356128,-3.18740411871625));
#61705=CARTESIAN_POINT('Ctrl Pts',(10.1701327838924,-38.2742356128,-3.2057333538454));
#61706=CARTESIAN_POINT('Ctrl Pts',(10.1636924803055,-38.2742356128,-3.22402768868211));
#61707=CARTESIAN_POINT('Ctrl Pts',(10.1571585890214,-38.2742356128,-3.24228545796317));
#61708=CARTESIAN_POINT('Ctrl Pts',(10.1253246654115,-38.2742356128,-3.33123956009105));
#61709=CARTESIAN_POINT('Ctrl Pts',(10.0912547039976,-38.2742356128,-3.41935554389994));
#61710=CARTESIAN_POINT('Ctrl Pts',(10.055047525097,-38.2742356128,-3.506496931939));
#61711=CARTESIAN_POINT('Ctrl Pts',(10.0175120766863,-38.2742356128,-3.5968351238248));
#61712=CARTESIAN_POINT('Ctrl Pts',(9.9776798930849,-38.2742356128,-3.6861260009171));
#61713=CARTESIAN_POINT('Ctrl Pts',(9.93569575213086,-38.2742356128,-3.77426091291076));
#61714=CARTESIAN_POINT('Ctrl Pts',(9.93138836113134,-38.2742356128,-3.78330317310804));
#61715=CARTESIAN_POINT('Ctrl Pts',(9.92705834651865,-38.2742356128,-3.79233330120649));
#61716=CARTESIAN_POINT('Ctrl Pts',(9.92270588308604,-38.2742356128,-3.80135120370286));
#61717=CARTESIAN_POINT('Ctrl Pts',(9.87657224942915,-38.2742356128,-3.8969358344672));
#61718=CARTESIAN_POINT('Ctrl Pts',(9.82789890031301,-38.2742356128,-3.99117465821485));
#61719=CARTESIAN_POINT('Ctrl Pts',(9.77688915570328,-38.2742356128,-4.08401465291981));
#61720=CARTESIAN_POINT('Ctrl Pts',(9.72389056639723,-38.2742356128,-4.18047443306944));
#61721=CARTESIAN_POINT('Ctrl Pts',(9.66837026041182,-38.2742356128,-4.27542463113601));
#61722=CARTESIAN_POINT('Ctrl Pts',(9.61058522072467,-38.2742356128,-4.36885021802721));
#61723=CARTESIAN_POINT('Ctrl Pts',(9.57944428658444,-38.2742356128,-4.41919819847582));
#61724=CARTESIAN_POINT('Ctrl Pts',(9.54764507174215,-38.2742356128,-4.46910587319495));
#61725=CARTESIAN_POINT('Ctrl Pts',(9.51522480958567,-38.2742356128,-4.51858291647522));
#61726=CARTESIAN_POINT('Ctrl Pts',(9.44022898792422,-38.2742356128,-4.63303515305101));
#61727=CARTESIAN_POINT('Ctrl Pts',(9.36191723932152,-38.2742356128,-4.74516444844837));
#61728=CARTESIAN_POINT('Ctrl Pts',(9.28085520537354,-38.2742356128,-4.85501095685734));
#61729=CARTESIAN_POINT('Ctrl Pts',(9.25126730820571,-38.2742356128,-4.89510527767262));
#61730=CARTESIAN_POINT('Ctrl Pts',(9.221313265791,-38.2742356128,-4.93489597715081));
#61731=CARTESIAN_POINT('Ctrl Pts',(9.19102120554409,-38.2742356128,-4.97438641804631));
#61732=CARTESIAN_POINT('Ctrl Pts',(9.11515162680019,-38.2742356128,-5.07329428666702));
#61733=CARTESIAN_POINT('Ctrl Pts',(9.03715669685487,-38.2742356128,-5.17033255715841));
#61734=CARTESIAN_POINT('Ctrl Pts',(8.95733536342387,-38.2742356128,-5.26565777720866));
#61735=CARTESIAN_POINT('Ctrl Pts',(8.87614395347642,-38.2742356128,-5.36261918698168));
#61736=CARTESIAN_POINT('Ctrl Pts',(8.79306294442929,-38.2742356128,-5.45780803995178));
#61737=CARTESIAN_POINT('Ctrl Pts',(8.70837234666383,-38.2742356128,-5.55134671849507));
#61738=CARTESIAN_POINT('Ctrl Pts',(8.62213413938125,-38.2742356128,-5.64659469361852));
#61739=CARTESIAN_POINT('Ctrl Pts',(8.53422702575129,-38.2742356128,-5.74013141101811));
#61740=CARTESIAN_POINT('Ctrl Pts',(8.44491040792852,-38.2742356128,-5.83204571560467));
#61741=CARTESIAN_POINT('Ctrl Pts',(8.35291571815627,-38.2742356128,-5.92671598125279));
#61742=CARTESIAN_POINT('Ctrl Pts',(8.25942585235678,-38.2742356128,-6.01966488169897));
#61743=CARTESIAN_POINT('Ctrl Pts',(8.16468476449867,-38.2742356128,-6.11095020924391));
#61744=CARTESIAN_POINT('Ctrl Pts',(8.06824182207186,-38.2742356128,-6.20387531479065));
#61745=CARTESIAN_POINT('Ctrl Pts',(7.97050234489563,-38.2742356128,-6.2950762146568));
#61746=CARTESIAN_POINT('Ctrl Pts',(7.8716822016181,-38.2742356128,-6.38457794878723));
#61747=CARTESIAN_POINT('Ctrl Pts',(7.77009921254859,-38.2742356128,-6.47658200158788));
#61748=CARTESIAN_POINT('Ctrl Pts',(7.66737439888165,-38.2742356128,-6.56679020359953));
#61749=CARTESIAN_POINT('Ctrl Pts',(7.56369750800012,-38.2742356128,-6.65519724548669));
#61750=CARTESIAN_POINT('Ctrl Pts',(7.5159885341293,-38.2742356128,-6.69587949603962));
#61751=CARTESIAN_POINT('Ctrl Pts',(7.46807732954183,-38.2742356128,-6.73617992784729));
#61752=CARTESIAN_POINT('Ctrl Pts',(7.41997923973326,-38.2742356128,-6.77609613343191));
#61753=CARTESIAN_POINT('Ctrl Pts',(7.32791155601165,-38.2742356128,-6.85250234011827));
#61754=CARTESIAN_POINT('Ctrl Pts',(7.23515048086156,-38.2742356127366,-6.92750063651648));
#61755=CARTESIAN_POINT('Ctrl Pts',(7.14164675550522,-38.274235612635,-7.00113625961658));
#61756=CARTESIAN_POINT('Ctrl Pts',(7.08482858540921,-38.2742356125733,-7.04588144321736));
#61757=CARTESIAN_POINT('Ctrl Pts',(7.02773667956031,-38.2742356125682,-7.09012245084894));
#61758=CARTESIAN_POINT('Ctrl Pts',(6.97036425873578,-38.274235612668,-7.13386121169709));
#61759=CARTESIAN_POINT('Ctrl Pts',(6.86943011864084,-38.2742356128435,-7.21080992941861));
#61760=CARTESIAN_POINT('Ctrl Pts',(6.76757099008427,-38.2742356127991,-7.28622960703381));
#61761=CARTESIAN_POINT('Ctrl Pts',(6.66470672473084,-38.2742356127998,-7.36011874372879));
#61762=CARTESIAN_POINT('Ctrl Pts',(6.6128801431363,-38.2742356128002,-7.39734665138666));
#61763=CARTESIAN_POINT('Ctrl Pts',(6.5607987888592,-38.2742356128,-7.43418521583754));
#61764=CARTESIAN_POINT('Ctrl Pts',(6.50845458459114,-38.2742356128,-7.47062987547125));
#61765=CARTESIAN_POINT('Ctrl Pts',(6.38936601296616,-38.2742356128,-7.55354531032837));
#61766=CARTESIAN_POINT('Ctrl Pts',(6.26890066502405,-38.2742356128,-7.63443380526014));
#61767=CARTESIAN_POINT('Ctrl Pts',(6.14705288221731,-38.2742356128,-7.71315424109138));
#61768=CARTESIAN_POINT('Ctrl Pts',(6.01029189266294,-38.2742356128,-7.80150943684827));
#61769=CARTESIAN_POINT('Ctrl Pts',(5.87178900326465,-38.2742356128,-7.88713120988784));
#61770=CARTESIAN_POINT('Ctrl Pts',(5.73158927890684,-38.2742356128,-7.96978234287356));
#61771=CARTESIAN_POINT('Ctrl Pts',(5.66437973320283,-38.2742356128,-8.00940399780431));
#61772=CARTESIAN_POINT('Ctrl Pts',(5.59678215398082,-38.2742356128,-8.04834203293516));
#61773=CARTESIAN_POINT('Ctrl Pts',(5.52880173122316,-38.2742356128,-8.08657247318979));
#61774=CARTESIAN_POINT('Ctrl Pts',(5.39297979815478,-38.2742356128,-8.16295523291388));
#61775=CARTESIAN_POINT('Ctrl Pts',(5.25560722450796,-38.2742356128,-8.23652229137831));
#61776=CARTESIAN_POINT('Ctrl Pts',(5.11673653035794,-38.2742356128,-8.30710645917144));
#61777=CARTESIAN_POINT('Ctrl Pts',(4.99592856393252,-38.2742356128,-8.36850983750918));
#61778=CARTESIAN_POINT('Ctrl Pts',(4.873987551265,-38.2742356128,-8.42765509567402));
#61779=CARTESIAN_POINT('Ctrl Pts',(4.75096134365824,-38.2742356128,-8.48446936967895));
#61780=CARTESIAN_POINT('Ctrl Pts',(4.67791920577842,-38.2742356128,-8.518200686901));
#61781=CARTESIAN_POINT('Ctrl Pts',(4.60449475274289,-38.2742356128,-8.55111111808754));
#61782=CARTESIAN_POINT('Ctrl Pts',(4.53069936808626,-38.2742356128,-8.5831942594361));
#61783=CARTESIAN_POINT('Ctrl Pts',(4.39198916695835,-38.2742356128,-8.6434996431668));
#61784=CARTESIAN_POINT('Ctrl Pts',(4.25195587633228,-38.2742356128,-8.70088498843151));
#61785=CARTESIAN_POINT('Ctrl Pts',(4.11066678383247,-38.2742356128,-8.75528142586651));
#61786=CARTESIAN_POINT('Ctrl Pts',(3.96436874851434,-38.2742356128,-8.81160631113716));
#61787=CARTESIAN_POINT('Ctrl Pts',(3.81672386119578,-38.2742356128,-8.86472713193888));
#61788=CARTESIAN_POINT('Ctrl Pts',(3.6678316200746,-38.2742356128,-8.91461741066908));
#61789=CARTESIAN_POINT('Ctrl Pts',(3.51207949781546,-38.2742356127999,-8.96680627379463));
#61790=CARTESIAN_POINT('Ctrl Pts',(3.3549618224836,-38.2742356127999,-9.01546072920466));
#61791=CARTESIAN_POINT('Ctrl Pts',(3.19662740736046,-38.2742356127999,-9.06059499188016));
#61792=CARTESIAN_POINT('Ctrl Pts',(3.03129330521691,-38.2742356127999,-9.10772456121328));
#61793=CARTESIAN_POINT('Ctrl Pts',(2.8646317213971,-38.2742356127999,-9.15101681634443));
#61794=CARTESIAN_POINT('Ctrl Pts',(2.69686030237699,-38.2742356127999,-9.19052227789939));
#61795=CARTESIAN_POINT('Ctrl Pts',(2.52908888335688,-38.2742356127999,-9.23002773945435));
#61796=CARTESIAN_POINT('Ctrl Pts',(2.36020715659891,-38.2742356128,-9.26574773355228));
#61797=CARTESIAN_POINT('Ctrl Pts',(2.19048902652532,-38.2742356128,-9.2977482196728));
#61798=CARTESIAN_POINT('Ctrl Pts',(2.16685412882389,-38.2742356128,-9.3022045981135));
#61799=CARTESIAN_POINT('Ctrl Pts',(2.14320468147333,-38.2742356128,-9.30658854411333));
#61800=CARTESIAN_POINT('Ctrl Pts',(2.11953749589,-38.2742356128,-9.31090098978));
#61801=CARTESIAN_POINT('',(2.08573866528107,-38.2742356128,-9.31728218620194));
#61802=CARTESIAN_POINT('Ctrl Pts',(2.11953715342988,-38.2742356128,-9.31090105217976));
#61803=CARTESIAN_POINT('Ctrl Pts',(2.11797894915308,-38.2742356128,-9.31118497696086));
#61804=CARTESIAN_POINT('Ctrl Pts',(2.11642436145393,-38.2742356128002,-9.31146961094749));
#61805=CARTESIAN_POINT('Ctrl Pts',(2.11486501656171,-38.2742356127997,-9.31175659977283));
#61806=CARTESIAN_POINT('Ctrl Pts',(2.11438298834213,-38.2742356127995,-9.31184531440755));
#61807=CARTESIAN_POINT('Ctrl Pts',(2.11390088140109,-38.2742356127993,-9.31193417995486));
#61808=CARTESIAN_POINT('Ctrl Pts',(2.11341946076803,-38.2742356127989,-9.31202304609802));
#61809=CARTESIAN_POINT('Ctrl Pts',(2.11153045027428,-38.2742356127973,-9.3123717413251));
#61810=CARTESIAN_POINT('Ctrl Pts',(2.10961613871839,-38.2742356127953,-9.31272773883357));
#61811=CARTESIAN_POINT('Ctrl Pts',(2.1076821531108,-38.2742356127946,-9.31308956372315));
#61812=CARTESIAN_POINT('Ctrl Pts',(2.10497282330549,-38.2742356127937,-9.31359644596353));
#61813=CARTESIAN_POINT('Ctrl Pts',(2.10223212032299,-38.2742356127952,-9.31411334934674));
#61814=CARTESIAN_POINT('Ctrl Pts',(2.09955927298003,-38.2742356127967,-9.31462091916872));
#61815=CARTESIAN_POINT('Ctrl Pts',(2.09775952512019,-38.2742356127978,-9.31496268866904));
#61816=CARTESIAN_POINT('Ctrl Pts',(2.09599276630409,-38.2742356127987,-9.31529981756808));
#61817=CARTESIAN_POINT('Ctrl Pts',(2.09425998150645,-38.2742356127993,-9.31563221100442));
#61818=CARTESIAN_POINT('Ctrl Pts',(2.09279115396838,-38.2742356127997,-9.31591397053591));
#61819=CARTESIAN_POINT('Ctrl Pts',(2.09134719651597,-38.2742356127999,-9.31619224217171));
#61820=CARTESIAN_POINT('Ctrl Pts',(2.08989189609338,-38.2742356128,-9.31647410888022));
#61821=CARTESIAN_POINT('Ctrl Pts',(2.08892721858332,-38.2742356128,-9.31666095035317));
#61822=CARTESIAN_POINT('Ctrl Pts',(2.08795684384456,-38.2742356128,-9.31684950975924));
#61823=CARTESIAN_POINT('Ctrl Pts',(2.08695750245697,-38.2742356128,-9.31704430756847));
#61824=CARTESIAN_POINT('Ctrl Pts',(2.08655395799507,-38.2742356128,-9.31712296895295));
#61825=CARTESIAN_POINT('Ctrl Pts',(2.08614978311668,-38.2742356128,-9.31720185229));
#61826=CARTESIAN_POINT('Ctrl Pts',(2.08573866565001,-38.2742356128,-9.31728218809));
#61827=CARTESIAN_POINT('',(0.417273437277162,-38.2742356128,-7.9503178208061));
#61828=CARTESIAN_POINT('Ctrl Pts',(2.08573866481991,-38.2742356128,-9.31728218384186));
#61829=CARTESIAN_POINT('Ctrl Pts',(2.07763203559797,-38.2742356128,-9.31886622212027));
#61830=CARTESIAN_POINT('Ctrl Pts',(2.06950380369,-38.2742356128,-9.320380182645));
#61831=CARTESIAN_POINT('Ctrl Pts',(2.06136477179,-38.2742356128,-9.321821861545));
#61832=CARTESIAN_POINT('Ctrl Pts',(2.05322573989,-38.2742356128,-9.323263540445));
#61833=CARTESIAN_POINT('Ctrl Pts',(2.04507348953682,-38.2742356128,-9.32463342169253));
#61834=CARTESIAN_POINT('Ctrl Pts',(2.03690970729997,-38.2742356127999,-9.32593117246363));
#61835=CARTESIAN_POINT('Ctrl Pts',(2.02058253631524,-38.2742356127998,-9.32852661145511));
#61836=CARTESIAN_POINT('Ctrl Pts',(2.00420686669781,-38.2742356127997,-9.33083386430894));
#61837=CARTESIAN_POINT('Ctrl Pts',(1.98779626405356,-38.2742356127995,-9.33285066337887));
#61838=CARTESIAN_POINT('Ctrl Pts',(1.93350680188262,-38.2742356127992,-9.3395226265716));
#61839=CARTESIAN_POINT('Ctrl Pts',(1.87881722880592,-38.2742356127996,-9.34301407998262));
#61840=CARTESIAN_POINT('Ctrl Pts',(1.82410851328607,-38.2742356127998,-9.34329112627487));
#61841=CARTESIAN_POINT('Ctrl Pts',(1.77958953966205,-38.2742356128,-9.34351657146144));
#61842=CARTESIAN_POINT('Ctrl Pts',(1.73505802515345,-38.2742356128,-9.34161458422846));
#61843=CARTESIAN_POINT('Ctrl Pts',(1.69071856317199,-38.2742356128,-9.3375922987591));
#61844=CARTESIAN_POINT('Ctrl Pts',(1.63486128345798,-38.2742356128,-9.33252516635579));
#61845=CARTESIAN_POINT('Ctrl Pts',(1.57931009792603,-38.2742356128,-9.32409203444833));
#61846=CARTESIAN_POINT('Ctrl Pts',(1.52446757032607,-38.2742356128,-9.31235583273348));
#61847=CARTESIAN_POINT('Ctrl Pts',(1.46867636729189,-38.2742356128,-9.30041661619155));
#61848=CARTESIAN_POINT('Ctrl Pts',(1.41361897746577,-38.2742356128,-9.28505921699745));
#61849=CARTESIAN_POINT('Ctrl Pts',(1.35970641711599,-38.2742356128,-9.26640242007238));
#61850=CARTESIAN_POINT('Ctrl Pts',(1.30544267878404,-38.2742356128,-9.24762409569146));
#61851=CARTESIAN_POINT('Ctrl Pts',(1.25233916318076,-38.2742356128,-9.22550350962761));
#61852=CARTESIAN_POINT('Ctrl Pts',(1.20079564211786,-38.2742356128,-9.2002113020856));
#61853=CARTESIAN_POINT('Ctrl Pts',(1.14903365499695,-38.2742356128,-9.17481189408918));
#61854=CARTESIAN_POINT('Ctrl Pts',(1.09884535235233,-38.2742356128,-9.14621421029534));
#61855=CARTESIAN_POINT('Ctrl Pts',(1.05060964073121,-38.2742356128,-9.11463668493604));
#61856=CARTESIAN_POINT('Ctrl Pts',(1.01815169737214,-38.2742356128,-9.09338808104725));
#61857=CARTESIAN_POINT('Ctrl Pts',(0.98657734033846,-38.2742356128,-9.0707911498067));
#61858=CARTESIAN_POINT('Ctrl Pts',(0.955993931424741,-38.2742356128,-9.04692298582716));
#61859=CARTESIAN_POINT('Ctrl Pts',(0.909151723851522,-38.2742356128,-9.01036599197877));
#61860=CARTESIAN_POINT('Ctrl Pts',(0.864636917513829,-38.2742356128014,
-8.97082583521411));
#61861=CARTESIAN_POINT('Ctrl Pts',(0.822807595223311,-38.2742356127971,
-8.92862289484912));
#61862=CARTESIAN_POINT('Ctrl Pts',(0.781747848673634,-38.2742356127929,
-8.88719640404915));
#61863=CARTESIAN_POINT('Ctrl Pts',(0.743275948023315,-38.2742356127857,
-8.84320438706447));
#61864=CARTESIAN_POINT('Ctrl Pts',(0.707693495085963,-38.274235612732,-8.79698388515189));
#61865=CARTESIAN_POINT('Ctrl Pts',(0.698124380455637,-38.2742356127175,
-8.78455390226534));
#61866=CARTESIAN_POINT('Ctrl Pts',(0.688764013973583,-38.2742356126994,
-8.77196293551276));
#61867=CARTESIAN_POINT('Ctrl Pts',(0.679617753842452,-38.2742356126758,
-8.75921794590775));
#61868=CARTESIAN_POINT('Ctrl Pts',(0.64666137843158,-38.2742356125909,-8.71329440382516));
#61869=CARTESIAN_POINT('Ctrl Pts',(0.616487257383922,-38.2742356124953,
-8.66537096962203));
#61870=CARTESIAN_POINT('Ctrl Pts',(0.589321147407174,-38.2742356124624,
-8.61579545953694));
#61871=CARTESIAN_POINT('Ctrl Pts',(0.562636209375934,-38.27423561243,-8.56709804148113));
#61872=CARTESIAN_POINT('Ctrl Pts',(0.538853856273966,-38.2742356124619,
-8.51680672557378));
#61873=CARTESIAN_POINT('Ctrl Pts',(0.5181451821965,-38.2742356125444,-8.4652774514545));
#61874=CARTESIAN_POINT('Ctrl Pts',(0.510153982159852,-38.2742356125762,
-8.4453929945506));
#61875=CARTESIAN_POINT('Ctrl Pts',(0.502620005449637,-38.2742356126143,
-8.42532446288721));
#61876=CARTESIAN_POINT('Ctrl Pts',(0.49555124160412,-38.2742356126526,-8.40509330132935));
#61877=CARTESIAN_POINT('Ctrl Pts',(0.476947058283054,-38.2742356127534,
-8.3518471826803));
#61878=CARTESIAN_POINT('Ctrl Pts',(0.461573393384668,-38.274235612776,-8.29747876272508));
#61879=CARTESIAN_POINT('Ctrl Pts',(0.449535357169435,-38.2742356127884,
-8.24238015264472));
#61880=CARTESIAN_POINT('Ctrl Pts',(0.437781985872286,-38.2742356128005,
-8.18858446615129));
#61881=CARTESIAN_POINT('Ctrl Pts',(0.42920844174801,-38.2742356127996,-8.13409273336811));
#61882=CARTESIAN_POINT('Ctrl Pts',(0.423868058795757,-38.2742356127999,
-8.07929126394412));
#61883=CARTESIAN_POINT('Ctrl Pts',(0.420662885353337,-38.2742356128001,
-8.04640069860944));
#61884=CARTESIAN_POINT('Ctrl Pts',(0.418621474870239,-38.2742356128,-8.01339897157512));
#61885=CARTESIAN_POINT('Ctrl Pts',(0.417747123205582,-38.2742356128,-7.98037341588237));
#61886=CARTESIAN_POINT('Ctrl Pts',(0.417500472528033,-38.2742356128,-7.97105705495193));
#61887=CARTESIAN_POINT('Ctrl Pts',(0.417346628279231,-38.2742356128,-7.96173686793695));
#61888=CARTESIAN_POINT('Ctrl Pts',(0.417285628014923,-38.2742356128,-7.95241938665697));
#61889=CARTESIAN_POINT('Ctrl Pts',(0.417281041447002,-38.2742356128,-7.95171881164752));
#61890=CARTESIAN_POINT('Ctrl Pts',(0.417276979796764,-38.2742356128,-7.95101828445243));
#61891=CARTESIAN_POINT('Ctrl Pts',(0.417273442888032,-38.2742356128,-7.95031782080527));
#61892=CARTESIAN_POINT('',(0.417273426056,-38.2742356128,-3.28965091665));
#61893=CARTESIAN_POINT('',(0.417273426056,-38.2742356128,0.916320001688));
#61894=CARTESIAN_POINT('',(1.05996501343,-38.2742356128,-2.50526959142));
#61895=CARTESIAN_POINT('Ctrl Pts',(0.417273426056,-38.2742356128,-3.28965091665));
#61896=CARTESIAN_POINT('Ctrl Pts',(0.417273426056,-38.2742356128,-3.28687600563435));
#61897=CARTESIAN_POINT('Ctrl Pts',(0.417288267241563,-38.2742356128,-3.28403966420407));
#61898=CARTESIAN_POINT('Ctrl Pts',(0.417318551745409,-38.2742356128,-3.28120405870701));
#61899=CARTESIAN_POINT('Ctrl Pts',(0.417343821453037,-38.2742356128,-3.27883799974081));
#61900=CARTESIAN_POINT('Ctrl Pts',(0.417379796757908,-38.2742356128,-3.27647245778261));
#61901=CARTESIAN_POINT('Ctrl Pts',(0.417425416856367,-38.2742356128,-3.27414357493084));
#61902=CARTESIAN_POINT('Ctrl Pts',(0.41745011376523,-38.2742356128,-3.27288281027914));
#61903=CARTESIAN_POINT('Ctrl Pts',(0.417477564963489,-38.2742356128,-3.27163366066603));
#61904=CARTESIAN_POINT('Ctrl Pts',(0.417508047794076,-38.2742356128,-3.27038083299254));
#61905=CARTESIAN_POINT('Ctrl Pts',(0.417623703682738,-38.2742356128,-3.26562743919265));
#61906=CARTESIAN_POINT('Ctrl Pts',(0.417782029382677,-38.2742356128,-3.2608753558277));
#61907=CARTESIAN_POINT('Ctrl Pts',(0.417982831198984,-38.2742356128,-3.25612557957555));
#61908=CARTESIAN_POINT('Ctrl Pts',(0.419232573923149,-38.2742356128,-3.22656410238523));
#61909=CARTESIAN_POINT('Ctrl Pts',(0.422131989162464,-38.2742356128108,
-3.19706607707807));
#61910=CARTESIAN_POINT('Ctrl Pts',(0.426644322880871,-38.2742356127073,
-3.16783893396853));
#61911=CARTESIAN_POINT('Ctrl Pts',(0.431919124989423,-38.2742356125864,
-3.13367315507848));
#61912=CARTESIAN_POINT('Ctrl Pts',(0.439398461031886,-38.274235612256,-3.09987691259941));
#61913=CARTESIAN_POINT('Ctrl Pts',(0.449024112493034,-38.2742356120111,
-3.06670564901039));
#61914=CARTESIAN_POINT('Ctrl Pts',(0.452936926049543,-38.2742356119116,
-3.05322157778866));
#61915=CARTESIAN_POINT('Ctrl Pts',(0.457204357922259,-38.2742356118354,
-3.03984007280312));
#61916=CARTESIAN_POINT('Ctrl Pts',(0.461822173897898,-38.274235611817,-3.02657609664833));
#61917=CARTESIAN_POINT('Ctrl Pts',(0.474294774018725,-38.2742356117674,
-2.99075044411827));
#61918=CARTESIAN_POINT('Ctrl Pts',(0.489309772383553,-38.2742356121238,
-2.955834776464));
#61919=CARTESIAN_POINT('Ctrl Pts',(0.506727646325082,-38.2742356123874,
-2.92214655478451));
#61920=CARTESIAN_POINT('Ctrl Pts',(0.521654671661917,-38.2742356126133,
-2.89327592796457));
#61921=CARTESIAN_POINT('Ctrl Pts',(0.53834609093257,-38.2742356127471,-2.86530463487966));
#61922=CARTESIAN_POINT('Ctrl Pts',(0.55668064368847,-38.274235612782,-2.83844528990823));
#61923=CARTESIAN_POINT('Ctrl Pts',(0.568162427347117,-38.2742356128038,
-2.82162496206709));
#61924=CARTESIAN_POINT('Ctrl Pts',(0.580287959861297,-38.2742356128,-2.80524108228529));
#61925=CARTESIAN_POINT('Ctrl Pts',(0.593020083314608,-38.2742356128,-2.78935374684381));
#61926=CARTESIAN_POINT('Ctrl Pts',(0.616891823099495,-38.2742356128,-2.75956623033686));
#61927=CARTESIAN_POINT('Ctrl Pts',(0.642906462533144,-38.2742356128,-2.73151085070984));
#61928=CARTESIAN_POINT('Ctrl Pts',(0.670793009043573,-38.2742356128,-2.70545242330525));
#61929=CARTESIAN_POINT('Ctrl Pts',(0.699437797938788,-38.2742356128,-2.6786854605454));
#61930=CARTESIAN_POINT('Ctrl Pts',(0.730056969621417,-38.2742356128,-2.65402633543565));
#61931=CARTESIAN_POINT('Ctrl Pts',(0.762310842189897,-38.2742356128,-2.63173290731302));
#61932=CARTESIAN_POINT('Ctrl Pts',(0.773410204061867,-38.2742356128,-2.62406118276043));
#61933=CARTESIAN_POINT('Ctrl Pts',(0.784702809312063,-38.2742356128,-2.61666930347125));
#61934=CARTESIAN_POINT('Ctrl Pts',(0.796173849974241,-38.2742356128,-2.60956673778134));
#61935=CARTESIAN_POINT('Ctrl Pts',(0.830647647097411,-38.2742356128,-2.58822147226805));
#61936=CARTESIAN_POINT('Ctrl Pts',(0.866742606403394,-38.2742356128,-2.56948777529846));
#61937=CARTESIAN_POINT('Ctrl Pts',(0.904053286489635,-38.2742356128,-2.55358817651221));
#61938=CARTESIAN_POINT('Ctrl Pts',(0.940099610515895,-38.2742356127999,
-2.538227371284));
#61939=CARTESIAN_POINT('Ctrl Pts',(0.977279742329185,-38.2742356127999,
-2.52551220542387));
#61940=CARTESIAN_POINT('Ctrl Pts',(1.01521576655219,-38.2742356128,-2.51559656446267));
#61941=CARTESIAN_POINT('Ctrl Pts',(1.02599627385077,-38.2742356128,-2.51277877736078));
#61942=CARTESIAN_POINT('Ctrl Pts',(1.036837791067,-38.2742356128,-2.51018675230784));
#61943=CARTESIAN_POINT('Ctrl Pts',(1.04773160770174,-38.2742356128,-2.50782323579403));
#61944=CARTESIAN_POINT('Ctrl Pts',(1.05180229630503,-38.2742356128,-2.50694006141548));
#61945=CARTESIAN_POINT('Ctrl Pts',(1.05588045019742,-38.2742356128,-2.50608875312377));
#61946=CARTESIAN_POINT('Ctrl Pts',(1.05996501343,-38.2742356128,-2.50526959142));
#61947=CARTESIAN_POINT('',(2.29653396536691,-38.2742356128,-2.09683591201288));
#61948=CARTESIAN_POINT('Origin',(0.443861353289543,-38.2742356128,1.43817589094895));
#61949=CARTESIAN_POINT('',(6.27496281272,-38.2742356128,2.72284538598));
#61950=CARTESIAN_POINT('Ctrl Pts',(2.29653416635,-38.2742356128,-2.09683582206));
#61951=CARTESIAN_POINT('Ctrl Pts',(2.36220797012657,-38.2742356128,-2.06590956675441));
#61952=CARTESIAN_POINT('Ctrl Pts',(2.42765371624071,-38.2742356128,-2.03423134842919));
#61953=CARTESIAN_POINT('Ctrl Pts',(2.49302552130743,-38.2742356128,-2.00182212247038));
#61954=CARTESIAN_POINT('Ctrl Pts',(2.5004630785183,-38.2742356128,-1.99813482223471));
#61955=CARTESIAN_POINT('Ctrl Pts',(2.50789964478502,-38.2742356128,-1.99443801598111));
#61956=CARTESIAN_POINT('Ctrl Pts',(2.5153354213652,-38.2742356128,-1.99073170164066));
#61957=CARTESIAN_POINT('Ctrl Pts',(2.58810754953454,-38.2742356128,-1.95445890897253));
#61958=CARTESIAN_POINT('Ctrl Pts',(2.66068080708327,-38.2742356128,-1.91734068779584));
#61959=CARTESIAN_POINT('Ctrl Pts',(2.73288981233302,-38.2742356128,-1.879533522123));
#61960=CARTESIAN_POINT('Ctrl Pts',(2.76748989568229,-38.2742356128,-1.86141762260389));
#61961=CARTESIAN_POINT('Ctrl Pts',(2.80201510146988,-38.2742356128,-1.84313841771104));
#61962=CARTESIAN_POINT('Ctrl Pts',(2.83648773623042,-38.2742356128,-1.82468695240457));
#61963=CARTESIAN_POINT('Ctrl Pts',(2.87395812655656,-38.2742356128,-1.8046309395142));
#61964=CARTESIAN_POINT('Ctrl Pts',(2.91136644060994,-38.2742356128,-1.78437143803804));
#61965=CARTESIAN_POINT('Ctrl Pts',(2.94873835187512,-38.2742356128,-1.76389306709537));
#61966=CARTESIAN_POINT('Ctrl Pts',(3.02049221311562,-38.2742356128,-1.72457470907441));
#61967=CARTESIAN_POINT('Ctrl Pts',(3.09205299633584,-38.2742356128314,-1.68448376738218));
#61968=CARTESIAN_POINT('Ctrl Pts',(3.16330912697989,-38.2742356127677,-1.64363930500427));
#61969=CARTESIAN_POINT('Ctrl Pts',(3.24367404103224,-38.274235612696,-1.59757363067076));
#61970=CARTESIAN_POINT('Ctrl Pts',(3.3236414105591,-38.2742356125322,-1.55054807220068));
#61971=CARTESIAN_POINT('Ctrl Pts',(3.40304869483591,-38.2742356124157,-1.50252179228988));
#61972=CARTESIAN_POINT('Ctrl Pts',(3.48682359904184,-38.2742356122927,-1.45185393435296));
#61973=CARTESIAN_POINT('Ctrl Pts',(3.56997485440011,-38.2742356122232,-1.40007167360168));
#61974=CARTESIAN_POINT('Ctrl Pts',(3.65226355234279,-38.2742356122489,-1.34708967420857));
#61975=CARTESIAN_POINT('Ctrl Pts',(3.74435941007879,-38.2742356122777,-1.28779328478124));
#61976=CARTESIAN_POINT('Ctrl Pts',(3.83537474930273,-38.2742356124287,-1.22699330737691));
#61977=CARTESIAN_POINT('Ctrl Pts',(3.92491817722107,-38.2742356125816,-1.16453523334719));
#61978=CARTESIAN_POINT('Ctrl Pts',(3.94998723603213,-38.2742356126244,-1.14704913562369));
#61979=CARTESIAN_POINT('Ctrl Pts',(3.9749406287215,-38.2742356126663,-1.12943293494422));
#61980=CARTESIAN_POINT('Ctrl Pts',(3.99976913772119,-38.274235612702,-1.11168299588818));
#61981=CARTESIAN_POINT('Ctrl Pts',(4.1029832219094,-38.2742356128504,-1.03789508924876));
#61982=CARTESIAN_POINT('Ctrl Pts',(4.20409444599943,-38.2742356127998,-0.96176757421914));
#61983=CARTESIAN_POINT('Ctrl Pts',(4.3024268513798,-38.2742356128,-0.8830050686021));
#61984=CARTESIAN_POINT('Ctrl Pts',(4.33166644233314,-38.2742356128,-0.859584676943892));
#61985=CARTESIAN_POINT('Ctrl Pts',(4.36065997900015,-38.2742356128,-0.835931390211039));
#61986=CARTESIAN_POINT('Ctrl Pts',(4.38938894944612,-38.2742356128,-0.812037889005671));
#61987=CARTESIAN_POINT('Ctrl Pts',(4.47021753239654,-38.2742356128,-0.744813835578956));
#61988=CARTESIAN_POINT('Ctrl Pts',(4.54898225582855,-38.2742356128,-0.67565943355637));
#61989=CARTESIAN_POINT('Ctrl Pts',(4.62522401353323,-38.2742356128,-0.604467608051967));
#61990=CARTESIAN_POINT('Ctrl Pts',(4.66721344467678,-38.2742356128,-0.56525937958248));
#61991=CARTESIAN_POINT('Ctrl Pts',(4.70843765186859,-38.2742356128,-0.525433887573267));
#61992=CARTESIAN_POINT('Ctrl Pts',(4.74882153936151,-38.2742356128,-0.484980128874531));
#61993=CARTESIAN_POINT('Ctrl Pts',(4.80544979326116,-38.2742356128,-0.428253898167081));
#61994=CARTESIAN_POINT('Ctrl Pts',(4.86043388600898,-38.2742356128,-0.370281695042897));
#61995=CARTESIAN_POINT('Ctrl Pts',(4.9135816071207,-38.2742356128,-0.311043961171806));
#61996=CARTESIAN_POINT('Ctrl Pts',(4.96656054227607,-38.2742356128,-0.251994353853548));
#61997=CARTESIAN_POINT('Ctrl Pts',(5.01771478879239,-38.2742356128,-0.191686425068915));
#61998=CARTESIAN_POINT('Ctrl Pts',(5.06690551256612,-38.2742356128,-0.130100591119076));
#61999=CARTESIAN_POINT('Ctrl Pts',(5.11624778203621,-38.2742356128,-0.0683250248909378));
#62000=CARTESIAN_POINT('Ctrl Pts',(5.1636143955695,-38.2742356128,-0.0052628404116386));
#62001=CARTESIAN_POINT('Ctrl Pts',(5.20891710254948,-38.2742356128,0.0590936045073542));
#62002=CARTESIAN_POINT('Ctrl Pts',(5.25421980952947,-38.2742356128,0.123450049426347));
#62003=CARTESIAN_POINT('Ctrl Pts',(5.29745862035284,-38.2742356128,0.189101579445806));
#62004=CARTESIAN_POINT('Ctrl Pts',(5.3385970789696,-38.2742356128,0.256031336527183));
#62005=CARTESIAN_POINT('Ctrl Pts',(5.37557455438351,-38.2742356128,0.316191428328177));
#62006=CARTESIAN_POINT('Ctrl Pts',(5.41085446100392,-38.2742356128,0.377382687413388));
#62007=CARTESIAN_POINT('Ctrl Pts',(5.44446124996944,-38.2742356128,0.439578664361658));
#62008=CARTESIAN_POINT('Ctrl Pts',(5.47656905045249,-38.2742356128,0.499000468115407));
#62009=CARTESIAN_POINT('Ctrl Pts',(5.50714957085958,-38.2742356128,0.559339597971341));
#62010=CARTESIAN_POINT('Ctrl Pts',(5.53626992889454,-38.2742356128,0.620564294117294));
#62011=CARTESIAN_POINT('Ctrl Pts',(5.56110600265468,-38.2742356128,0.672781408604592));
#62012=CARTESIAN_POINT('Ctrl Pts',(5.58488055554933,-38.2742356128,0.725642638693521));
#62013=CARTESIAN_POINT('Ctrl Pts',(5.60766441565783,-38.2742356128,0.779121015828294));
#62014=CARTESIAN_POINT('Ctrl Pts',(5.61969038696963,-38.2742356128,0.807348428837395));
#62015=CARTESIAN_POINT('Ctrl Pts',(5.63144225779155,-38.2742356128,0.835752782091019));
#62016=CARTESIAN_POINT('Ctrl Pts',(5.64294118123923,-38.2742356128,0.86435562270076));
#62017=CARTESIAN_POINT('Ctrl Pts',(5.65633061319254,-38.2742356128,0.897660982959721));
#62018=CARTESIAN_POINT('Ctrl Pts',(5.66937655460697,-38.2742356128,0.931233997989407));
#62019=CARTESIAN_POINT('Ctrl Pts',(5.68209585008665,-38.2742356128,0.965033637032103));
#62020=CARTESIAN_POINT('Ctrl Pts',(5.69609333621808,-38.2742356128,1.00222987793265));
#62021=CARTESIAN_POINT('Ctrl Pts',(5.70969363110763,-38.2742356128,1.03969538642074));
#62022=CARTESIAN_POINT('Ctrl Pts',(5.72291809444913,-38.2742356128,1.07734587531081));
#62023=CARTESIAN_POINT('Ctrl Pts',(5.7334870169713,-38.2742356128,1.1074359507812));
#62024=CARTESIAN_POINT('Ctrl Pts',(5.74381549485532,-38.2742356128,1.13764226861823));
#62025=CARTESIAN_POINT('Ctrl Pts',(5.75392556483009,-38.2742356128,1.16794836395337));
#62026=CARTESIAN_POINT('Ctrl Pts',(5.76310014927473,-38.2742356128,1.19545023402284));
#62027=CARTESIAN_POINT('Ctrl Pts',(5.7720946772672,-38.2742356128,1.2230334474181));
#62028=CARTESIAN_POINT('Ctrl Pts',(5.78093944060798,-38.2742356128,1.25072622636446));
#62029=CARTESIAN_POINT('Ctrl Pts',(5.78906855841899,-38.2742356128,1.27617833332265));
#62030=CARTESIAN_POINT('Ctrl Pts',(5.79707109396125,-38.2742356128,1.30172265704213));
#62031=CARTESIAN_POINT('Ctrl Pts',(5.80498454924915,-38.2742356128,1.32742448428365));
#62032=CARTESIAN_POINT('Ctrl Pts',(5.8067223616598,-38.2742356128,1.33306866280388));
#62033=CARTESIAN_POINT('Ctrl Pts',(5.80845593782368,-38.2742356128,1.33872062536267));
#62034=CARTESIAN_POINT('Ctrl Pts',(5.81018578013775,-38.2742356128,1.34438139725192));
#62035=CARTESIAN_POINT('Ctrl Pts',(5.81567140688787,-38.2742356128,1.36233267607618));
#62036=CARTESIAN_POINT('Ctrl Pts',(5.82110692689557,-38.2742356127995,1.38032842460541));
#62037=CARTESIAN_POINT('Ctrl Pts',(5.82650005324596,-38.2742356127995,1.39836590318722));
#62038=CARTESIAN_POINT('Ctrl Pts',(5.82697260131895,-38.2742356127996,1.39994635489403));
#62039=CARTESIAN_POINT('Ctrl Pts',(5.82744483120366,-38.2742356127996,1.4015271585344));
#62040=CARTESIAN_POINT('Ctrl Pts',(5.82791675210203,-38.2742356127996,1.40310832963793));
#62041=CARTESIAN_POINT('Ctrl Pts',(5.83360773127681,-38.2742356127999,1.4221759569734));
#62042=CARTESIAN_POINT('Ctrl Pts',(5.83924444553751,-38.2742356127999,1.44126285712189));
#62043=CARTESIAN_POINT('Ctrl Pts',(5.84480916037222,-38.2742356128,1.46027646702416));
#62044=CARTESIAN_POINT('Ctrl Pts',(5.85080823572841,-38.2742356128,1.48077420715733));
#62045=CARTESIAN_POINT('Ctrl Pts',(5.85672364156798,-38.2742356128,1.50118680709605));
#62046=CARTESIAN_POINT('Ctrl Pts',(5.86255182978096,-38.2742356128,1.52146040862887));
#62047=CARTESIAN_POINT('Ctrl Pts',(5.86801153465465,-38.2742356128,1.54045222513357));
#62048=CARTESIAN_POINT('Ctrl Pts',(5.87339510515199,-38.2742356128,1.55932342003616));
#62049=CARTESIAN_POINT('Ctrl Pts',(5.87871159455216,-38.2742356128,1.57806935091714));
#62050=CARTESIAN_POINT('Ctrl Pts',(5.88587811874549,-38.2742356128,1.60333850074009));
#62051=CARTESIAN_POINT('Ctrl Pts',(5.89292575369051,-38.2742356128,1.6283904733301));
#62052=CARTESIAN_POINT('Ctrl Pts',(5.8999252541189,-38.2742356128,1.65338209442216));
#62053=CARTESIAN_POINT('Ctrl Pts',(5.9087612742733,-38.2742356128,1.68493098422072));
#62054=CARTESIAN_POINT('Ctrl Pts',(5.91752179783635,-38.2742356128,1.71638910609064));
#62055=CARTESIAN_POINT('Ctrl Pts',(5.92636835988832,-38.2742356128,1.74812750090717));
#62056=CARTESIAN_POINT('Ctrl Pts',(5.93257015502608,-38.2742356128,1.7703773897902));
#62057=CARTESIAN_POINT('Ctrl Pts',(5.93881483092627,-38.2742356128,1.79276689613811));
#62058=CARTESIAN_POINT('Ctrl Pts',(5.94515464644725,-38.2742356128,1.81540405784503));
#62059=CARTESIAN_POINT('Ctrl Pts',(5.9510135097083,-38.2742356128,1.83632391499546));
#62060=CARTESIAN_POINT('Ctrl Pts',(5.95695343702594,-38.2742356128,1.85745455864831));
#62061=CARTESIAN_POINT('Ctrl Pts',(5.96300290943211,-38.2742356128,1.87882926010439));
#62062=CARTESIAN_POINT('Ctrl Pts',(5.96868836264847,-38.2742356128,1.89891776650344));
#62063=CARTESIAN_POINT('Ctrl Pts',(5.97447073827174,-38.2742356128,1.91922240784038));
#62064=CARTESIAN_POINT('Ctrl Pts',(5.98036338205917,-38.2742356128,1.93972857692636));
#62065=CARTESIAN_POINT('Ctrl Pts',(5.98585680097295,-38.2742356128,1.95884545912217));
#62066=CARTESIAN_POINT('Ctrl Pts',(5.99144611848614,-38.2742356128,1.97813769237131));
#62067=CARTESIAN_POINT('Ctrl Pts',(5.99713141052935,-38.2742356128,1.99755056933384));
#62068=CARTESIAN_POINT('Ctrl Pts',(6.00188504763554,-38.2742356128,2.01378223721752));
#62069=CARTESIAN_POINT('Ctrl Pts',(6.00670564982786,-38.2742356128,2.03009770750313));
#62070=CARTESIAN_POINT('Ctrl Pts',(6.01158632787636,-38.2742356128,2.04643771535537));
#62071=CARTESIAN_POINT('Ctrl Pts',(6.02553662212153,-38.2742356128,2.09314186491048));
#62072=CARTESIAN_POINT('Ctrl Pts',(6.03996335521539,-38.2742356128,2.1400074331509));
#62073=CARTESIAN_POINT('Ctrl Pts',(6.05510272454428,-38.2742356128,2.18697705047249));
#62074=CARTESIAN_POINT('Ctrl Pts',(6.0707480680562,-38.2742356128,2.23551644347202));
#62075=CARTESIAN_POINT('Ctrl Pts',(6.08715459885474,-38.2742356128,2.28416696934139));
#62076=CARTESIAN_POINT('Ctrl Pts',(6.10461272043758,-38.2742356128,2.33281749388226));
#62077=CARTESIAN_POINT('Ctrl Pts',(6.12243742488736,-38.2742356128,2.38248957441811));
#62078=CARTESIAN_POINT('Ctrl Pts',(6.14135856879351,-38.2742356128,2.43216154123912));
#62079=CARTESIAN_POINT('Ctrl Pts',(6.16171298081537,-38.2742356128,2.4816669788947));
#62080=CARTESIAN_POINT('Ctrl Pts',(6.18281606494677,-38.2742356128,2.53299331613722));
#62081=CARTESIAN_POINT('Ctrl Pts',(6.20546001019525,-38.2742356128,2.58414062053214));
#62082=CARTESIAN_POINT('Ctrl Pts',(6.23004640194285,-38.2742356128,2.63487313183816));
#62083=CARTESIAN_POINT('Ctrl Pts',(6.24412952051531,-38.2742356128,2.66393278319065));
#62084=CARTESIAN_POINT('Ctrl Pts',(6.25885041805261,-38.2742356128,2.69285542631629));
#62085=CARTESIAN_POINT('Ctrl Pts',(6.27428775967426,-38.2742356128,2.7215898409063));
#62086=CARTESIAN_POINT('Ctrl Pts',(6.2745126230389,-38.2742356128,2.72200839206001));
#62087=CARTESIAN_POINT('Ctrl Pts',(6.27473763842,-38.2742356128,2.72242690309667));
#62088=CARTESIAN_POINT('Ctrl Pts',(6.27496281272,-38.2742356128,2.72284538598));
#62089=CARTESIAN_POINT('',(9.72829290598,-38.2742356128,2.64854903634));
#62090=CARTESIAN_POINT('Ctrl Pts',(6.27496281272,-38.2742356128,2.72284538598));
#62091=CARTESIAN_POINT('Ctrl Pts',(6.28175989394697,-38.2742356128,2.73547766265914));
#62092=CARTESIAN_POINT('Ctrl Pts',(6.28867511539028,-38.2742356128,2.74803334580149));
#62093=CARTESIAN_POINT('Ctrl Pts',(6.29570579837365,-38.2742356128,2.7605119793025));
#62094=CARTESIAN_POINT('Ctrl Pts',(6.31679767088927,-38.2742356128,2.79794756665514));
#62095=CARTESIAN_POINT('Ctrl Pts',(6.33892929501013,-38.2742356128,2.8346928281563));
#62096=CARTESIAN_POINT('Ctrl Pts',(6.36204152758071,-38.2742356128,2.87074139528003));
#62097=CARTESIAN_POINT('Ctrl Pts',(6.39312958850154,-38.2742356128,2.91923000612405));
#62098=CARTESIAN_POINT('Ctrl Pts',(6.42599242410214,-38.2742356128005,2.96646286247323));
#62099=CARTESIAN_POINT('Ctrl Pts',(6.46053080560081,-38.274235612799,3.01241529465755));
#62100=CARTESIAN_POINT('Ctrl Pts',(6.49461335324637,-38.2742356127974,3.05776125157252));
#62101=CARTESIAN_POINT('Ctrl Pts',(6.53032758958246,-38.2742356127949,3.10186048887922));
#62102=CARTESIAN_POINT('Ctrl Pts',(6.56761546044982,-38.274235612774,3.1446555715695));
#62103=CARTESIAN_POINT('Ctrl Pts',(6.60490333131718,-38.274235612753,3.18745065425978));
#62104=CARTESIAN_POINT('Ctrl Pts',(6.64376481920528,-38.2742356127153,3.22894179606692));
#62105=CARTESIAN_POINT('Ctrl Pts',(6.68417908704671,-38.2742356126072,3.26903493627089));
#62106=CARTESIAN_POINT('Ctrl Pts',(6.72499216754563,-38.2742356124981,3.30952372020778));
#62107=CARTESIAN_POINT('Ctrl Pts',(6.76739214163738,-38.2742356125106,3.34859605472038));
#62108=CARTESIAN_POINT('Ctrl Pts',(6.81138643758061,-38.2742356125827,3.38610169378874));
#62109=CARTESIAN_POINT('Ctrl Pts',(6.85538073352383,-38.2742356126549,3.4236073328571));
#62110=CARTESIAN_POINT('Ctrl Pts',(6.90096932910499,-38.2742356127469,3.45954646193985));
#62111=CARTESIAN_POINT('Ctrl Pts',(6.94819533003811,-38.2742356127783,3.49372702645337));
#62112=CARTESIAN_POINT('Ctrl Pts',(6.99542200208882,-38.2742356128096,3.52790807669885));
#62113=CARTESIAN_POINT('Ctrl Pts',(7.04429746417697,-38.2742356128,3.56033518713764));
#62114=CARTESIAN_POINT('Ctrl Pts',(7.09483438027948,-38.2742356128,3.59073893044824));
#62115=CARTESIAN_POINT('Ctrl Pts',(7.12010478766847,-38.2742356128,3.60594197485347));
#62116=CARTESIAN_POINT('Ctrl Pts',(7.1457927882084,-38.2742356128,3.62063995899852));
#62117=CARTESIAN_POINT('Ctrl Pts',(7.17190833253584,-38.2742356128,3.63479573700106));
#62118=CARTESIAN_POINT('Ctrl Pts',(7.21559274834165,-38.2742356128,3.65847461899427));
#62119=CARTESIAN_POINT('Ctrl Pts',(7.26049747083368,-38.2742356128,3.68064523031944));
#62120=CARTESIAN_POINT('Ctrl Pts',(7.30649486896597,-38.2742356128,3.70105528680162));
#62121=CARTESIAN_POINT('Ctrl Pts',(7.35087125777577,-38.2742356128,3.72074606582086));
#62122=CARTESIAN_POINT('Ctrl Pts',(7.3962665568332,-38.2742356128,3.73879895785097));
#62123=CARTESIAN_POINT('Ctrl Pts',(7.44252054843875,-38.2742356128,3.75500665859511));
#62124=CARTESIAN_POINT('Ctrl Pts',(7.49474913383961,-38.2742356128,3.77330789602529));
#62125=CARTESIAN_POINT('Ctrl Pts',(7.54806637498204,-38.2742356128,3.78925398043707));
#62126=CARTESIAN_POINT('Ctrl Pts',(7.60222777550352,-38.2742356128,3.80259777613426));
#62127=CARTESIAN_POINT('Ctrl Pts',(7.63544961672591,-38.2742356128,3.81078267271537));
#62128=CARTESIAN_POINT('Ctrl Pts',(7.66898820965766,-38.2742356128,3.81798915253491));
#62129=CARTESIAN_POINT('Ctrl Pts',(7.70277859341121,-38.2742356128,3.82416796478963));
#62130=CARTESIAN_POINT('Ctrl Pts',(7.72631962642329,-38.2742356128,3.82847261028655));
#62131=CARTESIAN_POINT('Ctrl Pts',(7.74998525345287,-38.2742356128,3.83227917534982));
#62132=CARTESIAN_POINT('Ctrl Pts',(7.77376022135309,-38.2742356128,3.83557357412904));
#62133=CARTESIAN_POINT('Ctrl Pts',(7.82237592899862,-38.2742356128,3.84231005127553));
#62134=CARTESIAN_POINT('Ctrl Pts',(7.87143743462109,-38.2742356128,3.84689957799316));
#62135=CARTESIAN_POINT('Ctrl Pts',(7.9207084710963,-38.2742356128,3.84923698483134));
#62136=CARTESIAN_POINT('Ctrl Pts',(7.96871304847685,-38.2742356128,3.85151431113621));
#62137=CARTESIAN_POINT('Ctrl Pts',(8.01691594294803,-38.2742356128,3.85165340893818));
#62138=CARTESIAN_POINT('Ctrl Pts',(8.06508596156888,-38.2742356128,3.84960442308835));
#62139=CARTESIAN_POINT('Ctrl Pts',(8.11160303203354,-38.2742356128,3.84762574793133));
#62140=CARTESIAN_POINT('Ctrl Pts',(8.15808896531939,-38.2742356128,3.84360638048735));
#62141=CARTESIAN_POINT('Ctrl Pts',(8.20433122212088,-38.2742356128,3.83755036990893));
#62142=CARTESIAN_POINT('Ctrl Pts',(8.21146146922977,-38.2742356128,3.83661657353079));
#62143=CARTESIAN_POINT('Ctrl Pts',(8.21858592202528,-38.2742356128,3.83563445576886));
#62144=CARTESIAN_POINT('Ctrl Pts',(8.22570380264635,-38.2742356128,3.83460414414139));
#62145=CARTESIAN_POINT('Ctrl Pts',(8.26916917773586,-38.2742356128,3.82831254082139));
#62146=CARTESIAN_POINT('Ctrl Pts',(8.31238904500106,-38.2742356128,3.82022080412619));
#62147=CARTESIAN_POINT('Ctrl Pts',(8.35515073174464,-38.2742356128,3.8103893337697));
#62148=CARTESIAN_POINT('Ctrl Pts',(8.39587250007142,-38.2742356128,3.80102686730364));
#62149=CARTESIAN_POINT('Ctrl Pts',(8.43617935502698,-38.2742356128,3.79008717922198));
#62150=CARTESIAN_POINT('Ctrl Pts',(8.47592446037656,-38.2742356128,3.77764625378023));
#62151=CARTESIAN_POINT('Ctrl Pts',(8.51817884137633,-38.2742356128,3.76441988039459));
#62152=CARTESIAN_POINT('Ctrl Pts',(8.55978146889371,-38.2742356128,3.7495011054138));
#62153=CARTESIAN_POINT('Ctrl Pts',(8.6005665880081,-38.2742356128,3.73302424017688));
#62154=CARTESIAN_POINT('Ctrl Pts',(8.63470715191798,-38.2742356128,3.71923172263934));
#62155=CARTESIAN_POINT('Ctrl Pts',(8.66827574390385,-38.2742356128,3.70434819246818));
#62156=CARTESIAN_POINT('Ctrl Pts',(8.70119857853243,-38.2742356128,3.68846751861937));
#62157=CARTESIAN_POINT('Ctrl Pts',(8.73601365099068,-38.2742356128,3.67167410404952));
#62158=CARTESIAN_POINT('Ctrl Pts',(8.77011496511053,-38.2742356128,3.65376173724068));
#62159=CARTESIAN_POINT('Ctrl Pts',(8.80344116958025,-38.2742356128,3.63485089925167));
#62160=CARTESIAN_POINT('Ctrl Pts',(8.83063668774854,-38.2742356128,3.61941889772942));
#62161=CARTESIAN_POINT('Ctrl Pts',(8.85731345058671,-38.2742356128,3.60332407304967));
#62162=CARTESIAN_POINT('Ctrl Pts',(8.88345088080642,-38.2742356128,3.58663584779668));
#62163=CARTESIAN_POINT('Ctrl Pts',(8.9259593054728,-38.2742356128,3.55949507075703));
#62164=CARTESIAN_POINT('Ctrl Pts',(8.96705449595305,-38.2742356128,3.53077491258169));
#62165=CARTESIAN_POINT('Ctrl Pts',(9.00671405321108,-38.2742356128,3.50076505793843));
#62166=CARTESIAN_POINT('Ctrl Pts',(9.02448445149716,-38.2742356128,3.48731843608009));
#62167=CARTESIAN_POINT('Ctrl Pts',(9.0419679384425,-38.2742356128,3.47361257263251));
#62168=CARTESIAN_POINT('Ctrl Pts',(9.05917102804987,-38.2742356128,3.45966884100842));
#62169=CARTESIAN_POINT('Ctrl Pts',(9.09613287534507,-38.2742356128,3.42970991556087));
#62170=CARTESIAN_POINT('Ctrl Pts',(9.13178298861802,-38.2742356128,3.39866330865085));
#62171=CARTESIAN_POINT('Ctrl Pts',(9.16610497039632,-38.2742356128,3.36683543275146));
#62172=CARTESIAN_POINT('Ctrl Pts',(9.19617038556613,-38.2742356128,3.33895480776106));
#62173=CARTESIAN_POINT('Ctrl Pts',(9.22522040844852,-38.2742356128,3.31047255605014));
#62174=CARTESIAN_POINT('Ctrl Pts',(9.2532655075239,-38.2742356128,3.28159842813157));
#62175=CARTESIAN_POINT('Ctrl Pts',(9.26335772601788,-38.2742356128,3.27120787800393));
#62176=CARTESIAN_POINT('Ctrl Pts',(9.27331759521306,-38.2742356128,3.26076909600295));
#62177=CARTESIAN_POINT('Ctrl Pts',(9.28315033923572,-38.2742356128,3.25028745674481));
#62178=CARTESIAN_POINT('Ctrl Pts',(9.28944952698189,-38.2742356128,3.24357256480595));
#62179=CARTESIAN_POINT('Ctrl Pts',(9.29569777098763,-38.2742356128,3.23683882068643));
#62180=CARTESIAN_POINT('Ctrl Pts',(9.30190371288055,-38.2742356128,3.23007938120359));
#62181=CARTESIAN_POINT('Ctrl Pts',(9.33233023873494,-38.2742356128,3.19693916433808));
#62182=CARTESIAN_POINT('Ctrl Pts',(9.36168036792281,-38.2742356128,3.163242504528));
#62183=CARTESIAN_POINT('Ctrl Pts',(9.38997095611936,-38.2742356128,3.12926408303275));
#62184=CARTESIAN_POINT('Ctrl Pts',(9.4175861925723,-38.2742356128,3.09609679300081));
#62185=CARTESIAN_POINT('Ctrl Pts',(9.44419272126028,-38.2742356128,3.06266214394091));
#62186=CARTESIAN_POINT('Ctrl Pts',(9.46984227971996,-38.2742356128,3.0291824106293));
#62187=CARTESIAN_POINT('Ctrl Pts',(9.48358594054153,-38.2742356128,3.01124315059272));
#62188=CARTESIAN_POINT('Ctrl Pts',(9.49705539415298,-38.2742356128,2.99329026953402));
#62189=CARTESIAN_POINT('Ctrl Pts',(9.51026170167303,-38.2742356128,2.97535239382229));
#62190=CARTESIAN_POINT('Ctrl Pts',(9.52286799378051,-38.2742356128,2.95822950760549));
#62191=CARTESIAN_POINT('Ctrl Pts',(9.53522797161959,-38.2742356128,2.94113004374477));
#62192=CARTESIAN_POINT('Ctrl Pts',(9.54740400575136,-38.2742356128,2.92400110327784));
#62193=CARTESIAN_POINT('Ctrl Pts',(9.56979774633823,-38.2742356128,2.89249814876958));
#62194=CARTESIAN_POINT('Ctrl Pts',(9.59154723077383,-38.2742356128,2.86092587153871));
#62195=CARTESIAN_POINT('Ctrl Pts',(9.61272092465214,-38.2742356128,2.82935643568641));
#62196=CARTESIAN_POINT('Ctrl Pts',(9.63294559994359,-38.2742356128,2.79920196226685));
#62197=CARTESIAN_POINT('Ctrl Pts',(9.65264538214872,-38.2742356128,2.76905020393921));
#62198=CARTESIAN_POINT('Ctrl Pts',(9.67188544590519,-38.2742356128,2.73891828907923));
#62199=CARTESIAN_POINT('Ctrl Pts',(9.68150547778342,-38.2742356128,2.72385233164924));
#62200=CARTESIAN_POINT('Ctrl Pts',(9.69101062804654,-38.2742356128,2.7087905913421));
#62201=CARTESIAN_POINT('Ctrl Pts',(9.70040909814045,-38.2742356128,2.69373054093805));
#62202=CARTESIAN_POINT('Ctrl Pts',(9.70510833318741,-38.2742356128,2.68620051573602));
#62203=CARTESIAN_POINT('Ctrl Pts',(9.70978089686981,-38.2742356128,2.67867086274479));
#62204=CARTESIAN_POINT('Ctrl Pts',(9.71442779933124,-38.2742356128,2.67114095997344));
#62205=CARTESIAN_POINT('Ctrl Pts',(9.71734973513711,-38.2742356128,2.66640621619413));
#62206=CARTESIAN_POINT('Ctrl Pts',(9.72026152477054,-38.2742356128,2.66167136955722));
#62207=CARTESIAN_POINT('Ctrl Pts',(9.72316341608076,-38.2742356128,2.65693622339584));
#62208=CARTESIAN_POINT('Ctrl Pts',(9.7248765494556,-38.2742356128,2.65414082685731));
#62209=CARTESIAN_POINT('Ctrl Pts',(9.72658528778543,-38.2742356128,2.65134687498826));
#62210=CARTESIAN_POINT('Ctrl Pts',(9.72829290598,-38.2742356128,2.64854903634));
#62211=CARTESIAN_POINT('Ctrl Pts',(9.72829290598,-38.2742356128,2.64854903634));
#62212=CARTESIAN_POINT('Ctrl Pts',(9.73633081950354,-38.2742356128,2.63537941280583));
#62213=CARTESIAN_POINT('Ctrl Pts',(9.74437282162921,-38.2742356128,2.62207734293453));
#62214=CARTESIAN_POINT('Ctrl Pts',(9.75239609347846,-38.2742356128,2.60866170311115));
#62215=CARTESIAN_POINT('Ctrl Pts',(9.7706178726226,-38.2742356128,2.57819323207684));
#62216=CARTESIAN_POINT('Ctrl Pts',(9.78873121305153,-38.2742356128045,2.54715338833482));
#62217=CARTESIAN_POINT('Ctrl Pts',(9.80656454330723,-38.2742356127903,2.51565633011237));
#62218=CARTESIAN_POINT('Ctrl Pts',(9.82522540644807,-38.2742356127755,2.48269769118174));
#62219=CARTESIAN_POINT('Ctrl Pts',(9.84357974189825,-38.2742356127495,2.44923836084657));
#62220=CARTESIAN_POINT('Ctrl Pts',(9.8614863558543,-38.2742356125523,2.41538824559926));
#62221=CARTESIAN_POINT('Ctrl Pts',(9.87920707925459,-38.2742356123572,2.38188953217205));
#62222=CARTESIAN_POINT('Ctrl Pts',(9.89648992214151,-38.2742356120062,2.34800784985536));
#62223=CARTESIAN_POINT('Ctrl Pts',(9.91324521507938,-38.2742356110565,2.31383240769414));
#62224=CARTESIAN_POINT('Ctrl Pts',(9.93224345730128,-38.2742356099796,2.27508206589903));
#62225=CARTESIAN_POINT('Ctrl Pts',(9.95057689163532,-38.2742356082693,2.2359335436681));
#62226=CARTESIAN_POINT('Ctrl Pts',(9.96819415283343,-38.2742356072486,2.19645698119026));
#62227=CARTESIAN_POINT('Ctrl Pts',(9.97735837586944,-38.2742356067177,2.17592189238311));
#62228=CARTESIAN_POINT('Ctrl Pts',(9.98632969007421,-38.2742356064057,2.15529765960282));
#62229=CARTESIAN_POINT('Ctrl Pts',(9.99510586294375,-38.2742356065093,2.13459208982059));
#62230=CARTESIAN_POINT('Ctrl Pts',(10.007929849719,-38.2742356066606,2.10433653799763));
#62231=CARTESIAN_POINT('Ctrl Pts',(10.0203432583176,-38.2742356075538,2.07388879803855));
#62232=CARTESIAN_POINT('Ctrl Pts',(10.032324733776,-38.2742356086601,2.04332373370437));
#62233=CARTESIAN_POINT('Ctrl Pts',(10.0443062092338,-38.2742356097665,2.01275866937166));
#62234=CARTESIAN_POINT('Ctrl Pts',(10.0558513452567,-38.2742356112677,1.98209385668015));
#62235=CARTESIAN_POINT('Ctrl Pts',(10.0669588760154,-38.2742356120342,1.95138103326328));
#62236=CARTESIAN_POINT('Ctrl Pts',(10.0891452831127,-38.2742356135653,1.89003461719298));
#62237=CARTESIAN_POINT('Ctrl Pts',(10.1095692104436,-38.2742356128,1.82848655467785));
#62238=CARTESIAN_POINT('Ctrl Pts',(10.128456408996,-38.2742356128,1.76681870077139));
#62239=CARTESIAN_POINT('Ctrl Pts',(10.1379001404091,-38.2742356128,1.73598434238294));
#62240=CARTESIAN_POINT('Ctrl Pts',(10.14696167855,-38.2742356128,1.70511412639515));
#62241=CARTESIAN_POINT('Ctrl Pts',(10.1556583365498,-38.2742356128,1.67424279728339));
#62242=CARTESIAN_POINT('Ctrl Pts',(10.16435499455,-38.2742356128,1.64337146817015));
#62243=CARTESIAN_POINT('Ctrl Pts',(10.1726823665861,-38.2742356128,1.61251259232094));
#62244=CARTESIAN_POINT('Ctrl Pts',(10.1806640744349,-38.2742356128,1.58173198537152));
#62245=CARTESIAN_POINT('Ctrl Pts',(10.1922325743438,-38.2742356128,1.53711929652927));
#62246=CARTESIAN_POINT('Ctrl Pts',(10.203080052512,-38.2742356128,1.49265202704484));
#62247=CARTESIAN_POINT('Ctrl Pts',(10.2133104720004,-38.2742356128,1.44845116652768));
#62248=CARTESIAN_POINT('Ctrl Pts',(10.2231958315931,-38.2742356128,1.40574114852592));
#62249=CARTESIAN_POINT('Ctrl Pts',(10.2325058502182,-38.2742356128,1.36328013780716));
#62250=CARTESIAN_POINT('Ctrl Pts',(10.2413469161846,-38.2742356128,1.32113143513957));
#62251=CARTESIAN_POINT('Ctrl Pts',(10.248425021219,-38.2742356128,1.28738743349139));
#62252=CARTESIAN_POINT('Ctrl Pts',(10.2552029211007,-38.2742356128,1.25384284282264));
#62253=CARTESIAN_POINT('Ctrl Pts',(10.2617364169019,-38.2742356128,1.22050596333499));
#62254=CARTESIAN_POINT('Ctrl Pts',(10.2694791647119,-38.2742356128,1.18099892782147));
#62255=CARTESIAN_POINT('Ctrl Pts',(10.2768783835795,-38.2742356128,1.14178928445506));
#62256=CARTESIAN_POINT('Ctrl Pts',(10.2840216413865,-38.2742356128,1.10284902512591));
#62257=CARTESIAN_POINT('Ctrl Pts',(10.2908559963421,-38.2742356128,1.06559269733981));
#62258=CARTESIAN_POINT('Ctrl Pts',(10.2974564253937,-38.2742356128,1.02858294877892));
#62259=CARTESIAN_POINT('Ctrl Pts',(10.3038885583826,-38.2742356128,0.991749116652807));
#62260=CARTESIAN_POINT('Ctrl Pts',(10.310175485487,-38.2742356128,0.955746811048525));
#62261=CARTESIAN_POINT('Ctrl Pts',(10.3163019642676,-38.2742356128,0.919912681263671));
#62262=CARTESIAN_POINT('Ctrl Pts',(10.3223133025257,-38.2742356128,0.884134704814115));
#62263=CARTESIAN_POINT('Ctrl Pts',(10.3281353526992,-38.2742356128,0.849483323531461));
#62264=CARTESIAN_POINT('Ctrl Pts',(10.3338496369459,-38.2742356128,0.814884622669424));
#62265=CARTESIAN_POINT('Ctrl Pts',(10.3394780744938,-38.2742356128,0.780192405435676));
#62266=CARTESIAN_POINT('Ctrl Pts',(10.3433361101194,-38.2742356128,0.756412482698574));
#62267=CARTESIAN_POINT('Ctrl Pts',(10.3471534165005,-38.2742356128,0.73258771295533));
#62268=CARTESIAN_POINT('Ctrl Pts',(10.3509307018976,-38.2742356128,0.708658267877187));
#62269=CARTESIAN_POINT('Ctrl Pts',(10.3517926022542,-38.2742356128,0.703198051061031));
#62270=CARTESIAN_POINT('Ctrl Pts',(10.3526516477296,-38.2742356128,0.697737184145745));
#62271=CARTESIAN_POINT('Ctrl Pts',(10.3535092619,-38.2742356128,0.692265445118));
#62272=CARTESIAN_POINT('',(-2.11954040870134,-38.2742356128,-9.31090046842523));
#62273=CARTESIAN_POINT('',(-10.3535102065,-38.2742356128,0.692259352582));
#62274=CARTESIAN_POINT('Ctrl Pts',(-2.119540611027,-38.2742356128,-9.31090043155947));
#62275=CARTESIAN_POINT('Ctrl Pts',(-2.13364472791917,-38.2742356128,-9.3083306064183));
#62276=CARTESIAN_POINT('Ctrl Pts',(-2.14773674018183,-38.2742356128,-9.30573625661834));
#62277=CARTESIAN_POINT('Ctrl Pts',(-2.16182796614952,-38.2742356128,-9.30311552892601));
#62278=CARTESIAN_POINT('Ctrl Pts',(-2.32376865139767,-38.2742356127999,
-9.27299732350397));
#62279=CARTESIAN_POINT('Ctrl Pts',(-2.48495687112191,-38.2742356127996,
-9.239499459851));
#62280=CARTESIAN_POINT('Ctrl Pts',(-2.64515420185416,-38.2742356127995,
-9.20256165403099));
#62281=CARTESIAN_POINT('Ctrl Pts',(-2.80768594553618,-38.2742356127993,
-9.16508558648185));
#62282=CARTESIAN_POINT('Ctrl Pts',(-2.96919808080522,-38.2742356127992,
-9.12406802380528));
#62283=CARTESIAN_POINT('Ctrl Pts',(-3.1294916921194,-38.2742356127992,-9.07946595465591));
#62284=CARTESIAN_POINT('Ctrl Pts',(-3.29639584579064,-38.2742356127992,
-9.03302448676254));
#62285=CARTESIAN_POINT('Ctrl Pts',(-3.46197915083997,-38.2742356127993,
-8.98269593782396));
#62286=CARTESIAN_POINT('Ctrl Pts',(-3.62606644740541,-38.2742356127994,
-8.92846416277601));
#62287=CARTESIAN_POINT('Ctrl Pts',(-3.78404198900947,-38.2742356127996,
-8.87625235714162));
#62288=CARTESIAN_POINT('Ctrl Pts',(-3.94063166288899,-38.2742356127997,
-8.82042234815021));
#62289=CARTESIAN_POINT('Ctrl Pts',(-4.09571540570172,-38.2742356127998,
-8.76099703017426));
#62290=CARTESIAN_POINT('Ctrl Pts',(-4.24910473352082,-38.2742356127999,
-8.70222098173459));
#62291=CARTESIAN_POINT('Ctrl Pts',(-4.40102139726561,-38.2742356127999,
-8.63992732111316));
#62292=CARTESIAN_POINT('Ctrl Pts',(-4.55137602984186,-38.2742356128,-8.57418123317398));
#62293=CARTESIAN_POINT('Ctrl Pts',(-4.69850394264876,-38.2742356128,-8.50984610409968));
#62294=CARTESIAN_POINT('Ctrl Pts',(-4.84413666293673,-38.2742356128,-8.4422048415258));
#62295=CARTESIAN_POINT('Ctrl Pts',(-4.98820847473103,-38.2742356128,-8.37136522774251));
#62296=CARTESIAN_POINT('Ctrl Pts',(-5.01189799059617,-38.2742356128,-8.35971717436067));
#62297=CARTESIAN_POINT('Ctrl Pts',(-5.03554533520149,-38.2742356128,-8.34798275813522));
#62298=CARTESIAN_POINT('Ctrl Pts',(-5.05915024982113,-38.2742356128,-8.33616259113913));
#62299=CARTESIAN_POINT('Ctrl Pts',(-5.19613226349434,-38.2742356128,-8.26756881297181));
#62300=CARTESIAN_POINT('Ctrl Pts',(-5.33169516861775,-38.2742356128,-8.19607801844391));
#62301=CARTESIAN_POINT('Ctrl Pts',(-5.46577814671631,-38.2742356128,-8.12182944272581));
#62302=CARTESIAN_POINT('Ctrl Pts',(-5.61311054623041,-38.2742356128,-8.04024398738926));
#62303=CARTESIAN_POINT('Ctrl Pts',(-5.75865383549873,-38.2742356128,-7.95533085578545));
#62304=CARTESIAN_POINT('Ctrl Pts',(-5.90234076261512,-38.2742356128,-7.86732671859547));
#62305=CARTESIAN_POINT('Ctrl Pts',(-6.02299132476987,-38.2742356128,-7.79343169671003));
#62306=CARTESIAN_POINT('Ctrl Pts',(-6.14232928483772,-38.2742356128,-7.71736146010781));
#62307=CARTESIAN_POINT('Ctrl Pts',(-6.26035030960864,-38.2742356128,-7.63925451488464));
#62308=CARTESIAN_POINT('Ctrl Pts',(-6.37527408486149,-38.2742356128,-7.56319734595277));
#62309=CARTESIAN_POINT('Ctrl Pts',(-6.4889488059138,-38.2742356128,-7.48520986313824));
#62310=CARTESIAN_POINT('Ctrl Pts',(-6.60140601560954,-38.2742356128,-7.40540258312093));
#62311=CARTESIAN_POINT('Ctrl Pts',(-6.65006200218209,-38.2742356128,-7.37087298777154));
#62312=CARTESIAN_POINT('Ctrl Pts',(-6.69849058187879,-38.2742356128,-7.33600241844901));
#62313=CARTESIAN_POINT('Ctrl Pts',(-6.74669690172057,-38.2742356128,-7.30079801871046));
#62314=CARTESIAN_POINT('Ctrl Pts',(-6.82975104074592,-38.2742356128,-7.24014474503625));
#62315=CARTESIAN_POINT('Ctrl Pts',(-6.9121479426546,-38.2742356128,-7.17849976034897));
#62316=CARTESIAN_POINT('Ctrl Pts',(-6.99396258843833,-38.2742356128,-7.11583561689136));
#62317=CARTESIAN_POINT('Ctrl Pts',(-7.03977098542883,-38.2742356128,-7.08074967435529));
#62318=CARTESIAN_POINT('Ctrl Pts',(-7.0853959556089,-38.2742356128,-7.04534466400566));
#62319=CARTESIAN_POINT('Ctrl Pts',(-7.13084411519291,-38.2742356128,-7.00961848116238));
#62320=CARTESIAN_POINT('Ctrl Pts',(-7.17503106878152,-38.2742356128,-6.97488371527431));
#62321=CARTESIAN_POINT('Ctrl Pts',(-7.21905664702566,-38.2742356128,-6.93984085852948));
#62322=CARTESIAN_POINT('Ctrl Pts',(-7.26292627354035,-38.2742356128,-6.90448613736163));
#62323=CARTESIAN_POINT('Ctrl Pts',(-7.35159910518294,-38.2742356128,-6.83302431999608));
#62324=CARTESIAN_POINT('Ctrl Pts',(-7.43963202886674,-38.2742356128,-6.76029286715303));
#62325=CARTESIAN_POINT('Ctrl Pts',(-7.52698205911756,-38.2742356128,-6.68630420512345));
#62326=CARTESIAN_POINT('Ctrl Pts',(-7.61357936644008,-38.2742356128,-6.61295312687243));
#62327=CARTESIAN_POINT('Ctrl Pts',(-7.699504982201,-38.2742356128,-6.53836760366721));
#62328=CARTESIAN_POINT('Ctrl Pts',(-7.78468609109267,-38.2742356128,-6.46254133509157));
#62329=CARTESIAN_POINT('Ctrl Pts',(-7.87064681191647,-38.2742356128,-6.38602107386287));
#62330=CARTESIAN_POINT('Ctrl Pts',(-7.95584901699601,-38.2742356128,-6.30823809256242));
#62331=CARTESIAN_POINT('Ctrl Pts',(-8.04016575030431,-38.2742356128,-6.22917475735306));
#62332=CARTESIAN_POINT('Ctrl Pts',(-8.12178277687235,-38.2742356128,-6.15264292224573));
#62333=CARTESIAN_POINT('Ctrl Pts',(-8.20256954986649,-38.2742356128,-6.07491203715707));
#62334=CARTESIAN_POINT('Ctrl Pts',(-8.28236940693681,-38.2742356128,-5.99594511180924));
#62335=CARTESIAN_POINT('Ctrl Pts',(-8.35550578536951,-38.2742356128,-5.92357211331106));
#62336=CARTESIAN_POINT('Ctrl Pts',(-8.4278174655938,-38.2742356128084,-5.85015814590171));
#62337=CARTESIAN_POINT('Ctrl Pts',(-8.49920181258907,-38.2742356127916,
-5.77567763240077));
#62338=CARTESIAN_POINT('Ctrl Pts',(-8.57629785140191,-38.2742356127735,
-5.69523769281501));
#62339=CARTESIAN_POINT('Ctrl Pts',(-8.65231208372804,-38.2742356128263,
-5.61355320700452));
#62340=CARTESIAN_POINT('Ctrl Pts',(-8.72705743520762,-38.2742356121211,
-5.53056955773554));
#62341=CARTESIAN_POINT('Ctrl Pts',(-8.75811629125898,-38.274235611828,-5.49608745060457));
#62342=CARTESIAN_POINT('Ctrl Pts',(-8.78895542105945,-38.2742356113856,
-5.46138081859757));
#62343=CARTESIAN_POINT('Ctrl Pts',(-8.81955894353799,-38.2742356106072,
-5.42644509309065));
#62344=CARTESIAN_POINT('Ctrl Pts',(-8.90083523945013,-38.2742356085398,
-5.33366340868826));
#62345=CARTESIAN_POINT('Ctrl Pts',(-8.98046977411646,-38.2742356029034,
-5.23924732892919));
#62346=CARTESIAN_POINT('Ctrl Pts',(-9.05817344688913,-38.2742355974438,
-5.14307642848394));
#62347=CARTESIAN_POINT('Ctrl Pts',(-9.14533591774263,-38.2742355913196,
-5.03519873097103));
#62348=CARTESIAN_POINT('Ctrl Pts',(-9.23006783067603,-38.2742355884836,
-4.92511093215123));
#62349=CARTESIAN_POINT('Ctrl Pts',(-9.31189953927549,-38.2742355969756,
-4.81264955992679));
#62350=CARTESIAN_POINT('Ctrl Pts',(-9.38468149790253,-38.2742356045285,
-4.71262526518252));
#62351=CARTESIAN_POINT('Ctrl Pts',(-9.45510686120649,-38.2742356077932,
-4.61074833045805));
#62352=CARTESIAN_POINT('Ctrl Pts',(-9.52280503538855,-38.2742356097278,
-4.5069508612583));
#62353=CARTESIAN_POINT('Ctrl Pts',(-9.58549262089299,-38.2742356115191,
-4.4108358211672));
#62354=CARTESIAN_POINT('Ctrl Pts',(-9.64584072223927,-38.2742356120949,
-4.31307350300637));
#62355=CARTESIAN_POINT('Ctrl Pts',(-9.70356017216965,-38.274235612415,-4.21364954117544));
#62356=CARTESIAN_POINT('Ctrl Pts',(-9.75795283707027,-38.2742356127166,
-4.11995609389752));
#62357=CARTESIAN_POINT('Ctrl Pts',(-9.81001048715776,-38.2742356127563,
-4.02478670142455));
#62358=CARTESIAN_POINT('Ctrl Pts',(-9.85950734173672,-38.2742356127813,
-3.92817163468304));
#62359=CARTESIAN_POINT('Ctrl Pts',(-9.90588532561234,-38.2742356128046,
-3.83764442753836));
#62360=CARTESIAN_POINT('Ctrl Pts',(-9.95001471143252,-38.2742356127998,
-3.74584789685752));
#62361=CARTESIAN_POINT('Ctrl Pts',(-9.99173117763725,-38.2742356128,-3.65284794031525));
#62362=CARTESIAN_POINT('Ctrl Pts',(-10.0066488616391,-38.2742356128,-3.61959143299102));
#62363=CARTESIAN_POINT('Ctrl Pts',(-10.0212582251145,-38.2742356128,-3.58618144349341));
#62364=CARTESIAN_POINT('Ctrl Pts',(-10.0355526046835,-38.2742356128,-3.552622411423));
#62365=CARTESIAN_POINT('Ctrl Pts',(-10.0741195067863,-38.2742356128,-3.46207857926293));
#62366=CARTESIAN_POINT('Ctrl Pts',(-10.1103924680514,-38.2742356128,-3.37044307950816));
#62367=CARTESIAN_POINT('Ctrl Pts',(-10.144251066512,-38.2742356128,-3.27786011867359));
#62368=CARTESIAN_POINT('Ctrl Pts',(-10.175727743706,-38.2742356128,-3.19179028399764));
#62369=CARTESIAN_POINT('Ctrl Pts',(-10.2051178215566,-38.2742356128,-3.10490182707557));
#62370=CARTESIAN_POINT('Ctrl Pts',(-10.2323555261849,-38.2742356128,-3.01735062523928));
#62371=CARTESIAN_POINT('Ctrl Pts',(-10.2344166734751,-38.2742356128,-3.01072540021072));
#62372=CARTESIAN_POINT('Ctrl Pts',(-10.2364655111735,-38.2742356128,-3.00409639946743));
#62373=CARTESIAN_POINT('Ctrl Pts',(-10.2385020185954,-38.2742356128,-2.99746370018176));
#62374=CARTESIAN_POINT('Ctrl Pts',(-10.2652522054426,-38.2742356128,-2.91034103945238));
#62375=CARTESIAN_POINT('Ctrl Pts',(-10.289883505425,-38.2742356128,-2.82254091265382));
#62376=CARTESIAN_POINT('Ctrl Pts',(-10.31239561938,-38.2742356128,-2.7342474625325));
#62377=CARTESIAN_POINT('Ctrl Pts',(-10.3357459688454,-38.2742356128,-2.64266641776911));
#62378=CARTESIAN_POINT('Ctrl Pts',(-10.3568166272029,-38.2742356128,-2.55055473011936));
#62379=CARTESIAN_POINT('Ctrl Pts',(-10.3756579174403,-38.2742356128,-2.45809496166693));
#62380=CARTESIAN_POINT('Ctrl Pts',(-10.3779672486567,-38.2742356128,-2.44676239224857));
#62381=CARTESIAN_POINT('Ctrl Pts',(-10.3802431458191,-38.2742356128,-2.43542456529753));
#62382=CARTESIAN_POINT('Ctrl Pts',(-10.3824857483227,-38.2742356128,-2.42408179326659));
#62383=CARTESIAN_POINT('Ctrl Pts',(-10.4015615745755,-38.2742356128,-2.3275989131542));
#62384=CARTESIAN_POINT('Ctrl Pts',(-10.4182263197844,-38.2742356132236,
-2.23074979392517));
#62385=CARTESIAN_POINT('Ctrl Pts',(-10.4325715436647,-38.2742356123768,
-2.13373877808311));
#62386=CARTESIAN_POINT('Ctrl Pts',(-10.4384491467123,-38.2742356120298,
-2.09399089773411));
#62387=CARTESIAN_POINT('Ctrl Pts',(-10.4439379332837,-38.2742356114086,
-2.05421557115579));
#62388=CARTESIAN_POINT('Ctrl Pts',(-10.4490464009529,-38.2742356094761,
-2.01442572807813));
#62389=CARTESIAN_POINT('Ctrl Pts',(-10.4624519394082,-38.2742356044048,
-1.91001001948507));
#62390=CARTESIAN_POINT('Ctrl Pts',(-10.4732528313444,-38.2742355890201,
-1.80547263371963));
#62391=CARTESIAN_POINT('Ctrl Pts',(-10.4816751574859,-38.2742355691515,
-1.70099454498701));
#62392=CARTESIAN_POINT('Ctrl Pts',(-10.4842956528958,-38.2742355629696,
-1.66848756919981));
#62393=CARTESIAN_POINT('Ctrl Pts',(-10.4866861639936,-38.2742355566081,
-1.63598605690851));
#62394=CARTESIAN_POINT('Ctrl Pts',(-10.4888541645596,-38.2742355508364,
-1.6034947186437));
#62395=CARTESIAN_POINT('Ctrl Pts',(-10.4966767706617,-38.2742355300108,
-1.48625907536859));
#62396=CARTESIAN_POINT('Ctrl Pts',(-10.5016038327303,-38.2742355215113,
-1.36916012272759));
#62397=CARTESIAN_POINT('Ctrl Pts',(-10.5039692096414,-38.2742355269209,
-1.25235963069119));
#62398=CARTESIAN_POINT('Ctrl Pts',(-10.5063926047028,-38.2742355324631,
-1.13269424703444));
#62399=CARTESIAN_POINT('Ctrl Pts',(-10.5061290346563,-38.2742355509457,
-1.01334217949223));
#62400=CARTESIAN_POINT('Ctrl Pts',(-10.5035454403602,-38.2742355688688,
-0.894425537132182));
#62401=CARTESIAN_POINT('Ctrl Pts',(-10.5027611104684,-38.2742355743099,
-0.858324715351389));
#62402=CARTESIAN_POINT('Ctrl Pts',(-10.501762905098,-38.2742355796852,-0.822263666891019));
#62403=CARTESIAN_POINT('Ctrl Pts',(-10.5005608009666,-38.2742355846559,
-0.786244887924867));
#62404=CARTESIAN_POINT('Ctrl Pts',(-10.4969275725192,-38.2742355996795,
-0.677382062346776));
#62405=CARTESIAN_POINT('Ctrl Pts',(-10.4914181220826,-38.2742356052499,
-0.56887949337425));
#62406=CARTESIAN_POINT('Ctrl Pts',(-10.4842985290207,-38.274235608431,-0.46080570269692));
#62407=CARTESIAN_POINT('Ctrl Pts',(-10.4775343560835,-38.2742356114532,
-0.358127108041158));
#62408=CARTESIAN_POINT('Ctrl Pts',(-10.4693176834151,-38.2742356120957,
-0.255835196844215));
#62409=CARTESIAN_POINT('Ctrl Pts',(-10.4598437918636,-38.2742356124577,
-0.153959246988123));
#62410=CARTESIAN_POINT('Ctrl Pts',(-10.4508887624302,-38.2742356127998,
-0.0576627964168982));
#62411=CARTESIAN_POINT('Ctrl Pts',(-10.440810958642,-38.2742356127839,0.038262303108895));
#62412=CARTESIAN_POINT('Ctrl Pts',(-10.4297355589646,-38.2742356127946,
0.133813795867807));
#62413=CARTESIAN_POINT('Ctrl Pts',(-10.4186601592872,-38.2742356128053,
0.229365288626718));
#62414=CARTESIAN_POINT('Ctrl Pts',(-10.4065879660116,-38.2742356128,0.324543251269931));
#62415=CARTESIAN_POINT('Ctrl Pts',(-10.39359317545,-38.2742356128,0.419366129591117));
#62416=CARTESIAN_POINT('Ctrl Pts',(-10.3849069819887,-38.2742356128,0.482749210815547));
#62417=CARTESIAN_POINT('Ctrl Pts',(-10.3758063040751,-38.2742356128,0.545983232075174));
#62418=CARTESIAN_POINT('Ctrl Pts',(-10.3662947439406,-38.2742356128,0.60909237278372));
#62419=CARTESIAN_POINT('Ctrl Pts',(-10.3621130485487,-38.2742356128,0.636837894985739));
#62420=CARTESIAN_POINT('Ctrl Pts',(-10.3578515477501,-38.2742356128,0.664560643170705));
#62421=CARTESIAN_POINT('Ctrl Pts',(-10.3535102065,-38.2742356128,0.692259352582));
#62422=CARTESIAN_POINT('',(-9.72829242121,-38.2742356128,2.64854983337));
#62423=CARTESIAN_POINT('Ctrl Pts',(-10.3535102065,-38.2742356128,0.692259352582));
#62424=CARTESIAN_POINT('Ctrl Pts',(-10.348101240468,-38.2742356128,0.726769549321815));
#62425=CARTESIAN_POINT('Ctrl Pts',(-10.3426100454796,-38.2742356128,0.761029055591791));
#62426=CARTESIAN_POINT('Ctrl Pts',(-10.3370342145885,-38.2742356128,0.795218909178925));
#62427=CARTESIAN_POINT('Ctrl Pts',(-10.3312466866877,-38.2742356128,0.830706845492452));
#62428=CARTESIAN_POINT('Ctrl Pts',(-10.3253677818713,-38.2742356128,0.866119791080294));
#62429=CARTESIAN_POINT('Ctrl Pts',(-10.3193700787744,-38.2742356128,0.901609037191189));
#62430=CARTESIAN_POINT('Ctrl Pts',(-10.3132171268777,-38.2742356128,0.93801691211283));
#62431=CARTESIAN_POINT('Ctrl Pts',(-10.306938841305,-38.2742356128,0.974505008243299));
#62432=CARTESIAN_POINT('Ctrl Pts',(-10.3004839950347,-38.2742356128,1.01118418143873));
#62433=CARTESIAN_POINT('Ctrl Pts',(-10.2938473921693,-38.2742356128,1.04889617266743));
#62434=CARTESIAN_POINT('Ctrl Pts',(-10.2870237702254,-38.2742356128,1.08681005209566));
#62435=CARTESIAN_POINT('Ctrl Pts',(-10.2799401349208,-38.2742356128,1.12499289079426));
#62436=CARTESIAN_POINT('Ctrl Pts',(-10.2726428438253,-38.2742356128,1.16432739586815));
#62437=CARTESIAN_POINT('Ctrl Pts',(-10.2650691490111,-38.2742356128,1.20394719453697));
#62438=CARTESIAN_POINT('Ctrl Pts',(-10.2571276523262,-38.2742356128,1.24387150137696));
#62439=CARTESIAN_POINT('Ctrl Pts',(-10.2488260848449,-38.2742356128,1.28560599306385));
#62440=CARTESIAN_POINT('Ctrl Pts',(-10.2401219944262,-38.2742356128,1.32767315514082));
#62441=CARTESIAN_POINT('Ctrl Pts',(-10.2309068988015,-38.2742356128,1.37003813026781));
#62442=CARTESIAN_POINT('Ctrl Pts',(-10.2214777127999,-38.2742356128,1.41338735274933));
#62443=CARTESIAN_POINT('Ctrl Pts',(-10.211512734,-38.2742356128,1.45704802894355));
#62444=CARTESIAN_POINT('Ctrl Pts',(-10.2009022991903,-38.2742356128,1.50092829815079));
#62445=CARTESIAN_POINT('Ctrl Pts',(-10.1900848893554,-38.2742356128,1.54566452849331));
#62446=CARTESIAN_POINT('Ctrl Pts',(-10.1785957116405,-38.2742356128,1.59062853587755));
#62447=CARTESIAN_POINT('Ctrl Pts',(-10.166337985387,-38.2742356128,1.63567333892064));
#62448=CARTESIAN_POINT('Ctrl Pts',(-10.1651785470143,-38.2742356128,1.63993405351455));
#62449=CARTESIAN_POINT('Ctrl Pts',(-10.1640122525023,-38.2742356128,1.64419545815897));
#62450=CARTESIAN_POINT('Ctrl Pts',(-10.1628390332839,-38.2742356128,1.64845740848264));
#62451=CARTESIAN_POINT('Ctrl Pts',(-10.1452994394432,-38.2742356128,1.71217344421608));
#62452=CARTESIAN_POINT('Ctrl Pts',(-10.1262142672278,-38.2742356128,1.77600560337412));
#62453=CARTESIAN_POINT('Ctrl Pts',(-10.1054102946297,-38.2742356128,1.83964368181909));
#62454=CARTESIAN_POINT('Ctrl Pts',(-10.0886973273238,-38.2742356128,1.89076762554912));
#62455=CARTESIAN_POINT('Ctrl Pts',(-10.0708718635335,-38.2742356128,1.94176903797927));
#62456=CARTESIAN_POINT('Ctrl Pts',(-10.0518653199246,-38.2742356128,1.99250278927512));
#62457=CARTESIAN_POINT('Ctrl Pts',(-10.0354055571795,-38.2742356128,2.03643847409421));
#62458=CARTESIAN_POINT('Ctrl Pts',(-10.0180592615806,-38.2742356128,2.08017418180857));
#62459=CARTESIAN_POINT('Ctrl Pts',(-9.99982048572652,-38.2742356128,2.1236102911859));
#62460=CARTESIAN_POINT('Ctrl Pts',(-9.98302404946877,-38.2742356128,2.16361143206724));
#62461=CARTESIAN_POINT('Ctrl Pts',(-9.96547026680263,-38.2742356128,2.20335885372652));
#62462=CARTESIAN_POINT('Ctrl Pts',(-9.94719756114367,-38.2742356128,2.24276275517514));
#62463=CARTESIAN_POINT('Ctrl Pts',(-9.93038362357603,-38.2742356128,2.27902091810099));
#62464=CARTESIAN_POINT('Ctrl Pts',(-9.91296086855031,-38.2742356128,2.31498837465569));
#62465=CARTESIAN_POINT('Ctrl Pts',(-9.89500060023452,-38.2742356128,2.35058121284723));
#62466=CARTESIAN_POINT('Ctrl Pts',(-9.87764982370093,-38.2742356128,2.38496618810477));
#62467=CARTESIAN_POINT('Ctrl Pts',(-9.85979710564341,-38.2742356128,2.41900172326089));
#62468=CARTESIAN_POINT('Ctrl Pts',(-9.84155018037255,-38.2742356128,2.45259607912348));
#62469=CARTESIAN_POINT('Ctrl Pts',(-9.82324565167511,-38.2742356128,2.48629648847082));
#62470=CARTESIAN_POINT('Ctrl Pts',(-9.80454387289279,-38.2742356128,2.51955320597992));
#62471=CARTESIAN_POINT('Ctrl Pts',(-9.78560470964861,-38.2742356128,2.55225359104964));
#62472=CARTESIAN_POINT('Ctrl Pts',(-9.76789593607952,-38.2742356128,2.58282958362946));
#62473=CARTESIAN_POINT('Ctrl Pts',(-9.74997974302908,-38.2742356128,2.61291917292839));
#62474=CARTESIAN_POINT('Ctrl Pts',(-9.73203341524801,-38.2742356128,2.64241129302391));
#62475=CARTESIAN_POINT('Ctrl Pts',(-9.73078652051974,-38.2742356128,2.64446037902754));
#62476=CARTESIAN_POINT('Ctrl Pts',(-9.7295394997446,-38.2742356128,2.6465065727843));
#62477=CARTESIAN_POINT('Ctrl Pts',(-9.72829242121,-38.2742356128,2.64854983337));
#62478=CARTESIAN_POINT('',(-6.27496226640491,-38.2742356128,2.72284437887685));
#62479=CARTESIAN_POINT('Ctrl Pts',(-9.72829242121,-38.2742356128,2.64854983337));
#62480=CARTESIAN_POINT('Ctrl Pts',(-9.72206121244163,-38.2742356128,2.65875928126896));
#62481=CARTESIAN_POINT('Ctrl Pts',(-9.71578443101656,-38.2742356128,2.66896737401849));
#62482=CARTESIAN_POINT('Ctrl Pts',(-9.70945997971752,-38.2742356128,2.67917591849475));
#62483=CARTESIAN_POINT('Ctrl Pts',(-9.68961023804503,-38.2742356128,2.71121616374684));
#62484=CARTESIAN_POINT('Ctrl Pts',(-9.66928954578558,-38.2742356128159,
2.74326894858221));
#62485=CARTESIAN_POINT('Ctrl Pts',(-9.64842622432582,-38.2742356127842,
2.77533913689464));
#62486=CARTESIAN_POINT('Ctrl Pts',(-9.62681851214317,-38.2742356127513,
2.80855357017819));
#62487=CARTESIAN_POINT('Ctrl Pts',(-9.60462804880873,-38.2742356128199,
2.84178667887765));
#62488=CARTESIAN_POINT('Ctrl Pts',(-9.58176124412416,-38.2742356116715,
2.87499009644905));
#62489=CARTESIAN_POINT('Ctrl Pts',(-9.57746571331455,-38.2742356114558,
2.88122736068993));
#62490=CARTESIAN_POINT('Ctrl Pts',(-9.57314629616008,-38.274235611189,2.88746343032177));
#62491=CARTESIAN_POINT('Ctrl Pts',(-9.56880235347363,-38.2742356108485,
2.89369778504064));
#62492=CARTESIAN_POINT('Ctrl Pts',(-9.55457338499666,-38.2742356097332,
2.91411896533052));
#62493=CARTESIAN_POINT('Ctrl Pts',(-9.54008537245569,-38.2742356075311,
2.93451375044048));
#62494=CARTESIAN_POINT('Ctrl Pts',(-9.52529795253179,-38.274235603801,2.95489149144129));
#62495=CARTESIAN_POINT('Ctrl Pts',(-9.51051053260789,-38.2742356000709,
2.97526923244211));
#62496=CARTESIAN_POINT('Ctrl Pts',(-9.49539922664665,-38.2742355942278,
2.99565922465192));
#62497=CARTESIAN_POINT('Ctrl Pts',(-9.47992884555872,-38.2742355857358,
3.01604818304434));
#62498=CARTESIAN_POINT('Ctrl Pts',(-9.45461973979981,-38.2742355718433,
3.04940394211287));
#62499=CARTESIAN_POINT('Ctrl Pts',(-9.42835325782335,-38.274235553646,3.08276228151732));
#62500=CARTESIAN_POINT('Ctrl Pts',(-9.40112223778464,-38.2742355507865,
3.11587315896628));
#62501=CARTESIAN_POINT('Ctrl Pts',(-9.39506355579132,-38.2742355501503,
3.12324006173738));
#62502=CARTESIAN_POINT('Ctrl Pts',(-9.38895728119517,-38.2742355502767,
3.1305945808947));
#62503=CARTESIAN_POINT('Ctrl Pts',(-9.38280362499654,-38.2742355512933,
3.13793375497978));
#62504=CARTESIAN_POINT('Ctrl Pts',(-9.36533624499038,-38.2742355541788,
3.15876627121689));
#62505=CARTESIAN_POINT('Ctrl Pts',(-9.34748426667175,-38.2742355624319,
3.17947444717405));
#62506=CARTESIAN_POINT('Ctrl Pts',(-9.32922579032951,-38.2742355701077,
3.20000463237014));
#62507=CARTESIAN_POINT('Ctrl Pts',(-9.31096731398727,-38.2742355777835,
3.22053481756623));
#62508=CARTESIAN_POINT('Ctrl Pts',(-9.29231098634183,-38.2742355844588,
3.24087680479964));
#62509=CARTESIAN_POINT('Ctrl Pts',(-9.27317694561511,-38.2742355906155,
3.26105029981677));
#62510=CARTESIAN_POINT('Ctrl Pts',(-9.24445970593352,-38.2742355998558,
3.29132759983388));
#62511=CARTESIAN_POINT('Ctrl Pts',(-9.2146430488724,-38.2742356060047,3.32123956762131));
#62512=CARTESIAN_POINT('Ctrl Pts',(-9.1837237029298,-38.2742356090617,3.35053363451095));
#62513=CARTESIAN_POINT('Ctrl Pts',(-9.17344190202117,-38.2742356100783,
3.36027497134655));
#62514=CARTESIAN_POINT('Ctrl Pts',(-9.16303855804864,-38.2742356107937,
3.36994782914819));
#62515=CARTESIAN_POINT('Ctrl Pts',(-9.15251479486197,-38.2742356113,3.37954254011418));
#62516=CARTESIAN_POINT('Ctrl Pts',(-9.12005297789161,-38.2742356128614,
3.40913858344363));
#62517=CARTESIAN_POINT('Ctrl Pts',(-9.08643042979346,-38.2742356127779,
3.43800495025951));
#62518=CARTESIAN_POINT('Ctrl Pts',(-9.05165103904656,-38.274235612796,3.46590721443792));
#62519=CARTESIAN_POINT('Ctrl Pts',(-9.04124376010983,-38.2742356128014,
3.47425660297047));
#62520=CARTESIAN_POINT('Ctrl Pts',(-9.03073321972762,-38.2742356128,3.48251953511692));
#62521=CARTESIAN_POINT('Ctrl Pts',(-9.02012039388568,-38.2742356128,3.49068942360137));
#62522=CARTESIAN_POINT('Ctrl Pts',(-8.98898741571359,-38.2742356128,3.51465598666788));
#62523=CARTESIAN_POINT('Ctrl Pts',(-8.95695978201797,-38.2742356127997,
3.53783475496327));
#62524=CARTESIAN_POINT('Ctrl Pts',(-8.92403276743319,-38.2742356127993,
3.56007714970093));
#62525=CARTESIAN_POINT('Ctrl Pts',(-8.90822535481241,-38.2742356127992,
3.57075515120596));
#62526=CARTESIAN_POINT('Ctrl Pts',(-8.89221146739688,-38.2742356127992,
3.58121732420375));
#62527=CARTESIAN_POINT('Ctrl Pts',(-8.87599478577521,-38.2742356127994,
3.59144734775174));
#62528=CARTESIAN_POINT('Ctrl Pts',(-8.838986370624,-38.2742356128,3.61479349015639));
#62529=CARTESIAN_POINT('Ctrl Pts',(-8.80091222203195,-38.2742356128,3.63693279720875));
#62530=CARTESIAN_POINT('Ctrl Pts',(-8.76183764917323,-38.2742356128,3.65768687538109));
#62531=CARTESIAN_POINT('Ctrl Pts',(-8.72811628805191,-38.2742356128,3.67559764736368));
#62532=CARTESIAN_POINT('Ctrl Pts',(-8.69365111458049,-38.2742356128,3.69247656469757));
#62533=CARTESIAN_POINT('Ctrl Pts',(-8.6585144938953,-38.2742356128,3.70821531441722));
#62534=CARTESIAN_POINT('Ctrl Pts',(-8.62258077045391,-38.2742356128,3.72431111044742));
#62535=CARTESIAN_POINT('Ctrl Pts',(-8.58593577278161,-38.2742356128,3.73921800415691));
#62536=CARTESIAN_POINT('Ctrl Pts',(-8.54868983724074,-38.2742356128,3.75282640854491));
#62537=CARTESIAN_POINT('Ctrl Pts',(-8.52053919883706,-38.2742356128,3.76311169915756));
#62538=CARTESIAN_POINT('Ctrl Pts',(-8.49203815841643,-38.2742356128,3.77265815994509));
#62539=CARTESIAN_POINT('Ctrl Pts',(-8.46324819816481,-38.2742356128,3.78142244205252));
#62540=CARTESIAN_POINT('Ctrl Pts',(-8.4190268755565,-38.2742356128,3.79488436221898));
#62541=CARTESIAN_POINT('Ctrl Pts',(-8.37413308186376,-38.2742356128,3.80649598015092));
#62542=CARTESIAN_POINT('Ctrl Pts',(-8.32878118257724,-38.2742356128,3.81614800469356));
#62543=CARTESIAN_POINT('Ctrl Pts',(-8.28437937400409,-38.2742356128,3.82559782604234));
#62544=CARTESIAN_POINT('Ctrl Pts',(-8.23953875934846,-38.2742356128,3.83316896757169));
#62545=CARTESIAN_POINT('Ctrl Pts',(-8.1944704803585,-38.2742356128,3.8388044770508));
#62546=CARTESIAN_POINT('Ctrl Pts',(-8.150885627809,-38.2742356128,3.84425449323055));
#62547=CARTESIAN_POINT('Ctrl Pts',(-8.10708856365568,-38.2742356128,3.84789392309733));
#62548=CARTESIAN_POINT('Ctrl Pts',(-8.06326914099037,-38.2742356128,3.84971947920494));
#62549=CARTESIAN_POINT('Ctrl Pts',(-8.02135496316993,-38.2742356128,3.85146566111837));
#62550=CARTESIAN_POINT('Ctrl Pts',(-7.97942083965261,-38.2742356128,3.85155218090322));
#62551=CARTESIAN_POINT('Ctrl Pts',(-7.93762323916678,-38.2742356128,3.85002349382485));
#62552=CARTESIAN_POINT('Ctrl Pts',(-7.93004509331808,-38.2742356128,3.84974633404769));
#62553=CARTESIAN_POINT('Ctrl Pts',(-7.92247139718219,-38.2742356128,3.84941621215186));
#62554=CARTESIAN_POINT('Ctrl Pts',(-7.91490302783018,-38.2742356128,3.8490335730693));
#62555=CARTESIAN_POINT('Ctrl Pts',(-7.86845145763927,-38.2742356128,3.84668509014325));
#62556=CARTESIAN_POINT('Ctrl Pts',(-7.82219973451753,-38.2742356127606,
3.84234260710909));
#62557=CARTESIAN_POINT('Ctrl Pts',(-7.77633328742756,-38.2742356120254,
3.83608056160565));
#62558=CARTESIAN_POINT('Ctrl Pts',(-7.73831945958442,-38.274235611416,3.83089061699872));
#62559=CARTESIAN_POINT('Ctrl Pts',(-7.70056988557531,-38.274235610423,3.82438341370477));
#62560=CARTESIAN_POINT('Ctrl Pts',(-7.66317673260836,-38.2742356104353,
3.81662470151561));
#62561=CARTESIAN_POINT('Ctrl Pts',(-7.62192562203549,-38.2742356104488,
3.80806550099296));
#62562=CARTESIAN_POINT('Ctrl Pts',(-7.58110415372514,-38.2742356113252,
3.7979804666135));
#62563=CARTESIAN_POINT('Ctrl Pts',(-7.54080563372603,-38.2742356118068,
3.78645483313038));
#62564=CARTESIAN_POINT('Ctrl Pts',(-7.50050711372516,-38.2742356122885,
3.77492919964675));
#62565=CARTESIAN_POINT('Ctrl Pts',(-7.4607274036797,-38.2742356123951,3.76195892946109));
#62566=CARTESIAN_POINT('Ctrl Pts',(-7.4215996682472,-38.2742356124429,3.74767352673602));
#62567=CARTESIAN_POINT('Ctrl Pts',(-7.37576953416442,-38.2742356124989,
3.73094110112845));
#62568=CARTESIAN_POINT('Ctrl Pts',(-7.33080966098452,-38.2742356125197,
3.71239779074037));
#62569=CARTESIAN_POINT('Ctrl Pts',(-7.28688698368685,-38.274235612542,3.69227097596761));
#62570=CARTESIAN_POINT('Ctrl Pts',(-7.27485803495137,-38.2742356125482,
3.68675891618425));
#62571=CARTESIAN_POINT('Ctrl Pts',(-7.26290659591565,-38.2742356125543,
3.68112819714996));
#62572=CARTESIAN_POINT('Ctrl Pts',(-7.25103543965387,-38.2742356125609,
3.67538366592419));
#62573=CARTESIAN_POINT('Ctrl Pts',(-7.22342437675913,-38.2742356125763,
3.6620224895166));
#62574=CARTESIAN_POINT('Ctrl Pts',(-7.1962409699365,-38.27423561257,3.64804144895993));
#62575=CARTESIAN_POINT('Ctrl Pts',(-7.16951458768156,-38.2742356125657,
3.6335010353345));
#62576=CARTESIAN_POINT('Ctrl Pts',(-7.14278820542818,-38.2742356125615,
3.61896062170992));
#62577=CARTESIAN_POINT('Ctrl Pts',(-7.11650711974314,-38.2742356125844,
3.60385590787456));
#62578=CARTESIAN_POINT('Ctrl Pts',(-7.09066450610827,-38.2742356125935,
3.58822340182743));
#62579=CARTESIAN_POINT('Ctrl Pts',(-7.05214811130959,-38.274235612607,3.56492437398485));
#62580=CARTESIAN_POINT('Ctrl Pts',(-7.01458513687742,-38.2742356126672,
3.54044242465216));
#62581=CARTESIAN_POINT('Ctrl Pts',(-6.97799376259113,-38.2742356127132,
3.51491020294578));
#62582=CARTESIAN_POINT('Ctrl Pts',(-6.94358319795952,-38.2742356127564,
3.49089967635714));
#62583=CARTESIAN_POINT('Ctrl Pts',(-6.91003167756674,-38.2742356127845,
3.46596081997936));
#62584=CARTESIAN_POINT('Ctrl Pts',(-6.87732102706461,-38.2742356127938,
3.44017356082324));
#62585=CARTESIAN_POINT('Ctrl Pts',(-6.85147274014318,-38.2742356128012,
3.41979620777913));
#62586=CARTESIAN_POINT('Ctrl Pts',(-6.82614890728275,-38.2742356128,3.39888862739908));
#62587=CARTESIAN_POINT('Ctrl Pts',(-6.80132545127044,-38.2742356128,3.37747264929914));
#62588=CARTESIAN_POINT('Ctrl Pts',(-6.76339210431094,-38.2742356128,3.34474635496934));
#62589=CARTESIAN_POINT('Ctrl Pts',(-6.72665003782783,-38.2742356128499,
3.31084645522773));
#62590=CARTESIAN_POINT('Ctrl Pts',(-6.69110550144799,-38.2742356122268,
3.27587871692887));
#62591=CARTESIAN_POINT('Ctrl Pts',(-6.65332467546997,-38.2742356115645,
3.23871097836573));
#62592=CARTESIAN_POINT('Ctrl Pts',(-6.61689595956591,-38.2742356099512,
3.20033652698392));
#62593=CARTESIAN_POINT('Ctrl Pts',(-6.58182417042585,-38.2742356089708,
3.16082406650467));
#62594=CARTESIAN_POINT('Ctrl Pts',(-6.57342708240585,-38.274235608736,3.15136376759588));
#62595=CARTESIAN_POINT('Ctrl Pts',(-6.56510780276211,-38.2742356085496,
3.14183799650869));
#62596=CARTESIAN_POINT('Ctrl Pts',(-6.55686646545738,-38.2742356084435,
3.13224727289733));
#62597=CARTESIAN_POINT('Ctrl Pts',(-6.51731755512019,-38.2742356079345,
3.08622286518904));
#62598=CARTESIAN_POINT('Ctrl Pts',(-6.4795690142431,-38.2742356094994,3.03871550253006));
#62599=CARTESIAN_POINT('Ctrl Pts',(-6.44370529454587,-38.2742356107499,
2.98978551465853));
#62600=CARTESIAN_POINT('Ctrl Pts',(-6.41151588994877,-38.2742356118723,
2.94586850912135));
#62601=CARTESIAN_POINT('Ctrl Pts',(-6.38084419077031,-38.2742356125538,
2.90080380260923));
#62602=CARTESIAN_POINT('Ctrl Pts',(-6.35177864059283,-38.2742356127166,
2.8546119171942));
#62603=CARTESIAN_POINT('Ctrl Pts',(-6.32630607497036,-38.2742356128592,
2.81413011570496));
#62604=CARTESIAN_POINT('Ctrl Pts',(-6.30206526745315,-38.2742356128,2.77277584410025));
#62605=CARTESIAN_POINT('Ctrl Pts',(-6.27913862688043,-38.2742356128,2.73056930062515));
#62606=CARTESIAN_POINT('Ctrl Pts',(-6.27774176197317,-38.2742356128,2.72799775774035));
#62607=CARTESIAN_POINT('Ctrl Pts',(-6.27634984587968,-38.2742356128,2.72542318548171));
#62608=CARTESIAN_POINT('Ctrl Pts',(-6.27496226376,-38.2742356128,2.7228443803));
#62609=CARTESIAN_POINT('',(-2.29653415164,-38.2742356128,-2.09683582826));
#62610=CARTESIAN_POINT('Ctrl Pts',(-6.27496226971104,-38.2742356128,2.72284437709791));
#62611=CARTESIAN_POINT('Ctrl Pts',(-6.25343867541546,-38.2742356128,2.68284304096698));
#62612=CARTESIAN_POINT('Ctrl Pts',(-6.23329489033184,-38.2742356128021,
2.64244474672542));
#62613=CARTESIAN_POINT('Ctrl Pts',(-6.2143366952227,-38.2742356127979,2.60182941082557));
#62614=CARTESIAN_POINT('Ctrl Pts',(-6.19786423880922,-38.2742356127943,
2.56653942955479));
#62615=CARTESIAN_POINT('Ctrl Pts',(-6.18228642632628,-38.2742356127937,
2.53108405257986));
#62616=CARTESIAN_POINT('Ctrl Pts',(-6.16747377524522,-38.2742356127121,
2.4955497011575));
#62617=CARTESIAN_POINT('Ctrl Pts',(-6.14601564749822,-38.2742356125939,
2.44407338891229));
#62618=CARTESIAN_POINT('Ctrl Pts',(-6.12614048873929,-38.2742356124173,
2.39239502058356));
#62619=CARTESIAN_POINT('Ctrl Pts',(-6.10746783960564,-38.2742356124274,
2.3407042372701));
#62620=CARTESIAN_POINT('Ctrl Pts',(-6.0984087265777,-38.2742356124324,2.31562623975684));
#62621=CARTESIAN_POINT('Ctrl Pts',(-6.08963297438635,-38.2742356124787,
2.29054439503083));
#62622=CARTESIAN_POINT('Ctrl Pts',(-6.08109996571743,-38.2742356125507,
2.26547728984694));
#62623=CARTESIAN_POINT('Ctrl Pts',(-6.06532733137766,-38.2742356126837,
2.21914260306032));
#62624=CARTESIAN_POINT('Ctrl Pts',(-6.05038236765882,-38.2742356127776,
2.17285465240021));
#62625=CARTESIAN_POINT('Ctrl Pts',(-6.03602763222168,-38.2742356127936,
2.12669144192736));
#62626=CARTESIAN_POINT('Ctrl Pts',(-6.03255557415966,-38.2742356127975,
2.11552569472197));
#62627=CARTESIAN_POINT('Ctrl Pts',(-6.02911825580295,-38.2742356127989,
2.1043673476744));
#62628=CARTESIAN_POINT('Ctrl Pts',(-6.02571273819095,-38.2742356127995,
2.09321776498803));
#62629=CARTESIAN_POINT('Ctrl Pts',(-6.01988428400387,-38.2742356128005,
2.07413554627808));
#62630=CARTESIAN_POINT('Ctrl Pts',(-6.0141467501015,-38.2742356128,2.05507181057947));
#62631=CARTESIAN_POINT('Ctrl Pts',(-6.00849013333293,-38.2742356128,2.03604840855248));
#62632=CARTESIAN_POINT('Ctrl Pts',(-6.00270430180311,-38.2742356128,2.01659045271859));
#62633=CARTESIAN_POINT('Ctrl Pts',(-5.99700616637023,-38.2742356128,1.99718554365947));
#62634=CARTESIAN_POINT('Ctrl Pts',(-5.9914048278946,-38.2742356128,1.97792452860784));
#62635=CARTESIAN_POINT('Ctrl Pts',(-5.98556329602797,-38.2742356128,1.95783757373137));
#62636=CARTESIAN_POINT('Ctrl Pts',(-5.97982692637279,-38.2742356128,1.93790670946469));
#62637=CARTESIAN_POINT('Ctrl Pts',(-5.97419138868625,-38.2742356128,1.91817685111571));
#62638=CARTESIAN_POINT('Ctrl Pts',(-5.96803366204245,-38.2742356128,1.8966188239688));
#62639=CARTESIAN_POINT('Ctrl Pts',(-5.96199623521128,-38.2742356128,1.87530052368112));
#62640=CARTESIAN_POINT('Ctrl Pts',(-5.95605774049402,-38.2742356128,1.85421720432329));
#62641=CARTESIAN_POINT('Ctrl Pts',(-5.9522628450401,-38.2742356128,1.8407442626783));
#62642=CARTESIAN_POINT('Ctrl Pts',(-5.94850803272726,-38.2742356128,1.82736599721998));
#62643=CARTESIAN_POINT('Ctrl Pts',(-5.94478517864091,-38.2742356128,1.81407063595496));
#62644=CARTESIAN_POINT('Ctrl Pts',(-5.93738839707275,-38.2742356128,1.78765464412012));
#62645=CARTESIAN_POINT('Ctrl Pts',(-5.93012019351236,-38.2742356128,1.76157544910232));
#62646=CARTESIAN_POINT('Ctrl Pts',(-5.92289628650845,-38.2742356128,1.73565584384684));
#62647=CARTESIAN_POINT('Ctrl Pts',(-5.914084877134,-38.2742356128,1.70404023021749));
#62648=CARTESIAN_POINT('Ctrl Pts',(-5.90533754480164,-38.2742356128,1.67265553896624));
#62649=CARTESIAN_POINT('Ctrl Pts',(-5.89649392943623,-38.2742356128,1.64113094127172));
#62650=CARTESIAN_POINT('Ctrl Pts',(-5.89117577007019,-38.2742356128,1.62217344170142));
#62651=CARTESIAN_POINT('Ctrl Pts',(-5.88582275743926,-38.2742356128,1.60316479414047));
#62652=CARTESIAN_POINT('Ctrl Pts',(-5.88040459967885,-38.2742356128,1.58403821721294));
#62653=CARTESIAN_POINT('Ctrl Pts',(-5.87474911442545,-38.2742356128,1.56407385320862));
#62654=CARTESIAN_POINT('Ctrl Pts',(-5.86902251787269,-38.2742356128,1.54398063176711));
#62655=CARTESIAN_POINT('Ctrl Pts',(-5.86320917856773,-38.2742356128,1.52374749789215));
#62656=CARTESIAN_POINT('Ctrl Pts',(-5.85808049136635,-38.2742356128,1.50589727286574));
#62657=CARTESIAN_POINT('Ctrl Pts',(-5.85288428367078,-38.2742356128,1.4879380970169));
#62658=CARTESIAN_POINT('Ctrl Pts',(-5.84761945870423,-38.2742356128,1.46989499107882));
#62659=CARTESIAN_POINT('Ctrl Pts',(-5.8421991165419,-38.2742356128,1.45131891144139));
#62660=CARTESIAN_POINT('Ctrl Pts',(-5.83670655669577,-38.2742356128,1.43265575185725));
#62661=CARTESIAN_POINT('Ctrl Pts',(-5.83115983090085,-38.2742356128,1.41399731968152));
#62662=CARTESIAN_POINT('Ctrl Pts',(-5.83086484275531,-38.2742356128,1.41300501962742));
#62663=CARTESIAN_POINT('Ctrl Pts',(-5.830569704989,-38.2742356128,1.4120127447957));
#62664=CARTESIAN_POINT('Ctrl Pts',(-5.83027442154199,-38.2742356128,1.41102051304804));
#62665=CARTESIAN_POINT('Ctrl Pts',(-5.82494465487051,-38.2742356127999,
1.39311106450725));
#62666=CARTESIAN_POINT('Ctrl Pts',(-5.81957326542789,-38.2742356128,1.37523596643992));
#62667=CARTESIAN_POINT('Ctrl Pts',(-5.81415451162564,-38.2742356128,1.35740490081377));
#62668=CARTESIAN_POINT('Ctrl Pts',(-5.81362807119891,-38.2742356128,1.35567258483487));
#62669=CARTESIAN_POINT('Ctrl Pts',(-5.81310119326957,-38.2742356128,1.35394072452064));
#62670=CARTESIAN_POINT('Ctrl Pts',(-5.81257387902922,-38.2742356128,1.3522093558744));
#62671=CARTESIAN_POINT('Ctrl Pts',(-5.80520753857709,-38.2742356128,1.32802292220685));
#62672=CARTESIAN_POINT('Ctrl Pts',(-5.79777116024211,-38.2742356128,1.30398347871627));
#62673=CARTESIAN_POINT('Ctrl Pts',(-5.79022912459579,-38.2742356128,1.28002336192701));
#62674=CARTESIAN_POINT('Ctrl Pts',(-5.78202497565214,-38.2742356128,1.25395979287694));
#62675=CARTESIAN_POINT('Ctrl Pts',(-5.77369596379631,-38.2742356128,1.22799072420539));
#62676=CARTESIAN_POINT('Ctrl Pts',(-5.7652157517049,-38.2742356128,1.20209112335984));
#62677=CARTESIAN_POINT('Ctrl Pts',(-5.75504575170402,-38.2742356128,1.17103070437704));
#62678=CARTESIAN_POINT('Ctrl Pts',(-5.74465852701919,-38.2742356128,1.14007133411449));
#62679=CARTESIAN_POINT('Ctrl Pts',(-5.73403313082186,-38.2742356128,1.10924352573199));
#62680=CARTESIAN_POINT('Ctrl Pts',(-5.72151165526241,-38.2742356128,1.07291456048266));
#62681=CARTESIAN_POINT('Ctrl Pts',(-5.70866115126366,-38.2742356128,1.03677487726414));
#62682=CARTESIAN_POINT('Ctrl Pts',(-5.69546311036074,-38.2742356128,1.00090701483098));
#62683=CARTESIAN_POINT('Ctrl Pts',(-5.68570249198199,-38.2742356128,0.974380917522556));
#62684=CARTESIAN_POINT('Ctrl Pts',(-5.67575238409884,-38.2742356128,0.948005045359147));
#62685=CARTESIAN_POINT('Ctrl Pts',(-5.66559884051821,-38.2742356128,0.92178185094905));
#62686=CARTESIAN_POINT('Ctrl Pts',(-5.66202304049715,-38.2742356128,0.912546759930898));
#62687=CARTESIAN_POINT('Ctrl Pts',(-5.65842190859526,-38.2742356128,0.90333018961899));
#62688=CARTESIAN_POINT('Ctrl Pts',(-5.65479443282628,-38.2742356128,0.89413063357453));
#62689=CARTESIAN_POINT('Ctrl Pts',(-5.63120997437853,-38.2742356128,0.834318642789297));
#62690=CARTESIAN_POINT('Ctrl Pts',(-5.60650655989423,-38.2742356128,0.775223123984615));
#62691=CARTESIAN_POINT('Ctrl Pts',(-5.58056333005086,-38.2742356128,0.716890523122717));
#62692=CARTESIAN_POINT('Ctrl Pts',(-5.55256032032622,-38.2742356128,0.653926566858942));
#62693=CARTESIAN_POINT('Ctrl Pts',(-5.52311298107293,-38.2742356128,0.591851719963286));
#62694=CARTESIAN_POINT('Ctrl Pts',(-5.49213034599839,-38.2742356128,0.530709651061986));
#62695=CARTESIAN_POINT('Ctrl Pts',(-5.45933890499242,-38.2742356128,0.465998029841364));
#62696=CARTESIAN_POINT('Ctrl Pts',(-5.42482839106383,-38.2742356128,0.402331539315345));
#62697=CARTESIAN_POINT('Ctrl Pts',(-5.38854948129966,-38.2742356128,0.339742119926858));
#62698=CARTESIAN_POINT('Ctrl Pts',(-5.34797421744951,-38.2742356128,0.269740506801641));
#62699=CARTESIAN_POINT('Ctrl Pts',(-5.30518791818639,-38.2742356128,0.201086868540641));
#62700=CARTESIAN_POINT('Ctrl Pts',(-5.2601797548669,-38.2742356128,0.13379375830936));
#62701=CARTESIAN_POINT('Ctrl Pts',(-5.24442214693411,-38.2742356128,0.110234066702396));
#62702=CARTESIAN_POINT('Ctrl Pts',(-5.22839258827465,-38.2742356128,0.0868408264598558));
#62703=CARTESIAN_POINT('Ctrl Pts',(-5.21209158864003,-38.2742356128,0.0636135438118852));
#62704=CARTESIAN_POINT('Ctrl Pts',(-5.16303895840601,-38.2742356128,-0.00628151370670113));
#62705=CARTESIAN_POINT('Ctrl Pts',(-5.11152067541813,-38.2742356128,-0.0746775353743387));
#62706=CARTESIAN_POINT('Ctrl Pts',(-5.05770039912222,-38.2742356128,-0.141553198717477));
#62707=CARTESIAN_POINT('Ctrl Pts',(-5.00070653692266,-38.2742356128,-0.212372276645049));
#62708=CARTESIAN_POINT('Ctrl Pts',(-4.94113150722171,-38.2742356128,-0.281486624304317));
#62709=CARTESIAN_POINT('Ctrl Pts',(-4.87920687688789,-38.2742356128,-0.348920019142021));
#62710=CARTESIAN_POINT('Ctrl Pts',(-4.81218558689648,-38.2742356128,-0.421903468314986));
#62711=CARTESIAN_POINT('Ctrl Pts',(-4.74241250105015,-38.2742356128,-0.492918183244864));
#62712=CARTESIAN_POINT('Ctrl Pts',(-4.67021747606694,-38.2742356128,-0.562046414701979));
#62713=CARTESIAN_POINT('Ctrl Pts',(-4.63784417473622,-38.2742356128,-0.593044521121934));
#62714=CARTESIAN_POINT('Ctrl Pts',(-4.60498324021259,-38.2742356128,-0.623664886468992));
#62715=CARTESIAN_POINT('Ctrl Pts',(-4.5716693681391,-38.2742356128,-0.653914580276434));
#62716=CARTESIAN_POINT('Ctrl Pts',(-4.48958434544408,-38.2742356128,-0.728449500661054));
#62717=CARTESIAN_POINT('Ctrl Pts',(-4.40477413851654,-38.2742356128,-0.800708714336258));
#62718=CARTESIAN_POINT('Ctrl Pts',(-4.31774788686279,-38.2742356128,-0.870862803916576));
#62719=CARTESIAN_POINT('Ctrl Pts',(-4.27180201100859,-38.2742356128,-0.907900950789164));
#62720=CARTESIAN_POINT('Ctrl Pts',(-4.22524096850355,-38.2742356128,-0.944351251618469));
#62721=CARTESIAN_POINT('Ctrl Pts',(-4.17813182275849,-38.2742356128,-0.980247599868581));
#62722=CARTESIAN_POINT('Ctrl Pts',(-4.09980474547713,-38.2742356128,-1.03993146802277));
#62723=CARTESIAN_POINT('Ctrl Pts',(-4.01995584057801,-38.2742356128,-1.09809026518485));
#62724=CARTESIAN_POINT('Ctrl Pts',(-3.93889540951161,-38.2742356128,-1.15486566991628));
#62725=CARTESIAN_POINT('Ctrl Pts',(-3.89820004443583,-38.2742356128,-1.1833690444046));
#62726=CARTESIAN_POINT('Ctrl Pts',(-3.8571990327442,-38.2742356128,-1.21152368000513));
#62727=CARTESIAN_POINT('Ctrl Pts',(-3.8159293073926,-38.2742356128,-1.23934650848657));
#62728=CARTESIAN_POINT('Ctrl Pts',(-3.77240858136084,-38.2742356128,-1.26868689506422));
#62729=CARTESIAN_POINT('Ctrl Pts',(-3.72858183608195,-38.2742356128,-1.29766321120108));
#62730=CARTESIAN_POINT('Ctrl Pts',(-3.68449058042176,-38.2742356128,-1.32629284236997));
#62731=CARTESIAN_POINT('Ctrl Pts',(-3.60314006363722,-38.2742356128,-1.37911590798846));
#62732=CARTESIAN_POINT('Ctrl Pts',(-3.52089527451447,-38.2742356128,-1.43075803920082));
#62733=CARTESIAN_POINT('Ctrl Pts',(-3.43801071125674,-38.2742356128,-1.48129673933209));
#62734=CARTESIAN_POINT('Ctrl Pts',(-3.3604874182667,-38.2742356128,-1.52856641541676));
#62735=CARTESIAN_POINT('Ctrl Pts',(-3.28240471810566,-38.2742356128,-1.57487116471378));
#62736=CARTESIAN_POINT('Ctrl Pts',(-3.20393382874924,-38.2742356128,-1.62024778862748));
#62737=CARTESIAN_POINT('Ctrl Pts',(-3.12983202014925,-38.2742356128,-1.66309794526191));
#62738=CARTESIAN_POINT('Ctrl Pts',(-3.05538418311467,-38.2742356128,-1.70512065770332));
#62739=CARTESIAN_POINT('Ctrl Pts',(-2.98069750636388,-38.2742356128,-1.74631839971243));
#62740=CARTESIAN_POINT('Ctrl Pts',(-2.95738588423248,-38.2742356128,-1.75917726873921));
#62741=CARTESIAN_POINT('Ctrl Pts',(-2.93405203055978,-38.2742356128,-1.77195479357069));
#62742=CARTESIAN_POINT('Ctrl Pts',(-2.91070243365683,-38.2742356128,-1.78464824943072));
#62743=CARTESIAN_POINT('Ctrl Pts',(-2.86043357653793,-38.2742356128,-1.81197572414581));
#62744=CARTESIAN_POINT('Ctrl Pts',(-2.81007886487402,-38.2742356128,-1.83892187073565));
#62745=CARTESIAN_POINT('Ctrl Pts',(-2.75958339447557,-38.2742356128,-1.86551280695808));
#62746=CARTESIAN_POINT('Ctrl Pts',(-2.72930698729957,-38.2742356128,-1.88145637587443));
#62747=CARTESIAN_POINT('Ctrl Pts',(-2.69897964236885,-38.2742356128,-1.89727208811875));
#62748=CARTESIAN_POINT('Ctrl Pts',(-2.66858803344439,-38.2742356128,-1.91296318395376));
#62749=CARTESIAN_POINT('Ctrl Pts',(-2.6077524293637,-38.2742356128,-1.94437242247689));
#62750=CARTESIAN_POINT('Ctrl Pts',(-2.54669259970672,-38.2742356128,-1.9752662642291));
#62751=CARTESIAN_POINT('Ctrl Pts',(-2.48550737802581,-38.2742356128,-2.00554502912596));
#62752=CARTESIAN_POINT('Ctrl Pts',(-2.4507304139965,-38.2742356128,-2.02275512477883));
#62753=CARTESIAN_POINT('Ctrl Pts',(-2.4159125560593,-38.2742356128,-2.03976628509963));
#62754=CARTESIAN_POINT('Ctrl Pts',(-2.38106878359342,-38.2742356128,-2.05655838691403));
#62755=CARTESIAN_POINT('Ctrl Pts',(-2.3546097942447,-38.2742356128,-2.06930964808947));
#62756=CARTESIAN_POINT('Ctrl Pts',(-2.32813281720675,-38.2742356128,-2.08193609605139));
#62757=CARTESIAN_POINT('Ctrl Pts',(-2.30161949261477,-38.2742356128,-2.09443938197145));
#62758=CARTESIAN_POINT('Ctrl Pts',(-2.29992454402612,-38.2742356128,-2.09523869428516));
#62759=CARTESIAN_POINT('Ctrl Pts',(-2.29822962710667,-38.2742356128,-2.09603741777667));
#62760=CARTESIAN_POINT('Ctrl Pts',(-2.29653415164,-38.2742356128,-2.09683582826));
#62761=CARTESIAN_POINT('',(-1.05996521274483,-38.2742356128,-2.50526954715394));
#62762=CARTESIAN_POINT('Origin',(-0.442664407162939,-38.2742356128,1.43778039829082));
#62763=CARTESIAN_POINT('',(-0.417273426023,-38.2742356128,-3.28965093269));
#62764=CARTESIAN_POINT('Ctrl Pts',(-1.05996499772,-38.2742356128,-2.50526959461));
#62765=CARTESIAN_POINT('Ctrl Pts',(-1.0545628851308,-38.2742356128,-2.50635300094287));
#62766=CARTESIAN_POINT('Ctrl Pts',(-1.04893587647229,-38.2742356128,-2.50754377045459));
#62767=CARTESIAN_POINT('Ctrl Pts',(-1.04355928227185,-38.2742356128,-2.50874100265385));
#62768=CARTESIAN_POINT('Ctrl Pts',(-1.03810376887435,-38.2742356128,-2.5099558081719));
#62769=CARTESIAN_POINT('Ctrl Pts',(-1.03266139142698,-38.2742356128,-2.51122815763621));
#62770=CARTESIAN_POINT('Ctrl Pts',(-1.02723368169931,-38.2742356128,-2.51255742238625));
#62771=CARTESIAN_POINT('Ctrl Pts',(-0.998495061676567,-38.2742356128,-2.51959560911282));
#62772=CARTESIAN_POINT('Ctrl Pts',(-0.970143039745548,-38.2742356128108,
-2.52823878716873));
#62773=CARTESIAN_POINT('Ctrl Pts',(-0.942373769726441,-38.2742356127073,
-2.53841013176227));
#62774=CARTESIAN_POINT('Ctrl Pts',(-0.909912208880344,-38.2742356125864,
-2.55030017140619));
#62775=CARTESIAN_POINT('Ctrl Pts',(-0.878246461049334,-38.274235612256,
-2.56427904455269));
#62776=CARTESIAN_POINT('Ctrl Pts',(-0.847615534382662,-38.2742356120111,
-2.58023943993716));
#62777=CARTESIAN_POINT('Ctrl Pts',(-0.835164165836895,-38.2742356119116,
-2.58672728691713));
#62778=CARTESIAN_POINT('Ctrl Pts',(-0.822883090372356,-38.2742356118354,
-2.59354265810511));
#62779=CARTESIAN_POINT('Ctrl Pts',(-0.810786145712179,-38.2742356118171,
-2.60067845985212));
#62780=CARTESIAN_POINT('Ctrl Pts',(-0.778112483915285,-38.2742356117674,
-2.61995215081137));
#62781=CARTESIAN_POINT('Ctrl Pts',(-0.746830967014757,-38.2742356121238,
-2.64153966888173));
#62782=CARTESIAN_POINT('Ctrl Pts',(-0.71722542326134,-38.2742356123874,
-2.66524179112785));
#62783=CARTESIAN_POINT('Ctrl Pts',(-0.691853613893979,-38.2742356126133,
-2.68555439650471));
#62784=CARTESIAN_POINT('Ctrl Pts',(-0.667710524559884,-38.2742356127472,
-2.70742011010636));
#62785=CARTESIAN_POINT('Ctrl Pts',(-0.644980774960419,-38.274235612782,
-2.73067823100576));
#62786=CARTESIAN_POINT('Ctrl Pts',(-0.63074658199222,-38.2742356128038,
-2.74524330923115));
#62787=CARTESIAN_POINT('Ctrl Pts',(-0.617066898747946,-38.2742356128,-2.76035374556724));
#62788=CARTESIAN_POINT('Ctrl Pts',(-0.603993341432776,-38.2742356128,-2.7759612906689));
#62789=CARTESIAN_POINT('Ctrl Pts',(-0.579481412026907,-38.2742356128,-2.80522425517872));
#62790=CARTESIAN_POINT('Ctrl Pts',(-0.557089172077376,-38.2742356128,-2.83624768270283));
#62791=CARTESIAN_POINT('Ctrl Pts',(-0.537022980088056,-38.2742356128,-2.86871379934565));
#62792=CARTESIAN_POINT('Ctrl Pts',(-0.516411183247313,-38.2742356128,-2.90206267793734));
#62793=CARTESIAN_POINT('Ctrl Pts',(-0.498254305254846,-38.2742356128,-2.9369329166477));
#62794=CARTESIAN_POINT('Ctrl Pts',(-0.482738377586076,-38.2742356128,-2.97294076116154));
#62795=CARTESIAN_POINT('Ctrl Pts',(-0.47739895586098,-38.2742356128,-2.98533196788636));
#62796=CARTESIAN_POINT('Ctrl Pts',(-0.472371914802775,-38.2742356128,-2.99785761789655));
#62797=CARTESIAN_POINT('Ctrl Pts',(-0.467663626133187,-38.2742356128,-3.01050133048556));
#62798=CARTESIAN_POINT('Ctrl Pts',(-0.453513865456522,-38.2742356128,-3.04849932078608));
#62799=CARTESIAN_POINT('Ctrl Pts',(-0.442243464789961,-38.2742356128,-3.08757329554101));
#62800=CARTESIAN_POINT('Ctrl Pts',(-0.433990885022559,-38.2742356128,-3.12728197170967));
#62801=CARTESIAN_POINT('Ctrl Pts',(-0.426017960141965,-38.2742356127999,
-3.16564504133441));
#62802=CARTESIAN_POINT('Ctrl Pts',(-0.42086197130703,-38.2742356127999,
-3.204599556636));
#62803=CARTESIAN_POINT('Ctrl Pts',(-0.418599488142137,-38.2742356128,-3.24374472071435));
#62804=CARTESIAN_POINT('Ctrl Pts',(-0.417956545491016,-38.2742356128,-3.25486882362997));
#62805=CARTESIAN_POINT('Ctrl Pts',(-0.417546953560373,-38.2742356128,-3.26600835246778));
#62806=CARTESIAN_POINT('Ctrl Pts',(-0.417371692423965,-38.2742356128,-3.27715422675297));
#62807=CARTESIAN_POINT('Ctrl Pts',(-0.417306202598934,-38.2742356128,-3.2813191053548));
#62808=CARTESIAN_POINT('Ctrl Pts',(-0.417273424670102,-38.2742356128,-3.28548503749));
#62809=CARTESIAN_POINT('Ctrl Pts',(-0.417273426023,-38.2742356128,-3.28965093269));
#62810=CARTESIAN_POINT('',(-0.417297207341341,-38.2742356124858,-7.95031781344913));
#62811=CARTESIAN_POINT('',(-0.417273426056,-38.2742356128,0.916320001688));
#62812=CARTESIAN_POINT('',(-2.08574231668,-38.2742356128,-9.3172814696));
#62813=CARTESIAN_POINT('Ctrl Pts',(-0.417320987633984,-38.2742356128,-7.9503177501852));
#62814=CARTESIAN_POINT('Ctrl Pts',(-0.417572749059598,-38.2742356128,-7.98992259023869));
#62815=CARTESIAN_POINT('Ctrl Pts',(-0.419478320445827,-38.2742356128,-8.02968070118645));
#62816=CARTESIAN_POINT('Ctrl Pts',(-0.423055995654528,-38.2742356128,-8.06934147447744));
#62817=CARTESIAN_POINT('Ctrl Pts',(-0.42677560847607,-38.2742356128,-8.11057571521752));
#62818=CARTESIAN_POINT('Ctrl Pts',(-0.432302579823145,-38.2742356128,-8.15170500580991));
#62819=CARTESIAN_POINT('Ctrl Pts',(-0.439630146125636,-38.2742356128,-8.19249683682004));
#62820=CARTESIAN_POINT('Ctrl Pts',(-0.447522256504563,-38.2742356128,-8.23643142841576));
#62821=CARTESIAN_POINT('Ctrl Pts',(-0.45750317150351,-38.2742356128,-8.27997470252336));
#62822=CARTESIAN_POINT('Ctrl Pts',(-0.469532954288344,-38.2742356128,-8.32288925071818));
#62823=CARTESIAN_POINT('Ctrl Pts',(-0.482341712347726,-38.2742356128,-8.36858268300095));
#62824=CARTESIAN_POINT('Ctrl Pts',(-0.497473211468047,-38.2742356128,-8.41356385330956));
#62825=CARTESIAN_POINT('Ctrl Pts',(-0.514844778617922,-38.2742356128,-8.45759880680696));
#62826=CARTESIAN_POINT('Ctrl Pts',(-0.533782263511972,-38.2742356128,-8.50560318427461));
#62827=CARTESIAN_POINT('Ctrl Pts',(-0.555381809168105,-38.2742356128,-8.55248392532889));
#62828=CARTESIAN_POINT('Ctrl Pts',(-0.579497316992987,-38.2742356128,-8.59798785499368));
#62829=CARTESIAN_POINT('Ctrl Pts',(-0.609099788346512,-38.2742356128,-8.65384522213503));
#62830=CARTESIAN_POINT('Ctrl Pts',(-0.642493917780337,-38.2742356128,-8.70762998352329));
#62831=CARTESIAN_POINT('Ctrl Pts',(-0.679347289484414,-38.2742356128,-8.75892505849224));
#62832=CARTESIAN_POINT('Ctrl Pts',(-0.712858980986859,-38.2742356128,-8.80556895153294));
#62833=CARTESIAN_POINT('Ctrl Pts',(-0.749229201825039,-38.2742356128,-8.85015749719262));
#62834=CARTESIAN_POINT('Ctrl Pts',(-0.788176879238902,-38.2742356128,-8.8923704480671));
#62835=CARTESIAN_POINT('Ctrl Pts',(-0.824990130602421,-38.2742356128,-8.93227002808121));
#62836=CARTESIAN_POINT('Ctrl Pts',(-0.864105064693452,-38.2742356128,-8.97004925769915));
#62837=CARTESIAN_POINT('Ctrl Pts',(-0.905273940415647,-38.2742356128,-9.00539581352769));
#62838=CARTESIAN_POINT('Ctrl Pts',(-0.956525180854692,-38.2742356128,-9.0493988327912));
#62839=CARTESIAN_POINT('Ctrl Pts',(-1.01096309064526,-38.2742356128,-9.08962219803601));
#62840=CARTESIAN_POINT('Ctrl Pts',(-1.06801175261871,-38.2742356128,-9.12571954250596));
#62841=CARTESIAN_POINT('Ctrl Pts',(-1.12236508635952,-38.2742356128,-9.16011142731555));
#62842=CARTESIAN_POINT('Ctrl Pts',(-1.17908764585001,-38.2742356128,-9.19075679716307));
#62843=CARTESIAN_POINT('Ctrl Pts',(-1.23764596567446,-38.2742356128,-9.21738500781742));
#62844=CARTESIAN_POINT('Ctrl Pts',(-1.29309164983784,-38.2742356128,-9.24259781040812));
#62845=CARTESIAN_POINT('Ctrl Pts',(-1.35018262233756,-38.2742356128,-9.26420845056948));
#62846=CARTESIAN_POINT('Ctrl Pts',(-1.40844166177688,-38.2742356128,-9.28202664749419));
#62847=CARTESIAN_POINT('Ctrl Pts',(-1.46299899906197,-38.2742356128,-9.29871269980107));
#62848=CARTESIAN_POINT('Ctrl Pts',(-1.51858030850855,-38.2742356128,-9.31207260921611));
#62849=CARTESIAN_POINT('Ctrl Pts',(-1.57477777606112,-38.2742356128,-9.32199254814538));
#62850=CARTESIAN_POINT('Ctrl Pts',(-1.62868478067783,-38.2742356128,-9.33150817610776));
#62851=CARTESIAN_POINT('Ctrl Pts',(-1.68315851183546,-38.2742356128,-9.33785820793617));
#62852=CARTESIAN_POINT('Ctrl Pts',(-1.73782801715715,-38.2742356128,-9.34098723621135));
#62853=CARTESIAN_POINT('Ctrl Pts',(-1.79089269674258,-38.2742356128,-9.34402441172372));
#62854=CARTESIAN_POINT('Ctrl Pts',(-1.84414165890464,-38.2742356128,-9.34402660305071));
#62855=CARTESIAN_POINT('Ctrl Pts',(-1.89722788544739,-38.2742356128,-9.34099112391457));
#62856=CARTESIAN_POINT('Ctrl Pts',(-1.94839107668105,-38.2742356128,-9.33806560425264));
#62857=CARTESIAN_POINT('Ctrl Pts',(-1.99940296981809,-38.2742356128,-9.33231833411543));
#62858=CARTESIAN_POINT('Ctrl Pts',(-2.04994776736356,-38.2742356128,-9.32379549157948));
#62859=CARTESIAN_POINT('Ctrl Pts',(-2.06190685559861,-38.2742356128,-9.32177895514348));
#62860=CARTESIAN_POINT('Ctrl Pts',(-2.07383977686135,-38.2742356128,-9.31960726587291));
#62861=CARTESIAN_POINT('Ctrl Pts',(-2.08574231668,-38.2742356128,-9.3172814696));
#62862=CARTESIAN_POINT('Ctrl Pts',(-2.08574231668,-38.2742356128,-9.3172814696));
#62863=CARTESIAN_POINT('Ctrl Pts',(-2.08729719662647,-38.2742356128,-9.31697764277153));
#62864=CARTESIAN_POINT('Ctrl Pts',(-2.08885006320223,-38.2742356128002,
-9.3166755848767));
#62865=CARTESIAN_POINT('Ctrl Pts',(-2.09040818399078,-38.2742356127997,
-9.31637399587293));
#62866=CARTESIAN_POINT('Ctrl Pts',(-2.09088805053492,-38.2742356127995,
-9.31628111316829));
#62867=CARTESIAN_POINT('Ctrl Pts',(-2.09136804121834,-38.2742356127993,
-9.31618834238779));
#62868=CARTESIAN_POINT('Ctrl Pts',(-2.09184736274659,-38.2742356127989,
-9.31609582751137));
#62869=CARTESIAN_POINT('Ctrl Pts',(-2.09373347566305,-38.2742356127973,
-9.31573178481124));
#62870=CARTESIAN_POINT('Ctrl Pts',(-2.0956458104322,-38.2742356127953,-9.31536531693948));
#62871=CARTESIAN_POINT('Ctrl Pts',(-2.0975785896359,-38.2742356127946,-9.31499710213531));
#62872=CARTESIAN_POINT('Ctrl Pts',(-2.10028622939785,-38.2742356127937,
-9.31448126823001));
#62873=CARTESIAN_POINT('Ctrl Pts',(-2.10302673644695,-38.2742356127952,
-9.31396332695846));
#62874=CARTESIAN_POINT('Ctrl Pts',(-2.10570065575222,-38.2742356127967,
-9.31346143484423));
#62875=CARTESIAN_POINT('Ctrl Pts',(-2.10750112540457,-38.2742356127978,
-9.31312348840036));
#62876=CARTESIAN_POINT('Ctrl Pts',(-2.10926918488457,-38.2742356127987,
-9.31279324863373));
#62877=CARTESIAN_POINT('Ctrl Pts',(-2.11100388243363,-38.2742356127993,
-9.31247098633571));
#62878=CARTESIAN_POINT('Ctrl Pts',(-2.11247433135277,-38.2742356127997,
-9.31219781465339));
#62879=CARTESIAN_POINT('Ctrl Pts',(-2.11392035045784,-38.2742356127999,
-9.31193046282621));
#62880=CARTESIAN_POINT('Ctrl Pts',(-2.11537824249551,-38.2742356128,-9.31166232294267));
#62881=CARTESIAN_POINT('Ctrl Pts',(-2.11634463787306,-38.2742356128,-9.31148458060147));
#62882=CARTESIAN_POINT('Ctrl Pts',(-2.11731696466449,-38.2742356128,-9.3113063607223));
#62883=CARTESIAN_POINT('Ctrl Pts',(-2.11831853867763,-38.2742356128,-9.31112338855063));
#62884=CARTESIAN_POINT('Ctrl Pts',(-2.11872298471233,-38.2742356128,-9.31104950247899));
#62885=CARTESIAN_POINT('Ctrl Pts',(-2.11912809869579,-38.2742356128,-9.31097559323517));
#62886=CARTESIAN_POINT('Ctrl Pts',(-2.11954020693,-38.2742356128,-9.31090050519));
#62887=CARTESIAN_POINT('',(-2.3929454134173E-5,-38.2742356128,10.9643459683816));
#62888=CARTESIAN_POINT('',(5.53988693785,-38.2742356128,5.6069786219));
#62889=CARTESIAN_POINT('Ctrl Pts',(2.41089864840838E-5,-38.2742356128,10.9643459827));
#62890=CARTESIAN_POINT('Ctrl Pts',(0.00400146984433971,-38.2742356128,10.9643456323764));
#62891=CARTESIAN_POINT('Ctrl Pts',(0.00791495370935219,-38.2742356128,10.9643411554458));
#62892=CARTESIAN_POINT('Ctrl Pts',(0.011860445155913,-38.2742356128,10.9643324386718));
#62893=CARTESIAN_POINT('Ctrl Pts',(0.165738700552314,-38.2742356128,10.9639924754519));
#62894=CARTESIAN_POINT('Ctrl Pts',(0.319616215076356,-38.2742356128,10.957256326624));
#62895=CARTESIAN_POINT('Ctrl Pts',(0.472948512224986,-38.2742356128,10.9441347145538));
#62896=CARTESIAN_POINT('Ctrl Pts',(0.630182100908691,-38.2742356128,10.9306792443529));
#62897=CARTESIAN_POINT('Ctrl Pts',(0.786842159219016,-38.2742356128,10.9105091862989));
#62898=CARTESIAN_POINT('Ctrl Pts',(0.942351550939209,-38.2742356128,10.8836912177522));
#62899=CARTESIAN_POINT('Ctrl Pts',(1.09720894779707,-38.2742356128,10.8569856872874));
#62900=CARTESIAN_POINT('Ctrl Pts',(1.25092513683212,-38.2742356128,10.8236880870954));
#62901=CARTESIAN_POINT('Ctrl Pts',(1.40294280938938,-38.2742356128,10.7839166298021));
#62902=CARTESIAN_POINT('Ctrl Pts',(1.55603723521693,-38.2742356128,10.7438634681123));
#62903=CARTESIAN_POINT('Ctrl Pts',(1.70740879773239,-38.2742356128,10.6972445345565));
#62904=CARTESIAN_POINT('Ctrl Pts',(1.85650388541951,-38.2742356128,10.6442314384632));
#62905=CARTESIAN_POINT('Ctrl Pts',(2.00655796045027,-38.2742356128,10.5908773593839));
#62906=CARTESIAN_POINT('Ctrl Pts',(2.15430597357976,-38.2742356128,10.5310467305738));
#62907=CARTESIAN_POINT('Ctrl Pts',(2.29920241562008,-38.2742356128,10.464963920862));
#62908=CARTESIAN_POINT('Ctrl Pts',(2.44531547700217,-38.2742356128,10.3983262484957));
#62909=CARTESIAN_POINT('Ctrl Pts',(2.58852865334315,-38.2742356128,10.325331087339));
#62910=CARTESIAN_POINT('Ctrl Pts',(2.72830498882052,-38.2742356128,10.24625667601));
#62911=CARTESIAN_POINT('Ctrl Pts',(2.86857898067867,-38.2742356128,10.1669007300048));
#62912=CARTESIAN_POINT('Ctrl Pts',(3.00539139940937,-38.2742356128,10.0814223376914));
#62913=CARTESIAN_POINT('Ctrl Pts',(3.1382253222981,-38.2742356128,9.99014874576276));
#62914=CARTESIAN_POINT('Ctrl Pts',(3.27158660817497,-38.2742356128,9.89851278921275));
#62915=CARTESIAN_POINT('Ctrl Pts',(3.40093752166825,-38.2742356128,9.80103569854775));
#62916=CARTESIAN_POINT('Ctrl Pts',(3.52578422220404,-38.2742356128,9.69809237381965));
#62917=CARTESIAN_POINT('Ctrl Pts',(3.63868710847119,-38.2742356128,9.60499741469088));
#62918=CARTESIAN_POINT('Ctrl Pts',(3.74790663024948,-38.2742356128,9.50743272839668));
#62919=CARTESIAN_POINT('Ctrl Pts',(3.85310031128157,-38.2742356128,9.40570437828926));
#62920=CARTESIAN_POINT('Ctrl Pts',(3.96946942632073,-38.2742356128,9.29316873964397));
#62921=CARTESIAN_POINT('Ctrl Pts',(4.08091079548935,-38.2742356128,9.17553770727189));
#62922=CARTESIAN_POINT('Ctrl Pts',(4.18699742316105,-38.2742356128,9.05326075891791));
#62923=CARTESIAN_POINT('Ctrl Pts',(4.29267288764379,-38.2742356128,8.93145772307417));
#62924=CARTESIAN_POINT('Ctrl Pts',(4.39303483490137,-38.2742356128,8.8050449466975));
#62925=CARTESIAN_POINT('Ctrl Pts',(4.48769986111669,-38.2742356128,8.67450088215508));
#62926=CARTESIAN_POINT('Ctrl Pts',(4.58196381342408,-38.2742356128,8.54450990274046));
#62927=CARTESIAN_POINT('Ctrl Pts',(4.67057882212817,-38.2742356128,8.41042279546363));
#62928=CARTESIAN_POINT('Ctrl Pts',(4.75320767903444,-38.2742356128,8.27274247619464));
#62929=CARTESIAN_POINT('Ctrl Pts',(4.83538544616229,-38.2742356128,8.13581378519496));
#62930=CARTESIAN_POINT('Ctrl Pts',(4.91164206561261,-38.2742356128,7.99533123305691));
#62931=CARTESIAN_POINT('Ctrl Pts',(4.98168954890516,-38.2742356128,7.85181640625091));
#62932=CARTESIAN_POINT('Ctrl Pts',(5.05128204576803,-38.2742356128,7.70923376566466));
#62933=CARTESIAN_POINT('Ctrl Pts',(5.11474564573329,-38.2742356128,7.56365833443839));
#62934=CARTESIAN_POINT('Ctrl Pts',(5.17184371427649,-38.2742356128,7.41562486313624));
#62935=CARTESIAN_POINT('Ctrl Pts',(5.22816763835185,-38.2742356128,7.26959845259441));
#62936=CARTESIAN_POINT('Ctrl Pts',(5.27829737858524,-38.2742356128,7.12118043150776));
#62937=CARTESIAN_POINT('Ctrl Pts',(5.3220522683345,-38.2742356128,6.97090344328457));
#62938=CARTESIAN_POINT('Ctrl Pts',(5.36561634579287,-38.2742356128,6.8212818034477));
#62939=CARTESIAN_POINT('Ctrl Pts',(5.40286095423434,-38.2742356128,6.66981726674409));
#62940=CARTESIAN_POINT('Ctrl Pts',(5.43365592808345,-38.2742356128,6.51705274736088));
#62941=CARTESIAN_POINT('Ctrl Pts',(5.46427229224842,-38.2742356128,6.36517425641491));
#62942=CARTESIAN_POINT('Ctrl Pts',(5.48851348780113,-38.2742356128,6.21201176152061));
#62943=CARTESIAN_POINT('Ctrl Pts',(5.50630233117215,-38.2742356128,6.05810659766053));
#62944=CARTESIAN_POINT('Ctrl Pts',(5.52221910466512,-38.2742356128,5.92039817100981));
#62945=CARTESIAN_POINT('Ctrl Pts',(5.5329706903284,-38.2742356128,5.7820954092002));
#62946=CARTESIAN_POINT('Ctrl Pts',(5.53853645057666,-38.2742356128,5.6435933685011));
#62947=CARTESIAN_POINT('Ctrl Pts',(5.5390268466287,-38.2742356128,5.63139003042518));
#62948=CARTESIAN_POINT('Ctrl Pts',(5.53947703988333,-38.2742356128,5.61918414506667));
#62949=CARTESIAN_POINT('Ctrl Pts',(5.53988693785,-38.2742356128,5.6069786219));
#62950=CARTESIAN_POINT('',(4.6779495981,-38.2742356128,1.76615927471));
#62951=CARTESIAN_POINT('Ctrl Pts',(5.53988693785,-38.2742356128,5.6069786219));
#62952=CARTESIAN_POINT('Ctrl Pts',(5.5408707778169,-38.2742356128,5.57768291907289));
#62953=CARTESIAN_POINT('Ctrl Pts',(5.5417145820876,-38.2742356128,5.54821580128025));
#62954=CARTESIAN_POINT('Ctrl Pts',(5.54238546405316,-38.2742356128,5.51860736517105));
#62955=CARTESIAN_POINT('Ctrl Pts',(5.54360264640407,-38.2742356128,5.46488872654174));
#62956=CARTESIAN_POINT('Ctrl Pts',(5.54424776974383,-38.2742356128,5.41070491753419));
#62957=CARTESIAN_POINT('Ctrl Pts',(5.54416647607367,-38.2742356128,5.356201243868));
#62958=CARTESIAN_POINT('Ctrl Pts',(5.54408327235616,-38.2742356128,5.30041697114259));
#62959=CARTESIAN_POINT('Ctrl Pts',(5.54323922336175,-38.2742356128,5.24429785430791));
#62960=CARTESIAN_POINT('Ctrl Pts',(5.54152183085376,-38.2742356128,5.18799081545841));
#62961=CARTESIAN_POINT('Ctrl Pts',(5.53976334092991,-38.2742356128,5.13033634218082));
#62962=CARTESIAN_POINT('Ctrl Pts',(5.53708939114766,-38.2742356128,5.07248493669536));
#62963=CARTESIAN_POINT('Ctrl Pts',(5.533431865951,-38.2742356128,5.01457955231402));
#62964=CARTESIAN_POINT('Ctrl Pts',(5.53019201388825,-38.2742356128,4.9632867056636));
#62965=CARTESIAN_POINT('Ctrl Pts',(5.52618150714167,-38.2742356128,4.91195309409164));
#62966=CARTESIAN_POINT('Ctrl Pts',(5.52138355179064,-38.2742356128,4.86066207249638));
#62967=CARTESIAN_POINT('Ctrl Pts',(5.51558760341417,-38.2742356128,4.79870232264617));
#62968=CARTESIAN_POINT('Ctrl Pts',(5.50864099523777,-38.2742356128,4.73680019248161));
#62969=CARTESIAN_POINT('Ctrl Pts',(5.50056362356443,-38.2742356128,4.67509378178074));
#62970=CARTESIAN_POINT('Ctrl Pts',(5.49221771425977,-38.2742356128,4.61133590012658));
#62971=CARTESIAN_POINT('Ctrl Pts',(5.48266496019185,-38.2742356128,4.54778714929663));
#62972=CARTESIAN_POINT('Ctrl Pts',(5.47197926103978,-38.2742356128,4.48457601750013));
#62973=CARTESIAN_POINT('Ctrl Pts',(5.46089265811182,-38.2742356128,4.41899334397718));
#62974=CARTESIAN_POINT('Ctrl Pts',(5.4485869730846,-38.2742356128,4.35377433151512));
#62975=CARTESIAN_POINT('Ctrl Pts',(5.43519340909869,-38.2742356128,4.28903396005194));
#62976=CARTESIAN_POINT('Ctrl Pts',(5.42264344003186,-38.2742356128,4.22837126712776));
#62977=CARTESIAN_POINT('Ctrl Pts',(5.40913973384347,-38.2742356128,4.16813036669957));
#62978=CARTESIAN_POINT('Ctrl Pts',(5.39481880192551,-38.2742356128,4.10837559914741));
#62979=CARTESIAN_POINT('Ctrl Pts',(5.3781374913988,-38.2742356128,4.0387720399168));
#62980=CARTESIAN_POINT('Ctrl Pts',(5.36034716023229,-38.2742356128,3.96982796097921));
#62981=CARTESIAN_POINT('Ctrl Pts',(5.3417000881902,-38.2742356128,3.90161742158706));
#62982=CARTESIAN_POINT('Ctrl Pts',(5.32221924839775,-38.2742356128,3.83035697989119));
#62983=CARTESIAN_POINT('Ctrl Pts',(5.3018051238064,-38.2742356128,3.75989900003693));
#62984=CARTESIAN_POINT('Ctrl Pts',(5.28076410474724,-38.2742356128,3.69026592387477));
#62985=CARTESIAN_POINT('Ctrl Pts',(5.27503606815184,-38.2742356128,3.67130957925166));
#62986=CARTESIAN_POINT('Ctrl Pts',(5.26926164898527,-38.2742356128,3.65241415260537));
#62987=CARTESIAN_POINT('Ctrl Pts',(5.26344711753933,-38.2742356128,3.63357953459848));
#62988=CARTESIAN_POINT('Ctrl Pts',(5.24611610407497,-38.2742356128,3.57744035617824));
#62989=CARTESIAN_POINT('Ctrl Pts',(5.22843389032803,-38.2742356128,3.52185747179269));
#62990=CARTESIAN_POINT('Ctrl Pts',(5.2105541140774,-38.2742356128,3.46672743974292));
#62991=CARTESIAN_POINT('Ctrl Pts',(5.1858694840972,-38.2742356128,3.39061550059619));
#62992=CARTESIAN_POINT('Ctrl Pts',(5.1607833225832,-38.274235612979,3.31530922761688));
#62993=CARTESIAN_POINT('Ctrl Pts',(5.13571635392379,-38.2742356120079,3.24065429314394));
#62994=CARTESIAN_POINT('Ctrl Pts',(5.11431248675456,-38.2742356111787,3.17690887890189));
#62995=CARTESIAN_POINT('Ctrl Pts',(5.09292396027743,-38.2742356093749,3.11363951367482));
#62996=CARTESIAN_POINT('Ctrl Pts',(5.07177465707568,-38.2742356058314,3.05075329270464));
#62997=CARTESIAN_POINT('Ctrl Pts',(5.05292453439443,-38.2742356026731,2.99470355106825));
#62998=CARTESIAN_POINT('Ctrl Pts',(5.03426482326032,-38.2742355981201,2.93895860539514));
#62999=CARTESIAN_POINT('Ctrl Pts',(5.01591135851897,-38.2742355924515,2.88344603236812));
#63000=CARTESIAN_POINT('Ctrl Pts',(5.0101086493214,-38.2742355906593,2.86589494200869));
#63001=CARTESIAN_POINT('Ctrl Pts',(5.00433618370494,-38.2742355887626,2.84836700203233));
#63002=CARTESIAN_POINT('Ctrl Pts',(4.99859652036895,-38.2742355867898,2.83085967177776));
#63003=CARTESIAN_POINT('Ctrl Pts',(4.98176280681453,-38.2742355810037,2.77951286529167));
#63004=CARTESIAN_POINT('Ctrl Pts',(4.96522842306461,-38.2742355779867,2.72836284548135));
#63005=CARTESIAN_POINT('Ctrl Pts',(4.94899975664859,-38.2742355797489,2.67725154299494));
#63006=CARTESIAN_POINT('Ctrl Pts',(4.93277109023257,-38.2742355815112,2.62614024050852));
#63007=CARTESIAN_POINT('Ctrl Pts',(4.91684884973871,-38.2742355882266,2.57506820416811));
#63008=CARTESIAN_POINT('Ctrl Pts',(4.90118858468214,-38.2742355962476,2.52386041864114));
#63009=CARTESIAN_POINT('Ctrl Pts',(4.8873576701826,-38.2742356033317,2.47863445977162));
#63010=CARTESIAN_POINT('Ctrl Pts',(4.87370757924121,-38.2742356092055,2.43323262376226));
#63011=CARTESIAN_POINT('Ctrl Pts',(4.86023592795867,-38.2742356113118,2.38779762831885));
#63012=CARTESIAN_POINT('Ctrl Pts',(4.85845407162556,-38.2742356115904,2.38178807294382));
#63013=CARTESIAN_POINT('Ctrl Pts',(4.8566752645847,-38.274235611819,2.37577791889541));
#63014=CARTESIAN_POINT('Ctrl Pts',(4.8548994354018,-38.2742356120049,2.36976748068112));
#63015=CARTESIAN_POINT('Ctrl Pts',(4.84118585806346,-38.2742356134407,2.32335276349828));
#63016=CARTESIAN_POINT('Ctrl Pts',(4.82764687675358,-38.2742356128,2.27693340916131));
#63017=CARTESIAN_POINT('Ctrl Pts',(4.81416496783716,-38.2742356128,2.23034909238133));
#63018=CARTESIAN_POINT('Ctrl Pts',(4.81270177571342,-38.2742356128,2.2252932945841));
#63019=CARTESIAN_POINT('Ctrl Pts',(4.81123920827819,-38.2742356128,2.22023553573263));
#63020=CARTESIAN_POINT('Ctrl Pts',(4.80977707990551,-38.2742356128,2.21517559722572));
#63021=CARTESIAN_POINT('Ctrl Pts',(4.79712845252832,-38.2742356128,2.17140291767094));
#63022=CARTESIAN_POINT('Ctrl Pts',(4.78448254464563,-38.2742356128,2.12735099607628));
#63023=CARTESIAN_POINT('Ctrl Pts',(4.77169660280957,-38.2742356128,2.08292184394826));
#63024=CARTESIAN_POINT('Ctrl Pts',(4.75910524756551,-38.2742356128,2.03916884985447));
#63025=CARTESIAN_POINT('Ctrl Pts',(4.74637822653476,-38.2742356128,1.99505008609926));
#63026=CARTESIAN_POINT('Ctrl Pts',(4.73333245418105,-38.2742356128,1.95045340767228));
#63027=CARTESIAN_POINT('Ctrl Pts',(4.72050617381001,-38.2742356128,1.90660705763549));
#63028=CARTESIAN_POINT('Ctrl Pts',(4.70737184763075,-38.2742356128,1.86229877714485));
#63029=CARTESIAN_POINT('Ctrl Pts',(4.69370843473059,-38.2742356128,1.8174031505342));
#63030=CARTESIAN_POINT('Ctrl Pts',(4.69099699337357,-38.2742356128,1.80849382022039));
#63031=CARTESIAN_POINT('Ctrl Pts',(4.68826456393529,-38.2742356128,1.79956129861167));
#63032=CARTESIAN_POINT('Ctrl Pts',(4.68550919055206,-38.2742356128,1.79060451360579));
#63033=CARTESIAN_POINT('Ctrl Pts',(4.68300579177684,-38.2742356128,1.78246681265023));
#63034=CARTESIAN_POINT('Ctrl Pts',(4.68048944473333,-38.2742356128,1.77432846099333));
#63035=CARTESIAN_POINT('Ctrl Pts',(4.6779495981,-38.2742356128,1.76615927471));
#63036=CARTESIAN_POINT('',(0.665818565616232,-38.2742356128,-2.24488964565501));
#63037=CARTESIAN_POINT('Ctrl Pts',(4.67793826508075,-38.2742356128,1.76612282898476));
#63038=CARTESIAN_POINT('Ctrl Pts',(4.66625916152122,-38.2742356128,1.72856428599569));
#63039=CARTESIAN_POINT('Ctrl Pts',(4.6543341741093,-38.2742356127995,1.69115199273253));
#63040=CARTESIAN_POINT('Ctrl Pts',(4.64214427561065,-38.2742356127994,1.65382542234142));
#63041=CARTESIAN_POINT('Ctrl Pts',(4.61351356519473,-38.274235612799,1.5661556006603));
#63042=CARTESIAN_POINT('Ctrl Pts',(4.58345943425045,-38.2742356127991,1.47908977905003));
#63043=CARTESIAN_POINT('Ctrl Pts',(4.55201232353028,-38.2742356127993,1.39274184425048));
#63044=CARTESIAN_POINT('Ctrl Pts',(4.52087865885848,-38.2742356127995,1.30725457417742));
#63045=CARTESIAN_POINT('Ctrl Pts',(4.48838047126944,-38.2742356127998,1.22247155017572));
#63046=CARTESIAN_POINT('Ctrl Pts',(4.45453692836458,-38.2742356127999,1.13845087330955));
#63047=CARTESIAN_POINT('Ctrl Pts',(4.42346864479657,-38.2742356128,1.06132011244941));
#63048=CARTESIAN_POINT('Ctrl Pts',(4.39126697360346,-38.2742356128,0.98483161327673));
#63049=CARTESIAN_POINT('Ctrl Pts',(4.3579300357631,-38.2742356128,0.908984266315246));
#63050=CARTESIAN_POINT('Ctrl Pts',(4.35495212268333,-38.2742356128,0.902208994763186));
#63051=CARTESIAN_POINT('Ctrl Pts',(4.351965136915,-38.2742356128,0.895438807446463));
#63052=CARTESIAN_POINT('Ctrl Pts',(4.34896906853151,-38.2742356128,0.888673684522422));
#63053=CARTESIAN_POINT('Ctrl Pts',(4.31737828769537,-38.2742356128,0.817341695973576));
#63054=CARTESIAN_POINT('Ctrl Pts',(4.28477673375403,-38.2742356128,0.746569834090829));
#63055=CARTESIAN_POINT('Ctrl Pts',(4.2511436165332,-38.2742356128,0.676318084245987));
#63056=CARTESIAN_POINT('Ctrl Pts',(4.218057486707,-38.2742356128,0.607208863693416));
#63057=CARTESIAN_POINT('Ctrl Pts',(4.18397338482654,-38.2742356128,0.538603157868374));
#63058=CARTESIAN_POINT('Ctrl Pts',(4.14884788520354,-38.2742356128,0.47041966398888));
#63059=CARTESIAN_POINT('Ctrl Pts',(4.113432034225,-38.2742356128,0.401672557631684));
#63060=CARTESIAN_POINT('Ctrl Pts',(4.0769545471813,-38.2742356128921,0.333349597983933));
#63061=CARTESIAN_POINT('Ctrl Pts',(4.03940122487231,-38.274235612524,0.265434758630409));
#63062=CARTESIAN_POINT('Ctrl Pts',(4.00184790256332,-38.2742356121559,0.197519919276885));
#63063=CARTESIAN_POINT('Ctrl Pts',(3.96321789575712,-38.2742356113281,0.130011089054838));
#63064=CARTESIAN_POINT('Ctrl Pts',(3.92344185138896,-38.2742356083775,0.0629003525950581));
#63065=CARTESIAN_POINT('Ctrl Pts',(3.88612562855177,-38.2742356056093,-6.01362187938465E-5));
#63066=CARTESIAN_POINT('Ctrl Pts',(3.84781048176032,-38.2742356015818,-0.0626636364542783));
#63067=CARTESIAN_POINT('Ctrl Pts',(3.80840389490981,-38.2742355992333,-0.124899081227493));
#63068=CARTESIAN_POINT('Ctrl Pts',(3.77176973331138,-38.27423559705,-0.18275599102843));
#63069=CARTESIAN_POINT('Ctrl Pts',(3.73419160393593,-38.2742355967026,-0.240295480291296));
#63070=CARTESIAN_POINT('Ctrl Pts',(3.69557523382837,-38.2742355994774,-0.297467499682426));
#63071=CARTESIAN_POINT('Ctrl Pts',(3.68694928634095,-38.2742356000972,-0.310238322927692));
#63072=CARTESIAN_POINT('Ctrl Pts',(3.67827147240523,-38.2742356008542,-0.3229906163664));
#63073=CARTESIAN_POINT('Ctrl Pts',(3.66954064238787,-38.2742356017192,-0.335723465675104));
#63074=CARTESIAN_POINT('Ctrl Pts',(3.63311022119051,-38.2742356053286,-0.388852785846986));
#63075=CARTESIAN_POINT('Ctrl Pts',(3.59575012859676,-38.274235608571,-0.441644506020237));
#63076=CARTESIAN_POINT('Ctrl Pts',(3.5573773434737,-38.2742356103788,-0.493982525844108));
#63077=CARTESIAN_POINT('Ctrl Pts',(3.52096146858376,-38.2742356120944,-0.543651445516754));
#63078=CARTESIAN_POINT('Ctrl Pts',(3.48363327179107,-38.274235612611,-0.592911952877165));
#63079=CARTESIAN_POINT('Ctrl Pts',(3.4453206588264,-38.274235612743,-0.641618100247041));
#63080=CARTESIAN_POINT('Ctrl Pts',(3.4244230264332,-38.2742356128151,-0.668184890770134));
#63081=CARTESIAN_POINT('Ctrl Pts',(3.40323251844803,-38.2742356128,-0.69458590493586));
#63082=CARTESIAN_POINT('Ctrl Pts',(3.38173771803535,-38.2742356128,-0.720790831280737));
#63083=CARTESIAN_POINT('Ctrl Pts',(3.33624725963509,-38.2742356128,-0.77624955101233));
#63084=CARTESIAN_POINT('Ctrl Pts',(3.28938062812393,-38.2742356128,-0.830852886945385));
#63085=CARTESIAN_POINT('Ctrl Pts',(3.24111081333509,-38.2742356128,-0.884357982845603));
#63086=CARTESIAN_POINT('Ctrl Pts',(3.19288461412186,-38.2742356128,-0.937814732681796));
#63087=CARTESIAN_POINT('Ctrl Pts',(3.14325806188673,-38.2742356128,-0.990174807210689));
#63088=CARTESIAN_POINT('Ctrl Pts',(3.09224670761339,-38.2742356128,-1.04122585806989));
#63089=CARTESIAN_POINT('Ctrl Pts',(3.07805424639482,-38.2742356128,-1.05542936373657));
#63090=CARTESIAN_POINT('Ctrl Pts',(3.06375482962459,-38.2742356128,-1.06953173993419));
#63091=CARTESIAN_POINT('Ctrl Pts',(3.04934932888766,-38.2742356128,-1.08352889162963));
#63092=CARTESIAN_POINT('Ctrl Pts',(2.99733269917098,-38.2742356128,-1.13407101926035));
#63093=CARTESIAN_POINT('Ctrl Pts',(2.94390821224003,-38.2742356128,-1.18325961424795));
#63094=CARTESIAN_POINT('Ctrl Pts',(2.88913019863473,-38.2742356128,-1.2309284391068));
#63095=CARTESIAN_POINT('Ctrl Pts',(2.83542091306856,-38.2742356128,-1.27766723736619));
#63096=CARTESIAN_POINT('Ctrl Pts',(2.78041078264352,-38.2742356128,-1.32294475248435));
#63097=CARTESIAN_POINT('Ctrl Pts',(2.7241807257774,-38.2742356128,-1.36664371639806));
#63098=CARTESIAN_POINT('Ctrl Pts',(2.68656652166145,-38.2742356128,-1.39587544476389));
#63099=CARTESIAN_POINT('Ctrl Pts',(2.64840877536037,-38.2742356128,-1.4244005783711));
#63100=CARTESIAN_POINT('Ctrl Pts',(2.60972219620018,-38.2742356128,-1.45220579524711));
#63101=CARTESIAN_POINT('Ctrl Pts',(2.55332475186832,-38.2742356128,-1.49274034766661));
#63102=CARTESIAN_POINT('Ctrl Pts',(2.49581071755516,-38.2742356128,-1.53173612384503));
#63103=CARTESIAN_POINT('Ctrl Pts',(2.43730150766331,-38.2742356128,-1.56914474154156));
#63104=CARTESIAN_POINT('Ctrl Pts',(2.37879229777147,-38.2742356128,-1.60655335923809));
#63105=CARTESIAN_POINT('Ctrl Pts',(2.31928819316852,-38.2742356128,-1.64237451439411));
#63106=CARTESIAN_POINT('Ctrl Pts',(2.25892891673801,-38.2742356128,-1.6766100621915));
#63107=CARTESIAN_POINT('Ctrl Pts',(2.19511841977279,-38.2742356128,-1.71280312890831));
#63108=CARTESIAN_POINT('Ctrl Pts',(2.13031943918726,-38.2742356128252,-1.74724581047013));
#63109=CARTESIAN_POINT('Ctrl Pts',(2.06475207097091,-38.2742356127748,-1.77998075758362));
#63110=CARTESIAN_POINT('Ctrl Pts',(1.9952421880732,-38.2742356127214,-1.81468403152032));
#63111=CARTESIAN_POINT('Ctrl Pts',(1.92486912697262,-38.274235612856,-1.84746868240433));
#63112=CARTESIAN_POINT('Ctrl Pts',(1.8538610151458,-38.2742356108741,-1.87843249901246));
#63113=CARTESIAN_POINT('Ctrl Pts',(1.84076584838186,-38.2742356105085,-1.88414278100278));
#63114=CARTESIAN_POINT('Ctrl Pts',(1.82764898574597,-38.2742356100572,-1.88979124085339));
#63115=CARTESIAN_POINT('Ctrl Pts',(1.81451172471327,-38.2742356094821,-1.89537862184467));
#63116=CARTESIAN_POINT('Ctrl Pts',(1.73807179708742,-38.2742356061358,-1.92788912746134));
#63117=CARTESIAN_POINT('Ctrl Pts',(1.66096465259571,-38.2742356025828,-1.95834639660289));
#63118=CARTESIAN_POINT('Ctrl Pts',(1.58339648228159,-38.2742356015641,-1.98692473901088));
#63119=CARTESIAN_POINT('Ctrl Pts',(1.50608662566594,-38.2742356005489,-2.01540791123124));
#63120=CARTESIAN_POINT('Ctrl Pts',(1.42831878001412,-38.2742356016823,-2.04202631360568));
#63121=CARTESIAN_POINT('Ctrl Pts',(1.35024806210187,-38.2742356035753,-2.06695847219112));
#63122=CARTESIAN_POINT('Ctrl Pts',(1.27521671791387,-38.2742356053945,-2.09091999607869));
#63123=CARTESIAN_POINT('Ctrl Pts',(1.19990534194343,-38.2742356077503,-2.11332534295206));
#63124=CARTESIAN_POINT('Ctrl Pts',(1.12440899952419,-38.2742356094292,-2.13431684042754));
#63125=CARTESIAN_POINT('Ctrl Pts',(1.05063454131336,-38.2742356110698,-2.15482957394101));
#63126=CARTESIAN_POINT('Ctrl Pts',(0.976683314121403,-38.2742356120552,
-2.17399333744373));
#63127=CARTESIAN_POINT('Ctrl Pts',(0.902605394673177,-38.2742356124601,
-2.19190749111279));
#63128=CARTESIAN_POINT('Ctrl Pts',(0.834186928837262,-38.2742356128341,
-2.2084530274874));
#63129=CARTESIAN_POINT('Ctrl Pts',(0.765659995525827,-38.2742356127997,
-2.22393298752294));
#63130=CARTESIAN_POINT('Ctrl Pts',(0.697035032190242,-38.2742356128,-2.23838703956805));
#63131=CARTESIAN_POINT('Ctrl Pts',(0.691358497472616,-38.2742356128,-2.23958265300457));
#63132=CARTESIAN_POINT('Ctrl Pts',(0.68568127619484,-38.2742356128,-2.24077122154839));
#63133=CARTESIAN_POINT('Ctrl Pts',(0.680003365706886,-38.2742356128,-2.24195275347034));
#63134=CARTESIAN_POINT('Ctrl Pts',(0.675275609675362,-38.2742356128,-2.24293656515288));
#63135=CARTESIAN_POINT('Ctrl Pts',(0.670548709585667,-38.2742356128,-2.24391524728333));
#63136=CARTESIAN_POINT('Ctrl Pts',(0.665818566089,-38.2742356128,-2.24488964795));
#63137=CARTESIAN_POINT('',(-0.665819792855,-38.2742356128,-2.24488937901));
#63138=CARTESIAN_POINT('Origin',(0.000369776183994502,-38.2742356128,0.228538425659855));
#63139=CARTESIAN_POINT('',(-4.67790721121502,-38.2742356127993,1.7660251822171));
#63140=CARTESIAN_POINT('Ctrl Pts',(-0.665819792855,-38.2742356128,-2.24488937901));
#63141=CARTESIAN_POINT('Ctrl Pts',(-0.704646928243065,-38.2742356128,-2.23689100011484));
#63142=CARTESIAN_POINT('Ctrl Pts',(-0.743453331885261,-38.2742356128,-2.22856728027694));
#63143=CARTESIAN_POINT('Ctrl Pts',(-0.782230669443798,-38.2742356128,-2.21991217212279));
#63144=CARTESIAN_POINT('Ctrl Pts',(-0.861978408748563,-38.2742356128,-2.2021124635252));
#63145=CARTESIAN_POINT('Ctrl Pts',(-0.941609929902936,-38.2742356128618,
-2.18290567003262));
#63146=CARTESIAN_POINT('Ctrl Pts',(-1.02105429711175,-38.274235612313,-2.16219578205612));
#63147=CARTESIAN_POINT('Ctrl Pts',(-1.10290476162442,-38.2742356117475,
-2.14085866262982));
#63148=CARTESIAN_POINT('Ctrl Pts',(-1.18455818824905,-38.2742356103604,
-2.11792477960474));
#63149=CARTESIAN_POINT('Ctrl Pts',(-1.26591655734601,-38.2742356089745,
-2.09323731023742));
#63150=CARTESIAN_POINT('Ctrl Pts',(-1.3439080125386,-38.274235607646,-2.06957150077798));
#63151=CARTESIAN_POINT('Ctrl Pts',(-1.42162941951018,-38.2742356065559,
-2.0442927105919));
#63152=CARTESIAN_POINT('Ctrl Pts',(-1.49895641008838,-38.2742356071964,
-2.0172372185917));
#63153=CARTESIAN_POINT('Ctrl Pts',(-1.52916899268689,-38.2742356074466,
-2.00666631339175));
#63154=CARTESIAN_POINT('Ctrl Pts',(-1.55932085791326,-38.2742356079481,
-1.99582401911051));
#63155=CARTESIAN_POINT('Ctrl Pts',(-1.58940238356075,-38.2742356086409,
-1.98470018387681));
#63156=CARTESIAN_POINT('Ctrl Pts',(-1.65827743543357,-38.2742356102272,
-1.95923090623033));
#63157=CARTESIAN_POINT('Ctrl Pts',(-1.72679211337431,-38.2742356121567,
-1.93228407763729));
#63158=CARTESIAN_POINT('Ctrl Pts',(-1.79480399594728,-38.2742356125605,
-1.90371427925461));
#63159=CARTESIAN_POINT('Ctrl Pts',(-1.80225554318575,-38.2742356126047,
-1.90058410267092));
#63160=CARTESIAN_POINT('Ctrl Pts',(-1.80970100322648,-38.2742356126389,
-1.8974344502975));
#63161=CARTESIAN_POINT('Ctrl Pts',(-1.81714014934601,-38.2742356126655,
-1.8942651365982));
#63162=CARTESIAN_POINT('Ctrl Pts',(-1.88215012246053,-38.2742356128977,
-1.86656881297826));
#63163=CARTESIAN_POINT('Ctrl Pts',(-1.9466690398652,-38.2742356128,-1.83737781683262));
#63164=CARTESIAN_POINT('Ctrl Pts',(-2.01050469177384,-38.2742356128,-1.8066078872014));
#63165=CARTESIAN_POINT('Ctrl Pts',(-2.02064600006318,-38.2742356128,-1.80171959463914));
#63166=CARTESIAN_POINT('Ctrl Pts',(-2.03076996375684,-38.2742356128,-1.79679149040022));
#63167=CARTESIAN_POINT('Ctrl Pts',(-2.04087569583709,-38.2742356128,-1.79182328305228));
#63168=CARTESIAN_POINT('Ctrl Pts',(-2.10389818516883,-38.2742356128,-1.76083999632974));
#63169=CARTESIAN_POINT('Ctrl Pts',(-2.16623248706984,-38.2742356128,-1.72828190095184));
#63170=CARTESIAN_POINT('Ctrl Pts',(-2.22770535961108,-38.2742356128,-1.69410472600633));
#63171=CARTESIAN_POINT('Ctrl Pts',(-2.28968314957015,-38.2742356128,-1.65964683128625));
#63172=CARTESIAN_POINT('Ctrl Pts',(-2.3507852148703,-38.2742356128,-1.62354325629355));
#63173=CARTESIAN_POINT('Ctrl Pts',(-2.41085879928969,-38.2742356128,-1.58579533568302));
#63174=CARTESIAN_POINT('Ctrl Pts',(-2.45562897187998,-38.2742356128,-1.5576634880999));
#63175=CARTESIAN_POINT('Ctrl Pts',(-2.4998261921559,-38.2742356128,-1.52862112939009));
#63176=CARTESIAN_POINT('Ctrl Pts',(-2.54341537278903,-38.2742356128,-1.49867112182991));
#63177=CARTESIAN_POINT('Ctrl Pts',(-2.6033372665094,-38.2742356128,-1.45749895149135));
#63178=CARTESIAN_POINT('Ctrl Pts',(-2.66210134842506,-38.2742356128,-1.41461433672546));
#63179=CARTESIAN_POINT('Ctrl Pts',(-2.71958929396136,-38.2742356128,-1.37009585559334));
#63180=CARTESIAN_POINT('Ctrl Pts',(-2.76961721589123,-38.2742356128,-1.33135439287906));
#63181=CARTESIAN_POINT('Ctrl Pts',(-2.8186791267139,-38.2742356128,-1.29137639594389));
#63182=CARTESIAN_POINT('Ctrl Pts',(-2.8667147611275,-38.2742356128,-1.25024041056458));
#63183=CARTESIAN_POINT('Ctrl Pts',(-2.92283268399407,-38.2742356128,-1.20218304476235));
#63184=CARTESIAN_POINT('Ctrl Pts',(-2.97757449459017,-38.2742356128,-1.15252277207788));
#63185=CARTESIAN_POINT('Ctrl Pts',(-3.0308692710291,-38.2742356128,-1.10142066322325));
#63186=CARTESIAN_POINT('Ctrl Pts',(-3.08490320715715,-38.2742356128,-1.04960980538011));
#63187=CARTESIAN_POINT('Ctrl Pts',(-3.13744957757337,-38.2742356128,-0.996317007609141));
#63188=CARTESIAN_POINT('Ctrl Pts',(-3.18846749637239,-38.2742356128,-0.941752210541535));
#63189=CARTESIAN_POINT('Ctrl Pts',(-3.19984156223126,-38.2742356128,-0.929587394531143));
#63190=CARTESIAN_POINT('Ctrl Pts',(-3.21113979101621,-38.2742356128,-0.917359513398042));
#63191=CARTESIAN_POINT('Ctrl Pts',(-3.22236195773395,-38.2742356128,-0.90507115917739));
#63192=CARTESIAN_POINT('Ctrl Pts',(-3.26759437276338,-38.2742356128,-0.855541335559813));
#63193=CARTESIAN_POINT('Ctrl Pts',(-3.3115962220051,-38.2742356130343,-0.805026964631294));
#63194=CARTESIAN_POINT('Ctrl Pts',(-3.35442080548355,-38.2742356125657,
-0.753747455454356));
#63195=CARTESIAN_POINT('Ctrl Pts',(-3.39860538542766,-38.2742356120822,
-0.70083944354426));
#63196=CARTESIAN_POINT('Ctrl Pts',(-3.44153700222848,-38.2742356130572,
-0.647116843795417));
#63197=CARTESIAN_POINT('Ctrl Pts',(-3.48328433696875,-38.2742355963193,
-0.592765882196818));
#63198=CARTESIAN_POINT('Ctrl Pts',(-3.5004252969157,-38.2742355894469,-0.570450022714151));
#63199=CARTESIAN_POINT('Ctrl Pts',(-3.5173667001797,-38.2742355791753,-0.548027614240496));
#63200=CARTESIAN_POINT('Ctrl Pts',(-3.53411360439285,-38.2742355614603,
-0.525509056348052));
#63201=CARTESIAN_POINT('Ctrl Pts',(-3.5758719966679,-38.2742355172881,-0.469359050235111));
#63202=CARTESIAN_POINT('Ctrl Pts',(-3.61643933142103,-38.2742354330541,
-0.412633362231607));
#63203=CARTESIAN_POINT('Ctrl Pts',(-3.65591884381001,-38.2742353633462,
-0.355511048503402));
#63204=CARTESIAN_POINT('Ctrl Pts',(-3.66231665555709,-38.2742353520498,
-0.346254150743627));
#63205=CARTESIAN_POINT('Ctrl Pts',(-3.66868591455307,-38.2742353413087,
-0.336986727039308));
#63206=CARTESIAN_POINT('Ctrl Pts',(-3.67502707437779,-38.2742353315075,
-0.32770941450126));
#63207=CARTESIAN_POINT('Ctrl Pts',(-3.71582855026059,-38.274235268443,-0.268015595982058));
#63208=CARTESIAN_POINT('Ctrl Pts',(-3.75546633556578,-38.2742352456737,
-0.20791359818607));
#63209=CARTESIAN_POINT('Ctrl Pts',(-3.79406195827873,-38.2742352691212,
-0.147455189639169));
#63210=CARTESIAN_POINT('Ctrl Pts',(-3.79847911440783,-38.2742352718047,
-0.140535901619011));
#63211=CARTESIAN_POINT('Ctrl Pts',(-3.80288260521456,-38.2742352750323,
-0.133611891455309));
#63212=CARTESIAN_POINT('Ctrl Pts',(-3.80727260057058,-38.274235278769,-0.1266831960356));
#63213=CARTESIAN_POINT('Ctrl Pts',(-3.84951550837526,-38.2742353147257,
-0.0600115442261541));
#63214=CARTESIAN_POINT('Ctrl Pts',(-3.89050327927577,-38.274235371207,0.00711033372151271));
#63215=CARTESIAN_POINT('Ctrl Pts',(-3.93033830324993,-38.2742354234395,
0.074631574892402));
#63216=CARTESIAN_POINT('Ctrl Pts',(-3.96932598119582,-38.2742354745609,
0.140716545921541));
#63217=CARTESIAN_POINT('Ctrl Pts',(-4.00721011573223,-38.2742355208942,
0.207185040203976));
#63218=CARTESIAN_POINT('Ctrl Pts',(-4.04405961795798,-38.2742355520696,
0.274037052391819));
#63219=CARTESIAN_POINT('Ctrl Pts',(-4.08211043356015,-38.2742355842614,
0.343068475742127));
#63220=CARTESIAN_POINT('Ctrl Pts',(-4.11905913677954,-38.2742356005673,
0.412509522792078));
#63221=CARTESIAN_POINT('Ctrl Pts',(-4.15493864924535,-38.2742356072897,
0.482399519863388));
#63222=CARTESIAN_POINT('Ctrl Pts',(-4.18875568288618,-38.2742356136257,
0.548271997488862));
#63223=CARTESIAN_POINT('Ctrl Pts',(-4.22162316150445,-38.2742356127982,
0.614544288831008));
#63224=CARTESIAN_POINT('Ctrl Pts',(-4.25352261766768,-38.2742356127999,
0.681270513461267));
#63225=CARTESIAN_POINT('Ctrl Pts',(-4.25546814469304,-38.2742356128,0.685340102380078));
#63226=CARTESIAN_POINT('Ctrl Pts',(-4.2574100553188,-38.2742356128,0.689411384115315));
#63227=CARTESIAN_POINT('Ctrl Pts',(-4.25934833912097,-38.2742356128,0.693484372475847));
#63228=CARTESIAN_POINT('Ctrl Pts',(-4.28903323078085,-38.2742356128,0.755862347300288));
#63229=CARTESIAN_POINT('Ctrl Pts',(-4.31789233067801,-38.2742356128,0.818650643278417));
#63230=CARTESIAN_POINT('Ctrl Pts',(-4.34595980192137,-38.2742356128,0.881889756801076));
#63231=CARTESIAN_POINT('Ctrl Pts',(-4.37622528401063,-38.2742356128,0.950081231589276));
#63232=CARTESIAN_POINT('Ctrl Pts',(-4.40556985037429,-38.2742356127999,
1.01879649029968));
#63233=CARTESIAN_POINT('Ctrl Pts',(-4.43400163081888,-38.2742356127999,
1.08803594876579));
#63234=CARTESIAN_POINT('Ctrl Pts',(-4.46837585055085,-38.2742356127998,
1.17174693422715));
#63235=CARTESIAN_POINT('Ctrl Pts',(-4.50141511800001,-38.2742356127997,
1.25622383278628));
#63236=CARTESIAN_POINT('Ctrl Pts',(-4.53309301902471,-38.2742356127996,
1.34140008502369));
#63237=CARTESIAN_POINT('Ctrl Pts',(-4.5726759465089,-38.2742356127996,1.44783155007117));
#63238=CARTESIAN_POINT('Ctrl Pts',(-4.61012817527797,-38.2742356127997,
1.55535047338883));
#63239=CARTESIAN_POINT('Ctrl Pts',(-4.64538460757811,-38.2742356127999,
1.66376470978849));
#63240=CARTESIAN_POINT('Ctrl Pts',(-4.65528938830893,-38.2742356128,1.69422210917864));
#63241=CARTESIAN_POINT('Ctrl Pts',(-4.66502111917286,-38.2742356128,1.7247501570161));
#63242=CARTESIAN_POINT('Ctrl Pts',(-4.67457931908424,-38.2742356128,1.75534499646853));
#63243=CARTESIAN_POINT('Ctrl Pts',(-4.6756911332579,-38.2742356128,1.75890380214947));
#63244=CARTESIAN_POINT('Ctrl Pts',(-4.67680044999003,-38.2742356128,1.76246301601769));
#63245=CARTESIAN_POINT('Ctrl Pts',(-4.67790796861,-38.2742356128,1.76602494395));
#63246=CARTESIAN_POINT('',(-5.53988688529846,-38.2742356128,5.60698050627013));
#63247=CARTESIAN_POINT('Ctrl Pts',(-4.67800175055493,-38.2742356128,1.7663265757088));
#63248=CARTESIAN_POINT('Ctrl Pts',(-4.69251924365702,-38.2742356128,1.8130288213493));
#63249=CARTESIAN_POINT('Ctrl Pts',(-4.70639030202568,-38.274235612792,1.85910573504843));
#63250=CARTESIAN_POINT('Ctrl Pts',(-4.71985822559416,-38.2742356127938,
1.90464595121774));
#63251=CARTESIAN_POINT('Ctrl Pts',(-4.73322084691452,-38.2742356127955,
1.94983010008994));
#63252=CARTESIAN_POINT('Ctrl Pts',(-4.74618665047486,-38.2742356127992,
1.99448599975856));
#63253=CARTESIAN_POINT('Ctrl Pts',(-4.75894398307504,-38.2742356127998,
2.03868484514955));
#63254=CARTESIAN_POINT('Ctrl Pts',(-4.76431621360322,-38.2742356128,2.05729738696853));
#63255=CARTESIAN_POINT('Ctrl Pts',(-4.76965087070964,-38.2742356128,2.07582868278896));
#63256=CARTESIAN_POINT('Ctrl Pts',(-4.77495939222068,-38.2742356128,2.09428318197623));
#63257=CARTESIAN_POINT('Ctrl Pts',(-4.78796234557368,-38.2742356128,2.13948653880281));
#63258=CARTESIAN_POINT('Ctrl Pts',(-4.80084040354426,-38.2742356128176,
2.18432693740341));
#63259=CARTESIAN_POINT('Ctrl Pts',(-4.81375974350727,-38.2742356127822,
2.22898466812738));
#63260=CARTESIAN_POINT('Ctrl Pts',(-4.82734652173961,-38.274235612745,2.27594950421374));
#63261=CARTESIAN_POINT('Ctrl Pts',(-4.84097877771399,-38.2742356128325,
2.32271208442447));
#63262=CARTESIAN_POINT('Ctrl Pts',(-4.85479666640947,-38.2742356114848,
2.36946043386112));
#63263=CARTESIAN_POINT('Ctrl Pts',(-4.8587801405254,-38.2742356110963,2.38293722789582));
#63264=CARTESIAN_POINT('Ctrl Pts',(-4.86277872827033,-38.2742356105678,
2.39641271970806));
#63265=CARTESIAN_POINT('Ctrl Pts',(-4.86679505182229,-38.274235609794,2.40989114382001));
#63266=CARTESIAN_POINT('Ctrl Pts',(-4.88059037731783,-38.2742356071361,
2.45618702745232));
#63267=CARTESIAN_POINT('Ctrl Pts',(-4.89456039340916,-38.2742356002741,
2.50239264268077));
#63268=CARTESIAN_POINT('Ctrl Pts',(-4.90873520412703,-38.2742355926928,
2.54846227156529));
#63269=CARTESIAN_POINT('Ctrl Pts',(-4.91028381252858,-38.2742355918645,
2.55349541209652));
#63270=CARTESIAN_POINT('Ctrl Pts',(-4.91183481649938,-38.2742355910419,
2.55852691419768));
#63271=CARTESIAN_POINT('Ctrl Pts',(-4.91338821986879,-38.2742355902393,
2.56355670680289));
#63272=CARTESIAN_POINT('Ctrl Pts',(-4.92878136479561,-38.2742355822858,
2.61339844659059));
#63273=CARTESIAN_POINT('Ctrl Pts',(-4.94446242793141,-38.2742355777817,
2.66322253982865));
#63274=CARTESIAN_POINT('Ctrl Pts',(-4.96043781291716,-38.2742355779049,
2.71312250655352));
#63275=CARTESIAN_POINT('Ctrl Pts',(-4.97766141629314,-38.2742355780377,
2.76692134996855));
#63276=CARTESIAN_POINT('Ctrl Pts',(-4.99522708121126,-38.2742355830336,
2.82080823788669));
#63277=CARTESIAN_POINT('Ctrl Pts',(-5.01308247143858,-38.2742355888683,
2.87488233891121));
#63278=CARTESIAN_POINT('Ctrl Pts',(-5.03196312008577,-38.2742355950381,
2.93206138061001));
#63279=CARTESIAN_POINT('Ctrl Pts',(-5.05116721886563,-38.2742356017569,
2.98944941342246));
#63280=CARTESIAN_POINT('Ctrl Pts',(-5.07057244294407,-38.2742356059748,
3.04714821864261));
#63281=CARTESIAN_POINT('Ctrl Pts',(-5.0926331575463,-38.2742356107698,3.11274276522994));
#63282=CARTESIAN_POINT('Ctrl Pts',(-5.11495343239751,-38.2742356123442,
3.17873841755785));
#63283=CARTESIAN_POINT('Ctrl Pts',(-5.1372834033019,-38.2742356126751,3.24527209500931));
#63284=CARTESIAN_POINT('Ctrl Pts',(-5.14793271821097,-38.2742356128329,
3.27700245803906));
#63285=CARTESIAN_POINT('Ctrl Pts',(-5.15858332970118,-38.2742356128,3.30885507470597));
#63286=CARTESIAN_POINT('Ctrl Pts',(-5.1692042386179,-38.2742356128,3.34084464185392));
#63287=CARTESIAN_POINT('Ctrl Pts',(-5.18615827832582,-38.2742356128,3.39190923490501));
#63288=CARTESIAN_POINT('Ctrl Pts',(-5.2030376480001,-38.2742356128,3.44329909325076));
#63289=CARTESIAN_POINT('Ctrl Pts',(-5.21971989492434,-38.2742356128,3.49509480363394));
#63290=CARTESIAN_POINT('Ctrl Pts',(-5.23206581250308,-38.2742356128,3.53342690447306));
#63291=CARTESIAN_POINT('Ctrl Pts',(-5.24430626641809,-38.2742356128,3.57198986757135));
#63292=CARTESIAN_POINT('Ctrl Pts',(-5.2563876606808,-38.2742356128,3.61080945089639));
#63293=CARTESIAN_POINT('Ctrl Pts',(-5.26204241065736,-38.2742356128,3.62897912842896));
#63294=CARTESIAN_POINT('Ctrl Pts',(-5.2676622425971,-38.2742356128,3.64720481174824));
#63295=CARTESIAN_POINT('Ctrl Pts',(-5.2732416422671,-38.2742356128,3.66548897551996));
#63296=CARTESIAN_POINT('Ctrl Pts',(-5.29415732881792,-38.2742356128,3.73403144620004));
#63297=CARTESIAN_POINT('Ctrl Pts',(-5.31450074962474,-38.2742356128,3.80338813483685));
#63298=CARTESIAN_POINT('Ctrl Pts',(-5.33397236668635,-38.2742356128,3.87353289876993));
#63299=CARTESIAN_POINT('Ctrl Pts',(-5.35283131746884,-38.2742356128,3.94147058707169));
#63300=CARTESIAN_POINT('Ctrl Pts',(-5.37087127259599,-38.2742356128,4.01014719863215));
#63301=CARTESIAN_POINT('Ctrl Pts',(-5.38783722079999,-38.2742356128,4.07949471936758));
#63302=CARTESIAN_POINT('Ctrl Pts',(-5.40408962754407,-38.2742356128,4.14592567271799));
#63303=CARTESIAN_POINT('Ctrl Pts',(-5.41935563770956,-38.2742356128,4.21297193948276));
#63304=CARTESIAN_POINT('Ctrl Pts',(-5.43344131574358,-38.2742356128,4.28053748855896));
#63305=CARTESIAN_POINT('Ctrl Pts',(-5.4454597515054,-38.2742356128,4.33818698255723));
#63306=CARTESIAN_POINT('Ctrl Pts',(-5.45661884192655,-38.2742356128,4.39621219347407));
#63307=CARTESIAN_POINT('Ctrl Pts',(-5.46682548455427,-38.2742356128,4.45454748070309));
#63308=CARTESIAN_POINT('Ctrl Pts',(-5.47770583464895,-38.2742356128,4.51673329155941));
#63309=CARTESIAN_POINT('Ctrl Pts',(-5.48750209793833,-38.2742356128,4.57926820462705));
#63310=CARTESIAN_POINT('Ctrl Pts',(-5.49613554366455,-38.2742356128,4.6420318749869));
#63311=CARTESIAN_POINT('Ctrl Pts',(-5.50453362460369,-38.2742356128,4.70308448369432));
#63312=CARTESIAN_POINT('Ctrl Pts',(-5.51183107041303,-38.2742356128,4.76435340279378));
#63313=CARTESIAN_POINT('Ctrl Pts',(-5.51799936991938,-38.2742356128,4.82570765700624));
#63314=CARTESIAN_POINT('Ctrl Pts',(-5.5239505945413,-38.2742356128,4.88490273142708));
#63315=CARTESIAN_POINT('Ctrl Pts',(-5.52885055510356,-38.2742356128,4.94417709295067));
#63316=CARTESIAN_POINT('Ctrl Pts',(-5.53271894510559,-38.2742356128,5.003396179467));
#63317=CARTESIAN_POINT('Ctrl Pts',(-5.53470010105145,-38.2742356128,5.03372462238493));
#63318=CARTESIAN_POINT('Ctrl Pts',(-5.53641144935291,-38.2742356128,5.06403830324197));
#63319=CARTESIAN_POINT('Ctrl Pts',(-5.53786073495758,-38.2742356128,5.09431751427075));
#63320=CARTESIAN_POINT('Ctrl Pts',(-5.54057010536452,-38.2742356128,5.15092305705868));
#63321=CARTESIAN_POINT('Ctrl Pts',(-5.54236123784421,-38.2742356128,5.20742199664858));
#63322=CARTESIAN_POINT('Ctrl Pts',(-5.54331935811328,-38.2742356128,5.26367049854319));
#63323=CARTESIAN_POINT('Ctrl Pts',(-5.54427311748046,-38.2742356128,5.31966298435481));
#63324=CARTESIAN_POINT('Ctrl Pts',(-5.5444011346495,-38.2742356128,5.3754072468512));
#63325=CARTESIAN_POINT('Ctrl Pts',(-5.5438384561933,-38.2742356128,5.43074893164346));
#63326=CARTESIAN_POINT('Ctrl Pts',(-5.54327577773709,-38.2742356128,5.48609061643572));
#63327=CARTESIAN_POINT('Ctrl Pts',(-5.54202208977835,-38.2742356128,5.54102966902184));
#63328=CARTESIAN_POINT('Ctrl Pts',(-5.54026815741874,-38.2742356128,5.59540007603281));
#63329=CARTESIAN_POINT('Ctrl Pts',(-5.54014355072925,-38.2742356128,5.59926277711513));
#63330=CARTESIAN_POINT('Ctrl Pts',(-5.54001645927,-38.2742356128,5.60312234544667));
#63331=CARTESIAN_POINT('Ctrl Pts',(-5.53988688857,-38.2742356128,5.60698050638));
#63332=CARTESIAN_POINT('Ctrl Pts',(-5.53988688120902,-38.2742356128,5.60698050613279));
#63333=CARTESIAN_POINT('Ctrl Pts',(-5.53835461888468,-38.2742356128,5.65260642340235));
#63334=CARTESIAN_POINT('Ctrl Pts',(-5.536259875995,-38.2742356128,5.69821935187167));
#63335=CARTESIAN_POINT('Ctrl Pts',(-5.5336031510825,-38.2742356128,5.743797561555));
#63336=CARTESIAN_POINT('Ctrl Pts',(-5.53094642617,-38.2742356128,5.78937577123833));
#63337=CARTESIAN_POINT('Ctrl Pts',(-5.52772748735596,-38.2742356128,5.83492380218515));
#63338=CARTESIAN_POINT('Ctrl Pts',(-5.52394721644107,-38.2742356128,5.88042392815046));
#63339=CARTESIAN_POINT('Ctrl Pts',(-5.51115082727157,-38.2742356128,6.03444392624604));
#63340=CARTESIAN_POINT('Ctrl Pts',(-5.49191715811991,-38.2742356128,6.18793486599567));
#63341=CARTESIAN_POINT('Ctrl Pts',(-5.46630422780706,-38.2742356127999,
6.34035255218782));
#63342=CARTESIAN_POINT('Ctrl Pts',(-5.44035409258864,-38.2742356127999,
6.49477688076138));
#63343=CARTESIAN_POINT('Ctrl Pts',(-5.40785568517866,-38.2742356127999,
6.64809930316969));
#63344=CARTESIAN_POINT('Ctrl Pts',(-5.36892159353684,-38.2742356127999,
6.79976605176687));
#63345=CARTESIAN_POINT('Ctrl Pts',(-5.32969944639958,-38.2742356127999,
6.95255491310809));
#63346=CARTESIAN_POINT('Ctrl Pts',(-5.28394615822592,-38.2742356127999,
7.10366330310781));
#63347=CARTESIAN_POINT('Ctrl Pts',(-5.23182799159665,-38.2742356127999,
7.25254050637488));
#63348=CARTESIAN_POINT('Ctrl Pts',(-5.17936032583359,-38.2742356127999,
7.40241606505134));
#63349=CARTESIAN_POINT('Ctrl Pts',(-5.12044226986684,-38.2742356127999,
7.55003019609581));
#63350=CARTESIAN_POINT('Ctrl Pts',(-5.05529310484516,-38.2742356127999,
7.69483982044707));
#63351=CARTESIAN_POINT('Ctrl Pts',(-4.98976338672371,-38.2742356127999,
7.84049531521595));
#63352=CARTESIAN_POINT('Ctrl Pts',(-4.91792970568151,-38.2742356127999,
7.98331322084872));
#63353=CARTESIAN_POINT('Ctrl Pts',(-4.84006305112756,-38.2742356127999,
8.12276314875079));
#63354=CARTESIAN_POINT('Ctrl Pts',(-4.76166290620733,-38.2742356128,8.26316849452125));
#63355=CARTESIAN_POINT('Ctrl Pts',(-4.67714699130435,-38.2742356128,8.40015931653317));
#63356=CARTESIAN_POINT('Ctrl Pts',(-4.58683794520934,-38.2742356128,8.53322024142848));
#63357=CARTESIAN_POINT('Ctrl Pts',(-4.49629467958833,-38.2742356128,8.66662626427471));
#63358=CARTESIAN_POINT('Ctrl Pts',(-4.39992838652888,-38.2742356128,8.79608175399285));
#63359=CARTESIAN_POINT('Ctrl Pts',(-4.2981076828134,-38.2742356128,8.92109681428887));
#63360=CARTESIAN_POINT('Ctrl Pts',(-4.19608210028847,-38.2742356128,9.04636342398282));
#63361=CARTESIAN_POINT('Ctrl Pts',(-4.08858033437217,-38.2742356128,9.16717149106921));
#63362=CARTESIAN_POINT('Ctrl Pts',(-3.9760138595325,-38.2742356128,9.28306111775555));
#63363=CARTESIAN_POINT('Ctrl Pts',(-3.90539029603414,-38.2742356128,9.3557696077455));
#63364=CARTESIAN_POINT('Ctrl Pts',(-3.83277394124446,-38.2742356128,9.42654275117891));
#63365=CARTESIAN_POINT('Ctrl Pts',(-3.75827401203565,-38.2742356128,9.49527417891981));
#63366=CARTESIAN_POINT('Ctrl Pts',(-3.63965885290044,-38.2742356128,9.60470501094418));
#63367=CARTESIAN_POINT('Ctrl Pts',(-3.51626710819725,-38.2742356128,9.70895831597016));
#63368=CARTESIAN_POINT('Ctrl Pts',(-3.38856684804589,-38.2742356128,9.80763610928524));
#63369=CARTESIAN_POINT('Ctrl Pts',(-3.26114695780359,-38.2742356128,9.90609725242353));
#63370=CARTESIAN_POINT('Ctrl Pts',(-3.12943768874386,-38.2742356128,9.99900714103251));
#63371=CARTESIAN_POINT('Ctrl Pts',(-2.9939361381078,-38.2742356128,10.0860110380169));
#63372=CARTESIAN_POINT('Ctrl Pts',(-2.85892760240792,-38.2742356128,10.1726983761093));
#63373=CARTESIAN_POINT('Ctrl Pts',(-2.72015457125465,-38.2742356128,10.2535224381057));
#63374=CARTESIAN_POINT('Ctrl Pts',(-2.57813705267921,-38.2742356128,10.3281755642702));
#63375=CARTESIAN_POINT('Ctrl Pts',(-2.43727514445134,-38.2742356128,10.4022212306936));
#63376=CARTESIAN_POINT('Ctrl Pts',(-2.29322158416204,-38.2742356128,10.4701958383899));
#63377=CARTESIAN_POINT('Ctrl Pts',(-2.14650802776576,-38.2742356127999,
10.5318441397132));
#63378=CARTESIAN_POINT('Ctrl Pts',(-2.00061624306781,-38.2742356127999,
10.5931471366862));
#63379=CARTESIAN_POINT('Ctrl Pts',(-1.85209440527852,-38.2742356127999,
10.6481943461997));
#63380=CARTESIAN_POINT('Ctrl Pts',(-1.70148582143208,-38.2742356127999,
10.6967816414531));
#63381=CARTESIAN_POINT('Ctrl Pts',(-1.55244458158058,-38.2742356127999,
10.7448633014797));
#63382=CARTESIAN_POINT('Ctrl Pts',(-1.4013600311476,-38.2742356127999,10.7866186970661));
#63383=CARTESIAN_POINT('Ctrl Pts',(-1.24877544147231,-38.2742356127999,
10.8218978649459));
#63384=CARTESIAN_POINT('Ctrl Pts',(-1.11051101261617,-38.2742356127998,
10.8538660604747));
#63385=CARTESIAN_POINT('Ctrl Pts',(-0.97101520004087,-38.2742356127998,
10.8805170667324));
#63386=CARTESIAN_POINT('Ctrl Pts',(-0.830701999895475,-38.2742356127998,
10.9017749796494));
#63387=CARTESIAN_POINT('Ctrl Pts',(-0.677686947127854,-38.2742356127998,
10.9249572651603));
#63388=CARTESIAN_POINT('Ctrl Pts',(-0.523701733229498,-38.2742356127999,
10.941724955098));
#63389=CARTESIAN_POINT('Ctrl Pts',(-0.369289497635685,-38.2742356128,10.9520282985498));
#63390=CARTESIAN_POINT('Ctrl Pts',(-0.248348049539687,-38.2742356128,10.9600982631643));
#63391=CARTESIAN_POINT('Ctrl Pts',(-0.127144870043233,-38.2742356128,10.9642035478476));
#63392=CARTESIAN_POINT('Ctrl Pts',(-0.00594433456959664,-38.2742356128,
10.9643423600255));
#63393=CARTESIAN_POINT('Ctrl Pts',(-0.00397084641091772,-38.2742356128,
10.9643446202811));
#63394=CARTESIAN_POINT('Ctrl Pts',(-0.00199736053559199,-38.2742356128,
10.9643458293));
#63395=CARTESIAN_POINT('Ctrl Pts',(-2.39294621618E-5,-38.2742356128,10.9643459873));
#63396=CARTESIAN_POINT('Ctrl Pts',(-2.08574170933,-36.2742356128,-9.31728158894));
#63397=CARTESIAN_POINT('Ctrl Pts',(-2.06766727163,-36.2742356128,-9.22478316375));
#63398=CARTESIAN_POINT('Ctrl Pts',(-2.04959283393,-36.3112466293,-9.13228473856));
#63399=CARTESIAN_POINT('Ctrl Pts',(-2.03530680234,-36.3857400536,-9.05917400362));
#63400=CARTESIAN_POINT('Ctrl Pts',(-2.02820898726,-36.4799878332,-9.02284995699));
#63401=CARTESIAN_POINT('Ctrl Pts',(-2.02820898726,-36.5742356128,-9.02284995699));
#63402=CARTESIAN_POINT('Ctrl Pts',(-2.08911689677,-36.2742356128,-9.31662206836));
#63403=CARTESIAN_POINT('Ctrl Pts',(-2.07116027711,-36.2742356128,-9.22410062121));
#63404=CARTESIAN_POINT('Ctrl Pts',(-2.05320365744,-36.3112466293,-9.13157917406));
#63405=CARTESIAN_POINT('Ctrl Pts',(-2.03901074921,-36.3857400536,-9.05845024258));
#63406=CARTESIAN_POINT('Ctrl Pts',(-2.03195920116,-36.4799878332,-9.02211715524));
#63407=CARTESIAN_POINT('Ctrl Pts',(-2.03195920116,-36.5742356128,-9.02211715524));
#63408=CARTESIAN_POINT('Ctrl Pts',(-2.0924931363,-36.2742356128,-9.31596792123));
#63409=CARTESIAN_POINT('Ctrl Pts',(-2.0746543701,-36.2742356128,-9.22342363995));
#63410=CARTESIAN_POINT('Ctrl Pts',(-2.0568156039,-36.3112466293,-9.13087935867));
#63411=CARTESIAN_POINT('Ctrl Pts',(-2.04271584702,-36.3857400536,-9.05773237909));
#63412=CARTESIAN_POINT('Ctrl Pts',(-2.03571057991,-36.4799878332,-9.02139032482));
#63413=CARTESIAN_POINT('Ctrl Pts',(-2.03571057991,-36.5742356128,-9.02139032482));
#63414=CARTESIAN_POINT('Ctrl Pts',(-2.09585558711,-36.2742356128,-9.31532184587));
#63415=CARTESIAN_POINT('Ctrl Pts',(-2.07813573018,-36.2742356128,-9.22275473257));
#63416=CARTESIAN_POINT('Ctrl Pts',(-2.06041587325,-36.3112466293,-9.13018761926));
#63417=CARTESIAN_POINT('Ctrl Pts',(-2.04640963715,-36.3857400536,-9.05702267764));
#63418=CARTESIAN_POINT('Ctrl Pts',(-2.03945153068,-36.4799878332,-9.02067157287));
#63419=CARTESIAN_POINT('Ctrl Pts',(-2.03945153068,-36.5742356128,-9.02067157287));
#63420=CARTESIAN_POINT('Ctrl Pts',(-2.10264192286,-36.2742356128,-9.31402965523));
#63421=CARTESIAN_POINT('Ctrl Pts',(-2.08515587597,-36.2742356128,-9.22141799595));
#63422=CARTESIAN_POINT('Ctrl Pts',(-2.06766982907,-36.3112466293,-9.12880633666));
#63423=CARTESIAN_POINT('Ctrl Pts',(-2.05384932652,-36.3857400536,-9.05560601714));
#63424=CARTESIAN_POINT('Ctrl Pts',(-2.04698210689,-36.4799878332,-9.01923758796));
#63425=CARTESIAN_POINT('Ctrl Pts',(-2.04698210689,-36.5742356128,-9.01923758796));
#63426=CARTESIAN_POINT('Ctrl Pts',(-2.10937295423,-36.2742356128,-9.31276977998));
#63427=CARTESIAN_POINT('Ctrl Pts',(-2.09212493888,-36.2742356128,-9.22011358344));
#63428=CARTESIAN_POINT('Ctrl Pts',(-2.07487692352,-36.3112466293,-9.1274573869));
#63429=CARTESIAN_POINT('Ctrl Pts',(-2.06124363091,-36.3857400536,-9.0542220339));
#63430=CARTESIAN_POINT('Ctrl Pts',(-2.05447081618,-36.4799878332,-9.01783594623));
#63431=CARTESIAN_POINT('Ctrl Pts',(-2.05447081618,-36.5742356128,-9.01783594623));
#63432=CARTESIAN_POINT('Ctrl Pts',(-2.11282966913,-36.2742356128,-9.31212882607));
#63433=CARTESIAN_POINT('Ctrl Pts',(-2.09569451045,-36.2742356128,-9.21945167612));
#63434=CARTESIAN_POINT('Ctrl Pts',(-2.07855935176,-36.3112466293,-9.12677452618));
#63435=CARTESIAN_POINT('Ctrl Pts',(-2.06501758638,-36.3857400536,-9.05352218973));
#63436=CARTESIAN_POINT('Ctrl Pts',(-2.05828676503,-36.4799878332,-9.01712829556));
#63437=CARTESIAN_POINT('Ctrl Pts',(-2.05828676503,-36.5742356128,-9.01712829556));
#63438=CARTESIAN_POINT('Ctrl Pts',(-2.11610882906,-36.2742356128,-9.31152571954));
#63439=CARTESIAN_POINT('Ctrl Pts',(-2.09909881001,-36.2742356128,-9.21882557494));
#63440=CARTESIAN_POINT('Ctrl Pts',(-2.08208879095,-36.3112466293,-9.12612543034));
#63441=CARTESIAN_POINT('Ctrl Pts',(-2.06864283545,-36.3857400536,-9.05285548143));
#63442=CARTESIAN_POINT('Ctrl Pts',(-2.06196425677,-36.4799878332,-9.01645199477));
#63443=CARTESIAN_POINT('Ctrl Pts',(-2.06196425677,-36.5742356128,-9.01645199477));
#63444=CARTESIAN_POINT('Ctrl Pts',(-2.11953809664,-36.2742356128,-9.31090088679));
#63445=CARTESIAN_POINT('Ctrl Pts',(-2.10264304655,-36.2742356128,-9.21817979292));
#63446=CARTESIAN_POINT('Ctrl Pts',(-2.08574799646,-36.3112466293,-9.12545869905));
#63447=CARTESIAN_POINT('Ctrl Pts',(-2.07239415258,-36.3857400536,-9.05217196684));
#63448=CARTESIAN_POINT('Ctrl Pts',(-2.06575948192,-36.4799878332,-9.01576047842));
#63449=CARTESIAN_POINT('Ctrl Pts',(-2.06575948192,-36.5742356128,-9.01576047842));
#63450=CARTESIAN_POINT('',(-2.02820898726,-36.5742356128,-9.02284995699));
#63451=CARTESIAN_POINT('Origin',(-2.08533438268287,-36.5721143203773,-9.31519977054305));
#63452=CARTESIAN_POINT('',(-2.06575948151871,-36.5742356128,-9.01576047619305));
#63453=CARTESIAN_POINT('Origin',(-2.11915857361596,-36.5721143085717,-9.308813819988));
#63454=CARTESIAN_POINT('Origin',(-2.46533767222342,-36.5742356128,-11.2351029262791));
#63455=CARTESIAN_POINT('Ctrl Pts',(-2.06575948222,-37.9742356128,-9.01576048002));
#63456=CARTESIAN_POINT('Ctrl Pts',(-2.0657594822,-38.0684833925,-9.01576048002));
#63457=CARTESIAN_POINT('Ctrl Pts',(-2.07239441316,-38.1627311721,-9.05217192117));
#63458=CARTESIAN_POINT('Ctrl Pts',(-2.08574878097,-38.2372245964,-9.12545855823));
#63459=CARTESIAN_POINT('Ctrl Pts',(-2.10264449395,-38.2742356129,-9.21817953172));
#63460=CARTESIAN_POINT('Ctrl Pts',(-2.11954020693,-38.2742356128,-9.31090050519));
#63461=CARTESIAN_POINT('Ctrl Pts',(-2.05815374966,-37.9742356128,-9.01714631048));
#63462=CARTESIAN_POINT('Ctrl Pts',(-2.05815374989,-38.0684833923,-9.01714631044));
#63463=CARTESIAN_POINT('Ctrl Pts',(-2.06487519089,-38.1627311717,-9.05354198334));
#63464=CARTESIAN_POINT('Ctrl Pts',(-2.07840770897,-38.2372245959,-9.12679615488));
#63465=CARTESIAN_POINT('Ctrl Pts',(-2.09552712261,-38.2742356126,-9.21947635948));
#63466=CARTESIAN_POINT('Ctrl Pts',(-2.11264653618,-38.2742356128,-9.3121565642));
#63467=CARTESIAN_POINT('Ctrl Pts',(-2.05152801719,-37.9742356128,-9.01837808851));
#63468=CARTESIAN_POINT('Ctrl Pts',(-2.05152801591,-38.0684833934,-9.01837808874));
#63469=CARTESIAN_POINT('Ctrl Pts',(-2.05839882311,-38.162731174,-9.05474628549));
#63470=CARTESIAN_POINT('Ctrl Pts',(-2.07226541572,-38.2372245982,-9.12793903416));
#63471=CARTESIAN_POINT('Ctrl Pts',(-2.08975388938,-38.2742356144,-9.22055135079));
#63472=CARTESIAN_POINT('Ctrl Pts',(-2.10724236369,-38.2742356128,-9.3131636663));
#63473=CARTESIAN_POINT('Ctrl Pts',(-2.04377025976,-37.9742356128,-9.01983403466));
#63474=CARTESIAN_POINT('Ctrl Pts',(-2.04377013041,-38.0684833525,-9.01983405993));
#63475=CARTESIAN_POINT('Ctrl Pts',(-2.05055250717,-38.1627310922,-9.05621942074));
#63476=CARTESIAN_POINT('Ctrl Pts',(-2.06436433537,-38.2372244929,-9.12942216681));
#63477=CARTESIAN_POINT('Ctrl Pts',(-2.08149565721,-38.2742355501,-9.22210406029));
#63478=CARTESIAN_POINT('Ctrl Pts',(-2.09862701806,-38.2742356128,-9.31478596379));
#63479=CARTESIAN_POINT('Ctrl Pts',(-2.03570878929,-37.9742356128,-9.02138447577));
#63480=CARTESIAN_POINT('Ctrl Pts',(-2.03570878929,-38.0684833924,-9.02138447577));
#63481=CARTESIAN_POINT('Ctrl Pts',(-2.04272147106,-38.1627311721,-9.05772515867));
#63482=CARTESIAN_POINT('Ctrl Pts',(-2.05681387623,-38.2372245951,-9.13087372673));
#63483=CARTESIAN_POINT('Ctrl Pts',(-2.07465269973,-38.2742356128,-9.22341819256));
#63484=CARTESIAN_POINT('Ctrl Pts',(-2.09249152102,-38.2742356128,-9.31596265782));
#63485=CARTESIAN_POINT('Ctrl Pts',(-2.02820898726,-37.9742356128,-9.02284995699));
#63486=CARTESIAN_POINT('Ctrl Pts',(-2.02820898726,-38.0684833924,-9.02284995699));
#63487=CARTESIAN_POINT('Ctrl Pts',(-2.03530680234,-38.1627311721,-9.05917400362));
#63488=CARTESIAN_POINT('Ctrl Pts',(-2.04959283393,-38.2372245963,-9.13228473856));
#63489=CARTESIAN_POINT('Ctrl Pts',(-2.06766727163,-38.2742356128,-9.22478316375));
#63490=CARTESIAN_POINT('Ctrl Pts',(-2.08574170933,-38.2742356128,-9.31728158894));
#63491=CARTESIAN_POINT('',(-2.02820898726,-37.9742356128,-9.02284995699));
#63492=CARTESIAN_POINT('Origin',(-2.08533572939304,-37.9763569039443,-9.3151995089407));
#63493=CARTESIAN_POINT('',(-2.06576130603488,-37.9742356128,-9.01576016653796));
#63494=CARTESIAN_POINT('Origin',(-2.46533597282467,-37.9742356128,-11.2350939774593));
#63495=CARTESIAN_POINT('Origin',(-2.11915381796855,-37.9763566360376,-9.30881475751182));
#63496=CARTESIAN_POINT('Origin',(-2.60353950403013,-37.9742356128,-11.9671837342904));
#63497=CARTESIAN_POINT('',(-2.02820898725,-37.2742356128,-9.02284995699));
#63498=CARTESIAN_POINT('',(-2.06575948168,-37.2742356128,-9.01576047707));
#63499=CARTESIAN_POINT('Ctrl Pts',(-2.11953749589,-36.2742356128,-9.31090098978));
#63500=CARTESIAN_POINT('Ctrl Pts',(-2.10264256193,-36.2742356128,-9.21817987482));
#63501=CARTESIAN_POINT('Ctrl Pts',(-2.08574762796,-36.3112466293,-9.12545875985));
#63502=CARTESIAN_POINT('Ctrl Pts',(-2.07239387587,-36.3857400536,-9.05217201097));
#63503=CARTESIAN_POINT('Ctrl Pts',(-2.06575925082,-36.4799878332,-9.01576051427));
#63504=CARTESIAN_POINT('Ctrl Pts',(-2.06575925082,-36.5742356128,-9.01576051427));
#63505=CARTESIAN_POINT('Ctrl Pts',(-2.61883842747,-36.2742356128,-9.21992235908));
#63506=CARTESIAN_POINT('Ctrl Pts',(-2.59793617609,-36.2742356128,-9.12793143196));
#63507=CARTESIAN_POINT('Ctrl Pts',(-2.57703392472,-36.3112466293,-9.03594050483));
#63508=CARTESIAN_POINT('Ctrl Pts',(-2.56051279612,-36.3857400536,-8.96323089513));
#63509=CARTESIAN_POINT('Ctrl Pts',(-2.5523044949,-36.4799878332,-8.92710614364));
#63510=CARTESIAN_POINT('Ctrl Pts',(-2.5523044949,-36.5742356128,-8.92710614364));
#63511=CARTESIAN_POINT('Ctrl Pts',(-3.11244995705,-36.2742356128,-9.10225947341));
#63512=CARTESIAN_POINT('Ctrl Pts',(-3.08747265848,-36.2742356128,-9.0112321755));
#63513=CARTESIAN_POINT('Ctrl Pts',(-3.06249535992,-36.3112466293,-8.92020487759));
#63514=CARTESIAN_POINT('Ctrl Pts',(-3.0427532992,-36.3857400536,-8.84825692301));
#63515=CARTESIAN_POINT('Ctrl Pts',(-3.03294474641,-36.4799878332,-8.81251058504));
#63516=CARTESIAN_POINT('Ctrl Pts',(-3.03294474641,-36.5742356128,-8.81251058504));
#63517=CARTESIAN_POINT('Ctrl Pts',(-3.59670238728,-36.2742356128,-8.9571409937));
#63518=CARTESIAN_POINT('Ctrl Pts',(-3.56742906565,-36.2742356128,-8.86737676632));
#63519=CARTESIAN_POINT('Ctrl Pts',(-3.53815574401,-36.3112466293,-8.77761253894));
#63520=CARTESIAN_POINT('Ctrl Pts',(-3.5150181194,-36.3857400536,-8.70666291293));
#63521=CARTESIAN_POINT('Ctrl Pts',(-3.50352251051,-36.4799878332,-8.6714125837));
#63522=CARTESIAN_POINT('Ctrl Pts',(-3.50352251051,-36.5742356128,-8.6714125837));
#63523=CARTESIAN_POINT('Ctrl Pts',(-4.71225848168,-36.2742356128,-8.54787678002));
#63524=CARTESIAN_POINT('Ctrl Pts',(-4.67300397879,-36.2742356128,-8.46179505057));
#63525=CARTESIAN_POINT('Ctrl Pts',(-4.6337494759,-36.3112466293,-8.37571332112));
#63526=CARTESIAN_POINT('Ctrl Pts',(-4.60272272226,-36.3857400536,-8.30767434165));
#63527=CARTESIAN_POINT('Ctrl Pts',(-4.58730751821,-36.4799878332,-8.27387012499));
#63528=CARTESIAN_POINT('Ctrl Pts',(-4.58730751821,-36.5742356128,-8.27387012499));
#63529=CARTESIAN_POINT('Ctrl Pts',(-5.76024912723,-36.2742356128,-7.98940147532));
#63530=CARTESIAN_POINT('Ctrl Pts',(-5.71191143403,-36.2742356128,-7.90816087535));
#63531=CARTESIAN_POINT('Ctrl Pts',(-5.66357374084,-36.3112466293,-7.82692027539));
#63532=CARTESIAN_POINT('Ctrl Pts',(-5.62536764306,-36.3857400536,-7.76270772231));
#63533=CARTESIAN_POINT('Ctrl Pts',(-5.60638547104,-36.4799878332,-7.73080461404));
#63534=CARTESIAN_POINT('Ctrl Pts',(-5.60638547104,-36.5742356128,-7.73080461404));
#63535=CARTESIAN_POINT('Ctrl Pts',(-6.33821543401,-36.2742356128,-7.61896694326));
#63536=CARTESIAN_POINT('Ctrl Pts',(-6.28525641384,-36.2742356128,-7.54080551103));
#63537=CARTESIAN_POINT('Ctrl Pts',(-6.23229739367,-36.3112466293,-7.46264407879));
#63538=CARTESIAN_POINT('Ctrl Pts',(-6.1904385957,-36.3857400536,-7.40086530005));
#63539=CARTESIAN_POINT('Ctrl Pts',(-6.16964163719,-36.4799878332,-7.37017137728));
#63540=CARTESIAN_POINT('Ctrl Pts',(-6.16964163719,-36.5742356128,-7.37017137728));
#63541=CARTESIAN_POINT('Ctrl Pts',(-7.2863768604,-36.2742356128,-6.92663027622));
#63542=CARTESIAN_POINT('Ctrl Pts',(-7.2271227297,-36.2742356128,-6.8530659898));
#63543=CARTESIAN_POINT('Ctrl Pts',(-7.167868599,-36.3112466293,-6.77950170338));
#63544=CARTESIAN_POINT('Ctrl Pts',(-7.12103414712,-36.3857400536,-6.72135650754));
#63545=CARTESIAN_POINT('Ctrl Pts',(-7.0977651044,-36.4799878332,-6.69246787984));
#63546=CARTESIAN_POINT('Ctrl Pts',(-7.0977651044,-36.5742356128,-6.69246787984));
#63547=CARTESIAN_POINT('Ctrl Pts',(-8.17808008644,-36.2742356128,-6.11829341209));
#63548=CARTESIAN_POINT('Ctrl Pts',(-8.11276510867,-36.2742356128,-6.05021218498));
#63549=CARTESIAN_POINT('Ctrl Pts',(-8.0474501309,-36.3112466293,-5.98213095786));
#63550=CARTESIAN_POINT('Ctrl Pts',(-7.99582518686,-36.3857400536,-5.9283195709));
#63551=CARTESIAN_POINT('Ctrl Pts',(-7.97017605504,-36.4799878332,-5.90158413555));
#63552=CARTESIAN_POINT('Ctrl Pts',(-7.97017605504,-36.5742356128,-5.90158413555));
#63553=CARTESIAN_POINT('Ctrl Pts',(-8.53884026615,-36.2742356128,-5.7594573392));
#63554=CARTESIAN_POINT('Ctrl Pts',(-8.47082512858,-36.2742356128,-5.69401108691));
#63555=CARTESIAN_POINT('Ctrl Pts',(-8.402809991,-36.3112466293,-5.62856483461));
#63556=CARTESIAN_POINT('Ctrl Pts',(-8.34905084127,-36.3857400536,-5.57683613125));
#63557=CARTESIAN_POINT('Ctrl Pts',(-8.32234135915,-36.4799878332,-5.55113544801));
#63558=CARTESIAN_POINT('Ctrl Pts',(-8.32234135915,-36.5742356128,-5.55113544801));
#63559=CARTESIAN_POINT('Ctrl Pts',(-9.14391387257,-36.2742356128,-5.08624796937));
#63560=CARTESIAN_POINT('Ctrl Pts',(-9.07021258959,-36.2742356128,-5.02690763905));
#63561=CARTESIAN_POINT('Ctrl Pts',(-8.99651130661,-36.3112466293,-4.96756730873));
#63562=CARTESIAN_POINT('Ctrl Pts',(-8.93825782872,-36.3857400536,-4.92066472472));
#63563=CARTESIAN_POINT('Ctrl Pts',(-8.9093154026,-36.4799878332,-4.89736183147));
#63564=CARTESIAN_POINT('Ctrl Pts',(-8.9093154026,-36.5742356128,-4.89736183147));
#63565=CARTESIAN_POINT('Ctrl Pts',(-9.65506365996,-36.2742356128,-4.33036740431));
#63566=CARTESIAN_POINT('Ctrl Pts',(-9.57455339335,-36.2742356128,-4.28091564854));
#63567=CARTESIAN_POINT('Ctrl Pts',(-9.49404312674,-36.3112466293,-4.23146389278));
#63568=CARTESIAN_POINT('Ctrl Pts',(-9.43040782971,-36.3857400536,-4.19237723581));
#63569=CARTESIAN_POINT('Ctrl Pts',(-9.39879152194,-36.4799878332,-4.17295757681));
#63570=CARTESIAN_POINT('Ctrl Pts',(-9.39879152194,-36.5742356128,-4.17295757681));
#63571=CARTESIAN_POINT('Ctrl Pts',(-9.85393064124,-36.2742356128,-3.98362416377));
#63572=CARTESIAN_POINT('Ctrl Pts',(-9.77024228393,-36.2742356128,-3.93958894582));
#63573=CARTESIAN_POINT('Ctrl Pts',(-9.68655392663,-36.3112466293,-3.89555372787));
#63574=CARTESIAN_POINT('Ctrl Pts',(-9.62040666759,-36.3857400536,-3.86074830211));
#63575=CARTESIAN_POINT('Ctrl Pts',(-9.58754232635,-36.4799878332,-3.84345571163));
#63576=CARTESIAN_POINT('Ctrl Pts',(-9.58754232635,-36.5742356128,-3.84345571163));
#63577=CARTESIAN_POINT('Ctrl Pts',(-10.363444524,-36.2742356128,-2.88078522158));
#63578=CARTESIAN_POINT('Ctrl Pts',(-10.2712984823,-36.2742356128,-2.85484986236));
#63579=CARTESIAN_POINT('Ctrl Pts',(-10.1791524407,-36.3112466293,-2.82891450314));
#63580=CARTESIAN_POINT('Ctrl Pts',(-10.1063202294,-36.3857400536,-2.80841519904));
#63581=CARTESIAN_POINT('Ctrl Pts',(-10.0701345637,-36.4799878332,-2.79823040916));
#63582=CARTESIAN_POINT('Ctrl Pts',(-10.0701345637,-36.5742356128,-2.79823040916));
#63583=CARTESIAN_POINT('Ctrl Pts',(-10.5676336782,-36.2742356128,-1.65939737822));
#63584=CARTESIAN_POINT('Ctrl Pts',(-10.4719619497,-36.2742356128,-1.65453645426));
#63585=CARTESIAN_POINT('Ctrl Pts',(-10.3762902212,-36.3112466293,-1.64967553031));
#63586=CARTESIAN_POINT('Ctrl Pts',(-10.3006713084,-36.3857400536,-1.64583346123));
#63587=CARTESIAN_POINT('Ctrl Pts',(-10.2631011081,-36.4799878332,-1.64392457671));
#63588=CARTESIAN_POINT('Ctrl Pts',(-10.2631011081,-36.5742356128,-1.64392457671));
#63589=CARTESIAN_POINT('Ctrl Pts',(-10.5419165386,-36.2742356128,-0.848067876402));
#63590=CARTESIAN_POINT('Ctrl Pts',(-10.4477463127,-36.2742356128,-0.852679034501));
#63591=CARTESIAN_POINT('Ctrl Pts',(-10.3535760868,-36.3112466293,-0.8572901926));
#63592=CARTESIAN_POINT('Ctrl Pts',(-10.2791439585,-36.3857400536,-0.860934836052));
#63593=CARTESIAN_POINT('Ctrl Pts',(-10.2421633997,-36.4799878332,-0.862745648498));
#63594=CARTESIAN_POINT('Ctrl Pts',(-10.2421633997,-36.5742356128,-0.862745648498));
#63595=CARTESIAN_POINT('Ctrl Pts',(-10.473089026,-36.2742356128,-0.0706759998857));
#63596=CARTESIAN_POINT('Ctrl Pts',(-10.3792034004,-36.2742356128,-0.080327881531));
#63597=CARTESIAN_POINT('Ctrl Pts',(-10.2853177749,-36.3112466293,-0.0899797631762));
#63598=CARTESIAN_POINT('Ctrl Pts',(-10.2111105988,-36.3857400536,-0.0976086182963));
#63599=CARTESIAN_POINT('Ctrl Pts',(-10.1742417982,-36.4799878332,-0.101398893365));
#63600=CARTESIAN_POINT('Ctrl Pts',(-10.1742417982,-36.5742356128,-0.101398893365));
#63601=CARTESIAN_POINT('Ctrl Pts',(-10.3535104648,-36.2742356128,0.692257829523));
#63602=CARTESIAN_POINT('Ctrl Pts',(-10.2603995032,-36.2742356128,0.67766355641));
#63603=CARTESIAN_POINT('Ctrl Pts',(-10.1672885415,-36.3112466293,0.663069283296));
#63604=CARTESIAN_POINT('Ctrl Pts',(-10.0936936579,-36.3857400536,0.651533973036));
#63605=CARTESIAN_POINT('Ctrl Pts',(-10.0571290687,-36.4799878332,0.645802815386));
#63606=CARTESIAN_POINT('Ctrl Pts',(-10.0571290687,-36.5742356128,0.645802815386));
#63607=CARTESIAN_POINT('',(-10.0571285787,-36.5742356128,0.645805825719));
#63608=CARTESIAN_POINT('Origin',(-10.3514149258478,-36.5721143559387,0.691928460092334));
#63609=CARTESIAN_POINT('Ctrl Pts',(-2.06575948168,-36.5742356128,-9.01576047707));
#63610=CARTESIAN_POINT('Ctrl Pts',(-2.88684751198,-36.5742356128,-8.86614972783));
#63611=CARTESIAN_POINT('Ctrl Pts',(-3.69023581935,-36.5742356128,-8.64282630111));
#63612=CARTESIAN_POINT('Ctrl Pts',(-4.45617471096,-36.5742356128,-8.3426574972));
#63613=CARTESIAN_POINT('Ctrl Pts',(-5.4347519266,-36.5742356128,-7.8381799988));
#63614=CARTESIAN_POINT('Ctrl Pts',(-6.34892734604,-36.5742356128,-7.22182745264));
#63615=CARTESIAN_POINT('Ctrl Pts',(-6.57301164304,-36.5742356128,-7.06148474597));
#63616=CARTESIAN_POINT('Ctrl Pts',(-7.23577044161,-36.5742356128,-6.56118503754));
#63617=CARTESIAN_POINT('Ctrl Pts',(-7.87223833418,-36.5742356128,-6.00004951347));
#63618=CARTESIAN_POINT('Ctrl Pts',(-8.28331893233,-36.5742356128,-5.59939000156));
#63619=CARTESIAN_POINT('Ctrl Pts',(-8.90941365274,-36.5742356128,-4.90631405862));
#63620=CARTESIAN_POINT('Ctrl Pts',(-9.42196991537,-36.5742356128,-4.13127436126));
#63621=CARTESIAN_POINT('Ctrl Pts',(-9.59767693443,-36.5742356128,-3.81973064431));
#63622=CARTESIAN_POINT('Ctrl Pts',(-9.84427307953,-36.5742356128,-3.28258152507));
#63623=CARTESIAN_POINT('Ctrl Pts',(-10.0147288891,-36.5742356128,-2.71679407199));
#63624=CARTESIAN_POINT('Ctrl Pts',(-10.0694270847,-36.5742356128,-2.49123410795));
#63625=CARTESIAN_POINT('Ctrl Pts',(-10.154755688,-36.5742356128,-2.03576280704));
#63626=CARTESIAN_POINT('Ctrl Pts',(-10.1959693718,-36.5742356128,-1.57549366979));
#63627=CARTESIAN_POINT('Ctrl Pts',(-10.2066163947,-36.5742356128,-1.34483444272));
#63628=CARTESIAN_POINT('Ctrl Pts',(-10.2113958308,-36.5742356128,-0.80319628916));
#63629=CARTESIAN_POINT('Ctrl Pts',(-10.1751569467,-36.5742356128,-0.265526349602));
#63630=CARTESIAN_POINT('Ctrl Pts',(-10.1436911823,-36.5742356128,0.0415756246997));
#63631=CARTESIAN_POINT('Ctrl Pts',(-10.1043144812,-36.5742356128,0.344751093937));
#63632=CARTESIAN_POINT('Ctrl Pts',(-10.0571285787,-36.5742356128,0.645805825719));
#63633=CARTESIAN_POINT('Ctrl Pts',(-10.0571285552,-37.9742356128,0.645805969836));
#63634=CARTESIAN_POINT('Ctrl Pts',(-10.0571285554,-38.0684833925,0.645805968571));
#63635=CARTESIAN_POINT('Ctrl Pts',(-10.0936931762,-38.1627311721,0.651536924187));
#63636=CARTESIAN_POINT('Ctrl Pts',(-10.1672881231,-38.2372245963,0.663071829355));
#63637=CARTESIAN_POINT('Ctrl Pts',(-10.2603991649,-38.2742356128,0.67766559072));
#63638=CARTESIAN_POINT('Ctrl Pts',(-10.3535102065,-38.2742356128,0.692259352582));
#63639=CARTESIAN_POINT('Ctrl Pts',(-10.166801105,-37.9742356128,-0.0539288837089));
#63640=CARTESIAN_POINT('Ctrl Pts',(-10.1668011785,-38.0684833943,-0.0539293520197));
#63641=CARTESIAN_POINT('Ctrl Pts',(-10.2036480968,-38.1627311757,-0.0499995227518));
#63642=CARTESIAN_POINT('Ctrl Pts',(-10.2778111132,-38.2372246007,-0.0420890384201));
#63643=CARTESIAN_POINT('Ctrl Pts',(-10.3716408342,-38.2742356157,-0.0320806300088));
#63644=CARTESIAN_POINT('Ctrl Pts',(-10.4654705253,-38.2742356128,-0.0220720388979));
#63645=CARTESIAN_POINT('Ctrl Pts',(-10.233499836,-37.9742356128,-0.766569459386));
#63646=CARTESIAN_POINT('Ctrl Pts',(-10.2334997254,-38.0684833762,-0.766568752312));
#63647=CARTESIAN_POINT('Ctrl Pts',(-10.2704792366,-38.1627311396,-0.764558608417));
#63648=CARTESIAN_POINT('Ctrl Pts',(-10.3449094314,-38.2372245581,-0.760513883966));
#63649=CARTESIAN_POINT('Ctrl Pts',(-10.4390772685,-38.2742355874,-0.755396874269));
#63650=CARTESIAN_POINT('Ctrl Pts',(-10.5332451587,-38.2742356128,-0.750280139627));
#63651=CARTESIAN_POINT('Ctrl Pts',(-10.2589747967,-37.9742356128,-1.49377249196));
#63652=CARTESIAN_POINT('Ctrl Pts',(-10.2589748319,-38.0684834037,-1.49377265296));
#63653=CARTESIAN_POINT('Ctrl Pts',(-10.2963782615,-38.1627311946,-1.49497949399));
#63654=CARTESIAN_POINT('Ctrl Pts',(-10.3716614552,-38.2372246229,-1.49740827406));
#63655=CARTESIAN_POINT('Ctrl Pts',(-10.4669084166,-38.2742356306,-1.50048105645));
#63656=CARTESIAN_POINT('Ctrl Pts',(-10.5621553577,-38.2742356128,-1.5035537741));
#63657=CARTESIAN_POINT('Ctrl Pts',(-10.07136584,-37.9742356128,-2.91801448478));
#63658=CARTESIAN_POINT('Ctrl Pts',(-10.0713658062,-38.0684833816,-2.91801433022));
#63659=CARTESIAN_POINT('Ctrl Pts',(-10.1076744141,-38.1627311504,-2.92880207761));
#63660=CARTESIAN_POINT('Ctrl Pts',(-10.1807541274,-38.2372245708,-2.95051523186));
#63661=CARTESIAN_POINT('Ctrl Pts',(-10.2732133244,-38.2742355958,-2.97798640082));
#63662=CARTESIAN_POINT('Ctrl Pts',(-10.3656725408,-38.2742356128,-3.00545763192));
#63663=CARTESIAN_POINT('Ctrl Pts',(-9.43888580477,-37.9742356128,-4.19731493645));
#63664=CARTESIAN_POINT('Ctrl Pts',(-9.43888583723,-38.0684834029,-4.19731508481));
#63665=CARTESIAN_POINT('Ctrl Pts',(-9.47062176951,-38.1627311929,-4.21722149235));
#63666=CARTESIAN_POINT('Ctrl Pts',(-9.53449778852,-38.2372246208,-4.2572875957));
#63667=CARTESIAN_POINT('Ctrl Pts',(-9.61531259337,-38.2742356292,-4.30797846695));
#63668=CARTESIAN_POINT('Ctrl Pts',(-9.6961273796,-38.2742356128,-4.35866927856));
#63669=CARTESIAN_POINT('Ctrl Pts',(-9.02777291595,-37.9742356128,-4.76329520136));
#63670=CARTESIAN_POINT('Ctrl Pts',(-9.02777292761,-38.0684834,-4.76329519358));
#63671=CARTESIAN_POINT('Ctrl Pts',(-9.057065221,-38.1627311872,-4.78613151867));
#63672=CARTESIAN_POINT('Ctrl Pts',(-9.11602287492,-38.2372246142,-4.83209503424));
#63673=CARTESIAN_POINT('Ctrl Pts',(-9.19061506035,-38.2742356247,-4.89024727341));
#63674=CARTESIAN_POINT('Ctrl Pts',(-9.26520723838,-38.2742356128,-4.94839951173));
#63675=CARTESIAN_POINT('Ctrl Pts',(-8.30376468439,-37.9742356128,-5.59440760207));
#63676=CARTESIAN_POINT('Ctrl Pts',(-8.30376467773,-38.0684833881,-5.59440760651));
#63677=CARTESIAN_POINT('Ctrl Pts',(-8.33036893671,-38.1627311634,-5.62029070861));
#63678=CARTESIAN_POINT('Ctrl Pts',(-8.38391630832,-38.2372245861,-5.67238656763));
#63679=CARTESIAN_POINT('Ctrl Pts',(-8.45166351292,-38.274235606,-5.7382973376));
#63680=CARTESIAN_POINT('Ctrl Pts',(-8.51941072175,-38.2742356128,-5.80420810805));
#63681=CARTESIAN_POINT('Ctrl Pts',(-7.49360195673,-37.9742356128,-6.33060530722));
#63682=CARTESIAN_POINT('Ctrl Pts',(-7.49360196054,-38.0684833949,-6.33060530468));
#63683=CARTESIAN_POINT('Ctrl Pts',(-7.51791854842,-38.162731177,-6.35853121169));
#63684=CARTESIAN_POINT('Ctrl Pts',(-7.5668614281,-38.2372246022,-6.41473870745));
#63685=CARTESIAN_POINT('Ctrl Pts',(-7.62878310191,-38.2742356167,-6.48585145033));
#63686=CARTESIAN_POINT('Ctrl Pts',(-7.6907047733,-38.2742356128,-6.55696419293));
#63687=CARTESIAN_POINT('Ctrl Pts',(-7.19158531474,-37.9742356128,-6.58638782253));
#63688=CARTESIAN_POINT('Ctrl Pts',(-7.19158531103,-38.0684833899,-6.58638782576));
#63689=CARTESIAN_POINT('Ctrl Pts',(-7.21512703478,-38.162731167,-6.61497407193));
#63690=CARTESIAN_POINT('Ctrl Pts',(-7.26251032621,-38.2372245904,-6.67251064937));
#63691=CARTESIAN_POINT('Ctrl Pts',(-7.32245884208,-38.2742356089,-6.74530492126));
#63692=CARTESIAN_POINT('Ctrl Pts',(-7.38240736043,-38.2742356128,-6.81809919304));
#63693=CARTESIAN_POINT('Ctrl Pts',(-6.57881164637,-37.9742356128,-7.06987433056));
#63694=CARTESIAN_POINT('Ctrl Pts',(-6.57881165007,-38.068483395,-7.06987432735));
#63695=CARTESIAN_POINT('Ctrl Pts',(-6.60071832324,-38.1627311771,-7.09975694193));
#63696=CARTESIAN_POINT('Ctrl Pts',(-6.64481067968,-38.2372246022,-7.15990277537));
#63697=CARTESIAN_POINT('Ctrl Pts',(-6.7005955562,-38.2742356168,-7.23599823476));
#63698=CARTESIAN_POINT('Ctrl Pts',(-6.75638043023,-38.2742356128,-7.31209369426));
#63699=CARTESIAN_POINT('Ctrl Pts',(-5.9353899124,-37.9742356128,-7.5039276571));
#63700=CARTESIAN_POINT('Ctrl Pts',(-5.93538990872,-38.06848339,-7.5039276603));
#63701=CARTESIAN_POINT('Ctrl Pts',(-5.95536133185,-38.1627311671,-7.53512169599));
#63702=CARTESIAN_POINT('Ctrl Pts',(-5.99555854896,-38.2372245905,-7.5979070666));
#63703=CARTESIAN_POINT('Ctrl Pts',(-6.046415369,-38.2742356089,-7.67734202));
#63704=CARTESIAN_POINT('Ctrl Pts',(-6.09727219151,-38.2742356128,-7.75677697329));
#63705=CARTESIAN_POINT('Ctrl Pts',(-5.60614917144,-37.9742356128,-7.70722191498));
#63706=CARTESIAN_POINT('Ctrl Pts',(-5.60614918073,-38.0684833903,-7.707221912));
#63707=CARTESIAN_POINT('Ctrl Pts',(-5.6250617684,-38.1627311678,-7.73907597951));
#63708=CARTESIAN_POINT('Ctrl Pts',(-5.6631278099,-38.2372245913,-7.80318982834));
#63709=CARTESIAN_POINT('Ctrl Pts',(-5.71128829675,-38.2742356095,-7.88430555277));
#63710=CARTESIAN_POINT('Ctrl Pts',(-5.75944878038,-38.2742356128,-7.96542127963));
#63711=CARTESIAN_POINT('Ctrl Pts',(-4.74244689379,-37.9742356128,-8.18975922749));
#63712=CARTESIAN_POINT('Ctrl Pts',(-4.74244687927,-38.0684833958,-8.18975923215));
#63713=CARTESIAN_POINT('Ctrl Pts',(-4.75843542755,-38.1627311787,-8.22325041568));
#63714=CARTESIAN_POINT('Ctrl Pts',(-4.79061618477,-38.2372246042,-8.29065933715));
#63715=CARTESIAN_POINT('Ctrl Pts',(-4.83133072336,-38.2742356181,-8.37594392375));
#63716=CARTESIAN_POINT('Ctrl Pts',(-4.87204526698,-38.2742356128,-8.46122850655));
#63717=CARTESIAN_POINT('Ctrl Pts',(-3.8297049454,-37.9742356128,-8.56858316919));
#63718=CARTESIAN_POINT('Ctrl Pts',(-3.8297049681,-38.0684833872,-8.5685831619));
#63719=CARTESIAN_POINT('Ctrl Pts',(-3.84237809363,-38.1627311616,-8.60346422097));
#63720=CARTESIAN_POINT('Ctrl Pts',(-3.86788572113,-38.237224584,-8.67367061231));
#63721=CARTESIAN_POINT('Ctrl Pts',(-3.90015751593,-38.2742356046,-8.76249451857));
#63722=CARTESIAN_POINT('Ctrl Pts',(-3.93242930286,-38.2742356128,-8.85131843076));
#63723=CARTESIAN_POINT('Ctrl Pts',(-3.25582231846,-37.9742356128,-8.75788647545));
#63724=CARTESIAN_POINT('Ctrl Pts',(-3.25582230332,-38.0684834022,-8.75788647812));
#63725=CARTESIAN_POINT('Ctrl Pts',(-3.2663841251,-38.1627311915,-8.79345058999));
#63726=CARTESIAN_POINT('Ctrl Pts',(-3.28764233655,-38.2372246192,-8.86503176831));
#63727=CARTESIAN_POINT('Ctrl Pts',(-3.31453785051,-38.2742356281,-8.95559502193));
#63728=CARTESIAN_POINT('Ctrl Pts',(-3.34143336856,-38.2742356128,-9.04615826881));
#63729=CARTESIAN_POINT('Ctrl Pts',(-2.66537560342,-37.9742356128,-8.90650444612));
#63730=CARTESIAN_POINT('Ctrl Pts',(-2.66537564264,-38.0684833929,-8.90650443911));
#63731=CARTESIAN_POINT('Ctrl Pts',(-2.67394959074,-38.1627311729,-8.94256257595));
#63732=CARTESIAN_POINT('Ctrl Pts',(-2.69120662213,-38.2372245974,-9.0151381165));
#63733=CARTESIAN_POINT('Ctrl Pts',(-2.71303990103,-38.2742356135,-9.10695942575));
#63734=CARTESIAN_POINT('Ctrl Pts',(-2.73487316451,-38.2742356128,-9.19878073748));
#63735=CARTESIAN_POINT('Ctrl Pts',(-2.0657631474,-37.9742356128,-9.01575989378));
#63736=CARTESIAN_POINT('Ctrl Pts',(-2.06576314406,-38.0684833924,-9.01575989438));
#63737=CARTESIAN_POINT('Ctrl Pts',(-2.07239767256,-38.162731172,-9.05217140948));
#63738=CARTESIAN_POINT('Ctrl Pts',(-2.08575123441,-38.2372245963,-9.12545819469));
#63739=CARTESIAN_POINT('Ctrl Pts',(-2.10264592972,-38.2742356128,-9.21817935525));
#63740=CARTESIAN_POINT('Ctrl Pts',(-2.11954062634,-38.2742356128,-9.3109005156));
#63741=CARTESIAN_POINT('',(-10.0571285787,-37.9742356128,0.645805825719));
#63742=CARTESIAN_POINT('Ctrl Pts',(-2.0657631474,-37.9742356128,-9.01575989378));
#63743=CARTESIAN_POINT('Ctrl Pts',(-2.21055756124637,-37.9742356128,-8.98937688864956));
#63744=CARTESIAN_POINT('Ctrl Pts',(-2.35470583880119,-37.9742356128,-8.96023914137939));
#63745=CARTESIAN_POINT('Ctrl Pts',(-2.49801140128497,-37.9742356128,-8.92830835678781));
#63746=CARTESIAN_POINT('Ctrl Pts',(-2.64661454196291,-37.9742356128,-8.89519718655563));
#63747=CARTESIAN_POINT('Ctrl Pts',(-2.7943118638327,-37.9742356128,-8.85908222926721));
#63748=CARTESIAN_POINT('Ctrl Pts',(-2.94094133902924,-37.9742356128,-8.81992924536183));
#63749=CARTESIAN_POINT('Ctrl Pts',(-3.09326087237576,-37.9742356128,-8.77925690284954));
#63750=CARTESIAN_POINT('Ctrl Pts',(-3.24442857386082,-37.9742356128,-8.73530560793822));
#63751=CARTESIAN_POINT('Ctrl Pts',(-3.39431677839277,-37.9742356128,-8.6880537429529));
#63752=CARTESIAN_POINT('Ctrl Pts',(-3.55149447503361,-37.9742356128,-8.6385038846197));
#63753=CARTESIAN_POINT('Ctrl Pts',(-3.70726586213417,-37.9742356128,-8.58532381792461));
#63754=CARTESIAN_POINT('Ctrl Pts',(-3.86153295951299,-37.9742356128,-8.52851746693305));
#63755=CARTESIAN_POINT('Ctrl Pts',(-4.0172550578266,-37.9742356128,-8.47117533549836));
#63756=CARTESIAN_POINT('Ctrl Pts',(-4.17144546130456,-37.9742356128,-8.41013749149708));
#63757=CARTESIAN_POINT('Ctrl Pts',(-4.32403828257966,-37.9742356128,-8.34544797793615));
#63758=CARTESIAN_POINT('Ctrl Pts',(-4.47348519624443,-37.9742356128,-8.28209212628224));
#63759=CARTESIAN_POINT('Ctrl Pts',(-4.62140087163535,-37.9742356128,-8.21523318084772));
#63760=CARTESIAN_POINT('Ctrl Pts',(-4.76773975955357,-37.9742356128,-8.1449588479227));
#63761=CARTESIAN_POINT('Ctrl Pts',(-4.82030561847545,-37.9742356128,-8.11971586075151));
#63762=CARTESIAN_POINT('Ctrl Pts',(-4.87266809902291,-37.9742356128,-8.0940326613706));
#63763=CARTESIAN_POINT('Ctrl Pts',(-4.92482519221318,-37.9742356128,-8.06791498369728));
#63764=CARTESIAN_POINT('Ctrl Pts',(-5.06040908297022,-37.9742356128,-8.00002131593537));
#63765=CARTESIAN_POINT('Ctrl Pts',(-5.19460591643175,-37.9742356128,-7.92918756170566));
#63766=CARTESIAN_POINT('Ctrl Pts',(-5.32737904492262,-37.9742356128,-7.85553870103708));
#63767=CARTESIAN_POINT('Ctrl Pts',(-5.48706475962,-37.9742356128,-7.76696150860226));
#63768=CARTESIAN_POINT('Ctrl Pts',(-5.64468815179341,-37.9742356128,-7.67431398917331));
#63769=CARTESIAN_POINT('Ctrl Pts',(-5.80019139110691,-37.9742356128,-7.57788422162767));
#63770=CARTESIAN_POINT('Ctrl Pts',(-5.9314757506791,-37.9742356128,-7.49647292542694));
#63771=CARTESIAN_POINT('Ctrl Pts',(-6.06124785245264,-37.9742356128,-7.41236864383582));
#63772=CARTESIAN_POINT('Ctrl Pts',(-6.18950386976392,-37.9742356128,-7.32575186448882));
#63773=CARTESIAN_POINT('Ctrl Pts',(-6.3059579274687,-37.9742356128,-7.24710545372591));
#63774=CARTESIAN_POINT('Ctrl Pts',(-6.42116159360231,-37.9742356128,-7.16638882252908));
#63775=CARTESIAN_POINT('Ctrl Pts',(-6.53514946295618,-37.9742356128,-7.08371932032296));
#63776=CARTESIAN_POINT('Ctrl Pts',(-6.54670148833218,-37.9742356128,-7.07534123419221));
#63777=CARTESIAN_POINT('Ctrl Pts',(-6.55824106452687,-37.9742356128,-7.06694306644521));
#63778=CARTESIAN_POINT('Ctrl Pts',(-6.56976825429465,-37.9742356128,-7.05852492131865));
#63779=CARTESIAN_POINT('Ctrl Pts',(-6.64878179524979,-37.9742356128,-7.00082243978382));
#63780=CARTESIAN_POINT('Ctrl Pts',(-6.72721753878092,-37.9742356128,-6.94217924661947));
#63781=CARTESIAN_POINT('Ctrl Pts',(-6.80514089959812,-37.9742356128,-6.88257070926825));
#63782=CARTESIAN_POINT('Ctrl Pts',(-6.88589195492991,-37.9742356128,-6.82079908844215));
#63783=CARTESIAN_POINT('Ctrl Pts',(-6.96609266210244,-37.9742356128,-6.75799124102026));
#63784=CARTESIAN_POINT('Ctrl Pts',(-7.0457631144731,-37.9742356128,-6.69414250228203));
#63785=CARTESIAN_POINT('Ctrl Pts',(-7.12865126771334,-37.9742356128,-6.62771506421366));
#63786=CARTESIAN_POINT('Ctrl Pts',(-7.21096532137975,-37.9742356128,-6.56016156130215));
#63787=CARTESIAN_POINT('Ctrl Pts',(-7.29267376299196,-37.9742356128,-6.49149273615506));
#63788=CARTESIAN_POINT('Ctrl Pts',(-7.37939561494801,-37.9742356128,-6.41861057647975));
#63789=CARTESIAN_POINT('Ctrl Pts',(-7.46543516586726,-37.9742356128,-6.34447289356002));
#63790=CARTESIAN_POINT('Ctrl Pts',(-7.55069654496993,-37.9742356128,-6.26909869682082));
#63791=CARTESIAN_POINT('Ctrl Pts',(-7.6393847665147,-37.9742356128,-6.19069504525525));
#63792=CARTESIAN_POINT('Ctrl Pts',(-7.72723055271955,-37.9742356128,-6.11095470869088));
#63793=CARTESIAN_POINT('Ctrl Pts',(-7.814069401565,-37.9742356128,-6.02988909397397));
#63794=CARTESIAN_POINT('Ctrl Pts',(-7.90090825041046,-37.9742356128,-5.94882347925705));
#63795=CARTESIAN_POINT('Ctrl Pts',(-7.98673929450905,-37.9742356128,-5.86643381460967));
#63796=CARTESIAN_POINT('Ctrl Pts',(-8.0713531761618,-37.9742356128,-5.78270311231078));
#63797=CARTESIAN_POINT('Ctrl Pts',(-8.1467028994669,-37.9742356128,-5.70813987130199));
#63798=CARTESIAN_POINT('Ctrl Pts',(-8.22108885952716,-37.9742356128,-5.63251312569528));
#63799=CARTESIAN_POINT('Ctrl Pts',(-8.29437508920965,-37.9742356128,-5.55581755269425));
#63800=CARTESIAN_POINT('Ctrl Pts',(-8.37310090860936,-37.9742356128,-5.47342933522153));
#63801=CARTESIAN_POINT('Ctrl Pts',(-8.45055738224527,-37.9742356128,-5.38980730088329));
#63802=CARTESIAN_POINT('Ctrl Pts',(-8.52652404805359,-37.9742356128,-5.30491282776207));
#63803=CARTESIAN_POINT('Ctrl Pts',(-8.61219204089014,-37.9742356128,-5.20917690151302));
#63804=CARTESIAN_POINT('Ctrl Pts',(-8.69596499022727,-37.9742356128,-5.11182198372865));
#63805=CARTESIAN_POINT('Ctrl Pts',(-8.77746802781235,-37.9742356128,-5.0127629061177));
#63806=CARTESIAN_POINT('Ctrl Pts',(-8.88365772022927,-37.9742356128,-4.88369958167865));
#63807=CARTESIAN_POINT('Ctrl Pts',(-8.98599271413021,-37.9742356128,-4.7517397333071));
#63808=CARTESIAN_POINT('Ctrl Pts',(-9.08355926863292,-37.9742356128,-4.61668045648252));
#63809=CARTESIAN_POINT('Ctrl Pts',(-9.16215290844201,-37.9742356128,-4.5078849762103));
#63810=CARTESIAN_POINT('Ctrl Pts',(-9.23764895184771,-37.9742356128,-4.39707658418915));
#63811=CARTESIAN_POINT('Ctrl Pts',(-9.30956694400941,-37.9742356128,-4.28417925211255));
#63812=CARTESIAN_POINT('Ctrl Pts',(-9.37213796405824,-37.9742356128,-4.18595485768087));
#63813=CARTESIAN_POINT('Ctrl Pts',(-9.43199962616356,-37.9742356128,-4.08614884411721));
#63814=CARTESIAN_POINT('Ctrl Pts',(-9.4888561786539,-37.9742356128,-3.984747468796));
#63815=CARTESIAN_POINT('Ctrl Pts',(-9.53965553238558,-37.9742356128,-3.89414886391758));
#63816=CARTESIAN_POINT('Ctrl Pts',(-9.58805567524611,-37.9742356128,-3.80227667672272));
#63817=CARTESIAN_POINT('Ctrl Pts',(-9.63387055719901,-37.9742356128,-3.70915455341205));
#63818=CARTESIAN_POINT('Ctrl Pts',(-9.67774260674016,-37.9742356128,-3.61998138013043));
#63819=CARTESIAN_POINT('Ctrl Pts',(-9.71924365336037,-37.9742356128,-3.5296617836214));
#63820=CARTESIAN_POINT('Ctrl Pts',(-9.75823923133626,-37.9742356128,-3.43825143381026));
#63821=CARTESIAN_POINT('Ctrl Pts',(-9.79512552212818,-37.9742356128,-3.3517855081966));
#63822=CARTESIAN_POINT('Ctrl Pts',(-9.82976990344546,-37.9742356128,-3.26434356911638));
#63823=CARTESIAN_POINT('Ctrl Pts',(-9.86208840966277,-37.9742356128,-3.17600670010489));
#63824=CARTESIAN_POINT('Ctrl Pts',(-9.89428974958264,-37.9742356128,-3.08799008425733));
#63825=CARTESIAN_POINT('Ctrl Pts',(-9.92418167132371,-37.9742356128,-2.99908468371943));
#63826=CARTESIAN_POINT('Ctrl Pts',(-9.95171582590476,-37.9742356128,-2.90940871914275));
#63827=CARTESIAN_POINT('Ctrl Pts',(-9.97851922512363,-37.9742356128,-2.82211275108205));
#63828=CARTESIAN_POINT('Ctrl Pts',(-10.0030868945867,-37.9742356128,-2.73409104825337));
#63829=CARTESIAN_POINT('Ctrl Pts',(-10.0254224159267,-37.9742356128,-2.64549978022437));
#63830=CARTESIAN_POINT('Ctrl Pts',(-10.0486642310802,-37.9742356128,-2.55331380236448));
#63831=CARTESIAN_POINT('Ctrl Pts',(-10.0694893669665,-37.9742356128,-2.46051118720013));
#63832=CARTESIAN_POINT('Ctrl Pts',(-10.087957545448,-37.9742356128,-2.36725121569743));
#63833=CARTESIAN_POINT('Ctrl Pts',(-10.1073441963928,-37.9742356128,-2.26935317358935));
#63834=CARTESIAN_POINT('Ctrl Pts',(-10.1241340090463,-37.9742356128,-2.17095128248165));
#63835=CARTESIAN_POINT('Ctrl Pts',(-10.1384510808335,-37.9742356128,-2.07221001847922));
#63836=CARTESIAN_POINT('Ctrl Pts',(-10.153674187722,-37.9742356128,-1.96722005694614));
#63837=CARTESIAN_POINT('Ctrl Pts',(-10.1661022453971,-37.9742356128,-1.86184661853482));
#63838=CARTESIAN_POINT('Ctrl Pts',(-10.1759378701588,-37.9742356128,-1.75626284034153));
#63839=CARTESIAN_POINT('Ctrl Pts',(-10.1870815562795,-37.9742356128,-1.63663724337702));
#63840=CARTESIAN_POINT('Ctrl Pts',(-10.194898157712,-37.9742356128,-1.51674233002038));
#63841=CARTESIAN_POINT('Ctrl Pts',(-10.199739349461,-37.9742356128,-1.39679152753606));
#63842=CARTESIAN_POINT('Ctrl Pts',(-10.2049385442023,-37.9742356128,-1.26797044094861));
#63843=CARTESIAN_POINT('Ctrl Pts',(-10.2067084649352,-37.9742356128,-1.13908538627714));
#63844=CARTESIAN_POINT('Ctrl Pts',(-10.2055200313416,-37.9742356128,-1.01034972448036));
#63845=CARTESIAN_POINT('Ctrl Pts',(-10.2043825812601,-37.9742356128,-0.887136791259177));
#63846=CARTESIAN_POINT('Ctrl Pts',(-10.2005378334161,-37.9742356128,-0.764060290648597));
#63847=CARTESIAN_POINT('Ctrl Pts',(-10.19439037226,-37.9742356128,-0.641263249215135));
#63848=CARTESIAN_POINT('Ctrl Pts',(-10.1889620856855,-37.9742356128,-0.53283189609585));
#63849=CARTESIAN_POINT('Ctrl Pts',(-10.1817393597794,-37.9742356128,-0.424617787571569));
#63850=CARTESIAN_POINT('Ctrl Pts',(-10.1729711247451,-37.9742356128,-0.31669226407076));
#63851=CARTESIAN_POINT('Ctrl Pts',(-10.1647993631123,-37.9742356128,-0.216108549253679));
#63852=CARTESIAN_POINT('Ctrl Pts',(-10.155285824146,-37.9742356128,-0.115775221617667));
#63853=CARTESIAN_POINT('Ctrl Pts',(-10.144593847242,-37.9742356128,-0.0157306628922133));
#63854=CARTESIAN_POINT('Ctrl Pts',(-10.134369024781,-37.9742356128,0.0799427434699424));
#63855=CARTESIAN_POINT('Ctrl Pts',(-10.1230669838381,-37.9742356128,0.175352208840096));
#63856=CARTESIAN_POINT('Ctrl Pts',(-10.1107865597769,-37.9742356128,0.27047974645221));
#63857=CARTESIAN_POINT('Ctrl Pts',(-10.099126263622,-37.9742356128,0.360803602983524));
#63858=CARTESIAN_POINT('Ctrl Pts',(-10.0865841425898,-37.9742356128,0.450873416758909));
#63859=CARTESIAN_POINT('Ctrl Pts',(-10.0731992305874,-37.9742356128,0.540686188874415));
#63860=CARTESIAN_POINT('Ctrl Pts',(-10.067971383564,-37.9742356128,0.575765047314226));
#63861=CARTESIAN_POINT('Ctrl Pts',(-10.0626144400519,-37.9742356128,0.61080482232795));
#63862=CARTESIAN_POINT('Ctrl Pts',(-10.05712857781,-37.9742356128,0.6458058255795));
#63863=CARTESIAN_POINT('Origin',(-10.3514144928172,-37.9763569061288,0.691930920254248));
#63864=CARTESIAN_POINT('Ctrl Pts',(-2.06575948168,-37.9742356128,-9.01576047707));
#63865=CARTESIAN_POINT('Ctrl Pts',(-2.06575948168,-36.2942356128,-9.01576047707));
#63866=CARTESIAN_POINT('Ctrl Pts',(-2.88684751198,-37.9742356128,-8.86614972783));
#63867=CARTESIAN_POINT('Ctrl Pts',(-2.88684751198,-36.2942356128,-8.86614972783));
#63868=CARTESIAN_POINT('Ctrl Pts',(-3.69023581935,-37.9742356128,-8.64282630111));
#63869=CARTESIAN_POINT('Ctrl Pts',(-3.69023581935,-36.2942356128,-8.64282630111));
#63870=CARTESIAN_POINT('Ctrl Pts',(-4.45617471096,-37.9742356128,-8.3426574972));
#63871=CARTESIAN_POINT('Ctrl Pts',(-4.45617471096,-36.2942356128,-8.3426574972));
#63872=CARTESIAN_POINT('Ctrl Pts',(-5.4347519266,-37.9742356128,-7.8381799988));
#63873=CARTESIAN_POINT('Ctrl Pts',(-5.4347519266,-36.2942356128,-7.8381799988));
#63874=CARTESIAN_POINT('Ctrl Pts',(-6.34892734604,-37.9742356128,-7.22182745264));
#63875=CARTESIAN_POINT('Ctrl Pts',(-6.34892734604,-36.2942356128,-7.22182745264));
#63876=CARTESIAN_POINT('Ctrl Pts',(-6.57301164304,-37.9742356128,-7.06148474597));
#63877=CARTESIAN_POINT('Ctrl Pts',(-6.57301164304,-36.2942356128,-7.06148474597));
#63878=CARTESIAN_POINT('Ctrl Pts',(-7.23577044161,-37.9742356128,-6.56118503754));
#63879=CARTESIAN_POINT('Ctrl Pts',(-7.23577044161,-36.2942356128,-6.56118503754));
#63880=CARTESIAN_POINT('Ctrl Pts',(-7.87223833418,-37.9742356128,-6.00004951347));
#63881=CARTESIAN_POINT('Ctrl Pts',(-7.87223833418,-36.2942356128,-6.00004951347));
#63882=CARTESIAN_POINT('Ctrl Pts',(-8.28331893233,-37.9742356128,-5.59939000156));
#63883=CARTESIAN_POINT('Ctrl Pts',(-8.28331893233,-36.2942356128,-5.59939000156));
#63884=CARTESIAN_POINT('Ctrl Pts',(-8.90941365274,-37.9742356128,-4.90631405862));
#63885=CARTESIAN_POINT('Ctrl Pts',(-8.90941365274,-36.2942356128,-4.90631405862));
#63886=CARTESIAN_POINT('Ctrl Pts',(-9.42196991537,-37.9742356128,-4.13127436126));
#63887=CARTESIAN_POINT('Ctrl Pts',(-9.42196991537,-36.2942356128,-4.13127436126));
#63888=CARTESIAN_POINT('Ctrl Pts',(-9.59767693443,-37.9742356128,-3.81973064431));
#63889=CARTESIAN_POINT('Ctrl Pts',(-9.59767693443,-36.2942356128,-3.81973064431));
#63890=CARTESIAN_POINT('Ctrl Pts',(-9.84427307953,-37.9742356128,-3.28258152507));
#63891=CARTESIAN_POINT('Ctrl Pts',(-9.84427307953,-36.2942356128,-3.28258152507));
#63892=CARTESIAN_POINT('Ctrl Pts',(-10.0147288891,-37.9742356128,-2.71679407199));
#63893=CARTESIAN_POINT('Ctrl Pts',(-10.0147288891,-36.2942356128,-2.71679407199));
#63894=CARTESIAN_POINT('Ctrl Pts',(-10.0694270847,-37.9742356128,-2.49123410795));
#63895=CARTESIAN_POINT('Ctrl Pts',(-10.0694270847,-36.2942356128,-2.49123410795));
#63896=CARTESIAN_POINT('Ctrl Pts',(-10.154755688,-37.9742356128,-2.03576280704));
#63897=CARTESIAN_POINT('Ctrl Pts',(-10.154755688,-36.2942356128,-2.03576280704));
#63898=CARTESIAN_POINT('Ctrl Pts',(-10.1959693718,-37.9742356128,-1.57549366979));
#63899=CARTESIAN_POINT('Ctrl Pts',(-10.1959693718,-36.2942356128,-1.57549366979));
#63900=CARTESIAN_POINT('Ctrl Pts',(-10.2066163947,-37.9742356128,-1.34483444272));
#63901=CARTESIAN_POINT('Ctrl Pts',(-10.2066163947,-36.2942356128,-1.34483444272));
#63902=CARTESIAN_POINT('Ctrl Pts',(-10.2113958308,-37.9742356128,-0.80319628916));
#63903=CARTESIAN_POINT('Ctrl Pts',(-10.2113958308,-36.2942356128,-0.80319628916));
#63904=CARTESIAN_POINT('Ctrl Pts',(-10.1751569467,-37.9742356128,-0.265526349602));
#63905=CARTESIAN_POINT('Ctrl Pts',(-10.1751569467,-36.2942356128,-0.265526349602));
#63906=CARTESIAN_POINT('Ctrl Pts',(-10.1436911823,-37.9742356128,0.0415756246997));
#63907=CARTESIAN_POINT('Ctrl Pts',(-10.1436911823,-36.2942356128,0.0415756246997));
#63908=CARTESIAN_POINT('Ctrl Pts',(-10.1043144812,-37.9742356128,0.344751093937));
#63909=CARTESIAN_POINT('Ctrl Pts',(-10.1043144812,-36.2942356128,0.344751093937));
#63910=CARTESIAN_POINT('Ctrl Pts',(-10.0571285787,-37.9742356128,0.645805825719));
#63911=CARTESIAN_POINT('Ctrl Pts',(-10.0571285787,-36.2942356128,0.645805825719));
#63912=CARTESIAN_POINT('',(-10.0571285787,-37.2742356128,0.645805825719));
#63913=CARTESIAN_POINT('Ctrl Pts',(-10.3535102174,-36.2742356128,0.692259289483));
#63914=CARTESIAN_POINT('Ctrl Pts',(-10.2603991795,-36.2742356128,0.677665503434));
#63915=CARTESIAN_POINT('Ctrl Pts',(-10.1672881417,-36.3112466293,0.663071717384));
#63916=CARTESIAN_POINT('Ctrl Pts',(-10.0936931978,-36.3857400536,0.651536792099));
#63917=CARTESIAN_POINT('Ctrl Pts',(-10.0571285787,-36.4799878332,0.645805825719));
#63918=CARTESIAN_POINT('Ctrl Pts',(-10.0571285787,-36.5742356128,0.645805825719));
#63919=CARTESIAN_POINT('Ctrl Pts',(-10.3243887019,-36.2742356128,0.878059911334));
#63920=CARTESIAN_POINT('Ctrl Pts',(-10.2314618653,-36.2742356128,0.862290887462));
#63921=CARTESIAN_POINT('Ctrl Pts',(-10.1385350287,-36.3112466293,0.846521863591));
#63922=CARTESIAN_POINT('Ctrl Pts',(-10.0650856774,-36.3857400536,0.83405803183));
#63923=CARTESIAN_POINT('Ctrl Pts',(-10.0285933941,-36.4799878332,0.827865549396));
#63924=CARTESIAN_POINT('Ctrl Pts',(-10.0285933941,-36.5742356128,0.827865549396));
#63925=CARTESIAN_POINT('Ctrl Pts',(-10.2932212121,-36.2742356128,1.05777080235));
#63926=CARTESIAN_POINT('Ctrl Pts',(-10.2003615355,-36.2742356128,1.04171956338));
#63927=CARTESIAN_POINT('Ctrl Pts',(-10.1075018589,-36.3112466293,1.02566832442));
#63928=CARTESIAN_POINT('Ctrl Pts',(-10.0341055912,-36.3857400536,1.01298142707));
#63929=CARTESIAN_POINT('Ctrl Pts',(-9.99763968115,-36.4799878332,1.00667812186));
#63930=CARTESIAN_POINT('Ctrl Pts',(-9.99763968115,-36.5742356128,1.00667812186));
#63931=CARTESIAN_POINT('Ctrl Pts',(-10.2607745073,-36.2742356128,1.24596085714));
#63932=CARTESIAN_POINT('Ctrl Pts',(-10.1681333202,-36.2742356128,1.22834540563));
#63933=CARTESIAN_POINT('Ctrl Pts',(-10.0754921331,-36.3112466293,1.21072995412));
#63934=CARTESIAN_POINT('Ctrl Pts',(-10.0022685812,-36.3857400536,1.19680667032));
#63935=CARTESIAN_POINT('Ctrl Pts',(-9.96588844999,-36.4799878332,1.18988913349));
#63936=CARTESIAN_POINT('Ctrl Pts',(-9.96588844999,-36.5742356128,1.18988913349));
#63937=CARTESIAN_POINT('Ctrl Pts',(-10.1749701856,-36.2742356128,1.65068933105));
#63938=CARTESIAN_POINT('Ctrl Pts',(-10.0835898455,-36.2742356128,1.62659066301));
#63939=CARTESIAN_POINT('Ctrl Pts',(-9.99220950546,-36.3112466293,1.60249199497));
#63940=CARTESIAN_POINT('Ctrl Pts',(-9.91998248138,-36.3857400536,1.5834444508));
#63941=CARTESIAN_POINT('Ctrl Pts',(-9.88409752911,-36.4799878332,1.57398088825));
#63942=CARTESIAN_POINT('Ctrl Pts',(-9.88409752911,-36.5742356128,1.57398088825));
#63943=CARTESIAN_POINT('Ctrl Pts',(-10.0369131944,-36.2742356128,2.06011773698));
#63944=CARTESIAN_POINT('Ctrl Pts',(-9.94892100813,-36.2742356128,2.02559357059));
#63945=CARTESIAN_POINT('Ctrl Pts',(-9.8609288219,-36.3112466293,1.99106940419));
#63946=CARTESIAN_POINT('Ctrl Pts',(-9.79137984198,-36.3857400536,1.96378146973));
#63947=CARTESIAN_POINT('Ctrl Pts',(-9.75682536651,-36.4799878332,1.95022390222));
#63948=CARTESIAN_POINT('Ctrl Pts',(-9.75682536651,-36.5742356128,1.95022390222));
#63949=CARTESIAN_POINT('Ctrl Pts',(-9.94917208334,-36.2742356128,2.2667545433));
#63950=CARTESIAN_POINT('Ctrl Pts',(-9.86363693513,-36.2742356128,2.22630952643));
#63951=CARTESIAN_POINT('Ctrl Pts',(-9.77810178691,-36.3112466293,2.18586450956));
#63952=CARTESIAN_POINT('Ctrl Pts',(-9.71049472475,-36.3857400536,2.15389693954));
#63953=CARTESIAN_POINT('Ctrl Pts',(-9.67690525041,-36.4799878332,2.13801405614));
#63954=CARTESIAN_POINT('Ctrl Pts',(-9.67690525041,-36.5742356128,2.13801405614));
#63955=CARTESIAN_POINT('Ctrl Pts',(-9.83902583182,-36.2742356128,2.46711999934));
#63956=CARTESIAN_POINT('Ctrl Pts',(-9.75664708714,-36.2742356128,2.42118386819));
#63957=CARTESIAN_POINT('Ctrl Pts',(-9.67426834245,-36.3112466293,2.37524773705));
#63958=CARTESIAN_POINT('Ctrl Pts',(-9.60915626728,-36.3857400536,2.33893972063));
#63959=CARTESIAN_POINT('Ctrl Pts',(-9.57680614337,-36.4799878332,2.32090075257));
#63960=CARTESIAN_POINT('Ctrl Pts',(-9.57680614337,-36.5742356128,2.32090075257));
#63961=CARTESIAN_POINT('Ctrl Pts',(-9.72829200824,-36.2742356128,2.64855052214));
#63962=CARTESIAN_POINT('Ctrl Pts',(-9.64784465104,-36.2742356128,2.59944994453));
#63963=CARTESIAN_POINT('Ctrl Pts',(-9.56739729384,-36.3112466293,2.55034936692));
#63964=CARTESIAN_POINT('Ctrl Pts',(-9.5038117204,-36.3857400536,2.51154028118));
#63965=CARTESIAN_POINT('Ctrl Pts',(-9.4722201171,-36.4799878332,2.49225852944));
#63966=CARTESIAN_POINT('Ctrl Pts',(-9.4722201171,-36.5742356128,2.49225852944));
#63967=CARTESIAN_POINT('',(-9.47221988254214,-36.5742356128,2.49225890563289));
#63968=CARTESIAN_POINT('Origin',(-9.7264810754177,-36.5721143332941,2.64744582231073));
#63969=CARTESIAN_POINT('Ctrl Pts',(-10.0571285787,-36.5742356128,0.645805825719));
#63970=CARTESIAN_POINT('Ctrl Pts',(-10.0512202390646,-36.5742356128,0.683502118786429));
#63971=CARTESIAN_POINT('Ctrl Pts',(-10.045191880218,-36.5742356128,0.721027397434276));
#63972=CARTESIAN_POINT('Ctrl Pts',(-10.039052830587,-36.5742356128,0.758520627395506));
#63973=CARTESIAN_POINT('Ctrl Pts',(-10.0327166412668,-36.5742356128,0.797217855392582));
#63974=CARTESIAN_POINT('Ctrl Pts',(-10.0262621747024,-36.5742356128,0.835880865268867));
#63975=CARTESIAN_POINT('Ctrl Pts',(-10.0196616405614,-36.5742356128,0.874617705186171));
#63976=CARTESIAN_POINT('Ctrl Pts',(-10.0128144444338,-36.5742356128,0.914802140962507));
#63977=CARTESIAN_POINT('Ctrl Pts',(-10.0058096288593,-36.5742356128,0.955065985035107));
#63978=CARTESIAN_POINT('Ctrl Pts',(-9.99858199734885,-36.5742356128,0.995483360467456));
#63979=CARTESIAN_POINT('Ctrl Pts',(-9.99106528890846,-36.5742356128,1.03751727249131));
#63980=CARTESIAN_POINT('Ctrl Pts',(-9.9833070137521,-36.5742356128,1.0797172147409));
#63981=CARTESIAN_POINT('Ctrl Pts',(-9.97520532678219,-36.5742356128,1.12211771621868));
#63982=CARTESIAN_POINT('Ctrl Pts',(-9.96662488168625,-36.5742356128,1.1670238174198));
#63983=CARTESIAN_POINT('Ctrl Pts',(-9.95765844421231,-36.5742356128,1.21215499974358));
#63984=CARTESIAN_POINT('Ctrl Pts',(-9.94816426041759,-36.5742356128,1.25749762852443));
#63985=CARTESIAN_POINT('Ctrl Pts',(-9.93844008755608,-36.5742356128,1.30393864649854));
#63986=CARTESIAN_POINT('Ctrl Pts',(-9.92816108637949,-36.5742356128,1.35060127886798));
#63987=CARTESIAN_POINT('Ctrl Pts',(-9.91716946674835,-36.5742356128,1.39741623621432));
#63988=CARTESIAN_POINT('Ctrl Pts',(-9.90621039827007,-36.5742356128,1.44409255331622));
#63989=CARTESIAN_POINT('Ctrl Pts',(-9.89454156630661,-36.5742356128,1.49091987282535));
#63990=CARTESIAN_POINT('Ctrl Pts',(-9.88202055604576,-36.5742356128,1.53778090756651));
#63991=CARTESIAN_POINT('Ctrl Pts',(-9.8800220437476,-36.5742356128,1.54526052400987));
#63992=CARTESIAN_POINT('Ctrl Pts',(-9.87800187545779,-36.5742356128,1.55274090613695));
#63993=CARTESIAN_POINT('Ctrl Pts',(-9.87595954226258,-36.5742356128,1.56022147294422));
#63994=CARTESIAN_POINT('Ctrl Pts',(-9.87217026083382,-36.5742356128,1.57410068371447));
#63995=CARTESIAN_POINT('Ctrl Pts',(-9.86830430955095,-36.5742356128,1.58798172214129));
#63996=CARTESIAN_POINT('Ctrl Pts',(-9.8643642042847,-36.5742356128,1.60184532111123));
#63997=CARTESIAN_POINT('Ctrl Pts',(-9.84832680476092,-36.5742356128,1.65827428950022));
#63998=CARTESIAN_POINT('Ctrl Pts',(-9.83104562941538,-36.5742356128,1.71447457739543));
#63999=CARTESIAN_POINT('Ctrl Pts',(-9.81234709545891,-36.5742356128,1.77036490831683));
#64000=CARTESIAN_POINT('Ctrl Pts',(-9.80179728711155,-36.5742356128,1.80189851844177));
#64001=CARTESIAN_POINT('Ctrl Pts',(-9.79079560997722,-36.5742356128,1.83333468885662));
#64002=CARTESIAN_POINT('Ctrl Pts',(-9.77931157200682,-36.5742356128,1.86466494021047));
#64003=CARTESIAN_POINT('Ctrl Pts',(-9.77215186764178,-36.5742356128,1.8841977332885));
#64004=CARTESIAN_POINT('Ctrl Pts',(-9.76480472005903,-36.5742356128,1.90368942396184));
#64005=CARTESIAN_POINT('Ctrl Pts',(-9.75726381835173,-36.5742356128,1.92313827869078));
#64006=CARTESIAN_POINT('Ctrl Pts',(-9.75220095002517,-36.5742356128,1.93619599969247));
#64007=CARTESIAN_POINT('Ctrl Pts',(-9.7470500063913,-36.5742356128,1.94923629340378));
#64008=CARTESIAN_POINT('Ctrl Pts',(-9.74181183174468,-36.5742356128,1.96225262541807));
#64009=CARTESIAN_POINT('Ctrl Pts',(-9.72550464318401,-36.5742356128,2.00277433285331));
#64010=CARTESIAN_POINT('Ctrl Pts',(-9.70837226896001,-36.5742356128,2.0430049326535));
#64011=CARTESIAN_POINT('Ctrl Pts',(-9.69043140056761,-36.5742356128,2.08287240096882));
#64012=CARTESIAN_POINT('Ctrl Pts',(-9.67400285885705,-36.5742356128,2.11937923841878));
#64013=CARTESIAN_POINT('Ctrl Pts',(-9.65689624141328,-36.5742356128,2.1555819110846));
#64014=CARTESIAN_POINT('Ctrl Pts',(-9.63916750428284,-36.5742356128,2.19141965241515));
#64015=CARTESIAN_POINT('Ctrl Pts',(-9.62199168890653,-36.5742356128,2.2261396905131));
#64016=CARTESIAN_POINT('Ctrl Pts',(-9.6042316575573,-36.5742356128,2.2605174515297));
#64017=CARTESIAN_POINT('Ctrl Pts',(-9.58598418264596,-36.5742356128,2.29448826760494));
#64018=CARTESIAN_POINT('Ctrl Pts',(-9.56778747896572,-36.5742356128,2.32836456429256));
#64019=CARTESIAN_POINT('Ctrl Pts',(-9.54910565419454,-36.5742356128,2.36183641627422));
#64020=CARTESIAN_POINT('Ctrl Pts',(-9.53008640475237,-36.5742356128,2.39482653491171));
#64021=CARTESIAN_POINT('Ctrl Pts',(-9.51106715531021,-36.5742356128,2.4278166535492));
#64022=CARTESIAN_POINT('Ctrl Pts',(-9.49171019387024,-36.5742356128,2.46032523638466));
#64023=CARTESIAN_POINT('Ctrl Pts',(-9.4722201171,-36.5742356128,2.49225852944));
#64024=CARTESIAN_POINT('Ctrl Pts',(-9.47221976653,-37.9742356128,2.49225909299));
#64025=CARTESIAN_POINT('Ctrl Pts',(-9.47221976653,-38.0684833924,2.49225909299));
#64026=CARTESIAN_POINT('Ctrl Pts',(-9.50381146403,-38.1627311721,2.51154069023));
#64027=CARTESIAN_POINT('Ctrl Pts',(-9.56739722707,-38.2372245963,2.55034946501));
#64028=CARTESIAN_POINT('Ctrl Pts',(-9.64784482414,-38.2742356128,2.59944964919));
#64029=CARTESIAN_POINT('Ctrl Pts',(-9.72829242121,-38.2742356128,2.64854983337));
#64030=CARTESIAN_POINT('Ctrl Pts',(-9.57590405793,-37.9742356128,2.32237883269));
#64031=CARTESIAN_POINT('Ctrl Pts',(-9.57590405797,-38.0684833925,2.32237883264));
#64032=CARTESIAN_POINT('Ctrl Pts',(-9.60823780617,-38.1627311721,2.3404446279));
#64033=CARTESIAN_POINT('Ctrl Pts',(-9.67331602956,-38.2372245964,2.37680809748));
#64034=CARTESIAN_POINT('Ctrl Pts',(-9.75565231855,-38.2742356129,2.42281377752));
#64035=CARTESIAN_POINT('Ctrl Pts',(-9.83798860831,-38.2742356128,2.4688194563));
#64036=CARTESIAN_POINT('Ctrl Pts',(-9.67510718944,-37.9742356128,2.14132026528));
#64037=CARTESIAN_POINT('Ctrl Pts',(-9.67510717979,-38.0684833832,2.14132028047));
#64038=CARTESIAN_POINT('Ctrl Pts',(-9.70868867607,-38.1627311536,2.15721813848));
#64039=CARTESIAN_POINT('Ctrl Pts',(-9.7762810279,-38.2372245746,2.18921365099));
#64040=CARTESIAN_POINT('Ctrl Pts',(-9.86179701536,-38.2742355984,2.22969492403));
#64041=CARTESIAN_POINT('Ctrl Pts',(-9.94731301056,-38.2742356128,2.27017619541));
#64042=CARTESIAN_POINT('Ctrl Pts',(-9.75470839831,-37.9742356128,1.95515325352));
#64043=CARTESIAN_POINT('Ctrl Pts',(-9.75470839104,-38.0684833997,1.95515330638));
#64044=CARTESIAN_POINT('Ctrl Pts',(-9.78923398698,-38.1627311865,1.96877814974));
#64045=CARTESIAN_POINT('Ctrl Pts',(-9.85872451082,-38.2372246133,1.99620198352));
#64046=CARTESIAN_POINT('Ctrl Pts',(-9.94664288255,-38.2742356242,2.03089782227));
#64047=CARTESIAN_POINT('Ctrl Pts',(-10.0345612532,-38.2742356128,2.06559363831));
#64048=CARTESIAN_POINT('Ctrl Pts',(-9.88272651401,-37.9742356128,1.57928798862));
#64049=CARTESIAN_POINT('Ctrl Pts',(-9.88272652097,-38.0684833856,1.57928793803));
#64050=CARTESIAN_POINT('Ctrl Pts',(-9.9186033632,-38.1627311583,1.58879684875));
#64051=CARTESIAN_POINT('Ctrl Pts',(-9.9908143753,-38.2372245801,1.60793521244));
#64052=CARTESIAN_POINT('Ctrl Pts',(-10.0821743219,-38.274235602,1.63214903103));
#64053=CARTESIAN_POINT('Ctrl Pts',(-10.1735342695,-38.2742356128,1.65636287136));
#64054=CARTESIAN_POINT('Ctrl Pts',(-9.96501416235,-37.9742356128,1.19500960441));
#64055=CARTESIAN_POINT('Ctrl Pts',(-9.96501415569,-38.068483399,1.19500965283));
#64056=CARTESIAN_POINT('Ctrl Pts',(-10.0013888155,-38.1627311853,1.20195148351));
#64057=CARTESIAN_POINT('Ctrl Pts',(-10.0746010604,-38.2372246119,1.21592408453));
#64058=CARTESIAN_POINT('Ctrl Pts',(-10.1672280703,-38.2742356232,1.23360170088));
#64059=CARTESIAN_POINT('Ctrl Pts',(-10.2598550792,-38.2742356128,1.25127929642));
#64060=CARTESIAN_POINT('Ctrl Pts',(-9.9970648974,-37.9742356128,1.00998816846));
#64061=CARTESIAN_POINT('Ctrl Pts',(-9.99706491924,-38.0684833994,1.00998803024));
#64062=CARTESIAN_POINT('Ctrl Pts',(-10.0335312152,-38.162731186,1.01628939441));
#64063=CARTESIAN_POINT('Ctrl Pts',(-10.1069282296,-38.2372246127,1.02897258238));
#64064=CARTESIAN_POINT('Ctrl Pts',(-10.1997888365,-38.2742356238,1.04501919899));
#64065=CARTESIAN_POINT('Ctrl Pts',(-10.2926494305,-38.2742356128,1.06106586964));
#64066=CARTESIAN_POINT('Ctrl Pts',(-10.0283268609,-37.9742356128,0.829566080345));
#64067=CARTESIAN_POINT('Ctrl Pts',(-10.0283268609,-38.0684833924,0.829566080345));
#64068=CARTESIAN_POINT('Ctrl Pts',(-10.0648184673,-38.1627311721,0.835762881167));
#64069=CARTESIAN_POINT('Ctrl Pts',(-10.13826646,-38.2372245963,0.848235381488));
#64070=CARTESIAN_POINT('Ctrl Pts',(-10.231191576,-38.2742356128,0.864015382991));
#64071=CARTESIAN_POINT('Ctrl Pts',(-10.3241166921,-38.2742356128,0.879795384186));
#64072=CARTESIAN_POINT('Ctrl Pts',(-10.0571285787,-37.9742356128,0.645805825719));
#64073=CARTESIAN_POINT('Ctrl Pts',(-10.0571285787,-38.0684833924,0.645805825719));
#64074=CARTESIAN_POINT('Ctrl Pts',(-10.0936931978,-38.1627311721,0.651536792099));
#64075=CARTESIAN_POINT('Ctrl Pts',(-10.1672881417,-38.2372245963,0.663071717384));
#64076=CARTESIAN_POINT('Ctrl Pts',(-10.2603991795,-38.2742356128,0.677665503434));
#64077=CARTESIAN_POINT('Ctrl Pts',(-10.3535102174,-38.2742356128,0.692259289483));
#64078=CARTESIAN_POINT('',(-9.47221976654,-37.9742356128,2.49225909299));
#64079=CARTESIAN_POINT('Ctrl Pts',(-10.0571285787,-37.9742356128,0.645805825719));
#64080=CARTESIAN_POINT('Ctrl Pts',(-10.0283268609,-37.9742356128,0.829566080345));
#64081=CARTESIAN_POINT('Ctrl Pts',(-9.9970648974,-37.9742356128,1.00998816846));
#64082=CARTESIAN_POINT('Ctrl Pts',(-9.96501416235,-37.9742356128,1.19500960441));
#64083=CARTESIAN_POINT('Ctrl Pts',(-9.88272651401,-37.9742356128,1.57928798862));
#64084=CARTESIAN_POINT('Ctrl Pts',(-9.75470839830999,-37.9742356128,1.95515325352));
#64085=CARTESIAN_POINT('Ctrl Pts',(-9.67510718944,-37.9742356128,2.14132026528));
#64086=CARTESIAN_POINT('Ctrl Pts',(-9.57590405793,-37.9742356128,2.32237883269));
#64087=CARTESIAN_POINT('Ctrl Pts',(-9.47221976654,-37.9742356128,2.49225909299));
#64088=CARTESIAN_POINT('Origin',(-9.72648173905357,-37.9763569039206,2.64744470617795));
#64089=CARTESIAN_POINT('Ctrl Pts',(-10.0571285787,-37.9742356128,0.645805825719));
#64090=CARTESIAN_POINT('Ctrl Pts',(-10.0571285787,-36.2942356128,0.645805825719));
#64091=CARTESIAN_POINT('Ctrl Pts',(-10.0282717836,-37.9742356128,0.829917483843));
#64092=CARTESIAN_POINT('Ctrl Pts',(-10.0282717836,-36.2942356128,0.829917483843));
#64093=CARTESIAN_POINT('Ctrl Pts',(-9.9971133399,-37.9742356128,1.00951164248));
#64094=CARTESIAN_POINT('Ctrl Pts',(-9.9971133399,-36.2942356128,1.00951164248));
#64095=CARTESIAN_POINT('Ctrl Pts',(-9.9650475466,-37.9742356128,1.19577528245));
#64096=CARTESIAN_POINT('Ctrl Pts',(-9.9650475466,-36.2942356128,1.19577528245));
#64097=CARTESIAN_POINT('Ctrl Pts',(-9.90758702482,-37.9742356128,1.46388856511));
#64098=CARTESIAN_POINT('Ctrl Pts',(-9.90758702482,-36.2942356128,1.46388856511));
#64099=CARTESIAN_POINT('Ctrl Pts',(-9.82673775568,-37.9742356128,1.73070069002));
#64100=CARTESIAN_POINT('Ctrl Pts',(-9.82673775568,-36.2942356128,1.73070069002));
#64101=CARTESIAN_POINT('Ctrl Pts',(-9.80156823449,-37.9742356128,1.80635994999));
#64102=CARTESIAN_POINT('Ctrl Pts',(-9.80156823449,-36.2942356128,1.80635994999));
#64103=CARTESIAN_POINT('Ctrl Pts',(-9.7321123512,-37.9742356128,1.99616841131));
#64104=CARTESIAN_POINT('Ctrl Pts',(-9.7321123512,-36.2942356128,1.99616841131));
#64105=CARTESIAN_POINT('Ctrl Pts',(-9.64855478712,-37.9742356128,2.17984420246));
#64106=CARTESIAN_POINT('Ctrl Pts',(-9.64855478712,-36.2942356128,2.17984420246));
#64107=CARTESIAN_POINT('Ctrl Pts',(-9.59357915013,-37.9742356128,2.28708022821));
#64108=CARTESIAN_POINT('Ctrl Pts',(-9.59357915013,-36.2942356128,2.28708022821));
#64109=CARTESIAN_POINT('Ctrl Pts',(-9.53312961496,-37.9742356128,2.39246209578));
#64110=CARTESIAN_POINT('Ctrl Pts',(-9.53312961496,-36.2942356128,2.39246209578));
#64111=CARTESIAN_POINT('Ctrl Pts',(-9.47221976654,-37.9742356128,2.49225909299));
#64112=CARTESIAN_POINT('Ctrl Pts',(-9.47221976654,-36.2942356128,2.49225909299));
#64113=CARTESIAN_POINT('',(-9.47221976654,-37.2742356128,2.49225909299));
#64114=CARTESIAN_POINT('Ctrl Pts',(-9.72829242121,-36.2742356128,2.64854983337));
#64115=CARTESIAN_POINT('Ctrl Pts',(-9.64784482414,-36.2742356128,2.59944964919));
#64116=CARTESIAN_POINT('Ctrl Pts',(-9.56739722707,-36.3112466293,2.55034946501));
#64117=CARTESIAN_POINT('Ctrl Pts',(-9.50381146403,-36.3857400536,2.51154069022));
#64118=CARTESIAN_POINT('Ctrl Pts',(-9.47221976654,-36.4799878332,2.49225909299));
#64119=CARTESIAN_POINT('Ctrl Pts',(-9.47221976654,-36.5742356128,2.49225909299));
#64120=CARTESIAN_POINT('Ctrl Pts',(-9.62204834183,-36.2742356128,2.82262414757));
#64121=CARTESIAN_POINT('Ctrl Pts',(-9.54341206422,-36.2742356128,2.77055622916));
#64122=CARTESIAN_POINT('Ctrl Pts',(-9.4647757866,-36.3112466293,2.71848831074));
#64123=CARTESIAN_POINT('Ctrl Pts',(-9.40262168945,-36.3857400536,2.67733384035));
#64124=CARTESIAN_POINT('Ctrl Pts',(-9.37174129605,-36.4799878332,2.65688681573));
#64125=CARTESIAN_POINT('Ctrl Pts',(-9.37174129605,-36.5742356128,2.65688681573));
#64126=CARTESIAN_POINT('Ctrl Pts',(-9.50506026008,-36.2742356128,2.99588690652));
#64127=CARTESIAN_POINT('Ctrl Pts',(-9.42877576551,-36.2742356128,2.94035855976));
#64128=CARTESIAN_POINT('Ctrl Pts',(-9.35249127094,-36.3112466293,2.884830213));
#64129=CARTESIAN_POINT('Ctrl Pts',(-9.29219602419,-36.3857400536,2.84094061937));
#64130=CARTESIAN_POINT('Ctrl Pts',(-9.26223917223,-36.4799878332,2.81913468915));
#64131=CARTESIAN_POINT('Ctrl Pts',(-9.26223917223,-36.5742356128,2.81913468915));
#64132=CARTESIAN_POINT('Ctrl Pts',(-9.3722775174,-36.2742356128,3.17398231372));
#64133=CARTESIAN_POINT('Ctrl Pts',(-9.2994440476,-36.2742356128,3.1133047435));
#64134=CARTESIAN_POINT('Ctrl Pts',(-9.22661057779,-36.3112466293,3.05262717327));
#64135=CARTESIAN_POINT('Ctrl Pts',(-9.1690430188,-36.3857400536,3.00466763756));
#64136=CARTESIAN_POINT('Ctrl Pts',(-9.14044138256,-36.4799878332,2.98083960899));
#64137=CARTESIAN_POINT('Ctrl Pts',(-9.14044138256,-36.5742356128,2.98083960899));
#64138=CARTESIAN_POINT('Ctrl Pts',(-9.06627193321,-36.2742356128,3.49560197264));
#64139=CARTESIAN_POINT('Ctrl Pts',(-9.00530329208,-36.2742356128,3.4216519532));
#64140=CARTESIAN_POINT('Ctrl Pts',(-8.94433465096,-36.3112466293,3.34770193375));
#64141=CARTESIAN_POINT('Ctrl Pts',(-8.896145051,-36.3857400536,3.28925185434));
#64142=CARTESIAN_POINT('Ctrl Pts',(-8.87220272103,-36.4799878332,3.26021174991));
#64143=CARTESIAN_POINT('Ctrl Pts',(-8.87220272103,-36.5742356128,3.26021174991));
#64144=CARTESIAN_POINT('Ctrl Pts',(-8.6627303904,-36.2742356128,3.72995773168));
#64145=CARTESIAN_POINT('Ctrl Pts',(-8.62340519663,-36.2742356128,3.64301562554));
#64146=CARTESIAN_POINT('Ctrl Pts',(-8.58408000286,-36.3112466293,3.55607351941));
#64147=CARTESIAN_POINT('Ctrl Pts',(-8.55299737767,-36.3857400536,3.48735449644));
#64148=CARTESIAN_POINT('Ctrl Pts',(-8.53755441086,-36.4799878332,3.45321241259));
#64149=CARTESIAN_POINT('Ctrl Pts',(-8.53755441086,-36.5742356128,3.45321241259));
#64150=CARTESIAN_POINT('Ctrl Pts',(-8.44964730021,-36.2742356128,3.81095134586));
#64151=CARTESIAN_POINT('Ctrl Pts',(-8.42281522522,-36.2742356128,3.71904827968));
#64152=CARTESIAN_POINT('Ctrl Pts',(-8.39598315023,-36.3112466293,3.62714521349));
#64153=CARTESIAN_POINT('Ctrl Pts',(-8.37477508233,-36.3857400536,3.5545050494));
#64154=CARTESIAN_POINT('Ctrl Pts',(-8.36423815285,-36.4799878332,3.51841480048));
#64155=CARTESIAN_POINT('Ctrl Pts',(-8.36423815285,-36.5742356128,3.51841480048));
#64156=CARTESIAN_POINT('Ctrl Pts',(-8.00109574604,-36.2742356128,3.88930872087));
#64157=CARTESIAN_POINT('Ctrl Pts',(-8.00108575718,-36.2742356128,3.79282946445));
#64158=CARTESIAN_POINT('Ctrl Pts',(-8.00107576832,-36.3112466293,3.69635020803));
#64159=CARTESIAN_POINT('Ctrl Pts',(-8.001067873,-36.3857400536,3.62009302536));
#64160=CARTESIAN_POINT('Ctrl Pts',(-8.00106395051,-36.4799878332,3.58220570956));
#64161=CARTESIAN_POINT('Ctrl Pts',(-8.00106395051,-36.5742356128,3.58220570956));
#64162=CARTESIAN_POINT('Ctrl Pts',(-7.55893216723,-36.2742356128,3.81476466023));
#64163=CARTESIAN_POINT('Ctrl Pts',(-7.58431240017,-36.2742356128,3.72263792299));
#64164=CARTESIAN_POINT('Ctrl Pts',(-7.60969263311,-36.3112466293,3.63051118575));
#64165=CARTESIAN_POINT('Ctrl Pts',(-7.62975316565,-36.3857400536,3.55769423287));
#64166=CARTESIAN_POINT('Ctrl Pts',(-7.63971995782,-36.4799878332,3.52151614777));
#64167=CARTESIAN_POINT('Ctrl Pts',(-7.63971995782,-36.5742356128,3.52151614777));
#64168=CARTESIAN_POINT('Ctrl Pts',(-7.3474262191,-36.2742356128,3.73898310239));
#64169=CARTESIAN_POINT('Ctrl Pts',(-7.38416955592,-36.2742356128,3.65120125317));
#64170=CARTESIAN_POINT('Ctrl Pts',(-7.42091289275,-36.3112466293,3.56341940395));
#64171=CARTESIAN_POINT('Ctrl Pts',(-7.44995483128,-36.3857400536,3.49403667229));
#64172=CARTESIAN_POINT('Ctrl Pts',(-7.46438389272,-36.4799878332,3.45956479805));
#64173=CARTESIAN_POINT('Ctrl Pts',(-7.46438389272,-36.5742356128,3.45956479805));
#64174=CARTESIAN_POINT('Ctrl Pts',(-6.95886520076,-36.2742356128,3.53476719039));
#64175=CARTESIAN_POINT('Ctrl Pts',(-7.01431452426,-36.2742356128,3.45705331726));
#64176=CARTESIAN_POINT('Ctrl Pts',(-7.06976384776,-36.3112466293,3.37933944414));
#64177=CARTESIAN_POINT('Ctrl Pts',(-7.11359096799,-36.3857400536,3.31791439199));
#64178=CARTESIAN_POINT('Ctrl Pts',(-7.13536587928,-36.4799878332,3.2873962493));
#64179=CARTESIAN_POINT('Ctrl Pts',(-7.13536587928,-36.5742356128,3.2873962493));
#64180=CARTESIAN_POINT('Ctrl Pts',(-6.64385972405,-36.2742356128,3.24906826835));
#64181=CARTESIAN_POINT('Ctrl Pts',(-6.71208744564,-36.2742356128,3.18320934231));
#64182=CARTESIAN_POINT('Ctrl Pts',(-6.78031516723,-36.3112466293,3.11735041628));
#64183=CARTESIAN_POINT('Ctrl Pts',(-6.83424235588,-36.3857400536,3.06529556086));
#64184=CARTESIAN_POINT('Ctrl Pts',(-6.86103530699,-36.4799878332,3.03943279584));
#64185=CARTESIAN_POINT('Ctrl Pts',(-6.86103530699,-36.5742356128,3.03943279584));
#64186=CARTESIAN_POINT('Ctrl Pts',(-6.50139236315,-36.2742356128,3.08803899971));
#64187=CARTESIAN_POINT('Ctrl Pts',(-6.57495070071,-36.2742356128,3.02825036242));
#64188=CARTESIAN_POINT('Ctrl Pts',(-6.64850903826,-36.3112466293,2.96846172512));
#64189=CARTESIAN_POINT('Ctrl Pts',(-6.7066494798,-36.3857400536,2.92120470051));
#64190=CARTESIAN_POINT('Ctrl Pts',(-6.73553582371,-36.4799878332,2.89772585638));
#64191=CARTESIAN_POINT('Ctrl Pts',(-6.73553582371,-36.5742356128,2.89772585638));
#64192=CARTESIAN_POINT('Ctrl Pts',(-6.37711509272,-36.2742356128,2.91269406835));
#64193=CARTESIAN_POINT('Ctrl Pts',(-6.45574912481,-36.2742356128,2.85992970991));
#64194=CARTESIAN_POINT('Ctrl Pts',(-6.5343831569,-36.3112466293,2.80716535147));
#64195=CARTESIAN_POINT('Ctrl Pts',(-6.59653551323,-36.3857400536,2.76546048015));
#64196=CARTESIAN_POINT('Ctrl Pts',(-6.62741499076,-36.4799878332,2.74473989905));
#64197=CARTESIAN_POINT('Ctrl Pts',(-6.62741499076,-36.5742356128,2.74473989905));
#64198=CARTESIAN_POINT('Ctrl Pts',(-6.27496307903,-36.2742356128,2.72284588841));
#64199=CARTESIAN_POINT('Ctrl Pts',(-6.35795892644,-36.2742356128,2.67818792885));
#64200=CARTESIAN_POINT('Ctrl Pts',(-6.44095477384,-36.3112466293,2.63352996929));
#64201=CARTESIAN_POINT('Ctrl Pts',(-6.50655467338,-36.3857400536,2.59823232788));
#64202=CARTESIAN_POINT('Ctrl Pts',(-6.53914706644,-36.4799878332,2.58069518817));
#64203=CARTESIAN_POINT('Ctrl Pts',(-6.53914706644,-36.5742356128,2.58069518817));
#64204=CARTESIAN_POINT('',(-6.53914703399611,-36.5742356128,2.5806951245344));
#64205=CARTESIAN_POINT('Origin',(-6.27683128588048,-36.5721143277297,2.72184106982266));
#64206=CARTESIAN_POINT('Ctrl Pts',(-9.47221976654,-36.5742356128,2.49225909299));
#64207=CARTESIAN_POINT('Ctrl Pts',(-9.45178452931047,-36.5742356128,2.52574095783471));
#64208=CARTESIAN_POINT('Ctrl Pts',(-9.43084330217428,-36.5742356128,2.55920754094306));
#64209=CARTESIAN_POINT('Ctrl Pts',(-9.40933378143277,-36.5742356128,2.59263503957777));
#64210=CARTESIAN_POINT('Ctrl Pts',(-9.38762982918854,-36.5742356128,2.62636470016531));
#64211=CARTESIAN_POINT('Ctrl Pts',(-9.3653466531979,-36.5742356128,2.66005418215412));
#64212=CARTESIAN_POINT('Ctrl Pts',(-9.34240607923193,-36.5742356128,2.69362043224762));
#64213=CARTESIAN_POINT('Ctrl Pts',(-9.33286416290745,-36.5742356128,2.70758199878009));
#64214=CARTESIAN_POINT('Ctrl Pts',(-9.32320839801377,-36.5742356128,2.72152158549076));
#64215=CARTESIAN_POINT('Ctrl Pts',(-9.31343285049753,-36.5742356128,2.73543055204732));
#64216=CARTESIAN_POINT('Ctrl Pts',(-9.3067521540374,-36.5742356128,2.74493606398759));
#64217=CARTESIAN_POINT('Ctrl Pts',(-9.30001551073448,-36.5742356128,2.75442724329928));
#64218=CARTESIAN_POINT('Ctrl Pts',(-9.29322102418923,-36.5742356128,2.76390095330808));
#64219=CARTESIAN_POINT('Ctrl Pts',(-9.28846887090744,-36.5742356128,2.77052699072964));
#64220=CARTESIAN_POINT('Ctrl Pts',(-9.28368898333415,-36.5742356128,2.77714375911308));
#64221=CARTESIAN_POINT('Ctrl Pts',(-9.27887112661667,-36.5742356128,2.78376311685622));
#64222=CARTESIAN_POINT('Ctrl Pts',(-9.25361775870907,-36.5742356128,2.81845926624413));
#64223=CARTESIAN_POINT('Ctrl Pts',(-9.22738194732705,-36.5742356128,2.85314293661054));
#64224=CARTESIAN_POINT('Ctrl Pts',(-9.2001122283292,-36.5742356128,2.88751310400007));
#64225=CARTESIAN_POINT('Ctrl Pts',(-9.17396931118659,-36.5742356128,2.92046307456312));
#64226=CARTESIAN_POINT('Ctrl Pts',(-9.14687516035206,-36.5742356128,2.95312341883169));
#64227=CARTESIAN_POINT('Ctrl Pts',(-9.11881276730823,-36.5742356128,2.98519628971722));
#64228=CARTESIAN_POINT('Ctrl Pts',(-9.10657791227766,-36.5742356128,2.99917966330499));
#64229=CARTESIAN_POINT('Ctrl Pts',(-9.09415946971097,-36.5742356128,3.01305106866214));
#64230=CARTESIAN_POINT('Ctrl Pts',(-9.08155851754365,-36.5742356128,3.02678491299355));
#64231=CARTESIAN_POINT('Ctrl Pts',(-9.07585005623246,-36.5742356128,3.03300659513144));
#64232=CARTESIAN_POINT('Ctrl Pts',(-9.07010538548969,-36.5742356128,3.03919874111963));
#64233=CARTESIAN_POINT('Ctrl Pts',(-9.06432087221495,-36.5742356128,3.04536306782802));
#64234=CARTESIAN_POINT('Ctrl Pts',(-9.03453905552488,-36.5742356128,3.07710037040262));
#64235=CARTESIAN_POINT('Ctrl Pts',(-9.00355542500468,-36.5742356128,3.10825234925048));
#64236=CARTESIAN_POINT('Ctrl Pts',(-8.97133952680228,-36.5742356128,3.13849784243435));
#64237=CARTESIAN_POINT('Ctrl Pts',(-8.94121606492088,-36.5742356128,3.1667788779431));
#64238=CARTESIAN_POINT('Ctrl Pts',(-8.91001482010756,-36.5742356128,3.19426625312343));
#64239=CARTESIAN_POINT('Ctrl Pts',(-8.8777556198925,-36.5742356128,3.22069087225574));
#64240=CARTESIAN_POINT('Ctrl Pts',(-8.86422662034783,-36.5742356128,3.23177294055954));
#64241=CARTESIAN_POINT('Ctrl Pts',(-8.85051214048935,-36.5742356128,3.24266809673354));
#64242=CARTESIAN_POINT('Ctrl Pts',(-8.83661643344406,-36.5742356128,3.25335680269378));
#64243=CARTESIAN_POINT('Ctrl Pts',(-8.81836242792662,-36.5742356128,3.26739795201684));
#64244=CARTESIAN_POINT('Ctrl Pts',(-8.79979723642711,-36.5742356128,3.28108152158642));
#64245=CARTESIAN_POINT('Ctrl Pts',(-8.78091542981201,-36.5742356128,3.29437421039659));
#64246=CARTESIAN_POINT('Ctrl Pts',(-8.7489680446299,-36.5742356128,3.31686499521297));
#64247=CARTESIAN_POINT('Ctrl Pts',(-8.71609229015667,-36.5742356128,3.33825047301422));
#64248=CARTESIAN_POINT('Ctrl Pts',(-8.68229792411548,-36.5742356128,3.35836411240285));
#64249=CARTESIAN_POINT('Ctrl Pts',(-8.6475947598128,-36.5742356128,3.37901864788303));
#64250=CARTESIAN_POINT('Ctrl Pts',(-8.61192315156315,-36.5742356128,3.39833127668768));
#64251=CARTESIAN_POINT('Ctrl Pts',(-8.57534988837971,-36.5742356128,3.41612220858467));
#64252=CARTESIAN_POINT('Ctrl Pts',(-8.5490844798751,-36.5742356128,3.42889892177015));
#64253=CARTESIAN_POINT('Ctrl Pts',(-8.5223552581089,-36.5742356128,3.44089078500327));
#64254=CARTESIAN_POINT('Ctrl Pts',(-8.49520280272183,-36.5742356128,3.45203482771473));
#64255=CARTESIAN_POINT('Ctrl Pts',(-8.47642666650715,-36.5742356128,3.45974102079929));
#64256=CARTESIAN_POINT('Ctrl Pts',(-8.45744605695094,-36.5742356128,3.46704270285512));
#64257=CARTESIAN_POINT('Ctrl Pts',(-8.43828543372318,-36.5742356128,3.47391782434403));
#64258=CARTESIAN_POINT('Ctrl Pts',(-8.4005107660617,-36.5742356128,3.48747194658153));
#64259=CARTESIAN_POINT('Ctrl Pts',(-8.36205258057802,-36.5742356128,3.49935947844771));
#64260=CARTESIAN_POINT('Ctrl Pts',(-8.32308624720095,-36.5742356128,3.50946141251245));
#64261=CARTESIAN_POINT('Ctrl Pts',(-8.28498059057218,-36.5742356128,3.5193402180709));
#64262=CARTESIAN_POINT('Ctrl Pts',(-8.24638977185156,-36.5742356128,3.52751083953927));
#64263=CARTESIAN_POINT('Ctrl Pts',(-8.20750090981374,-36.5742356128,3.53390471385943));
#64264=CARTESIAN_POINT('Ctrl Pts',(-8.17019437411012,-36.5742356128,3.54003843153873));
#64265=CARTESIAN_POINT('Ctrl Pts',(-8.1326142429901,-36.5742356128,3.54453677805079));
#64266=CARTESIAN_POINT('Ctrl Pts',(-8.09493654742072,-36.5742356128,3.54738491301163));
#64267=CARTESIAN_POINT('Ctrl Pts',(-8.06426248640137,-36.5742356128,3.54970362874676));
#64268=CARTESIAN_POINT('Ctrl Pts',(-8.03352409131106,-36.5742356128,3.55092933198329));
#64269=CARTESIAN_POINT('Ctrl Pts',(-8.00281747813575,-36.5742356128,3.55107964607802));
#64270=CARTESIAN_POINT('Ctrl Pts',(-7.96270277011772,-36.5742356128,3.55127601439733));
#64271=CARTESIAN_POINT('Ctrl Pts',(-7.92264137730165,-36.5742356128,3.54963567943145));
#64272=CARTESIAN_POINT('Ctrl Pts',(-7.88278787617713,-36.5742356128,3.54619249889203));
#64273=CARTESIAN_POINT('Ctrl Pts',(-7.8405011481773,-36.5742356128,3.54253909743881));
#64274=CARTESIAN_POINT('Ctrl Pts',(-7.79844929680864,-36.5742356128,3.53685642893967));
#64275=CARTESIAN_POINT('Ctrl Pts',(-7.75682042603883,-36.5742356128,3.52924798342734));
#64276=CARTESIAN_POINT('Ctrl Pts',(-7.73188548808965,-36.5742356128,3.52469066267299));
#64277=CARTESIAN_POINT('Ctrl Pts',(-7.70710231204621,-36.5742356128,3.51944358499482));
#64278=CARTESIAN_POINT('Ctrl Pts',(-7.68250988053131,-36.5742356128,3.51353757033189));
#64279=CARTESIAN_POINT('Ctrl Pts',(-7.66774913753318,-36.5742356128,3.50999269252955));
#64280=CARTESIAN_POINT('Ctrl Pts',(-7.65305760413022,-36.5742356128,3.50621083142867));
#64281=CARTESIAN_POINT('Ctrl Pts',(-7.63842877546141,-36.5742356128,3.50219506857823));
#64282=CARTESIAN_POINT('Ctrl Pts',(-7.59473414475351,-36.5742356128,3.49020044626549));
#64283=CARTESIAN_POINT('Ctrl Pts',(-7.55163483891475,-36.5742356128,3.47612347756162));
#64284=CARTESIAN_POINT('Ctrl Pts',(-7.50935266584155,-36.5742356128,3.4601746702419));
#64285=CARTESIAN_POINT('Ctrl Pts',(-7.46870308154542,-36.5742356128,3.44484167431373));
#64286=CARTESIAN_POINT('Ctrl Pts',(-7.4288095588,-36.5742356128,3.42778024800884));
#64287=CARTESIAN_POINT('Ctrl Pts',(-7.38982831413737,-36.5742356128,3.40920241830386));
#64288=CARTESIAN_POINT('Ctrl Pts',(-7.3633352747518,-36.5742356128,3.39657626492337));
#64289=CARTESIAN_POINT('Ctrl Pts',(-7.33726275758436,-36.5742356128,3.38325016153255));
#64290=CARTESIAN_POINT('Ctrl Pts',(-7.31164578606096,-36.5742356128,3.36929213910639));
#64291=CARTESIAN_POINT('Ctrl Pts',(-7.29176246227058,-36.5742356128,3.35845823240828));
#64292=CARTESIAN_POINT('Ctrl Pts',(-7.27214586950384,-36.5742356128,3.34723983933327));
#64293=CARTESIAN_POINT('Ctrl Pts',(-7.25279266780678,-36.5742356128,3.33565750429941));
#64294=CARTESIAN_POINT('Ctrl Pts',(-7.21928492757203,-36.5742356128,3.31560408473085));
#64295=CARTESIAN_POINT('Ctrl Pts',(-7.18657606175943,-36.5742356128,3.29446497149353));
#64296=CARTESIAN_POINT('Ctrl Pts',(-7.15465499843816,-36.5742356128,3.27234915626901));
#64297=CARTESIAN_POINT('Ctrl Pts',(-7.11154237878949,-36.5742356128,3.24247951438399));
#64298=CARTESIAN_POINT('Ctrl Pts',(-7.06985594727397,-36.5742356128,3.21082568782116));
#64299=CARTESIAN_POINT('Ctrl Pts',(-7.02958048187159,-36.5742356128,3.17758678921859));
#64300=CARTESIAN_POINT('Ctrl Pts',(-6.98830979588565,-36.5742356128,3.14352654601492));
#64301=CARTESIAN_POINT('Ctrl Pts',(-6.94852125819688,-36.5742356128,3.10780256054435));
#64302=CARTESIAN_POINT('Ctrl Pts',(-6.91024718858311,-36.5742356128,3.07060371749456));
#64303=CARTESIAN_POINT('Ctrl Pts',(-6.87168160917733,-36.5742356128,3.03312155398501));
#64304=CARTESIAN_POINT('Ctrl Pts',(-6.83465434719058,-36.5742356128,2.99414259605905));
#64305=CARTESIAN_POINT('Ctrl Pts',(-6.79923734995239,-36.5742356128,2.95382526881695));
#64306=CARTESIAN_POINT('Ctrl Pts',(-6.76426659337508,-36.5742356128,2.91401592452532));
#64307=CARTESIAN_POINT('Ctrl Pts',(-6.7308664945914,-36.5742356128,2.87290222361067));
#64308=CARTESIAN_POINT('Ctrl Pts',(-6.6991334408564,-36.5742356128,2.83059477854831));
#64309=CARTESIAN_POINT('Ctrl Pts',(-6.66863403289319,-36.5742356128,2.78993206648746));
#64310=CARTESIAN_POINT('Ctrl Pts',(-6.63967521531564,-36.5742356128,2.74816688282246));
#64311=CARTESIAN_POINT('Ctrl Pts',(-6.61235787702105,-36.5742356128,2.70535332001463));
#64312=CARTESIAN_POINT('Ctrl Pts',(-6.58644612667648,-36.5742356128,2.66474268881497));
#64313=CARTESIAN_POINT('Ctrl Pts',(-6.56201175880056,-36.5742356128,2.62318890122085));
#64314=CARTESIAN_POINT('Ctrl Pts',(-6.53914706644,-36.5742356128,2.58069518817));
#64315=CARTESIAN_POINT('Ctrl Pts',(-6.53914719008,-37.9742356128,2.58069542603));
#64316=CARTESIAN_POINT('Ctrl Pts',(-6.53914719078,-38.0684833925,2.58069542736));
#64317=CARTESIAN_POINT('Ctrl Pts',(-6.50655468231,-38.1627311721,2.59823235248));
#64318=CARTESIAN_POINT('Ctrl Pts',(-6.44095454962,-38.2372245964,2.63352956036));
#64319=CARTESIAN_POINT('Ctrl Pts',(-6.35795840683,-38.2742356129,2.67818697059));
#64320=CARTESIAN_POINT('Ctrl Pts',(-6.27496226376,-38.2742356128,2.7228443803));
#64321=CARTESIAN_POINT('Ctrl Pts',(-6.60862882414,-37.9742356128,2.70982607508));
#64322=CARTESIAN_POINT('Ctrl Pts',(-6.60862879596,-38.0684833921,2.70982602153));
#64323=CARTESIAN_POINT('Ctrl Pts',(-6.57738634684,-38.1627311713,2.72987203609));
#64324=CARTESIAN_POINT('Ctrl Pts',(-6.5145035418,-38.2372245954,2.7702194031));
#64325=CARTESIAN_POINT('Ctrl Pts',(-6.43494534104,-38.2742356122,2.8212662386));
#64326=CARTESIAN_POINT('Ctrl Pts',(-6.35538715106,-38.2742356128,2.8723130951));
#64327=CARTESIAN_POINT('Ctrl Pts',(-6.69040968596,-37.9742356128,2.83211943121));
#64328=CARTESIAN_POINT('Ctrl Pts',(-6.69040972795,-38.0684833969,2.83211950901));
#64329=CARTESIAN_POINT('Ctrl Pts',(-6.66068017578,-38.162731181,2.85439814262));
#64330=CARTESIAN_POINT('Ctrl Pts',(-6.60084240217,-38.2372246069,2.89923913281));
#64331=CARTESIAN_POINT('Ctrl Pts',(-6.52513665775,-38.2742356199,2.95597109413));
#64332=CARTESIAN_POINT('Ctrl Pts',(-6.44943089912,-38.2742356128,3.0127030234));
#64333=CARTESIAN_POINT('Ctrl Pts',(-6.78293784481,-37.9742356128,2.94714618869));
#64334=CARTESIAN_POINT('Ctrl Pts',(-6.78293783118,-38.0684833893,2.94714616566));
#64335=CARTESIAN_POINT('Ctrl Pts',(-6.75483332907,-38.1627311657,2.97143599883));
#64336=CARTESIAN_POINT('Ctrl Pts',(-6.69826638119,-38.2372245888,3.02032504454));
#64337=CARTESIAN_POINT('Ctrl Pts',(-6.62669887685,-38.2742356078,3.0821786334));
#64338=CARTESIAN_POINT('Ctrl Pts',(-6.55513137645,-38.2742356128,3.14403223264));
#64339=CARTESIAN_POINT('Ctrl Pts',(-7.02925067951,-37.9742356128,3.20337077768));
#64340=CARTESIAN_POINT('Ctrl Pts',(-7.02925069855,-38.0684833969,3.20337080984));
#64341=CARTESIAN_POINT('Ctrl Pts',(-7.0054973778,-38.1627311809,3.23224071513));
#64342=CARTESIAN_POINT('Ctrl Pts',(-6.95768819081,-38.2372246068,3.29034821166));
#64343=CARTESIAN_POINT('Ctrl Pts',(-6.89720082675,-38.2742356198,3.36386477088));
#64344=CARTESIAN_POINT('Ctrl Pts',(-6.8367134572,-38.2742356128,3.43738131562));
#64345=CARTESIAN_POINT('Ctrl Pts',(-7.32593788713,-37.9742356128,3.39828475585));
#64346=CARTESIAN_POINT('Ctrl Pts',(-7.32593786055,-38.0684833862,3.39828471095));
#64347=CARTESIAN_POINT('Ctrl Pts',(-7.30823659937,-38.1627311597,3.43122238484));
#64348=CARTESIAN_POINT('Ctrl Pts',(-7.27260863663,-38.2372245817,3.49751726565));
#64349=CARTESIAN_POINT('Ctrl Pts',(-7.22753278341,-38.2742356031,3.58139243425));
#64350=CARTESIAN_POINT('Ctrl Pts',(-7.18245693785,-38.2742356128,3.66526762307));
#64351=CARTESIAN_POINT('Ctrl Pts',(-7.51861181031,-37.9742356128,3.48826721235));
#64352=CARTESIAN_POINT('Ctrl Pts',(-7.51861177171,-38.0684833924,3.48826721752));
#64353=CARTESIAN_POINT('Ctrl Pts',(-7.50543345832,-38.1627311719,3.52352395259));
#64354=CARTESIAN_POINT('Ctrl Pts',(-7.4789090267,-38.2372245962,3.59448646302));
#64355=CARTESIAN_POINT('Ctrl Pts',(-7.44535080562,-38.2742356127,3.68426698954));
#64356=CARTESIAN_POINT('Ctrl Pts',(-7.4117926006,-38.2742356128,3.77404751415));
#64357=CARTESIAN_POINT('Ctrl Pts',(-7.91545972539,-37.9742356128,3.58665245723));
#64358=CARTESIAN_POINT('Ctrl Pts',(-7.91545976172,-38.0684833925,3.58665245236));
#64359=CARTESIAN_POINT('Ctrl Pts',(-7.91297425904,-38.1627311722,3.62465357638));
#64360=CARTESIAN_POINT('Ctrl Pts',(-7.90797155303,-38.2372245965,3.70113983127));
#64361=CARTESIAN_POINT('Ctrl Pts',(-7.90164219398,-38.2742356129,3.79790890862));
#64362=CARTESIAN_POINT('Ctrl Pts',(-7.89531281982,-38.2742356128,3.89467798777));
#64363=CARTESIAN_POINT('Ctrl Pts',(-8.32196834325,-37.9742356128,3.53349085056));
#64364=CARTESIAN_POINT('Ctrl Pts',(-8.32196830907,-38.0684833924,3.53349085514));
#64365=CARTESIAN_POINT('Ctrl Pts',(-8.33127827363,-38.1627311719,3.57001419685));
#64366=CARTESIAN_POINT('Ctrl Pts',(-8.35001682583,-38.2372245962,3.64352605744));
#64367=CARTESIAN_POINT('Ctrl Pts',(-8.37372453412,-38.2742356127,3.73653197592));
#64368=CARTESIAN_POINT('Ctrl Pts',(-8.39743225663,-38.2742356128,3.82953789272));
#64369=CARTESIAN_POINT('Ctrl Pts',(-8.51257873567,-37.9742356128,3.46755862103));
#64370=CARTESIAN_POINT('Ctrl Pts',(-8.51257875377,-38.0684833947,3.46755862147));
#64371=CARTESIAN_POINT('Ctrl Pts',(-8.52738481159,-38.1627311765,3.50208416494));
#64372=CARTESIAN_POINT('Ctrl Pts',(-8.55718585956,-38.2372246016,3.57157437773));
#64373=CARTESIAN_POINT('Ctrl Pts',(-8.59488945106,-38.2742356164,3.65949244318));
#64374=CARTESIAN_POINT('Ctrl Pts',(-8.63259303718,-38.2742356128,3.74741050329));
#64375=CARTESIAN_POINT('Ctrl Pts',(-8.86229619026,-37.9742356128,3.27052379371));
#64376=CARTESIAN_POINT('Ctrl Pts',(-8.86229617129,-38.0684833901,3.27052379325));
#64377=CARTESIAN_POINT('Ctrl Pts',(-8.88606803187,-38.1627311673,3.2997528949));
#64378=CARTESIAN_POINT('Ctrl Pts',(-8.9339141532,-38.2372245908,3.35858401846));
#64379=CARTESIAN_POINT('Ctrl Pts',(-8.99444841221,-38.2742356091,3.43301585235));
#64380=CARTESIAN_POINT('Ctrl Pts',(-9.05498267684,-38.2742356128,3.50744769184));
#64381=CARTESIAN_POINT('Ctrl Pts',(-9.14074177278,-37.9742356128,2.98053227682));
#64382=CARTESIAN_POINT('Ctrl Pts',(-9.14074179266,-38.0684833949,2.9805322773));
#64383=CARTESIAN_POINT('Ctrl Pts',(-9.16934690231,-38.162731177,3.00435821305));
#64384=CARTESIAN_POINT('Ctrl Pts',(-9.22692183769,-38.2372246021,3.05231286426));
#64385=CARTESIAN_POINT('Ctrl Pts',(-9.29976445069,-38.2742356167,3.11298454342));
#64386=CARTESIAN_POINT('Ctrl Pts',(-9.37260705779,-38.2742356128,3.1736562167));
#64387=CARTESIAN_POINT('Ctrl Pts',(-9.26235716204,-37.9742356128,2.81894517549));
#64388=CARTESIAN_POINT('Ctrl Pts',(-9.2623571652,-38.0684833948,2.81894517181));
#64389=CARTESIAN_POINT('Ctrl Pts',(-9.29231496964,-38.1627311767,2.84074916224));
#64390=CARTESIAN_POINT('Ctrl Pts',(-9.35261048666,-38.2372246019,2.88463754863));
#64391=CARTESIAN_POINT('Ctrl Pts',(-9.42889602942,-38.2742356165,2.94016320761));
#64392=CARTESIAN_POINT('Ctrl Pts',(-9.50518155925,-38.2742356128,2.99568888448));
#64393=CARTESIAN_POINT('Ctrl Pts',(-9.37180357922,-37.9742356128,2.65678476864));
#64394=CARTESIAN_POINT('Ctrl Pts',(-9.37180357922,-38.0684833924,2.65678476864));
#64395=CARTESIAN_POINT('Ctrl Pts',(-9.40268405231,-38.1627311721,2.67723166281));
#64396=CARTESIAN_POINT('Ctrl Pts',(-9.46483940501,-38.2372245963,2.71838407584));
#64397=CARTESIAN_POINT('Ctrl Pts',(-9.54347679851,-38.2742356128,2.77045016604));
#64398=CARTESIAN_POINT('Ctrl Pts',(-9.6221141989,-38.2742356128,2.82251624486));
#64399=CARTESIAN_POINT('Ctrl Pts',(-9.47221976654,-37.9742356128,2.49225909299));
#64400=CARTESIAN_POINT('Ctrl Pts',(-9.47221976654,-38.0684833924,2.49225909299));
#64401=CARTESIAN_POINT('Ctrl Pts',(-9.50381146403,-38.1627311721,2.51154069022));
#64402=CARTESIAN_POINT('Ctrl Pts',(-9.56739722707,-38.2372245963,2.55034946501));
#64403=CARTESIAN_POINT('Ctrl Pts',(-9.64784482414,-38.2742356128,2.59944964919));
#64404=CARTESIAN_POINT('Ctrl Pts',(-9.72829242121,-38.2742356128,2.64854983337));
#64405=CARTESIAN_POINT('',(-6.53914701908,-37.9742356128,2.5806950957));
#64406=CARTESIAN_POINT('Ctrl Pts',(-9.47221976654,-37.9742356128,2.49225909299));
#64407=CARTESIAN_POINT('Ctrl Pts',(-9.37180357922,-37.9742356128,2.65678476864));
#64408=CARTESIAN_POINT('Ctrl Pts',(-9.26235716204,-37.9742356128,2.81894517549));
#64409=CARTESIAN_POINT('Ctrl Pts',(-9.14074177278,-37.9742356128,2.98053227682));
#64410=CARTESIAN_POINT('Ctrl Pts',(-8.86229619026,-37.9742356128,3.27052379371));
#64411=CARTESIAN_POINT('Ctrl Pts',(-8.51257873567,-37.9742356128,3.46755862103));
#64412=CARTESIAN_POINT('Ctrl Pts',(-8.32196834325,-37.9742356128,3.53349085056));
#64413=CARTESIAN_POINT('Ctrl Pts',(-7.91545972539,-37.9742356128,3.58665245723));
#64414=CARTESIAN_POINT('Ctrl Pts',(-7.51861181031,-37.9742356128,3.48826721235));
#64415=CARTESIAN_POINT('Ctrl Pts',(-7.32593788713,-37.9742356128,3.39828475585));
#64416=CARTESIAN_POINT('Ctrl Pts',(-7.02925067951,-37.9742356128,3.20337077768));
#64417=CARTESIAN_POINT('Ctrl Pts',(-6.78293784481,-37.9742356128,2.94714618869));
#64418=CARTESIAN_POINT('Ctrl Pts',(-6.69040968596,-37.9742356128,2.83211943121));
#64419=CARTESIAN_POINT('Ctrl Pts',(-6.60862882414,-37.9742356128,2.70982607508));
#64420=CARTESIAN_POINT('Ctrl Pts',(-6.53914701908,-37.9742356128,2.5806950957));
#64421=CARTESIAN_POINT('Origin',(-6.2768299648437,-37.9763568910239,2.72183863295591));
#64422=CARTESIAN_POINT('Ctrl Pts',(-9.47221976654,-37.9742356128,2.49225909299));
#64423=CARTESIAN_POINT('Ctrl Pts',(-9.47221976654,-36.2942356128,2.49225909299));
#64424=CARTESIAN_POINT('Ctrl Pts',(-9.43799021757,-37.9742356128,2.54834207942));
#64425=CARTESIAN_POINT('Ctrl Pts',(-9.43799021757,-36.2942356128,2.54834207942));
#64426=CARTESIAN_POINT('Ctrl Pts',(-9.40258508843,-37.9742356128,2.60436998551));
#64427=CARTESIAN_POINT('Ctrl Pts',(-9.40258508843,-36.2942356128,2.60436998551));
#64428=CARTESIAN_POINT('Ctrl Pts',(-9.36584102959,-37.9742356128,2.66040353433));
#64429=CARTESIAN_POINT('Ctrl Pts',(-9.36584102959,-36.2942356128,2.66040353433));
#64430=CARTESIAN_POINT('Ctrl Pts',(-9.28925382834,-37.9742356128,2.77218463031));
#64431=CARTESIAN_POINT('Ctrl Pts',(-9.28925382834,-36.2942356128,2.77218463031));
#64432=CARTESIAN_POINT('Ctrl Pts',(-9.20593013024,-37.9742356128,2.88194354511));
#64433=CARTESIAN_POINT('Ctrl Pts',(-9.20593013024,-36.2942356128,2.88194354511));
#64434=CARTESIAN_POINT('Ctrl Pts',(-9.16069630404,-37.9742356128,2.93809779908));
#64435=CARTESIAN_POINT('Ctrl Pts',(-9.16069630404,-36.2942356128,2.93809779908));
#64436=CARTESIAN_POINT('Ctrl Pts',(-9.06741515882,-37.9742356128,3.0462171446));
#64437=CARTESIAN_POINT('Ctrl Pts',(-9.06741515882,-36.2942356128,3.0462171446));
#64438=CARTESIAN_POINT('Ctrl Pts',(-8.9630009386,-37.9742356128,3.14917335528));
#64439=CARTESIAN_POINT('Ctrl Pts',(-8.9630009386,-36.2942356128,3.14917335528));
#64440=CARTESIAN_POINT('Ctrl Pts',(-8.90717355699,-37.9742356128,3.19917508688));
#64441=CARTESIAN_POINT('Ctrl Pts',(-8.90717355699,-36.2942356128,3.19917508688));
#64442=CARTESIAN_POINT('Ctrl Pts',(-8.78922597568,-37.9742356128,3.29398598989));
#64443=CARTESIAN_POINT('Ctrl Pts',(-8.78922597568,-36.2942356128,3.29398598989));
#64444=CARTESIAN_POINT('Ctrl Pts',(-8.65978894936,-37.9742356128,3.37495922004));
#64445=CARTESIAN_POINT('Ctrl Pts',(-8.65978894936,-36.2942356128,3.37495922004));
#64446=CARTESIAN_POINT('Ctrl Pts',(-8.59150582736,-37.9742356128,3.41174862899));
#64447=CARTESIAN_POINT('Ctrl Pts',(-8.59150582736,-36.2942356128,3.41174862899));
#64448=CARTESIAN_POINT('Ctrl Pts',(-8.37641925249,-37.9742356128,3.50886242158));
#64449=CARTESIAN_POINT('Ctrl Pts',(-8.37641925249,-36.2942356128,3.50886242158));
#64450=CARTESIAN_POINT('Ctrl Pts',(-8.13973403839,-37.9742356128,3.5585372531));
#64451=CARTESIAN_POINT('Ctrl Pts',(-8.13973403839,-36.2942356128,3.5585372531));
#64452=CARTESIAN_POINT('Ctrl Pts',(-7.97806372235,-37.9742356128,3.56548871191));
#64453=CARTESIAN_POINT('Ctrl Pts',(-7.97806372235,-36.2942356128,3.56548871191));
#64454=CARTESIAN_POINT('Ctrl Pts',(-7.74013214217,-37.9742356128,3.53951961667));
#64455=CARTESIAN_POINT('Ctrl Pts',(-7.74013214217,-36.2942356128,3.53951961667));
#64456=CARTESIAN_POINT('Ctrl Pts',(-7.51591788103,-37.9742356128,3.46603879043));
#64457=CARTESIAN_POINT('Ctrl Pts',(-7.51591788103,-36.2942356128,3.46603879043));
#64458=CARTESIAN_POINT('Ctrl Pts',(-7.44307437439,-37.9742356128,3.43661441301));
#64459=CARTESIAN_POINT('Ctrl Pts',(-7.44307437439,-36.2942356128,3.43661441301));
#64460=CARTESIAN_POINT('Ctrl Pts',(-7.16744129772,-37.9742356128,3.30480694269));
#64461=CARTESIAN_POINT('Ctrl Pts',(-7.16744129772,-36.2942356128,3.30480694269));
#64462=CARTESIAN_POINT('Ctrl Pts',(-6.93248240874,-37.9742356128,3.11682904882));
#64463=CARTESIAN_POINT('Ctrl Pts',(-6.93248240874,-36.2942356128,3.11682904882));
#64464=CARTESIAN_POINT('Ctrl Pts',(-6.77645737492,-37.9742356128,2.95406352231));
#64465=CARTESIAN_POINT('Ctrl Pts',(-6.77645737492,-36.2942356128,2.95406352231));
#64466=CARTESIAN_POINT('Ctrl Pts',(-6.64407030457,-37.9742356128,2.77569349664));
#64467=CARTESIAN_POINT('Ctrl Pts',(-6.64407030457,-36.2942356128,2.77569349664));
#64468=CARTESIAN_POINT('Ctrl Pts',(-6.53914701908,-37.9742356128,2.5806950957));
#64469=CARTESIAN_POINT('Ctrl Pts',(-6.53914701908,-36.2942356128,2.5806950957));
#64470=CARTESIAN_POINT('',(-6.53914701908,-37.2742356128,2.5806950957));
#64471=CARTESIAN_POINT('Ctrl Pts',(-6.2749628032,-36.2742356128,2.72284536858));
#64472=CARTESIAN_POINT('Ctrl Pts',(-6.35795872238,-36.2742356128,2.67818754328));
#64473=CARTESIAN_POINT('Ctrl Pts',(-6.44095464156,-36.3112466293,2.63352971798));
#64474=CARTESIAN_POINT('Ctrl Pts',(-6.50655459783,-36.3857400536,2.59823218268));
#64475=CARTESIAN_POINT('Ctrl Pts',(-6.53914701908,-36.4799878332,2.5806950957));
#64476=CARTESIAN_POINT('Ctrl Pts',(-6.53914701908,-36.5742356128,2.5806950957));
#64477=CARTESIAN_POINT('Ctrl Pts',(-6.20857721065,-36.2742356128,2.59946870979));
#64478=CARTESIAN_POINT('Ctrl Pts',(-6.29440217543,-36.2742356128,2.56006862461));
#64479=CARTESIAN_POINT('Ctrl Pts',(-6.3802271402,-36.3112466293,2.52066853944));
#64480=CARTESIAN_POINT('Ctrl Pts',(-6.44806317297,-36.3857400536,2.48952672142));
#64481=CARTESIAN_POINT('Ctrl Pts',(-6.48176655835,-36.4799878332,2.4740543435));
#64482=CARTESIAN_POINT('Ctrl Pts',(-6.48176655835,-36.5742356128,2.4740543435));
#64483=CARTESIAN_POINT('Ctrl Pts',(-6.15321817523,-36.2742356128,2.47317175996));
#64484=CARTESIAN_POINT('Ctrl Pts',(-6.24090872024,-36.2742356128,2.43823633957));
#64485=CARTESIAN_POINT('Ctrl Pts',(-6.32859926526,-36.3112466293,2.40330091918));
#64486=CARTESIAN_POINT('Ctrl Pts',(-6.39790985368,-36.3857400536,2.37568796974));
#64487=CARTESIAN_POINT('Ctrl Pts',(-6.43234584926,-36.4799878332,2.36196886307));
#64488=CARTESIAN_POINT('Ctrl Pts',(-6.43234584926,-36.5742356128,2.36196886307));
#64489=CARTESIAN_POINT('Ctrl Pts',(-6.10591213658,-36.2742356128,2.34560093633));
#64490=CARTESIAN_POINT('Ctrl Pts',(-6.19476895256,-36.2742356128,2.31400987032));
#64491=CARTESIAN_POINT('Ctrl Pts',(-6.28362576853,-36.3112466293,2.2824188043));
#64492=CARTESIAN_POINT('Ctrl Pts',(-6.35385817691,-36.3857400536,2.2574492336));
#64493=CARTESIAN_POINT('Ctrl Pts',(-6.38875216637,-36.4799878332,2.24504345006));
#64494=CARTESIAN_POINT('Ctrl Pts',(-6.38875216637,-36.5742356128,2.24504345006));
#64495=CARTESIAN_POINT('Ctrl Pts',(-6.04521899885,-36.2742356128,2.16171106337));
#64496=CARTESIAN_POINT('Ctrl Pts',(-6.13521792579,-36.2742356128,2.13366813026));
#64497=CARTESIAN_POINT('Ctrl Pts',(-6.22521685274,-36.3112466293,2.10562519715));
#64498=CARTESIAN_POINT('Ctrl Pts',(-6.29635198481,-36.3857400536,2.08346006881));
#64499=CARTESIAN_POINT('Ctrl Pts',(-6.33169448077,-36.4799878332,2.0724476349));
#64500=CARTESIAN_POINT('Ctrl Pts',(-6.33169448077,-36.5742356128,2.0724476349));
#64501=CARTESIAN_POINT('Ctrl Pts',(-5.99141530911,-36.2742356128,1.9788243735));
#64502=CARTESIAN_POINT('Ctrl Pts',(-6.0819421462,-36.2742356128,1.95259666444));
#64503=CARTESIAN_POINT('Ctrl Pts',(-6.17246898329,-36.3112466293,1.92636895538));
#64504=CARTESIAN_POINT('Ctrl Pts',(-6.2440213753,-36.3857400536,1.90563857988));
#64505=CARTESIAN_POINT('Ctrl Pts',(-6.27957118122,-36.4799878332,1.89533898265));
#64506=CARTESIAN_POINT('Ctrl Pts',(-6.27957118122,-36.5742356128,1.89533898265));
#64507=CARTESIAN_POINT('Ctrl Pts',(-5.97520112534,-36.2742356128,1.92228832367));
#64508=CARTESIAN_POINT('Ctrl Pts',(-6.06583420961,-36.2742356128,1.89643429474));
#64509=CARTESIAN_POINT('Ctrl Pts',(-6.15646729387,-36.3112466293,1.87058026582));
#64510=CARTESIAN_POINT('Ctrl Pts',(-6.2281036639,-36.3857400536,1.85014524757));
#64511=CARTESIAN_POINT('Ctrl Pts',(-6.26369519271,-36.4799878332,1.83999239363));
#64512=CARTESIAN_POINT('Ctrl Pts',(-6.26369519271,-36.5742356128,1.83999239363));
#64513=CARTESIAN_POINT('Ctrl Pts',(-5.9347525703,-36.2742356128,1.77898877676));
#64514=CARTESIAN_POINT('Ctrl Pts',(-6.02559800101,-36.2742356128,1.75388963588));
#64515=CARTESIAN_POINT('Ctrl Pts',(-6.11644343173,-36.3112466293,1.728790495));
#64516=CARTESIAN_POINT('Ctrl Pts',(-6.18824763999,-36.3857400536,1.70895213871));
#64517=CARTESIAN_POINT('Ctrl Pts',(-6.22392255742,-36.4799878332,1.69909572999));
#64518=CARTESIAN_POINT('Ctrl Pts',(-6.22392255742,-36.5742356128,1.69909572999));
#64519=CARTESIAN_POINT('Ctrl Pts',(-5.89729646051,-36.2742356128,1.64334906184));
#64520=CARTESIAN_POINT('Ctrl Pts',(-5.9880924731,-36.2742356128,1.61807905477));
#64521=CARTESIAN_POINT('Ctrl Pts',(-6.0788884857,-36.3112466293,1.5928090477));
#64522=CARTESIAN_POINT('Ctrl Pts',(-6.15065363436,-36.3857400536,1.57283564109));
#64523=CARTESIAN_POINT('Ctrl Pts',(-6.18630914486,-36.4799878332,1.5629121311));
#64524=CARTESIAN_POINT('Ctrl Pts',(-6.18630914486,-36.5742356128,1.5629121311));
#64525=CARTESIAN_POINT('Ctrl Pts',(-5.87402738023,-36.2742356128,1.56021991543));
#64526=CARTESIAN_POINT('Ctrl Pts',(-5.96471053981,-36.2742356128,1.53453784372));
#64527=CARTESIAN_POINT('Ctrl Pts',(-6.0553936994,-36.3112466293,1.508855772));
#64528=CARTESIAN_POINT('Ctrl Pts',(-6.12706965104,-36.3857400536,1.48855667603));
#64529=CARTESIAN_POINT('Ctrl Pts',(-6.16268084229,-36.4799878332,1.47847134219));
#64530=CARTESIAN_POINT('Ctrl Pts',(-6.16268084229,-36.5742356128,1.47847134219));
#64531=CARTESIAN_POINT('Ctrl Pts',(-5.82268928074,-36.2742356128,1.38179028229));
#64532=CARTESIAN_POINT('Ctrl Pts',(-5.91303885618,-36.2742356128,1.35492687511));
#64533=CARTESIAN_POINT('Ctrl Pts',(-6.00338843162,-36.3112466293,1.32806346794));
#64534=CARTESIAN_POINT('Ctrl Pts',(-6.07480071619,-36.3857400536,1.30683063676));
#64535=CARTESIAN_POINT('Ctrl Pts',(-6.11028091149,-36.4799878332,1.29628140149));
#64536=CARTESIAN_POINT('Ctrl Pts',(-6.11028091149,-36.5742356128,1.29628140149));
#64537=CARTESIAN_POINT('Ctrl Pts',(-5.76820785146,-36.2742356128,1.20835208937));
#64538=CARTESIAN_POINT('Ctrl Pts',(-5.85784448561,-36.2742356128,1.17919014597));
#64539=CARTESIAN_POINT('Ctrl Pts',(-5.94748111977,-36.3112466293,1.15002820258));
#64540=CARTESIAN_POINT('Ctrl Pts',(-6.01832989343,-36.3857400536,1.12697860118));
#64541=CARTESIAN_POINT('Ctrl Pts',(-6.05353011961,-36.4799878332,1.11552674054));
#64542=CARTESIAN_POINT('Ctrl Pts',(-6.05353011961,-36.5742356128,1.11552674054));
#64543=CARTESIAN_POINT('Ctrl Pts',(-5.73947450501,-36.2742356128,1.12179370849));
#64544=CARTESIAN_POINT('Ctrl Pts',(-5.82870044481,-36.2742356128,1.09138518818));
#64545=CARTESIAN_POINT('Ctrl Pts',(-5.91792638462,-36.3112466293,1.06097666786));
#64546=CARTESIAN_POINT('Ctrl Pts',(-5.9884505474,-36.3857400536,1.03694177877));
#64547=CARTESIAN_POINT('Ctrl Pts',(-6.02348949244,-36.4799878332,1.02500038208));
#64548=CARTESIAN_POINT('Ctrl Pts',(-6.02348949244,-36.5742356128,1.02500038208));
#64549=CARTESIAN_POINT('Ctrl Pts',(-5.6492991896,-36.2742356128,0.867227348791));
#64550=CARTESIAN_POINT('Ctrl Pts',(-5.73699523894,-36.2742356128,0.832468736018));
#64551=CARTESIAN_POINT('Ctrl Pts',(-5.82469128829,-36.3112466293,0.797710123244));
#64552=CARTESIAN_POINT('Ctrl Pts',(-5.89400622723,-36.3857400536,0.770236926332));
#64553=CARTESIAN_POINT('Ctrl Pts',(-5.92844438446,-36.4799878332,0.756587248033));
#64554=CARTESIAN_POINT('Ctrl Pts',(-5.92844438446,-36.5742356128,0.756587248033));
#64555=CARTESIAN_POINT('Ctrl Pts',(-5.54369220774,-36.2742356128,0.622753928119));
#64556=CARTESIAN_POINT('Ctrl Pts',(-5.62907055641,-36.2742356128,0.582523808606));
#64557=CARTESIAN_POINT('Ctrl Pts',(-5.71444890507,-36.3112466293,0.542293689093));
#64558=CARTESIAN_POINT('Ctrl Pts',(-5.78193193149,-36.3857400536,0.510495804805));
#64559=CARTESIAN_POINT('Ctrl Pts',(-5.8154599322,-36.4799878332,0.494697480486));
#64560=CARTESIAN_POINT('Ctrl Pts',(-5.8154599322,-36.5742356128,0.494697480486));
#64561=CARTESIAN_POINT('Ctrl Pts',(-5.46501384857,-36.2742356128,0.465072251063));
#64562=CARTESIAN_POINT('Ctrl Pts',(-5.54848443428,-36.2742356128,0.420970712728));
#64563=CARTESIAN_POINT('Ctrl Pts',(-5.63195502,-36.3112466293,0.376869174394));
#64564=CARTESIAN_POINT('Ctrl Pts',(-5.69793015283,-36.3857400536,0.342011328363));
#64565=CARTESIAN_POINT('Ctrl Pts',(-5.73070897496,-36.4799878332,0.324692694584));
#64566=CARTESIAN_POINT('Ctrl Pts',(-5.73070897496,-36.5742356128,0.324692694584));
#64567=CARTESIAN_POINT('Ctrl Pts',(-5.29016221704,-36.2742356128,0.160644480083));
#64568=CARTESIAN_POINT('Ctrl Pts',(-5.36921773106,-36.2742356128,0.108867903392));
#64569=CARTESIAN_POINT('Ctrl Pts',(-5.44827324508,-36.3112466293,0.0570913267005));
#64570=CARTESIAN_POINT('Ctrl Pts',(-5.51075870596,-36.3857400536,0.0161671319651));
#64571=CARTESIAN_POINT('Ctrl Pts',(-5.54180373374,-36.4799878332,-0.00416548225244));
#64572=CARTESIAN_POINT('Ctrl Pts',(-5.54180373374,-36.5742356128,-0.00416548225244));
#64573=CARTESIAN_POINT('Ctrl Pts',(-5.08056917549,-36.2742356128,-0.122448531423));
#64574=CARTESIAN_POINT('Ctrl Pts',(-5.15445489674,-36.2742356128,-0.181197969595));
#64575=CARTESIAN_POINT('Ctrl Pts',(-5.22834061799,-36.3112466293,-0.239947407767));
#64576=CARTESIAN_POINT('Ctrl Pts',(-5.28673987564,-36.3857400536,-0.286382951148));
#64577=CARTESIAN_POINT('Ctrl Pts',(-5.31575473071,-36.4799878332,-0.309453801202));
#64578=CARTESIAN_POINT('Ctrl Pts',(-5.31575473071,-36.5742356128,-0.309453801202));
#64579=CARTESIAN_POINT('Ctrl Pts',(-4.96743305836,-36.2742356128,-0.258380923711));
#64580=CARTESIAN_POINT('Ctrl Pts',(-5.03866455064,-36.2742356128,-0.320282770268));
#64581=CARTESIAN_POINT('Ctrl Pts',(-5.10989604293,-36.3112466293,-0.382184616825));
#64582=CARTESIAN_POINT('Ctrl Pts',(-5.1661974009,-36.3857400536,-0.431111821797));
#64583=CARTESIAN_POINT('Ctrl Pts',(-5.19416994037,-36.4799878332,-0.455420621033));
#64584=CARTESIAN_POINT('Ctrl Pts',(-5.19416994037,-36.5742356128,-0.455420621033));
#64585=CARTESIAN_POINT('Ctrl Pts',(-4.46114659269,-36.2742356128,-0.80567930031));
#64586=CARTESIAN_POINT('Ctrl Pts',(-4.52141506071,-36.2742356128,-0.879333647364));
#64587=CARTESIAN_POINT('Ctrl Pts',(-4.58168352872,-36.3112466293,-0.952987994419));
#64588=CARTESIAN_POINT('Ctrl Pts',(-4.62931970603,-36.3857400536,-1.0112043772));
#64589=CARTESIAN_POINT('Ctrl Pts',(-4.65298708463,-36.4799878332,-1.04012836859));
#64590=CARTESIAN_POINT('Ctrl Pts',(-4.65298708463,-36.5742356128,-1.04012836859));
#64591=CARTESIAN_POINT('Ctrl Pts',(-3.8375375961,-36.2742356128,-1.26315776015));
#64592=CARTESIAN_POINT('Ctrl Pts',(-3.88883264536,-36.2742356128,-1.34257410025));
#64593=CARTESIAN_POINT('Ctrl Pts',(-3.94012769463,-36.3112466293,-1.42199044035));
#64594=CARTESIAN_POINT('Ctrl Pts',(-3.98067131041,-36.3857400536,-1.48476108812));
#64595=CARTESIAN_POINT('Ctrl Pts',(-4.00081480904,-36.4799878332,-1.51594782192));
#64596=CARTESIAN_POINT('Ctrl Pts',(-4.00081480904,-36.5742356128,-1.51594782192));
#64597=CARTESIAN_POINT('Ctrl Pts',(-3.32820147129,-36.2742356128,-1.56569218035));
#64598=CARTESIAN_POINT('Ctrl Pts',(-3.37548175785,-36.2742356128,-1.64720794633));
#64599=CARTESIAN_POINT('Ctrl Pts',(-3.42276204441,-36.3112466293,-1.72872371231));
#64600=CARTESIAN_POINT('Ctrl Pts',(-3.46013228594,-36.3857400536,-1.79315379649));
#64601=CARTESIAN_POINT('Ctrl Pts',(-3.47869929762,-36.4799878332,-1.82516492226));
#64602=CARTESIAN_POINT('Ctrl Pts',(-3.47869929762,-36.5742356128,-1.82516492226));
#64603=CARTESIAN_POINT('Ctrl Pts',(-2.8169014355,-36.2742356128,-1.85179112224));
#64604=CARTESIAN_POINT('Ctrl Pts',(-2.8619505579,-36.2742356128,-1.93475206073));
#64605=CARTESIAN_POINT('Ctrl Pts',(-2.90699968031,-36.3112466293,-2.01771299922));
#64606=CARTESIAN_POINT('Ctrl Pts',(-2.94260655437,-36.3857400536,-2.08328527962));
#64607=CARTESIAN_POINT('Ctrl Pts',(-2.96029724575,-36.4799878332,-2.11586399113));
#64608=CARTESIAN_POINT('Ctrl Pts',(-2.96029724575,-36.5742356128,-2.11586399113));
#64609=CARTESIAN_POINT('Ctrl Pts',(-2.29653265536,-36.2742356128,-2.09683653367));
#64610=CARTESIAN_POINT('Ctrl Pts',(-2.33668543274,-36.2742356128,-2.18210316522));
#64611=CARTESIAN_POINT('Ctrl Pts',(-2.37683821013,-36.3112466293,-2.26736979677));
#64612=CARTESIAN_POINT('Ctrl Pts',(-2.40857495654,-36.3857400536,-2.3347645236));
#64613=CARTESIAN_POINT('Ctrl Pts',(-2.42434291535,-36.4799878332,-2.36824865151));
#64614=CARTESIAN_POINT('Ctrl Pts',(-2.42434291535,-36.5742356128,-2.36824865151));
#64615=CARTESIAN_POINT('',(-2.42434411094,-36.5742356128,-2.36824808793));
#64616=CARTESIAN_POINT('Origin',(-2.29743546385133,-36.5721143210983,-2.09875612122949));
#64617=CARTESIAN_POINT('Ctrl Pts',(-6.53914701908,-36.5742356128,2.5806950957));
#64618=CARTESIAN_POINT('Ctrl Pts',(-6.52032174685649,-36.5742356128,2.54570860091162));
#64619=CARTESIAN_POINT('Ctrl Pts',(-6.50258208588932,-36.5742356128,2.51012495658173));
#64620=CARTESIAN_POINT('Ctrl Pts',(-6.48575331803117,-36.5742356128,2.47402330026177));
#64621=CARTESIAN_POINT('Ctrl Pts',(-6.4630511932899,-36.5742356128,2.42532191510686));
#64622=CARTESIAN_POINT('Ctrl Pts',(-6.44200610676348,-36.5742356128,2.37568107869865));
#64623=CARTESIAN_POINT('Ctrl Pts',(-6.42224329823567,-36.5742356128,2.32538225843607));
#64624=CARTESIAN_POINT('Ctrl Pts',(-6.40593172984875,-36.5742356128,2.28386727612268));
#64625=CARTESIAN_POINT('Ctrl Pts',(-6.39049545136789,-36.5742356128,2.24190846192766));
#64626=CARTESIAN_POINT('Ctrl Pts',(-6.37573913119417,-36.5742356128,2.1996479726803));
#64627=CARTESIAN_POINT('Ctrl Pts',(-6.36347989451579,-36.5742356128,2.16453885782453));
#64628=CARTESIAN_POINT('Ctrl Pts',(-6.35169041632424,-36.5742356128,2.12922211872938));
#64629=CARTESIAN_POINT('Ctrl Pts',(-6.34025906051022,-36.5742356128,2.09374334947018));
#64630=CARTESIAN_POINT('Ctrl Pts',(-6.33082632142642,-36.5742356128,2.06446755936433));
#64631=CARTESIAN_POINT('Ctrl Pts',(-6.32163750734452,-36.5742356128,2.03508116248095));
#64632=CARTESIAN_POINT('Ctrl Pts',(-6.31262755192929,-36.5742356128,2.00558278534094));
#64633=CARTESIAN_POINT('Ctrl Pts',(-6.30858018488047,-36.5742356128,1.99233180305214));
#64634=CARTESIAN_POINT('Ctrl Pts',(-6.30456863126258,-36.5742356128,1.97905704388498));
#64635=CARTESIAN_POINT('Ctrl Pts',(-6.3005918933596,-36.5742356128,1.96577575871319));
#64636=CARTESIAN_POINT('Ctrl Pts',(-6.29838938787337,-36.5742356128,1.95841995499448));
#64637=CARTESIAN_POINT('Ctrl Pts',(-6.29619809600555,-36.5742356128,1.95106389512971));
#64638=CARTESIAN_POINT('Ctrl Pts',(-6.29402063675644,-36.5742356128,1.94371992905133));
#64639=CARTESIAN_POINT('Ctrl Pts',(-6.28642198061935,-36.5742356128,1.91809176956468));
#64640=CARTESIAN_POINT('Ctrl Pts',(-6.27898255033723,-36.5742356128,1.89258187965036));
#64641=CARTESIAN_POINT('Ctrl Pts',(-6.27170351106231,-36.5742356128,1.86733365133418));
#64642=CARTESIAN_POINT('Ctrl Pts',(-6.26599905047914,-36.5742356128,1.84754703969699));
#64643=CARTESIAN_POINT('Ctrl Pts',(-6.26039372562493,-36.5742356128,1.82792283460782));
#64644=CARTESIAN_POINT('Ctrl Pts',(-6.25488121131594,-36.5742356128,1.80849670939161));
#64645=CARTESIAN_POINT('Ctrl Pts',(-6.2500278231648,-36.5742356128,1.79139334771996));
#64646=CARTESIAN_POINT('Ctrl Pts',(-6.24524653645831,-36.5742356128,1.77444394963674));
#64647=CARTESIAN_POINT('Ctrl Pts',(-6.24052289064231,-36.5742356128,1.75763262190247));
#64648=CARTESIAN_POINT('Ctrl Pts',(-6.23822440223965,-36.5742356128,1.74945236382733));
#64649=CARTESIAN_POINT('Ctrl Pts',(-6.23593938575314,-36.5742356128,1.74130411709365));
#64650=CARTESIAN_POINT('Ctrl Pts',(-6.23366500246872,-36.5742356128,1.73318159032846));
#64651=CARTESIAN_POINT('Ctrl Pts',(-6.22636543920889,-36.5742356128,1.7071125902799));
#64652=CARTESIAN_POINT('Ctrl Pts',(-6.21917568075214,-36.5742356128,1.68131097734659));
#64653=CARTESIAN_POINT('Ctrl Pts',(-6.21200825626089,-36.5742356128,1.6555906033367));
#64654=CARTESIAN_POINT('Ctrl Pts',(-6.20391515965567,-36.5742356128,1.62654844574745));
#64655=CARTESIAN_POINT('Ctrl Pts',(-6.19584885745646,-36.5742356128,1.5976035761512));
#64656=CARTESIAN_POINT('Ctrl Pts',(-6.18768109822354,-36.5742356128,1.56845713212407));
#64657=CARTESIAN_POINT('Ctrl Pts',(-6.18155527879886,-36.5742356128,1.54659729910371));
#64658=CARTESIAN_POINT('Ctrl Pts',(-6.17537213047874,-36.5742356128,1.52462259154949));
#64659=CARTESIAN_POINT('Ctrl Pts',(-6.16908668276109,-36.5742356128,1.50243475193452));
#64660=CARTESIAN_POINT('Ctrl Pts',(-6.16347986492664,-36.5742356128,1.48264249839117));
#64661=CARTESIAN_POINT('Ctrl Pts',(-6.15779151472513,-36.5742356128,1.46268004755247));
#64662=CARTESIAN_POINT('Ctrl Pts',(-6.15200028273329,-36.5742356128,1.4425146091755));
#64663=CARTESIAN_POINT('Ctrl Pts',(-6.14655542305962,-36.5742356128,1.42355526125516));
#64664=CARTESIAN_POINT('Ctrl Pts',(-6.14101948977268,-36.5742356128,1.40441593963609));
#64665=CARTESIAN_POINT('Ctrl Pts',(-6.13538648341178,-36.5742356128,1.38511197583127));
#64666=CARTESIAN_POINT('Ctrl Pts',(-6.13112388099663,-36.5742356128,1.37050430144494));
#64667=CARTESIAN_POINT('Ctrl Pts',(-6.12680589496271,-36.5742356128,1.35580307774514));
#64668=CARTESIAN_POINT('Ctrl Pts',(-6.12243557585458,-36.5742356128,1.34103577276729));
#64669=CARTESIAN_POINT('Ctrl Pts',(-6.11956939397697,-36.5742356128,1.33135094635955));
#64670=CARTESIAN_POINT('Ctrl Pts',(-6.11668080562675,-36.5742356128,1.32163807644753));
#64671=CARTESIAN_POINT('Ctrl Pts',(-6.11377204094819,-36.5742356128,1.31191000022643));
#64672=CARTESIAN_POINT('Ctrl Pts',(-6.112245556784,-36.5742356128,1.30680482468269));
#64673=CARTESIAN_POINT('Ctrl Pts',(-6.11071368512088,-36.5742356128,1.30169604289404));
#64674=CARTESIAN_POINT('Ctrl Pts',(-6.10917821149739,-36.5742356128,1.29659039499181));
#64675=CARTESIAN_POINT('Ctrl Pts',(-6.09951672157609,-36.5742356128,1.26446469449489));
#64676=CARTESIAN_POINT('Ctrl Pts',(-6.08969773032946,-36.5742356128,1.23241427306604));
#64677=CARTESIAN_POINT('Ctrl Pts',(-6.0796753566568,-36.5742356128,1.20041384530431));
#64678=CARTESIAN_POINT('Ctrl Pts',(-6.06788110894677,-36.5742356128,1.16275600254416));
#64679=CARTESIAN_POINT('Ctrl Pts',(-6.05580535299258,-36.5742356128,1.12516843034084));
#64680=CARTESIAN_POINT('Ctrl Pts',(-6.043399902687,-36.5742356128,1.08767767748112));
#64681=CARTESIAN_POINT('Ctrl Pts',(-6.02909273273903,-36.5742356128,1.04443970067024));
#64682=CARTESIAN_POINT('Ctrl Pts',(-6.01434819002561,-36.5742356128,1.00133527281449));
#64683=CARTESIAN_POINT('Ctrl Pts',(-5.99911484370015,-36.5742356128,0.958441660976139));
#64684=CARTESIAN_POINT('Ctrl Pts',(-5.98578029087872,-36.5742356128,0.920894616450256));
#64685=CARTESIAN_POINT('Ctrl Pts',(-5.97207239113828,-36.5742356128,0.883512523022658));
#64686=CARTESIAN_POINT('Ctrl Pts',(-5.9579543699754,-36.5742356128,0.846312852561985));
#64687=CARTESIAN_POINT('Ctrl Pts',(-5.93414560884613,-36.5742356128,0.783578985126351));
#64688=CARTESIAN_POINT('Ctrl Pts',(-5.9091635512488,-36.5742356128,0.721350159380157));
#64689=CARTESIAN_POINT('Ctrl Pts',(-5.8828848071143,-36.5742356128,0.65973995614056));
#64690=CARTESIAN_POINT('Ctrl Pts',(-5.85568555938991,-36.5742356128,0.595971643176817));
#64691=CARTESIAN_POINT('Ctrl Pts',(-5.82709727613897,-36.5742356128,0.532866069549744));
#64692=CARTESIAN_POINT('Ctrl Pts',(-5.79703519303637,-36.5742356128,0.470527628371927));
#64693=CARTESIAN_POINT('Ctrl Pts',(-5.76636583046652,-36.5742356128,0.40692989803514));
#64694=CARTESIAN_POINT('Ctrl Pts',(-5.73416273827395,-36.5742356128,0.344130578955812));
#64695=CARTESIAN_POINT('Ctrl Pts',(-5.70038666343235,-36.5742356128,0.282218621126629));
#64696=CARTESIAN_POINT('Ctrl Pts',(-5.66556277133928,-36.5742356128,0.218386001474261));
#64697=CARTESIAN_POINT('Ctrl Pts',(-5.62906692815191,-36.5742356128,0.155496671561614));
#64698=CARTESIAN_POINT('Ctrl Pts',(-5.59090689045679,-36.5742356128,0.0936250953297072));
#64699=CARTESIAN_POINT('Ctrl Pts',(-5.57176245947455,-36.5742356128,0.0625848712503234));
#64700=CARTESIAN_POINT('Ctrl Pts',(-5.55219993689747,-36.5742356128,0.031800449018197));
#64701=CARTESIAN_POINT('Ctrl Pts',(-5.53222471364869,-36.5742356128,0.0012791285066921));
#64702=CARTESIAN_POINT('Ctrl Pts',(-5.48858293589753,-36.5742356128,-0.0654037150263174));
#64703=CARTESIAN_POINT('Ctrl Pts',(-5.44296905804018,-36.5742356128,-0.130827416139679));
#64704=CARTESIAN_POINT('Ctrl Pts',(-5.39547709946709,-36.5742356128,-0.194942398547811));
#64705=CARTESIAN_POINT('Ctrl Pts',(-5.34538435552397,-36.5742356128,-0.262568487114894));
#64706=CARTESIAN_POINT('Ctrl Pts',(-5.29320246599191,-36.5742356128,-0.328739090927756));
#64707=CARTESIAN_POINT('Ctrl Pts',(-5.23908298414192,-36.5742356128,-0.393442819708286));
#64708=CARTESIAN_POINT('Ctrl Pts',(-5.17794521020509,-36.5742356128,-0.46653742090972));
#64709=CARTESIAN_POINT('Ctrl Pts',(-5.11433476327847,-36.5742356128,-0.537760505216273));
#64710=CARTESIAN_POINT('Ctrl Pts',(-5.04851964288569,-36.5742356128,-0.607146788830764));
#64711=CARTESIAN_POINT('Ctrl Pts',(-5.00958808586998,-36.5742356128,-0.648190792708977));
#64712=CARTESIAN_POINT('Ctrl Pts',(-4.96988601884903,-36.5742356128,-0.688593005831337));
#64713=CARTESIAN_POINT('Ctrl Pts',(-4.92947512198836,-36.5742356128,-0.728365937491898));
#64714=CARTESIAN_POINT('Ctrl Pts',(-4.86990495862107,-36.5742356128,-0.786995669090893));
#64715=CARTESIAN_POINT('Ctrl Pts',(-4.80879601831302,-36.5742356128,-0.844256936244762));
#64716=CARTESIAN_POINT('Ctrl Pts',(-4.74633115403261,-36.5742356128,-0.900225234060358));
#64717=CARTESIAN_POINT('Ctrl Pts',(-4.69540993206243,-36.5742356128,-0.945850469129586));
#64718=CARTESIAN_POINT('Ctrl Pts',(-4.6435838315632,-36.5742356128,-0.990619526802198));
#64719=CARTESIAN_POINT('Ctrl Pts',(-4.59098076191512,-36.5742356128,-1.03455313729565));
#64720=CARTESIAN_POINT('Ctrl Pts',(-4.5059924451459,-36.5742356128,-1.10553461481043));
#64721=CARTESIAN_POINT('Ctrl Pts',(-4.41897174588524,-36.5742356128,-1.17433980339564));
#64722=CARTESIAN_POINT('Ctrl Pts',(-4.33038782770431,-36.5742356128,-1.24113580021237));
#64723=CARTESIAN_POINT('Ctrl Pts',(-4.24567268322767,-36.5742356128,-1.30501457908094));
#64724=CARTESIAN_POINT('Ctrl Pts',(-4.15952863925796,-36.5742356128,-1.36705753414624));
#64725=CARTESIAN_POINT('Ctrl Pts',(-4.0723260509289,-36.5742356128,-1.42743079196531));
#64726=CARTESIAN_POINT('Ctrl Pts',(-3.99046174632389,-36.5742356128,-1.4841081780705));
#64727=CARTESIAN_POINT('Ctrl Pts',(-3.9076648219601,-36.5742356128,-1.53931520624295));
#64728=CARTESIAN_POINT('Ctrl Pts',(-3.82419873102831,-36.5742356128,-1.59318740760338));
#64729=CARTESIAN_POINT('Ctrl Pts',(-3.74518523665179,-36.5742356128,-1.64418573317157));
#64730=CARTESIAN_POINT('Ctrl Pts',(-3.66557219084631,-36.5742356128,-1.693988594353));
#64731=CARTESIAN_POINT('Ctrl Pts',(-3.58554050425563,-36.5742356128,-1.74269603728047));
#64732=CARTESIAN_POINT('Ctrl Pts',(-3.50892602437149,-36.5742356128,-1.78932376144004));
#64733=CARTESIAN_POINT('Ctrl Pts',(-3.43192795463034,-36.5742356128,-1.83494812133376));
#64734=CARTESIAN_POINT('Ctrl Pts',(-3.35466350954136,-36.5742356128,-1.87963404280889));
#64735=CARTESIAN_POINT('Ctrl Pts',(-3.27816415521591,-36.5742356128,-1.92387747374725));
#64736=CARTESIAN_POINT('Ctrl Pts',(-3.20140389346523,-36.5742356128,-1.96720148429358));
#64737=CARTESIAN_POINT('Ctrl Pts',(-3.1244525163683,-36.5742356128,-2.0096384987399));
#64738=CARTESIAN_POINT('Ctrl Pts',(-3.0852866454685,-36.5742356128,-2.03123762655128));
#64739=CARTESIAN_POINT('Ctrl Pts',(-3.04607053863626,-36.5742356128,-2.05260643753161));
#64740=CARTESIAN_POINT('Ctrl Pts',(-3.00680870232973,-36.5742356128,-2.07374547713585));
#64741=CARTESIAN_POINT('Ctrl Pts',(-2.988900471926,-36.5742356128,-2.08338748136588));
#64742=CARTESIAN_POINT('Ctrl Pts',(-2.97097518539882,-36.5742356128,-2.09298568668701));
#64743=CARTESIAN_POINT('Ctrl Pts',(-2.95303040996166,-36.5742356128,-2.1025412036186));
#64744=CARTESIAN_POINT('Ctrl Pts',(-2.88078777831576,-36.5742356128,-2.14101009905238));
#64745=CARTESIAN_POINT('Ctrl Pts',(-2.80824941916113,-36.5742356128,-2.17878051698545));
#64746=CARTESIAN_POINT('Ctrl Pts',(-2.73544576469779,-36.5742356128,-2.21579026646871));
#64747=CARTESIAN_POINT('Ctrl Pts',(-2.66430005808082,-36.5742356128,-2.25195719789698));
#64748=CARTESIAN_POINT('Ctrl Pts',(-2.59290098389418,-36.5742356128,-2.28739789677643));
#64749=CARTESIAN_POINT('Ctrl Pts',(-2.52123973657706,-36.5742356128,-2.32202099352562));
#64750=CARTESIAN_POINT('Ctrl Pts',(-2.48899587984796,-36.5742356128,-2.33759959720465));
#64751=CARTESIAN_POINT('Ctrl Pts',(-2.45669843912861,-36.5742356128,-2.35301220297855));
#64752=CARTESIAN_POINT('Ctrl Pts',(-2.42434411115899,-36.5742356128,-2.36824808839505));
#64753=CARTESIAN_POINT('Ctrl Pts',(-2.42434398441,-37.9742356128,-2.3682481465));
#64754=CARTESIAN_POINT('Ctrl Pts',(-2.42434398591,-38.0684833924,-2.36824814579));
#64755=CARTESIAN_POINT('Ctrl Pts',(-2.40857608072,-38.1627311721,-2.33476399274));
#64756=CARTESIAN_POINT('Ctrl Pts',(-2.37683944038,-38.2372245963,-2.26736921615));
#64757=CARTESIAN_POINT('Ctrl Pts',(-2.33668679631,-38.2742356128,-2.18210252207));
#64758=CARTESIAN_POINT('Ctrl Pts',(-2.29653415164,-38.2742356128,-2.09683582826));
#64759=CARTESIAN_POINT('Ctrl Pts',(-3.10523376345,-37.9742356128,-2.04761278031));
#64760=CARTESIAN_POINT('Ctrl Pts',(-3.10523328188,-38.0684833917,-2.04761300582));
#64761=CARTESIAN_POINT('Ctrl Pts',(-3.087034044,-38.1627311705,-2.01527377228));
#64762=CARTESIAN_POINT('Ctrl Pts',(-3.05040417654,-38.2372245945,-1.9501832279));
#64763=CARTESIAN_POINT('Ctrl Pts',(-3.00406107947,-38.2742356116,-1.86783163316));
#64764=CARTESIAN_POINT('Ctrl Pts',(-2.95771817057,-38.2742356128,-1.78547994979));
#64765=CARTESIAN_POINT('Ctrl Pts',(-3.75558799721,-37.9742356128,-1.66539056819));
#64766=CARTESIAN_POINT('Ctrl Pts',(-3.75558871127,-38.0684833959,-1.66539023156));
#64767=CARTESIAN_POINT('Ctrl Pts',(-3.73654782615,-38.162731179,-1.63381112995));
#64768=CARTESIAN_POINT('Ctrl Pts',(-3.69822294792,-38.2372246046,-1.5702509984));
#64769=CARTESIAN_POINT('Ctrl Pts',(-3.6497344282,-38.2742356183,-1.48983609251));
#64770=CARTESIAN_POINT('Ctrl Pts',(-3.6012456292,-38.2742356128,-1.409421321));
#64771=CARTESIAN_POINT('Ctrl Pts',(-4.42784969665,-37.9742356128,-1.26351165773));
#64772=CARTESIAN_POINT('Ctrl Pts',(-4.42784946111,-38.0684834383,-1.26351181731));
#64773=CARTESIAN_POINT('Ctrl Pts',(-4.40636826728,-38.1627312638,-1.23261755234));
#64774=CARTESIAN_POINT('Ctrl Pts',(-4.36313251053,-38.2372247045,-1.17043536123));
#64775=CARTESIAN_POINT('Ctrl Pts',(-4.30843157333,-38.2742356849,-1.09176343887));
#64776=CARTESIAN_POINT('Ctrl Pts',(-4.2537307561,-38.2742356128,-1.01309146202));
#64777=CARTESIAN_POINT('Ctrl Pts',(-5.17355249507,-37.9742356128,-0.596349454932));
#64778=CARTESIAN_POINT('Ctrl Pts',(-5.17355255747,-38.0684833803,-0.596349412654));
#64779=CARTESIAN_POINT('Ctrl Pts',(-5.14592211519,-38.1627311477,-0.570516664483));
#64780=CARTESIAN_POINT('Ctrl Pts',(-5.09030925685,-38.2372245677,-0.51852219394));
#64781=CARTESIAN_POINT('Ctrl Pts',(-5.01994878926,-38.2742355937,-0.452739724933));
#64782=CARTESIAN_POINT('Ctrl Pts',(-4.94958828989,-38.2742356128,-0.386957270362));
#64783=CARTESIAN_POINT('Ctrl Pts',(-5.68047245792,-37.9742356128,0.230713175531));
#64784=CARTESIAN_POINT('Ctrl Pts',(-5.68047244139,-38.0684833957,0.23071316433));
#64785=CARTESIAN_POINT('Ctrl Pts',(-5.64814706462,-38.1627311785,0.248875697229));
#64786=CARTESIAN_POINT('Ctrl Pts',(-5.58308461353,-38.2372246039,0.285432101802));
#64787=CARTESIAN_POINT('Ctrl Pts',(-5.50076875003,-38.2742356179,0.331682633922));
#64788=CARTESIAN_POINT('Ctrl Pts',(-5.41845289496,-38.2742356128,0.377933169868));
#64789=CARTESIAN_POINT('Ctrl Pts',(-5.77561843229,-37.9742356128,0.410354854144));
#64790=CARTESIAN_POINT('Ctrl Pts',(-5.77561842674,-38.0684833594,0.410354840082));
#64791=CARTESIAN_POINT('Ctrl Pts',(-5.74243084804,-38.1627311059,0.426883018809));
#64792=CARTESIAN_POINT('Ctrl Pts',(-5.67563300366,-38.2372245184,0.460149908026));
#64793=CARTESIAN_POINT('Ctrl Pts',(-5.59112152855,-38.2742355609,0.50223860778));
#64794=CARTESIAN_POINT('Ctrl Pts',(-5.50661003688,-38.2742356128,0.544327321176));
#64795=CARTESIAN_POINT('Ctrl Pts',(-5.90159361138,-37.9742356128,0.688319077788));
#64796=CARTESIAN_POINT('Ctrl Pts',(-5.90159361416,-38.0684834091,0.688319084849));
#64797=CARTESIAN_POINT('Ctrl Pts',(-5.86735372253,-38.1627312053,0.702481569163));
#64798=CARTESIAN_POINT('Ctrl Pts',(-5.79843783889,-38.2372246355,0.730986909385));
#64799=CARTESIAN_POINT('Ctrl Pts',(-5.71124667074,-38.2742356389,0.767051361344));
#64800=CARTESIAN_POINT('Ctrl Pts',(-5.6240555109,-38.2742356128,0.803115806453));
#64801=CARTESIAN_POINT('Ctrl Pts',(-6.00622257558,-37.9742356128,0.974515968157));
#64802=CARTESIAN_POINT('Ctrl Pts',(-6.00622257418,-38.0684833841,0.974515964611));
#64803=CARTESIAN_POINT('Ctrl Pts',(-5.97128603775,-38.1627311554,0.986759517919));
#64804=CARTESIAN_POINT('Ctrl Pts',(-5.90096799706,-38.2372245767,1.01140256866));
#64805=CARTESIAN_POINT('Ctrl Pts',(-5.81200283764,-38.2742355997,1.04258052978));
#64806=CARTESIAN_POINT('Ctrl Pts',(-5.72303767403,-38.2742356128,1.07375849433));
#64807=CARTESIAN_POINT('Ctrl Pts',(-6.03928188172,-37.9742356128,1.07177315099));
#64808=CARTESIAN_POINT('Ctrl Pts',(-6.03928188245,-38.0684833854,1.07177315347));
#64809=CARTESIAN_POINT('Ctrl Pts',(-6.00415419262,-38.162731158,1.08344922785));
#64810=CARTESIAN_POINT('Ctrl Pts',(-5.93345140837,-38.2372245797,1.1069500878));
#64811=CARTESIAN_POINT('Ctrl Pts',(-5.84399947699,-38.2742356018,1.13668296404));
#64812=CARTESIAN_POINT('Ctrl Pts',(-5.75454754116,-38.2742356128,1.16641584059));
#64813=CARTESIAN_POINT('Ctrl Pts',(-6.11490875363,-37.9742356128,1.3080717033));
#64814=CARTESIAN_POINT('Ctrl Pts',(-6.11490875256,-38.0684834027,1.30807169968));
#64815=CARTESIAN_POINT('Ctrl Pts',(-6.07939173589,-38.1627311927,1.31851561198));
#64816=CARTESIAN_POINT('Ctrl Pts',(-6.00790534004,-38.2372246206,1.33953645854));
#64817=CARTESIAN_POINT('Ctrl Pts',(-5.91746200522,-38.274235629,1.36613166813));
#64818=CARTESIAN_POINT('Ctrl Pts',(-5.82701867689,-38.2742356128,1.39272687728));
#64819=CARTESIAN_POINT('Ctrl Pts',(-6.18342174186,-37.9742356128,1.55058013554));
#64820=CARTESIAN_POINT('Ctrl Pts',(-6.18342174342,-38.0684833774,1.55058014082));
#64821=CARTESIAN_POINT('Ctrl Pts',(-6.14774991166,-38.162731142,1.56044830715));
#64822=CARTESIAN_POINT('Ctrl Pts',(-6.07595191287,-38.2372245609,1.58031032001));
#64823=CARTESIAN_POINT('Ctrl Pts',(-5.9851143313,-38.2742355892,1.60543939017));
#64824=CARTESIAN_POINT('Ctrl Pts',(-5.89427674024,-38.2742356128,1.63056846098));
#64825=CARTESIAN_POINT('Ctrl Pts',(-6.21567787488,-37.9742356128,1.6694593188));
#64826=CARTESIAN_POINT('Ctrl Pts',(-6.21567765711,-38.0684833891,1.66945891565));
#64827=CARTESIAN_POINT('Ctrl Pts',(-6.17998213943,-38.1627311653,1.67922401337));
#64828=CARTESIAN_POINT('Ctrl Pts',(-6.1081367461,-38.2372245883,1.69887910028));
#64829=CARTESIAN_POINT('Ctrl Pts',(-6.01723933466,-38.2742356075,1.72374660724));
#64830=CARTESIAN_POINT('Ctrl Pts',(-5.92634200668,-38.2742356128,1.74861427291));
#64831=CARTESIAN_POINT('Ctrl Pts',(-6.29122760158,-37.9742356128,1.9445646743));
#64832=CARTESIAN_POINT('Ctrl Pts',(-6.29122780783,-38.0684833957,1.94456505612));
#64833=CARTESIAN_POINT('Ctrl Pts',(-6.25561493004,-38.1627311785,1.95469580701));
#64834=CARTESIAN_POINT('Ctrl Pts',(-6.18393533208,-38.2372246039,1.97508586283));
#64835=CARTESIAN_POINT('Ctrl Pts',(-6.09324743523,-38.2742356179,2.00088277762));
#64836=CARTESIAN_POINT('Ctrl Pts',(-6.00255945933,-38.2742356128,2.02667954206));
#64837=CARTESIAN_POINT('Ctrl Pts',(-6.37726427032,-37.9742356128,2.21399278029));
#64838=CARTESIAN_POINT('Ctrl Pts',(-6.37726407498,-38.0684833894,2.21399241868));
#64839=CARTESIAN_POINT('Ctrl Pts',(-6.34224466402,-38.162731166,2.22603592739));
#64840=CARTESIAN_POINT('Ctrl Pts',(-6.27176005687,-38.2372245892,2.25027677467));
#64841=CARTESIAN_POINT('Ctrl Pts',(-6.18258427948,-38.2742356081,2.28094609277));
#64842=CARTESIAN_POINT('Ctrl Pts',(-6.09340857698,-38.2742356128,2.31161555329));
#64843=CARTESIAN_POINT('Ctrl Pts',(-6.42332792062,-37.9742356128,2.34131663126));
#64844=CARTESIAN_POINT('Ctrl Pts',(-6.42332843985,-38.0684833825,2.34131759612));
#64845=CARTESIAN_POINT('Ctrl Pts',(-6.38877124366,-38.1627311522,2.35472949107));
#64846=CARTESIAN_POINT('Ctrl Pts',(-6.31921605307,-38.237224573,2.38172288062));
#64847=CARTESIAN_POINT('Ctrl Pts',(-6.2312157327,-38.2742355973,2.41587387978));
#64848=CARTESIAN_POINT('Ctrl Pts',(-6.14321520267,-38.2742356128,2.45002450227));
#64849=CARTESIAN_POINT('Ctrl Pts',(-6.47655499797,-37.9742356128,2.4643687343));
#64850=CARTESIAN_POINT('Ctrl Pts',(-6.47655499797,-38.0684833924,2.4643687343));
#64851=CARTESIAN_POINT('Ctrl Pts',(-6.44275070506,-38.1627311721,2.47965357706));
#64852=CARTESIAN_POINT('Ctrl Pts',(-6.37471158618,-38.2372245963,2.51041796246));
#64853=CARTESIAN_POINT('Ctrl Pts',(-6.28862967417,-38.2742356128,2.54934051494));
#64854=CARTESIAN_POINT('Ctrl Pts',(-6.20254776231,-38.2742356128,2.5882630677));
#64855=CARTESIAN_POINT('Ctrl Pts',(-6.53914701908,-37.9742356128,2.5806950957));
#64856=CARTESIAN_POINT('Ctrl Pts',(-6.53914701908,-38.0684833924,2.5806950957));
#64857=CARTESIAN_POINT('Ctrl Pts',(-6.50655459783,-38.1627311721,2.59823218268));
#64858=CARTESIAN_POINT('Ctrl Pts',(-6.44095464156,-38.2372245963,2.63352971798));
#64859=CARTESIAN_POINT('Ctrl Pts',(-6.35795872238,-38.2742356128,2.67818754328));
#64860=CARTESIAN_POINT('Ctrl Pts',(-6.2749628032,-38.2742356128,2.72284536858));
#64861=CARTESIAN_POINT('',(-2.42434411094,-37.9742356128,-2.36824808793));
#64862=CARTESIAN_POINT('Ctrl Pts',(-6.53914701908,-37.9742356128,2.5806950957));
#64863=CARTESIAN_POINT('Ctrl Pts',(-6.47656235486,-37.9742356128,2.46438240697));
#64864=CARTESIAN_POINT('Ctrl Pts',(-6.42402346497,-37.9742356128,2.34266436496));
#64865=CARTESIAN_POINT('Ctrl Pts',(-6.3783983006,-37.9742356128,2.21678838042));
#64866=CARTESIAN_POINT('Ctrl Pts',(-6.29416488484,-37.9742356128,1.9543061278));
#64867=CARTESIAN_POINT('Ctrl Pts',(-6.22058475422,-37.9742356128,1.68729407213));
#64868=CARTESIAN_POINT('Ctrl Pts',(-6.19138019874,-37.9742356128,1.57972238661));
#64869=CARTESIAN_POINT('Ctrl Pts',(-6.00694923806,-37.9742356128,0.922077056884));
#64870=CARTESIAN_POINT('Ctrl Pts',(-5.76642241656,-37.9742356128,0.278662479729));
#64871=CARTESIAN_POINT('Ctrl Pts',(-5.47236260901,-37.9742356128,-0.180892800215));
#64872=CARTESIAN_POINT('Ctrl Pts',(-4.83098837638,-37.9742356128,-0.890342468217));
#64873=CARTESIAN_POINT('Ctrl Pts',(-4.05512009519,-37.9742356128,-1.45762154474));
#64874=CARTESIAN_POINT('Ctrl Pts',(-3.70906725492,-37.9742356128,-1.67871445411));
#64875=CARTESIAN_POINT('Ctrl Pts',(-3.24315352431,-37.9742356128,-1.95213056689));
#64876=CARTESIAN_POINT('Ctrl Pts',(-2.77407974243,-37.9742356128,-2.19713947482));
#64877=CARTESIAN_POINT('Ctrl Pts',(-2.65752099961,-37.9742356128,-2.2562168661));
#64878=CARTESIAN_POINT('Ctrl Pts',(-2.54136162566,-37.9742356128,-2.31314371737));
#64879=CARTESIAN_POINT('Ctrl Pts',(-2.42434411094,-37.9742356128,-2.36824808793));
#64880=CARTESIAN_POINT('Origin',(-2.29743788266369,-37.9763569026624,-2.09875497968932));
#64881=CARTESIAN_POINT('Ctrl Pts',(-6.53914701908,-37.9742356128,2.5806950957));
#64882=CARTESIAN_POINT('Ctrl Pts',(-6.53914701908,-36.2942356128,2.5806950957));
#64883=CARTESIAN_POINT('Ctrl Pts',(-6.47656235486,-37.9742356128,2.46438240697));
#64884=CARTESIAN_POINT('Ctrl Pts',(-6.47656235486,-36.2942356128,2.46438240697));
#64885=CARTESIAN_POINT('Ctrl Pts',(-6.42402346497,-37.9742356128,2.34266436496));
#64886=CARTESIAN_POINT('Ctrl Pts',(-6.42402346497,-36.2942356128,2.34266436496));
#64887=CARTESIAN_POINT('Ctrl Pts',(-6.3783983006,-37.9742356128,2.21678838042));
#64888=CARTESIAN_POINT('Ctrl Pts',(-6.3783983006,-36.2942356128,2.21678838042));
#64889=CARTESIAN_POINT('Ctrl Pts',(-6.29416488484,-37.9742356128,1.9543061278));
#64890=CARTESIAN_POINT('Ctrl Pts',(-6.29416488484,-36.2942356128,1.9543061278));
#64891=CARTESIAN_POINT('Ctrl Pts',(-6.22058475422,-37.9742356128,1.68729407213));
#64892=CARTESIAN_POINT('Ctrl Pts',(-6.22058475422,-36.2942356128,1.68729407213));
#64893=CARTESIAN_POINT('Ctrl Pts',(-6.19138019874,-37.9742356128,1.57972238661));
#64894=CARTESIAN_POINT('Ctrl Pts',(-6.19138019874,-36.2942356128,1.57972238661));
#64895=CARTESIAN_POINT('Ctrl Pts',(-6.00694923806,-37.9742356128,0.922077056884));
#64896=CARTESIAN_POINT('Ctrl Pts',(-6.00694923806,-36.2942356128,0.922077056884));
#64897=CARTESIAN_POINT('Ctrl Pts',(-5.76642241656,-37.9742356128,0.278662479729));
#64898=CARTESIAN_POINT('Ctrl Pts',(-5.76642241656,-36.2942356128,0.278662479729));
#64899=CARTESIAN_POINT('Ctrl Pts',(-5.47236260901,-37.9742356128,-0.180892800215));
#64900=CARTESIAN_POINT('Ctrl Pts',(-5.47236260901,-36.2942356128,-0.180892800215));
#64901=CARTESIAN_POINT('Ctrl Pts',(-4.83098837638,-37.9742356128,-0.890342468217));
#64902=CARTESIAN_POINT('Ctrl Pts',(-4.83098837638,-36.2942356128,-0.890342468217));
#64903=CARTESIAN_POINT('Ctrl Pts',(-4.05512009519,-37.9742356128,-1.45762154474));
#64904=CARTESIAN_POINT('Ctrl Pts',(-4.05512009519,-36.2942356128,-1.45762154474));
#64905=CARTESIAN_POINT('Ctrl Pts',(-3.70906725492,-37.9742356128,-1.67871445411));
#64906=CARTESIAN_POINT('Ctrl Pts',(-3.70906725492,-36.2942356128,-1.67871445411));
#64907=CARTESIAN_POINT('Ctrl Pts',(-3.24315352431,-37.9742356128,-1.95213056689));
#64908=CARTESIAN_POINT('Ctrl Pts',(-3.24315352431,-36.2942356128,-1.95213056689));
#64909=CARTESIAN_POINT('Ctrl Pts',(-2.77407974243,-37.9742356128,-2.19713947482));
#64910=CARTESIAN_POINT('Ctrl Pts',(-2.77407974243,-36.2942356128,-2.19713947482));
#64911=CARTESIAN_POINT('Ctrl Pts',(-2.65752099961,-37.9742356128,-2.2562168661));
#64912=CARTESIAN_POINT('Ctrl Pts',(-2.65752099961,-36.2942356128,-2.2562168661));
#64913=CARTESIAN_POINT('Ctrl Pts',(-2.54136162566,-37.9742356128,-2.31314371737));
#64914=CARTESIAN_POINT('Ctrl Pts',(-2.54136162566,-36.2942356128,-2.31314371737));
#64915=CARTESIAN_POINT('Ctrl Pts',(-2.42434411094,-37.9742356128,-2.36824808793));
#64916=CARTESIAN_POINT('Ctrl Pts',(-2.42434411094,-36.2942356128,-2.36824808793));
#64917=CARTESIAN_POINT('',(-2.42434411094,-37.2742356128,-2.36824808793));
#64918=CARTESIAN_POINT('Ctrl Pts',(-2.29653416635,-36.2742356128,-2.09683582206));
#64919=CARTESIAN_POINT('Ctrl Pts',(-2.33668684465,-36.2742356128,-2.18210250012));
#64920=CARTESIAN_POINT('Ctrl Pts',(-2.37683952295,-36.3112466293,-2.26736917817));
#64921=CARTESIAN_POINT('Ctrl Pts',(-2.40857619105,-36.3857400536,-2.33476394176));
#64922=CARTESIAN_POINT('Ctrl Pts',(-2.42434411094,-36.4799878332,-2.36824808793));
#64923=CARTESIAN_POINT('Ctrl Pts',(-2.42434411094,-36.5742356128,-2.36824808793));
#64924=CARTESIAN_POINT('Ctrl Pts',(-2.17844599916,-36.2742356128,-2.1524443704));
#64925=CARTESIAN_POINT('Ctrl Pts',(-2.21652342692,-36.2742356128,-2.23868829852));
#64926=CARTESIAN_POINT('Ctrl Pts',(-2.25460085469,-36.3112466293,-2.32493222664));
#64927=CARTESIAN_POINT('Ctrl Pts',(-2.28469724522,-36.3857400536,-2.39309940847));
#64928=CARTESIAN_POINT('Ctrl Pts',(-2.29965021614,-36.4799878332,-2.42696731985));
#64929=CARTESIAN_POINT('Ctrl Pts',(-2.29965021614,-36.5742356128,-2.42696731985));
#64930=CARTESIAN_POINT('Ctrl Pts',(-2.05865446461,-36.2742356128,-2.20446579111));
#64931=CARTESIAN_POINT('Ctrl Pts',(-2.09463456858,-36.2742356128,-2.29162022708));
#64932=CARTESIAN_POINT('Ctrl Pts',(-2.13061467256,-36.3112466293,-2.37877466305));
#64933=CARTESIAN_POINT('Ctrl Pts',(-2.15905333884,-36.3857400536,-2.44766151009));
#64934=CARTESIAN_POINT('Ctrl Pts',(-2.17318269263,-36.4799878332,-2.48188697706));
#64935=CARTESIAN_POINT('Ctrl Pts',(-2.17318269263,-36.5742356128,-2.48188697706));
#64936=CARTESIAN_POINT('Ctrl Pts',(-1.93731975861,-36.2742356128,-2.25284642822));
#64937=CARTESIAN_POINT('Ctrl Pts',(-1.97117776269,-36.2742356128,-2.3408461829));
#64938=CARTESIAN_POINT('Ctrl Pts',(-2.00503576677,-36.3112466293,-2.42884593757));
#64939=CARTESIAN_POINT('Ctrl Pts',(-2.03179719321,-36.3857400536,-2.49840091092));
#64940=CARTESIAN_POINT('Ctrl Pts',(-2.04509313286,-36.4799878332,-2.53295834717));
#64941=CARTESIAN_POINT('Ctrl Pts',(-2.04509313286,-36.5742356128,-2.53295834717));
#64942=CARTESIAN_POINT('Ctrl Pts',(-1.69184409393,-36.2742356128,-2.34222839622));
#64943=CARTESIAN_POINT('Ctrl Pts',(-1.7214278807,-36.2742356128,-2.4317855696));
#64944=CARTESIAN_POINT('Ctrl Pts',(-1.75101166748,-36.3112466293,-2.52134274297));
#64945=CARTESIAN_POINT('Ctrl Pts',(-1.77439461858,-36.3857400536,-2.59212872651));
#64946=CARTESIAN_POINT('Ctrl Pts',(-1.78601221194,-36.4799878332,-2.62729773286));
#64947=CARTESIAN_POINT('Ctrl Pts',(-1.78601221194,-36.5742356128,-2.62729773286));
#64948=CARTESIAN_POINT('Ctrl Pts',(-1.44144377776,-36.2742356128,-2.41663224395));
#64949=CARTESIAN_POINT('Ctrl Pts',(-1.46665418431,-36.2742356128,-2.50748826439));
#64950=CARTESIAN_POINT('Ctrl Pts',(-1.49186459086,-36.3112466293,-2.59834428482));
#64951=CARTESIAN_POINT('Ctrl Pts',(-1.51179095812,-36.3857400536,-2.67015685));
#64952=CARTESIAN_POINT('Ctrl Pts',(-1.52169099416,-36.4799878332,-2.70583593919));
#64953=CARTESIAN_POINT('Ctrl Pts',(-1.52169099416,-36.5742356128,-2.70583593919));
#64954=CARTESIAN_POINT('Ctrl Pts',(-1.31513154012,-36.2742356128,-2.45004581652));
#64955=CARTESIAN_POINT('Ctrl Pts',(-1.33815301486,-36.2742356128,-2.54148212378));
#64956=CARTESIAN_POINT('Ctrl Pts',(-1.3611744896,-36.3112466293,-2.63291843104));
#64957=CARTESIAN_POINT('Ctrl Pts',(-1.37937038832,-36.3857400536,-2.70518972178));
#64958=CARTESIAN_POINT('Ctrl Pts',(-1.38841117016,-36.4799878332,-2.7410966221));
#64959=CARTESIAN_POINT('Ctrl Pts',(-1.38841117016,-36.5742356128,-2.7410966221));
#64960=CARTESIAN_POINT('Ctrl Pts',(-1.18795712379,-36.2742356128,-2.47960053242));
#64961=CARTESIAN_POINT('Ctrl Pts',(-1.20872995768,-36.2742356128,-2.57155896492));
#64962=CARTESIAN_POINT('Ctrl Pts',(-1.22950279157,-36.3112466293,-2.66351739742));
#64963=CARTESIAN_POINT('Ctrl Pts',(-1.24592181481,-36.3857400536,-2.73620128653));
#64964=CARTESIAN_POINT('Ctrl Pts',(-1.2540791077,-36.4799878332,-2.77231331425));
#64965=CARTESIAN_POINT('Ctrl Pts',(-1.2540791077,-36.5742356128,-2.77231331425));
#64966=CARTESIAN_POINT('Ctrl Pts',(-1.05996478409,-36.2742356128,-2.50526963826));
#64967=CARTESIAN_POINT('Ctrl Pts',(-1.07849731386,-36.2742356128,-2.59767737229));
#64968=CARTESIAN_POINT('Ctrl Pts',(-1.09702984363,-36.3112466293,-2.69008510632));
#64969=CARTESIAN_POINT('Ctrl Pts',(-1.11167795108,-36.3857400536,-2.76312415899));
#64970=CARTESIAN_POINT('Ctrl Pts',(-1.1189556585,-36.4799878332,-2.79941259128));
#64971=CARTESIAN_POINT('Ctrl Pts',(-1.1189556585,-36.5742356128,-2.79941259128));
#64972=CARTESIAN_POINT('',(-1.11895565834,-36.5742356128,-2.79941259037));
#64973=CARTESIAN_POINT('Origin',(-1.06038177374648,-36.572114319719,-2.50734954270403));
#64974=CARTESIAN_POINT('Origin',(-0.445434424830266,-36.5742356128,1.4314036149712));
#64975=CARTESIAN_POINT('Ctrl Pts',(-1.11895565712,-37.9742356128,-2.79941258318));
#64976=CARTESIAN_POINT('Ctrl Pts',(-1.11895565712,-38.0684833925,-2.79941258318));
#64977=CARTESIAN_POINT('Ctrl Pts',(-1.1116780293,-38.1627311721,-2.76312413504));
#64978=CARTESIAN_POINT('Ctrl Pts',(-1.09703008208,-38.2372245964,-2.6900850505));
#64979=CARTESIAN_POINT('Ctrl Pts',(-1.07849775503,-38.2742356129,-2.59767727615));
#64980=CARTESIAN_POINT('Ctrl Pts',(-1.05996542799,-38.2742356128,-2.50526950182));
#64981=CARTESIAN_POINT('Ctrl Pts',(-1.25407581983,-37.9742356128,-2.7723140373));
#64982=CARTESIAN_POINT('Ctrl Pts',(-1.25407581979,-38.0684833925,-2.77231403731));
#64983=CARTESIAN_POINT('Ctrl Pts',(-1.24591947351,-38.1627311723,-2.73620181852));
#64984=CARTESIAN_POINT('Ctrl Pts',(-1.22950248938,-38.2372245966,-2.66351751812));
#64985=CARTESIAN_POINT('Ctrl Pts',(-1.20873217919,-38.274235613,-2.57155857651));
#64986=CARTESIAN_POINT('Ctrl Pts',(-1.18796186904,-38.2742356128,-2.47959963495));
#64987=CARTESIAN_POINT('Ctrl Pts',(-1.38841813634,-37.9742356128,-2.74109509296));
#64988=CARTESIAN_POINT('Ctrl Pts',(-1.38841812984,-38.0684833917,-2.74109509422));
#64989=CARTESIAN_POINT('Ctrl Pts',(-1.37937582186,-38.1627311705,-2.70518850284));
#64990=CARTESIAN_POINT('Ctrl Pts',(-1.36117665871,-38.2372245946,-2.63291787243));
#64991=CARTESIAN_POINT('Ctrl Pts',(-1.33815114202,-38.2742356116,-2.54148238272));
#64992=CARTESIAN_POINT('Ctrl Pts',(-1.31512562779,-38.2742356128,-2.45004689205));
#64993=CARTESIAN_POINT('Ctrl Pts',(-1.52169104358,-37.9742356128,-2.70583567795));
#64994=CARTESIAN_POINT('Ctrl Pts',(-1.52169102758,-38.068483392,-2.70583568235));
#64995=CARTESIAN_POINT('Ctrl Pts',(-1.51179115796,-38.1627311711,-2.67015661522));
#64996=CARTESIAN_POINT('Ctrl Pts',(-1.49186535352,-38.2372245952,-2.59834400459));
#64997=CARTESIAN_POINT('Ctrl Pts',(-1.46665558121,-38.2742356121,-2.50748795926));
#64998=CARTESIAN_POINT('Ctrl Pts',(-1.44144581512,-38.2742356128,-2.41663191191));
#64999=CARTESIAN_POINT('Ctrl Pts',(-1.78601349475,-37.9742356128,-2.62729758713));
#65000=CARTESIAN_POINT('Ctrl Pts',(-1.7860134747,-38.0684833923,-2.62729759371));
#65001=CARTESIAN_POINT('Ctrl Pts',(-1.77439565629,-38.1627311718,-2.59212858833));
#65002=CARTESIAN_POINT('Ctrl Pts',(-1.75101206839,-38.2372245961,-2.52134268314));
#65003=CARTESIAN_POINT('Ctrl Pts',(-1.72142757559,-38.2742356127,-2.4317855694));
#65004=CARTESIAN_POINT('Ctrl Pts',(-1.69184309062,-38.2742356128,-2.34222845301));
#65005=CARTESIAN_POINT('Ctrl Pts',(-2.04509216583,-37.9742356128,-2.53295838102));
#65006=CARTESIAN_POINT('Ctrl Pts',(-2.04509215359,-38.0684833931,-2.53295838601));
#65007=CARTESIAN_POINT('Ctrl Pts',(-2.03179639085,-38.1627311734,-2.49840097113));
#65008=CARTESIAN_POINT('Ctrl Pts',(-2.00503554375,-38.2372245979,-2.42884595021));
#65009=CARTESIAN_POINT('Ctrl Pts',(-1.97117819268,-38.2742356139,-2.34084616804));
#65010=CARTESIAN_POINT('Ctrl Pts',(-1.93732084657,-38.2742356128,-2.25284638431));
#65011=CARTESIAN_POINT('Ctrl Pts',(-2.17317993067,-37.9742356128,-2.48188822357));
#65012=CARTESIAN_POINT('Ctrl Pts',(-2.17317993101,-38.0684833925,-2.48188822361));
#65013=CARTESIAN_POINT('Ctrl Pts',(-2.15905113355,-38.1627311721,-2.44766249585));
#65014=CARTESIAN_POINT('Ctrl Pts',(-2.13061295397,-38.2372245964,-2.37877542164));
#65015=CARTESIAN_POINT('Ctrl Pts',(-2.09463373126,-38.2742356129,-2.29162057324));
#65016=CARTESIAN_POINT('Ctrl Pts',(-2.05865450841,-38.2742356128,-2.2044657248));
#65017=CARTESIAN_POINT('Ctrl Pts',(-2.2996499723,-37.9742356128,-2.42696743467));
#65018=CARTESIAN_POINT('Ctrl Pts',(-2.2996499723,-38.0684833924,-2.42696743467));
#65019=CARTESIAN_POINT('Ctrl Pts',(-2.28469686299,-38.1627311721,-2.39309958844));
#65020=CARTESIAN_POINT('Ctrl Pts',(-2.25460061566,-38.2372245963,-2.32493233923));
#65021=CARTESIAN_POINT('Ctrl Pts',(-2.21652319195,-38.2742356128,-2.23868840917));
#65022=CARTESIAN_POINT('Ctrl Pts',(-2.17844576824,-38.2742356128,-2.15244447914));
#65023=CARTESIAN_POINT('Ctrl Pts',(-2.42434411094,-37.9742356128,-2.36824808793));
#65024=CARTESIAN_POINT('Ctrl Pts',(-2.42434411094,-38.0684833924,-2.36824808793));
#65025=CARTESIAN_POINT('Ctrl Pts',(-2.40857619105,-38.1627311721,-2.33476394176));
#65026=CARTESIAN_POINT('Ctrl Pts',(-2.37683952295,-38.2372245963,-2.26736917817));
#65027=CARTESIAN_POINT('Ctrl Pts',(-2.33668684465,-38.2742356128,-2.18210250012));
#65028=CARTESIAN_POINT('Ctrl Pts',(-2.29653416635,-38.2742356128,-2.09683582206));
#65029=CARTESIAN_POINT('',(-1.11895565834,-37.9742356128,-2.79941259037));
#65030=CARTESIAN_POINT('Origin',(-0.44543442481793,-37.9742356128,1.43140361501597));
#65031=CARTESIAN_POINT('Origin',(-1.06038281360066,-37.9763568917485,-2.50734931579821));
#65032=CARTESIAN_POINT('Ctrl Pts',(-2.42434411094,-37.9742356128,-2.36824808793));
#65033=CARTESIAN_POINT('Ctrl Pts',(-2.42434411094,-36.2942356128,-2.36824808793));
#65034=CARTESIAN_POINT('Ctrl Pts',(-2.1749855611,-37.9742356128,-2.48567278256));
#65035=CARTESIAN_POINT('Ctrl Pts',(-2.1749855611,-36.2942356128,-2.48567278256));
#65036=CARTESIAN_POINT('Ctrl Pts',(-1.91849016776,-37.9742356128,-2.58792345825));
#65037=CARTESIAN_POINT('Ctrl Pts',(-1.91849016776,-36.2942356128,-2.58792345825));
#65038=CARTESIAN_POINT('Ctrl Pts',(-1.65613520407,-37.9742356128,-2.67457823688));
#65039=CARTESIAN_POINT('Ctrl Pts',(-1.65613520407,-36.2942356128,-2.67457823688));
#65040=CARTESIAN_POINT('Ctrl Pts',(-1.38919794322,-37.9742356128,-2.7452152403));
#65041=CARTESIAN_POINT('Ctrl Pts',(-1.38919794322,-36.2942356128,-2.7452152403));
#65042=CARTESIAN_POINT('Ctrl Pts',(-1.11895565834,-37.9742356128,-2.79941259037));
#65043=CARTESIAN_POINT('Ctrl Pts',(-1.11895565834,-36.2942356128,-2.79941259037));
#65044=CARTESIAN_POINT('',(-1.11895565834,-37.2742356128,-2.79941259037));
#65045=CARTESIAN_POINT('Ctrl Pts',(-1.05996499772,-36.2742356128,-2.50526959461));
#65046=CARTESIAN_POINT('Ctrl Pts',(-1.07849746032,-36.2742356128,-2.59767734207));
#65047=CARTESIAN_POINT('Ctrl Pts',(-1.09702992293,-36.3112466293,-2.69008508953));
#65048=CARTESIAN_POINT('Ctrl Pts',(-1.1116779773,-36.3857400536,-2.7631241528));
#65049=CARTESIAN_POINT('Ctrl Pts',(-1.11895565834,-36.4799878332,-2.79941259037));
#65050=CARTESIAN_POINT('Ctrl Pts',(-1.11895565834,-36.5742356128,-2.79941259037));
#65051=CARTESIAN_POINT('Ctrl Pts',(-0.937988992329,-36.2742356128,-2.52973199977));
#65052=CARTESIAN_POINT('Ctrl Pts',(-0.970994450831,-36.2742356128,-2.61923717399));
#65053=CARTESIAN_POINT('Ctrl Pts',(-1.00399990933,-36.3112466293,-2.7087423482));
#65054=CARTESIAN_POINT('Ctrl Pts',(-1.03008741817,-36.3857400536,-2.77948721657));
#65055=CARTESIAN_POINT('Ctrl Pts',(-1.04304862972,-36.4799878332,-2.81463581795));
#65056=CARTESIAN_POINT('Ctrl Pts',(-1.04304862972,-36.5742356128,-2.81463581795));
#65057=CARTESIAN_POINT('Ctrl Pts',(-0.821076773765,-36.2742356128,-2.57798936015));
#65058=CARTESIAN_POINT('Ctrl Pts',(-0.86770125157,-36.2742356128,-2.66182817053));
#65059=CARTESIAN_POINT('Ctrl Pts',(-0.914325729375,-36.3112466293,-2.74566698092));
#65060=CARTESIAN_POINT('Ctrl Pts',(-0.951177701909,-36.3857400536,-2.81193316369));
#65061=CARTESIAN_POINT('Ctrl Pts',(-0.969487096,-36.4799878332,-2.84485658206));
#65062=CARTESIAN_POINT('Ctrl Pts',(-0.969487096,-36.5742356128,-2.84485658206));
#65063=CARTESIAN_POINT('Ctrl Pts',(-0.714826514539,-36.2742356128,-2.64836711386));
#65064=CARTESIAN_POINT('Ctrl Pts',(-0.773989357268,-36.2742356128,-2.72393749335));
#65065=CARTESIAN_POINT('Ctrl Pts',(-0.833152199997,-36.3112466293,-2.79950787283));
#65066=CARTESIAN_POINT('Ctrl Pts',(-0.879914501023,-36.3857400536,-2.85923932342));
#65067=CARTESIAN_POINT('Ctrl Pts',(-0.903147691892,-36.4799878332,-2.88891510279));
#65068=CARTESIAN_POINT('Ctrl Pts',(-0.903147691892,-36.5742356128,-2.88891510279));
#65069=CARTESIAN_POINT('Ctrl Pts',(-0.556197836783,-36.2742356128,-2.80610207254));
#65070=CARTESIAN_POINT('Ctrl Pts',(-0.634097615818,-36.2742356128,-2.86306407596));
#65071=CARTESIAN_POINT('Ctrl Pts',(-0.711997394853,-36.3112466293,-2.92002607939));
#65072=CARTESIAN_POINT('Ctrl Pts',(-0.773569356126,-36.3857400536,-2.9650483506));
#65073=CARTESIAN_POINT('Ctrl Pts',(-0.804160534767,-36.4799878332,-2.98741776081));
#65074=CARTESIAN_POINT('Ctrl Pts',(-0.804160534767,-36.5742356128,-2.98741776081));
#65075=CARTESIAN_POINT('Ctrl Pts',(-0.460021515721,-36.2742356128,-3.00625265901));
#65076=CARTESIAN_POINT('Ctrl Pts',(-0.549251084872,-36.2742356128,-3.03960036015));
#65077=CARTESIAN_POINT('Ctrl Pts',(-0.638480654024,-36.3112466293,-3.0729480613));
#65078=CARTESIAN_POINT('Ctrl Pts',(-0.709007694683,-36.3857400536,-3.09930644297));
#65079=CARTESIAN_POINT('Ctrl Pts',(-0.744048055729,-36.4799878332,-3.11240168856));
#65080=CARTESIAN_POINT('Ctrl Pts',(-0.744048055729,-36.5742356128,-3.11240168856));
#65081=CARTESIAN_POINT('Ctrl Pts',(-0.431626462484,-36.2742356128,-3.09869414072));
#65082=CARTESIAN_POINT('Ctrl Pts',(-0.524172700417,-36.2742356128,-3.12125741915));
#65083=CARTESIAN_POINT('Ctrl Pts',(-0.616718938351,-36.3112466293,-3.14382069757));
#65084=CARTESIAN_POINT('Ctrl Pts',(-0.689867444729,-36.3857400536,-3.16165322052));
#65085=CARTESIAN_POINT('Ctrl Pts',(-0.726210287117,-36.4799878332,-3.17051528659));
#65086=CARTESIAN_POINT('Ctrl Pts',(-0.726210287117,-36.5742356128,-3.17051528659));
#65087=CARTESIAN_POINT('Ctrl Pts',(-0.417273517967,-36.2742356128,-3.19418486389));
#65088=CARTESIAN_POINT('Ctrl Pts',(-0.511521247419,-36.2742356128,-3.2054748872));
#65089=CARTESIAN_POINT('Ctrl Pts',(-0.605768976872,-36.3112466293,-3.21676491052));
#65090=CARTESIAN_POINT('Ctrl Pts',(-0.680262375652,-36.3857400536,-3.22568953251));
#65091=CARTESIAN_POINT('Ctrl Pts',(-0.717273358318,-36.4799878332,-3.23012212425));
#65092=CARTESIAN_POINT('Ctrl Pts',(-0.717273358318,-36.5742356128,-3.23012212425));
#65093=CARTESIAN_POINT('Ctrl Pts',(-0.41727348535,-36.2742356128,-3.28965270484));
#65094=CARTESIAN_POINT('Ctrl Pts',(-0.511521248788,-36.2742356128,-3.28965214022));
#65095=CARTESIAN_POINT('Ctrl Pts',(-0.605769012226,-36.3112466293,-3.28965157561));
#65096=CARTESIAN_POINT('Ctrl Pts',(-0.680262423725,-36.3857400536,-3.28965112934));
#65097=CARTESIAN_POINT('Ctrl Pts',(-0.71727343388,-36.4799878332,-3.28965090762));
#65098=CARTESIAN_POINT('Ctrl Pts',(-0.71727343388,-36.5742356128,-3.28965090762));
#65099=CARTESIAN_POINT('',(-0.717273428011933,-36.5742356128,-3.28965091325724));
#65100=CARTESIAN_POINT('Origin',(-0.419394826283105,-36.5721142715659,-3.28965392582749));
#65101=CARTESIAN_POINT('Ctrl Pts',(-1.11895565834,-36.5742356128,-2.79941259037));
#65102=CARTESIAN_POINT('Ctrl Pts',(-0.984348856958,-36.5742356128,-2.82640811382));
#65103=CARTESIAN_POINT('Ctrl Pts',(-0.858305199948,-36.5742356128,-2.90029762813));
#65104=CARTESIAN_POINT('Ctrl Pts',(-0.764935707726,-36.5742356128,-3.0142516443));
#65105=CARTESIAN_POINT('Ctrl Pts',(-0.717273426056,-36.5742356128,-3.15236381141));
#65106=CARTESIAN_POINT('Ctrl Pts',(-0.717273426056,-36.5742356128,-3.28965091665));
#65107=CARTESIAN_POINT('Ctrl Pts',(-0.717273426048,-37.9742356128,-3.28965091666));
#65108=CARTESIAN_POINT('Ctrl Pts',(-0.717273426048,-38.0684833924,-3.28965091666));
#65109=CARTESIAN_POINT('Ctrl Pts',(-0.680262409542,-38.1627311721,-3.28965091863));
#65110=CARTESIAN_POINT('Ctrl Pts',(-0.605768985255,-38.2372245963,-3.28965092261));
#65111=CARTESIAN_POINT('Ctrl Pts',(-0.51152120564,-38.2742356128,-3.28965092765));
#65112=CARTESIAN_POINT('Ctrl Pts',(-0.417273426023,-38.2742356128,-3.28965093269));
#65113=CARTESIAN_POINT('Ctrl Pts',(-0.717273419177,-37.9742356128,-3.22013522682));
#65114=CARTESIAN_POINT('Ctrl Pts',(-0.717273419176,-38.0684833915,-3.22013522525));
#65115=CARTESIAN_POINT('Ctrl Pts',(-0.680262405917,-38.1627311702,-3.2149372275));
#65116=CARTESIAN_POINT('Ctrl Pts',(-0.6057689684,-38.2372245936,-3.20445862027));
#65117=CARTESIAN_POINT('Ctrl Pts',(-0.51152117913,-38.2742356114,-3.19120816235));
#65118=CARTESIAN_POINT('Ctrl Pts',(-0.41727338975,-38.2742356128,-3.1779577045));
#65119=CARTESIAN_POINT('Ctrl Pts',(-0.729496094549,-37.9742356128,-3.15011357747));
#65120=CARTESIAN_POINT('Ctrl Pts',(-0.729496105134,-38.0684833954,-3.15011362984));
#65121=CARTESIAN_POINT('Ctrl Pts',(-0.693397562691,-38.1627311779,-3.13978673356));
#65122=CARTESIAN_POINT('Ctrl Pts',(-0.620740718576,-38.2372246041,-3.1190259698));
#65123=CARTESIAN_POINT('Ctrl Pts',(-0.528816534376,-38.2742356175,-3.09274944111));
#65124=CARTESIAN_POINT('Ctrl Pts',(-0.436892347128,-38.2742356128,-3.06647289285));
#65125=CARTESIAN_POINT('Ctrl Pts',(-0.753979035124,-37.9742356128,-3.08313484153));
#65126=CARTESIAN_POINT('Ctrl Pts',(-0.753979001334,-38.0684833919,-3.08313487243));
#65127=CARTESIAN_POINT('Ctrl Pts',(-0.719665250065,-38.162731171,-3.06787499254));
#65128=CARTESIAN_POINT('Ctrl Pts',(-0.650603626306,-38.237224595,-3.0371540007));
#65129=CARTESIAN_POINT('Ctrl Pts',(-0.563226878153,-38.274235612,-2.99828919133));
#65130=CARTESIAN_POINT('Ctrl Pts',(-0.475850143134,-38.2742356128,-2.95942436955));
#65131=CARTESIAN_POINT('Ctrl Pts',(-0.823421763256,-37.9742356128,-2.96275807432));
#65132=CARTESIAN_POINT('Ctrl Pts',(-0.823421795982,-38.068483393,-2.96275804439));
#65133=CARTESIAN_POINT('Ctrl Pts',(-0.794269071684,-38.1627311731,-2.93855494734));
#65134=CARTESIAN_POINT('Ctrl Pts',(-0.735589477825,-38.2372245976,-2.88984716793));
#65135=CARTESIAN_POINT('Ctrl Pts',(-0.661350237699,-38.2742356137,-2.8282201644));
#65136=CARTESIAN_POINT('Ctrl Pts',(-0.587110984843,-38.2742356128,-2.7665931729));
#65137=CARTESIAN_POINT('Ctrl Pts',(-0.929441126526,-37.9742356128,-2.87248382646));
#65138=CARTESIAN_POINT('Ctrl Pts',(-0.929441094831,-38.0684833919,-2.87248385545));
#65139=CARTESIAN_POINT('Ctrl Pts',(-0.908153241286,-38.162731171,-2.84158573857));
#65140=CARTESIAN_POINT('Ctrl Pts',(-0.865309169175,-38.2372245951,-2.77938948391));
#65141=CARTESIAN_POINT('Ctrl Pts',(-0.811102469518,-38.274235612,-2.70070256092));
#65142=CARTESIAN_POINT('Ctrl Pts',(-0.756895782199,-38.2742356128,-2.62201562628));
#65143=CARTESIAN_POINT('Ctrl Pts',(-0.988199684399,-37.9742356128,-2.83740276005));
#65144=CARTESIAN_POINT('Ctrl Pts',(-0.98819966439,-38.0684833915,-2.83740274799));
#65145=CARTESIAN_POINT('Ctrl Pts',(-0.971255993125,-38.1627311702,-2.80393138744));
#65146=CARTESIAN_POINT('Ctrl Pts',(-0.937141997279,-38.2372245934,-2.7365650062));
#65147=CARTESIAN_POINT('Ctrl Pts',(-0.893986145252,-38.2742356114,-2.6513331367));
#65148=CARTESIAN_POINT('Ctrl Pts',(-0.850830300288,-38.2742356128,-2.56610127211));
#65149=CARTESIAN_POINT('Ctrl Pts',(-1.05294849577,-37.9742356128,-2.81265039029));
#65150=CARTESIAN_POINT('Ctrl Pts',(-1.05294849577,-38.0684833924,-2.81265039029));
#65151=CARTESIAN_POINT('Ctrl Pts',(-1.04072612657,-38.1627311721,-2.77735371605));
#65152=CARTESIAN_POINT('Ctrl Pts',(-1.01613297159,-38.2372245968,-2.70630905049));
#65153=CARTESIAN_POINT('Ctrl Pts',(-0.985015094421,-38.2742356128,-2.61642532043));
#65154=CARTESIAN_POINT('Ctrl Pts',(-0.953897217654,-38.2742356128,-2.52654158988));
#65155=CARTESIAN_POINT('Ctrl Pts',(-1.11895565834,-37.9742356128,-2.79941259037));
#65156=CARTESIAN_POINT('Ctrl Pts',(-1.11895565834,-38.0684833924,-2.79941259037));
#65157=CARTESIAN_POINT('Ctrl Pts',(-1.1116779773,-38.1627311721,-2.7631241528));
#65158=CARTESIAN_POINT('Ctrl Pts',(-1.09702992293,-38.2372245963,-2.69008508953));
#65159=CARTESIAN_POINT('Ctrl Pts',(-1.07849746032,-38.2742356128,-2.59767734207));
#65160=CARTESIAN_POINT('Ctrl Pts',(-1.05996499772,-38.2742356128,-2.50526959461));
#65161=CARTESIAN_POINT('',(-0.717273426056,-37.9742356128,-3.28965091665));
#65162=CARTESIAN_POINT('Ctrl Pts',(-1.11895565834,-37.9742356128,-2.79941259037));
#65163=CARTESIAN_POINT('Ctrl Pts',(-1.05294849577,-37.9742356128,-2.81265039029));
#65164=CARTESIAN_POINT('Ctrl Pts',(-0.988199684399,-37.9742356128,-2.83740276005));
#65165=CARTESIAN_POINT('Ctrl Pts',(-0.929441126526,-37.9742356128,-2.87248382646));
#65166=CARTESIAN_POINT('Ctrl Pts',(-0.823421763256,-37.9742356128,-2.96275807432));
#65167=CARTESIAN_POINT('Ctrl Pts',(-0.753979035124,-37.9742356128,-3.08313484153));
#65168=CARTESIAN_POINT('Ctrl Pts',(-0.729496094549,-37.9742356128,-3.15011357747));
#65169=CARTESIAN_POINT('Ctrl Pts',(-0.717273419177,-37.9742356128,-3.22013522682));
#65170=CARTESIAN_POINT('Ctrl Pts',(-0.717273426056,-37.9742356128,-3.28965091665));
#65171=CARTESIAN_POINT('Origin',(-0.419394766787071,-37.9763569535626,-3.28965094375126));
#65172=CARTESIAN_POINT('Ctrl Pts',(-1.11895565834,-37.9742356128,-2.79941259037));
#65173=CARTESIAN_POINT('Ctrl Pts',(-1.11895565834,-36.2942356128,-2.79941259037));
#65174=CARTESIAN_POINT('Ctrl Pts',(-0.984348856958,-37.9742356128,-2.82640811382));
#65175=CARTESIAN_POINT('Ctrl Pts',(-0.984348856958,-36.2942356128,-2.82640811382));
#65176=CARTESIAN_POINT('Ctrl Pts',(-0.858305199948,-37.9742356128,-2.90029762813));
#65177=CARTESIAN_POINT('Ctrl Pts',(-0.858305199948,-36.2942356128,-2.90029762813));
#65178=CARTESIAN_POINT('Ctrl Pts',(-0.764935707726,-37.9742356128,-3.0142516443));
#65179=CARTESIAN_POINT('Ctrl Pts',(-0.764935707726,-36.2942356128,-3.0142516443));
#65180=CARTESIAN_POINT('Ctrl Pts',(-0.717273426056,-37.9742356128,-3.15236381141));
#65181=CARTESIAN_POINT('Ctrl Pts',(-0.717273426056,-36.2942356128,-3.15236381141));
#65182=CARTESIAN_POINT('Ctrl Pts',(-0.717273426056,-37.9742356128,-3.28965091665));
#65183=CARTESIAN_POINT('Ctrl Pts',(-0.717273426056,-36.2942356128,-3.28965091665));
#65184=CARTESIAN_POINT('',(-0.717273426056,-37.2742356128,-3.28965091665));
#65185=CARTESIAN_POINT('Origin',(-0.417273426056,-36.5742356128,0.915007091638));
#65186=CARTESIAN_POINT('',(-0.717294771012954,-36.5742356128,-7.94951669056715));
#65187=CARTESIAN_POINT('Ctrl Pts',(-0.717273426055526,-36.5742356127522,
-7.94951682269996));
#65188=CARTESIAN_POINT('Ctrl Pts',(-0.717273426052653,-36.5562023660265,
-7.94949943022529));
#65189=CARTESIAN_POINT('Ctrl Pts',(-0.715643103341005,-36.5381711705819,
-7.94948981501555));
#65190=CARTESIAN_POINT('Ctrl Pts',(-0.712409414919946,-36.5204327497068,
-7.94948727993358));
#65191=CARTESIAN_POINT('Ctrl Pts',(-0.709174428725905,-36.5026872098889,
-7.94948474383421));
#65192=CARTESIAN_POINT('Ctrl Pts',(-0.704334899389936,-36.4852352845449,
-7.94948929354667));
#65193=CARTESIAN_POINT('Ctrl Pts',(-0.697969075237865,-36.4683585495138,
-7.9495002310941));
#65194=CARTESIAN_POINT('Ctrl Pts',(-0.691605209984622,-36.4514870078113,
-7.94951116527583));
#65195=CARTESIAN_POINT('Ctrl Pts',(-0.683716207778636,-36.4351908765912,
-7.94952848336179));
#65196=CARTESIAN_POINT('Ctrl Pts',(-0.674428984546402,-36.4197331249972,
-7.94955148801929));
#65197=CARTESIAN_POINT('Ctrl Pts',(-0.665142406327905,-36.4042764469708,
-7.94957449107908));
#65198=CARTESIAN_POINT('Ctrl Pts',(-0.654458114349865,-36.389658560481,
-7.94960317992055));
#65199=CARTESIAN_POINT('Ctrl Pts',(-0.642547746664798,-36.3761157488943,
-7.94963685735628));
#65200=CARTESIAN_POINT('Ctrl Pts',(-0.63832252716711,-36.3713114176525,
-7.94964880447344));
#65201=CARTESIAN_POINT('Ctrl Pts',(-0.633943394736352,-36.366642101442,
-7.94966137939795));
#65202=CARTESIAN_POINT('Ctrl Pts',(-0.629419239159912,-36.3621173580875,
-7.94967455100391));
#65203=CARTESIAN_POINT('Ctrl Pts',(-0.616649081950513,-36.34934554178,-7.9497117299815));
#65204=CARTESIAN_POINT('Ctrl Pts',(-0.60272441955601,-36.3377319027218,
-7.94975346407593));
#65205=CARTESIAN_POINT('Ctrl Pts',(-0.587870725940692,-36.327463326528,
-7.9497985353943));
#65206=CARTESIAN_POINT('Ctrl Pts',(-0.573010913676518,-36.3171905204226,
-7.9498436252788));
#65207=CARTESIAN_POINT('Ctrl Pts',(-0.557221806446512,-36.3082642321724,
-7.9498920551372));
#65208=CARTESIAN_POINT('Ctrl Pts',(-0.540758644704151,-36.3008285887949,
-7.94994260557092));
#65209=CARTESIAN_POINT('Ctrl Pts',(-0.524300920430384,-36.2933954012688,
-7.9499931393088));
#65210=CARTESIAN_POINT('Ctrl Pts',(-0.507170142757527,-36.2874521238513,
-7.95004579222147));
#65211=CARTESIAN_POINT('Ctrl Pts',(-0.489642808887459,-36.2830953159867,
-7.95009934611819));
#65212=CARTESIAN_POINT('Ctrl Pts',(-0.47211842679632,-36.2787392418523,
-7.95015289099589));
#65213=CARTESIAN_POINT('Ctrl Pts',(-0.454198211897778,-36.2759692553201,
-7.95020733655421));
#65214=CARTESIAN_POINT('Ctrl Pts',(-0.436171421743446,-36.274831428195,
-7.95026146521776));
#65215=CARTESIAN_POINT('Ctrl Pts',(-0.429888168625485,-36.2744348375779,
-7.95028033180971));
#65216=CARTESIAN_POINT('Ctrl Pts',(-0.423592041068198,-36.2742360758603,
-7.95029915990285));
#65217=CARTESIAN_POINT('Ctrl Pts',(-0.417295449967826,-36.2742356136084,
-7.95031789793937));
#65218=CARTESIAN_POINT('',(-0.717273426056,-36.5742356128,-5.61958386968));
#65219=CARTESIAN_POINT('Origin',(-0.417273426056,-37.9742356128,0.916320001688));
#65220=CARTESIAN_POINT('',(-0.717273426055838,-37.9742356128056,-7.94951682185356));
#65221=CARTESIAN_POINT('',(-0.717273426056,-37.9742356128,-5.61958386968));
#65222=CARTESIAN_POINT('Ctrl Pts',(-0.417297207529238,-38.2742356118574,
-7.95031787674147));
#65223=CARTESIAN_POINT('Ctrl Pts',(-0.435362516829087,-38.2742341797918,
-7.95026423190646));
#65224=CARTESIAN_POINT('Ctrl Pts',(-0.453423450071235,-38.2725966404015,
-7.95020987106186));
#65225=CARTESIAN_POINT('Ctrl Pts',(-0.471188408770116,-38.269351140414,
-7.95015599844639));
#65226=CARTESIAN_POINT('Ctrl Pts',(-0.488964591978895,-38.2661035898084,
-7.95010209179235));
#65227=CARTESIAN_POINT('Ctrl Pts',(-0.50644382759733,-38.2612461595882,
-7.95004867398459));
#65228=CARTESIAN_POINT('Ctrl Pts',(-0.523343807223555,-38.2548582673361,
-7.94999695154591));
#65229=CARTESIAN_POINT('Ctrl Pts',(-0.540240303205797,-38.2484716918395,
-7.94994523976893));
#65230=CARTESIAN_POINT('Ctrl Pts',(-0.556557214267629,-38.2405555058911,
-7.94989522266216));
#65231=CARTESIAN_POINT('Ctrl Pts',(-0.572031007252925,-38.2312377354798,
-7.94984810600243));
#65232=CARTESIAN_POINT('Ctrl Pts',(-0.587504862496621,-38.2219199275787,
-7.94980098915313));
#65233=CARTESIAN_POINT('Ctrl Pts',(-0.602135070451866,-38.2112008365223,
-7.94975677277421));
#65234=CARTESIAN_POINT('Ctrl Pts',(-0.615684888811112,-38.1992531486659,
-7.94971666265708));
#65235=CARTESIAN_POINT('Ctrl Pts',(-0.620396768694504,-38.195098401453,
-7.94970271456943));
#65236=CARTESIAN_POINT('Ctrl Pts',(-0.624978274211824,-38.1907954572478,
-7.94968926303764));
#65237=CARTESIAN_POINT('Ctrl Pts',(-0.629420380828565,-38.1863527256893,
-7.94967635876712));
#65238=CARTESIAN_POINT('Ctrl Pts',(-0.642172077260688,-38.1735992352735,
-7.94963931523024));
#65239=CARTESIAN_POINT('Ctrl Pts',(-0.65376871421763,-38.1596947618457,
-7.94960697677183));
#65240=CARTESIAN_POINT('Ctrl Pts',(-0.664024067325533,-38.1448642183526,
-7.94958002984277));
#65241=CARTESIAN_POINT('Ctrl Pts',(-0.674284581348108,-38.1300262115211,
-7.94955306935291));
#65242=CARTESIAN_POINT('Ctrl Pts',(-0.683202112686164,-38.1142617086487,
-7.94953150582025));
#65243=CARTESIAN_POINT('Ctrl Pts',(-0.690633204454852,-38.0978253840331,
-7.94951602673255));
#65244=CARTESIAN_POINT('Ctrl Pts',(-0.698062440582742,-38.0813931637827,
-7.94950055151018));
#65245=CARTESIAN_POINT('Ctrl Pts',(-0.704005730097513,-38.0642900186617,
-7.94949115769443));
#65246=CARTESIAN_POINT('Ctrl Pts',(-0.708367224207067,-38.0467918025958,
-7.94948853225816));
#65247=CARTESIAN_POINT('Ctrl Pts',(-0.712728772489379,-38.02929336919,-7.94948590678928));
#65248=CARTESIAN_POINT('Ctrl Pts',(-0.715508335709052,-38.0114004503762,
-7.94949004986802));
#65249=CARTESIAN_POINT('Ctrl Pts',(-0.716660575355175,-37.9934015939698,
-7.94950164849284));
#65250=CARTESIAN_POINT('Ctrl Pts',(-0.717068990960827,-37.9870218327239,
-7.94950575966832));
#65251=CARTESIAN_POINT('Ctrl Pts',(-0.717273426055341,-37.9806288349119,
-7.94951080753942));
#65252=CARTESIAN_POINT('Ctrl Pts',(-0.717273426055477,-37.9742356128064,
-7.9495168227));
#65253=CARTESIAN_POINT('Origin',(-0.717273426056,-38.2742356128,-3.28965091665));
#65254=CARTESIAN_POINT('',(-0.717273426056,-37.2742356128,-7.9495168227));
#65255=CARTESIAN_POINT('Ctrl Pts',(-0.417871464025,-36.2742356128,-7.90065580382));
#65256=CARTESIAN_POINT('Ctrl Pts',(-0.512080830433,-36.2742356128,-7.90334683551));
#65257=CARTESIAN_POINT('Ctrl Pts',(-0.606290196842,-36.3112466293,-7.90603786721));
#65258=CARTESIAN_POINT('Ctrl Pts',(-0.680753259338,-36.3857400536,-7.90816485807));
#65259=CARTESIAN_POINT('Ctrl Pts',(-0.717749191014,-36.4799878332,-7.90922162374));
#65260=CARTESIAN_POINT('Ctrl Pts',(-0.717749191014,-36.5742356128,-7.90922162374));
#65261=CARTESIAN_POINT('Ctrl Pts',(-0.411668939385,-36.2742356128,-8.11771935816));
#65262=CARTESIAN_POINT('Ctrl Pts',(-0.506253640511,-36.2742356128,-8.10730633567));
#65263=CARTESIAN_POINT('Ctrl Pts',(-0.600838341638,-36.3112466293,-8.09689331319));
#65264=CARTESIAN_POINT('Ctrl Pts',(-0.675598077836,-36.3857400536,-8.08866280292));
#65265=CARTESIAN_POINT('Ctrl Pts',(-0.712741393888,-36.4799878332,-8.08457367815));
#65266=CARTESIAN_POINT('Ctrl Pts',(-0.712741393888,-36.5742356128,-8.08457367815));
#65267=CARTESIAN_POINT('Ctrl Pts',(-0.446634901181,-36.2742356128,-8.34322072055));
#65268=CARTESIAN_POINT('Ctrl Pts',(-0.538971580196,-36.2742356128,-8.31457120306));
#65269=CARTESIAN_POINT('Ctrl Pts',(-0.631308259211,-36.3112466293,-8.28592168556));
#65270=CARTESIAN_POINT('Ctrl Pts',(-0.704291136778,-36.3857400536,-8.26327720324));
#65271=CARTESIAN_POINT('Ctrl Pts',(-0.74055167906,-36.4799878332,-8.25202647401));
#65272=CARTESIAN_POINT('Ctrl Pts',(-0.74055167906,-36.5742356128,-8.25202647401));
#65273=CARTESIAN_POINT('Ctrl Pts',(-0.527277494643,-36.2742356128,-8.55090781155));
#65274=CARTESIAN_POINT('Ctrl Pts',(-0.614087616783,-36.2742356128,-8.51039722073));
#65275=CARTESIAN_POINT('Ctrl Pts',(-0.700897738923,-36.3112466293,-8.46988662992));
#65276=CARTESIAN_POINT('Ctrl Pts',(-0.769512681606,-36.3857400536,-8.43786699893));
#65277=CARTESIAN_POINT('Ctrl Pts',(-0.803602695624,-36.4799878332,-8.42195859603));
#65278=CARTESIAN_POINT('Ctrl Pts',(-0.803602695624,-36.5742356128,-8.42195859603));
#65279=CARTESIAN_POINT('Ctrl Pts',(-0.799039246885,-36.2742356128,-8.98598340477));
#65280=CARTESIAN_POINT('Ctrl Pts',(-0.86757857227,-36.2742356128,-8.91521826287));
#65281=CARTESIAN_POINT('Ctrl Pts',(-0.936117897654,-36.3112466293,-8.84445312098));
#65282=CARTESIAN_POINT('Ctrl Pts',(-0.990291056463,-36.3857400536,-8.78852045906));
#65283=CARTESIAN_POINT('Ctrl Pts',(-1.01720669551,-36.4799878332,-8.76073096214));
#65284=CARTESIAN_POINT('Ctrl Pts',(-1.01720669551,-36.5742356128,-8.76073096214));
#65285=CARTESIAN_POINT('Ctrl Pts',(-1.23565010735,-36.2742356128,-9.26373079525));
#65286=CARTESIAN_POINT('Ctrl Pts',(-1.27482326726,-36.2742356128,-9.17557264423));
#65287=CARTESIAN_POINT('Ctrl Pts',(-1.31399642717,-36.3112466293,-9.08741449321));
#65288=CARTESIAN_POINT('Ctrl Pts',(-1.3449592797,-36.3857400536,-9.01773419077));
#65289=CARTESIAN_POINT('Ctrl Pts',(-1.36034214807,-36.4799878332,-8.98311468508));
#65290=CARTESIAN_POINT('Ctrl Pts',(-1.36034214807,-36.5742356128,-8.98311468508));
#65291=CARTESIAN_POINT('Ctrl Pts',(-1.51660510295,-36.2742356128,-9.35601196175));
#65292=CARTESIAN_POINT('Ctrl Pts',(-1.53690836451,-36.2742356128,-9.2608811536));
#65293=CARTESIAN_POINT('Ctrl Pts',(-1.55721162606,-36.3112466293,-9.16575034545));
#65294=CARTESIAN_POINT('Ctrl Pts',(-1.573257749,-36.3857400536,-9.09055929278));
#65295=CARTESIAN_POINT('Ctrl Pts',(-1.5812323917,-36.4799878332,-9.0532011946));
#65296=CARTESIAN_POINT('Ctrl Pts',(-1.5812323917,-36.5742356128,-9.0532011946));
#65297=CARTESIAN_POINT('Ctrl Pts',(-1.80824865356,-36.2742356128,-9.37150440154));
#65298=CARTESIAN_POINT('Ctrl Pts',(-1.80877064489,-36.2742356128,-9.27537219373));
#65299=CARTESIAN_POINT('Ctrl Pts',(-1.80929263621,-36.3112466293,-9.17923998592));
#65300=CARTESIAN_POINT('Ctrl Pts',(-1.80970626455,-36.3857400536,-9.10325689802));
#65301=CARTESIAN_POINT('Ctrl Pts',(-1.80991020356,-36.4799878332,-9.06550608028));
#65302=CARTESIAN_POINT('Ctrl Pts',(-1.80991020356,-36.5742356128,-9.06550608028));
#65303=CARTESIAN_POINT('Ctrl Pts',(-2.08574139369,-36.2742356128,-9.31728165018));
#65304=CARTESIAN_POINT('Ctrl Pts',(-2.06766705511,-36.2742356128,-9.22478320569));
#65305=CARTESIAN_POINT('Ctrl Pts',(-2.04959271653,-36.3112466293,-9.13228476119));
#65306=CARTESIAN_POINT('Ctrl Pts',(-2.03530676328,-36.3857400536,-9.059174011));
#65307=CARTESIAN_POINT('Ctrl Pts',(-2.02820898712,-36.4799878332,-9.02284995679));
#65308=CARTESIAN_POINT('Ctrl Pts',(-2.02820898712,-36.5742356128,-9.02284995679));
#65309=CARTESIAN_POINT('Ctrl Pts',(-0.717294771012954,-36.5742356128,-7.94951669056715));
#65310=CARTESIAN_POINT('Ctrl Pts',(-0.717469199646846,-36.5742356128,-7.97769417776938));
#65311=CARTESIAN_POINT('Ctrl Pts',(-0.718686505327239,-36.5742356128,-8.00568861695275));
#65312=CARTESIAN_POINT('Ctrl Pts',(-0.72096154011341,-36.5742356128,-8.03353757677499));
#65313=CARTESIAN_POINT('Ctrl Pts',(-0.723452189808266,-36.5742356128,-8.06402590324145));
#65314=CARTESIAN_POINT('Ctrl Pts',(-0.727210703773945,-36.5742356128,-8.09433991822543));
#65315=CARTESIAN_POINT('Ctrl Pts',(-0.732240265268736,-36.5742356128,-8.12446475504702));
#65316=CARTESIAN_POINT('Ctrl Pts',(-0.737584387333829,-36.5742356128,-8.15647366980674));
#65317=CARTESIAN_POINT('Ctrl Pts',(-0.744363567783376,-36.5742356128,-8.18826835117234));
#65318=CARTESIAN_POINT('Ctrl Pts',(-0.752562528474982,-36.5742356128,-8.21976675650004));
#65319=CARTESIAN_POINT('Ctrl Pts',(-0.761700247367715,-36.5742356128,-8.25487164165317));
#65320=CARTESIAN_POINT('Ctrl Pts',(-0.772601684950244,-36.5742356128,-8.28960751029073));
#65321=CARTESIAN_POINT('Ctrl Pts',(-0.785220319760699,-36.5742356128,-8.32379577982941));
#65322=CARTESIAN_POINT('Ctrl Pts',(-0.80131191002952,-36.5742356128,-8.36739349334441));
#65323=CARTESIAN_POINT('Ctrl Pts',(-0.820197223142365,-36.5742356128,-8.41009700371508));
#65324=CARTESIAN_POINT('Ctrl Pts',(-0.841726991467189,-36.5742356128,-8.45146835090127));
#65325=CARTESIAN_POINT('Ctrl Pts',(-0.85905852894392,-36.5742356128,-8.48477242753611));
#65326=CARTESIAN_POINT('Ctrl Pts',(-0.878102400020843,-36.5742356128,-8.5172097589679));
#65327=CARTESIAN_POINT('Ctrl Pts',(-0.898758903658759,-36.5742356128,-8.54857028838719));
#65328=CARTESIAN_POINT('Ctrl Pts',(-0.916170691277028,-36.5742356128,-8.57500471734074));
#65329=CARTESIAN_POINT('Ctrl Pts',(-0.934727842012251,-36.5742356128,-8.60067345421032));
#65330=CARTESIAN_POINT('Ctrl Pts',(-0.954362786820594,-36.5742356128,-8.62548528033089));
#65331=CARTESIAN_POINT('Ctrl Pts',(-0.973577822556822,-36.5742356128,-8.64976648561266));
#65332=CARTESIAN_POINT('Ctrl Pts',(-0.993824890950002,-36.5742356128,-8.67322601345517));
#65333=CARTESIAN_POINT('Ctrl Pts',(-1.01503616875631,-36.5742356128,-8.69582657056637));
#65334=CARTESIAN_POINT('Ctrl Pts',(-1.0434088924849,-36.5742356128,-8.72605762825577));
#65335=CARTESIAN_POINT('Ctrl Pts',(-1.07350815510844,-36.5742356128,-8.75475646899135));
#65336=CARTESIAN_POINT('Ctrl Pts',(-1.10513647482402,-36.5742356128,-8.78168472107411));
#65337=CARTESIAN_POINT('Ctrl Pts',(-1.13768537200219,-36.5742356128,-8.80939674991761));
#65338=CARTESIAN_POINT('Ctrl Pts',(-1.1718534896272,-36.5742356128,-8.83523358574093));
#65339=CARTESIAN_POINT('Ctrl Pts',(-1.20740369439064,-36.5742356128,-8.85898666122346));
#65340=CARTESIAN_POINT('Ctrl Pts',(-1.24369561876335,-36.5742356128,-8.88323532096443));
#65341=CARTESIAN_POINT('Ctrl Pts',(-1.2814276875808,-36.5742356128,-8.90531243574938));
#65342=CARTESIAN_POINT('Ctrl Pts',(-1.32032791047747,-36.5742356128,-8.92504834875626));
#65343=CARTESIAN_POINT('Ctrl Pts',(-1.36014940215674,-36.5742356128,-8.94525166475457));
#65344=CARTESIAN_POINT('Ctrl Pts',(-1.40119477440393,-36.5742356128,-8.96300167001931));
#65345=CARTESIAN_POINT('Ctrl Pts',(-1.44315545812899,-36.5742356128,-8.9781692782255));
#65346=CARTESIAN_POINT('Ctrl Pts',(-1.48624235752379,-36.5742356128,-8.99374398175327));
#65347=CARTESIAN_POINT('Ctrl Pts',(-1.53029404515485,-36.5742356128,-9.00659593404456));
#65348=CARTESIAN_POINT('Ctrl Pts',(-1.57496335937971,-36.5742356128,-9.01663882853403));
#65349=CARTESIAN_POINT('Ctrl Pts',(-1.62168047791899,-36.5742356128,-9.02714212594264));
#65350=CARTESIAN_POINT('Ctrl Pts',(-1.66907275594992,-36.5742356128,-9.03457295234747));
#65351=CARTESIAN_POINT('Ctrl Pts',(-1.71673443676159,-36.5742356128,-9.03888917782942));
#65352=CARTESIAN_POINT('Ctrl Pts',(-1.76580780739923,-36.5742356128,-9.04333324545826));
#65353=CARTESIAN_POINT('Ctrl Pts',(-1.8151662456494,-36.5742356128,-9.04447577049441));
#65354=CARTESIAN_POINT('Ctrl Pts',(-1.86436515483982,-36.5742356128,-9.04232661394204));
#65355=CARTESIAN_POINT('Ctrl Pts',(-1.9156186980022,-36.5742356128,-9.04008770478873));
#65356=CARTESIAN_POINT('Ctrl Pts',(-1.96669841756014,-36.5742356128,-9.03427676321613));
#65357=CARTESIAN_POINT('Ctrl Pts',(-2.01710937080252,-36.5742356128,-9.02496003509282));
#65358=CARTESIAN_POINT('Ctrl Pts',(-2.02081291067215,-36.5742356128,-9.02427556332945));
#65359=CARTESIAN_POINT('Ctrl Pts',(-2.02451284712871,-36.5742356128,-9.02357219170736));
#65360=CARTESIAN_POINT('Ctrl Pts',(-2.02820898712,-36.5742356128,-9.02284995679));
#65361=CARTESIAN_POINT('Ctrl Pts',(-2.02820898715,-37.9742356128,-9.02284995683));
#65362=CARTESIAN_POINT('Ctrl Pts',(-2.02820898715,-38.0684833924,-9.02284995683));
#65363=CARTESIAN_POINT('Ctrl Pts',(-2.03530687718,-38.162731172,-9.05917398875));
#65364=CARTESIAN_POINT('Ctrl Pts',(-2.0495930596,-38.2372245963,-9.13228469408));
#65365=CARTESIAN_POINT('Ctrl Pts',(-2.06766768814,-38.2742356128,-9.22478308183));
#65366=CARTESIAN_POINT('Ctrl Pts',(-2.08574231668,-38.2742356128,-9.3172814696));
#65367=CARTESIAN_POINT('Ctrl Pts',(-1.83318359957,-37.9742356128,-9.06095854776));
#65368=CARTESIAN_POINT('Ctrl Pts',(-1.83318360004,-38.0684833904,-9.06095854767));
#65369=CARTESIAN_POINT('Ctrl Pts',(-1.83376258883,-38.1627311679,-9.09855639141));
#65370=CARTESIAN_POINT('Ctrl Pts',(-1.83492595186,-38.2372245913,-9.17423135128));
#65371=CARTESIAN_POINT('Ctrl Pts',(-1.83639865331,-38.2742356096,-9.26997381923));
#65372=CARTESIAN_POINT('Ctrl Pts',(-1.83787135482,-38.2742356128,-9.36571628839));
#65373=CARTESIAN_POINT('Ctrl Pts',(-1.62996049743,-37.9742356128,-9.05518464578));
#65374=CARTESIAN_POINT('Ctrl Pts',(-1.62996053955,-38.068483395,-9.05518463237));
#65375=CARTESIAN_POINT('Ctrl Pts',(-1.62363224748,-38.1627311772,-9.09260850541));
#65376=CARTESIAN_POINT('Ctrl Pts',(-1.61089799618,-38.2372246026,-9.16793230913));
#65377=CARTESIAN_POINT('Ctrl Pts',(-1.59478556452,-38.2742356169,-9.26323093271));
#65378=CARTESIAN_POINT('Ctrl Pts',(-1.57867311595,-38.2742356128,-9.35852956011));
#65379=CARTESIAN_POINT('Ctrl Pts',(-1.43126328637,-37.9742356128,-9.0035760363));
#65380=CARTESIAN_POINT('Ctrl Pts',(-1.43126339204,-38.0684833845,-9.00357619207));
#65381=CARTESIAN_POINT('Ctrl Pts',(-1.41826547793,-38.1627311561,-9.03899098571));
#65382=CARTESIAN_POINT('Ctrl Pts',(-1.39210322077,-38.2372245775,-9.11027159813));
#65383=CARTESIAN_POINT('Ctrl Pts',(-1.35900343843,-38.2742356003,-9.20045442478));
#65384=CARTESIAN_POINT('Ctrl Pts',(-1.3259036101,-38.2742356128,-9.2906371902));
#65385=CARTESIAN_POINT('Ctrl Pts',(-1.07356983998,-37.9742356128,-8.81183251553));
#65386=CARTESIAN_POINT('Ctrl Pts',(-1.07356973553,-38.0684834003,-8.81183236157));
#65387=CARTESIAN_POINT('Ctrl Pts',(-1.04853912901,-38.1627311879,-8.84130344029));
#65388=CARTESIAN_POINT('Ctrl Pts',(-0.998159990023,-38.237224615,-8.90062099705));
#65389=CARTESIAN_POINT('Ctrl Pts',(-0.934420934844,-38.2742356252,-8.97566868954));
#65390=CARTESIAN_POINT('Ctrl Pts',(-0.870681925128,-38.2742356128,-9.05071644255));
#65391=CARTESIAN_POINT('Ctrl Pts',(-0.831386669736,-37.9742356128,-8.48987492086));
#65392=CARTESIAN_POINT('Ctrl Pts',(-0.831386772977,-38.0684833846,-8.48987507304));
#65393=CARTESIAN_POINT('Ctrl Pts',(-0.798242271358,-38.1627311564,-8.50804339173));
#65394=CARTESIAN_POINT('Ctrl Pts',(-0.731530250254,-38.2372245779,-8.54461138493));
#65395=CARTESIAN_POINT('Ctrl Pts',(-0.647127613959,-38.2742356006,-8.59087641987));
#65396=CARTESIAN_POINT('Ctrl Pts',(-0.562724932724,-38.2742356128,-8.63714139499));
#65397=CARTESIAN_POINT('Ctrl Pts',(-0.748943343284,-37.9742356128,-8.29926876182));
#65398=CARTESIAN_POINT('Ctrl Pts',(-0.748943241627,-38.0684834236,-8.29926864484));
#65399=CARTESIAN_POINT('Ctrl Pts',(-0.712958599203,-38.1627312344,-8.31224349504));
#65400=CARTESIAN_POINT('Ctrl Pts',(-0.640531165206,-38.2372246698,-8.33835860351));
#65401=CARTESIAN_POINT('Ctrl Pts',(-0.548897295487,-38.2742356618,-8.37139905011));
#65402=CARTESIAN_POINT('Ctrl Pts',(-0.457263484888,-38.2742356128,-8.40443954395));
#65403=CARTESIAN_POINT('Ctrl Pts',(-0.712043400129,-37.9742356128,-8.10864879918));
#65404=CARTESIAN_POINT('Ctrl Pts',(-0.712043400168,-38.0684833681,-8.10864879958));
#65405=CARTESIAN_POINT('Ctrl Pts',(-0.674879713076,-38.1627311233,-8.11345818589));
#65406=CARTESIAN_POINT('Ctrl Pts',(-0.600078971346,-38.2372245389,-8.12313820437));
#65407=CARTESIAN_POINT('Ctrl Pts',(-0.505442382683,-38.2742355746,-8.13538519743));
#65408=CARTESIAN_POINT('Ctrl Pts',(-0.410805778999,-38.2742356128,-8.14763218938));
#65409=CARTESIAN_POINT('Ctrl Pts',(-0.717751010187,-37.9742356128,-7.90915770911));
#65410=CARTESIAN_POINT('Ctrl Pts',(-0.717751010183,-38.0684833977,-7.90915770865));
#65411=CARTESIAN_POINT('Ctrl Pts',(-0.680755121224,-38.1627311826,-7.90809921391));
#65412=CARTESIAN_POINT('Ctrl Pts',(-0.606292144623,-38.2372246088,-7.90596874344));
#65413=CARTESIAN_POINT('Ctrl Pts',(-0.512082889029,-38.2742356211,-7.90327330976));
#65414=CARTESIAN_POINT('Ctrl Pts',(-0.417873636697,-38.2742356128,-7.90057787635));
#65415=CARTESIAN_POINT('Ctrl Pts',(-0.717273426056,-37.9742356128,-7.9495168227));
#65416=CARTESIAN_POINT('Ctrl Pts',(-0.719470863523,-37.9742356128,-8.33628951564));
#65417=CARTESIAN_POINT('Ctrl Pts',(-0.890959353803,-37.9742356128,-8.72278991704));
#65418=CARTESIAN_POINT('Ctrl Pts',(-1.23586688919,-37.9742356128,-9.00518418336));
#65419=CARTESIAN_POINT('Ctrl Pts',(-1.64860914359,-37.9742356128,-9.09702477361));
#65420=CARTESIAN_POINT('Ctrl Pts',(-2.02820898725,-37.9742356128,-9.02284995699));
#65421=CARTESIAN_POINT('Ctrl Pts',(-0.717273426056,-37.9742356128,-7.9495168227));
#65422=CARTESIAN_POINT('Ctrl Pts',(-0.717273426056,-36.2942356128,-7.9495168227));
#65423=CARTESIAN_POINT('Ctrl Pts',(-0.719470863523,-37.9742356128,-8.33628951564));
#65424=CARTESIAN_POINT('Ctrl Pts',(-0.719470863523,-36.2942356128,-8.33628951564));
#65425=CARTESIAN_POINT('Ctrl Pts',(-0.890959353803,-37.9742356128,-8.72278991704));
#65426=CARTESIAN_POINT('Ctrl Pts',(-0.890959353803,-36.2942356128,-8.72278991704));
#65427=CARTESIAN_POINT('Ctrl Pts',(-1.23586688919,-37.9742356128,-9.00518418336));
#65428=CARTESIAN_POINT('Ctrl Pts',(-1.23586688919,-36.2942356128,-9.00518418336));
#65429=CARTESIAN_POINT('Ctrl Pts',(-1.64860914359,-37.9742356128,-9.09702477361));
#65430=CARTESIAN_POINT('Ctrl Pts',(-1.64860914359,-36.2942356128,-9.09702477361));
#65431=CARTESIAN_POINT('Ctrl Pts',(-2.02820898725,-37.9742356128,-9.02284995699));
#65432=CARTESIAN_POINT('Ctrl Pts',(-2.02820898725,-36.2942356128,-9.02284995699));
#65433=CARTESIAN_POINT('Ctrl Pts',(-4.67800175618,-36.2742356128,1.76632657396));
#65434=CARTESIAN_POINT('Ctrl Pts',(-4.58800309105,-36.2742356128,1.79430664252));
#65435=CARTESIAN_POINT('Ctrl Pts',(-4.49800442593,-36.3112466293,1.82228671108));
#65436=CARTESIAN_POINT('Ctrl Pts',(-4.4268695008,-36.3857400536,1.84440215111));
#65437=CARTESIAN_POINT('Ctrl Pts',(-4.39152710765,-36.4799878332,1.85538989834));
#65438=CARTESIAN_POINT('Ctrl Pts',(-4.39152710765,-36.5742356128,1.85538989834));
#65439=CARTESIAN_POINT('Ctrl Pts',(-4.79388308266,-36.2742356128,2.13906206864));
#65440=CARTESIAN_POINT('Ctrl Pts',(-4.70258956167,-36.2742356128,2.16287719746));
#65441=CARTESIAN_POINT('Ctrl Pts',(-4.61129604067,-36.3112466293,2.18669232628));
#65442=CARTESIAN_POINT('Ctrl Pts',(-4.53913766232,-36.3857400536,2.20551579977));
#65443=CARTESIAN_POINT('Ctrl Pts',(-4.5032867799,-36.4799878332,2.21486797807));
#65444=CARTESIAN_POINT('Ctrl Pts',(-4.5032867799,-36.5742356128,2.21486797807));
#65445=CARTESIAN_POINT('Ctrl Pts',(-4.874573183,-36.2742356128,2.47604452564));
#65446=CARTESIAN_POINT('Ctrl Pts',(-4.78398140424,-36.2742356128,2.50204305306));
#65447=CARTESIAN_POINT('Ctrl Pts',(-4.69338962548,-36.3112466293,2.52804158049));
#65448=CARTESIAN_POINT('Ctrl Pts',(-4.62178590273,-36.3857400536,2.54859080965));
#65449=CARTESIAN_POINT('Ctrl Pts',(-4.58621059513,-36.4799878332,2.55880040869));
#65450=CARTESIAN_POINT('Ctrl Pts',(-4.58621059513,-36.5742356128,2.55880040869));
#65451=CARTESIAN_POINT('Ctrl Pts',(-4.98880289939,-36.2742356128,2.81842348726));
#65452=CARTESIAN_POINT('Ctrl Pts',(-4.89986264517,-36.2742356128,2.84961910006));
#65453=CARTESIAN_POINT('Ctrl Pts',(-4.81092239094,-36.3112466293,2.88081471287));
#65454=CARTESIAN_POINT('Ctrl Pts',(-4.74062403475,-36.3857400536,2.90547169884));
#65455=CARTESIAN_POINT('Ctrl Pts',(-4.70569727739,-36.4799878332,2.91772220687));
#65456=CARTESIAN_POINT('Ctrl Pts',(-4.70569727739,-36.5742356128,2.91772220687));
#65457=CARTESIAN_POINT('Ctrl Pts',(-5.24786437575,-36.2742356128,3.5327503947));
#65458=CARTESIAN_POINT('Ctrl Pts',(-5.15891348452,-36.2742356128,3.56414221201));
#65459=CARTESIAN_POINT('Ctrl Pts',(-5.06996259329,-36.3112466293,3.59553402932));
#65460=CARTESIAN_POINT('Ctrl Pts',(-4.99965582749,-36.3857400536,3.62034613592));
#65461=CARTESIAN_POINT('Ctrl Pts',(-4.96472489511,-36.4799878332,3.63267365265));
#65462=CARTESIAN_POINT('Ctrl Pts',(-4.96472489511,-36.5742356128,3.63267365265));
#65463=CARTESIAN_POINT('Ctrl Pts',(-5.46683572271,-36.2742356128,4.323032583));
#65464=CARTESIAN_POINT('Ctrl Pts',(-5.37431098316,-36.2742356128,4.342975072));
#65465=CARTESIAN_POINT('Ctrl Pts',(-5.2817862436,-36.3112466293,4.362917561));
#65466=CARTESIAN_POINT('Ctrl Pts',(-5.20865471042,-36.3857400536,4.37868007713));
#65467=CARTESIAN_POINT('Ctrl Pts',(-5.17232032954,-36.4799878332,4.38651149704));
#65468=CARTESIAN_POINT('Ctrl Pts',(-5.17232032954,-36.5742356128,4.38651149704));
#65469=CARTESIAN_POINT('Ctrl Pts',(-5.54455876033,-36.2742356128,4.75670536352));
#65470=CARTESIAN_POINT('Ctrl Pts',(-5.45006559684,-36.2742356128,4.7675841363));
#65471=CARTESIAN_POINT('Ctrl Pts',(-5.35557243336,-36.3112466293,4.77846290907));
#65472=CARTESIAN_POINT('Ctrl Pts',(-5.28088505457,-36.3857400536,4.78706157927));
#65473=CARTESIAN_POINT('Ctrl Pts',(-5.24377767918,-36.4799878332,4.79133357276));
#65474=CARTESIAN_POINT('Ctrl Pts',(-5.24377767918,-36.5742356128,4.79133357276));
#65475=CARTESIAN_POINT('Ctrl Pts',(-5.55370519489,-36.2742356128,5.19552744206));
#65476=CARTESIAN_POINT('Ctrl Pts',(-5.45936283056,-36.2742356128,5.19676129607));
#65477=CARTESIAN_POINT('Ctrl Pts',(-5.36502046622,-36.3112466293,5.19799515009));
#65478=CARTESIAN_POINT('Ctrl Pts',(-5.2904522842,-36.3857400536,5.19897032753));
#65479=CARTESIAN_POINT('Ctrl Pts',(-5.25340412236,-36.4799878332,5.19945492138));
#65480=CARTESIAN_POINT('Ctrl Pts',(-5.25340412236,-36.5742356128,5.19945492138));
#65481=CARTESIAN_POINT('Ctrl Pts',(-5.5398869008,-36.2742356128,5.60697988192));
#65482=CARTESIAN_POINT('Ctrl Pts',(-5.44569223012,-36.2742356128,5.60381634432));
#65483=CARTESIAN_POINT('Ctrl Pts',(-5.35149755944,-36.3112466293,5.60065280673));
#65484=CARTESIAN_POINT('Ctrl Pts',(-5.27704611245,-36.3857400536,5.59815234731));
#65485=CARTESIAN_POINT('Ctrl Pts',(-5.24005595177,-36.4799878332,5.596910029));
#65486=CARTESIAN_POINT('Ctrl Pts',(-5.24005595177,-36.5742356128,5.596910029));
#65487=CARTESIAN_POINT('',(-4.39149643123322,-36.5742356128,1.8552912333684));
#65488=CARTESIAN_POINT('Ctrl Pts',(-4.39152710765,-36.5742356128,1.85538989834));
#65489=CARTESIAN_POINT('Ctrl Pts',(-4.39152710765,-36.4799879394397,1.85538989834));
#65490=CARTESIAN_POINT('Ctrl Pts',(-4.42686942112142,-36.3857402660795,
1.84440217588161));
#65491=CARTESIAN_POINT('Ctrl Pts',(-4.49800418537203,-36.3112468812157,
1.82228678586809));
#65492=CARTESIAN_POINT('Ctrl Pts',(-4.58800268525026,-36.2742357796813,
1.79430676868081));
#65493=CARTESIAN_POINT('Ctrl Pts',(-4.67790730062965,-36.2742356128005,
1.76602456790413));
#65494=CARTESIAN_POINT('',(-5.24005595428587,-36.5742356128,5.59690998217945));
#65495=CARTESIAN_POINT('Origin',(-5.5377667962234,-36.5721143211971,5.60690896671464));
#65496=CARTESIAN_POINT('Ctrl Pts',(-4.39152710765,-36.5742356128,1.85538989834));
#65497=CARTESIAN_POINT('Ctrl Pts',(-4.43790342461,-36.5742356128,2.00456060571));
#65498=CARTESIAN_POINT('Ctrl Pts',(-4.47967500954,-36.5742356128,2.15155097868));
#65499=CARTESIAN_POINT('Ctrl Pts',(-4.51875357762,-36.5742356128,2.29074629422));
#65500=CARTESIAN_POINT('Ctrl Pts',(-4.62316453233,-36.5742356128,2.64995398242));
#65501=CARTESIAN_POINT('Ctrl Pts',(-4.7368681034,-36.5742356128,3.00222967269));
#65502=CARTESIAN_POINT('Ctrl Pts',(-4.81153097626,-36.5742356128,3.21707824382));
#65503=CARTESIAN_POINT('Ctrl Pts',(-5.00839926013,-36.5742356128,3.79030695886));
#65504=CARTESIAN_POINT('Ctrl Pts',(-5.17504642388,-36.5742356128,4.39981761668));
#65505=CARTESIAN_POINT('Ctrl Pts',(-5.24470483276,-36.5742356128,4.80219931419));
#65506=CARTESIAN_POINT('Ctrl Pts',(-5.25311376105,-36.5742356128,5.20808711269));
#65507=CARTESIAN_POINT('Ctrl Pts',(-5.2400559546,-36.5742356128,5.59690998219));
#65508=CARTESIAN_POINT('Ctrl Pts',(-5.24005597119,-37.9742356128,5.59690969873));
#65509=CARTESIAN_POINT('Ctrl Pts',(-5.24005597123,-38.0684833924,5.59690969762));
#65510=CARTESIAN_POINT('Ctrl Pts',(-5.27704612802,-38.162731172,5.59815213305));
#65511=CARTESIAN_POINT('Ctrl Pts',(-5.35149756715,-38.2372245963,5.60065282954));
#65512=CARTESIAN_POINT('Ctrl Pts',(-5.44569222786,-38.2742356128,5.60381666774));
#65513=CARTESIAN_POINT('Ctrl Pts',(-5.53988688857,-38.2742356128,5.60698050638));
#65514=CARTESIAN_POINT('Ctrl Pts',(-5.25247857027,-37.9742356128,5.22700723411));
#65515=CARTESIAN_POINT('Ctrl Pts',(-5.25247856712,-38.0684833932,5.22700731824));
#65516=CARTESIAN_POINT('Ctrl Pts',(-5.28952290833,-38.1627311736,5.22663645984));
#65517=CARTESIAN_POINT('Ctrl Pts',(-5.36408340703,-38.2372245982,5.22589001703));
#65518=CARTESIAN_POINT('Ctrl Pts',(-5.458416051,-38.2742356141,5.22494553728));
#65519=CARTESIAN_POINT('Ctrl Pts',(-5.55274869571,-38.2742356128,5.22400102455));
#65520=CARTESIAN_POINT('Ctrl Pts',(-5.24502230691,-37.9742356128,4.84784070798));
#65521=CARTESIAN_POINT('Ctrl Pts',(-5.24502231123,-38.0684833706,4.84784059887));
#65522=CARTESIAN_POINT('Ctrl Pts',(-5.28211738334,-38.1627311283,4.84408996285));
#65523=CARTESIAN_POINT('Ctrl Pts',(-5.35677998902,-38.2372245448,4.83654090413));
#65524=CARTESIAN_POINT('Ctrl Pts',(-5.45124181784,-38.2742355785,4.82699009502));
#65525=CARTESIAN_POINT('Ctrl Pts',(-5.54570365822,-38.2742356128,4.81743932663));
#65526=CARTESIAN_POINT('Ctrl Pts',(-5.18672938264,-37.9742356128,4.4719460563));
#65527=CARTESIAN_POINT('Ctrl Pts',(-5.1867294224,-38.0684834176,4.47194621772));
#65528=CARTESIAN_POINT('Ctrl Pts',(-5.22320733103,-38.1627312223,4.46483612118));
#65529=CARTESIAN_POINT('Ctrl Pts',(-5.29662769908,-38.2372246556,4.45052520587));
#65530=CARTESIAN_POINT('Ctrl Pts',(-5.3895178338,-38.2742356523,4.43241917655));
#65531=CARTESIAN_POINT('Ctrl Pts',(-5.4824079379,-38.2742356128,4.41431308756));
#65532=CARTESIAN_POINT('Ctrl Pts',(-4.99350448344,-37.9742356128,3.70895298504));
#65533=CARTESIAN_POINT('Ctrl Pts',(-4.99350444008,-38.068483365,3.70895280905));
#65534=CARTESIAN_POINT('Ctrl Pts',(-5.02859209909,-38.1627311172,3.69695602726));
#65535=CARTESIAN_POINT('Ctrl Pts',(-5.09921436755,-38.2372245317,3.67280984657));
#65536=CARTESIAN_POINT('Ctrl Pts',(-5.18856446387,-38.2742355698,3.64226063907));
#65537=CARTESIAN_POINT('Ctrl Pts',(-5.27791459357,-38.2742356128,3.61171149664));
#65538=CARTESIAN_POINT('Ctrl Pts',(-4.73234118526,-37.9742356128,2.99459752937));
#65539=CARTESIAN_POINT('Ctrl Pts',(-4.73234123253,-38.0684834223,2.99459772126));
#65540=CARTESIAN_POINT('Ctrl Pts',(-4.76713902192,-38.1627312318,2.98201159698));
#65541=CARTESIAN_POINT('Ctrl Pts',(-4.83717774109,-38.2372246668,2.95667884794));
#65542=CARTESIAN_POINT('Ctrl Pts',(-4.92578946733,-38.2742356598,2.92462816718));
#65543=CARTESIAN_POINT('Ctrl Pts',(-5.01440115718,-38.2742356128,2.89257741547));
#65544=CARTESIAN_POINT('Ctrl Pts',(-4.59818751884,-37.9742356128,2.61020157177));
#65545=CARTESIAN_POINT('Ctrl Pts',(-4.59818738771,-38.0684833728,2.61020114916));
#65546=CARTESIAN_POINT('Ctrl Pts',(-4.63371504264,-38.1627311328,2.5997905378));
#65547=CARTESIAN_POINT('Ctrl Pts',(-4.70522301975,-38.2372245501,2.57883726165));
#65548=CARTESIAN_POINT('Ctrl Pts',(-4.79569374678,-38.274235582,2.55232778505));
#65549=CARTESIAN_POINT('Ctrl Pts',(-4.88616453703,-38.2742356128,2.52581847142));
#65550=CARTESIAN_POINT('Ctrl Pts',(-4.51145651853,-37.9742356128,2.24114616857));
#65551=CARTESIAN_POINT('Ctrl Pts',(-4.51145651853,-38.0684833924,2.24114616857));
#65552=CARTESIAN_POINT('Ctrl Pts',(-4.54734457339,-38.1627311721,2.23191355632));
#65553=CARTESIAN_POINT('Ctrl Pts',(-4.61957776562,-38.2372245963,2.21333072384));
#65554=CARTESIAN_POINT('Ctrl Pts',(-4.71096594196,-38.2742356128,2.18982005656));
#65555=CARTESIAN_POINT('Ctrl Pts',(-4.80235411815,-38.2742356128,2.16630938881));
#65556=CARTESIAN_POINT('Ctrl Pts',(-4.39152710765,-37.9742356128,1.85538989834));
#65557=CARTESIAN_POINT('Ctrl Pts',(-4.39152710765,-38.0684833924,1.85538989834));
#65558=CARTESIAN_POINT('Ctrl Pts',(-4.4268695008,-38.1627311721,1.84440215111));
#65559=CARTESIAN_POINT('Ctrl Pts',(-4.49800442593,-38.2372245963,1.82228671108));
#65560=CARTESIAN_POINT('Ctrl Pts',(-4.58800309105,-38.2742356128,1.79430664252));
#65561=CARTESIAN_POINT('Ctrl Pts',(-4.67800175618,-38.2742356128,1.76632657396));
#65562=CARTESIAN_POINT('',(-4.39147468411897,-37.9742356128,1.85522128783252));
#65563=CARTESIAN_POINT('Ctrl Pts',(-4.67790746367798,-38.2742356127995,
1.76602510278827));
#65564=CARTESIAN_POINT('Ctrl Pts',(-4.58800268668313,-38.274235446508,1.79430676823534));
#65565=CARTESIAN_POINT('Ctrl Pts',(-4.49800418622144,-38.2372243452739,
1.82228678560402));
#65566=CARTESIAN_POINT('Ctrl Pts',(-4.42686942140277,-38.1627309603708,
1.84440217579414));
#65567=CARTESIAN_POINT('Ctrl Pts',(-4.39152710765,-38.0684832865354,1.85538989834));
#65568=CARTESIAN_POINT('Ctrl Pts',(-4.39152710765,-37.9742356128,1.85538989834));
#65569=CARTESIAN_POINT('',(-5.2400559546,-37.9742356128,5.59690998219));
#65570=CARTESIAN_POINT('Ctrl Pts',(-4.39152710765,-37.9742356128,1.85538989834));
#65571=CARTESIAN_POINT('Ctrl Pts',(-4.43790342461,-37.9742356128,2.00456060571));
#65572=CARTESIAN_POINT('Ctrl Pts',(-4.47967500954,-37.9742356128,2.15155097868));
#65573=CARTESIAN_POINT('Ctrl Pts',(-4.51875357762,-37.9742356128,2.29074629422));
#65574=CARTESIAN_POINT('Ctrl Pts',(-4.62316453233,-37.9742356128,2.64995398242));
#65575=CARTESIAN_POINT('Ctrl Pts',(-4.7368681034,-37.9742356128,3.00222967269));
#65576=CARTESIAN_POINT('Ctrl Pts',(-4.81153097626,-37.9742356128,3.21707824382));
#65577=CARTESIAN_POINT('Ctrl Pts',(-5.00839926013,-37.9742356128,3.79030695886));
#65578=CARTESIAN_POINT('Ctrl Pts',(-5.17504642388,-37.9742356128,4.39981761668));
#65579=CARTESIAN_POINT('Ctrl Pts',(-5.24470483276,-37.9742356128,4.80219931419));
#65580=CARTESIAN_POINT('Ctrl Pts',(-5.25311376105,-37.9742356128,5.20808711269));
#65581=CARTESIAN_POINT('Ctrl Pts',(-5.2400559546,-37.9742356128,5.59690998219));
#65582=CARTESIAN_POINT('Origin',(-5.5377667758297,-37.9763568898754,5.60691012513041));
#65583=CARTESIAN_POINT('Ctrl Pts',(-4.39143626758763,-37.9742356128,1.8550977087646));
#65584=CARTESIAN_POINT('Ctrl Pts',(-4.39143626758763,-36.2942356128,1.8550977087646));
#65585=CARTESIAN_POINT('Ctrl Pts',(-4.3914544356001,-37.9742356128,1.85515614667968));
#65586=CARTESIAN_POINT('Ctrl Pts',(-4.3914544356001,-36.2942356128,1.85515614667968));
#65587=CARTESIAN_POINT('Ctrl Pts',(-4.39147260361258,-37.9742356128,1.85521458459476));
#65588=CARTESIAN_POINT('Ctrl Pts',(-4.39147260361258,-36.2942356128,1.85521458459476));
#65589=CARTESIAN_POINT('Ctrl Pts',(-4.39149077162505,-37.9742356128,1.85527302250984));
#65590=CARTESIAN_POINT('Ctrl Pts',(-4.39149077162505,-36.2942356128,1.85527302250984));
#65591=CARTESIAN_POINT('Ctrl Pts',(-4.39150893963753,-37.9742356128,1.85533146042492));
#65592=CARTESIAN_POINT('Ctrl Pts',(-4.39150893963753,-36.2942356128,1.85533146042492));
#65593=CARTESIAN_POINT('Ctrl Pts',(-4.39152710765,-37.9742356128,1.85538989834));
#65594=CARTESIAN_POINT('Ctrl Pts',(-4.39152710765,-36.2942356128,1.85538989834));
#65595=CARTESIAN_POINT('Ctrl Pts',(-4.43790342461,-37.9742356128,2.00456060571));
#65596=CARTESIAN_POINT('Ctrl Pts',(-4.43790342461,-36.2942356128,2.00456060571));
#65597=CARTESIAN_POINT('Ctrl Pts',(-4.47967500954,-37.9742356128,2.15155097868));
#65598=CARTESIAN_POINT('Ctrl Pts',(-4.47967500954,-36.2942356128,2.15155097868));
#65599=CARTESIAN_POINT('Ctrl Pts',(-4.51875357762,-37.9742356128,2.29074629422));
#65600=CARTESIAN_POINT('Ctrl Pts',(-4.51875357762,-36.2942356128,2.29074629422));
#65601=CARTESIAN_POINT('Ctrl Pts',(-4.62316453233,-37.9742356128,2.64995398242));
#65602=CARTESIAN_POINT('Ctrl Pts',(-4.62316453233,-36.2942356128,2.64995398242));
#65603=CARTESIAN_POINT('Ctrl Pts',(-4.7368681034,-37.9742356128,3.00222967269));
#65604=CARTESIAN_POINT('Ctrl Pts',(-4.7368681034,-36.2942356128,3.00222967269));
#65605=CARTESIAN_POINT('Ctrl Pts',(-4.81153097626,-37.9742356128,3.21707824382));
#65606=CARTESIAN_POINT('Ctrl Pts',(-4.81153097626,-36.2942356128,3.21707824382));
#65607=CARTESIAN_POINT('Ctrl Pts',(-5.00839926013,-37.9742356128,3.79030695886));
#65608=CARTESIAN_POINT('Ctrl Pts',(-5.00839926013,-36.2942356128,3.79030695886));
#65609=CARTESIAN_POINT('Ctrl Pts',(-5.17504642388,-37.9742356128,4.39981761668));
#65610=CARTESIAN_POINT('Ctrl Pts',(-5.17504642388,-36.2942356128,4.39981761668));
#65611=CARTESIAN_POINT('Ctrl Pts',(-5.24470483276,-37.9742356128,4.80219931419));
#65612=CARTESIAN_POINT('Ctrl Pts',(-5.24470483276,-36.2942356128,4.80219931419));
#65613=CARTESIAN_POINT('Ctrl Pts',(-5.25311376105,-37.9742356128,5.20808711269));
#65614=CARTESIAN_POINT('Ctrl Pts',(-5.25311376105,-36.2942356128,5.20808711269));
#65615=CARTESIAN_POINT('Ctrl Pts',(-5.2400559546,-37.9742356128,5.59690998219));
#65616=CARTESIAN_POINT('Ctrl Pts',(-5.2400559546,-36.2942356128,5.59690998219));
#65617=CARTESIAN_POINT('',(-4.39143626207,-37.2742356128,1.85509771048));
#65618=CARTESIAN_POINT('',(-5.2400559546,-37.2742356128,5.59690998219));
#65619=CARTESIAN_POINT('Ctrl Pts',(-5.53988692571,-36.2742356128,5.60697918103));
#65620=CARTESIAN_POINT('Ctrl Pts',(-5.4456922481,-36.2742356128,5.60381584892));
#65621=CARTESIAN_POINT('Ctrl Pts',(-5.35149757048,-36.3112466293,5.60065251681));
#65622=CARTESIAN_POINT('Ctrl Pts',(-5.277046118,-36.3857400536,5.59815221981));
#65623=CARTESIAN_POINT('Ctrl Pts',(-5.2400559546,-36.4799878332,5.59690998219));
#65624=CARTESIAN_POINT('Ctrl Pts',(-5.2400559546,-36.5742356128,5.59690998219));
#65625=CARTESIAN_POINT('Ctrl Pts',(-5.51566436809,-36.2742356128,6.32825533085));
#65626=CARTESIAN_POINT('Ctrl Pts',(-5.42188047368,-36.2742356128,6.31286008937));
#65627=CARTESIAN_POINT('Ctrl Pts',(-5.32809657928,-36.3112466293,6.29746484788));
#65628=CARTESIAN_POINT('Ctrl Pts',(-5.25396980975,-36.3857400536,6.28529645234));
#65629=CARTESIAN_POINT('Ctrl Pts',(-5.21714096054,-36.4799878332,6.27925075521));
#65630=CARTESIAN_POINT('Ctrl Pts',(-5.21714096054,-36.5742356128,6.27925075521));
#65631=CARTESIAN_POINT('Ctrl Pts',(-5.37435587484,-36.2742356128,7.04580159469));
#65632=CARTESIAN_POINT('Ctrl Pts',(-5.28297016404,-36.2742356128,7.01818508491));
#65633=CARTESIAN_POINT('Ctrl Pts',(-5.19158445325,-36.3112466293,6.99056857513));
#65634=CARTESIAN_POINT('Ctrl Pts',(-5.11935320751,-36.3857400536,6.96874049199));
#65635=CARTESIAN_POINT('Ctrl Pts',(-5.08346612282,-36.4799878332,6.95789551384));
#65636=CARTESIAN_POINT('Ctrl Pts',(-5.08346612282,-36.5742356128,6.95789551384));
#65637=CARTESIAN_POINT('Ctrl Pts',(-5.11602160615,-36.2742356128,7.73361379617));
#65638=CARTESIAN_POINT('Ctrl Pts',(-5.02905151582,-36.2742356128,7.69427724615));
#65639=CARTESIAN_POINT('Ctrl Pts',(-4.94208142549,-36.3112466293,7.65494069614));
#65640=CARTESIAN_POINT('Ctrl Pts',(-4.87334027673,-36.3857400536,7.6238490956));
#65641=CARTESIAN_POINT('Ctrl Pts',(-4.83918721061,-36.4799878332,7.60840166858));
#65642=CARTESIAN_POINT('Ctrl Pts',(-4.83918721061,-36.5742356128,7.60840166858));
#65643=CARTESIAN_POINT('Ctrl Pts',(-4.25296434,-36.2742356128,9.22903839862));
#65644=CARTESIAN_POINT('Ctrl Pts',(-4.1806520628,-36.2742356128,9.16427735215));
#65645=CARTESIAN_POINT('Ctrl Pts',(-4.10833978559,-36.3112466293,9.09951630568));
#65646=CARTESIAN_POINT('Ctrl Pts',(-4.05118418906,-36.3857400536,9.04832918894));
#65647=CARTESIAN_POINT('Ctrl Pts',(-4.02278721273,-36.4799878332,9.02289758531));
#65648=CARTESIAN_POINT('Ctrl Pts',(-4.02278721273,-36.5742356128,9.02289758531));
#65649=CARTESIAN_POINT('Ctrl Pts',(-2.88301385607,-36.2742356128,10.310599153));
#65650=CARTESIAN_POINT('Ctrl Pts',(-2.83398118867,-36.2742356128,10.2274899849));
#65651=CARTESIAN_POINT('Ctrl Pts',(-2.78494852128,-36.3112466293,10.1443808169));
#65652=CARTESIAN_POINT('Ctrl Pts',(-2.74619309625,-36.3857400536,10.0786913484));
#65653=CARTESIAN_POINT('Ctrl Pts',(-2.7269380283,-36.4799878332,10.0460544548));
#65654=CARTESIAN_POINT('Ctrl Pts',(-2.7269380283,-36.5742356128,10.0460544548));
#65655=CARTESIAN_POINT('Ctrl Pts',(-1.96549293319,-36.2742356128,10.7471218767));
#65656=CARTESIAN_POINT('Ctrl Pts',(-1.93197492963,-36.2742356128,10.6565618655));
#65657=CARTESIAN_POINT('Ctrl Pts',(-1.89845692606,-36.3112466293,10.5660018543));
#65658=CARTESIAN_POINT('Ctrl Pts',(-1.87196436596,-36.3857400536,10.4944232419));
#65659=CARTESIAN_POINT('Ctrl Pts',(-1.85880181419,-36.4799878332,10.4588604081));
#65660=CARTESIAN_POINT('Ctrl Pts',(-1.85880181419,-36.5742356128,10.4588604081));
#65661=CARTESIAN_POINT('Ctrl Pts',(-0.9824065633,-36.2742356128,10.9642669745));
#65662=CARTESIAN_POINT('Ctrl Pts',(-0.965785252294,-36.2742356128,10.8700205667));
#65663=CARTESIAN_POINT('Ctrl Pts',(-0.949163941288,-36.3112466293,10.7757741588));
#65664=CARTESIAN_POINT('Ctrl Pts',(-0.936026419048,-36.3857400536,10.7012818184));
#65665=CARTESIAN_POINT('Ctrl Pts',(-0.929499287155,-36.4799878332,10.664271341));
#65666=CARTESIAN_POINT('Ctrl Pts',(-0.929499287155,-36.5742356128,10.664271341));
#65667=CARTESIAN_POINT('Ctrl Pts',(-2.46701990947E-5,-36.2742356128,10.9643459861));
#65668=CARTESIAN_POINT('Ctrl Pts',(-1.69198316304E-5,-36.2742356128,10.8700982068));
#65669=CARTESIAN_POINT('Ctrl Pts',(-9.16946416574E-6,-36.3112466293,10.7758504274));
#65670=CARTESIAN_POINT('Ctrl Pts',(-3.04357542591E-6,-36.3857400536,10.7013570034));
#65671=CARTESIAN_POINT('Ctrl Pts',(-1.32396316133E-11,-36.4799878332,10.664345987));
#65672=CARTESIAN_POINT('Ctrl Pts',(-1.32396316133E-11,-36.5742356128,10.664345987));
#65673=CARTESIAN_POINT('',(3.21923099319093E-10,-36.5742356128,10.66434598565));
#65674=CARTESIAN_POINT('Origin',(-5.43957144643002E-5,-36.5721143038111,
10.9622246741472));
#65675=CARTESIAN_POINT('Ctrl Pts',(-5.2400559546,-36.5742356128,5.59690998219));
#65676=CARTESIAN_POINT('Ctrl Pts',(-5.18595136098,-36.5742356128,7.20798481558));
#65677=CARTESIAN_POINT('Ctrl Pts',(-4.51434339457,-36.5742356128,8.79964985146));
#65678=CARTESIAN_POINT('Ctrl Pts',(-3.22524412625,-36.5742356128,10.0462831132));
#65679=CARTESIAN_POINT('Ctrl Pts',(-1.61198306736,-36.5742356128,10.6642180635));
#65680=CARTESIAN_POINT('Ctrl Pts',(-8.881784197E-16,-36.5742356128,10.664345987));
#65681=CARTESIAN_POINT('Ctrl Pts',(2.47493525452E-10,-37.9742356128,10.6643459881));
#65682=CARTESIAN_POINT('Ctrl Pts',(2.51954845654E-10,-38.0684833924,10.6643459881));
#65683=CARTESIAN_POINT('Ctrl Pts',(-2.95195493277E-6,-38.1627311721,10.7013570045));
#65684=CARTESIAN_POINT('Ctrl Pts',(-8.89397497965E-6,-38.2372245963,10.7758504286));
#65685=CARTESIAN_POINT('Ctrl Pts',(-1.64117176949E-5,-38.2742356128,10.8700982079));
#65686=CARTESIAN_POINT('Ctrl Pts',(-2.39294621618E-5,-38.2742356128,10.9643459873));
#65687=CARTESIAN_POINT('Ctrl Pts',(-0.781410362137,-37.9742356128,10.6642834957));
#65688=CARTESIAN_POINT('Ctrl Pts',(-0.781410363148,-38.068483393,10.6642834957));
#65689=CARTESIAN_POINT('Ctrl Pts',(-0.786907976509,-38.1627311731,10.7012940655));
#65690=CARTESIAN_POINT('Ctrl Pts',(-0.797973495794,-38.2372245975,10.7757865915));
#65691=CARTESIAN_POINT('Ctrl Pts',(-0.811973282143,-38.2742356136,10.8700332341));
#65692=CARTESIAN_POINT('Ctrl Pts',(-0.8259730681,-38.2742356128,10.9642798764));
#65693=CARTESIAN_POINT('Ctrl Pts',(-1.56278771434,-37.9742356128,10.5190720913));
#65694=CARTESIAN_POINT('Ctrl Pts',(-1.56278775086,-38.0684833913,10.5190720271));
#65695=CARTESIAN_POINT('Ctrl Pts',(-1.57383244467,-38.1627311698,10.5550601671));
#65696=CARTESIAN_POINT('Ctrl Pts',(-1.59606204838,-38.2372245937,10.6274948874));
#65697=CARTESIAN_POINT('Ctrl Pts',(-1.6241867049,-38.2742356111,10.7191380707));
#65698=CARTESIAN_POINT('Ctrl Pts',(-1.65231134708,-38.2742356128,10.8107812798));
#65699=CARTESIAN_POINT('Ctrl Pts',(-2.30773304724,-37.9742356128,10.2275491754));
#65700=CARTESIAN_POINT('Ctrl Pts',(-2.3077327816,-38.0684833927,10.2275493948));
#65701=CARTESIAN_POINT('Ctrl Pts',(-2.32403298045,-38.1627311726,10.2614708417));
#65702=CARTESIAN_POINT('Ctrl Pts',(-2.3568414097,-38.237224597,10.3297456012));
#65703=CARTESIAN_POINT('Ctrl Pts',(-2.39835018111,-38.2742356133,10.4161254622));
#65704=CARTESIAN_POINT('Ctrl Pts',(-2.43985905679,-38.2742356128,10.5025052368));
#65705=CARTESIAN_POINT('Ctrl Pts',(-3.69592891366,-37.9742356128,9.354903989));
#65706=CARTESIAN_POINT('Ctrl Pts',(-3.69592919608,-38.0684833921,9.35490375571));
#65707=CARTESIAN_POINT('Ctrl Pts',(-3.72202345283,-38.1627311714,9.38267044843));
#65708=CARTESIAN_POINT('Ctrl Pts',(-3.77454386522,-38.2372245956,9.43855767121));
#65709=CARTESIAN_POINT('Ctrl Pts',(-3.84099164681,-38.2742356124,9.50926539283));
#65710=CARTESIAN_POINT('Ctrl Pts',(-3.90743931755,-38.2742356128,9.57997320631));
#65711=CARTESIAN_POINT('Ctrl Pts',(-4.66459380705,-37.9742356128,8.0273898467));
#65712=CARTESIAN_POINT('Ctrl Pts',(-4.66459350678,-38.0684833928,8.02739009474));
#65713=CARTESIAN_POINT('Ctrl Pts',(-4.69751121102,-38.1627311727,8.04579864842));
#65714=CARTESIAN_POINT('Ctrl Pts',(-4.76376635599,-38.2372245971,8.08285001799));
#65715=CARTESIAN_POINT('Ctrl Pts',(-4.84759134344,-38.2742356134,8.12972656905));
#65716=CARTESIAN_POINT('Ctrl Pts',(-4.93141644876,-38.2742356128,8.17660302246));
#65717=CARTESIAN_POINT('Ctrl Pts',(-5.02028636901,-37.9742356128,7.25209197216));
#65718=CARTESIAN_POINT('Ctrl Pts',(-5.02028638981,-38.0684833959,7.25209217123));
#65719=CARTESIAN_POINT('Ctrl Pts',(-5.05572819588,-38.162731179,7.26502088603));
#65720=CARTESIAN_POINT('Ctrl Pts',(-5.12706320165,-38.2372246045,7.29104232124));
#65721=CARTESIAN_POINT('Ctrl Pts',(-5.21731498541,-38.2742356183,7.32396424097));
#65722=CARTESIAN_POINT('Ctrl Pts',(-5.30756675884,-38.2742356128,7.35688608211));
#65723=CARTESIAN_POINT('Ctrl Pts',(-5.21217205227,-37.9742356128,6.4272101526));
#65724=CARTESIAN_POINT('Ctrl Pts',(-5.21217205227,-38.0684833924,6.4272101526));
#65725=CARTESIAN_POINT('Ctrl Pts',(-5.24896592505,-38.1627311721,6.43429734393));
#65726=CARTESIAN_POINT('Ctrl Pts',(-5.32302228695,-38.2372245964,6.44856227116));
#65727=CARTESIAN_POINT('Ctrl Pts',(-5.41671710674,-38.2742356128,6.46660989106));
#65728=CARTESIAN_POINT('Ctrl Pts',(-5.51041192654,-38.2742356128,6.48465751096));
#65729=CARTESIAN_POINT('Ctrl Pts',(-5.2400559546,-37.9742356128,5.59690998219));
#65730=CARTESIAN_POINT('Ctrl Pts',(-5.2400559546,-38.0684833924,5.59690998219));
#65731=CARTESIAN_POINT('Ctrl Pts',(-5.277046118,-38.1627311721,5.59815221981));
#65732=CARTESIAN_POINT('Ctrl Pts',(-5.35149757048,-38.2372245963,5.60065251681));
#65733=CARTESIAN_POINT('Ctrl Pts',(-5.4456922481,-38.2742356128,5.60381584892));
#65734=CARTESIAN_POINT('Ctrl Pts',(-5.53988692571,-38.2742356128,5.60697918103));
#65735=CARTESIAN_POINT('',(1.72248049157275E-10,-37.9742356128,10.6643459863));
#65736=CARTESIAN_POINT('Ctrl Pts',(-5.2400559546,-37.9742356128,5.59690998219));
#65737=CARTESIAN_POINT('Ctrl Pts',(-5.18595136098,-37.9742356128,7.20798481558));
#65738=CARTESIAN_POINT('Ctrl Pts',(-4.51434339457,-37.9742356128,8.79964985146));
#65739=CARTESIAN_POINT('Ctrl Pts',(-3.22524412625,-37.9742356128,10.0462831132));
#65740=CARTESIAN_POINT('Ctrl Pts',(-1.61198306736,-37.9742356128,10.6642180635));
#65741=CARTESIAN_POINT('Ctrl Pts',(-8.881784197E-16,-37.9742356128,10.664345987));
#65742=CARTESIAN_POINT('Ctrl Pts',(-2.39294567467071E-5,-38.2742356128,
10.9643459746877));
#65743=CARTESIAN_POINT('Ctrl Pts',(1.65351811779069E-5,-38.2742356089377,
10.8700981935102));
#65744=CARTESIAN_POINT('Ctrl Pts',(8.96134118167951E-6,-38.2372245904188,
10.7758504184188));
#65745=CARTESIAN_POINT('Ctrl Pts',(2.97497562388355E-6,-38.1627311670551,
10.7013569985189));
#65746=CARTESIAN_POINT('Ctrl Pts',(7.28328000219216E-10,-38.0684833899775,
10.6643459842));
#65747=CARTESIAN_POINT('Ctrl Pts',(-8.881784197E-16,-37.9742356128,10.664345987));
#65748=CARTESIAN_POINT('Ctrl Pts',(-5.2400559546,-37.9742356128,5.59690998219));
#65749=CARTESIAN_POINT('Ctrl Pts',(-5.2400559546,-36.2942356128,5.59690998219));
#65750=CARTESIAN_POINT('Ctrl Pts',(-5.18595136098,-37.9742356128,7.20798481558));
#65751=CARTESIAN_POINT('Ctrl Pts',(-5.18595136098,-36.2942356128,7.20798481558));
#65752=CARTESIAN_POINT('Ctrl Pts',(-4.51434339457,-37.9742356128,8.79964985146));
#65753=CARTESIAN_POINT('Ctrl Pts',(-4.51434339457,-36.2942356128,8.79964985146));
#65754=CARTESIAN_POINT('Ctrl Pts',(-3.22524412625,-37.9742356128,10.0462831132));
#65755=CARTESIAN_POINT('Ctrl Pts',(-3.22524412625,-36.2942356128,10.0462831132));
#65756=CARTESIAN_POINT('Ctrl Pts',(-1.61198306736,-37.9742356128,10.6642180635));
#65757=CARTESIAN_POINT('Ctrl Pts',(-1.61198306736,-36.2942356128,10.6642180635));
#65758=CARTESIAN_POINT('Ctrl Pts',(1.22124532709E-15,-37.9742356128,10.664345987));
#65759=CARTESIAN_POINT('Ctrl Pts',(1.22124532709E-15,-36.2942356128,10.664345987));
#65760=CARTESIAN_POINT('',(-4.4408920985E-16,-37.2742356128,10.664345987));
#65761=CARTESIAN_POINT('Ctrl Pts',(2.32481332798E-5,-36.2742356128,10.9643459795));
#65762=CARTESIAN_POINT('Ctrl Pts',(1.59449213495E-5,-36.2742356128,10.8700982006));
#65763=CARTESIAN_POINT('Ctrl Pts',(8.64170941739E-6,-36.3112466293,10.7758504216));
#65764=CARTESIAN_POINT('Ctrl Pts',(2.86925231308E-6,-36.3857400536,10.7013569978));
#65765=CARTESIAN_POINT('Ctrl Pts',(1.2876946176E-9,-36.4799878332,10.6643459816));
#65766=CARTESIAN_POINT('Ctrl Pts',(1.2876946176E-9,-36.5742356128,10.6643459816));
#65767=CARTESIAN_POINT('Ctrl Pts',(0.852036142414,-36.2742356128,10.9642783046));
#65768=CARTESIAN_POINT('Ctrl Pts',(0.837609587463,-36.2742356128,10.8700316767));
#65769=CARTESIAN_POINT('Ctrl Pts',(0.823183032512,-36.3112466293,10.7757850489));
#65770=CARTESIAN_POINT('Ctrl Pts',(0.811780239059,-36.3857400536,10.7012925346));
#65771=CARTESIAN_POINT('Ctrl Pts',(0.806114991769,-36.4799878332,10.6642819707));
#65772=CARTESIAN_POINT('Ctrl Pts',(0.806114991769,-36.5742356128,10.6642819707));
#65773=CARTESIAN_POINT('Ctrl Pts',(1.70453832905,-36.2742356128,10.8009343674));
#65774=CARTESIAN_POINT('Ctrl Pts',(1.6754994877,-36.2742356128,10.7094585914));
#65775=CARTESIAN_POINT('Ctrl Pts',(1.64646064634,-36.3112466293,10.6179828154));
#65776=CARTESIAN_POINT('Ctrl Pts',(1.62350842394,-36.3857400536,10.5456803825));
#65777=CARTESIAN_POINT('Ctrl Pts',(1.61210482618,-36.4799878332,10.5097579288));
#65778=CARTESIAN_POINT('Ctrl Pts',(1.61210482618,-36.5742356128,10.5097579288));
#65779=CARTESIAN_POINT('Ctrl Pts',(2.51436099301,-36.2742356128,10.4728151835));
#65780=CARTESIAN_POINT('Ctrl Pts',(2.47159007241,-36.2742356128,10.3869496626));
#65781=CARTESIAN_POINT('Ctrl Pts',(2.42881915182,-36.3112466293,10.3010841417));
#65782=CARTESIAN_POINT('Ctrl Pts',(2.39501300852,-36.3857400536,10.2332160276));
#65783=CARTESIAN_POINT('Ctrl Pts',(2.37821692435,-36.4799878332,10.1994967416));
#65784=CARTESIAN_POINT('Ctrl Pts',(2.37821692435,-36.5742356128,10.1994967416));
#65785=CARTESIAN_POINT('Ctrl Pts',(3.9668324501,-36.2742356128,9.52325772634));
#65786=CARTESIAN_POINT('Ctrl Pts',(3.89937291488,-36.2742356128,9.45350328533));
#65787=CARTESIAN_POINT('Ctrl Pts',(3.83191337967,-36.3112466293,9.38374884432));
#65788=CARTESIAN_POINT('Ctrl Pts',(3.77859339503,-36.3857400536,9.32861497459));
#65789=CARTESIAN_POINT('Ctrl Pts',(3.75210208034,-36.4799878332,9.30122244455));
#65790=CARTESIAN_POINT('Ctrl Pts',(3.75210208034,-36.5742356128,9.30122244455));
#65791=CARTESIAN_POINT('Ctrl Pts',(4.96450063028,-36.2742356128,8.10336572511));
#65792=CARTESIAN_POINT('Ctrl Pts',(4.88011657299,-36.2742356128,8.05774290187));
#65793=CARTESIAN_POINT('Ctrl Pts',(4.7957325157,-36.3112466293,8.01212007863));
#65794=CARTESIAN_POINT('Ctrl Pts',(4.72903535812,-36.3857400536,7.97605978415));
#65795=CARTESIAN_POINT('Ctrl Pts',(4.69589783357,-36.4799878332,7.95814376839));
#65796=CARTESIAN_POINT('Ctrl Pts',(4.69589783357,-36.5742356128,7.95814376839));
#65797=CARTESIAN_POINT('Ctrl Pts',(5.31945709196,-36.2742356128,7.30507701677));
#65798=CARTESIAN_POINT('Ctrl Pts',(5.22900416127,-36.2742356128,7.27301018271));
#65799=CARTESIAN_POINT('Ctrl Pts',(5.13855123059,-36.3112466293,7.24094334865));
#65800=CARTESIAN_POINT('Ctrl Pts',(5.06705725129,-36.3857400536,7.21559783004));
#65801=CARTESIAN_POINT('Ctrl Pts',(5.03153647124,-36.4799878332,7.20300511378));
#65802=CARTESIAN_POINT('Ctrl Pts',(5.03153647124,-36.5742356128,7.20300511378));
#65803=CARTESIAN_POINT('Ctrl Pts',(5.51128814508,-36.2742356128,6.45856839125));
#65804=CARTESIAN_POINT('Ctrl Pts',(5.41757775177,-36.2742356128,6.44098444573));
#65805=CARTESIAN_POINT('Ctrl Pts',(5.32386735846,-36.3112466293,6.4234005002));
#65806=CARTESIAN_POINT('Ctrl Pts',(5.24979868601,-36.3857400536,6.40950208689));
#65807=CARTESIAN_POINT('Ctrl Pts',(5.21299869879,-36.4799878332,6.40259695426));
#65808=CARTESIAN_POINT('Ctrl Pts',(5.21299869879,-36.5742356128,6.40259695426));
#65809=CARTESIAN_POINT('Ctrl Pts',(5.53988691225,-36.2742356128,5.60697948238));
#65810=CARTESIAN_POINT('Ctrl Pts',(5.44569223796,-36.2742356128,5.60381605578));
#65811=CARTESIAN_POINT('Ctrl Pts',(5.35149756366,-36.3112466293,5.60065262919));
#65812=CARTESIAN_POINT('Ctrl Pts',(5.27704611381,-36.3857400536,5.5981522575));
#65813=CARTESIAN_POINT('Ctrl Pts',(5.24005595171,-36.4799878332,5.59690998278));
#65814=CARTESIAN_POINT('Ctrl Pts',(5.24005595171,-36.5742356128,5.59690998278));
#65815=CARTESIAN_POINT('',(5.2400559538775,-36.5742356128,5.5969099823375));
#65816=CARTESIAN_POINT('Origin',(5.53776680476872,-36.5721143148321,5.60690846915117));
#65817=CARTESIAN_POINT('Ctrl Pts',(1.28769461759875E-9,-36.5742356128,10.6643459816));
#65818=CARTESIAN_POINT('Ctrl Pts',(0.147840141500339,-36.5742356128,10.6643342421081));
#65819=CARTESIAN_POINT('Ctrl Pts',(0.295679233170314,-36.5742356128,10.6580838271699));
#65820=CARTESIAN_POINT('Ctrl Pts',(0.442988225077906,-36.5742356128,10.6456029881052));
#65821=CARTESIAN_POINT('Ctrl Pts',(0.592364761454907,-36.5742356128,10.6329469751461));
#65822=CARTESIAN_POINT('Ctrl Pts',(0.741195961727722,-36.5742356128,10.6138844583169));
#65823=CARTESIAN_POINT('Ctrl Pts',(0.888934980438098,-36.5742356128,10.5884776060529));
#65824=CARTESIAN_POINT('Ctrl Pts',(1.03778268782953,-36.5742356128,10.5628800912965));
#65825=CARTESIAN_POINT('Ctrl Pts',(1.18552149683487,-36.5742356128,10.5308427707656));
#65826=CARTESIAN_POINT('Ctrl Pts',(1.33160089085122,-36.5742356128,10.4924820059666));
#65827=CARTESIAN_POINT('Ctrl Pts',(1.47862414497429,-36.5742356128,10.4538733814623));
#65828=CARTESIAN_POINT('Ctrl Pts',(1.62396619622945,-36.5742356128,10.408859457976));
#65829=CARTESIAN_POINT('Ctrl Pts',(1.76707866522786,-36.5742356128,10.3576103681606));
#65830=CARTESIAN_POINT('Ctrl Pts',(1.91093255878637,-36.5742356128,10.3060957715438));
#65831=CARTESIAN_POINT('Ctrl Pts',(2.05253342556236,-36.5742356128,10.2482813783103));
#65832=CARTESIAN_POINT('Ctrl Pts',(2.19134149631081,-36.5742356128,10.1843898178516));
#65833=CARTESIAN_POINT('Ctrl Pts',(2.33084529538293,-36.5742356128,10.1201780226399));
#65834=CARTESIAN_POINT('Ctrl Pts',(2.46752793929734,-36.5742356128,10.0498281384951));
#65835=CARTESIAN_POINT('Ctrl Pts',(2.60086315421496,-36.5742356128,9.97361415794421));
#65836=CARTESIAN_POINT('Ctrl Pts',(2.73433276278183,-36.5742356128,9.8973233584151));
#65837=CARTESIAN_POINT('Ctrl Pts',(2.86444790857184,-36.5742356128,9.8151568205301));
#65838=CARTESIAN_POINT('Ctrl Pts',(2.99070667424014,-36.5742356128,9.72743476808259));
#65839=CARTESIAN_POINT('Ctrl Pts',(3.11682204767723,-36.5742356128,9.63981234167499));
#65840=CARTESIAN_POINT('Ctrl Pts',(3.23908952393931,-36.5742356128,9.54664721325454));
#65841=CARTESIAN_POINT('Ctrl Pts',(3.3570389094003,-36.5742356128,9.44830087319822));
#65842=CARTESIAN_POINT('Ctrl Pts',(3.456001761657,-36.5742356128,9.36578552745953));
#65843=CARTESIAN_POINT('Ctrl Pts',(3.55192525354885,-36.5742356128,9.27962356642855));
#65844=CARTESIAN_POINT('Ctrl Pts',(3.64455010326894,-36.5742356128,9.19005000033049));
#65845=CARTESIAN_POINT('Ctrl Pts',(3.75506240265809,-36.5742356128,9.08317823984834));
#65846=CARTESIAN_POINT('Ctrl Pts',(3.86087792258727,-36.5742356128,8.97144924806346));
#65847=CARTESIAN_POINT('Ctrl Pts',(3.96158460510385,-36.5742356128,8.85529518741082));
#65848=CARTESIAN_POINT('Ctrl Pts',(4.06235959274001,-36.5742356128,8.73906234432981));
#65849=CARTESIAN_POINT('Ctrl Pts',(4.15801862492861,-36.5742356128,8.61839866232239));
#65850=CARTESIAN_POINT('Ctrl Pts',(4.24818890413247,-36.5742356128,8.49377048410246));
#65851=CARTESIAN_POINT('Ctrl Pts',(4.33823238792445,-36.5742356128,8.36931755521443));
#65852=CARTESIAN_POINT('Ctrl Pts',(4.42280237436131,-36.5742356128,8.24091151652117));
#65853=CARTESIAN_POINT('Ctrl Pts',(4.50157025117896,-36.5742356128,8.10904633222281));
#65854=CARTESIAN_POINT('Ctrl Pts',(4.58012232474487,-36.5742356128,7.97754242382412));
#65855=CARTESIAN_POINT('Ctrl Pts',(4.65290388085685,-36.5742356128,7.84259854510023));
#65856=CARTESIAN_POINT('Ctrl Pts',(4.71963384069473,-36.5742356128,7.70473036952541));
#65857=CARTESIAN_POINT('Ctrl Pts',(4.78609874864947,-36.5742356128,7.56740980734118));
#65858=CARTESIAN_POINT('Ctrl Pts',(4.84655989621262,-36.5742356128,7.42718837846509));
#65859=CARTESIAN_POINT('Ctrl Pts',(4.90078630758145,-36.5742356128,7.28459753902635));
#65860=CARTESIAN_POINT('Ctrl Pts',(4.95456804763369,-36.5742356128,7.14317598323936));
#65861=CARTESIAN_POINT('Ctrl Pts',(5.00221678397136,-36.5742356128,6.99942396510125));
#65862=CARTESIAN_POINT('Ctrl Pts',(5.04355503451248,-36.5742356128,6.85387786797466));
#65863=CARTESIAN_POINT('Ctrl Pts',(5.08466686288025,-36.5742356128,6.70912897109731));
#65864=CARTESIAN_POINT('Ctrl Pts',(5.11953702859418,-36.5742356128,6.56260582424903));
#65865=CARTESIAN_POINT('Ctrl Pts',(5.14804013322182,-36.5742356128,6.41485027913283));
#65866=CARTESIAN_POINT('Ctrl Pts',(5.17626254570044,-36.5742356128,6.26854979731691));
#65867=CARTESIAN_POINT('Ctrl Pts',(5.19824261046229,-36.5742356128,6.12104129530587));
#65868=CARTESIAN_POINT('Ctrl Pts',(5.21390829155022,-36.5742356128,5.9728613808213));
#65869=CARTESIAN_POINT('Ctrl Pts',(5.22711794574893,-36.5742356128,5.84791274829469));
#65870=CARTESIAN_POINT('Ctrl Pts',(5.23583872043894,-36.5742356128,5.7224869695072));
#65871=CARTESIAN_POINT('Ctrl Pts',(5.24005595171,-36.5742356128,5.59690998278));
#65872=CARTESIAN_POINT('Ctrl Pts',(5.24005594912,-37.9742356128,5.5969099833));
#65873=CARTESIAN_POINT('Ctrl Pts',(5.24005594912,-38.0684833924,5.59690998329));
#65874=CARTESIAN_POINT('Ctrl Pts',(5.27704611469,-38.162731172,5.59815215178));
#65875=CARTESIAN_POINT('Ctrl Pts',(5.35149757153,-38.2372245963,5.60065230967));
#65876=CARTESIAN_POINT('Ctrl Pts',(5.44569225468,-38.2742356128,5.60381546578));
#65877=CARTESIAN_POINT('Ctrl Pts',(5.53988693785,-38.2742356128,5.6069786219));
#65878=CARTESIAN_POINT('Ctrl Pts',(5.21299946948,-37.9742356128,6.40257078081));
#65879=CARTESIAN_POINT('Ctrl Pts',(5.21299946951,-38.068483391,6.40257077998));
#65880=CARTESIAN_POINT('Ctrl Pts',(5.24979957977,-38.1627311691,6.40947213682));
#65881=CARTESIAN_POINT('Ctrl Pts',(5.32386850147,-38.2372245928,6.42336289407));
#65882=CARTESIAN_POINT('Ctrl Pts',(5.41757921002,-38.2742356105,6.4409371779));
#65883=CARTESIAN_POINT('Ctrl Pts',(5.51128991946,-38.2742356128,6.4585114621));
#65884=CARTESIAN_POINT('Ctrl Pts',(5.03157376442,-37.9742356128,7.20293447587));
#65885=CARTESIAN_POINT('Ctrl Pts',(5.03157368764,-38.0684833946,7.20293453622));
#65886=CARTESIAN_POINT('Ctrl Pts',(5.06709410499,-38.1627311763,7.21553462796));
#65887=CARTESIAN_POINT('Ctrl Pts',(5.13858744567,-38.2372246013,7.24089500381));
#65888=CARTESIAN_POINT('Ctrl Pts',(5.22903961522,-38.2742356162,7.27298056211));
#65889=CARTESIAN_POINT('Ctrl Pts',(5.31949181364,-38.2742356128,7.30506609664));
#65890=CARTESIAN_POINT('Ctrl Pts',(4.69583353882,-37.9742356128,7.95822794629));
#65891=CARTESIAN_POINT('Ctrl Pts',(4.69583375753,-38.0684833911,7.9582276781));
#65892=CARTESIAN_POINT('Ctrl Pts',(4.72897185598,-38.1627311693,7.97614326012));
#65893=CARTESIAN_POINT('Ctrl Pts',(4.79566992348,-38.237224593,8.01220298795));
#65894=CARTESIAN_POINT('Ctrl Pts',(4.88005499,-38.2742356106,8.0578252665));
#65895=CARTESIAN_POINT('Ctrl Pts',(4.96443997088,-38.2742356128,8.10344765091));
#65896=CARTESIAN_POINT('Ctrl Pts',(3.75205884826,-37.9742356128,9.30126426068));
#65897=CARTESIAN_POINT('Ctrl Pts',(3.75205862954,-38.0684833938,9.30126452888));
#65898=CARTESIAN_POINT('Ctrl Pts',(3.77854861256,-38.1627311749,9.32865838142));
#65899=CARTESIAN_POINT('Ctrl Pts',(3.83186616208,-38.2372245996,9.38379460661));
#65900=CARTESIAN_POINT('Ctrl Pts',(3.89932275841,-38.274235615,9.45355185547));
#65901=CARTESIAN_POINT('Ctrl Pts',(3.9667794404,-38.2742356128,9.52330899846));
#65902=CARTESIAN_POINT('Ctrl Pts',(2.37813062282,-37.9742356128,10.1995581826));
#65903=CARTESIAN_POINT('Ctrl Pts',(2.37813084155,-38.068483391,10.1995579144));
#65904=CARTESIAN_POINT('Ctrl Pts',(2.39492734371,-38.1627311693,10.2332766055));
#65905=CARTESIAN_POINT('Ctrl Pts',(2.42873408312,-38.237224593,10.3011438287));
#65906=CARTESIAN_POINT('Ctrl Pts',(2.4715056159,-38.2742356106,10.3870083947));
#65907=CARTESIAN_POINT('Ctrl Pts',(2.51427706302,-38.2742356128,10.4728730665));
#65908=CARTESIAN_POINT('Ctrl Pts',(1.61217671584,-37.9742356128,10.5097230164));
#65909=CARTESIAN_POINT('Ctrl Pts',(1.61217703526,-38.0684834004,10.5097230175));
#65910=CARTESIAN_POINT('Ctrl Pts',(1.62357348219,-38.162731188,10.5456455438));
#65911=CARTESIAN_POINT('Ctrl Pts',(1.64651083532,-38.2372246151,10.6179481209));
#65912=CARTESIAN_POINT('Ctrl Pts',(1.67553070609,-38.2742356254,10.7094240756));
#65913=CARTESIAN_POINT('Ctrl Pts',(1.70455045076,-38.2742356128,10.8009000251));
#65914=CARTESIAN_POINT('Ctrl Pts',(0.806141183123,-37.9742356128,10.6642820769));
#65915=CARTESIAN_POINT('Ctrl Pts',(0.806141182686,-38.0684833912,10.6642820769));
#65916=CARTESIAN_POINT('Ctrl Pts',(0.811810207047,-38.1627311695,10.7012926437));
#65917=CARTESIAN_POINT('Ctrl Pts',(0.823220660712,-38.2372245933,10.7757851643));
#65918=CARTESIAN_POINT('Ctrl Pts',(0.837656883379,-38.2742356108,10.8700318005));
#65919=CARTESIAN_POINT('Ctrl Pts',(0.852093106215,-38.2742356128,10.9642784374));
#65920=CARTESIAN_POINT('Ctrl Pts',(6.88994417075E-10,-37.9742356128,10.6643459842));
#65921=CARTESIAN_POINT('Ctrl Pts',(6.97641722169E-10,-38.0684833925,10.6643459842));
#65922=CARTESIAN_POINT('Ctrl Pts',(2.97494488111E-6,-38.1627311721,10.7013570005));
#65923=CARTESIAN_POINT('Ctrl Pts',(8.96131032624E-6,-38.2372245964,10.7758504244));
#65924=CARTESIAN_POINT('Ctrl Pts',(1.65351501034E-5,-38.2742356129,10.8700982036));
#65925=CARTESIAN_POINT('Ctrl Pts',(2.41089864841E-5,-38.2742356128,10.9643459827));
#65926=CARTESIAN_POINT('',(5.24005595186,-37.9742356128,5.596909982745));
#65927=CARTESIAN_POINT('Ctrl Pts',(6.88994195030546E-10,-37.9742356128,
10.6643459842));
#65928=CARTESIAN_POINT('Ctrl Pts',(0.148543738141462,-37.9742356128,10.6643342083109));
#65929=CARTESIAN_POINT('Ctrl Pts',(0.297086910377638,-37.9742356128,10.6580232678524));
#65930=CARTESIAN_POINT('Ctrl Pts',(0.445090815547211,-37.9742356128,10.6454233478295));
#65931=CARTESIAN_POINT('Ctrl Pts',(0.59487372187678,-37.9742356128,10.63267197726));
#65932=CARTESIAN_POINT('Ctrl Pts',(0.744104091924914,-37.9742356128,10.6134795752124));
#65933=CARTESIAN_POINT('Ctrl Pts',(0.892229989798875,-37.9742356128,10.5879098461637));
#65934=CARTESIAN_POINT('Ctrl Pts',(1.04131204338439,-37.9742356128,10.5621750639892));
#65935=CARTESIAN_POINT('Ctrl Pts',(1.1892750857725,-37.9742356128,10.5299804567442));
#65936=CARTESIAN_POINT('Ctrl Pts',(1.33556638280071,-37.9742356128,10.4914433340022));
#65937=CARTESIAN_POINT('Ctrl Pts',(1.4826794306896,-37.9742356128,10.4526897396422));
#65938=CARTESIAN_POINT('Ctrl Pts',(1.62810165638871,-37.9742356128,10.4075222877044));
#65939=CARTESIAN_POINT('Ctrl Pts',(1.77128460050933,-37.9742356128,10.3561114475755));
#65940=CARTESIAN_POINT('Ctrl Pts',(1.91512843540153,-37.9742356128,10.3044633099808));
#65941=CARTESIAN_POINT('Ctrl Pts',(2.05671201996512,-37.9742356128,10.2465141426538));
#65942=CARTESIAN_POINT('Ctrl Pts',(2.19549670562412,-37.9742356128,10.182486467514));
#65943=CARTESIAN_POINT('Ctrl Pts',(2.33495214390865,-37.9742356128,10.1181493437415));
#65944=CARTESIAN_POINT('Ctrl Pts',(2.4715813047956,-37.9742356128,10.0476749455133));
#65945=CARTESIAN_POINT('Ctrl Pts',(2.6048590942595,-37.9742356128,9.97133714374602));
#65946=CARTESIAN_POINT('Ctrl Pts',(2.73831338899758,-37.9742356128,9.89489824467904));
#65947=CARTESIAN_POINT('Ctrl Pts',(2.86840717985693,-37.9742356128,9.81258056317965));
#65948=CARTESIAN_POINT('Ctrl Pts',(2.99463849904681,-37.9742356128,9.72470493579735));
#65949=CARTESIAN_POINT('Ctrl Pts',(3.12086957170909,-37.9742356128,9.63682948003464));
#65950=CARTESIAN_POINT('Ctrl Pts',(3.24323794320094,-37.9742356128,9.54339627268128));
#65951=CARTESIAN_POINT('Ctrl Pts',(3.36127054935203,-37.9742356128,9.44476947023749));
#65952=CARTESIAN_POINT('Ctrl Pts',(3.45873626436591,-37.9742356128,9.36332814539365));
#65953=CARTESIAN_POINT('Ctrl Pts',(3.55324602203091,-37.9742356128,9.27834630722957));
#65954=CARTESIAN_POINT('Ctrl Pts',(3.64455010326812,-37.9742356128,9.19005000034558));
#65955=CARTESIAN_POINT('Ctrl Pts',(3.75483187955168,-37.9742356128,9.08340116898452));
#65956=CARTESIAN_POINT('Ctrl Pts',(3.86043575496047,-37.9742356128,8.97191598143711));
#65957=CARTESIAN_POINT('Ctrl Pts',(3.96095362281167,-37.9742356128,8.85602145332094));
#65958=CARTESIAN_POINT('Ctrl Pts',(4.06169428001623,-37.9742356128,8.73987005478434));
#65959=CARTESIAN_POINT('Ctrl Pts',(4.15732614237061,-37.9742356128,8.61929000585443));
#65960=CARTESIAN_POINT('Ctrl Pts',(4.24747728584571,-37.9742356128,8.49474609398298));
#65961=CARTESIAN_POINT('Ctrl Pts',(4.33754043554632,-37.9742356128,8.3703237456156));
#65962=CARTESIAN_POINT('Ctrl Pts',(4.42213336493615,-37.9742356128,8.24194554434444));
#65963=CARTESIAN_POINT('Ctrl Pts',(4.50092708273691,-37.9742356128,8.11010570734388));
#65964=CARTESIAN_POINT('Ctrl Pts',(4.5795067479302,-37.9742356128,7.97862402911112));
#65965=CARTESIAN_POINT('Ctrl Pts',(4.65231848790631,-37.9742356128,7.84369977752986));
#65966=CARTESIAN_POINT('Ctrl Pts',(4.71908040770882,-37.9742356128,7.70584961888401));
#65967=CARTESIAN_POINT('Ctrl Pts',(4.78555342045735,-37.9742356128,7.56859599615778));
#65968=CARTESIAN_POINT('Ctrl Pts',(4.8460286985358,-37.9742356128,7.42844201386812));
#65969=CARTESIAN_POINT('Ctrl Pts',(4.90027461525642,-37.9742356128,7.28591974913334));
#65970=CARTESIAN_POINT('Ctrl Pts',(4.95401280665947,-37.9742356128,7.14473144954282));
#65971=CARTESIAN_POINT('Ctrl Pts',(5.00163758895503,-37.9742356128,7.0012192733805));
#65972=CARTESIAN_POINT('Ctrl Pts',(5.04297160369282,-37.9742356128,6.85591803740467));
#65973=CARTESIAN_POINT('Ctrl Pts',(5.08404289066266,-37.9742356128,6.71154036691482));
#65974=CARTESIAN_POINT('Ctrl Pts',(5.11890299934201,-37.9742356128,6.56539656577722));
#65975=CARTESIAN_POINT('Ctrl Pts',(5.14742718798799,-37.9742356128,6.41802472866415));
#65976=CARTESIAN_POINT('Ctrl Pts',(5.17562330555142,-37.9742356128,6.27234788939091));
#65977=CARTESIAN_POINT('Ctrl Pts',(5.1976283358666,-37.9742356128,6.12547135028398));
#65978=CARTESIAN_POINT('Ctrl Pts',(5.21337150408987,-37.9742356128,5.9779242168455));
#65979=CARTESIAN_POINT('Ctrl Pts',(5.22688216218712,-37.9742356128,5.85130047473441));
#65980=CARTESIAN_POINT('Ctrl Pts',(5.23578174108458,-37.9742356128,5.72418307648716));
#65981=CARTESIAN_POINT('Ctrl Pts',(5.24005594912,-37.9742356128,5.5969099833));
#65982=CARTESIAN_POINT('Origin',(5.5377668413967,-37.9763569043018,5.60690742687626));
#65983=CARTESIAN_POINT('Ctrl Pts',(0.,-37.9742356128,10.664345987));
#65984=CARTESIAN_POINT('Ctrl Pts',(0.,-36.2942356128,10.664345987));
#65985=CARTESIAN_POINT('Ctrl Pts',(1.61198306736,-37.9742356128,10.6642180635));
#65986=CARTESIAN_POINT('Ctrl Pts',(1.61198306736,-36.2942356128,10.6642180635));
#65987=CARTESIAN_POINT('Ctrl Pts',(3.22524412625,-37.9742356128,10.0462831132));
#65988=CARTESIAN_POINT('Ctrl Pts',(3.22524412625,-36.2942356128,10.0462831132));
#65989=CARTESIAN_POINT('Ctrl Pts',(4.51434339457,-37.9742356128,8.79964985146));
#65990=CARTESIAN_POINT('Ctrl Pts',(4.51434339457,-36.2942356128,8.79964985146));
#65991=CARTESIAN_POINT('Ctrl Pts',(5.18595136098,-37.9742356128,7.20798481558));
#65992=CARTESIAN_POINT('Ctrl Pts',(5.18595136098,-36.2942356128,7.20798481558));
#65993=CARTESIAN_POINT('Ctrl Pts',(5.2400559546,-37.9742356128,5.59690998219));
#65994=CARTESIAN_POINT('Ctrl Pts',(5.2400559546,-36.2942356128,5.59690998219));
#65995=CARTESIAN_POINT('',(5.2400559546,-37.2742356128,5.59690998219));
#65996=CARTESIAN_POINT('Ctrl Pts',(5.53988692571,-36.2742356128,5.60697918103));
#65997=CARTESIAN_POINT('Ctrl Pts',(5.4456922481,-36.2742356128,5.60381584892));
#65998=CARTESIAN_POINT('Ctrl Pts',(5.35149757048,-36.3112466293,5.60065251681));
#65999=CARTESIAN_POINT('Ctrl Pts',(5.277046118,-36.3857400536,5.59815221981));
#66000=CARTESIAN_POINT('Ctrl Pts',(5.2400559546,-36.4799878332,5.59690998219));
#66001=CARTESIAN_POINT('Ctrl Pts',(5.2400559546,-36.5742356128,5.59690998219));
#66002=CARTESIAN_POINT('Ctrl Pts',(5.55319667202,-36.2742356128,5.21065428735));
#66003=CARTESIAN_POINT('Ctrl Pts',(5.4588608737,-36.2742356128,5.21169311262));
#66004=CARTESIAN_POINT('Ctrl Pts',(5.36452507538,-36.3112466293,5.21273193789));
#66005=CARTESIAN_POINT('Ctrl Pts',(5.28996208088,-36.3857400536,5.21355302628));
#66006=CARTESIAN_POINT('Ctrl Pts',(5.25291649976,-36.4799878332,5.21396097089));
#66007=CARTESIAN_POINT('Ctrl Pts',(5.25291649976,-36.5742356128,5.21396097089));
#66008=CARTESIAN_POINT('Ctrl Pts',(5.54519742229,-36.2742356128,4.78859077007));
#66009=CARTESIAN_POINT('Ctrl Pts',(5.45071977967,-36.2742356128,4.79882974975));
#66010=CARTESIAN_POINT('Ctrl Pts',(5.35624213705,-36.3112466293,4.80906872944));
#66011=CARTESIAN_POINT('Ctrl Pts',(5.28156702935,-36.3857400536,4.81716161496));
#66012=CARTESIAN_POINT('Ctrl Pts',(5.24446574559,-36.4799878332,4.82118245465));
#66013=CARTESIAN_POINT('Ctrl Pts',(5.24446574559,-36.5742356128,4.82118245465));
#66014=CARTESIAN_POINT('Ctrl Pts',(5.47535951132,-36.2742356128,4.37143582924));
#66015=CARTESIAN_POINT('Ctrl Pts',(5.38263787774,-36.2742356128,4.39040588335));
#66016=CARTESIAN_POINT('Ctrl Pts',(5.28991624416,-36.3112466293,4.40937593746));
#66017=CARTESIAN_POINT('Ctrl Pts',(5.21662908074,-36.3857400536,4.42436985031));
#66018=CARTESIAN_POINT('Ctrl Pts',(5.180217385,-36.4799878332,4.43181938688));
#66019=CARTESIAN_POINT('Ctrl Pts',(5.180217385,-36.5742356128,4.43181938688));
#66020=CARTESIAN_POINT('Ctrl Pts',(5.26366547685,-36.2742356128,3.57390225037));
#66021=CARTESIAN_POINT('Ctrl Pts',(5.17451246306,-36.2742356128,3.60488329763));
#66022=CARTESIAN_POINT('Ctrl Pts',(5.08535944927,-36.3112466293,3.6358643449));
#66023=CARTESIAN_POINT('Ctrl Pts',(5.01489293121,-36.3857400536,3.66035177163));
#66024=CARTESIAN_POINT('Ctrl Pts',(4.97988262013,-36.4799878332,3.67251798666));
#66025=CARTESIAN_POINT('Ctrl Pts',(4.97988262013,-36.5742356128,3.67251798666));
#66026=CARTESIAN_POINT('Ctrl Pts',(5.00219757732,-36.2742356128,2.85773196192));
#66027=CARTESIAN_POINT('Ctrl Pts',(4.91343107087,-36.2742356128,2.88936313774));
#66028=CARTESIAN_POINT('Ctrl Pts',(4.82466456442,-36.3112466293,2.92099431357));
#66029=CARTESIAN_POINT('Ctrl Pts',(4.75450353299,-36.3857400536,2.94599557417));
#66030=CARTESIAN_POINT('Ctrl Pts',(4.71964501167,-36.4799878332,2.95841712169));
#66031=CARTESIAN_POINT('Ctrl Pts',(4.71964501167,-36.5742356128,2.95841712169));
#66032=CARTESIAN_POINT('Ctrl Pts',(4.8804439272,-36.2742356128,2.50135880489));
#66033=CARTESIAN_POINT('Ctrl Pts',(4.78990764639,-36.2742356128,2.5276002033));
#66034=CARTESIAN_POINT('Ctrl Pts',(4.69937136558,-36.3112466293,2.5538416017));
#66035=CARTESIAN_POINT('Ctrl Pts',(4.62781152696,-36.3857400536,2.57458285528));
#66036=CARTESIAN_POINT('Ctrl Pts',(4.59225799479,-36.4799878332,2.58488777028));
#66037=CARTESIAN_POINT('Ctrl Pts',(4.59225799479,-36.5742356128,2.58488777028));
#66038=CARTESIAN_POINT('Ctrl Pts',(4.79845683709,-36.2742356128,2.15377208868));
#66039=CARTESIAN_POINT('Ctrl Pts',(4.70711530139,-36.2742356128,2.17743291681));
#66040=CARTESIAN_POINT('Ctrl Pts',(4.61577376569,-36.3112466293,2.20109374493));
#66041=CARTESIAN_POINT('Ctrl Pts',(4.54357742413,-36.3857400536,2.21979521964));
#66042=CARTESIAN_POINT('Ctrl Pts',(4.50770769876,-36.4799878332,2.22908684376));
#66043=CARTESIAN_POINT('Ctrl Pts',(4.50770769876,-36.5742356128,2.22908684376));
#66044=CARTESIAN_POINT('Ctrl Pts',(4.67794710935,-36.2742356128,1.76615076209));
#66045=CARTESIAN_POINT('Ctrl Pts',(4.58794861595,-36.2742356128,1.79413138544));
#66046=CARTESIAN_POINT('Ctrl Pts',(4.49795012256,-36.3112466293,1.82211200878));
#66047=CARTESIAN_POINT('Ctrl Pts',(4.42681533316,-36.3857400536,1.84422788732));
#66048=CARTESIAN_POINT('Ctrl Pts',(4.39147300745,-36.4799878332,1.85521585242));
#66049=CARTESIAN_POINT('Ctrl Pts',(4.39147300745,-36.5742356128,1.85521585242));
#66050=CARTESIAN_POINT('Ctrl Pts',(4.67555993961595,-36.2742356128,1.75847239523564));
#66051=CARTESIAN_POINT('Ctrl Pts',(4.5855880504577,-36.2742356128,1.78653858914164));
#66052=CARTESIAN_POINT('Ctrl Pts',(4.49561616130965,-36.3112466293,1.81460478303764));
#66053=CARTESIAN_POINT('Ctrl Pts',(4.42450240013065,-36.3857400536,1.83678829729166));
#66054=CARTESIAN_POINT('Ctrl Pts',(4.38917052164785,-36.4799878332,1.84780986510509));
#66055=CARTESIAN_POINT('Ctrl Pts',(4.38917052164785,-36.5742356128,1.84780986510509));
#66056=CARTESIAN_POINT('Ctrl Pts',(4.6731727698819,-36.2742356128,1.75079402838127));
#66057=CARTESIAN_POINT('Ctrl Pts',(4.5832274849654,-36.2742356128,1.77894579284327));
#66058=CARTESIAN_POINT('Ctrl Pts',(4.4932822000593,-36.3112466293,1.80709755729528));
#66059=CARTESIAN_POINT('Ctrl Pts',(4.4221894671013,-36.3857400536,1.82934870726333));
#66060=CARTESIAN_POINT('Ctrl Pts',(4.38686803584571,-36.4799878332,1.84040387779018));
#66061=CARTESIAN_POINT('Ctrl Pts',(4.38686803584571,-36.5742356128,1.84040387779018));
#66062=CARTESIAN_POINT('Ctrl Pts',(4.67078560014785,-36.2742356128,1.7431156615269));
#66063=CARTESIAN_POINT('Ctrl Pts',(4.58086691947311,-36.2742356128,1.77135299654491));
#66064=CARTESIAN_POINT('Ctrl Pts',(4.49094823880895,-36.3112466293,1.79959033155291));
#66065=CARTESIAN_POINT('Ctrl Pts',(4.41987653407195,-36.3857400536,1.821909117235));
#66066=CARTESIAN_POINT('Ctrl Pts',(4.38456555004357,-36.4799878332,1.83299789047527));
#66067=CARTESIAN_POINT('Ctrl Pts',(4.38456555004357,-36.5742356128,1.83299789047527));
#66068=CARTESIAN_POINT('Ctrl Pts',(4.6683984304138,-36.2742356128,1.73543729467253));
#66069=CARTESIAN_POINT('Ctrl Pts',(4.57850635398081,-36.2742356128,1.76376020024654));
#66070=CARTESIAN_POINT('Ctrl Pts',(4.4886142775586,-36.3112466293,1.79208310581055));
#66071=CARTESIAN_POINT('Ctrl Pts',(4.4175636010426,-36.3857400536,1.81446952720666));
#66072=CARTESIAN_POINT('Ctrl Pts',(4.38226306424141,-36.4799878332,1.82559190316036));
#66073=CARTESIAN_POINT('Ctrl Pts',(4.38226306424141,-36.5742356128,1.82559190316036));
#66074=CARTESIAN_POINT('Ctrl Pts',(4.66601126067975,-36.2742356128,1.72775892781816));
#66075=CARTESIAN_POINT('Ctrl Pts',(4.57614578848851,-36.2742356128,1.75616740394817));
#66076=CARTESIAN_POINT('Ctrl Pts',(4.48628031630825,-36.3112466293,1.78457588006819));
#66077=CARTESIAN_POINT('Ctrl Pts',(4.41525066801324,-36.3857400536,1.80702993717832));
#66078=CARTESIAN_POINT('Ctrl Pts',(4.37996057843927,-36.4799878332,1.81818591584544));
#66079=CARTESIAN_POINT('Ctrl Pts',(4.37996057843927,-36.5742356128,1.81818591584544));
#66080=CARTESIAN_POINT('',(4.39146896866,-36.5742356128,1.85520291202));
#66081=CARTESIAN_POINT('Origin',(4.67591768253123,-36.5721143218718,1.76676845393353));
#66082=CARTESIAN_POINT('Ctrl Pts',(5.2400559546,-36.5742356128,5.59690998219));
#66083=CARTESIAN_POINT('Ctrl Pts',(5.25311376105,-36.5742356128,5.20808711269));
#66084=CARTESIAN_POINT('Ctrl Pts',(5.24470483276,-36.5742356128,4.80219931419));
#66085=CARTESIAN_POINT('Ctrl Pts',(5.17504642388,-36.5742356128,4.39981761669));
#66086=CARTESIAN_POINT('Ctrl Pts',(5.00839926013,-36.5742356128,3.79030695888));
#66087=CARTESIAN_POINT('Ctrl Pts',(4.81153097626,-36.5742356128,3.21707824383));
#66088=CARTESIAN_POINT('Ctrl Pts',(4.73686810339,-36.5742356128,3.00222967268));
#66089=CARTESIAN_POINT('Ctrl Pts',(4.62316453236,-36.5742356128,2.6499539825));
#66090=CARTESIAN_POINT('Ctrl Pts',(4.51875357768,-36.5742356128,2.29074629441));
#66091=CARTESIAN_POINT('Ctrl Pts',(4.47967500948,-36.5742356128,2.15155097848));
#66092=CARTESIAN_POINT('Ctrl Pts',(4.43790342458,-36.5742356128,2.00456060561));
#66093=CARTESIAN_POINT('Ctrl Pts',(4.39146896866,-36.5742356128,1.85520291202));
#66094=CARTESIAN_POINT('Ctrl Pts',(4.39147614152,-37.9742356128,1.85522626202));
#66095=CARTESIAN_POINT('Ctrl Pts',(4.3914761461,-38.0684833925,1.85522627644));
#66096=CARTESIAN_POINT('Ctrl Pts',(4.42681839499,-38.1627311722,1.84423808607));
#66097=CARTESIAN_POINT('Ctrl Pts',(4.49795302417,-38.2372245965,1.82212173648));
#66098=CARTESIAN_POINT('Ctrl Pts',(4.58795131206,-38.274235613,1.79414050842));
#66099=CARTESIAN_POINT('Ctrl Pts',(4.6779495981,-38.2742356128,1.76615927471));
#66100=CARTESIAN_POINT('Ctrl Pts',(4.50961312754,-37.9742356128,2.23520776943));
#66101=CARTESIAN_POINT('Ctrl Pts',(4.50961297784,-38.0684833942,2.23520729805));
#66102=CARTESIAN_POINT('Ctrl Pts',(4.54549269235,-38.1627311756,2.22594725384));
#66103=CARTESIAN_POINT('Ctrl Pts',(4.61770933618,-38.2372246005,2.20730995948));
#66104=CARTESIAN_POINT('Ctrl Pts',(4.70907664249,-38.2742356156,2.18373060025));
#66105=CARTESIAN_POINT('Ctrl Pts',(4.8004440065,-38.2742356128,2.16015142631));
#66106=CARTESIAN_POINT('Ctrl Pts',(4.59532849366,-37.9742356128,2.59792165201));
#66107=CARTESIAN_POINT('Ctrl Pts',(4.59532871153,-38.0684834119,2.59792233911));
#66108=CARTESIAN_POINT('Ctrl Pts',(4.63086911606,-38.162731211,2.58756440064));
#66109=CARTESIAN_POINT('Ctrl Pts',(4.70240224551,-38.2372246422,2.56671552146));
#66110=CARTESIAN_POINT('Ctrl Pts',(4.79290460312,-38.2742356434,2.54033756838));
#66111=CARTESIAN_POINT('Ctrl Pts',(4.88340686381,-38.2742356128,2.51395934938));
#66112=CARTESIAN_POINT('Ctrl Pts',(4.72598707696,-37.9742356128,2.97653900944));
#66113=CARTESIAN_POINT('Ctrl Pts',(4.72598702354,-38.0684833705,2.97653884209));
#66114=CARTESIAN_POINT('Ctrl Pts',(4.76081453341,-38.1627311281,2.96403785534));
#66115=CARTESIAN_POINT('Ctrl Pts',(4.83091321213,-38.2372245445,2.93887706303));
#66116=CARTESIAN_POINT('Ctrl Pts',(4.91960087198,-38.2742355783,2.90704408516));
#66117=CARTESIAN_POINT('Ctrl Pts',(5.00828856587,-38.2742356128,2.87521116975));
#66118=CARTESIAN_POINT('Ctrl Pts',(4.98677022447,-37.9742356128,3.69093161808));
#66119=CARTESIAN_POINT('Ctrl Pts',(4.98677027514,-38.0684834133,3.69093177682));
#66120=CARTESIAN_POINT('Ctrl Pts',(5.02181898916,-38.1627312138,3.6788456217));
#66121=CARTESIAN_POINT('Ctrl Pts',(5.09236274059,-38.2372246455,3.65451899528));
#66122=CARTESIAN_POINT('Ctrl Pts',(5.18161342975,-38.2742356456,3.62374135649));
#66123=CARTESIAN_POINT('Ctrl Pts',(5.27086408663,-38.2742356128,3.59296365845));
#66124=CARTESIAN_POINT('Ctrl Pts',(5.18352491332,-37.9742356128,4.45190028227));
#66125=CARTESIAN_POINT('Ctrl Pts',(5.18352486526,-38.0684833727,4.4519001317));
#66126=CARTESIAN_POINT('Ctrl Pts',(5.21997029761,-38.1627311325,4.44462444175));
#66127=CARTESIAN_POINT('Ctrl Pts',(5.29332542209,-38.2372245497,4.42998075713));
#66128=CARTESIAN_POINT('Ctrl Pts',(5.38613307587,-38.2742355818,4.41145383762));
#66129=CARTESIAN_POINT('Ctrl Pts',(5.47894076028,-38.2742356128,4.39292697431));
#66130=CARTESIAN_POINT('Ctrl Pts',(5.24475584762,-37.9742356128,4.83460482733));
#66131=CARTESIAN_POINT('Ctrl Pts',(5.24475584748,-38.0684834044,4.83460481263));
#66132=CARTESIAN_POINT('Ctrl Pts',(5.281854554,-38.1627311959,4.83070605882));
#66133=CARTESIAN_POINT('Ctrl Pts',(5.35652449165,-38.2372246244,4.82285841894));
#66134=CARTESIAN_POINT('Ctrl Pts',(5.45099558138,-38.2742356315,4.81292993959));
#66135=CARTESIAN_POINT('Ctrl Pts',(5.54546666392,-38.2742356128,4.80300146625));
#66136=CARTESIAN_POINT('Ctrl Pts',(5.2526976354,-37.9742356128,5.22047810427));
#66137=CARTESIAN_POINT('Ctrl Pts',(5.2526976354,-38.0684833924,5.22047810427));
#66138=CARTESIAN_POINT('Ctrl Pts',(5.28974227713,-38.1627311721,5.22009813259));
#66139=CARTESIAN_POINT('Ctrl Pts',(5.36430336964,-38.2372245963,5.21933367912));
#66140=CARTESIAN_POINT('Ctrl Pts',(5.45863676635,-38.2742356128,5.21836636703));
#66141=CARTESIAN_POINT('Ctrl Pts',(5.55297016303,-38.2742356128,5.21739905525));
#66142=CARTESIAN_POINT('Ctrl Pts',(5.2400559546,-37.9742356128,5.59690998219));
#66143=CARTESIAN_POINT('Ctrl Pts',(5.2400559546,-38.0684833924,5.59690998219));
#66144=CARTESIAN_POINT('Ctrl Pts',(5.277046118,-38.1627311721,5.59815221981));
#66145=CARTESIAN_POINT('Ctrl Pts',(5.35149757048,-38.2372245963,5.60065251681));
#66146=CARTESIAN_POINT('Ctrl Pts',(5.4456922481,-38.2742356128,5.60381584892));
#66147=CARTESIAN_POINT('Ctrl Pts',(5.53988692571,-38.2742356128,5.60697918103));
#66148=CARTESIAN_POINT('',(4.3914713655969,-37.9742356128,1.85521069141137));
#66149=CARTESIAN_POINT('Ctrl Pts',(5.2400559546,-37.9742356128,5.59690998219));
#66150=CARTESIAN_POINT('Ctrl Pts',(5.2418605608663,-37.9742356128,5.54317414306575));
#66151=CARTESIAN_POINT('Ctrl Pts',(5.24315737610566,-37.9742356128,5.48920776658016));
#66152=CARTESIAN_POINT('Ctrl Pts',(5.24376788585,-37.9742356128,5.43508810427703));
#66153=CARTESIAN_POINT('Ctrl Pts',(5.24439174263741,-37.9742356128,5.37978527090855));
#66154=CARTESIAN_POINT('Ctrl Pts',(5.24429909977124,-37.9742356128,5.32432243841033));
#66155=CARTESIAN_POINT('Ctrl Pts',(5.24335412274884,-37.9742356128,5.26877728160842));
#66156=CARTESIAN_POINT('Ctrl Pts',(5.24238610864014,-37.9742356128,5.2118780193198));
#66157=CARTESIAN_POINT('Ctrl Pts',(5.24052385945121,-37.9742356128,5.15489244461267));
#66158=CARTESIAN_POINT('Ctrl Pts',(5.23767577778745,-37.9742356128,5.0978980588865));
#66159=CARTESIAN_POINT('Ctrl Pts',(5.23470185843848,-37.9742356128,5.03838547234427));
#66160=CARTESIAN_POINT('Ctrl Pts',(5.23065312103343,-37.9742356128,4.97886339674345));
#66161=CARTESIAN_POINT('Ctrl Pts',(5.22548247270875,-37.9742356128,4.91941208132394));
#66162=CARTESIAN_POINT('Ctrl Pts',(5.22014830848689,-37.9742356128,4.85808068538671));
#66163=CARTESIAN_POINT('Ctrl Pts',(5.21362040513255,-37.9742356128,4.7968247209684));
#66164=CARTESIAN_POINT('Ctrl Pts',(5.20590409543257,-37.9742356128,4.73572210301911));
#66165=CARTESIAN_POINT('Ctrl Pts',(5.19790447046991,-37.9742356128,4.67237601572666));
#66166=CARTESIAN_POINT('Ctrl Pts',(5.18862788453177,-37.9742356128,4.60919490621015));
#66167=CARTESIAN_POINT('Ctrl Pts',(5.17813629890928,-37.9742356128,4.54625254168015));
#66168=CARTESIAN_POINT('Ctrl Pts',(5.16719017838142,-37.9742356128,4.48058327744837));
#66169=CARTESIAN_POINT('Ctrl Pts',(5.15492191671971,-37.9742356128,4.41517411713375));
#66170=CARTESIAN_POINT('Ctrl Pts',(5.14145615885331,-37.9742356128,4.35009182413807));
#66171=CARTESIAN_POINT('Ctrl Pts',(5.12692746384431,-37.9742356128,4.27987217554486));
#66172=CARTESIAN_POINT('Ctrl Pts',(5.11100518230485,-37.9742356128,4.21003348647402));
#66173=CARTESIAN_POINT('Ctrl Pts',(5.09390154139431,-37.9742356128,4.14063468475526));
#66174=CARTESIAN_POINT('Ctrl Pts',(5.07529743225982,-37.9742356128,4.06514766490191));
#66175=CARTESIAN_POINT('Ctrl Pts',(5.05529654521998,-37.9742356128,3.99018183403256));
#66176=CARTESIAN_POINT('Ctrl Pts',(5.03422469803328,-37.9742356128,3.91577491776497));
#66177=CARTESIAN_POINT('Ctrl Pts',(5.01581896365487,-37.9742356128,3.85078232719598));
#66178=CARTESIAN_POINT('Ctrl Pts',(4.99659773718505,-37.9742356128,3.78621567165843));
#66179=CARTESIAN_POINT('Ctrl Pts',(4.9767959506457,-37.9742356128,3.72207308531392));
#66180=CARTESIAN_POINT('Ctrl Pts',(4.95996155632885,-37.9742356128,3.66754257167158));
#66181=CARTESIAN_POINT('Ctrl Pts',(4.94270644688682,-37.9742356128,3.6133124923039));
#66182=CARTESIAN_POINT('Ctrl Pts',(4.92516971522254,-37.9742356128,3.55925405827158));
#66183=CARTESIAN_POINT('Ctrl Pts',(4.90642740291784,-37.9742356128,3.50147932163688));
#66184=CARTESIAN_POINT('Ctrl Pts',(4.88736441624655,-37.9742356128,3.44390092271876));
#66185=CARTESIAN_POINT('Ctrl Pts',(4.86816362318974,-37.9742356128,3.38642084337562));
#66186=CARTESIAN_POINT('Ctrl Pts',(4.84680217663087,-37.9742356128,3.32247256585111));
#66187=CARTESIAN_POINT('Ctrl Pts',(4.82527213582349,-37.9742356128,3.25864633151042));
#66188=CARTESIAN_POINT('Ctrl Pts',(4.80381712909044,-37.9742356128,3.19487377343086));
#66189=CARTESIAN_POINT('Ctrl Pts',(4.78399437868539,-37.9742356128,3.13595291093793));
#66190=CARTESIAN_POINT('Ctrl Pts',(4.76423690135756,-37.9742356128,3.07707965248936));
#66191=CARTESIAN_POINT('Ctrl Pts',(4.74470721823347,-37.9742356128,3.01823474641582));
#66192=CARTESIAN_POINT('Ctrl Pts',(4.72646159352314,-37.9742356128,2.96325883792256));
#66193=CARTESIAN_POINT('Ctrl Pts',(4.7084154678586,-37.9742356128,2.9083087377769));
#66194=CARTESIAN_POINT('Ctrl Pts',(4.69066177721658,-37.9742356128,2.85338122442281));
#66195=CARTESIAN_POINT('Ctrl Pts',(4.67394673917456,-37.9742356128,2.80166716148346));
#66196=CARTESIAN_POINT('Ctrl Pts',(4.65749130213224,-37.9742356128,2.74997378582983));
#66197=CARTESIAN_POINT('Ctrl Pts',(4.64132952175512,-37.9742356128,2.69829811051436));
#66198=CARTESIAN_POINT('Ctrl Pts',(4.62594632441804,-37.9742356128,2.64911187655035));
#66199=CARTESIAN_POINT('Ctrl Pts',(4.61082943066444,-37.9742356128,2.5999421252798));
#66200=CARTESIAN_POINT('Ctrl Pts',(4.59596307105996,-37.9742356128,2.55077829977098));
#66201=CARTESIAN_POINT('Ctrl Pts',(4.58169099754295,-37.9742356128,2.50357980930611));
#66202=CARTESIAN_POINT('Ctrl Pts',(4.56765002431437,-37.9742356128,2.4563871039601));
#66203=CARTESIAN_POINT('Ctrl Pts',(4.55378028303625,-37.9742356128,2.40917787062285));
#66204=CARTESIAN_POINT('Ctrl Pts',(4.54031359363548,-37.9742356128,2.36334052806158));
#66205=CARTESIAN_POINT('Ctrl Pts',(4.52700852277083,-37.9742356128,2.3174878454883));
#66206=CARTESIAN_POINT('Ctrl Pts',(4.51376315077643,-37.9742356128,2.27158273796349));
#66207=CARTESIAN_POINT('Ctrl Pts',(4.50111844828701,-37.9742356128,2.22775939894054));
#66208=CARTESIAN_POINT('Ctrl Pts',(4.48852817727415,-37.9742356128,2.1838885088515));
#66209=CARTESIAN_POINT('Ctrl Pts',(4.4758590226742,-37.9742356128,2.1399200426657));
#66210=CARTESIAN_POINT('Ctrl Pts',(4.4634537013424,-37.9742356128,2.09686721327618));
#66211=CARTESIAN_POINT('Ctrl Pts',(4.45097289120161,-37.9742356128,2.05372100321262));
#66212=CARTESIAN_POINT('Ctrl Pts',(4.43824617315795,-37.9742356128,2.0104141381816));
#66213=CARTESIAN_POINT('Ctrl Pts',(4.42584830060044,-37.9742356128,1.9682262786189));
#66214=CARTESIAN_POINT('Ctrl Pts',(4.41321713264896,-37.9742356128,1.92588608013858));
#66215=CARTESIAN_POINT('Ctrl Pts',(4.40015024268932,-37.9742356128,1.8833097637315));
#66216=CARTESIAN_POINT('Ctrl Pts',(4.39728088028414,-37.9742356128,1.87396041725143));
#66217=CARTESIAN_POINT('Ctrl Pts',(4.39439032942952,-37.9742356128,1.86459959675658));
#66218=CARTESIAN_POINT('Ctrl Pts',(4.39147614152,-37.9742356128,1.85522626202));
#66219=CARTESIAN_POINT('Ctrl Pts',(4.6779495981,-38.2742356128,1.76615927471));
#66220=CARTESIAN_POINT('Ctrl Pts',(4.58794136979949,-38.2742356128,1.79410813492836));
#66221=CARTESIAN_POINT('Ctrl Pts',(4.4979443455795,-38.2372245963,1.82209348096837));
#66222=CARTESIAN_POINT('Ctrl Pts',(4.4268107174295,-38.1627311721,1.84421309232839));
#66223=CARTESIAN_POINT('Ctrl Pts',(4.3914689686595,-38.0684833924,1.8552029120184));
#66224=CARTESIAN_POINT('Ctrl Pts',(4.39146896866,-37.9742356128,1.85520291202));
#66225=CARTESIAN_POINT('Ctrl Pts',(5.2400559546,-37.9742356128,5.59690998219));
#66226=CARTESIAN_POINT('Ctrl Pts',(5.2400559546,-36.2942356128,5.59690998219));
#66227=CARTESIAN_POINT('Ctrl Pts',(5.25311376105,-37.9742356128,5.20808711269));
#66228=CARTESIAN_POINT('Ctrl Pts',(5.25311376105,-36.2942356128,5.20808711269));
#66229=CARTESIAN_POINT('Ctrl Pts',(5.24470483276,-37.9742356128,4.80219931419));
#66230=CARTESIAN_POINT('Ctrl Pts',(5.24470483276,-36.2942356128,4.80219931419));
#66231=CARTESIAN_POINT('Ctrl Pts',(5.17504642388,-37.9742356128,4.39981761669));
#66232=CARTESIAN_POINT('Ctrl Pts',(5.17504642388,-36.2942356128,4.39981761669));
#66233=CARTESIAN_POINT('Ctrl Pts',(5.00839926013,-37.9742356128,3.79030695888));
#66234=CARTESIAN_POINT('Ctrl Pts',(5.00839926013,-36.2942356128,3.79030695888));
#66235=CARTESIAN_POINT('Ctrl Pts',(4.81153097626,-37.9742356128,3.21707824383));
#66236=CARTESIAN_POINT('Ctrl Pts',(4.81153097626,-36.2942356128,3.21707824383));
#66237=CARTESIAN_POINT('Ctrl Pts',(4.73686810339,-37.9742356128,3.00222967268));
#66238=CARTESIAN_POINT('Ctrl Pts',(4.73686810339,-36.2942356128,3.00222967268));
#66239=CARTESIAN_POINT('Ctrl Pts',(4.62316453236,-37.9742356128,2.6499539825));
#66240=CARTESIAN_POINT('Ctrl Pts',(4.62316453236,-36.2942356128,2.6499539825));
#66241=CARTESIAN_POINT('Ctrl Pts',(4.51875357768,-37.9742356128,2.29074629441));
#66242=CARTESIAN_POINT('Ctrl Pts',(4.51875357768,-36.2942356128,2.29074629441));
#66243=CARTESIAN_POINT('Ctrl Pts',(4.47967500948,-37.9742356128,2.15155097848));
#66244=CARTESIAN_POINT('Ctrl Pts',(4.47967500948,-36.2942356128,2.15155097848));
#66245=CARTESIAN_POINT('Ctrl Pts',(4.43790342458,-37.9742356128,2.00456060561));
#66246=CARTESIAN_POINT('Ctrl Pts',(4.43790342458,-36.2942356128,2.00456060561));
#66247=CARTESIAN_POINT('Ctrl Pts',(4.39146896866,-37.9742356128,1.85520291202));
#66248=CARTESIAN_POINT('Ctrl Pts',(4.39146896866,-36.2942356128,1.85520291202));
#66249=CARTESIAN_POINT('',(4.39146896866,-37.2742356128,1.85520291202));
#66250=CARTESIAN_POINT('Ctrl Pts',(4.67793839402,-36.2742356128,1.76612278889));
#66251=CARTESIAN_POINT('Ctrl Pts',(4.5879413698,-36.2742356128,1.79410813493));
#66252=CARTESIAN_POINT('Ctrl Pts',(4.49794434558,-36.3112466293,1.82209348097));
#66253=CARTESIAN_POINT('Ctrl Pts',(4.42681071743,-36.3857400536,1.84421309233));
#66254=CARTESIAN_POINT('Ctrl Pts',(4.39146896866,-36.4799878332,1.85520291202));
#66255=CARTESIAN_POINT('Ctrl Pts',(4.39146896866,-36.5742356128,1.85520291202));
#66256=CARTESIAN_POINT('Ctrl Pts',(4.57998241553,-36.2742356128,1.45110983336));
#66257=CARTESIAN_POINT('Ctrl Pts',(4.49109393546,-36.2742356128,1.48266010491));
#66258=CARTESIAN_POINT('Ctrl Pts',(4.40220545538,-36.3112466293,1.51421037645));
#66259=CARTESIAN_POINT('Ctrl Pts',(4.33194802025,-36.3857400536,1.5391477041));
#66260=CARTESIAN_POINT('Ctrl Pts',(4.29704159577,-36.4799878332,1.5515374668));
#66261=CARTESIAN_POINT('Ctrl Pts',(4.29704159577,-36.5742356128,1.5515374668));
#66262=CARTESIAN_POINT('Ctrl Pts',(4.46666859078,-36.2742356128,1.14155311765));
#66263=CARTESIAN_POINT('Ctrl Pts',(4.3790579831,-36.2742356128,1.17661454934));
#66264=CARTESIAN_POINT('Ctrl Pts',(4.29144737541,-36.3112466293,1.21167598103));
#66265=CARTESIAN_POINT('Ctrl Pts',(4.22219997042,-36.3857400536,1.23938852904));
#66266=CARTESIAN_POINT('Ctrl Pts',(4.18779536517,-36.4799878332,1.25315712095));
#66267=CARTESIAN_POINT('Ctrl Pts',(4.18779536517,-36.5742356128,1.25315712095));
#66268=CARTESIAN_POINT('Ctrl Pts',(4.33903994549,-36.2742356128,0.842275524713));
#66269=CARTESIAN_POINT('Ctrl Pts',(4.25305209744,-36.2742356128,0.881099274512));
#66270=CARTESIAN_POINT('Ctrl Pts',(4.16706424939,-36.3112466293,0.919923024311));
#66271=CARTESIAN_POINT('Ctrl Pts',(4.09909947328,-36.3857400536,0.950609307675));
#66272=CARTESIAN_POINT('Ctrl Pts',(4.06533212422,-36.4799878332,0.96585535851));
#66273=CARTESIAN_POINT('Ctrl Pts',(4.06533212422,-36.5742356128,0.96585535851));
#66274=CARTESIAN_POINT('Ctrl Pts',(4.09052289333,-36.2742356128,0.331506343655));
#66275=CARTESIAN_POINT('Ctrl Pts',(4.00737841693,-36.2742356128,0.37623718636));
#66276=CARTESIAN_POINT('Ctrl Pts',(3.92423394053,-36.3112466293,0.420968029064));
#66277=CARTESIAN_POINT('Ctrl Pts',(3.8585165647,-36.3857400536,0.456323277416));
#66278=CARTESIAN_POINT('Ctrl Pts',(3.82586580513,-36.4799878332,0.473889038156));
#66279=CARTESIAN_POINT('Ctrl Pts',(3.82586580513,-36.5742356128,0.473889038156));
#66280=CARTESIAN_POINT('Ctrl Pts',(3.79239464833,-36.2742356128,-0.161386595149));
#66281=CARTESIAN_POINT('Ctrl Pts',(3.71291098531,-36.2742356128,-0.110612175752));
#66282=CARTESIAN_POINT('Ctrl Pts',(3.6334273223,-36.3112466293,-0.0598377563554));
#66283=CARTESIAN_POINT('Ctrl Pts',(3.57060345243,-36.3857400536,-0.0197056666316));
#66284=CARTESIAN_POINT('Ctrl Pts',(3.53939029105,-36.4799878332,0.000233401443254));
#66285=CARTESIAN_POINT('Ctrl Pts',(3.53939029105,-36.5742356128,0.000233401443254));
#66286=CARTESIAN_POINT('Ctrl Pts',(3.65536373033,-36.2742356128,-0.369783971346));
#66287=CARTESIAN_POINT('Ctrl Pts',(3.57749719054,-36.2742356128,-0.316462440475));
#66288=CARTESIAN_POINT('Ctrl Pts',(3.49963065075,-36.3112466293,-0.263140909604));
#66289=CARTESIAN_POINT('Ctrl Pts',(3.43808495466,-36.3857400536,-0.220995583714));
#66290=CARTESIAN_POINT('Ctrl Pts',(3.40750683616,-36.4799878332,-0.200056267119));
#66291=CARTESIAN_POINT('Ctrl Pts',(3.40750683616,-36.5742356128,-0.200056267119));
#66292=CARTESIAN_POINT('Ctrl Pts',(3.30318535597,-36.2742356128,-0.851087598324));
#66293=CARTESIAN_POINT('Ctrl Pts',(3.23120788587,-36.2742356128,-0.789523577996));
#66294=CARTESIAN_POINT('Ctrl Pts',(3.15923041576,-36.3112466293,-0.727959557669));
#66295=CARTESIAN_POINT('Ctrl Pts',(3.10233943926,-36.3857400536,-0.679299369581));
#66296=CARTESIAN_POINT('Ctrl Pts',(3.0740739528,-36.4799878332,-0.65512323529));
#66297=CARTESIAN_POINT('Ctrl Pts',(3.0740739528,-36.5742356128,-0.65512323529));
#66298=CARTESIAN_POINT('Ctrl Pts',(2.87113584445,-36.2742356128,-1.27814713268));
#66299=CARTESIAN_POINT('Ctrl Pts',(2.80938320589,-36.2742356128,-1.20614411812));
#66300=CARTESIAN_POINT('Ctrl Pts',(2.74763056733,-36.3112466293,-1.13414110356));
#66301=CARTESIAN_POINT('Ctrl Pts',(2.69882129557,-36.3857400536,-1.07722993587));
#66302=CARTESIAN_POINT('Ctrl Pts',(2.67457109093,-36.4799878332,-1.04895441899));
#66303=CARTESIAN_POINT('Ctrl Pts',(2.67457109093,-36.5742356128,-1.04895441899));
#66304=CARTESIAN_POINT('Ctrl Pts',(2.59469364023,-36.2742356128,-1.49279721696));
#66305=CARTESIAN_POINT('Ctrl Pts',(2.54027280659,-36.2742356128,-1.41505897416));
#66306=CARTESIAN_POINT('Ctrl Pts',(2.48585197294,-36.3112466293,-1.33732073137));
#66307=CARTESIAN_POINT('Ctrl Pts',(2.44283775848,-36.3857400536,-1.27587644097));
#66308=CARTESIAN_POINT('Ctrl Pts',(2.42146674659,-36.4799878332,-1.2453487048));
#66309=CARTESIAN_POINT('Ctrl Pts',(2.42146674659,-36.5742356128,-1.2453487048));
#66310=CARTESIAN_POINT('Ctrl Pts',(2.05156482251,-36.2742356128,-1.81763077189));
#66311=CARTESIAN_POINT('Ctrl Pts',(2.0106619921,-36.2742356128,-1.73209067968));
#66312=CARTESIAN_POINT('Ctrl Pts',(1.96975916169,-36.3112466293,-1.64655058747));
#66313=CARTESIAN_POINT('Ctrl Pts',(1.93742957283,-36.3857400536,-1.57893971761));
#66314=CARTESIAN_POINT('Ctrl Pts',(1.92136706958,-36.4799878332,-1.54534820173));
#66315=CARTESIAN_POINT('Ctrl Pts',(1.92136706958,-36.5742356128,-1.54534820173));
#66316=CARTESIAN_POINT('Ctrl Pts',(1.46621585586,-36.2742356128,-2.03976910007));
#66317=CARTESIAN_POINT('Ctrl Pts',(1.43612509201,-36.2742356128,-1.95024888238));
#66318=CARTESIAN_POINT('Ctrl Pts',(1.40603432816,-36.3112466293,-1.86072866468));
#66319=CARTESIAN_POINT('Ctrl Pts',(1.38225059583,-36.3857400536,-1.78997190419));
#66320=CARTESIAN_POINT('Ctrl Pts',(1.37043397969,-36.4799878332,-1.75481739701));
#66321=CARTESIAN_POINT('Ctrl Pts',(1.37043397969,-36.5742356128,-1.75481739701));
#66322=CARTESIAN_POINT('Ctrl Pts',(1.20096079265,-36.2742356128,-2.12158773605));
#66323=CARTESIAN_POINT('Ctrl Pts',(1.17485210137,-36.2742356128,-2.03091619783));
#66324=CARTESIAN_POINT('Ctrl Pts',(1.14874341008,-36.3112466293,-1.9402446596));
#66325=CARTESIAN_POINT('Ctrl Pts',(1.1281071041,-36.3857400536,-1.86857789613));
#66326=CARTESIAN_POINT('Ctrl Pts',(1.11785424713,-36.4799878332,-1.83297126593));
#66327=CARTESIAN_POINT('Ctrl Pts',(1.11785424713,-36.5742356128,-1.83297126593));
#66328=CARTESIAN_POINT('Ctrl Pts',(0.933912767205,-36.2742356128,-2.18966247475));
#66329=CARTESIAN_POINT('Ctrl Pts',(0.911433093068,-36.2742356128,-2.09806650676));
#66330=CARTESIAN_POINT('Ctrl Pts',(0.888953418932,-36.3112466293,-2.00647053877));
#66331=CARTESIAN_POINT('Ctrl Pts',(0.871185490918,-36.3857400536,-1.93407310555));
#66332=CARTESIAN_POINT('Ctrl Pts',(0.862357742047,-36.4799878332,-1.89810345328));
#66333=CARTESIAN_POINT('Ctrl Pts',(0.862357742047,-36.5742356128,-1.89810345328));
#66334=CARTESIAN_POINT('Ctrl Pts',(0.665819006916,-36.2742356128,-2.24488956153));
#66335=CARTESIAN_POINT('Ctrl Pts',(0.646803823438,-36.2742356128,-2.1525799373));
#66336=CARTESIAN_POINT('Ctrl Pts',(0.62778863996,-36.3112466293,-2.06027031307));
#66337=CARTESIAN_POINT('Ctrl Pts',(0.61275904312,-36.3857400536,-1.98730880637));
#66338=CARTESIAN_POINT('Ctrl Pts',(0.60529179803,-36.4799878332,-1.9510589017));
#66339=CARTESIAN_POINT('Ctrl Pts',(0.60529179803,-36.5742356128,-1.9510589017));
#66340=CARTESIAN_POINT('',(0.605290655172242,-36.5742356128,-1.95105912937464));
#66341=CARTESIAN_POINT('Origin',(0.665390956717112,-36.5721143394352,-2.24281192044095));
#66342=CARTESIAN_POINT('Ctrl Pts',(4.39146896866,-36.5742356128,1.85520291202));
#66343=CARTESIAN_POINT('Ctrl Pts',(4.37092196604576,-36.5742356128,1.78912657731079));
#66344=CARTESIAN_POINT('Ctrl Pts',(4.34954081826218,-36.5742356128,1.72337655738574));
#66345=CARTESIAN_POINT('Ctrl Pts',(4.32735621433135,-36.5742356128,1.65805460794794));
#66346=CARTESIAN_POINT('Ctrl Pts',(4.30394651649965,-36.5742356128,1.58912540358241));
#66347=CARTESIAN_POINT('Ctrl Pts',(4.27964214656061,-36.5742356128,1.52067245888467));
#66348=CARTESIAN_POINT('Ctrl Pts',(4.25446325957601,-36.5742356128,1.45275525337923));
#66349=CARTESIAN_POINT('Ctrl Pts',(4.22739691464107,-36.5742356128,1.37974684310469));
#66350=CARTESIAN_POINT('Ctrl Pts',(4.19931999946701,-36.5742356128,1.30735692636008));
#66351=CARTESIAN_POINT('Ctrl Pts',(4.17024000686726,-36.5742356128,1.23559918194585));
#66352=CARTESIAN_POINT('Ctrl Pts',(4.14145877587494,-36.5742356128,1.16457866120843));
#66353=CARTESIAN_POINT('Ctrl Pts',(4.11169470089405,-36.5742356128,1.09417596395447));
#66354=CARTESIAN_POINT('Ctrl Pts',(4.08094114779705,-36.5742356128,1.02436413798126));
#66355=CARTESIAN_POINT('Ctrl Pts',(4.05224188440922,-36.5742356128,0.959215633843538));
#66356=CARTESIAN_POINT('Ctrl Pts',(4.02268063301999,-36.5742356128,0.894580469895503));
#66357=CARTESIAN_POINT('Ctrl Pts',(3.99224395132627,-36.5742356128,0.830420695088611));
#66358=CARTESIAN_POINT('Ctrl Pts',(3.97438465138359,-36.5742356128,0.792773731005568));
#66359=CARTESIAN_POINT('Ctrl Pts',(3.95622027870181,-36.5742356128,0.755282652752562));
#66360=CARTESIAN_POINT('Ctrl Pts',(3.9377422209914,-36.5742356128,0.717930475626564));
#66361=CARTESIAN_POINT('Ctrl Pts',(3.89734005075921,-36.5742356128,0.6362601484505));
#66362=CARTESIAN_POINT('Ctrl Pts',(3.8554424832124,-36.5742356128,0.555257996223974));
#66363=CARTESIAN_POINT('Ctrl Pts',(3.81197125901739,-36.5742356128,0.474816458033809));
#66364=CARTESIAN_POINT('Ctrl Pts',(3.80028137999852,-36.5742356128,0.453184864561387));
#66365=CARTESIAN_POINT('Ctrl Pts',(3.78847763386018,-36.5742356128,0.43159407411124));
#66366=CARTESIAN_POINT('Ctrl Pts',(3.77655836304664,-36.5742356128,0.410042706612038));
#66367=CARTESIAN_POINT('Ctrl Pts',(3.74584468184793,-36.5742356128,0.354508954495743));
#66368=CARTESIAN_POINT('Ctrl Pts',(3.71436491605534,-36.5742356128,0.299232780038763));
#66369=CARTESIAN_POINT('Ctrl Pts',(3.68208980817337,-36.5742356128,0.244210156230315));
#66370=CARTESIAN_POINT('Ctrl Pts',(3.64900348421455,-36.5742356128,0.187804570754112));
#66371=CARTESIAN_POINT('Ctrl Pts',(3.61508141465514,-36.5742356128,0.131665655865529));
#66372=CARTESIAN_POINT('Ctrl Pts',(3.58027857454058,-36.5742356128,0.0758427834194556));
#66373=CARTESIAN_POINT('Ctrl Pts',(3.54514722605774,-36.5742356128,0.0194929918863461));
#66374=CARTESIAN_POINT('Ctrl Pts',(3.50911845896627,-36.5742356128,-0.0365343947094508));
#66375=CARTESIAN_POINT('Ctrl Pts',(3.47213137149065,-36.5742356128,-0.0921391827048448));
#66376=CARTESIAN_POINT('Ctrl Pts',(3.43827624511192,-36.5742356128,-0.143035515812656));
#66377=CARTESIAN_POINT('Ctrl Pts',(3.40361565818781,-36.5742356128,-0.193580240571943));
#66378=CARTESIAN_POINT('Ctrl Pts',(3.3681038842297,-36.5742356128,-0.243648133987124));
#66379=CARTESIAN_POINT('Ctrl Pts',(3.32237639859336,-36.5742356128,-0.308119114222706));
#66380=CARTESIAN_POINT('Ctrl Pts',(3.27523990322948,-36.5742356128,-0.371798238816327));
#66381=CARTESIAN_POINT('Ctrl Pts',(3.22658364237517,-36.5742356128,-0.434351343972338));
#66382=CARTESIAN_POINT('Ctrl Pts',(3.1891805104024,-36.5742356128,-0.482437284124252));
#66383=CARTESIAN_POINT('Ctrl Pts',(3.15087884016424,-36.5742356128,-0.529856326762846));
#66384=CARTESIAN_POINT('Ctrl Pts',(3.11161932172789,-36.5742356128,-0.576438135300435));
#66385=CARTESIAN_POINT('Ctrl Pts',(3.07634816132177,-36.5742356128,-0.618287717424055));
#66386=CARTESIAN_POINT('Ctrl Pts',(3.04030401646786,-36.5742356128,-0.659457592247737));
#66387=CARTESIAN_POINT('Ctrl Pts',(3.00347671654498,-36.5742356128,-0.699843781432812));
#66388=CARTESIAN_POINT('Ctrl Pts',(2.95584798283857,-36.5742356128,-0.752075225338318));
#66389=CARTESIAN_POINT('Ctrl Pts',(2.90690574095255,-36.5742356128,-0.802997650979128));
#66390=CARTESIAN_POINT('Ctrl Pts',(2.85663353129263,-36.5742356128,-0.852444677426488));
#66391=CARTESIAN_POINT('Ctrl Pts',(2.80616628734769,-36.5742356128,-0.902083536807286));
#66392=CARTESIAN_POINT('Ctrl Pts',(2.75435852744095,-36.5742356128,-0.950235664741411));
#66393=CARTESIAN_POINT('Ctrl Pts',(2.70121735198846,-36.5742356128,-0.996779778325614));
#66394=CARTESIAN_POINT('Ctrl Pts',(2.64787457427578,-36.5742356128,-1.04350046682405));
#66395=CARTESIAN_POINT('Ctrl Pts',(2.59318803634864,-36.5742356128,-1.08860107508899));
#66396=CARTESIAN_POINT('Ctrl Pts',(2.5371919504335,-36.5742356128,-1.13200401281568));
#66397=CARTESIAN_POINT('Ctrl Pts',(2.48088732176473,-36.5742356128,-1.17564610407788));
#66398=CARTESIAN_POINT('Ctrl Pts',(2.42325845763622,-36.5742356128,-1.2175719302296));
#66399=CARTESIAN_POINT('Ctrl Pts',(2.36437063367713,-36.5742356128,-1.25774567927551));
#66400=CARTESIAN_POINT('Ctrl Pts',(2.30532530357416,-36.5742356128,-1.29802688028471));
#66401=CARTESIAN_POINT('Ctrl Pts',(2.24501407262125,-36.5742356128,-1.33654682218278));
#66402=CARTESIAN_POINT('Ctrl Pts',(2.18353641291566,-36.5742356128,-1.37330977651211));
#66403=CARTESIAN_POINT('Ctrl Pts',(2.1218304847959,-36.5742356128,-1.41020923280533));
#66404=CARTESIAN_POINT('Ctrl Pts',(2.05894925274633,-36.5742356128,-1.44533884235053));
#66405=CARTESIAN_POINT('Ctrl Pts',(1.99503015932727,-36.5742356128,-1.47874042189916));
#66406=CARTESIAN_POINT('Ctrl Pts',(1.94867287876171,-36.5742356128,-1.5029648955524));
#66407=CARTESIAN_POINT('Ctrl Pts',(1.90177045743172,-36.5742356128,-1.52628124306212));
#66408=CARTESIAN_POINT('Ctrl Pts',(1.85438824548848,-36.5742356128,-1.54871668750062));
#66409=CARTESIAN_POINT('Ctrl Pts',(1.80557874502425,-36.5742356128,-1.57182795206227));
#66410=CARTESIAN_POINT('Ctrl Pts',(1.75626193134941,-36.5742356128,-1.59400511597658));
#66411=CARTESIAN_POINT('Ctrl Pts',(1.70652627741759,-36.5742356128,-1.61529464396692));
#66412=CARTESIAN_POINT('Ctrl Pts',(1.6654769857331,-36.5742356128,-1.63286594292879));
#66413=CARTESIAN_POINT('Ctrl Pts',(1.62415059395768,-36.5742356128,-1.64982906877745));
#66414=CARTESIAN_POINT('Ctrl Pts',(1.58259075611606,-36.5742356128,-1.66621171622079));
#66415=CARTESIAN_POINT('Ctrl Pts',(1.50335243862315,-36.5742356128,-1.69744700218212));
#66416=CARTESIAN_POINT('Ctrl Pts',(1.4232675352806,-36.5742356128,-1.72657363957852));
#66417=CARTESIAN_POINT('Ctrl Pts',(1.34258681478873,-36.5742356128,-1.75377965505486));
#66418=CARTESIAN_POINT('Ctrl Pts',(1.26331159092117,-36.5742356128,-1.78051172876817));
#66419=CARTESIAN_POINT('Ctrl Pts',(1.18346058848082,-36.5742356128,-1.80539021068333));
#66420=CARTESIAN_POINT('Ctrl Pts',(1.1032221367378,-36.5742356128,-1.82857498991327));
#66421=CARTESIAN_POINT('Ctrl Pts',(1.02084982398067,-36.5742356128,-1.85237634505469));
#66422=CARTESIAN_POINT('Ctrl Pts',(0.938068982789468,-36.5742356128,-1.8743936397323));
#66423=CARTESIAN_POINT('Ctrl Pts',(0.85503576346161,-36.5742356128,-1.89476771454273));
#66424=CARTESIAN_POINT('Ctrl Pts',(0.772002544133753,-36.5742356128,-1.91514178935316));
#66425=CARTESIAN_POINT('Ctrl Pts',(0.688716543213015,-36.5742356128,-1.93387344834334));
#66426=CARTESIAN_POINT('Ctrl Pts',(0.60529179803,-36.5742356128,-1.9510589017));
#66427=CARTESIAN_POINT('Ctrl Pts',(0.605291698516,-37.9742356128,-1.9510589194));
#66428=CARTESIAN_POINT('Ctrl Pts',(0.605291702509,-38.0684833924,-1.9510589186));
#66429=CARTESIAN_POINT('Ctrl Pts',(0.612758907916,-38.162731172,-1.98730883125));
#66430=CARTESIAN_POINT('Ctrl Pts',(0.627788420004,-38.2372245963,-2.06027035501));
#66431=CARTESIAN_POINT('Ctrl Pts',(0.64680349383,-38.2742356128,-2.15258000132));
#66432=CARTESIAN_POINT('Ctrl Pts',(0.665818566089,-38.2742356128,-2.24488964795));
#66433=CARTESIAN_POINT('Ctrl Pts',(0.919213880749,-37.9742356128,-1.88639136854));
#66434=CARTESIAN_POINT('Ctrl Pts',(0.919213677207,-38.0684833929,-1.88639140934));
#66435=CARTESIAN_POINT('Ctrl Pts',(0.928343625497,-38.162731173,-1.9222988207));
#66436=CARTESIAN_POINT('Ctrl Pts',(0.946720057801,-38.2372245974,-1.99457092792));
#66437=CARTESIAN_POINT('Ctrl Pts',(0.969969721523,-38.2742356135,-2.0860083113));
#66438=CARTESIAN_POINT('Ctrl Pts',(0.993219464992,-38.2742356128,-2.17744567841));
#66439=CARTESIAN_POINT('Ctrl Pts',(1.23048109925,-37.9742356128,-1.80341900309));
#66440=CARTESIAN_POINT('Ctrl Pts',(1.23048134587,-38.0684833489,-1.8034189616));
#66441=CARTESIAN_POINT('Ctrl Pts',(1.24137540827,-38.162731085,-1.83884940092));
#66442=CARTESIAN_POINT('Ctrl Pts',(1.26330197813,-38.2372244937,-1.91016159119));
#66443=CARTESIAN_POINT('Ctrl Pts',(1.29104294839,-38.2742355444,-2.00038457075));
#66444=CARTESIAN_POINT('Ctrl Pts',(1.31878382917,-38.2742356128,-2.09060759247));
#66445=CARTESIAN_POINT('Ctrl Pts',(1.53827172349,-37.9742356128,-1.70133851312));
#66446=CARTESIAN_POINT('Ctrl Pts',(1.53827165445,-38.0684833944,-1.70133852637));
#66447=CARTESIAN_POINT('Ctrl Pts',(1.55116199328,-38.1627311759,-1.73618774441));
#66448=CARTESIAN_POINT('Ctrl Pts',(1.577106932,-38.2372246008,-1.80633002242));
#66449=CARTESIAN_POINT('Ctrl Pts',(1.60993205855,-38.2742356158,-1.8950727983));
#66450=CARTESIAN_POINT('Ctrl Pts',(1.64275721303,-38.2742356128,-1.98381556726));
#66451=CARTESIAN_POINT('Ctrl Pts',(2.08916968394,-37.9742356128,-1.4617720322));
#66452=CARTESIAN_POINT('Ctrl Pts',(2.08916974353,-38.0684833908,-1.46177202076));
#66453=CARTESIAN_POINT('Ctrl Pts',(2.10696029946,-38.1627311688,-1.49456736992));
#66454=CARTESIAN_POINT('Ctrl Pts',(2.14276792726,-38.2372245925,-1.56057578049));
#66455=CARTESIAN_POINT('Ctrl Pts',(2.18807107629,-38.2742356103,-1.64408847689));
#66456=CARTESIAN_POINT('Ctrl Pts',(2.23337420121,-38.2742356128,-1.72760117925));
#66457=CARTESIAN_POINT('Ctrl Pts',(2.57507298908,-37.9742356128,-1.12324782371));
#66458=CARTESIAN_POINT('Ctrl Pts',(2.57507293765,-38.0684833939,-1.12324783358));
#66459=CARTESIAN_POINT('Ctrl Pts',(2.5981428301,-38.1627311749,-1.15242255957));
#66460=CARTESIAN_POINT('Ctrl Pts',(2.64457651027,-38.2372245997,-1.21114358345));
#66461=CARTESIAN_POINT('Ctrl Pts',(2.7033236223,-38.2742356151,-1.28543639078));
#66462=CARTESIAN_POINT('Ctrl Pts',(2.76207075515,-38.2742356128,-1.35972919295));
#66463=CARTESIAN_POINT('Ctrl Pts',(2.7836528701,-37.9742356128,-0.943576895053));
#66464=CARTESIAN_POINT('Ctrl Pts',(2.78365286427,-38.0684833991,-0.943576903287));
#66465=CARTESIAN_POINT('Ctrl Pts',(2.80899055527,-38.1627311853,-0.970778224792));
#66466=CARTESIAN_POINT('Ctrl Pts',(2.85998865839,-38.237224612,-1.02552730908));
#66467=CARTESIAN_POINT('Ctrl Pts',(2.92451056942,-38.2742356233,-1.09479488721));
#66468=CARTESIAN_POINT('Ctrl Pts',(2.98903247965,-38.2742356128,-1.16406245943));
#66469=CARTESIAN_POINT('Ctrl Pts',(3.16286118659,-37.9742356128,-0.547454755393));
#66470=CARTESIAN_POINT('Ctrl Pts',(3.16286119234,-38.0684833859,-0.547454747271));
#66471=CARTESIAN_POINT('Ctrl Pts',(3.19188224207,-38.162731159,-0.57069685876));
#66472=CARTESIAN_POINT('Ctrl Pts',(3.25029396105,-38.2372245809,-0.617477115127));
#66473=CARTESIAN_POINT('Ctrl Pts',(3.32419544657,-38.2742356026,-0.676662685237));
#66474=CARTESIAN_POINT('Ctrl Pts',(3.39809693287,-38.2742356128,-0.735848261173));
#66475=CARTESIAN_POINT('Ctrl Pts',(3.48018648031,-37.9742356128,-0.0953176293782));
#66476=CARTESIAN_POINT('Ctrl Pts',(3.48018647464,-38.0684833989,-0.0953176373891));
#66477=CARTESIAN_POINT('Ctrl Pts',(3.51119197157,-38.162731185,-0.115616438491));
#66478=CARTESIAN_POINT('Ctrl Pts',(3.57359787491,-38.2372246116,-0.156472565458));
#66479=CARTESIAN_POINT('Ctrl Pts',(3.65255273532,-38.274235623,-0.208163017913));
#66480=CARTESIAN_POINT('Ctrl Pts',(3.73150759497,-38.2742356128,-0.25985346462));
#66481=CARTESIAN_POINT('Ctrl Pts',(3.62537652215,-37.9742356128,0.135235517809));
#66482=CARTESIAN_POINT('Ctrl Pts',(3.62537652521,-38.0684833915,0.135235523567));
#66483=CARTESIAN_POINT('Ctrl Pts',(3.65702258613,-38.1627311701,0.115978596807));
#66484=CARTESIAN_POINT('Ctrl Pts',(3.72071777861,-38.237224594,0.0772195150144));
#66485=CARTESIAN_POINT('Ctrl Pts',(3.80130381638,-38.2742356113,0.0281821786018));
#66486=CARTESIAN_POINT('Ctrl Pts',(3.88188985347,-38.2742356128,-0.0208551603171));
#66487=CARTESIAN_POINT('Ctrl Pts',(3.89322431128,-37.9742356128,0.603415611262));
#66488=CARTESIAN_POINT('Ctrl Pts',(3.89322430822,-38.0684833934,0.603415605503));
#66489=CARTESIAN_POINT('Ctrl Pts',(3.92618569708,-38.162731174,0.586451536215));
#66490=CARTESIAN_POINT('Ctrl Pts',(3.9925282778,-38.2372245987,0.552307296845));
#66491=CARTESIAN_POINT('Ctrl Pts',(4.07646375994,-38.2742356144,0.509108624308));
#66492=CARTESIAN_POINT('Ctrl Pts',(4.16039924278,-38.2742356128,0.465909954278));
#66493=CARTESIAN_POINT('Ctrl Pts',(4.11688435895,-37.9742356128,1.08932953896));
#66494=CARTESIAN_POINT('Ctrl Pts',(4.116884362,-38.0684833915,1.08932954472));
#66495=CARTESIAN_POINT('Ctrl Pts',(4.15092281005,-38.1627311701,1.0747166191));
#66496=CARTESIAN_POINT('Ctrl Pts',(4.21943324733,-38.237224594,1.04530468777));
#66497=CARTESIAN_POINT('Ctrl Pts',(4.3061114488,-38.2742356113,1.00809320298));
#66498=CARTESIAN_POINT('Ctrl Pts',(4.39278964957,-38.2742356128,0.970881715692));
#66499=CARTESIAN_POINT('Ctrl Pts',(4.21879577195,-37.9742356128,1.33879606859));
#66500=CARTESIAN_POINT('Ctrl Pts',(4.21879576946,-38.0684833923,1.33879606025));
#66501=CARTESIAN_POINT('Ctrl Pts',(4.25334110804,-38.1627311718,1.32542139016));
#66502=CARTESIAN_POINT('Ctrl Pts',(4.32287172004,-38.237224596,1.29850153552));
#66503=CARTESIAN_POINT('Ctrl Pts',(4.4108406614,-38.2742356126,1.26444308661));
#66504=CARTESIAN_POINT('Ctrl Pts',(4.49880960361,-38.2742356128,1.23038464024));
#66505=CARTESIAN_POINT('Ctrl Pts',(4.31054313212,-37.9742356128,1.59495655094));
#66506=CARTESIAN_POINT('Ctrl Pts',(4.31054313212,-38.0684833924,1.59495655094));
#66507=CARTESIAN_POINT('Ctrl Pts',(4.34551178853,-38.1627311721,1.58276691751));
#66508=CARTESIAN_POINT('Ctrl Pts',(4.41589451694,-38.2372245963,1.55823251586));
#66509=CARTESIAN_POINT('Ctrl Pts',(4.50494150016,-38.2742356128,1.52719196862));
#66510=CARTESIAN_POINT('Ctrl Pts',(4.59398848352,-38.2742356128,1.49615142185));
#66511=CARTESIAN_POINT('Ctrl Pts',(4.39146896866,-37.9742356128,1.85520291202));
#66512=CARTESIAN_POINT('Ctrl Pts',(4.39146896866,-38.0684833924,1.85520291202));
#66513=CARTESIAN_POINT('Ctrl Pts',(4.42681071743,-38.1627311721,1.84421309233));
#66514=CARTESIAN_POINT('Ctrl Pts',(4.49794434558,-38.2372245963,1.82209348097));
#66515=CARTESIAN_POINT('Ctrl Pts',(4.5879413698,-38.2742356128,1.79410813493));
#66516=CARTESIAN_POINT('Ctrl Pts',(4.67793839402,-38.2742356128,1.76612278889));
#66517=CARTESIAN_POINT('',(0.605290084208,-37.9742356128,-1.95105924441));
#66518=CARTESIAN_POINT('Ctrl Pts',(4.39146896866,-37.9742356128,1.85520291202));
#66519=CARTESIAN_POINT('Ctrl Pts',(4.32479970425,-37.9742356128,1.64080372629));
#66520=CARTESIAN_POINT('Ctrl Pts',(4.25081929042,-37.9742356128,1.42932711758));
#66521=CARTESIAN_POINT('Ctrl Pts',(4.17005920267,-37.9742356128,1.2223938778));
#66522=CARTESIAN_POINT('Ctrl Pts',(3.99422837986,-37.9742356128,0.815818314863));
#66523=CARTESIAN_POINT('Ctrl Pts',(3.78982855046,-37.9742356128,0.424030803924));
#66524=CARTESIAN_POINT('Ctrl Pts',(3.67898467854,-37.9742356128,0.229105997103));
#66525=CARTESIAN_POINT('Ctrl Pts',(3.50079208815,-37.9742356128,-0.0598766153727));
#66526=CARTESIAN_POINT('Ctrl Pts',(3.3007785305,-37.9742356128,-0.339537614852));
#66527=CARTESIAN_POINT('Ctrl Pts',(3.23140437767,-37.9742356128,-0.431505525867));
#66528=CARTESIAN_POINT('Ctrl Pts',(2.94231272615,-37.9742356128,-0.791436832827));
#66529=CARTESIAN_POINT('Ctrl Pts',(2.60717935657,-37.9742356128,-1.11036965749));
#66530=CARTESIAN_POINT('Ctrl Pts',(2.32835178279,-37.9742356128,-1.31285318023));
#66531=CARTESIAN_POINT('Ctrl Pts',(1.82071765691,-37.9742356128,-1.59091161501));
#66532=CARTESIAN_POINT('Ctrl Pts',(1.27370365618,-37.9742356128,-1.78402347955));
#66533=CARTESIAN_POINT('Ctrl Pts',(1.05241756576,-37.9742356128,-1.84948999718));
#66534=CARTESIAN_POINT('Ctrl Pts',(0.829282811325,-37.9742356128,-1.90491676645));
#66535=CARTESIAN_POINT('Ctrl Pts',(0.605290084208,-37.9742356128,-1.95105924441));
#66536=CARTESIAN_POINT('Origin',(0.66539024333551,-37.9763568939093,-2.24281205713374));
#66537=CARTESIAN_POINT('Ctrl Pts',(4.39146896866,-37.9742356128,1.85520291202));
#66538=CARTESIAN_POINT('Ctrl Pts',(4.39146896866,-36.2942356128,1.85520291202));
#66539=CARTESIAN_POINT('Ctrl Pts',(4.32479970425,-37.9742356128,1.64080372629));
#66540=CARTESIAN_POINT('Ctrl Pts',(4.32479970425,-36.2942356128,1.64080372629));
#66541=CARTESIAN_POINT('Ctrl Pts',(4.25081929042,-37.9742356128,1.42932711758));
#66542=CARTESIAN_POINT('Ctrl Pts',(4.25081929042,-36.2942356128,1.42932711758));
#66543=CARTESIAN_POINT('Ctrl Pts',(4.17005920267,-37.9742356128,1.2223938778));
#66544=CARTESIAN_POINT('Ctrl Pts',(4.17005920267,-36.2942356128,1.2223938778));
#66545=CARTESIAN_POINT('Ctrl Pts',(3.99422837986,-37.9742356128,0.815818314863));
#66546=CARTESIAN_POINT('Ctrl Pts',(3.99422837986,-36.2942356128,0.815818314863));
#66547=CARTESIAN_POINT('Ctrl Pts',(3.78982855046,-37.9742356128,0.424030803924));
#66548=CARTESIAN_POINT('Ctrl Pts',(3.78982855046,-36.2942356128,0.424030803924));
#66549=CARTESIAN_POINT('Ctrl Pts',(3.67898467854,-37.9742356128,0.229105997103));
#66550=CARTESIAN_POINT('Ctrl Pts',(3.67898467854,-36.2942356128,0.229105997103));
#66551=CARTESIAN_POINT('Ctrl Pts',(3.50079208815,-37.9742356128,-0.0598766153727));
#66552=CARTESIAN_POINT('Ctrl Pts',(3.50079208815,-36.2942356128,-0.0598766153727));
#66553=CARTESIAN_POINT('Ctrl Pts',(3.3007785305,-37.9742356128,-0.339537614852));
#66554=CARTESIAN_POINT('Ctrl Pts',(3.3007785305,-36.2942356128,-0.339537614852));
#66555=CARTESIAN_POINT('Ctrl Pts',(3.23140437767,-37.9742356128,-0.431505525867));
#66556=CARTESIAN_POINT('Ctrl Pts',(3.23140437767,-36.2942356128,-0.431505525867));
#66557=CARTESIAN_POINT('Ctrl Pts',(2.94231272615,-37.9742356128,-0.791436832827));
#66558=CARTESIAN_POINT('Ctrl Pts',(2.94231272615,-36.2942356128,-0.791436832827));
#66559=CARTESIAN_POINT('Ctrl Pts',(2.60717935657,-37.9742356128,-1.11036965749));
#66560=CARTESIAN_POINT('Ctrl Pts',(2.60717935657,-36.2942356128,-1.11036965749));
#66561=CARTESIAN_POINT('Ctrl Pts',(2.32835178279,-37.9742356128,-1.31285318023));
#66562=CARTESIAN_POINT('Ctrl Pts',(2.32835178279,-36.2942356128,-1.31285318023));
#66563=CARTESIAN_POINT('Ctrl Pts',(1.82071765691,-37.9742356128,-1.59091161501));
#66564=CARTESIAN_POINT('Ctrl Pts',(1.82071765691,-36.2942356128,-1.59091161501));
#66565=CARTESIAN_POINT('Ctrl Pts',(1.27370365618,-37.9742356128,-1.78402347955));
#66566=CARTESIAN_POINT('Ctrl Pts',(1.27370365618,-36.2942356128,-1.78402347955));
#66567=CARTESIAN_POINT('Ctrl Pts',(1.05241756576,-37.9742356128,-1.84948999718));
#66568=CARTESIAN_POINT('Ctrl Pts',(1.05241756576,-36.2942356128,-1.84948999718));
#66569=CARTESIAN_POINT('Ctrl Pts',(0.829282811325,-37.9742356128,-1.90491676645));
#66570=CARTESIAN_POINT('Ctrl Pts',(0.829282811325,-36.2942356128,-1.90491676645));
#66571=CARTESIAN_POINT('Ctrl Pts',(0.605290084208,-37.9742356128,-1.95105924441));
#66572=CARTESIAN_POINT('Ctrl Pts',(0.605290084208,-36.2942356128,-1.95105924441));
#66573=CARTESIAN_POINT('',(0.605290084208,-37.2742356128,-1.95105924441));
#66574=CARTESIAN_POINT('Ctrl Pts',(0.665819092629,-36.2742356128,-2.2448895341));
#66575=CARTESIAN_POINT('Ctrl Pts',(0.64680334381,-36.2742356128,-2.15258002616));
#66576=CARTESIAN_POINT('Ctrl Pts',(0.627787594992,-36.3112466293,-2.06027051821));
#66577=CARTESIAN_POINT('Ctrl Pts',(0.612757551307,-36.3857400536,-1.98730910342));
#66578=CARTESIAN_POINT('Ctrl Pts',(0.605290084208,-36.4799878332,-1.95105924441));
#66579=CARTESIAN_POINT('Ctrl Pts',(0.605290084208,-36.5742356128,-1.95105924441));
#66580=CARTESIAN_POINT('Ctrl Pts',(0.534429719062,-36.2742356128,-2.27195573108));
#66581=CARTESIAN_POINT('Ctrl Pts',(0.519212546478,-36.2742356128,-2.17886371683));
#66582=CARTESIAN_POINT('Ctrl Pts',(0.503995373894,-36.3112466293,-2.08577170258));
#66583=CARTESIAN_POINT('Ctrl Pts',(0.491967724046,-36.3857400536,-2.01219179502));
#66584=CARTESIAN_POINT('Ctrl Pts',(0.48599195433,-36.4799878332,-1.97563464648));
#66585=CARTESIAN_POINT('Ctrl Pts',(0.48599195433,-36.5742356128,-1.97563464648));
#66586=CARTESIAN_POINT('Ctrl Pts',(0.401708001693,-36.2742356128,-2.29225119574));
#66587=CARTESIAN_POINT('Ctrl Pts',(0.390294367497,-36.2742356128,-2.19857933068));
#66588=CARTESIAN_POINT('Ctrl Pts',(0.3788807333,-36.3112466293,-2.10490746561));
#66589=CARTESIAN_POINT('Ctrl Pts',(0.369859399314,-36.3857400536,-2.03086924402));
#66590=CARTESIAN_POINT('Ctrl Pts',(0.365377275672,-36.4799878332,-1.99408438867));
#66591=CARTESIAN_POINT('Ctrl Pts',(0.365377275672,-36.5742356128,-1.99408438867));
#66592=CARTESIAN_POINT('Ctrl Pts',(0.268094966815,-36.2742356128,-2.30577886056));
#66593=CARTESIAN_POINT('Ctrl Pts',(0.260489352365,-36.2742356128,-2.21172355227));
#66594=CARTESIAN_POINT('Ctrl Pts',(0.252883737915,-36.3112466293,-2.11766824397));
#66595=CARTESIAN_POINT('Ctrl Pts',(0.246872116974,-36.3857400536,-2.0433269187));
#66596=CARTESIAN_POINT('Ctrl Pts',(0.243885544115,-36.4799878332,-2.00639151578));
#66597=CARTESIAN_POINT('Ctrl Pts',(0.243885544115,-36.5742356128,-2.00639151578));
#66598=CARTESIAN_POINT('Ctrl Pts',(5.76690590749E-6,-36.2742356128,-2.31931022318));
#66599=CARTESIAN_POINT('Ctrl Pts',(1.95516921384E-6,-36.2742356128,-2.2248691397));
#66600=CARTESIAN_POINT('Ctrl Pts',(-1.85656748074E-6,-36.3112466293,-2.13042805622));
#66601=CARTESIAN_POINT('Ctrl Pts',(-4.72441517072E-6,-36.3857400536,-2.05578187487));
#66602=CARTESIAN_POINT('Ctrl Pts',(-6.36622882408E-6,-36.4799878332,-2.01869491784));
#66603=CARTESIAN_POINT('Ctrl Pts',(-6.36622882421E-6,-36.5742356128,-2.01869491784));
#66604=CARTESIAN_POINT('Ctrl Pts',(-0.268106045432,-36.2742356128,-2.30577884111));
#66605=CARTESIAN_POINT('Ctrl Pts',(-0.260493021619,-36.2742356128,-2.21172353811));
#66606=CARTESIAN_POINT('Ctrl Pts',(-0.252879997805,-36.3112466293,-2.11766823512));
#66607=CARTESIAN_POINT('Ctrl Pts',(-0.246862810402,-36.3857400536,-2.04332691403));
#66608=CARTESIAN_POINT('Ctrl Pts',(-0.243873037996,-36.4799878332,-2.00639151319));
#66609=CARTESIAN_POINT('Ctrl Pts',(-0.243873037996,-36.5742356128,-2.00639151319));
#66610=CARTESIAN_POINT('Ctrl Pts',(-0.401685240587,-36.2742356128,-2.29225613481));
#66611=CARTESIAN_POINT('Ctrl Pts',(-0.390286664018,-36.2742356128,-2.19858115746));
#66612=CARTESIAN_POINT('Ctrl Pts',(-0.378888087449,-36.3112466293,-2.10490618011));
#66613=CARTESIAN_POINT('Ctrl Pts',(-0.369878075217,-36.3857400536,-2.03086561975));
#66614=CARTESIAN_POINT('Ctrl Pts',(-0.365402444484,-36.4799878332,-1.99407942103));
#66615=CARTESIAN_POINT('Ctrl Pts',(-0.365402444484,-36.5742356128,-1.99407942103));
#66616=CARTESIAN_POINT('Ctrl Pts',(-0.53444473621,-36.2742356128,-2.27195243343));
#66617=CARTESIAN_POINT('Ctrl Pts',(-0.519217514301,-36.2742356128,-2.17886250595));
#66618=CARTESIAN_POINT('Ctrl Pts',(-0.503990292391,-36.3112466293,-2.08577257847));
#66619=CARTESIAN_POINT('Ctrl Pts',(-0.491955086087,-36.3857400536,-2.0121942395));
#66620=CARTESIAN_POINT('Ctrl Pts',(-0.485974983482,-36.4799878332,-1.97563799122));
#66621=CARTESIAN_POINT('Ctrl Pts',(-0.485974983482,-36.5742356128,-1.97563799122));
#66622=CARTESIAN_POINT('Ctrl Pts',(-0.665818883669,-36.2742356128,-2.24488957828));
#66623=CARTESIAN_POINT('Ctrl Pts',(-0.646803200563,-36.2742356128,-2.1525800567));
#66624=CARTESIAN_POINT('Ctrl Pts',(-0.627787517457,-36.3112466293,-2.06027053512));
#66625=CARTESIAN_POINT('Ctrl Pts',(-0.612757525711,-36.3857400536,-1.98730910956));
#66626=CARTESIAN_POINT('Ctrl Pts',(-0.605290084417,-36.4799878332,-1.9510592452));
#66627=CARTESIAN_POINT('Ctrl Pts',(-0.605290084417,-36.5742356128,-1.9510592452));
#66628=CARTESIAN_POINT('',(-0.605290084208,-36.5742356128,-1.95105924441));
#66629=CARTESIAN_POINT('Origin',(-0.665390756021192,-36.5721143232865,-2.24281194064002));
#66630=CARTESIAN_POINT('Origin',(3.40005801291454E-15,-36.5742356128,0.240847787955639));
#66631=CARTESIAN_POINT('Ctrl Pts',(-0.605290082239,-37.9742356128,-1.95105923702));
#66632=CARTESIAN_POINT('Ctrl Pts',(-0.605290082237,-38.0684833924,-1.95105923702));
#66633=CARTESIAN_POINT('Ctrl Pts',(-0.612757635964,-38.1627311719,-1.98730907779));
#66634=CARTESIAN_POINT('Ctrl Pts',(-0.627787854008,-38.2372245962,-2.06027045589));
#66635=CARTESIAN_POINT('Ctrl Pts',(-0.646803823428,-38.2742356128,-2.15257991743));
#66636=CARTESIAN_POINT('Ctrl Pts',(-0.665819792855,-38.2742356128,-2.24488937901));
#66637=CARTESIAN_POINT('Ctrl Pts',(-0.485962182438,-37.9742356128,-1.97564071896));
#66638=CARTESIAN_POINT('Ctrl Pts',(-0.485962182542,-38.0684833923,-1.97564071893));
#66639=CARTESIAN_POINT('Ctrl Pts',(-0.491944923867,-38.1627311718,-2.0121964271));
#66640=CARTESIAN_POINT('Ctrl Pts',(-0.503985876403,-38.237224596,-2.08577358875));
#66641=CARTESIAN_POINT('Ctrl Pts',(-0.519220185478,-38.2742356126,-2.17886206466));
#66642=CARTESIAN_POINT('Ctrl Pts',(-0.534454494532,-38.2742356128,-2.27195054066));
#66643=CARTESIAN_POINT('Ctrl Pts',(-0.365419065041,-37.9742356128,-1.99407581982));
#66644=CARTESIAN_POINT('Ctrl Pts',(-0.365419081723,-38.0684833948,-1.99407581622));
#66645=CARTESIAN_POINT('Ctrl Pts',(-0.369890629768,-38.1627311768,-2.03086284972));
#66646=CARTESIAN_POINT('Ctrl Pts',(-0.378891751271,-38.2372246019,-2.10490523008));
#66647=CARTESIAN_POINT('Ctrl Pts',(-0.390279343346,-38.2742356166,-2.19858245447));
#66648=CARTESIAN_POINT('Ctrl Pts',(-0.40166692858,-38.2742356128,-2.29225967882));
#66649=CARTESIAN_POINT('Ctrl Pts',(-0.243866233741,-37.9742356128,-2.0063927176));
#66650=CARTESIAN_POINT('Ctrl Pts',(-0.24386627647,-38.0684833946,-2.00639271368));
#66651=CARTESIAN_POINT('Ctrl Pts',(-0.246856907969,-38.1627311764,-2.04332784119));
#66652=CARTESIAN_POINT('Ctrl Pts',(-0.252876527386,-38.2372246015,-2.11766870518));
#66653=CARTESIAN_POINT('Ctrl Pts',(-0.260492285044,-38.2742356162,-2.21172339427));
#66654=CARTESIAN_POINT('Ctrl Pts',(-0.268108025841,-38.2742356128,-2.3057780836));
#66655=CARTESIAN_POINT('Ctrl Pts',(-9.79524459687E-6,-37.9742356128,-2.01869408534));
#66656=CARTESIAN_POINT('Ctrl Pts',(-9.85391250738E-6,-38.0684833926,-2.01869408524));
#66657=CARTESIAN_POINT('Ctrl Pts',(-7.45742464767E-6,-38.1627311723,-2.05578125539));
#66658=CARTESIAN_POINT('Ctrl Pts',(-2.24378715802E-6,-38.2372245966,-2.1304277776));
#66659=CARTESIAN_POINT('Ctrl Pts',(4.25428334891E-6,-38.2742356131,-2.22486932944));
#66660=CARTESIAN_POINT('Ctrl Pts',(1.07753114626E-5,-38.2742356128,-2.31931088122));
#66661=CARTESIAN_POINT('Ctrl Pts',(0.24388974966,-37.9742356128,-2.00639262475));
#66662=CARTESIAN_POINT('Ctrl Pts',(0.243889710559,-38.06848339,-2.00639262888));
#66663=CARTESIAN_POINT('Ctrl Pts',(0.246875395247,-38.1627311672,-2.04332774367));
#66664=CARTESIAN_POINT('Ctrl Pts',(0.252884521209,-38.2372245906,-2.11766857213));
#66665=CARTESIAN_POINT('Ctrl Pts',(0.26048731995,-38.274235609,-2.21172321325));
#66666=CARTESIAN_POINT('Ctrl Pts',(0.268090134128,-38.2742356128,-2.30577785428));
#66667=CARTESIAN_POINT('Ctrl Pts',(0.365375386943,-37.9742356128,-1.99408468454));
#66668=CARTESIAN_POINT('Ctrl Pts',(0.365375378581,-38.0684833912,-1.99408468674));
#66669=CARTESIAN_POINT('Ctrl Pts',(0.369856652983,-38.1627311695,-2.03086969573));
#66670=CARTESIAN_POINT('Ctrl Pts',(0.378878655381,-38.2372245932,-2.10490773566));
#66671=CARTESIAN_POINT('Ctrl Pts',(0.390292146263,-38.2742356108,-2.19857957522));
#66672=CARTESIAN_POINT('Ctrl Pts',(0.401705640577,-38.2742356128,-2.29225141461));
#66673=CARTESIAN_POINT('Ctrl Pts',(0.485990680767,-37.9742356128,-1.97563490883));
#66674=CARTESIAN_POINT('Ctrl Pts',(0.485990680767,-38.0684833924,-1.97563490883));
#66675=CARTESIAN_POINT('Ctrl Pts',(0.491966958449,-38.1627311721,-2.01219195263));
#66676=CARTESIAN_POINT('Ctrl Pts',(0.50399405237,-38.2372245964,-2.08577197488));
#66677=CARTESIAN_POINT('Ctrl Pts',(0.519211184386,-38.2742356128,-2.17886399742));
#66678=CARTESIAN_POINT('Ctrl Pts',(0.534428316418,-38.2742356128,-2.27195602003));
#66679=CARTESIAN_POINT('Ctrl Pts',(0.605290084208,-37.9742356128,-1.95105924441));
#66680=CARTESIAN_POINT('Ctrl Pts',(0.605290084208,-38.0684833924,-1.95105924441));
#66681=CARTESIAN_POINT('Ctrl Pts',(0.612757551307,-38.1627311721,-1.98730910342));
#66682=CARTESIAN_POINT('Ctrl Pts',(0.627787594992,-38.2372245963,-2.06027051821));
#66683=CARTESIAN_POINT('Ctrl Pts',(0.64680334381,-38.2742356128,-2.15258002616));
#66684=CARTESIAN_POINT('Ctrl Pts',(0.665819092629,-38.2742356128,-2.2448895341));
#66685=CARTESIAN_POINT('',(-0.605290084208,-37.9742356128,-1.95105924441));
#66686=CARTESIAN_POINT('Origin',(0.,-37.9742356128,0.240847787949066));
#66687=CARTESIAN_POINT('Origin',(-0.665392224177974,-37.9763569242406,-2.24281160936468));
#66688=CARTESIAN_POINT('Ctrl Pts',(0.605290084208,-37.9742356128,-1.95105924441));
#66689=CARTESIAN_POINT('Ctrl Pts',(0.605290084208,-36.2942356128,-1.95105924441));
#66690=CARTESIAN_POINT('Ctrl Pts',(0.366514216845,-37.9742356128,-2.00024704769));
#66691=CARTESIAN_POINT('Ctrl Pts',(0.366514216845,-36.2942356128,-2.00024704769));
#66692=CARTESIAN_POINT('Ctrl Pts',(0.122728100002,-37.9742356128,-2.02484094933));
#66693=CARTESIAN_POINT('Ctrl Pts',(0.122728100002,-36.2942356128,-2.02484094933));
#66694=CARTESIAN_POINT('Ctrl Pts',(-0.122728100002,-37.9742356128,-2.02484094933));
#66695=CARTESIAN_POINT('Ctrl Pts',(-0.122728100002,-36.2942356128,-2.02484094933));
#66696=CARTESIAN_POINT('Ctrl Pts',(-0.366514216845,-37.9742356128,-2.00024704769));
#66697=CARTESIAN_POINT('Ctrl Pts',(-0.366514216845,-36.2942356128,-2.00024704769));
#66698=CARTESIAN_POINT('Ctrl Pts',(-0.605290084208,-37.9742356128,-1.95105924441));
#66699=CARTESIAN_POINT('Ctrl Pts',(-0.605290084208,-36.2942356128,-1.95105924441));
#66700=CARTESIAN_POINT('',(-0.605290084208,-37.2742356128,-1.95105924441));
#66701=CARTESIAN_POINT('Ctrl Pts',(-0.665819092629,-36.2742356128,-2.2448895341));
#66702=CARTESIAN_POINT('Ctrl Pts',(-0.64680334381,-36.2742356128,-2.15258002616));
#66703=CARTESIAN_POINT('Ctrl Pts',(-0.627787594992,-36.3112466293,-2.06027051821));
#66704=CARTESIAN_POINT('Ctrl Pts',(-0.612757551307,-36.3857400536,-1.98730910342));
#66705=CARTESIAN_POINT('Ctrl Pts',(-0.605290084208,-36.4799878332,-1.95105924441));
#66706=CARTESIAN_POINT('Ctrl Pts',(-0.605290084208,-36.5742356128,-1.95105924441));
#66707=CARTESIAN_POINT('Ctrl Pts',(-0.993149878416,-36.2742356128,-2.17745942705));
#66708=CARTESIAN_POINT('Ctrl Pts',(-0.969939828056,-36.2742356128,-2.08601394477));
#66709=CARTESIAN_POINT('Ctrl Pts',(-0.946729777696,-36.3112466293,-1.9945684625));
#66710=CARTESIAN_POINT('Ctrl Pts',(-0.928384559091,-36.3857400536,-1.92228997336));
#66711=CARTESIAN_POINT('Ctrl Pts',(-0.919269993533,-36.4799878332,-1.88637941649));
#66712=CARTESIAN_POINT('Ctrl Pts',(-0.919269993533,-36.5742356128,-1.88637941649));
#66713=CARTESIAN_POINT('Ctrl Pts',(-1.31927689012,-36.2742356128,-2.09049838771));
#66714=CARTESIAN_POINT('Ctrl Pts',(-1.29146795967,-36.2742356128,-2.00028752065));
#66715=CARTESIAN_POINT('Ctrl Pts',(-1.26365902922,-36.3112466293,-1.91007665359));
#66716=CARTESIAN_POINT('Ctrl Pts',(-1.24167885673,-36.3857400536,-1.83877400414));
#66717=CARTESIAN_POINT('Ctrl Pts',(-1.23075831525,-36.4799878332,-1.80334827944));
#66718=CARTESIAN_POINT('Ctrl Pts',(-1.23075831525,-36.5742356128,-1.80334827944));
#66719=CARTESIAN_POINT('Ctrl Pts',(-1.64288399014,-36.2742356128,-1.98376552099));
#66720=CARTESIAN_POINT('Ctrl Pts',(-1.6100782863,-36.2742356128,-1.89502207335));
#66721=CARTESIAN_POINT('Ctrl Pts',(-1.57727258247,-36.3112466293,-1.80627862572));
#66722=CARTESIAN_POINT('Ctrl Pts',(-1.551342962,-36.3857400536,-1.73613582402));
#66723=CARTESIAN_POINT('Ctrl Pts',(-1.53846019159,-36.4799878332,-1.70128635382));
#66724=CARTESIAN_POINT('Ctrl Pts',(-1.53846019159,-36.5742356128,-1.70128635382));
#66725=CARTESIAN_POINT('Ctrl Pts',(-2.20014530314,-36.2742356128,-1.7420059745));
#66726=CARTESIAN_POINT('Ctrl Pts',(-2.15552738159,-36.2742356128,-1.65820058714));
#66727=CARTESIAN_POINT('Ctrl Pts',(-2.11090946003,-36.3112466293,-1.57439519979));
#66728=CARTESIAN_POINT('Ctrl Pts',(-2.07564346457,-36.3857400536,-1.50815544015));
#66729=CARTESIAN_POINT('Ctrl Pts',(-2.05812204783,-36.4799878332,-1.47524514139));
#66730=CARTESIAN_POINT('Ctrl Pts',(-2.05812204783,-36.5742356128,-1.47524514139));
#66731=CARTESIAN_POINT('Ctrl Pts',(-2.70184643694,-36.2742356128,-1.40107771811));
#66732=CARTESIAN_POINT('Ctrl Pts',(-2.64463417724,-36.2742356128,-1.32575196136));
#66733=CARTESIAN_POINT('Ctrl Pts',(-2.58742191754,-36.3112466293,-1.2504262046));
#66734=CARTESIAN_POINT('Ctrl Pts',(-2.54220135981,-36.3857400536,-1.19088874298));
#66735=CARTESIAN_POINT('Ctrl Pts',(-2.51973415821,-36.4799878332,-1.16130838751));
#66736=CARTESIAN_POINT('Ctrl Pts',(-2.51973415821,-36.5742356128,-1.16130838751));
#66737=CARTESIAN_POINT('Ctrl Pts',(-2.90464199721,-36.2742356128,-1.23493234649));
#66738=CARTESIAN_POINT('Ctrl Pts',(-2.84222259825,-36.2742356128,-1.16389392384));
#66739=CARTESIAN_POINT('Ctrl Pts',(-2.77980319928,-36.3112466293,-1.09285550119));
#66740=CARTESIAN_POINT('Ctrl Pts',(-2.73046692003,-36.3857400536,-1.03670674729));
#66741=CARTESIAN_POINT('Ctrl Pts',(-2.70595487941,-36.4799878332,-1.00881002421));
#66742=CARTESIAN_POINT('Ctrl Pts',(-2.70595487941,-36.5742356128,-1.00881002421));
#66743=CARTESIAN_POINT('Ctrl Pts',(-3.33998426273,-36.2742356128,-0.811260038282));
#66744=CARTESIAN_POINT('Ctrl Pts',(-3.26725361199,-36.2742356128,-0.750410980921));
#66745=CARTESIAN_POINT('Ctrl Pts',(-3.19452296125,-36.3112466293,-0.68956192356));
#66746=CARTESIAN_POINT('Ctrl Pts',(-3.13703667098,-36.3857400536,-0.64146684195));
#66747=CARTESIAN_POINT('Ctrl Pts',(-3.10847541114,-36.4799878332,-0.617571473053));
#66748=CARTESIAN_POINT('Ctrl Pts',(-3.10847541114,-36.5742356128,-0.617571473053));
#66749=CARTESIAN_POINT('Ctrl Pts',(-3.69323929211,-36.2742356128,-0.324903072136));
#66750=CARTESIAN_POINT('Ctrl Pts',(-3.61456370902,-36.2742356128,-0.272640413673));
#66751=CARTESIAN_POINT('Ctrl Pts',(-3.53588812594,-36.3112466293,-0.220377755209));
#66752=CARTESIAN_POINT('Ctrl Pts',(-3.47370296218,-36.3857400536,-0.17906936204));
#66753=CARTESIAN_POINT('Ctrl Pts',(-3.44280713313,-36.4799878332,-0.158545863464));
#66754=CARTESIAN_POINT('Ctrl Pts',(-3.44280713313,-36.5742356128,-0.158545863464));
#66755=CARTESIAN_POINT('Ctrl Pts',(-3.87117184632,-36.2742356128,-0.0435637631917));
#66756=CARTESIAN_POINT('Ctrl Pts',(-3.79075207379,-36.2742356128,0.00579319803729));
#66757=CARTESIAN_POINT('Ctrl Pts',(-3.71033230126,-36.3112466293,0.0551501592663));
#66758=CARTESIAN_POINT('Ctrl Pts',(-3.64676853057,-36.3857400536,0.0941618898987));
#66759=CARTESIAN_POINT('Ctrl Pts',(-3.6151877599,-36.4799878332,0.11354432392));
#66760=CARTESIAN_POINT('Ctrl Pts',(-3.6151877599,-36.5742356128,0.11354432392));
#66761=CARTESIAN_POINT('Ctrl Pts',(-4.16626079964,-36.2742356128,0.473398136763));
#66762=CARTESIAN_POINT('Ctrl Pts',(-4.0822299908,-36.2742356128,0.516477026574));
#66763=CARTESIAN_POINT('Ctrl Pts',(-3.99819918195,-36.3112466293,0.559555916386));
#66764=CARTESIAN_POINT('Ctrl Pts',(-3.93178124925,-36.3857400536,0.593605461971));
#66765=CARTESIAN_POINT('Ctrl Pts',(-3.89878242765,-36.4799878332,0.610522501891));
#66766=CARTESIAN_POINT('Ctrl Pts',(-3.89878242765,-36.5742356128,0.610522501891));
#66767=CARTESIAN_POINT('Ctrl Pts',(-4.40933595991,-36.2742356128,1.0118987705));
#66768=CARTESIAN_POINT('Ctrl Pts',(-4.32247527463,-36.2742356128,1.04863663853));
#66769=CARTESIAN_POINT('Ctrl Pts',(-4.23561458935,-36.3112466293,1.08537450657));
#66770=CARTESIAN_POINT('Ctrl Pts',(-4.16695992269,-36.3857400536,1.11441210894));
#66771=CARTESIAN_POINT('Ctrl Pts',(-4.13284981146,-36.4799878332,1.12883903643));
#66772=CARTESIAN_POINT('Ctrl Pts',(-4.13284981146,-36.5742356128,1.12883903643));
#66773=CARTESIAN_POINT('Ctrl Pts',(-4.50885918571,-36.2742356128,1.25857748739));
#66774=CARTESIAN_POINT('Ctrl Pts',(-4.42076765288,-36.2742356128,1.29228565071));
#66775=CARTESIAN_POINT('Ctrl Pts',(-4.33267612006,-36.3112466293,1.32599381403));
#66776=CARTESIAN_POINT('Ctrl Pts',(-4.26304859229,-36.3857400536,1.35263674045));
#66777=CARTESIAN_POINT('Ctrl Pts',(-4.22845512783,-36.4799878332,1.36587390368));
#66778=CARTESIAN_POINT('Ctrl Pts',(-4.22845512783,-36.5742356128,1.36587390368));
#66779=CARTESIAN_POINT('Ctrl Pts',(-4.59842586631,-36.2742356128,1.51040085421));
#66780=CARTESIAN_POINT('Ctrl Pts',(-4.50933622176,-36.2742356128,1.54130452507));
#66781=CARTESIAN_POINT('Ctrl Pts',(-4.42024657721,-36.3112466293,1.57220819593));
#66782=CARTESIAN_POINT('Ctrl Pts',(-4.34983014146,-36.3857400536,1.59663444954));
#66783=CARTESIAN_POINT('Ctrl Pts',(-4.31484472014,-36.4799878332,1.60877029375));
#66784=CARTESIAN_POINT('Ctrl Pts',(-4.31484472014,-36.5742356128,1.60877029375));
#66785=CARTESIAN_POINT('Ctrl Pts',(-4.67790780735,-36.2742356128,1.7660244085));
#66786=CARTESIAN_POINT('Ctrl Pts',(-4.58791007919,-36.2742356128,1.79400748948));
#66787=CARTESIAN_POINT('Ctrl Pts',(-4.49791235104,-36.3112466293,1.82199057046));
#66788=CARTESIAN_POINT('Ctrl Pts',(-4.42677816649,-36.3857400536,1.84410839151));
#66789=CARTESIAN_POINT('Ctrl Pts',(-4.39143614129,-36.4799878332,1.85509732172));
#66790=CARTESIAN_POINT('Ctrl Pts',(-4.39143614129,-36.5742356128,1.85509732172));
#66791=CARTESIAN_POINT('Ctrl Pts',(-0.605290084208,-36.5742356128,-1.95105924441));
#66792=CARTESIAN_POINT('Ctrl Pts',(-0.829298136681,-36.5742356128,-1.90491360943));
#66793=CARTESIAN_POINT('Ctrl Pts',(-1.05244809907,-36.5742356128,-1.84948241265));
#66794=CARTESIAN_POINT('Ctrl Pts',(-1.27374925479,-36.5742356128,-1.78401007325));
#66795=CARTESIAN_POINT('Ctrl Pts',(-1.82079921196,-36.5742356128,-1.59087876764));
#66796=CARTESIAN_POINT('Ctrl Pts',(-2.32845991742,-36.5742356128,-1.31278717238));
#66797=CARTESIAN_POINT('Ctrl Pts',(-2.60729776969,-36.5742356128,-1.11027831961));
#66798=CARTESIAN_POINT('Ctrl Pts',(-2.94243947089,-36.5742356128,-0.791306229273));
#66799=CARTESIAN_POINT('Ctrl Pts',(-3.23153488576,-36.5742356128,-0.431337329712));
#66800=CARTESIAN_POINT('Ctrl Pts',(-3.30090973533,-36.5742356128,-0.339360369535));
#66801=CARTESIAN_POINT('Ctrl Pts',(-3.5009243649,-36.5742356128,-0.0596747683079));
#66802=CARTESIAN_POINT('Ctrl Pts',(-3.67911538599,-36.5742356128,0.229327428773));
#66803=CARTESIAN_POINT('Ctrl Pts',(-3.7899456945,-36.5742356128,0.424245491898));
#66804=CARTESIAN_POINT('Ctrl Pts',(-3.99431489394,-36.5742356128,0.816003179174));
#66805=CARTESIAN_POINT('Ctrl Pts',(-4.17012108382,-36.5742356128,1.22254846374));
#66806=CARTESIAN_POINT('Ctrl Pts',(-4.25088448198,-36.5742356128,1.42950202983));
#66807=CARTESIAN_POINT('Ctrl Pts',(-4.32485281869,-36.5742356128,1.64095842297));
#66808=CARTESIAN_POINT('Ctrl Pts',(-4.39143626207,-36.5742356128,1.85509771048));
#66809=CARTESIAN_POINT('Ctrl Pts',(-4.39143629673,-37.9742356128,1.85509783551));
#66810=CARTESIAN_POINT('Ctrl Pts',(-4.39143629608,-38.0684833924,1.85509783338));
#66811=CARTESIAN_POINT('Ctrl Pts',(-4.4267783216,-38.162731172,1.84410890455));
#66812=CARTESIAN_POINT('Ctrl Pts',(-4.49791250759,-38.2372245963,1.82199108888));
#66813=CARTESIAN_POINT('Ctrl Pts',(-4.58791023798,-38.2742356128,1.794008016));
#66814=CARTESIAN_POINT('Ctrl Pts',(-4.67790796861,-38.2742356128,1.76602494395));
#66815=CARTESIAN_POINT('Ctrl Pts',(-4.32501378909,-37.9742356128,1.64147451647));
#66816=CARTESIAN_POINT('Ctrl Pts',(-4.32501382176,-38.0684833927,1.64147462346));
#66817=CARTESIAN_POINT('Ctrl Pts',(-4.36004662084,-38.1627311725,1.62949113947));
#66818=CARTESIAN_POINT('Ctrl Pts',(-4.43055837533,-38.2372245969,1.60537141509));
#66819=CARTESIAN_POINT('Ctrl Pts',(-4.51976859564,-38.2742356132,1.57485549503));
#66820=CARTESIAN_POINT('Ctrl Pts',(-4.608978803,-38.2742356128,1.54433953306));
#66821=CARTESIAN_POINT('Ctrl Pts',(-4.25125101365,-37.9742356128,1.4305487941));
#66822=CARTESIAN_POINT('Ctrl Pts',(-4.25125097569,-38.0684833922,1.43054866879));
#66823=CARTESIAN_POINT('Ctrl Pts',(-4.28594766261,-38.1627311716,1.41760586681));
#66824=CARTESIAN_POINT('Ctrl Pts',(-4.35578299682,-38.2372245958,1.39155556675));
#66825=CARTESIAN_POINT('Ctrl Pts',(-4.44413746573,-38.2742356125,1.35859725952));
#66826=CARTESIAN_POINT('Ctrl Pts',(-4.53249194964,-38.2742356128,1.32563900137));
#66827=CARTESIAN_POINT('Ctrl Pts',(-4.17047868854,-37.9742356128,1.22369574326));
#66828=CARTESIAN_POINT('Ctrl Pts',(-4.17047869492,-38.0684833917,1.22369577109));
#66829=CARTESIAN_POINT('Ctrl Pts',(-4.2047722621,-38.1627311705,1.20973057696));
#66830=CARTESIAN_POINT('Ctrl Pts',(-4.27379616937,-38.2372245945,1.18162228786));
#66831=CARTESIAN_POINT('Ctrl Pts',(-4.36112400783,-38.2742356116,1.14606015377));
#66832=CARTESIAN_POINT('Ctrl Pts',(-4.44845184422,-38.2742356128,1.11049800854));
#66833=CARTESIAN_POINT('Ctrl Pts',(-3.93989107509,-37.9742356128,0.689524409198));
#66834=CARTESIAN_POINT('Ctrl Pts',(-3.93989106463,-38.0684833937,0.689524363603));
#66835=CARTESIAN_POINT('Ctrl Pts',(-3.97309480476,-38.1627311746,0.672998474686));
#66836=CARTESIAN_POINT('Ctrl Pts',(-4.03992519733,-38.2372245994,0.639736268972));
#66837=CARTESIAN_POINT('Ctrl Pts',(-4.12447784909,-38.2742356149,0.597653535716));
#66838=CARTESIAN_POINT('Ctrl Pts',(-4.20903050423,-38.2742356128,0.555570820727));
#66839=CARTESIAN_POINT('Ctrl Pts',(-3.65912020129,-37.9742356128,0.180829797996));
#66840=CARTESIAN_POINT('Ctrl Pts',(-3.65912021842,-38.0684833903,0.180829872687));
#66841=CARTESIAN_POINT('Ctrl Pts',(-3.69090252358,-38.1627311678,0.161760353725));
#66842=CARTESIAN_POINT('Ctrl Pts',(-3.75487190895,-38.2372245914,0.123378347174));
#66843=CARTESIAN_POINT('Ctrl Pts',(-3.83580484849,-38.2742356095,0.0748180560692));
#66844=CARTESIAN_POINT('Ctrl Pts',(-3.91673778248,-38.2742356128,0.0262577350419));
#66845=CARTESIAN_POINT('Ctrl Pts',(-3.46498418373,-37.9742356128,-0.132403747894));
#66846=CARTESIAN_POINT('Ctrl Pts',(-3.46498418837,-38.0684833888,-0.132403740127));
#66847=CARTESIAN_POINT('Ctrl Pts',(-3.49608533501,-38.1627311648,-0.152658499093));
#66848=CARTESIAN_POINT('Ctrl Pts',(-3.55868374308,-38.2372245878,-0.193425999957));
#66849=CARTESIAN_POINT('Ctrl Pts',(-3.63788215363,-38.2742356071,-0.245004336915));
#66850=CARTESIAN_POINT('Ctrl Pts',(-3.71708056344,-38.2742356128,-0.296582679048));
#66851=CARTESIAN_POINT('Ctrl Pts',(-3.0835957445,-37.9742356128,-0.658993075077));
#66852=CARTESIAN_POINT('Ctrl Pts',(-3.083595741,-38.0684833952,-0.658993080934));
#66853=CARTESIAN_POINT('Ctrl Pts',(-3.11202351027,-38.1627311775,-0.683181209926));
#66854=CARTESIAN_POINT('Ctrl Pts',(-3.16924112354,-38.2372246028,-0.731865533214));
#66855=CARTESIAN_POINT('Ctrl Pts',(-3.2416318504,-38.2742356171,-0.793460084306));
#66856=CARTESIAN_POINT('Ctrl Pts',(-3.31402257782,-38.2742356128,-0.855054631493));
#66857=CARTESIAN_POINT('Ctrl Pts',(-2.61204098849,-37.9742356128,-1.09317303329));
#66858=CARTESIAN_POINT('Ctrl Pts',(-2.61204099113,-38.0684833904,-1.09317302887));
#66859=CARTESIAN_POINT('Ctrl Pts',(-2.63556888179,-38.1627311679,-1.12196789197));
#66860=CARTESIAN_POINT('Ctrl Pts',(-2.68292432324,-38.2372245915,-1.17992437049));
#66861=CARTESIAN_POINT('Ctrl Pts',(-2.74283759961,-38.2742356096,-1.25324989821));
#66862=CARTESIAN_POINT('Ctrl Pts',(-2.80275087556,-38.2742356128,-1.32657542887));
#66863=CARTESIAN_POINT('Ctrl Pts',(-2.39238741385,-37.9742356128,-1.25827080622));
#66864=CARTESIAN_POINT('Ctrl Pts',(-2.3923874135,-38.0684833927,-1.2582708065));
#66865=CARTESIAN_POINT('Ctrl Pts',(-2.41346117499,-38.1627311726,-1.28891123921));
#66866=CARTESIAN_POINT('Ctrl Pts',(-2.45587704856,-38.2372245969,-1.3505823687));
#66867=CARTESIAN_POINT('Ctrl Pts',(-2.50954089479,-38.2742356132,-1.4286075996));
#66868=CARTESIAN_POINT('Ctrl Pts',(-2.56320474031,-38.2742356128,-1.50663283058));
#66869=CARTESIAN_POINT('Ctrl Pts',(-1.92260910415,-37.9742356128,-1.54188431467));
#66870=CARTESIAN_POINT('Ctrl Pts',(-1.9226091045,-38.0684833922,-1.54188431439));
#66871=CARTESIAN_POINT('Ctrl Pts',(-1.93875777533,-38.1627311716,-1.57542603916));
#66872=CARTESIAN_POINT('Ctrl Pts',(-1.97126085078,-38.2372245957,-1.6429366818));
#66873=CARTESIAN_POINT('Ctrl Pts',(-2.01238315046,-38.2742356124,-1.72834997312));
#66874=CARTESIAN_POINT('Ctrl Pts',(-2.05350545084,-38.2742356128,-1.81376326435));
#66875=CARTESIAN_POINT('Ctrl Pts',(-1.4052886958,-37.9742356128,-1.74401925817));
#66876=CARTESIAN_POINT('Ctrl Pts',(-1.40528869546,-38.0684833927,-1.74401925844));
#66877=CARTESIAN_POINT('Ctrl Pts',(-1.4173138436,-38.1627311726,-1.77911246411));
#66878=CARTESIAN_POINT('Ctrl Pts',(-1.4415172419,-38.2372245969,-1.84974585166));
#66879=CARTESIAN_POINT('Ctrl Pts',(-1.47213898278,-38.2742356132,-1.93910997524));
#66880=CARTESIAN_POINT('Ctrl Pts',(-1.50276072296,-38.2742356128,-2.0284740989));
#66881=CARTESIAN_POINT('Ctrl Pts',(-1.14123834365,-37.9742356128,-1.82695117915));
#66882=CARTESIAN_POINT('Ctrl Pts',(-1.14123836074,-38.0684834104,-1.82695117356));
#66883=CARTESIAN_POINT('Ctrl Pts',(-1.15164521742,-38.162731208,-1.86251803088));
#66884=CARTESIAN_POINT('Ctrl Pts',(-1.17259168066,-38.2372246386,-1.9341047041));
#66885=CARTESIAN_POINT('Ctrl Pts',(-1.19909267267,-38.274235641,-2.0246749291));
#66886=CARTESIAN_POINT('Ctrl Pts',(-1.22559365574,-38.2742356128,-2.11524514549));
#66887=CARTESIAN_POINT('Ctrl Pts',(-0.874174535988,-37.9742356128,-1.89566907595));
#66888=CARTESIAN_POINT('Ctrl Pts',(-0.874174535988,-38.0684833924,-1.89566907595));
#66889=CARTESIAN_POINT('Ctrl Pts',(-0.88305258586,-38.1627311721,-1.93162835504));
#66890=CARTESIAN_POINT('Ctrl Pts',(-0.900921611695,-38.2372245963,-2.00400493982));
#66891=CARTESIAN_POINT('Ctrl Pts',(-0.923529254725,-38.2742356128,-2.09557451794));
#66892=CARTESIAN_POINT('Ctrl Pts',(-0.946136897282,-38.2742356128,-2.18714409616));
#66893=CARTESIAN_POINT('Ctrl Pts',(-0.605290084208,-37.9742356128,-1.95105924441));
#66894=CARTESIAN_POINT('Ctrl Pts',(-0.605290084208,-38.0684833924,-1.95105924441));
#66895=CARTESIAN_POINT('Ctrl Pts',(-0.612757551307,-38.1627311721,-1.98730910342));
#66896=CARTESIAN_POINT('Ctrl Pts',(-0.627787594992,-38.2372245963,-2.06027051821));
#66897=CARTESIAN_POINT('Ctrl Pts',(-0.64680334381,-38.2742356128,-2.15258002616));
#66898=CARTESIAN_POINT('Ctrl Pts',(-0.665819092629,-38.2742356128,-2.2448895341));
#66899=CARTESIAN_POINT('Ctrl Pts',(-0.605290084208,-37.9742356128,-1.95105924441));
#66900=CARTESIAN_POINT('Ctrl Pts',(-0.829298136681,-37.9742356128,-1.90491360943));
#66901=CARTESIAN_POINT('Ctrl Pts',(-1.05244809907,-37.9742356128,-1.84948241265));
#66902=CARTESIAN_POINT('Ctrl Pts',(-1.27374925479,-37.9742356128,-1.78401007325));
#66903=CARTESIAN_POINT('Ctrl Pts',(-1.82079921196,-37.9742356128,-1.59087876764));
#66904=CARTESIAN_POINT('Ctrl Pts',(-2.32845991742,-37.9742356128,-1.31278717238));
#66905=CARTESIAN_POINT('Ctrl Pts',(-2.60729776969,-37.9742356128,-1.11027831961));
#66906=CARTESIAN_POINT('Ctrl Pts',(-2.94243947089,-37.9742356128,-0.791306229273));
#66907=CARTESIAN_POINT('Ctrl Pts',(-3.23153488576,-37.9742356128,-0.431337329712));
#66908=CARTESIAN_POINT('Ctrl Pts',(-3.30090973533,-37.9742356128,-0.339360369535));
#66909=CARTESIAN_POINT('Ctrl Pts',(-3.5009243649,-37.9742356128,-0.0596747683079));
#66910=CARTESIAN_POINT('Ctrl Pts',(-3.67911538599,-37.9742356128,0.229327428773));
#66911=CARTESIAN_POINT('Ctrl Pts',(-3.7899456945,-37.9742356128,0.424245491898));
#66912=CARTESIAN_POINT('Ctrl Pts',(-3.99431489394,-37.9742356128,0.816003179174));
#66913=CARTESIAN_POINT('Ctrl Pts',(-4.17012108382,-37.9742356128,1.22254846374));
#66914=CARTESIAN_POINT('Ctrl Pts',(-4.25088448198,-37.9742356128,1.42950202983));
#66915=CARTESIAN_POINT('Ctrl Pts',(-4.32485281869,-37.9742356128,1.64095842297));
#66916=CARTESIAN_POINT('Ctrl Pts',(-4.39143626207,-37.9742356128,1.85509771048));
#66917=CARTESIAN_POINT('Ctrl Pts',(-0.605290084208,-37.9742356128,-1.95105924441));
#66918=CARTESIAN_POINT('Ctrl Pts',(-0.605290084208,-36.2942356128,-1.95105924441));
#66919=CARTESIAN_POINT('Ctrl Pts',(-0.829298136681,-37.9742356128,-1.90491360943));
#66920=CARTESIAN_POINT('Ctrl Pts',(-0.829298136681,-36.2942356128,-1.90491360943));
#66921=CARTESIAN_POINT('Ctrl Pts',(-1.05244809907,-37.9742356128,-1.84948241265));
#66922=CARTESIAN_POINT('Ctrl Pts',(-1.05244809907,-36.2942356128,-1.84948241265));
#66923=CARTESIAN_POINT('Ctrl Pts',(-1.27374925479,-37.9742356128,-1.78401007325));
#66924=CARTESIAN_POINT('Ctrl Pts',(-1.27374925479,-36.2942356128,-1.78401007325));
#66925=CARTESIAN_POINT('Ctrl Pts',(-1.82079921196,-37.9742356128,-1.59087876764));
#66926=CARTESIAN_POINT('Ctrl Pts',(-1.82079921196,-36.2942356128,-1.59087876764));
#66927=CARTESIAN_POINT('Ctrl Pts',(-2.32845991742,-37.9742356128,-1.31278717238));
#66928=CARTESIAN_POINT('Ctrl Pts',(-2.32845991742,-36.2942356128,-1.31278717238));
#66929=CARTESIAN_POINT('Ctrl Pts',(-2.60729776969,-37.9742356128,-1.11027831961));
#66930=CARTESIAN_POINT('Ctrl Pts',(-2.60729776969,-36.2942356128,-1.11027831961));
#66931=CARTESIAN_POINT('Ctrl Pts',(-2.94243947089,-37.9742356128,-0.791306229273));
#66932=CARTESIAN_POINT('Ctrl Pts',(-2.94243947089,-36.2942356128,-0.791306229273));
#66933=CARTESIAN_POINT('Ctrl Pts',(-3.23153488576,-37.9742356128,-0.431337329712));
#66934=CARTESIAN_POINT('Ctrl Pts',(-3.23153488576,-36.2942356128,-0.431337329712));
#66935=CARTESIAN_POINT('Ctrl Pts',(-3.30090973533,-37.9742356128,-0.339360369535));
#66936=CARTESIAN_POINT('Ctrl Pts',(-3.30090973533,-36.2942356128,-0.339360369535));
#66937=CARTESIAN_POINT('Ctrl Pts',(-3.5009243649,-37.9742356128,-0.0596747683079));
#66938=CARTESIAN_POINT('Ctrl Pts',(-3.5009243649,-36.2942356128,-0.0596747683079));
#66939=CARTESIAN_POINT('Ctrl Pts',(-3.67911538599,-37.9742356128,0.229327428773));
#66940=CARTESIAN_POINT('Ctrl Pts',(-3.67911538599,-36.2942356128,0.229327428773));
#66941=CARTESIAN_POINT('Ctrl Pts',(-3.7899456945,-37.9742356128,0.424245491898));
#66942=CARTESIAN_POINT('Ctrl Pts',(-3.7899456945,-36.2942356128,0.424245491898));
#66943=CARTESIAN_POINT('Ctrl Pts',(-3.99431489394,-37.9742356128,0.816003179174));
#66944=CARTESIAN_POINT('Ctrl Pts',(-3.99431489394,-36.2942356128,0.816003179174));
#66945=CARTESIAN_POINT('Ctrl Pts',(-4.17012108382,-37.9742356128,1.22254846374));
#66946=CARTESIAN_POINT('Ctrl Pts',(-4.17012108382,-36.2942356128,1.22254846374));
#66947=CARTESIAN_POINT('Ctrl Pts',(-4.25088448198,-37.9742356128,1.42950202983));
#66948=CARTESIAN_POINT('Ctrl Pts',(-4.25088448198,-36.2942356128,1.42950202983));
#66949=CARTESIAN_POINT('Ctrl Pts',(-4.32485281869,-37.9742356128,1.64095842297));
#66950=CARTESIAN_POINT('Ctrl Pts',(-4.32485281869,-36.2942356128,1.64095842297));
#66951=CARTESIAN_POINT('Ctrl Pts',(-4.39143626207,-37.9742356128,1.85509771048));
#66952=CARTESIAN_POINT('Ctrl Pts',(-4.39143626207,-36.2942356128,1.85509771048));
#66953=CARTESIAN_POINT('Ctrl Pts',(6.2749628032,-36.2742356128,2.72284536858));
#66954=CARTESIAN_POINT('Ctrl Pts',(6.35795872238,-36.2742356128,2.67818754328));
#66955=CARTESIAN_POINT('Ctrl Pts',(6.44095464156,-36.3112466293,2.63352971799));
#66956=CARTESIAN_POINT('Ctrl Pts',(6.50655459783,-36.3857400536,2.59823218269));
#66957=CARTESIAN_POINT('Ctrl Pts',(6.53914701908,-36.4799878332,2.5806950957));
#66958=CARTESIAN_POINT('Ctrl Pts',(6.53914701908,-36.5742356128,2.5806950957));
#66959=CARTESIAN_POINT('Ctrl Pts',(6.38937869213,-36.2742356128,2.93548563502));
#66960=CARTESIAN_POINT('Ctrl Pts',(6.46749860928,-36.2742356128,2.88176583084));
#66961=CARTESIAN_POINT('Ctrl Pts',(6.54561852644,-36.3112466293,2.82804602666));
#66962=CARTESIAN_POINT('Ctrl Pts',(6.60736449151,-36.3857400536,2.78558590522));
#66963=CARTESIAN_POINT('Ctrl Pts',(6.63804211152,-36.4799878332,2.76449018748));
#66964=CARTESIAN_POINT('Ctrl Pts',(6.63804211152,-36.5742356128,2.76449018748));
#66965=CARTESIAN_POINT('Ctrl Pts',(6.53170263971,-36.2742356128,3.13005192025));
#66966=CARTESIAN_POINT('Ctrl Pts',(6.60399596908,-36.2742356128,3.06855847302));
#66967=CARTESIAN_POINT('Ctrl Pts',(6.67628929845,-36.3112466293,3.0070650258));
#66968=CARTESIAN_POINT('Ctrl Pts',(6.7334299304,-36.3857400536,2.95846061908));
#66969=CARTESIAN_POINT('Ctrl Pts',(6.76181945414,-36.4799878332,2.93431219838));
#66970=CARTESIAN_POINT('Ctrl Pts',(6.76181945414,-36.5742356128,2.93431219838));
#66971=CARTESIAN_POINT('Ctrl Pts',(6.69660480532,-36.2742356128,3.30689976551));
#66972=CARTESIAN_POINT('Ctrl Pts',(6.76285398311,-36.2742356128,3.23884417488));
#66973=CARTESIAN_POINT('Ctrl Pts',(6.82910316091,-36.3112466293,3.17078858425));
#66974=CARTESIAN_POINT('Ctrl Pts',(6.88146649653,-36.3857400536,3.11699746158));
#66975=CARTESIAN_POINT('Ctrl Pts',(6.90748248775,-36.4799878332,3.09027209244));
#66976=CARTESIAN_POINT('Ctrl Pts',(6.90748248775,-36.5742356128,3.09027209244));
#66977=CARTESIAN_POINT('Ctrl Pts',(7.04173998877,-36.2742356128,3.59638619596));
#66978=CARTESIAN_POINT('Ctrl Pts',(7.09364765321,-36.2742356128,3.5158611957));
#66979=CARTESIAN_POINT('Ctrl Pts',(7.14555531764,-36.3112466293,3.43533619543));
#66980=CARTESIAN_POINT('Ctrl Pts',(7.18658312387,-36.3857400536,3.37168925288));
#66981=CARTESIAN_POINT('Ctrl Pts',(7.20696721636,-36.4799878332,3.34006715926));
#66982=CARTESIAN_POINT('Ctrl Pts',(7.20696721636,-36.5742356128,3.34006715926));
#66983=CARTESIAN_POINT('Ctrl Pts',(7.47286173787,-36.2742356128,3.78624010848));
#66984=CARTESIAN_POINT('Ctrl Pts',(7.50303684285,-36.2742356128,3.69590303443));
#66985=CARTESIAN_POINT('Ctrl Pts',(7.53321194782,-36.3112466293,3.60556596038));
#66986=CARTESIAN_POINT('Ctrl Pts',(7.55706234467,-36.3857400536,3.53416355611));
#66987=CARTESIAN_POINT('Ctrl Pts',(7.56891208017,-36.4799878332,3.49868827089));
#66988=CARTESIAN_POINT('Ctrl Pts',(7.56891208017,-36.5742356128,3.49868827089));
#66989=CARTESIAN_POINT('Ctrl Pts',(7.68849344064,-36.2742356128,3.84462968135));
#66990=CARTESIAN_POINT('Ctrl Pts',(7.70659023707,-36.2742356128,3.7507417713));
#66991=CARTESIAN_POINT('Ctrl Pts',(7.7246870335,-36.3112466293,3.65685386124));
#66992=CARTESIAN_POINT('Ctrl Pts',(7.73899073929,-36.3857400536,3.58264487732));
#66993=CARTESIAN_POINT('Ctrl Pts',(7.74609733275,-36.4799878332,3.54577518171));
#66994=CARTESIAN_POINT('Ctrl Pts',(7.74609733275,-36.5742356128,3.54577518171));
#66995=CARTESIAN_POINT('Ctrl Pts',(8.13777558599,-36.2742356128,3.88392944679));
#66996=CARTESIAN_POINT('Ctrl Pts',(8.12954327989,-36.2742356128,3.78776614015));
#66997=CARTESIAN_POINT('Ctrl Pts',(8.12131097379,-36.3112466293,3.6916028335));
#66998=CARTESIAN_POINT('Ctrl Pts',(8.11480416094,-36.3857400536,3.61559537748));
#66999=CARTESIAN_POINT('Ctrl Pts',(8.11157134181,-36.4799878332,3.57783213485));
#67000=CARTESIAN_POINT('Ctrl Pts',(8.11157134181,-36.5742356128,3.57783213485));
#67001=CARTESIAN_POINT('Ctrl Pts',(8.57834470762,-36.2742356128,3.76769789992));
#67002=CARTESIAN_POINT('Ctrl Pts',(8.54396564062,-36.2742356128,3.67834598136));
#67003=CARTESIAN_POINT('Ctrl Pts',(8.50958657363,-36.3112466293,3.5889940628));
#67004=CARTESIAN_POINT('Ctrl Pts',(8.48241336454,-36.3857400536,3.51837032565));
#67005=CARTESIAN_POINT('Ctrl Pts',(8.4689127386,-36.4799878332,3.48328190964));
#67006=CARTESIAN_POINT('Ctrl Pts',(8.4689127386,-36.5742356128,3.48328190964));
#67007=CARTESIAN_POINT('Ctrl Pts',(8.78308533434,-36.2742356128,3.66972997816));
#67008=CARTESIAN_POINT('Ctrl Pts',(8.73702748426,-36.2742356128,3.58626986161));
#67009=CARTESIAN_POINT('Ctrl Pts',(8.69096963417,-36.3112466293,3.50280974507));
#67010=CARTESIAN_POINT('Ctrl Pts',(8.65456547339,-36.3857400536,3.43684296027));
#67011=CARTESIAN_POINT('Ctrl Pts',(8.63647864415,-36.4799878332,3.40406817618));
#67012=CARTESIAN_POINT('Ctrl Pts',(8.63647864415,-36.5742356128,3.40406817618));
#67013=CARTESIAN_POINT('Ctrl Pts',(9.14359313033,-36.2742356128,3.42239438786));
#67014=CARTESIAN_POINT('Ctrl Pts',(9.07931134809,-36.2742356128,3.35190041238));
#67015=CARTESIAN_POINT('Ctrl Pts',(9.01502956586,-36.3112466293,3.28140643689));
#67016=CARTESIAN_POINT('Ctrl Pts',(8.96422130469,-36.3857400536,3.22568794017));
#67017=CARTESIAN_POINT('Ctrl Pts',(8.93897786246,-36.4799878332,3.19800509473));
#67018=CARTESIAN_POINT('Ctrl Pts',(8.93897786246,-36.5742356128,3.19800509473));
#67019=CARTESIAN_POINT('Ctrl Pts',(9.41617922373,-36.2742356128,3.11420778463));
#67020=CARTESIAN_POINT('Ctrl Pts',(9.34219142116,-36.2742356128,3.05525548641));
#67021=CARTESIAN_POINT('Ctrl Pts',(9.2682036186,-36.3112466293,2.99630318818));
#67022=CARTESIAN_POINT('Ctrl Pts',(9.20972363117,-36.3857400536,2.94970737964));
#67023=CARTESIAN_POINT('Ctrl Pts',(9.1806687336,-36.4799878332,2.92655679125));
#67024=CARTESIAN_POINT('Ctrl Pts',(9.1806687336,-36.5742356128,2.92655679125));
#67025=CARTESIAN_POINT('Ctrl Pts',(9.53134305607,-36.2742356128,2.95704414661));
#67026=CARTESIAN_POINT('Ctrl Pts',(9.45451736556,-36.2742356128,2.90229899704));
#67027=CARTESIAN_POINT('Ctrl Pts',(9.37769167505,-36.3112466293,2.84755384746));
#67028=CARTESIAN_POINT('Ctrl Pts',(9.31696884576,-36.3857400536,2.80428299887));
#67029=CARTESIAN_POINT('Ctrl Pts',(9.28679928804,-36.4799878332,2.78278492331));
#67030=CARTESIAN_POINT('Ctrl Pts',(9.28679928804,-36.5742356128,2.78278492331));
#67031=CARTESIAN_POINT('Ctrl Pts',(9.6338483591,-36.2742356128,2.80329114362));
#67032=CARTESIAN_POINT('Ctrl Pts',(9.55502306,-36.2742356128,2.75153288562));
#67033=CARTESIAN_POINT('Ctrl Pts',(9.47619776089,-36.3112466293,2.69977462761));
#67034=CARTESIAN_POINT('Ctrl Pts',(9.41389414223,-36.3857400536,2.65886510846));
#67035=CARTESIAN_POINT('Ctrl Pts',(9.38293963923,-36.4799878332,2.63853949148));
#67036=CARTESIAN_POINT('Ctrl Pts',(9.38293963923,-36.5742356128,2.63853949148));
#67037=CARTESIAN_POINT('Ctrl Pts',(9.7282927137,-36.2742356128,2.648549352));
#67038=CARTESIAN_POINT('Ctrl Pts',(9.64784505651,-36.2742356128,2.59944926648));
#67039=CARTESIAN_POINT('Ctrl Pts',(9.56739739932,-36.3112466293,2.55034918096));
#67040=CARTESIAN_POINT('Ctrl Pts',(9.50381158876,-36.3857400536,2.51154048417));
#67041=CARTESIAN_POINT('Ctrl Pts',(9.47221986766,-36.4799878332,2.49225892567));
#67042=CARTESIAN_POINT('Ctrl Pts',(9.47221986766,-36.5742356128,2.49225892567));
#67043=CARTESIAN_POINT('',(6.53914700256713,-36.5742356128,2.58069506468878));
#67044=CARTESIAN_POINT('Origin',(6.27683091638159,-36.5721143212222,2.72184035982094));
#67045=CARTESIAN_POINT('',(9.47221976654,-36.5742356128,2.49225909299));
#67046=CARTESIAN_POINT('Origin',(9.72648221077142,-36.572114319087,2.64744392713833));
#67047=CARTESIAN_POINT('Ctrl Pts',(6.53914701908,-36.5742356128,2.5806950957));
#67048=CARTESIAN_POINT('Ctrl Pts',(6.64407030457,-36.5742356128,2.77569349664));
#67049=CARTESIAN_POINT('Ctrl Pts',(6.77645737493,-36.5742356128,2.95406352232));
#67050=CARTESIAN_POINT('Ctrl Pts',(6.93248240874,-36.5742356128,3.11682904882));
#67051=CARTESIAN_POINT('Ctrl Pts',(7.16744129772,-36.5742356128,3.30480694269));
#67052=CARTESIAN_POINT('Ctrl Pts',(7.4430743744,-36.5742356128,3.43661441301));
#67053=CARTESIAN_POINT('Ctrl Pts',(7.51591788103,-36.5742356128,3.46603879043));
#67054=CARTESIAN_POINT('Ctrl Pts',(7.74013214217,-36.5742356128,3.53951961667));
#67055=CARTESIAN_POINT('Ctrl Pts',(7.97806372235,-36.5742356128,3.56548871191));
#67056=CARTESIAN_POINT('Ctrl Pts',(8.1397340384,-36.5742356128,3.5585372531));
#67057=CARTESIAN_POINT('Ctrl Pts',(8.37641925249,-36.5742356128,3.50886242158));
#67058=CARTESIAN_POINT('Ctrl Pts',(8.59150582736,-36.5742356128,3.41174862899));
#67059=CARTESIAN_POINT('Ctrl Pts',(8.65978894936,-36.5742356128,3.37495922004));
#67060=CARTESIAN_POINT('Ctrl Pts',(8.78922597568,-36.5742356128,3.29398598988));
#67061=CARTESIAN_POINT('Ctrl Pts',(8.90717355699,-36.5742356128,3.19917508688));
#67062=CARTESIAN_POINT('Ctrl Pts',(8.9630009386,-36.5742356128,3.14917335528));
#67063=CARTESIAN_POINT('Ctrl Pts',(9.06741515882,-36.5742356128,3.04621714461));
#67064=CARTESIAN_POINT('Ctrl Pts',(9.16069630403,-36.5742356128,2.93809779909));
#67065=CARTESIAN_POINT('Ctrl Pts',(9.20593013024,-36.5742356128,2.88194354511));
#67066=CARTESIAN_POINT('Ctrl Pts',(9.28925382834,-36.5742356128,2.77218463031));
#67067=CARTESIAN_POINT('Ctrl Pts',(9.36584102959,-36.5742356128,2.66040353433));
#67068=CARTESIAN_POINT('Ctrl Pts',(9.40258508843,-36.5742356128,2.60436998551));
#67069=CARTESIAN_POINT('Ctrl Pts',(9.43799021757,-36.5742356128,2.54834207942));
#67070=CARTESIAN_POINT('Ctrl Pts',(9.47221976654,-36.5742356128,2.49225909299));
#67071=CARTESIAN_POINT('Ctrl Pts',(9.47221982595,-37.9742356128,2.49225899398));
#67072=CARTESIAN_POINT('Ctrl Pts',(9.47221982473,-38.0684833924,2.49225899599));
#67073=CARTESIAN_POINT('Ctrl Pts',(9.50381157396,-38.1627311721,2.51154050833));
#67074=CARTESIAN_POINT('Ctrl Pts',(9.56739744262,-38.2372245963,2.55034910979));
#67075=CARTESIAN_POINT('Ctrl Pts',(9.64784517406,-38.2742356128,2.59944907346));
#67076=CARTESIAN_POINT('Ctrl Pts',(9.72829290598,-38.2742356128,2.64854903634));
#67077=CARTESIAN_POINT('Ctrl Pts',(9.30084216856,-37.9742356128,2.77305159559));
#67078=CARTESIAN_POINT('Ctrl Pts',(9.3008424815,-38.068483393,2.77305108007));
#67079=CARTESIAN_POINT('Ctrl Pts',(9.33120668218,-38.1627311731,2.79434389726));
#67080=CARTESIAN_POINT('Ctrl Pts',(9.39232167794,-38.2372245976,2.83720095717));
#67081=CARTESIAN_POINT('Ctrl Pts',(9.46964300891,-38.2742356137,2.89142344603));
#67082=CARTESIAN_POINT('Ctrl Pts',(9.54696421793,-38.2742356128,2.94564613514));
#67083=CARTESIAN_POINT('Ctrl Pts',(9.10325384448,-37.9742356128,3.047828936));
#67084=CARTESIAN_POINT('Ctrl Pts',(9.10325331016,-38.0684833792,3.04782978338));
#67085=CARTESIAN_POINT('Ctrl Pts',(9.13195333701,-38.1627311456,3.07124731643));
#67086=CARTESIAN_POINT('Ctrl Pts',(9.18971922197,-38.2372245651,3.1183802048));
#67087=CARTESIAN_POINT('Ctrl Pts',(9.26280409441,-38.274235592,3.17801114289));
#67088=CARTESIAN_POINT('Ctrl Pts',(9.33588918162,-38.2742356128,3.23764175597));
#67089=CARTESIAN_POINT('Ctrl Pts',(8.85947148585,-37.9742356128,3.32105398427));
#67090=CARTESIAN_POINT('Ctrl Pts',(8.85947171177,-38.0684834033,3.32105376337));
#67091=CARTESIAN_POINT('Ctrl Pts',(8.88406421364,-38.1627311937,3.35144391715));
#67092=CARTESIAN_POINT('Ctrl Pts',(8.93356227407,-38.2372246218,3.41261140709));
#67093=CARTESIAN_POINT('Ctrl Pts',(8.99618617025,-38.2742356298,3.4899996429));
#67094=CARTESIAN_POINT('Ctrl Pts',(9.05880997629,-38.2742356128,3.56738795876));
#67095=CARTESIAN_POINT('Ctrl Pts',(8.34379427784,-37.9742356128,3.58073008166));
#67096=CARTESIAN_POINT('Ctrl Pts',(8.34379415155,-38.0684833864,3.58073020515));
#67097=CARTESIAN_POINT('Ctrl Pts',(8.35368722351,-38.16273116,3.61862172685));
#67098=CARTESIAN_POINT('Ctrl Pts',(8.37359947265,-38.2372245821,3.69488730857));
#67099=CARTESIAN_POINT('Ctrl Pts',(8.39879220242,-38.2742356033,3.79137708216));
#67100=CARTESIAN_POINT('Ctrl Pts',(8.42398498258,-38.2742356128,3.88786681101));
#67101=CARTESIAN_POINT('Ctrl Pts',(7.79117707007,-37.9742356128,3.55728735353));
#67102=CARTESIAN_POINT('Ctrl Pts',(7.79117714067,-38.0684833958,3.5572872845));
#67103=CARTESIAN_POINT('Ctrl Pts',(7.78531841592,-38.1627311788,3.59445498488));
#67104=CARTESIAN_POINT('Ctrl Pts',(7.77352628455,-38.2372246043,3.66926381121));
#67105=CARTESIAN_POINT('Ctrl Pts',(7.75860703219,-38.2742356182,3.76391069234));
#67106=CARTESIAN_POINT('Ctrl Pts',(7.74368775165,-38.2742356128,3.85855759847));
#67107=CARTESIAN_POINT('Ctrl Pts',(7.59728307538,-37.9742356128,3.51091223408));
#67108=CARTESIAN_POINT('Ctrl Pts',(7.59728306128,-38.0684833949,3.51091223533));
#67109=CARTESIAN_POINT('Ctrl Pts',(7.58611021357,-38.1627311769,3.54668881381));
#67110=CARTESIAN_POINT('Ctrl Pts',(7.56362209461,-38.2372246021,3.61869738931));
#67111=CARTESIAN_POINT('Ctrl Pts',(7.53517058683,-38.2742356167,3.70980148529));
#67112=CARTESIAN_POINT('Ctrl Pts',(7.50671908595,-38.2742356128,3.8009055795));
#67113=CARTESIAN_POINT('Ctrl Pts',(7.21880270622,-37.9742356128,3.34989273073));
#67114=CARTESIAN_POINT('Ctrl Pts',(7.2188027215,-38.0684833898,3.34989272938));
#67115=CARTESIAN_POINT('Ctrl Pts',(7.19863591146,-38.1627311668,3.38170520801));
#67116=CARTESIAN_POINT('Ctrl Pts',(7.15804556552,-38.2372245901,3.44573561926));
#67117=CARTESIAN_POINT('Ctrl Pts',(7.10669129595,-38.2742356087,3.526745664));
#67118=CARTESIAN_POINT('Ctrl Pts',(7.05533701891,-38.2742356128,3.60775571067));
#67119=CARTESIAN_POINT('Ctrl Pts',(6.90753935367,-37.9742356128,3.09037088304));
#67120=CARTESIAN_POINT('Ctrl Pts',(6.90753933711,-38.0684833953,3.09037088451));
#67121=CARTESIAN_POINT('Ctrl Pts',(6.88153012601,-38.1627311778,3.11710058783));
#67122=CARTESIAN_POINT('Ctrl Pts',(6.82918029907,-38.237224603,3.17090013782));
#67123=CARTESIAN_POINT('Ctrl Pts',(6.76294829019,-38.2742356173,3.23896651325));
#67124=CARTESIAN_POINT('Ctrl Pts',(6.69671628941,-38.2742356128,3.30703288659));
#67125=CARTESIAN_POINT('Ctrl Pts',(6.76187341966,-37.9742356128,2.93438141705));
#67126=CARTESIAN_POINT('Ctrl Pts',(6.76187343027,-38.0684833881,2.93438143099));
#67127=CARTESIAN_POINT('Ctrl Pts',(6.7334846788,-38.1627311634,2.9585308759));
#67128=CARTESIAN_POINT('Ctrl Pts',(6.67634622409,-38.2372245862,3.00713850853));
#67129=CARTESIAN_POINT('Ctrl Pts',(6.60405537332,-38.2742356061,3.06863553104));
#67130=CARTESIAN_POINT('Ctrl Pts',(6.53176451731,-38.2742356128,3.13013255146));
#67131=CARTESIAN_POINT('Ctrl Pts',(6.63807025716,-37.9742356128,2.76454249575));
#67132=CARTESIAN_POINT('Ctrl Pts',(6.63807025716,-38.0684833924,2.76454249575));
#67133=CARTESIAN_POINT('Ctrl Pts',(6.60739332257,-38.1627311721,2.78563948738));
#67134=CARTESIAN_POINT('Ctrl Pts',(6.54564831339,-38.2372245963,2.82810138523));
#67135=CARTESIAN_POINT('Ctrl Pts',(6.46752978445,-38.2742356128,2.88182376944));
#67136=CARTESIAN_POINT('Ctrl Pts',(6.38941125501,-38.2742356128,2.93554615267));
#67137=CARTESIAN_POINT('Ctrl Pts',(6.53914701908,-37.9742356128,2.5806950957));
#67138=CARTESIAN_POINT('Ctrl Pts',(6.53914701908,-38.0684833924,2.5806950957));
#67139=CARTESIAN_POINT('Ctrl Pts',(6.50655459783,-38.1627311721,2.59823218269));
#67140=CARTESIAN_POINT('Ctrl Pts',(6.44095464156,-38.2372245963,2.63352971799));
#67141=CARTESIAN_POINT('Ctrl Pts',(6.35795872238,-38.2742356128,2.67818754328));
#67142=CARTESIAN_POINT('Ctrl Pts',(6.2749628032,-38.2742356128,2.72284536858));
#67143=CARTESIAN_POINT('',(6.53914701908,-37.9742356128,2.5806950957));
#67144=CARTESIAN_POINT('Origin',(6.27683084777394,-37.9763569039502,2.72184023891299));
#67145=CARTESIAN_POINT('',(9.47221976654,-37.9742356128,2.49225909299));
#67146=CARTESIAN_POINT('Ctrl Pts',(6.53914701908,-37.9742356128,2.5806950957));
#67147=CARTESIAN_POINT('Ctrl Pts',(6.63807025716,-37.9742356128831,2.76454249575));
#67148=CARTESIAN_POINT('Ctrl Pts',(6.76187341966,-37.9742356128831,2.93438141705));
#67149=CARTESIAN_POINT('Ctrl Pts',(6.90753935367,-37.9742356128831,3.09037088304));
#67150=CARTESIAN_POINT('Ctrl Pts',(7.21880270622,-37.9742356128831,3.34989273073));
#67151=CARTESIAN_POINT('Ctrl Pts',(7.59728307538,-37.9742356128831,3.51091223408));
#67152=CARTESIAN_POINT('Ctrl Pts',(7.79117707007001,-37.9742356128831,3.55728735353));
#67153=CARTESIAN_POINT('Ctrl Pts',(8.34379427784,-37.9742356128831,3.58073008166));
#67154=CARTESIAN_POINT('Ctrl Pts',(8.85947148585001,-37.9742356128831,3.32105398427));
#67155=CARTESIAN_POINT('Ctrl Pts',(9.10325384448,-37.9742356128831,3.047828936));
#67156=CARTESIAN_POINT('Ctrl Pts',(9.30084216856,-37.9742356128831,2.77305159559));
#67157=CARTESIAN_POINT('Ctrl Pts',(9.47221976654,-37.9742356128,2.49225909299));
#67158=CARTESIAN_POINT('Origin',(9.72648242188683,-37.9763569039244,2.64744358737807));
#67159=CARTESIAN_POINT('Ctrl Pts',(6.53914701908,-37.9742356128,2.5806950957));
#67160=CARTESIAN_POINT('Ctrl Pts',(6.53914701908,-36.2942356128,2.5806950957));
#67161=CARTESIAN_POINT('Ctrl Pts',(6.64407030457,-37.9742356128,2.77569349664));
#67162=CARTESIAN_POINT('Ctrl Pts',(6.64407030457,-36.2942356128,2.77569349664));
#67163=CARTESIAN_POINT('Ctrl Pts',(6.77645737493,-37.9742356128,2.95406352232));
#67164=CARTESIAN_POINT('Ctrl Pts',(6.77645737493,-36.2942356128,2.95406352232));
#67165=CARTESIAN_POINT('Ctrl Pts',(6.93248240874,-37.9742356128,3.11682904882));
#67166=CARTESIAN_POINT('Ctrl Pts',(6.93248240874,-36.2942356128,3.11682904882));
#67167=CARTESIAN_POINT('Ctrl Pts',(7.16744129772,-37.9742356128,3.30480694269));
#67168=CARTESIAN_POINT('Ctrl Pts',(7.16744129772,-36.2942356128,3.30480694269));
#67169=CARTESIAN_POINT('Ctrl Pts',(7.4430743744,-37.9742356128,3.43661441301));
#67170=CARTESIAN_POINT('Ctrl Pts',(7.4430743744,-36.2942356128,3.43661441301));
#67171=CARTESIAN_POINT('Ctrl Pts',(7.51591788103,-37.9742356128,3.46603879043));
#67172=CARTESIAN_POINT('Ctrl Pts',(7.51591788103,-36.2942356128,3.46603879043));
#67173=CARTESIAN_POINT('Ctrl Pts',(7.74013214217,-37.9742356128,3.53951961667));
#67174=CARTESIAN_POINT('Ctrl Pts',(7.74013214217,-36.2942356128,3.53951961667));
#67175=CARTESIAN_POINT('Ctrl Pts',(7.97806372235,-37.9742356128,3.56548871191));
#67176=CARTESIAN_POINT('Ctrl Pts',(7.97806372235,-36.2942356128,3.56548871191));
#67177=CARTESIAN_POINT('Ctrl Pts',(8.1397340384,-37.9742356128,3.5585372531));
#67178=CARTESIAN_POINT('Ctrl Pts',(8.1397340384,-36.2942356128,3.5585372531));
#67179=CARTESIAN_POINT('Ctrl Pts',(8.37641925249,-37.9742356128,3.50886242158));
#67180=CARTESIAN_POINT('Ctrl Pts',(8.37641925249,-36.2942356128,3.50886242158));
#67181=CARTESIAN_POINT('Ctrl Pts',(8.59150582736,-37.9742356128,3.41174862899));
#67182=CARTESIAN_POINT('Ctrl Pts',(8.59150582736,-36.2942356128,3.41174862899));
#67183=CARTESIAN_POINT('Ctrl Pts',(8.65978894936,-37.9742356128,3.37495922004));
#67184=CARTESIAN_POINT('Ctrl Pts',(8.65978894936,-36.2942356128,3.37495922004));
#67185=CARTESIAN_POINT('Ctrl Pts',(8.78922597568,-37.9742356128,3.29398598988));
#67186=CARTESIAN_POINT('Ctrl Pts',(8.78922597568,-36.2942356128,3.29398598988));
#67187=CARTESIAN_POINT('Ctrl Pts',(8.90717355699,-37.9742356128,3.19917508688));
#67188=CARTESIAN_POINT('Ctrl Pts',(8.90717355699,-36.2942356128,3.19917508688));
#67189=CARTESIAN_POINT('Ctrl Pts',(8.9630009386,-37.9742356128,3.14917335528));
#67190=CARTESIAN_POINT('Ctrl Pts',(8.9630009386,-36.2942356128,3.14917335528));
#67191=CARTESIAN_POINT('Ctrl Pts',(9.06741515882,-37.9742356128,3.04621714461));
#67192=CARTESIAN_POINT('Ctrl Pts',(9.06741515882,-36.2942356128,3.04621714461));
#67193=CARTESIAN_POINT('Ctrl Pts',(9.16069630403,-37.9742356128,2.93809779909));
#67194=CARTESIAN_POINT('Ctrl Pts',(9.16069630403,-36.2942356128,2.93809779909));
#67195=CARTESIAN_POINT('Ctrl Pts',(9.20593013024,-37.9742356128,2.88194354511));
#67196=CARTESIAN_POINT('Ctrl Pts',(9.20593013024,-36.2942356128,2.88194354511));
#67197=CARTESIAN_POINT('Ctrl Pts',(9.28925382834,-37.9742356128,2.77218463031));
#67198=CARTESIAN_POINT('Ctrl Pts',(9.28925382834,-36.2942356128,2.77218463031));
#67199=CARTESIAN_POINT('Ctrl Pts',(9.36584102959,-37.9742356128,2.66040353433));
#67200=CARTESIAN_POINT('Ctrl Pts',(9.36584102959,-36.2942356128,2.66040353433));
#67201=CARTESIAN_POINT('Ctrl Pts',(9.40258508843,-37.9742356128,2.60436998551));
#67202=CARTESIAN_POINT('Ctrl Pts',(9.40258508843,-36.2942356128,2.60436998551));
#67203=CARTESIAN_POINT('Ctrl Pts',(9.43799021757,-37.9742356128,2.54834207942));
#67204=CARTESIAN_POINT('Ctrl Pts',(9.43799021757,-36.2942356128,2.54834207942));
#67205=CARTESIAN_POINT('Ctrl Pts',(9.47221976654,-37.9742356128,2.49225909299));
#67206=CARTESIAN_POINT('Ctrl Pts',(9.47221976654,-36.2942356128,2.49225909299));
#67207=CARTESIAN_POINT('',(6.53914701908,-37.2742356128,2.5806950957));
#67208=CARTESIAN_POINT('',(9.47221976654,-37.2742356128,2.49225909299));
#67209=CARTESIAN_POINT('Ctrl Pts',(9.72829242121,-36.2742356128,2.64854983337));
#67210=CARTESIAN_POINT('Ctrl Pts',(9.64784482414,-36.2742356128,2.59944964919));
#67211=CARTESIAN_POINT('Ctrl Pts',(9.56739722707,-36.3112466293,2.55034946501));
#67212=CARTESIAN_POINT('Ctrl Pts',(9.50381146403,-36.3857400536,2.51154069022));
#67213=CARTESIAN_POINT('Ctrl Pts',(9.47221976654,-36.4799878332,2.49225909299));
#67214=CARTESIAN_POINT('Ctrl Pts',(9.47221976654,-36.5742356128,2.49225909299));
#67215=CARTESIAN_POINT('Ctrl Pts',(9.83429336167,-36.2742356128,2.47487388713));
#67216=CARTESIAN_POINT('Ctrl Pts',(9.75202069903,-36.2742356128,2.42876395934));
#67217=CARTESIAN_POINT('Ctrl Pts',(9.6697480364,-36.3112466293,2.38265403155));
#67218=CARTESIAN_POINT('Ctrl Pts',(9.60471974085,-36.3857400536,2.34620875598));
#67219=CARTESIAN_POINT('Ctrl Pts',(9.57241134287,-36.4799878332,2.32810142846));
#67220=CARTESIAN_POINT('Ctrl Pts',(9.57241134287,-36.5742356128,2.32810142846));
#67221=CARTESIAN_POINT('Ctrl Pts',(9.94000897933,-36.2742356128,2.28349205546));
#67222=CARTESIAN_POINT('Ctrl Pts',(9.85470074764,-36.2742356128,2.24265773253));
#67223=CARTESIAN_POINT('Ctrl Pts',(9.76939251595,-36.3112466293,2.20182340959));
#67224=CARTESIAN_POINT('Ctrl Pts',(9.70196490975,-36.3857400536,2.16954796843));
#67225=CARTESIAN_POINT('Ctrl Pts',(9.66846444414,-36.4799878332,2.15351236861));
#67226=CARTESIAN_POINT('Ctrl Pts',(9.66846444414,-36.5742356128,2.15351236861));
#67227=CARTESIAN_POINT('Ctrl Pts',(10.0256761637,-36.2742356128,2.08591224558));
#67228=CARTESIAN_POINT('Ctrl Pts',(9.93799442834,-36.2742356128,2.05066882697));
#67229=CARTESIAN_POINT('Ctrl Pts',(9.850312693,-36.3112466293,2.01542540835));
#67230=CARTESIAN_POINT('Ctrl Pts',(9.78100906698,-36.3857400536,1.98756902385));
#67231=CARTESIAN_POINT('Ctrl Pts',(9.74657653172,-36.4799878332,1.97372895991));
#67232=CARTESIAN_POINT('Ctrl Pts',(9.74657653172,-36.5742356128,1.97372895991));
#67233=CARTESIAN_POINT('Ctrl Pts',(10.1679814537,-36.2742356128,1.67805871095));
#67234=CARTESIAN_POINT('Ctrl Pts',(10.0767341523,-36.2742356128,1.65334546287));
#67235=CARTESIAN_POINT('Ctrl Pts',(9.98548685082,-36.3112466293,1.6286322148));
#67236=CARTESIAN_POINT('Ctrl Pts',(9.91336500486,-36.3857400536,1.60909886441));
#67237=CARTESIAN_POINT('Ctrl Pts',(9.87753227234,-36.4799878332,1.59939399912));
#67238=CARTESIAN_POINT('Ctrl Pts',(9.87753227234,-36.5742356128,1.59939399912));
#67239=CARTESIAN_POINT('Ctrl Pts',(10.2564553552,-36.2742356128,1.27104287483));
#67240=CARTESIAN_POINT('Ctrl Pts',(10.1638603619,-36.2742356128,1.25314895056));
#67241=CARTESIAN_POINT('Ctrl Pts',(10.0712653686,-36.3112466293,1.23525502628));
#67242=CARTESIAN_POINT('Ctrl Pts',(9.9980783059,-36.3857400536,1.22111167566));
#67243=CARTESIAN_POINT('Ctrl Pts',(9.96171633739,-36.4799878332,1.21408474484));
#67244=CARTESIAN_POINT('Ctrl Pts',(9.96171633739,-36.5742356128,1.21408474484));
#67245=CARTESIAN_POINT('Ctrl Pts',(10.2903320276,-36.2742356128,1.07432966245));
#67246=CARTESIAN_POINT('Ctrl Pts',(10.1974823607,-36.2742356128,1.05822737274));
#67247=CARTESIAN_POINT('Ctrl Pts',(10.1046326938,-36.3112466293,1.04212508303));
#67248=CARTESIAN_POINT('Ctrl Pts',(10.0312443404,-36.3857400536,1.02939781947));
#67249=CARTESIAN_POINT('Ctrl Pts',(9.99478235867,-36.4799878332,1.0230744824));
#67250=CARTESIAN_POINT('Ctrl Pts',(9.99478235867,-36.5742356128,1.0230744824));
#67251=CARTESIAN_POINT('Ctrl Pts',(10.3230522443,-36.2742356128,0.886587027226));
#67252=CARTESIAN_POINT('Ctrl Pts',(10.2301339285,-36.2742356128,0.870763630221));
#67253=CARTESIAN_POINT('Ctrl Pts',(10.1372156126,-36.3112466293,0.854940233215));
#67254=CARTESIAN_POINT('Ctrl Pts',(10.0637729945,-36.3857400536,0.842433434875));
#67255=CARTESIAN_POINT('Ctrl Pts',(10.0272840589,-36.4799878332,0.836219590227));
#67256=CARTESIAN_POINT('Ctrl Pts',(10.0272840589,-36.5742356128,0.836219590227));
#67257=CARTESIAN_POINT('Ctrl Pts',(10.3535102277,-36.2742356128,0.692259222377));
#67258=CARTESIAN_POINT('Ctrl Pts',(10.2603991896,-36.2742356128,0.677665438197));
#67259=CARTESIAN_POINT('Ctrl Pts',(10.1672881515,-36.3112466293,0.663071654016));
#67260=CARTESIAN_POINT('Ctrl Pts',(10.0936932074,-36.3857400536,0.651536730209));
#67261=CARTESIAN_POINT('Ctrl Pts',(10.0571285882,-36.4799878332,0.645805764563));
#67262=CARTESIAN_POINT('Ctrl Pts',(10.0571285882,-36.5742356128,0.645805764563));
#67263=CARTESIAN_POINT('',(10.0571285787,-36.5742356128,0.645805825719));
#67264=CARTESIAN_POINT('Origin',(10.3514145697721,-36.5721143181575,0.691930438083593));
#67265=CARTESIAN_POINT('Ctrl Pts',(9.47221976654,-36.5742356128,2.49225909299));
#67266=CARTESIAN_POINT('Ctrl Pts',(9.49100335387814,-36.5742356128,2.46148335373255));
#67267=CARTESIAN_POINT('Ctrl Pts',(9.50966311070764,-36.5742356128,2.43017846158239));
#67268=CARTESIAN_POINT('Ctrl Pts',(9.52801493081839,-36.5742356128,2.3984226649754));
#67269=CARTESIAN_POINT('Ctrl Pts',(9.54694614840981,-36.5742356128,2.36566428505843));
#67270=CARTESIAN_POINT('Ctrl Pts',(9.56554966655066,-36.5742356128,2.3324260390245));
#67271=CARTESIAN_POINT('Ctrl Pts',(9.58367847726007,-36.5742356128,2.29878225207235));
#67272=CARTESIAN_POINT('Ctrl Pts',(9.60236832147365,-36.5742356128,2.26409728861998));
#67273=CARTESIAN_POINT('Ctrl Pts',(9.62055378540715,-36.5742356128,2.22898119776554));
#67274=CARTESIAN_POINT('Ctrl Pts',(9.6381303125254,-36.5742356128,2.19350437114792));
#67275=CARTESIAN_POINT('Ctrl Pts',(9.65647984089947,-36.5742356128,2.15646730277473));
#67276=CARTESIAN_POINT('Ctrl Pts',(9.67416597091401,-36.5742356128,2.11903691913793));
#67277=CARTESIAN_POINT('Ctrl Pts',(9.69112721593196,-36.5742356128,2.08128335236617));
#67278=CARTESIAN_POINT('Ctrl Pts',(9.7086699786747,-36.5742356128,2.04223540135382));
#67279=CARTESIAN_POINT('Ctrl Pts',(9.72543795349894,-36.5742356128,2.00284146974368));
#67280=CARTESIAN_POINT('Ctrl Pts',(9.74141594767243,-36.5742356128,1.96317193046071));
#67281=CARTESIAN_POINT('Ctrl Pts',(9.7473379496166,-36.5742356128,1.94846901555118));
#67282=CARTESIAN_POINT('Ctrl Pts',(9.753149081602,-36.5742356128,1.93373509071006));
#67283=CARTESIAN_POINT('Ctrl Pts',(9.75884843233648,-36.5742356128,1.91897879964869));
#67284=CARTESIAN_POINT('Ctrl Pts',(9.78146372811979,-36.5742356128,1.86042513229877));
#67285=CARTESIAN_POINT('Ctrl Pts',(9.80232906854629,-36.5742356128,1.80148249645081));
#67286=CARTESIAN_POINT('Ctrl Pts',(9.82163170395721,-36.5742356128,1.74221229626608));
#67287=CARTESIAN_POINT('Ctrl Pts',(9.83683901853849,-36.5742356128,1.69551708805662));
#67288=CARTESIAN_POINT('Ctrl Pts',(9.8510796488562,-36.5742356128,1.64861775959349));
#67289=CARTESIAN_POINT('Ctrl Pts',(9.86444910264375,-36.5742356128,1.60155197403731));
#67290=CARTESIAN_POINT('Ctrl Pts',(9.86975108101274,-36.5742356128,1.58288690507463));
#67291=CARTESIAN_POINT('Ctrl Pts',(9.87491647744565,-36.5742356128,1.56419286401259));
#67292=CARTESIAN_POINT('Ctrl Pts',(9.87994527922462,-36.5742356128,1.54550492739863));
#67293=CARTESIAN_POINT('Ctrl Pts',(9.89160864620356,-36.5742356128,1.50216174697751));
#67294=CARTESIAN_POINT('Ctrl Pts',(9.90254290076312,-36.5742356128,1.45883011528504));
#67295=CARTESIAN_POINT('Ctrl Pts',(9.9128529548188,-36.5742356128,1.41562279736822));
#67296=CARTESIAN_POINT('Ctrl Pts',(9.92340473074946,-36.5742356128,1.37140247274521));
#67297=CARTESIAN_POINT('Ctrl Pts',(9.93330375339725,-36.5742356128,1.3273124158088));
#67298=CARTESIAN_POINT('Ctrl Pts',(9.94268006616696,-36.5742356128,1.28342079104392));
#67299=CARTESIAN_POINT('Ctrl Pts',(9.95209125516463,-36.5742356128,1.23936590654693));
#67300=CARTESIAN_POINT('Ctrl Pts',(9.96097693578902,-36.5742356128,1.19551086044026));
#67301=CARTESIAN_POINT('Ctrl Pts',(9.96946965611493,-36.5742356128,1.15187246591498));
#67302=CARTESIAN_POINT('Ctrl Pts',(9.97777858955746,-36.5742356128,1.10917842893572));
#67303=CARTESIAN_POINT('Ctrl Pts',(9.98571230740096,-36.5742356128,1.06669153948227));
#67304=CARTESIAN_POINT('Ctrl Pts',(9.99338108832957,-36.5742356128,1.0243803099396));
#67305=CARTESIAN_POINT('Ctrl Pts',(10.0007892024458,-36.5742356128,0.983507266392404));
#67306=CARTESIAN_POINT('Ctrl Pts',(10.0079507534458,-36.5742356128,0.942797893372109));
#67307=CARTESIAN_POINT('Ctrl Pts',(10.0149407365958,-36.5742356128,0.902182838501823));
#67308=CARTESIAN_POINT('Ctrl Pts',(10.021739685914,-36.5742356128,0.862677779090897));
#67309=CARTESIAN_POINT('Ctrl Pts',(10.0283768648537,-36.5742356128,0.823261802762564));
#67310=CARTESIAN_POINT('Ctrl Pts',(10.0348890100693,-36.5742356128,0.783834456310485));
#67311=CARTESIAN_POINT('Ctrl Pts',(10.0411561913072,-36.5742356128,0.745890227832604));
#67312=CARTESIAN_POINT('Ctrl Pts',(10.0473079284116,-36.5742356128,0.707935302701744));
#67313=CARTESIAN_POINT('Ctrl Pts',(10.0533402808925,-36.5742356128,0.669848094635844));
#67314=CARTESIAN_POINT('Ctrl Pts',(10.0546085605217,-36.5742356128,0.661840401074247));
#67315=CARTESIAN_POINT('Ctrl Pts',(10.0558714185436,-36.5742356128,0.653826748065928));
#67316=CARTESIAN_POINT('Ctrl Pts',(10.0571285786168,-36.5742356128,0.645805825705952));
#67317=CARTESIAN_POINT('Ctrl Pts',(10.0571274572,-37.9742356128,0.645813040595));
#67318=CARTESIAN_POINT('Ctrl Pts',(10.0571274557,-38.0684833925,0.645813050795));
#67319=CARTESIAN_POINT('Ctrl Pts',(10.0936920943,-38.1627311721,0.651543892692));
#67320=CARTESIAN_POINT('Ctrl Pts',(10.1672870793,-38.2372245964,0.663078554957));
#67321=CARTESIAN_POINT('Ctrl Pts',(10.2603981703,-38.2742356129,0.677672002041));
#67322=CARTESIAN_POINT('Ctrl Pts',(10.3535092619,-38.2742356128,0.692265445118));
#67323=CARTESIAN_POINT('Ctrl Pts',(10.0275848223,-37.9742356128,0.834300487763));
#67324=CARTESIAN_POINT('Ctrl Pts',(10.0275848525,-38.0684833923,0.834300292231));
#67325=CARTESIAN_POINT('Ctrl Pts',(10.064074095,-38.1627311719,0.840512185837));
#67326=CARTESIAN_POINT('Ctrl Pts',(10.137517286,-38.2372245961,0.853015346359));
#67327=CARTESIAN_POINT('Ctrl Pts',(10.2304363115,-38.2742356127,0.868834238919));
#67328=CARTESIAN_POINT('Ctrl Pts',(10.3233553253,-38.2742356128,0.884653208084));
#67329=CARTESIAN_POINT('Ctrl Pts',(9.99543705094,-37.9742356128,1.01939883766));
#67330=CARTESIAN_POINT('Ctrl Pts',(9.99543699511,-38.068483393,1.01939919322));
#67331=CARTESIAN_POINT('Ctrl Pts',(10.0319005469,-38.1627311731,1.0257074941));
#67332=CARTESIAN_POINT('Ctrl Pts',(10.1052921414,-38.2372245976,1.03840398068));
#67333=CARTESIAN_POINT('Ctrl Pts',(10.1981459373,-38.2742356137,1.05446714823));
#67334=CARTESIAN_POINT('Ctrl Pts',(10.2909997548,-38.2742356128,1.07053017617));
#67335=CARTESIAN_POINT('Ctrl Pts',(9.96252976109,-37.9742356128,1.2093437222));
#67336=CARTESIAN_POINT('Ctrl Pts',(9.96252977135,-38.0684833842,1.20934363522));
#67337=CARTESIAN_POINT('Ctrl Pts',(9.99889469961,-38.1627311555,1.21634966752));
#67338=CARTESIAN_POINT('Ctrl Pts',(10.0720874448,-38.2372245768,1.23045149981));
#67339=CARTESIAN_POINT('Ctrl Pts',(10.1646897356,-38.2742355998,1.24829276368));
#67340=CARTESIAN_POINT('Ctrl Pts',(10.2572920266,-38.2742356128,1.26613406435));
#67341=CARTESIAN_POINT('Ctrl Pts',(9.87888878289,-37.9742356128,1.59411409567));
#67342=CARTESIAN_POINT('Ctrl Pts',(9.87888877269,-38.0684834007,1.59411418207));
#67343=CARTESIAN_POINT('Ctrl Pts',(9.91473293696,-38.1627311885,1.60376825103));
#67344=CARTESIAN_POINT('Ctrl Pts',(9.98687806745,-38.2372246158,1.62319881203));
#67345=CARTESIAN_POINT('Ctrl Pts',(10.0781547196,-38.2742356258,1.64778214762));
#67346=CARTESIAN_POINT('Ctrl Pts',(10.1694313716,-38.2742356128,1.67236544666));
#67347=CARTESIAN_POINT('Ctrl Pts',(9.74871613381,-37.9742356128,1.96892463554));
#67348=CARTESIAN_POINT('Ctrl Pts',(9.74871614394,-38.0684833843,1.96892454973));
#67349=CARTESIAN_POINT('Ctrl Pts',(9.78317347076,-38.1627311557,1.9827075095));
#67350=CARTESIAN_POINT('Ctrl Pts',(9.85252671964,-38.237224577,2.01044951275));
#67351=CARTESIAN_POINT('Ctrl Pts',(9.94027134576,-38.2742356,2.04554808074));
#67352=CARTESIAN_POINT('Ctrl Pts',(10.028015972,-38.2742356128,2.08064668506));
#67353=CARTESIAN_POINT('Ctrl Pts',(9.67022825048,-37.9742356128,2.15028225121));
#67354=CARTESIAN_POINT('Ctrl Pts',(9.67022826459,-38.0684834011,2.15028222716));
#67355=CARTESIAN_POINT('Ctrl Pts',(9.70375002899,-38.1627311893,2.16628166859));
#67356=CARTESIAN_POINT('Ctrl Pts',(9.77122151877,-38.2372246167,2.19848267331));
#67357=CARTESIAN_POINT('Ctrl Pts',(9.85658482135,-38.2742356264,2.23922355047));
#67358=CARTESIAN_POINT('Ctrl Pts',(9.94194811633,-38.2742356128,2.27996443036));
#67359=CARTESIAN_POINT('Ctrl Pts',(9.57333706543,-37.9742356128,2.32658468963));
#67360=CARTESIAN_POINT('Ctrl Pts',(9.57333706543,-38.0684833924,2.32658468963));
#67361=CARTESIAN_POINT('Ctrl Pts',(9.60565231336,-38.1627311721,2.34468079402));
#67362=CARTESIAN_POINT('Ctrl Pts',(9.67069370749,-38.2372245963,2.38110460825));
#67363=CARTESIAN_POINT('Ctrl Pts',(9.75298323463,-38.2742356128,2.42718690466));
#67364=CARTESIAN_POINT('Ctrl Pts',(9.83527276,-38.2742356128,2.4732692039));
#67365=CARTESIAN_POINT('Ctrl Pts',(9.47221976654,-37.9742356128,2.49225909299));
#67366=CARTESIAN_POINT('Ctrl Pts',(9.47221976654,-38.0684833924,2.49225909299));
#67367=CARTESIAN_POINT('Ctrl Pts',(9.50381146403,-38.1627311721,2.51154069022));
#67368=CARTESIAN_POINT('Ctrl Pts',(9.56739722707,-38.2372245963,2.55034946501));
#67369=CARTESIAN_POINT('Ctrl Pts',(9.64784482414,-38.2742356128,2.59944964919));
#67370=CARTESIAN_POINT('Ctrl Pts',(9.72829242121,-38.2742356128,2.64854983337));
#67371=CARTESIAN_POINT('',(10.0571285787,-37.9742356128,0.645805825719));
#67372=CARTESIAN_POINT('Ctrl Pts',(9.47221976654,-37.9742356128,2.49225909299));
#67373=CARTESIAN_POINT('Ctrl Pts',(9.57333706543,-37.9742356128,2.32658468963));
#67374=CARTESIAN_POINT('Ctrl Pts',(9.67022825048,-37.9742356128,2.15028225121));
#67375=CARTESIAN_POINT('Ctrl Pts',(9.74871613381,-37.9742356128,1.96892463554));
#67376=CARTESIAN_POINT('Ctrl Pts',(9.87888878289,-37.9742356128,1.59411409567));
#67377=CARTESIAN_POINT('Ctrl Pts',(9.96252976109,-37.9742356128,1.2093437222));
#67378=CARTESIAN_POINT('Ctrl Pts',(9.99543705094,-37.9742356128,1.01939883766));
#67379=CARTESIAN_POINT('Ctrl Pts',(10.0275848223,-37.9742356128,0.834300487763));
#67380=CARTESIAN_POINT('Ctrl Pts',(10.0571285787,-37.9742356128,0.645805825719));
#67381=CARTESIAN_POINT('Origin',(10.3514120849986,-37.9763568300317,0.691946523729006));
#67382=CARTESIAN_POINT('Ctrl Pts',(9.47221976654,-37.9742356128,2.49225909299));
#67383=CARTESIAN_POINT('Ctrl Pts',(9.47221976654,-36.2942356128,2.49225909299));
#67384=CARTESIAN_POINT('Ctrl Pts',(9.53312961496,-37.9742356128,2.39246209578));
#67385=CARTESIAN_POINT('Ctrl Pts',(9.53312961496,-36.2942356128,2.39246209578));
#67386=CARTESIAN_POINT('Ctrl Pts',(9.59357915013,-37.9742356128,2.28708022821));
#67387=CARTESIAN_POINT('Ctrl Pts',(9.59357915013,-36.2942356128,2.28708022821));
#67388=CARTESIAN_POINT('Ctrl Pts',(9.64855478712,-37.9742356128,2.17984420246));
#67389=CARTESIAN_POINT('Ctrl Pts',(9.64855478712,-36.2942356128,2.17984420246));
#67390=CARTESIAN_POINT('Ctrl Pts',(9.7321123512,-37.9742356128,1.99616841131));
#67391=CARTESIAN_POINT('Ctrl Pts',(9.7321123512,-36.2942356128,1.99616841131));
#67392=CARTESIAN_POINT('Ctrl Pts',(9.80156823449,-37.9742356128,1.80635994999));
#67393=CARTESIAN_POINT('Ctrl Pts',(9.80156823449,-36.2942356128,1.80635994999));
#67394=CARTESIAN_POINT('Ctrl Pts',(9.82673775568,-37.9742356128,1.73070069002));
#67395=CARTESIAN_POINT('Ctrl Pts',(9.82673775568,-36.2942356128,1.73070069002));
#67396=CARTESIAN_POINT('Ctrl Pts',(9.90758702482,-37.9742356128,1.4638885651));
#67397=CARTESIAN_POINT('Ctrl Pts',(9.90758702482,-36.2942356128,1.4638885651));
#67398=CARTESIAN_POINT('Ctrl Pts',(9.9650475466,-37.9742356128,1.19577528243));
#67399=CARTESIAN_POINT('Ctrl Pts',(9.9650475466,-36.2942356128,1.19577528243));
#67400=CARTESIAN_POINT('Ctrl Pts',(9.9971133399,-37.9742356128,1.00951164249));
#67401=CARTESIAN_POINT('Ctrl Pts',(9.9971133399,-36.2942356128,1.00951164249));
#67402=CARTESIAN_POINT('Ctrl Pts',(10.0282717836,-37.9742356128,0.829917483849));
#67403=CARTESIAN_POINT('Ctrl Pts',(10.0282717836,-36.2942356128,0.829917483849));
#67404=CARTESIAN_POINT('Ctrl Pts',(10.0571285787,-37.9742356128,0.645805825719));
#67405=CARTESIAN_POINT('Ctrl Pts',(10.0571285787,-36.2942356128,0.645805825719));
#67406=CARTESIAN_POINT('',(10.0571285787,-37.2742356128,0.645805825719));
#67407=CARTESIAN_POINT('Ctrl Pts',(10.3535102065,-36.2742356128,0.692259352582));
#67408=CARTESIAN_POINT('Ctrl Pts',(10.2603991647,-36.2742356128,0.677665591985));
#67409=CARTESIAN_POINT('Ctrl Pts',(10.1672881228,-36.3112466293,0.663071831389));
#67410=CARTESIAN_POINT('Ctrl Pts',(10.0936931758,-36.3857400536,0.651536926221));
#67411=CARTESIAN_POINT('Ctrl Pts',(10.0571285552,-36.4799878332,0.645805969836));
#67412=CARTESIAN_POINT('Ctrl Pts',(10.0571285552,-36.5742356128,0.645805969836));
#67413=CARTESIAN_POINT('Ctrl Pts',(10.4654705253,-36.2742356128,-0.0220720388961));
#67414=CARTESIAN_POINT('Ctrl Pts',(10.3716407596,-36.2742356128,-0.0320801618586));
#67415=CARTESIAN_POINT('Ctrl Pts',(10.277810994,-36.3112466293,-0.042088284821));
#67416=CARTESIAN_POINT('Ctrl Pts',(10.2036479782,-36.3857400536,-0.0499987690501));
#67417=CARTESIAN_POINT('Ctrl Pts',(10.166801105,-36.4799878332,-0.0539288837071));
#67418=CARTESIAN_POINT('Ctrl Pts',(10.166801105,-36.5742356128,-0.0539288837071));
#67419=CARTESIAN_POINT('Ctrl Pts',(10.5332451587,-36.2742356128,-0.750280139625));
#67420=CARTESIAN_POINT('Ctrl Pts',(10.4390773883,-36.2742356128,-0.755397580353));
#67421=CARTESIAN_POINT('Ctrl Pts',(10.3449096179,-36.3112466293,-0.760515021082));
#67422=CARTESIAN_POINT('Ctrl Pts',(10.2704794173,-36.3857400536,-0.764559746152));
#67423=CARTESIAN_POINT('Ctrl Pts',(10.233499836,-36.4799878332,-0.766569459383));
#67424=CARTESIAN_POINT('Ctrl Pts',(10.233499836,-36.5742356128,-0.766569459383));
#67425=CARTESIAN_POINT('Ctrl Pts',(10.5621553524,-36.2742356128,-1.50355379103));
#67426=CARTESIAN_POINT('Ctrl Pts',(10.4669083702,-36.2742356128,-1.50048091028));
#67427=CARTESIAN_POINT('Ctrl Pts',(10.3716613881,-36.3112466293,-1.49740802953));
#67428=CARTESIAN_POINT('Ctrl Pts',(10.2963781981,-36.3857400536,-1.49497925029));
#67429=CARTESIAN_POINT('Ctrl Pts',(10.2589747918,-36.4799878332,-1.49377250781));
#67430=CARTESIAN_POINT('Ctrl Pts',(10.2589747918,-36.5742356128,-1.49377250781));
#67431=CARTESIAN_POINT('Ctrl Pts',(10.3656725489,-36.2742356128,-3.00545759266));
#67432=CARTESIAN_POINT('Ctrl Pts',(10.2732133718,-36.2742356128,-2.97798651849));
#67433=CARTESIAN_POINT('Ctrl Pts',(10.1807541948,-36.3112466293,-2.95051544432));
#67434=CARTESIAN_POINT('Ctrl Pts',(10.1076744778,-36.3857400536,-2.92880228958));
#67435=CARTESIAN_POINT('Ctrl Pts',(10.0713658476,-36.4799878332,-2.91801444773));
#67436=CARTESIAN_POINT('Ctrl Pts',(10.0713658476,-36.5742356128,-2.91801444773));
#67437=CARTESIAN_POINT('Ctrl Pts',(9.69612739523,-36.2742356128,-4.35866925271));
#67438=CARTESIAN_POINT('Ctrl Pts',(9.61531257083,-36.2742356128,-4.30797829153));
#67439=CARTESIAN_POINT('Ctrl Pts',(9.53449774643,-36.3112466293,-4.25728733035));
#67440=CARTESIAN_POINT('Ctrl Pts',(9.47062173065,-36.3857400536,-4.21722122832));
#67441=CARTESIAN_POINT('Ctrl Pts',(9.43888581966,-36.4799878332,-4.19731491187));
#67442=CARTESIAN_POINT('Ctrl Pts',(9.43888581966,-36.5742356128,-4.19731491187));
#67443=CARTESIAN_POINT('Ctrl Pts',(9.26520718698,-36.2742356128,-4.94839957983));
#67444=CARTESIAN_POINT('Ctrl Pts',(9.19061499526,-36.2742356128,-4.89024734488));
#67445=CARTESIAN_POINT('Ctrl Pts',(9.11602280354,-36.3112466293,-4.83209510993));
#67446=CARTESIAN_POINT('Ctrl Pts',(9.05706515172,-36.3857400536,-4.786131596));
#67447=CARTESIAN_POINT('Ctrl Pts',(9.02777286642,-36.4799878332,-4.76329526695));
#67448=CARTESIAN_POINT('Ctrl Pts',(9.02777286642,-36.5742356128,-4.76329526695));
#67449=CARTESIAN_POINT('Ctrl Pts',(8.51941071769,-36.2742356128,-5.80420810357));
#67450=CARTESIAN_POINT('Ctrl Pts',(8.45166351695,-36.2742356128,-5.73829733091));
#67451=CARTESIAN_POINT('Ctrl Pts',(8.38391631621,-36.3112466293,-5.67238655825));
#67452=CARTESIAN_POINT('Ctrl Pts',(8.33036894361,-36.3857400536,-5.62029069807));
#67453=CARTESIAN_POINT('Ctrl Pts',(8.30376468012,-36.4799878332,-5.59440759813));
#67454=CARTESIAN_POINT('Ctrl Pts',(8.30376468012,-36.5742356128,-5.59440759813));
#67455=CARTESIAN_POINT('Ctrl Pts',(7.6907047662,-36.2742356128,-6.55696420405));
#67456=CARTESIAN_POINT('Ctrl Pts',(7.62878309025,-36.2742356128,-6.48585146265));
#67457=CARTESIAN_POINT('Ctrl Pts',(7.5668614143,-36.3112466293,-6.41473872125));
#67458=CARTESIAN_POINT('Ctrl Pts',(7.51791853524,-36.3857400536,-6.3585312261));
#67459=CARTESIAN_POINT('Ctrl Pts',(7.49360194996,-36.4799878332,-6.33060531784));
#67460=CARTESIAN_POINT('Ctrl Pts',(7.49360194996,-36.5742356128,-6.33060531784));
#67461=CARTESIAN_POINT('Ctrl Pts',(7.38240736043,-36.2742356128,-6.81809919305));
#67462=CARTESIAN_POINT('Ctrl Pts',(7.32245884674,-36.2742356128,-6.74530491911));
#67463=CARTESIAN_POINT('Ctrl Pts',(7.26251033305,-36.3112466293,-6.67251064518));
#67464=CARTESIAN_POINT('Ctrl Pts',(7.21512704103,-36.3857400536,-6.61497406707));
#67465=CARTESIAN_POINT('Ctrl Pts',(7.19158531474,-36.4799878332,-6.58638782254));
#67466=CARTESIAN_POINT('Ctrl Pts',(7.19158531474,-36.5742356128,-6.58638782254));
#67467=CARTESIAN_POINT('Ctrl Pts',(6.75638043023,-36.2742356128,-7.31209369426));
#67468=CARTESIAN_POINT('Ctrl Pts',(6.70059555154,-36.2742356128,-7.23599823691));
#67469=CARTESIAN_POINT('Ctrl Pts',(6.64481067285,-36.3112466293,-7.15990277955));
#67470=CARTESIAN_POINT('Ctrl Pts',(6.60071831701,-36.3857400536,-7.09975694677));
#67471=CARTESIAN_POINT('Ctrl Pts',(6.57881164637,-36.4799878332,-7.06987433056));
#67472=CARTESIAN_POINT('Ctrl Pts',(6.57881164637,-36.5742356128,-7.06987433056));
#67473=CARTESIAN_POINT('Ctrl Pts',(6.0972721915,-36.2742356128,-7.7567769733));
#67474=CARTESIAN_POINT('Ctrl Pts',(6.04641537362,-36.2742356128,-7.67734201787));
#67475=CARTESIAN_POINT('Ctrl Pts',(5.99555855575,-36.3112466293,-7.59790706245));
#67476=CARTESIAN_POINT('Ctrl Pts',(5.95536133804,-36.3857400536,-7.53512169118));
#67477=CARTESIAN_POINT('Ctrl Pts',(5.9353899124,-36.4799878332,-7.5039276571));
#67478=CARTESIAN_POINT('Ctrl Pts',(5.9353899124,-36.5742356128,-7.5039276571));
#67479=CARTESIAN_POINT('Ctrl Pts',(5.75944878037,-36.2742356128,-7.96542127963));
#67480=CARTESIAN_POINT('Ctrl Pts',(5.71128828785,-36.2742356128,-7.88430555692));
#67481=CARTESIAN_POINT('Ctrl Pts',(5.66312779532,-36.3112466293,-7.80318983421));
#67482=CARTESIAN_POINT('Ctrl Pts',(5.62506175357,-36.3857400536,-7.73907598465));
#67483=CARTESIAN_POINT('Ctrl Pts',(5.60614917143,-36.4799878332,-7.70722191499));
#67484=CARTESIAN_POINT('Ctrl Pts',(5.60614917143,-36.5742356128,-7.70722191499));
#67485=CARTESIAN_POINT('Ctrl Pts',(4.87204527197,-36.2742356128,-8.46122850376));
#67486=CARTESIAN_POINT('Ctrl Pts',(4.83133074222,-36.2742356128,-8.37594391451));
#67487=CARTESIAN_POINT('Ctrl Pts',(4.79061621246,-36.3112466293,-8.29065932525));
#67488=CARTESIAN_POINT('Ctrl Pts',(4.75843545558,-36.3857400536,-8.22325040493));
#67489=CARTESIAN_POINT('Ctrl Pts',(4.74244689865,-36.4799878332,-8.18975922478));
#67490=CARTESIAN_POINT('Ctrl Pts',(4.74244689865,-36.5742356128,-8.18975922478));
#67491=CARTESIAN_POINT('Ctrl Pts',(3.93242931341,-36.2742356128,-8.85131842638));
#67492=CARTESIAN_POINT('Ctrl Pts',(3.90015750464,-36.2742356128,-8.76249452435));
#67493=CARTESIAN_POINT('Ctrl Pts',(3.86788569587,-36.3112466293,-8.67367062233));
#67494=CARTESIAN_POINT('Ctrl Pts',(3.8423780677,-36.3857400536,-8.60346422925));
#67495=CARTESIAN_POINT('Ctrl Pts',(3.82970495564,-36.4799878332,-8.56858316493));
#67496=CARTESIAN_POINT('Ctrl Pts',(3.82970495564,-36.5742356128,-8.56858316493));
#67497=CARTESIAN_POINT('Ctrl Pts',(3.34143335628,-36.2742356128,-9.04615827202));
#67498=CARTESIAN_POINT('Ctrl Pts',(3.31453785178,-36.2742356128,-8.95559501717));
#67499=CARTESIAN_POINT('Ctrl Pts',(3.28764234728,-36.3112466293,-8.86503176232));
#67500=CARTESIAN_POINT('Ctrl Pts',(3.26638413696,-36.3857400536,-8.79345058727));
#67501=CARTESIAN_POINT('Ctrl Pts',(3.25582230651,-36.4799878332,-8.75788647858));
#67502=CARTESIAN_POINT('Ctrl Pts',(3.25582230651,-36.5742356128,-8.75788647858));
#67503=CARTESIAN_POINT('Ctrl Pts',(2.73487315883,-36.2742356128,-9.19878073852));
#67504=CARTESIAN_POINT('Ctrl Pts',(2.71303985614,-36.2742356128,-9.10695943353));
#67505=CARTESIAN_POINT('Ctrl Pts',(2.69120655346,-36.3112466293,-9.01513812855));
#67506=CARTESIAN_POINT('Ctrl Pts',(2.67394952213,-36.3857400536,-8.94256258815));
#67507=CARTESIAN_POINT('Ctrl Pts',(2.66537559789,-36.4799878332,-8.90650444712));
#67508=CARTESIAN_POINT('Ctrl Pts',(2.66537559789,-36.5742356128,-8.90650444712));
#67509=CARTESIAN_POINT('Ctrl Pts',(2.11954062634,-36.2742356128,-9.3109005156));
#67510=CARTESIAN_POINT('Ctrl Pts',(2.10264593306,-36.2742356128,-9.21817935467));
#67511=CARTESIAN_POINT('Ctrl Pts',(2.08575123979,-36.3112466293,-9.12545819374));
#67512=CARTESIAN_POINT('Ctrl Pts',(2.07239767794,-36.3857400536,-9.05217140853));
#67513=CARTESIAN_POINT('Ctrl Pts',(2.0657631474,-36.4799878332,-9.01575989378));
#67514=CARTESIAN_POINT('Ctrl Pts',(2.0657631474,-36.5742356128,-9.01575989378));
#67515=CARTESIAN_POINT('',(2.06576130589928,-36.5742356128,-9.01576016580056));
#67516=CARTESIAN_POINT('Origin',(2.11916252104135,-36.5721144925218,-9.30881332409375));
#67517=CARTESIAN_POINT('Ctrl Pts',(10.05712857781,-36.5742356128,0.6458058255795));
#67518=CARTESIAN_POINT('Ctrl Pts',(10.0712039868866,-36.5742356128,0.556001631246168));
#67519=CARTESIAN_POINT('Ctrl Pts',(10.0844399589943,-36.5742356128,0.465906648280757));
#67520=CARTESIAN_POINT('Ctrl Pts',(10.096815487886,-36.5742356128,0.375515259159162));
#67521=CARTESIAN_POINT('Ctrl Pts',(10.1096992535075,-36.5742356128,0.281411687356653));
#67522=CARTESIAN_POINT('Ctrl Pts',(10.1216501586595,-36.5742356128,0.186986742025295));
#67523=CARTESIAN_POINT('Ctrl Pts',(10.1325881279532,-36.5742356128,0.0922479639907768));
#67524=CARTESIAN_POINT('Ctrl Pts',(10.1440788860828,-36.5742356128,-0.00727877215709816));
#67525=CARTESIAN_POINT('Ctrl Pts',(10.1544513400351,-36.5742356128,-0.107152044637042));
#67526=CARTESIAN_POINT('Ctrl Pts',(10.1635569310268,-36.5742356128,-0.207345680516345));
#67527=CARTESIAN_POINT('Ctrl Pts',(10.1737217027471,-36.5742356128,-0.319194042414421));
#67528=CARTESIAN_POINT('Ctrl Pts',(10.1823074911306,-36.5742356128,-0.431442176761078));
#67529=CARTESIAN_POINT('Ctrl Pts',(10.1890441337368,-36.5742356128,-0.544026357573112));
#67530=CARTESIAN_POINT('Ctrl Pts',(10.1952277414681,-36.5742356128,-0.647368103838791));
#67531=CARTESIAN_POINT('Ctrl Pts',(10.1998516599983,-36.5742356128,-0.750992719348358));
#67532=CARTESIAN_POINT('Ctrl Pts',(10.2026740714779,-36.5742356128,-0.854828666481071));
#67533=CARTESIAN_POINT('Ctrl Pts',(10.2048949078542,-36.5742356128,-0.936532787309225));
#67534=CARTESIAN_POINT('Ctrl Pts',(10.205999733603,-36.5742356128,-1.0183732282939));
#67535=CARTESIAN_POINT('Ctrl Pts',(10.205863143892,-36.5742356128,-1.10030594452211));
#67536=CARTESIAN_POINT('Ctrl Pts',(10.205657265768,-36.5742356128,-1.22380099984055));
#67537=CARTESIAN_POINT('Ctrl Pts',(10.2026292581837,-36.5742356128,-1.34750320034936));
#67538=CARTESIAN_POINT('Ctrl Pts',(10.1963512550468,-36.5742356128,-1.47120077077042));
#67539=CARTESIAN_POINT('Ctrl Pts',(10.1906356816034,-36.5742356128,-1.58381660308251));
#67540=CARTESIAN_POINT('Ctrl Pts',(10.1822248381961,-36.5742356128,-1.69642811272033));
#67541=CARTESIAN_POINT('Ctrl Pts',(10.1708230621608,-36.5742356128,-1.80884147526655));
#67542=CARTESIAN_POINT('Ctrl Pts',(10.1613744104428,-36.5742356128,-1.90199842799534));
#67543=CARTESIAN_POINT('Ctrl Pts',(10.1498715920879,-36.5742356128,-1.99501987510408));
#67544=CARTESIAN_POINT('Ctrl Pts',(10.1361734313148,-36.5742356128,-2.08777433560733));
#67545=CARTESIAN_POINT('Ctrl Pts',(10.1220621877022,-36.5742356128,-2.18332590709162));
#67546=CARTESIAN_POINT('Ctrl Pts',(10.1056205209072,-36.5742356128,-2.27859219750304));
#67547=CARTESIAN_POINT('Ctrl Pts',(10.0867343290288,-36.5742356128,-2.37341022121783));
#67548=CARTESIAN_POINT('Ctrl Pts',(10.0687364534174,-36.5742356128,-2.46376845794081));
#67549=CARTESIAN_POINT('Ctrl Pts',(10.0485182997365,-36.5742356128,-2.55371948411574));
#67550=CARTESIAN_POINT('Ctrl Pts',(10.0260250787213,-36.5742356128,-2.64310710082733));
#67551=CARTESIAN_POINT('Ctrl Pts',(10.0035318577062,-36.5742356128,-2.73249471753892));
#67552=CARTESIAN_POINT('Ctrl Pts',(9.97876296228436,-36.5742356128,-2.8213189237817));
#67553=CARTESIAN_POINT('Ctrl Pts',(9.95171582592092,-36.5742356128,-2.90940871914367));
#67554=CARTESIAN_POINT('Ctrl Pts',(9.92993931817063,-36.5742356128,-2.98033260866914));
#67555=CARTESIAN_POINT('Ctrl Pts',(9.90668774965613,-36.5742356128,-3.05077824731584));
#67556=CARTESIAN_POINT('Ctrl Pts',(9.88198479747963,-36.5742356128,-3.12067979234165));
#67557=CARTESIAN_POINT('Ctrl Pts',(9.86393211972182,-36.5742356128,-3.17176316319174));
#67558=CARTESIAN_POINT('Ctrl Pts',(9.84510545075928,-36.5742356128,-3.22255392981329));
#67559=CARTESIAN_POINT('Ctrl Pts',(9.82552203036848,-36.5742356128,-3.2730254094436));
#67560=CARTESIAN_POINT('Ctrl Pts',(9.78978496975496,-36.5742356128,-3.36512894860115));
#67561=CARTESIAN_POINT('Ctrl Pts',(9.75152280716754,-36.5742356128,-3.45617574805749));
#67562=CARTESIAN_POINT('Ctrl Pts',(9.7108497121987,-36.5742356128,-3.54609410175546));
#67563=CARTESIAN_POINT('Ctrl Pts',(9.6680049279269,-36.5742356128,-3.64081353407836));
#67564=CARTESIAN_POINT('Ctrl Pts',(9.62248519040241,-36.5742356128,-3.73428099545919));
#67565=CARTESIAN_POINT('Ctrl Pts',(9.57446091577429,-36.5742356128,-3.82645728198402));
#67566=CARTESIAN_POINT('Ctrl Pts',(9.52073520041125,-36.5742356128,-3.92957673503985));
#67567=CARTESIAN_POINT('Ctrl Pts',(9.4638752272999,-36.5742356128,-4.03108018727272));
#67568=CARTESIAN_POINT('Ctrl Pts',(9.4041607234943,-36.5742356128,-4.13096672981027));
#67569=CARTESIAN_POINT('Ctrl Pts',(9.3371221756021,-36.5742356128,-4.24310445748008));
#67570=CARTESIAN_POINT('Ctrl Pts',(9.2664869431227,-36.5742356128,-4.35320477522716));
#67571=CARTESIAN_POINT('Ctrl Pts',(9.19268999051769,-36.5742356128,-4.46132811226467));
#67572=CARTESIAN_POINT('Ctrl Pts',(9.13418828270235,-36.5742356128,-4.54704167695946));
#67573=CARTESIAN_POINT('Ctrl Pts',(9.07370082500083,-36.5742356128,-4.6315144538525));
#67574=CARTESIAN_POINT('Ctrl Pts',(9.01145050633955,-36.5742356128,-4.71479444137142));
#67575=CARTESIAN_POINT('Ctrl Pts',(8.9668168326544,-36.5742356128,-4.7745064535725));
#67576=CARTESIAN_POINT('Ctrl Pts',(8.92128231296221,-36.5742356128,-4.83359844391629));
#67577=CARTESIAN_POINT('Ctrl Pts',(8.87493145664548,-36.5742356128,-4.89208723168315));
#67578=CARTESIAN_POINT('Ctrl Pts',(8.79441053195804,-36.5742356128,-4.99369422773634));
#67579=CARTESIAN_POINT('Ctrl Pts',(8.71142780300561,-36.5742356128,-5.09348285810377));
#67580=CARTESIAN_POINT('Ctrl Pts',(8.6263979916159,-36.5742356128,-5.19154646335235));
#67581=CARTESIAN_POINT('Ctrl Pts',(8.54993426376687,-36.5742356128,-5.2797309330233));
#67582=CARTESIAN_POINT('Ctrl Pts',(8.47181575924716,-36.5742356128,-5.36652132950478));
#67583=CARTESIAN_POINT('Ctrl Pts',(8.39230621820942,-36.5742356128,-5.45196981180327));
#67584=CARTESIAN_POINT('Ctrl Pts',(8.31988794127727,-36.5742356128,-5.52979735015603));
#67585=CARTESIAN_POINT('Ctrl Pts',(8.24631587368035,-36.5742356128,-5.60651203021272));
#67586=CARTESIAN_POINT('Ctrl Pts',(8.17175117079795,-36.5742356128,-5.68213159754941));
#67587=CARTESIAN_POINT('Ctrl Pts',(8.13847955968082,-36.5742356128,-5.71587390107927));
#67588=CARTESIAN_POINT('Ctrl Pts',(8.10500975983473,-36.5742356128,-5.74939782796711));
#67589=CARTESIAN_POINT('Ctrl Pts',(8.07135317616891,-36.5742356128,-5.78270311230429));
#67590=CARTESIAN_POINT('Ctrl Pts',(7.98726197733494,-36.5742356128,-5.86591658742194));
#67591=CARTESIAN_POINT('Ctrl Pts',(7.90200681957206,-36.5742356128,-5.94776768512651));
#67592=CARTESIAN_POINT('Ctrl Pts',(7.81579962946374,-36.5742356128,-6.02827359551016));
#67593=CARTESIAN_POINT('Ctrl Pts',(7.7303665176099,-36.5742356128,-6.10805662101023));
#67594=CARTESIAN_POINT('Ctrl Pts',(7.64399912169157,-36.5742356128,-6.18651730248495));
#67595=CARTESIAN_POINT('Ctrl Pts',(7.5568608474066,-36.5742356128,-6.26364586505813));
#67596=CARTESIAN_POINT('Ctrl Pts',(7.47440298385371,-36.5742356128,-6.3366316631001));
#67597=CARTESIAN_POINT('Ctrl Pts',(7.39125503861802,-36.5742356128,-6.40842359127944));
#67598=CARTESIAN_POINT('Ctrl Pts',(7.30751084820958,-36.5742356128,-6.47900555413623));
#67599=CARTESIAN_POINT('Ctrl Pts',(7.23643171398355,-36.5742356128,-6.53891305085173));
#67600=CARTESIAN_POINT('Ctrl Pts',(7.16492249745893,-36.5742356128,-6.59794848505397));
#67601=CARTESIAN_POINT('Ctrl Pts',(7.09301131809069,-36.5742356128,-6.65610476540732));
#67602=CARTESIAN_POINT('Ctrl Pts',(7.007007109353,-36.5742356128,-6.72565841365588));
#67603=CARTESIAN_POINT('Ctrl Pts',(6.92043185960323,-36.5742356128,-6.79395229394742));
#67604=CARTESIAN_POINT('Ctrl Pts',(6.83324562170684,-36.5742356128,-6.86101265125115));
#67605=CARTESIAN_POINT('Ctrl Pts',(6.75618323322322,-36.5742356128,-6.92028612641282));
#67606=CARTESIAN_POINT('Ctrl Pts',(6.67864568902824,-36.5742356128,-6.97859342329466));
#67607=CARTESIAN_POINT('Ctrl Pts',(6.60056822518713,-36.5742356128,-7.03596299746881));
#67608=CARTESIAN_POINT('Ctrl Pts',(6.59031102317183,-36.5742356128,-7.04349976010027));
#67609=CARTESIAN_POINT('Ctrl Pts',(6.58004443577428,-36.5742356128,-7.05102037001382));
#67610=CARTESIAN_POINT('Ctrl Pts',(6.56976825429465,-36.5742356128,-7.05852492132114));
#67611=CARTESIAN_POINT('Ctrl Pts',(6.45579354456556,-36.5742356128,-7.14175905440781));
#67612=CARTESIAN_POINT('Ctrl Pts',(6.34063476844058,-36.5742356128,-7.22302068405111));
#67613=CARTESIAN_POINT('Ctrl Pts',(6.22422868607061,-36.5742356128,-7.30221428504094));
#67614=CARTESIAN_POINT('Ctrl Pts',(6.13966758898243,-36.5742356128,-7.359743046818));
#67615=CARTESIAN_POINT('Ctrl Pts',(6.05444938322057,-36.5742356128,-7.4161795741547));
#67616=CARTESIAN_POINT('Ctrl Pts',(5.96856201827064,-36.5742356128,-7.47147912409491));
#67617=CARTESIAN_POINT('Ctrl Pts',(5.88578700122719,-36.5742356128,-7.52477475368448));
#67618=CARTESIAN_POINT('Ctrl Pts',(5.80238971411301,-36.5742356128,-7.57701442935241));
#67619=CARTESIAN_POINT('Ctrl Pts',(5.71838751084297,-36.5742356128,-7.62814299484061));
#67620=CARTESIAN_POINT('Ctrl Pts',(5.57771899649851,-36.5742356128,-7.71376193181858));
#67621=CARTESIAN_POINT('Ctrl Pts',(5.43534417855391,-36.5742356128,-7.79626894567029));
#67622=CARTESIAN_POINT('Ctrl Pts',(5.29130214602209,-36.5742356128,-7.87546190675721));
#67623=CARTESIAN_POINT('Ctrl Pts',(5.17031042933696,-36.5742356128,-7.94198201996909));
#67624=CARTESIAN_POINT('Ctrl Pts',(5.04814359116801,-36.5742356128,-8.00616326407657));
#67625=CARTESIAN_POINT('Ctrl Pts',(4.92482519220396,-36.5742356128,-8.06791498370429));
#67626=CARTESIAN_POINT('Ctrl Pts',(4.77828868798353,-36.5742356128,-8.14129317544099));
#67627=CARTESIAN_POINT('Ctrl Pts',(4.63012513822672,-36.5742356128,-8.21124076793695));
#67628=CARTESIAN_POINT('Ctrl Pts',(4.48037267031824,-36.5742356128,-8.27765035657664));
#67629=CARTESIAN_POINT('Ctrl Pts',(4.32793376944481,-36.5742356128,-8.34525127722308));
#67630=CARTESIAN_POINT('Ctrl Pts',(4.17384721339769,-36.5742356128,-8.40918661356067));
#67631=CARTESIAN_POINT('Ctrl Pts',(4.01816442281152,-36.5742356128,-8.46939577180371));
#67632=CARTESIAN_POINT('Ctrl Pts',(3.86134597137964,-36.5742356128,-8.53004413840955));
#67633=CARTESIAN_POINT('Ctrl Pts',(3.70290662104831,-36.5742356128,-8.58691239389757));
#67634=CARTESIAN_POINT('Ctrl Pts',(3.54292923213171,-36.5742356128,-8.6399829259404));
#67635=CARTESIAN_POINT('Ctrl Pts',(3.3938750351181,-36.5742356128,-8.68942982335697));
#67636=CARTESIAN_POINT('Ctrl Pts',(3.24348513062699,-36.5742356128,-8.73558077178669));
#67637=CARTESIAN_POINT('Ctrl Pts',(3.09186488177117,-36.5742356128,-8.77844839317499));
#67638=CARTESIAN_POINT('Ctrl Pts',(2.94558178293629,-36.5742356128,-8.81980704113714));
#67639=CARTESIAN_POINT('Ctrl Pts',(2.79815290474148,-36.5742356128,-8.85810997089225));
#67640=CARTESIAN_POINT('Ctrl Pts',(2.64971757941682,-36.5742356128,-8.89338492401371));
#67641=CARTESIAN_POINT('Ctrl Pts',(2.50830664355868,-36.5742356128,-8.92699056419637));
#67642=CARTESIAN_POINT('Ctrl Pts',(2.3659820008866,-36.5742356128,-8.95784844431244));
#67643=CARTESIAN_POINT('Ctrl Pts',(2.22291081731417,-36.5742356128,-8.9859910514163));
#67644=CARTESIAN_POINT('Ctrl Pts',(2.17062417406695,-36.5742356128,-8.99627601880766));
#67645=CARTESIAN_POINT('Ctrl Pts',(2.11823830832693,-36.5742356128,-9.00619838927665));
#67646=CARTESIAN_POINT('Ctrl Pts',(2.0657631474,-36.5742356128,-9.01575989378));
#67647=CARTESIAN_POINT('Ctrl Pts',(2.06575925082,-37.9742356128,-9.01576051427));
#67648=CARTESIAN_POINT('Ctrl Pts',(2.06575925243,-38.0684833925,-9.01576051398));
#67649=CARTESIAN_POINT('Ctrl Pts',(2.07239387846,-38.1627311721,-9.0521720105));
#67650=CARTESIAN_POINT('Ctrl Pts',(2.08574763055,-38.2372245964,-9.12545875939));
#67651=CARTESIAN_POINT('Ctrl Pts',(2.10264256354,-38.2742356129,-9.21817987454));
#67652=CARTESIAN_POINT('Ctrl Pts',(2.11953749589,-38.2742356128,-9.31090098978));
#67653=CARTESIAN_POINT('Ctrl Pts',(2.55230448535,-37.9742356128,-8.92710614538));
#67654=CARTESIAN_POINT('Ctrl Pts',(2.55230457983,-38.0684833936,-8.92710612828));
#67655=CARTESIAN_POINT('Ctrl Pts',(2.56051293846,-38.1627311744,-8.96323086957));
#67656=CARTESIAN_POINT('Ctrl Pts',(2.57703406707,-38.2372245991,-9.0359404797));
#67657=CARTESIAN_POINT('Ctrl Pts',(2.59793626097,-38.2742356147,-9.12793141729));
#67658=CARTESIAN_POINT('Ctrl Pts',(2.61883841766,-38.2742356128,-9.21992236087));
#67659=CARTESIAN_POINT('Ctrl Pts',(3.03294472376,-37.9742356128,-8.81251059078));
#67660=CARTESIAN_POINT('Ctrl Pts',(3.03294455621,-38.0684833844,-8.81251062117));
#67661=CARTESIAN_POINT('Ctrl Pts',(3.04275300679,-38.1627311559,-8.84825697631));
#67662=CARTESIAN_POINT('Ctrl Pts',(3.06249506668,-38.2372245773,-8.92020492813));
#67663=CARTESIAN_POINT('Ctrl Pts',(3.08747246677,-38.2742356002,-9.01123220726));
#67664=CARTESIAN_POINT('Ctrl Pts',(3.11244993377,-38.2742356128,-9.1022594793));
#67665=CARTESIAN_POINT('Ctrl Pts',(3.50352252846,-37.9742356128,-8.67141257711));
#67666=CARTESIAN_POINT('Ctrl Pts',(3.50352256012,-38.0684833947,-8.67141257232));
#67667=CARTESIAN_POINT('Ctrl Pts',(3.51501818843,-38.1627311765,-8.70666289898));
#67668=CARTESIAN_POINT('Ctrl Pts',(3.5381558134,-38.2372246016,-8.7776125257));
#67669=CARTESIAN_POINT('Ctrl Pts',(3.56742911598,-38.2742356164,-8.86737675603));
#67670=CARTESIAN_POINT('Ctrl Pts',(3.59670240576,-38.2742356128,-8.95714098692));
#67671=CARTESIAN_POINT('Ctrl Pts',(4.58730752681,-37.9742356128,-8.27387012043));
#67672=CARTESIAN_POINT('Ctrl Pts',(4.58730748381,-38.0684833894,-8.27387012693));
#67673=CARTESIAN_POINT('Ctrl Pts',(4.60272266161,-38.162731166,-8.30767434705));
#67674=CARTESIAN_POINT('Ctrl Pts',(4.63374941501,-38.2372245892,-8.37571332545));
#67675=CARTESIAN_POINT('Ctrl Pts',(4.67300394407,-38.2742356081,-8.46179505077));
#67676=CARTESIAN_POINT('Ctrl Pts',(4.71225849052,-38.2742356128,-8.54787677533));
#67677=CARTESIAN_POINT('Ctrl Pts',(5.60638547087,-37.9742356128,-7.7308046141));
#67678=CARTESIAN_POINT('Ctrl Pts',(5.60638552928,-38.0684833966,-7.73080460527));
#67679=CARTESIAN_POINT('Ctrl Pts',(5.62536773699,-38.1627311803,-7.76270770883));
#67680=CARTESIAN_POINT('Ctrl Pts',(5.66357383517,-38.2372246061,-7.82692026332));
#67681=CARTESIAN_POINT('Ctrl Pts',(5.71191149292,-38.2742356193,-7.90816086883));
#67682=CARTESIAN_POINT('Ctrl Pts',(5.76024912705,-38.2742356128,-7.98940147537));
#67683=CARTESIAN_POINT('Ctrl Pts',(6.16964163718,-37.9742356128,-7.37017137729));
#67684=CARTESIAN_POINT('Ctrl Pts',(6.16964161946,-38.0684833871,-7.37017139274));
#67685=CARTESIAN_POINT('Ctrl Pts',(6.1904385669,-38.1627311614,-7.40086532392));
#67686=CARTESIAN_POINT('Ctrl Pts',(6.23229736424,-38.2372245838,-7.46264410061));
#67687=CARTESIAN_POINT('Ctrl Pts',(6.28525639509,-38.2742356045,-7.54080552318));
#67688=CARTESIAN_POINT('Ctrl Pts',(6.33821543401,-38.2742356128,-7.61896694326));
#67689=CARTESIAN_POINT('Ctrl Pts',(7.09776508839,-37.9742356128,-6.69246789154));
#67690=CARTESIAN_POINT('Ctrl Pts',(7.0977651012,-38.0684833963,-6.69246788036));
#67691=CARTESIAN_POINT('Ctrl Pts',(7.12103415187,-38.1627311798,-6.72135650201));
#67692=CARTESIAN_POINT('Ctrl Pts',(7.16786860412,-38.2372246054,-6.77950169941));
#67693=CARTESIAN_POINT('Ctrl Pts',(7.227122727,-38.2742356189,-6.85306599289));
#67694=CARTESIAN_POINT('Ctrl Pts',(7.28637684404,-38.2742356128,-6.92663028817));
#67695=CARTESIAN_POINT('Ctrl Pts',(7.97017602494,-37.9742356128,-5.90158416283));
#67696=CARTESIAN_POINT('Ctrl Pts',(7.97017601568,-38.0684833897,-5.9015841709));
#67697=CARTESIAN_POINT('Ctrl Pts',(7.99582514165,-38.1627311665,-5.92831961073));
#67698=CARTESIAN_POINT('Ctrl Pts',(8.04745008519,-38.2372245898,-5.98213099676));
#67699=CARTESIAN_POINT('Ctrl Pts',(8.11276506833,-38.2742356085,-6.05021221902));
#67700=CARTESIAN_POINT('Ctrl Pts',(8.17808005568,-38.2742356128,-6.11829343998));
#67701=CARTESIAN_POINT('Ctrl Pts',(8.32234138636,-37.9742356128,-5.5511354177));
#67702=CARTESIAN_POINT('Ctrl Pts',(8.322341377,-38.0684833626,-5.55113542953));
#67703=CARTESIAN_POINT('Ctrl Pts',(8.34905084971,-38.1627311123,-5.57683611657));
#67704=CARTESIAN_POINT('Ctrl Pts',(8.40280999154,-38.237224526,-5.62856481282));
#67705=CARTESIAN_POINT('Ctrl Pts',(8.47082513402,-38.2742355659,-5.69401105676));
#67706=CARTESIAN_POINT('Ctrl Pts',(8.5388402942,-38.2742356128,-5.759457308));
#67707=CARTESIAN_POINT('Ctrl Pts',(8.90931541395,-37.9742356128,-4.89736181467));
#67708=CARTESIAN_POINT('Ctrl Pts',(8.90931542119,-38.0684834156,-4.89736180551));
#67709=CARTESIAN_POINT('Ctrl Pts',(8.93825785475,-38.1627312183,-4.92066469564));
#67710=CARTESIAN_POINT('Ctrl Pts',(8.99651133904,-38.2372246508,-4.9675672848));
#67711=CARTESIAN_POINT('Ctrl Pts',(9.07021261859,-38.2742356492,-5.02690762115));
#67712=CARTESIAN_POINT('Ctrl Pts',(9.14391388443,-38.2742356128,-5.08624795184));
#67713=CARTESIAN_POINT('Ctrl Pts',(9.39879152195,-37.9742356128,-4.17295757679));
#67714=CARTESIAN_POINT('Ctrl Pts',(9.39879151634,-38.0684833745,-4.17295758389));
#67715=CARTESIAN_POINT('Ctrl Pts',(9.4304078184,-38.1627311363,-4.19237724524));
#67716=CARTESIAN_POINT('Ctrl Pts',(9.49404311057,-38.2372245542,-4.23146389807));
#67717=CARTESIAN_POINT('Ctrl Pts',(9.57455337996,-38.2742355847,-4.28091564899));
#67718=CARTESIAN_POINT('Ctrl Pts',(9.65506365997,-38.2742356128,-4.33036740429));
#67719=CARTESIAN_POINT('Ctrl Pts',(9.58754232636,-37.9742356128,-3.84345571161));
#67720=CARTESIAN_POINT('Ctrl Pts',(9.58754233174,-38.0684833927,-3.84345574942));
#67721=CARTESIAN_POINT('Ctrl Pts',(9.62040667626,-38.1627311725,-3.86074836295));
#67722=CARTESIAN_POINT('Ctrl Pts',(9.68655393532,-38.2372245968,-3.89555378883));
#67723=CARTESIAN_POINT('Ctrl Pts',(9.77024228936,-38.2742356132,-3.93958898382));
#67724=CARTESIAN_POINT('Ctrl Pts',(9.85393064124,-38.2742356128,-3.98362416376));
#67725=CARTESIAN_POINT('Ctrl Pts',(10.0701345637,-37.9742356128,-2.79823040916));
#67726=CARTESIAN_POINT('Ctrl Pts',(10.0701345528,-38.068483392,-2.79823033248));
#67727=CARTESIAN_POINT('Ctrl Pts',(10.1063202118,-38.1627311712,-2.80841507563));
#67728=CARTESIAN_POINT('Ctrl Pts',(10.1791524231,-38.2372245954,-2.82891437946));
#67729=CARTESIAN_POINT('Ctrl Pts',(10.2712984713,-38.2742356122,-2.85484978525));
#67730=CARTESIAN_POINT('Ctrl Pts',(10.363444524,-38.2742356128,-2.88078522158));
#67731=CARTESIAN_POINT('Ctrl Pts',(10.2631011081,-37.9742356128,-1.6439245767));
#67732=CARTESIAN_POINT('Ctrl Pts',(10.2631011302,-38.0684833933,-1.64392473221));
#67733=CARTESIAN_POINT('Ctrl Pts',(10.300671344,-38.1627311737,-1.6458337115));
#67734=CARTESIAN_POINT('Ctrl Pts',(10.3762902569,-38.2372245983,-1.64967578111));
#67735=CARTESIAN_POINT('Ctrl Pts',(10.471961972,-38.2742356142,-1.65453661061));
#67736=CARTESIAN_POINT('Ctrl Pts',(10.5676336782,-38.2742356128,-1.6593973782));
#67737=CARTESIAN_POINT('Ctrl Pts',(10.2421633997,-37.9742356128,-0.862745648495));
#67738=CARTESIAN_POINT('Ctrl Pts',(10.2421633045,-38.0684833989,-0.862745049409));
#67739=CARTESIAN_POINT('Ctrl Pts',(10.2791438065,-38.1627311851,-0.860933872727));
#67740=CARTESIAN_POINT('Ctrl Pts',(10.3535759371,-38.2372246117,-0.857289229083));
#67741=CARTESIAN_POINT('Ctrl Pts',(10.4477462212,-38.2742356231,-0.852678435106));
#67742=CARTESIAN_POINT('Ctrl Pts',(10.5419165386,-38.2742356128,-0.848067876398));
#67743=CARTESIAN_POINT('Ctrl Pts',(10.1742417982,-37.9742356128,-0.101398893364));
#67744=CARTESIAN_POINT('Ctrl Pts',(10.1742418626,-38.068483393,-0.101399296931));
#67745=CARTESIAN_POINT('Ctrl Pts',(10.2111107023,-38.1627311731,-0.0976092671479));
#67746=CARTESIAN_POINT('Ctrl Pts',(10.2853178786,-38.2372245976,-0.0899804119975));
#67747=CARTESIAN_POINT('Ctrl Pts',(10.3792034651,-38.2742356137,-0.0803282850477));
#67748=CARTESIAN_POINT('Ctrl Pts',(10.473089026,-38.2742356128,-0.0706759998837));
#67749=CARTESIAN_POINT('Ctrl Pts',(10.0571290687,-37.9742356128,0.645802815386));
#67750=CARTESIAN_POINT('Ctrl Pts',(10.057129068,-38.0684833924,0.645802819843));
#67751=CARTESIAN_POINT('Ctrl Pts',(10.0936936567,-38.162731172,0.651533980199));
#67752=CARTESIAN_POINT('Ctrl Pts',(10.1672885404,-38.2372245963,0.663069290459));
#67753=CARTESIAN_POINT('Ctrl Pts',(10.2603995024,-38.2742356128,0.677663560866));
#67754=CARTESIAN_POINT('Ctrl Pts',(10.3535104648,-38.2742356128,0.692257829523));
#67755=CARTESIAN_POINT('',(2.06575948168,-37.9742356128,-9.01576047707));
#67756=CARTESIAN_POINT('Ctrl Pts',(10.0571285787,-37.9742356128,0.645805825719));
#67757=CARTESIAN_POINT('Ctrl Pts',(10.1742417982,-37.9742356128081,-0.101398893364));
#67758=CARTESIAN_POINT('Ctrl Pts',(10.2421633997,-37.9742356128081,-0.862745648495));
#67759=CARTESIAN_POINT('Ctrl Pts',(10.2631011081,-37.9742356128081,-1.6439245767));
#67760=CARTESIAN_POINT('Ctrl Pts',(10.0701345637,-37.9742356128081,-2.79823040916));
#67761=CARTESIAN_POINT('Ctrl Pts',(9.58754232635999,-37.9742356128081,-3.84345571161));
#67762=CARTESIAN_POINT('Ctrl Pts',(9.39879152195,-37.9742356128081,-4.17295757679));
#67763=CARTESIAN_POINT('Ctrl Pts',(8.90931541394999,-37.9742356128081,-4.89736181467));
#67764=CARTESIAN_POINT('Ctrl Pts',(8.32234138636,-37.9742356128081,-5.5511354177));
#67765=CARTESIAN_POINT('Ctrl Pts',(7.97017602494,-37.9742356128081,-5.90158416283));
#67766=CARTESIAN_POINT('Ctrl Pts',(7.09776508839,-37.9742356128081,-6.69246789154));
#67767=CARTESIAN_POINT('Ctrl Pts',(6.16964163718,-37.9742356128081,-7.37017137729));
#67768=CARTESIAN_POINT('Ctrl Pts',(5.60638547087,-37.9742356128081,-7.7308046141));
#67769=CARTESIAN_POINT('Ctrl Pts',(4.58730752681,-37.9742356128081,-8.27387012042999));
#67770=CARTESIAN_POINT('Ctrl Pts',(3.50352252846,-37.9742356128081,-8.67141257711));
#67771=CARTESIAN_POINT('Ctrl Pts',(3.03294472376,-37.9742356128081,-8.81251059078));
#67772=CARTESIAN_POINT('Ctrl Pts',(2.55230448535,-37.9742356128081,-8.92710614538));
#67773=CARTESIAN_POINT('Ctrl Pts',(2.06575948168,-37.9742356128,-9.01576047707));
#67774=CARTESIAN_POINT('Origin',(2.11915744553878,-37.9763569133101,-9.30881401396193));
#67775=CARTESIAN_POINT('Ctrl Pts',(10.0571285787,-37.9742356128,0.645805825719));
#67776=CARTESIAN_POINT('Ctrl Pts',(10.0571285787,-36.2942356128,0.645805825719));
#67777=CARTESIAN_POINT('Ctrl Pts',(10.1043144812,-37.9742356128,0.34475109394));
#67778=CARTESIAN_POINT('Ctrl Pts',(10.1043144812,-36.2942356128,0.34475109394));
#67779=CARTESIAN_POINT('Ctrl Pts',(10.1436911823,-37.9742356128,0.0415756247073));
#67780=CARTESIAN_POINT('Ctrl Pts',(10.1436911823,-36.2942356128,0.0415756247073));
#67781=CARTESIAN_POINT('Ctrl Pts',(10.1751569467,-37.9742356128,-0.265526349591));
#67782=CARTESIAN_POINT('Ctrl Pts',(10.1751569467,-36.2942356128,-0.265526349591));
#67783=CARTESIAN_POINT('Ctrl Pts',(10.2113958308,-37.9742356128,-0.803196289146));
#67784=CARTESIAN_POINT('Ctrl Pts',(10.2113958308,-36.2942356128,-0.803196289146));
#67785=CARTESIAN_POINT('Ctrl Pts',(10.2066163947,-37.9742356128,-1.34483444271));
#67786=CARTESIAN_POINT('Ctrl Pts',(10.2066163947,-36.2942356128,-1.34483444271));
#67787=CARTESIAN_POINT('Ctrl Pts',(10.1959693719,-37.9742356128,-1.57549366978));
#67788=CARTESIAN_POINT('Ctrl Pts',(10.1959693719,-36.2942356128,-1.57549366978));
#67789=CARTESIAN_POINT('Ctrl Pts',(10.154755688,-37.9742356128,-2.03576280703));
#67790=CARTESIAN_POINT('Ctrl Pts',(10.154755688,-36.2942356128,-2.03576280703));
#67791=CARTESIAN_POINT('Ctrl Pts',(10.0694270848,-37.9742356128,-2.49123410794));
#67792=CARTESIAN_POINT('Ctrl Pts',(10.0694270848,-36.2942356128,-2.49123410794));
#67793=CARTESIAN_POINT('Ctrl Pts',(10.0147288892,-37.9742356128,-2.71679407199));
#67794=CARTESIAN_POINT('Ctrl Pts',(10.0147288892,-36.2942356128,-2.71679407199));
#67795=CARTESIAN_POINT('Ctrl Pts',(9.84427307953,-37.9742356128,-3.28258152506));
#67796=CARTESIAN_POINT('Ctrl Pts',(9.84427307953,-36.2942356128,-3.28258152506));
#67797=CARTESIAN_POINT('Ctrl Pts',(9.59767693443,-37.9742356128,-3.81973064429));
#67798=CARTESIAN_POINT('Ctrl Pts',(9.59767693443,-36.2942356128,-3.81973064429));
#67799=CARTESIAN_POINT('Ctrl Pts',(9.42196991538,-37.9742356128,-4.13127436125));
#67800=CARTESIAN_POINT('Ctrl Pts',(9.42196991538,-36.2942356128,-4.13127436125));
#67801=CARTESIAN_POINT('Ctrl Pts',(8.90941365275,-37.9742356128,-4.9063140586));
#67802=CARTESIAN_POINT('Ctrl Pts',(8.90941365275,-36.2942356128,-4.9063140586));
#67803=CARTESIAN_POINT('Ctrl Pts',(8.28331893235,-37.9742356128,-5.59939000154));
#67804=CARTESIAN_POINT('Ctrl Pts',(8.28331893235,-36.2942356128,-5.59939000154));
#67805=CARTESIAN_POINT('Ctrl Pts',(7.87223833419,-37.9742356128,-6.00004951346));
#67806=CARTESIAN_POINT('Ctrl Pts',(7.87223833419,-36.2942356128,-6.00004951346));
#67807=CARTESIAN_POINT('Ctrl Pts',(7.23577044162,-37.9742356128,-6.56118503753));
#67808=CARTESIAN_POINT('Ctrl Pts',(7.23577044162,-36.2942356128,-6.56118503753));
#67809=CARTESIAN_POINT('Ctrl Pts',(6.57301164306,-37.9742356128,-7.06148474596));
#67810=CARTESIAN_POINT('Ctrl Pts',(6.57301164306,-36.2942356128,-7.06148474596));
#67811=CARTESIAN_POINT('Ctrl Pts',(6.34892734606,-37.9742356128,-7.22182745263));
#67812=CARTESIAN_POINT('Ctrl Pts',(6.34892734606,-36.2942356128,-7.22182745263));
#67813=CARTESIAN_POINT('Ctrl Pts',(5.43475192661,-37.9742356128,-7.8381799988));
#67814=CARTESIAN_POINT('Ctrl Pts',(5.43475192661,-36.2942356128,-7.8381799988));
#67815=CARTESIAN_POINT('Ctrl Pts',(4.45617471097,-37.9742356128,-8.34265749719));
#67816=CARTESIAN_POINT('Ctrl Pts',(4.45617471097,-36.2942356128,-8.34265749719));
#67817=CARTESIAN_POINT('Ctrl Pts',(3.69023581936,-37.9742356128,-8.64282630111));
#67818=CARTESIAN_POINT('Ctrl Pts',(3.69023581936,-36.2942356128,-8.64282630111));
#67819=CARTESIAN_POINT('Ctrl Pts',(2.88684751199,-37.9742356128,-8.86614972783));
#67820=CARTESIAN_POINT('Ctrl Pts',(2.88684751199,-36.2942356128,-8.86614972783));
#67821=CARTESIAN_POINT('Ctrl Pts',(2.06575948168,-37.9742356128,-9.01576047707));
#67822=CARTESIAN_POINT('Ctrl Pts',(2.06575948168,-36.2942356128,-9.01576047707));
#67823=CARTESIAN_POINT('',(2.06575948168,-37.2742356128,-9.01576047707));
#67824=CARTESIAN_POINT('Ctrl Pts',(2.11953715431,-36.2742356128,-9.31090105701));
#67825=CARTESIAN_POINT('Ctrl Pts',(2.10264240018,-36.2742356128,-9.21817990924));
#67826=CARTESIAN_POINT('Ctrl Pts',(2.08574764605,-36.3112466293,-9.12545876147));
#67827=CARTESIAN_POINT('Ctrl Pts',(2.07239403611,-36.3857400536,-9.05217198666));
#67828=CARTESIAN_POINT('Ctrl Pts',(2.06575948168,-36.4799878332,-9.01576047707));
#67829=CARTESIAN_POINT('Ctrl Pts',(2.06575948168,-36.5742356128,-9.01576047707));
#67830=CARTESIAN_POINT('Ctrl Pts',(2.11615383992,-36.2742356128,-9.31151753196));
#67831=CARTESIAN_POINT('Ctrl Pts',(2.09914098406,-36.2742356128,-9.21881790355));
#67832=CARTESIAN_POINT('Ctrl Pts',(2.08212812821,-36.3112466293,-9.12611827514));
#67833=CARTESIAN_POINT('Ctrl Pts',(2.06868117069,-36.3857400536,-9.05284850922));
#67834=CARTESIAN_POINT('Ctrl Pts',(2.06200023781,-36.4799878332,-9.01644545027));
#67835=CARTESIAN_POINT('Ctrl Pts',(2.06200023781,-36.5742356128,-9.01644545027));
#67836=CARTESIAN_POINT('Ctrl Pts',(2.11277150501,-36.2742356128,-9.31213939407));
#67837=CARTESIAN_POINT('Ctrl Pts',(2.09564058293,-36.2742356128,-9.21946147283));
#67838=CARTESIAN_POINT('Ctrl Pts',(2.07850966085,-36.3112466293,-9.12678355158));
#67839=CARTESIAN_POINT('Ctrl Pts',(2.0649693838,-36.3857400536,-9.05353094301));
#67840=CARTESIAN_POINT('Ctrl Pts',(2.05824208644,-36.4799878332,-9.01713640844));
#67841=CARTESIAN_POINT('Ctrl Pts',(2.05824208644,-36.5742356128,-9.01713640844));
#67842=CARTESIAN_POINT('Ctrl Pts',(2.10940495264,-36.2742356128,-9.31276374494));
#67843=CARTESIAN_POINT('Ctrl Pts',(2.09215498197,-36.2742356128,-9.22010791777));
#67844=CARTESIAN_POINT('Ctrl Pts',(2.0749050113,-36.3112466293,-9.12745209061));
#67845=CARTESIAN_POINT('Ctrl Pts',(2.0612711021,-36.3857400536,-9.0542168542));
#67846=CARTESIAN_POINT('Ctrl Pts',(2.05449659064,-36.4799878332,-9.01783108696));
#67847=CARTESIAN_POINT('Ctrl Pts',(2.05449659064,-36.5742356128,-9.01783108696));
#67848=CARTESIAN_POINT('Ctrl Pts',(2.10261462813,-36.2742356128,-9.31403480844));
#67849=CARTESIAN_POINT('Ctrl Pts',(2.08513070049,-36.2742356128,-9.22142274904));
#67850=CARTESIAN_POINT('Ctrl Pts',(2.06764677286,-36.3112466293,-9.12881068964));
#67851=CARTESIAN_POINT('Ctrl Pts',(2.05382701648,-36.3857400536,-9.05561022924));
#67852=CARTESIAN_POINT('Ctrl Pts',(2.04696155797,-36.4799878332,-9.01924146757));
#67853=CARTESIAN_POINT('Ctrl Pts',(2.04696155797,-36.5742356128,-9.01924146757));
#67854=CARTESIAN_POINT('Ctrl Pts',(2.09588758326,-36.2742356128,-9.31531579883));
#67855=CARTESIAN_POINT('Ctrl Pts',(2.07816577093,-36.2742356128,-9.22274905448));
#67856=CARTESIAN_POINT('Ctrl Pts',(2.0604439586,-36.3112466293,-9.13018231014));
#67857=CARTESIAN_POINT('Ctrl Pts',(2.04643710585,-36.3857400536,-9.05701748476));
#67858=CARTESIAN_POINT('Ctrl Pts',(2.03947730261,-36.4799878332,-9.02066670026));
#67859=CARTESIAN_POINT('Ctrl Pts',(2.03947730261,-36.5742356128,-9.02066670026));
#67860=CARTESIAN_POINT('Ctrl Pts',(2.0924351229,-36.2742356128,-9.31597928737));
#67861=CARTESIAN_POINT('Ctrl Pts',(2.07460058288,-36.2742356128,-9.22343417963));
#67862=CARTESIAN_POINT('Ctrl Pts',(2.05676604286,-36.3112466293,-9.13088907189));
#67863=CARTESIAN_POINT('Ctrl Pts',(2.04266777108,-36.3857400536,-9.05774180306));
#67864=CARTESIAN_POINT('Ctrl Pts',(2.03566601887,-36.4799878332,-9.02139906025));
#67865=CARTESIAN_POINT('Ctrl Pts',(2.03566601887,-36.5742356128,-9.02139906025));
#67866=CARTESIAN_POINT('Ctrl Pts',(2.08916179444,-36.2742356128,-9.31661328133));
#67867=CARTESIAN_POINT('Ctrl Pts',(2.07120234504,-36.2742356128,-9.22409238783));
#67868=CARTESIAN_POINT('Ctrl Pts',(2.05324289565,-36.3112466293,-9.13157149433));
#67869=CARTESIAN_POINT('Ctrl Pts',(2.03904898765,-36.3857400536,-9.05844275779));
#67870=CARTESIAN_POINT('Ctrl Pts',(2.03199509152,-36.4799878332,-9.02211013053));
#67871=CARTESIAN_POINT('Ctrl Pts',(2.03199509152,-36.5742356128,-9.02211013053));
#67872=CARTESIAN_POINT('Ctrl Pts',(2.08574076981,-36.2742356128,-9.31728177401));
#67873=CARTESIAN_POINT('Ctrl Pts',(2.06766662735,-36.2742356128,-9.2247832911));
#67874=CARTESIAN_POINT('Ctrl Pts',(2.04959248489,-36.3112466293,-9.13228480819));
#67875=CARTESIAN_POINT('Ctrl Pts',(2.03530668666,-36.3857400536,-9.05917402763));
#67876=CARTESIAN_POINT('Ctrl Pts',(2.02820898752,-36.4799878332,-9.02284995833));
#67877=CARTESIAN_POINT('Ctrl Pts',(2.02820898752,-36.5742356128,-9.02284995833));
#67878=CARTESIAN_POINT('',(2.02820898731014,-36.5742356128,-9.02284995728736));
#67879=CARTESIAN_POINT('Origin',(2.08533354520416,-36.5721143212383,-9.31519993529546));
#67880=CARTESIAN_POINT('Origin',(2.46549092919547,-36.5742356128,-11.235936157823));
#67881=CARTESIAN_POINT('Ctrl Pts',(2.02820898783,-37.9742356128,-9.02284995993));
#67882=CARTESIAN_POINT('Ctrl Pts',(2.02820898784,-38.0684833925,-9.02284995993));
#67883=CARTESIAN_POINT('Ctrl Pts',(2.03530642737,-38.1627311721,-9.05917408011));
#67884=CARTESIAN_POINT('Ctrl Pts',(2.04959170303,-38.2372245964,-9.1322849631));
#67885=CARTESIAN_POINT('Ctrl Pts',(2.06766518434,-38.2742356129,-9.2247835756));
#67886=CARTESIAN_POINT('Ctrl Pts',(2.08573866565,-38.2742356128,-9.31728218809));
#67887=CARTESIAN_POINT('Ctrl Pts',(2.03579644621,-37.9742356128,-9.02136733755));
#67888=CARTESIAN_POINT('Ctrl Pts',(2.03579644598,-38.0684833923,-9.0213673376));
#67889=CARTESIAN_POINT('Ctrl Pts',(2.04280758136,-38.1627311717,-9.05770831662));
#67890=CARTESIAN_POINT('Ctrl Pts',(2.05691513298,-38.2372245959,-9.13085392264));
#67891=CARTESIAN_POINT('Ctrl Pts',(2.07476544794,-38.2742356126,-9.22339613411));
#67892=CARTESIAN_POINT('Ctrl Pts',(2.09261576301,-38.2742356128,-9.31593834568));
#67893=CARTESIAN_POINT('Ctrl Pts',(2.04241519624,-37.9742356128,-9.02009857614));
#67894=CARTESIAN_POINT('Ctrl Pts',(2.04241519751,-38.0684833934,-9.02009857588));
#67895=CARTESIAN_POINT('Ctrl Pts',(2.04927723066,-38.162731174,-9.05646842916));
#67896=CARTESIAN_POINT('Ctrl Pts',(2.06305130931,-38.2372245982,-9.12967864434));
#67897=CARTESIAN_POINT('Ctrl Pts',(2.0805332169,-38.2742356144,-9.22229220064));
#67898=CARTESIAN_POINT('Ctrl Pts',(2.09801512347,-38.2742356128,-9.31490575612));
#67899=CARTESIAN_POINT('Ctrl Pts',(2.05016977896,-37.9742356128,-9.01862581454));
#67900=CARTESIAN_POINT('Ctrl Pts',(2.05016990862,-38.0684833525,-9.01862579091));
#67901=CARTESIAN_POINT('Ctrl Pts',(2.05712054303,-38.1627310922,-9.05497938491));
#67902=CARTESIAN_POINT('Ctrl Pts',(2.07094926138,-38.2372244929,-9.12817894215));
#67903=CARTESIAN_POINT('Ctrl Pts',(2.08878910363,-38.2742355501,-9.22072706798));
#67904=CARTESIAN_POINT('Ctrl Pts',(2.1066289132,-38.2742356128,-9.31327521737));
#67905=CARTESIAN_POINT('Ctrl Pts',(2.05824162123,-37.9742356128,-9.01713030917));
#67906=CARTESIAN_POINT('Ctrl Pts',(2.05824162123,-38.0684833924,-9.01713030917));
#67907=CARTESIAN_POINT('Ctrl Pts',(2.06496151432,-38.1627311721,-9.05352627015));
#67908=CARTESIAN_POINT('Ctrl Pts',(2.07850921618,-38.2372245951,-9.12677767742));
#67909=CARTESIAN_POINT('Ctrl Pts',(2.0956401522,-38.2742356128,-9.2194557914));
#67910=CARTESIAN_POINT('Ctrl Pts',(2.11277109007,-38.2742356128,-9.31213390404));
#67911=CARTESIAN_POINT('Ctrl Pts',(2.06575948168,-37.9742356128,-9.01576047707));
#67912=CARTESIAN_POINT('Ctrl Pts',(2.06575948168,-38.0684833924,-9.01576047707));
#67913=CARTESIAN_POINT('Ctrl Pts',(2.07239403611,-38.1627311721,-9.05217198666));
#67914=CARTESIAN_POINT('Ctrl Pts',(2.08574764605,-38.2372245963,-9.12545876147));
#67915=CARTESIAN_POINT('Ctrl Pts',(2.10264240018,-38.2742356128,-9.21817990924));
#67916=CARTESIAN_POINT('Ctrl Pts',(2.11953715431,-38.2742356128,-9.31090105701));
#67917=CARTESIAN_POINT('',(2.02820898738765,-37.9742356128,-9.02284995768736));
#67918=CARTESIAN_POINT('Origin',(2.46549092919547,-37.9742356128,-11.235936157823));
#67919=CARTESIAN_POINT('Origin',(2.08533051776226,-37.9763569038635,-9.3152005273479));
#67920=CARTESIAN_POINT('Origin',(2.60353950659216,-37.9742356128,-11.9671837481076));
#67921=CARTESIAN_POINT('',(2.02820898725,-37.2742356128,-9.02284995699));
#67922=CARTESIAN_POINT('Ctrl Pts',(2.08574170933,-36.2742356128,-9.31728158894));
#67923=CARTESIAN_POINT('Ctrl Pts',(2.06766727163,-36.2742356128,-9.22478316375));
#67924=CARTESIAN_POINT('Ctrl Pts',(2.04959283393,-36.3112466293,-9.13228473855));
#67925=CARTESIAN_POINT('Ctrl Pts',(2.03530680234,-36.3857400536,-9.05917400362));
#67926=CARTESIAN_POINT('Ctrl Pts',(2.02820898725,-36.4799878332,-9.02284995699));
#67927=CARTESIAN_POINT('Ctrl Pts',(2.02820898725,-36.5742356128,-9.02284995699));
#67928=CARTESIAN_POINT('Ctrl Pts',(1.88030492013,-36.2742356128,-9.35742448262));
#67929=CARTESIAN_POINT('Ctrl Pts',(1.87601517131,-36.2742356128,-9.26223249264));
#67930=CARTESIAN_POINT('Ctrl Pts',(1.87172542249,-36.3112466293,-9.16704050267));
#67931=CARTESIAN_POINT('Ctrl Pts',(1.86833480716,-36.3857400536,-9.09180077438));
#67932=CARTESIAN_POINT('Ctrl Pts',(1.86665022554,-36.4799878332,-9.05441896768));
#67933=CARTESIAN_POINT('Ctrl Pts',(1.86665022554,-36.5742356128,-9.05441896768));
#67934=CARTESIAN_POINT('Ctrl Pts',(1.66720984854,-36.2742356128,-9.35934604645));
#67935=CARTESIAN_POINT('Ctrl Pts',(1.6772952561,-36.2742356128,-9.26400888229));
#67936=CARTESIAN_POINT('Ctrl Pts',(1.68738066366,-36.3112466293,-9.16867171814));
#67937=CARTESIAN_POINT('Ctrl Pts',(1.69535216508,-36.3857400536,-9.09331724462));
#67938=CARTESIAN_POINT('Ctrl Pts',(1.69931269786,-36.4799878332,-9.05587842773));
#67939=CARTESIAN_POINT('Ctrl Pts',(1.69931269786,-36.5742356128,-9.05587842773));
#67940=CARTESIAN_POINT('Ctrl Pts',(1.45620168108,-36.2742356128,-9.32056455888));
#67941=CARTESIAN_POINT('Ctrl Pts',(1.48053714367,-36.2742356128,-9.22791078978));
#67942=CARTESIAN_POINT('Ctrl Pts',(1.50487260626,-36.3112466293,-9.13525702068));
#67943=CARTESIAN_POINT('Ctrl Pts',(1.52410735302,-36.3857400536,-9.06202365388));
#67944=CARTESIAN_POINT('Ctrl Pts',(1.53366386436,-36.4799878332,-9.02563845191));
#67945=CARTESIAN_POINT('Ctrl Pts',(1.53366386436,-36.5742356128,-9.02563845191));
#67946=CARTESIAN_POINT('Ctrl Pts',(0.987909440581,-36.2742356128,-9.13885167431));
#67947=CARTESIAN_POINT('Ctrl Pts',(1.04376958449,-36.2742356128,-9.05831007195));
#67948=CARTESIAN_POINT('Ctrl Pts',(1.0996297284,-36.3112466293,-8.9777684696));
#67949=CARTESIAN_POINT('Ctrl Pts',(1.14378156832,-36.3857400536,-8.91410819697));
#67950=CARTESIAN_POINT('Ctrl Pts',(1.16571780109,-36.4799878332,-8.88247979152));
#67951=CARTESIAN_POINT('Ctrl Pts',(1.16571780109,-36.5742356128,-8.88247979152));
#67952=CARTESIAN_POINT('Ctrl Pts',(0.634280235908,-36.2742356128,-8.77195100368));
#67953=CARTESIAN_POINT('Ctrl Pts',(0.713875172545,-36.2742356128,-8.71622821272));
#67954=CARTESIAN_POINT('Ctrl Pts',(0.793470109182,-36.3112466293,-8.66050542177));
#67955=CARTESIAN_POINT('Ctrl Pts',(0.856381940119,-36.3857400536,-8.61646242435));
#67956=CARTESIAN_POINT('Ctrl Pts',(0.887638788125,-36.4799878332,-8.59457985122));
#67957=CARTESIAN_POINT('Ctrl Pts',(0.887638788125,-36.5742356128,-8.59457985122));
#67958=CARTESIAN_POINT('Ctrl Pts',(0.489143266094,-36.2742356128,-8.5130156531));
#67959=CARTESIAN_POINT('Ctrl Pts',(0.578565086551,-36.2742356128,-8.47420086576));
#67960=CARTESIAN_POINT('Ctrl Pts',(0.667986907007,-36.3112466293,-8.43538607842));
#67961=CARTESIAN_POINT('Ctrl Pts',(0.738665869701,-36.3857400536,-8.40470575012));
#67962=CARTESIAN_POINT('Ctrl Pts',(0.773781761013,-36.4799878332,-8.3894643477));
#67963=CARTESIAN_POINT('Ctrl Pts',(0.773781761013,-36.5742356128,-8.3894643477));
#67964=CARTESIAN_POINT('Ctrl Pts',(0.417258904585,-36.2742356128,-8.22711946983));
#67965=CARTESIAN_POINT('Ctrl Pts',(0.511506458023,-36.2742356128,-8.20836329279));
#67966=CARTESIAN_POINT('Ctrl Pts',(0.60575401146,-36.3112466293,-8.18960711575));
#67967=CARTESIAN_POINT('Ctrl Pts',(0.680247273964,-36.3857400536,-8.17478299056));
#67968=CARTESIAN_POINT('Ctrl Pts',(0.717258184663,-36.4799878332,-8.16741670403));
#67969=CARTESIAN_POINT('Ctrl Pts',(0.717258184663,-36.5742356128,-8.16741670403));
#67970=CARTESIAN_POINT('Ctrl Pts',(0.417255480809,-36.2742356128,-7.94319578605));
#67971=CARTESIAN_POINT('Ctrl Pts',(0.51150326041,-36.2742356128,-7.94319464953));
#67972=CARTESIAN_POINT('Ctrl Pts',(0.60575104001,-36.3112466293,-7.94319351302));
#67973=CARTESIAN_POINT('Ctrl Pts',(0.680244464285,-36.3857400536,-7.94319261472));
#67974=CARTESIAN_POINT('Ctrl Pts',(0.717255480787,-36.4799878332,-7.94319216841));
#67975=CARTESIAN_POINT('Ctrl Pts',(0.717255480787,-36.5742356128,-7.94319216841));
#67976=CARTESIAN_POINT('',(0.717273457110329,-36.5742356128,-7.94951682245649));
#67977=CARTESIAN_POINT('Ctrl Pts',(0.717273550273509,-36.5742356128,-7.94951682199161));
#67978=CARTESIAN_POINT('Ctrl Pts',(0.717273718212123,-36.5569116248149,
-7.94954627039414));
#67979=CARTESIAN_POINT('Ctrl Pts',(0.715768903123445,-36.5395872493805,
-7.94957487707452));
#67980=CARTESIAN_POINT('Ctrl Pts',(0.71277861671105,-36.5225244523691,-7.9496036226719));
#67981=CARTESIAN_POINT('Ctrl Pts',(0.709713242042008,-36.505033196172,-7.94963309009205));
#67982=CARTESIAN_POINT('Ctrl Pts',(0.705087023665518,-36.4878172698378,
-7.94966269785234));
#67983=CARTESIAN_POINT('Ctrl Pts',(0.698974456303144,-36.4711465076226,
-7.94969279420693));
#67984=CARTESIAN_POINT('Ctrl Pts',(0.692790765864684,-36.4542817719394,
-7.94972324074913));
#67985=CARTESIAN_POINT('Ctrl Pts',(0.685086262181111,-36.4379754276189,
-7.94975417739394));
#67986=CARTESIAN_POINT('Ctrl Pts',(0.67598818460903,-36.4224873686871,-7.94978537077702));
#67987=CARTESIAN_POINT('Ctrl Pts',(0.666789257765644,-36.4068276295904,
-7.94981690992874));
#67988=CARTESIAN_POINT('Ctrl Pts',(0.656166059019434,-36.3920049178971,
-7.94984869974283));
#67989=CARTESIAN_POINT('Ctrl Pts',(0.644295761307527,-36.3782607241328,
-7.94988006139291));
#67990=CARTESIAN_POINT('Ctrl Pts',(0.639508097400346,-36.3727172590896,
-7.94989271053144));
#67991=CARTESIAN_POINT('Ctrl Pts',(0.634518043105347,-36.3673488954339,
-7.94990528609214));
#67992=CARTESIAN_POINT('Ctrl Pts',(0.62933907671151,-36.3621699634842,-7.94991773054105));
#67993=CARTESIAN_POINT('Ctrl Pts',(0.616486900705681,-36.3493178729552,
-7.94994861281282));
#67994=CARTESIAN_POINT('Ctrl Pts',(0.602465787135931,-36.3376319498832,
-7.94997981454275));
#67995=CARTESIAN_POINT('Ctrl Pts',(0.587504932485788,-36.3273064223065,
-7.95001101814882));
#67996=CARTESIAN_POINT('Ctrl Pts',(0.572728201972024,-36.3171079716177,
-7.95004183773024));
#67997=CARTESIAN_POINT('Ctrl Pts',(0.557035218119696,-36.3082369941902,
-7.95007264840558));
#67998=CARTESIAN_POINT('Ctrl Pts',(0.540675695845687,-36.3008391875838,
-7.95010325026941));
#67999=CARTESIAN_POINT('Ctrl Pts',(0.524509427466709,-36.2935287707505,
-7.95013349063556));
#68000=CARTESIAN_POINT('Ctrl Pts',(0.507692734616536,-36.287657247099,-7.95016351980852));
#68001=CARTESIAN_POINT('Ctrl Pts',(0.490487885069218,-36.2833194732264,
-7.95019338220779));
#68002=CARTESIAN_POINT('Ctrl Pts',(0.473641257747844,-36.2790720161571,
-7.95022262284195));
#68003=CARTESIAN_POINT('Ctrl Pts',(0.456422901148918,-36.2762953079016,
-7.95025170029614));
#68004=CARTESIAN_POINT('Ctrl Pts',(0.439093000583099,-36.2750305592133,
-7.95028096141245));
#68005=CARTESIAN_POINT('Ctrl Pts',(0.431832792919537,-36.2745007040024,
-7.95029322009679));
#68006=CARTESIAN_POINT('Ctrl Pts',(0.424553142006894,-36.2742356128,-7.95030551501276));
#68007=CARTESIAN_POINT('Ctrl Pts',(0.417273658050834,-36.2742356128,-7.95031788947841));
#68008=CARTESIAN_POINT('Ctrl Pts',(2.02820898725,-36.5742356128,-9.02284995699));
#68009=CARTESIAN_POINT('Ctrl Pts',(1.64860914359,-36.5742356128,-9.09702477361));
#68010=CARTESIAN_POINT('Ctrl Pts',(1.23586688919,-36.5742356128,-9.00518418336));
#68011=CARTESIAN_POINT('Ctrl Pts',(0.890959353803,-36.5742356128,-8.72278991704));
#68012=CARTESIAN_POINT('Ctrl Pts',(0.719470863523,-36.5742356128,-8.33628951564));
#68013=CARTESIAN_POINT('Ctrl Pts',(0.717273426056,-36.5742356128,-7.9495168227));
#68014=CARTESIAN_POINT('Ctrl Pts',(0.7172606582,-37.9742356128,-7.94658833073));
#68015=CARTESIAN_POINT('Ctrl Pts',(0.7172606582,-38.0684833924,-7.94658833073));
#68016=CARTESIAN_POINT('Ctrl Pts',(0.680249812977,-38.1627311721,-7.94670092992));
#68017=CARTESIAN_POINT('Ctrl Pts',(0.605756733441,-38.2372245963,-7.94692756242));
#68018=CARTESIAN_POINT('Ctrl Pts',(0.511509389998,-38.2742356128,-7.9472142939));
#68019=CARTESIAN_POINT('Ctrl Pts',(0.417262046555,-38.2742356128,-7.94750102538));
#68020=CARTESIAN_POINT('Ctrl Pts',(0.717867533103,-37.9742356128,-8.14606537112));
#68021=CARTESIAN_POINT('Ctrl Pts',(0.717867533103,-38.0684833924,-8.14606537112));
#68022=CARTESIAN_POINT('Ctrl Pts',(0.680876846203,-38.1627311721,-8.15279980919));
#68023=CARTESIAN_POINT('Ctrl Pts',(0.60642431038,-38.237224596,-8.16635699061));
#68024=CARTESIAN_POINT('Ctrl Pts',(0.512228274053,-38.2742356128,-8.18350823638));
#68025=CARTESIAN_POINT('Ctrl Pts',(0.418032238021,-38.2742356128,-8.20065948222));
#68026=CARTESIAN_POINT('Ctrl Pts',(0.763363662931,-37.9742356128,-8.34442356823));
#68027=CARTESIAN_POINT('Ctrl Pts',(0.763363667813,-38.0684833919,-8.34442352344));
#68028=CARTESIAN_POINT('Ctrl Pts',(0.727897495111,-38.1627311709,-8.35801562032));
#68029=CARTESIAN_POINT('Ctrl Pts',(0.656513470554,-38.2372245955,-8.38536918483));
#68030=CARTESIAN_POINT('Ctrl Pts',(0.566199629112,-38.2742356119,-8.41997806019));
#68031=CARTESIAN_POINT('Ctrl Pts',(0.47588578497,-38.2742356128,-8.45458695312));
#68032=CARTESIAN_POINT('Ctrl Pts',(0.854204420009,-37.9742356128,-8.52995308217));
#68033=CARTESIAN_POINT('Ctrl Pts',(0.854204232522,-38.0684833927,-8.52995300167));
#68034=CARTESIAN_POINT('Ctrl Pts',(0.821817681684,-38.1627311726,-8.5496918088));
#68035=CARTESIAN_POINT('Ctrl Pts',(0.756629824743,-38.2372245969,-8.58942235372));
#68036=CARTESIAN_POINT('Ctrl Pts',(0.674156446967,-38.2742356133,-8.6396881941));
#68037=CARTESIAN_POINT('Ctrl Pts',(0.591683143127,-38.2742356128,-8.68995406613));
#68038=CARTESIAN_POINT('Ctrl Pts',(1.10581964187,-37.9742356128,-8.83717100477));
#68039=CARTESIAN_POINT('Ctrl Pts',(1.1058198191,-38.0684833922,-8.83717108086));
#68040=CARTESIAN_POINT('Ctrl Pts',(1.08188082307,-38.1627311716,-8.8672647092));
#68041=CARTESIAN_POINT('Ctrl Pts',(1.03370006531,-38.2372245958,-8.92783380533));
#68042=CARTESIAN_POINT('Ctrl Pts',(0.972741517449,-38.2742356124,-9.00446529129));
#68043=CARTESIAN_POINT('Ctrl Pts',(0.911782899689,-38.2742356128,-9.08109674732));
#68044=CARTESIAN_POINT('Ctrl Pts',(1.46215717903,-37.9742356128,-9.01047889206));
#68045=CARTESIAN_POINT('Ctrl Pts',(1.46215701149,-38.0684833927,-9.01047882012));
#68046=CARTESIAN_POINT('Ctrl Pts',(1.450187899,-38.1627311725,-9.04635771927));
#68047=CARTESIAN_POINT('Ctrl Pts',(1.4260952181,-38.2372245969,-9.11857386339));
#68048=CARTESIAN_POINT('Ctrl Pts',(1.3956146111,-38.2742356132,-9.2099399714));
#68049=CARTESIAN_POINT('Ctrl Pts',(1.36513407019,-38.2742356128,-9.30130610772));
#68050=CARTESIAN_POINT('Ctrl Pts',(1.65094597751,-37.9742356128,-9.0556796597));
#68051=CARTESIAN_POINT('Ctrl Pts',(1.65094609924,-38.0684833926,-9.05567973396));
#68052=CARTESIAN_POINT('Ctrl Pts',(1.64534839287,-38.1627311724,-9.09311495351));
#68053=CARTESIAN_POINT('Ctrl Pts',(1.63409038501,-38.2372245964,-9.16846036625));
#68054=CARTESIAN_POINT('Ctrl Pts',(1.61984316027,-38.2742356131,-9.26378674848));
#68055=CARTESIAN_POINT('Ctrl Pts',(1.60559588761,-38.2742356128,-9.35911310119));
#68056=CARTESIAN_POINT('Ctrl Pts',(1.8433625614,-37.9742356128,-9.05896943904));
#68057=CARTESIAN_POINT('Ctrl Pts',(1.8433625614,-38.0684833924,-9.05896943904));
#68058=CARTESIAN_POINT('Ctrl Pts',(1.84426881625,-38.1627311721,-9.09650333241));
#68059=CARTESIAN_POINT('Ctrl Pts',(1.84608697067,-38.2372245966,-9.17205032437));
#68060=CARTESIAN_POINT('Ctrl Pts',(1.84838974451,-38.2742356128,-9.26763057434));
#68061=CARTESIAN_POINT('Ctrl Pts',(1.85069251843,-38.2742356128,-9.36321082448));
#68062=CARTESIAN_POINT('Ctrl Pts',(2.02820898725,-37.9742356128,-9.02284995699));
#68063=CARTESIAN_POINT('Ctrl Pts',(2.02820898725,-38.0684833924,-9.02284995699));
#68064=CARTESIAN_POINT('Ctrl Pts',(2.03530680234,-38.1627311721,-9.05917400362));
#68065=CARTESIAN_POINT('Ctrl Pts',(2.04959283393,-38.2372245963,-9.13228473855));
#68066=CARTESIAN_POINT('Ctrl Pts',(2.06766727163,-38.2742356128,-9.22478316375));
#68067=CARTESIAN_POINT('Ctrl Pts',(2.08574170933,-38.2742356128,-9.31728158894));
#68068=CARTESIAN_POINT('',(0.717273429106671,-37.9742356128,-7.94951682267615));
#68069=CARTESIAN_POINT('Ctrl Pts',(2.02820898725,-37.9742356128,-9.02284995699));
#68070=CARTESIAN_POINT('Ctrl Pts',(1.64860914359,-37.9742356128,-9.09702477361));
#68071=CARTESIAN_POINT('Ctrl Pts',(1.23586688919,-37.9742356128,-9.00518418336));
#68072=CARTESIAN_POINT('Ctrl Pts',(0.890959353803,-37.9742356128,-8.72278991704));
#68073=CARTESIAN_POINT('Ctrl Pts',(0.719470863523,-37.9742356128,-8.33628951564));
#68074=CARTESIAN_POINT('Ctrl Pts',(0.717273426056,-37.9742356128,-7.9495168227));
#68075=CARTESIAN_POINT('Ctrl Pts',(0.417273442888033,-38.2742356128,-7.95031782080527));
#68076=CARTESIAN_POINT('Ctrl Pts',(0.434598525986889,-38.2742356128,-7.95028837214399));
#68077=CARTESIAN_POINT('Ctrl Pts',(0.451923974993303,-38.2727304797968,
-7.95025935917568));
#68078=CARTESIAN_POINT('Ctrl Pts',(0.468987789398651,-38.2697397345538,
-7.95023028762418));
#68079=CARTESIAN_POINT('Ctrl Pts',(0.486480149422269,-38.2666738788613,
-7.95020048596125));
#68080=CARTESIAN_POINT('Ctrl Pts',(0.503697118834521,-38.2620470205853,
-7.9501706245799));
#68081=CARTESIAN_POINT('Ctrl Pts',(0.520368827692176,-38.2559336669727,
-7.95014052771515));
#68082=CARTESIAN_POINT('Ctrl Pts',(0.53723453530731,-38.2497491759011,-7.95011008063109));
#68083=CARTESIAN_POINT('Ctrl Pts',(0.553541752130104,-38.2420437192392,
-7.95007939879925));
#68084=CARTESIAN_POINT('Ctrl Pts',(0.56903054794127,-38.2329445513992,-7.95004859832233));
#68085=CARTESIAN_POINT('Ctrl Pts',(0.584691001018681,-38.2237445404532,
-7.95001745649379));
#68086=CARTESIAN_POINT('Ctrl Pts',(0.599514291550423,-38.2131201228315,
-7.94998620332128));
#68087=CARTESIAN_POINT('Ctrl Pts',(0.613258891559137,-38.2012484884415,
-7.94995513871314));
#68088=CARTESIAN_POINT('Ctrl Pts',(0.618798575895286,-38.1964636924465,
-7.94994261829618));
#68089=CARTESIAN_POINT('Ctrl Pts',(0.624163379983104,-38.1914767749953,
-7.94993012967329));
#68090=CARTESIAN_POINT('Ctrl Pts',(0.629339001124755,-38.1863011865543,
-7.94991769434846));
#68091=CARTESIAN_POINT('Ctrl Pts',(0.642190475730227,-38.1734497931471,
-7.94988681645827));
#68092=CARTESIAN_POINT('Ctrl Pts',(0.653875928692519,-38.1594295641484,
-7.9498551419374));
#68093=CARTESIAN_POINT('Ctrl Pts',(0.664201133736344,-38.1444696525599,
-7.94982348173407));
#68094=CARTESIAN_POINT('Ctrl Pts',(0.674399245792677,-38.129693882579,-7.94979221123631));
#68095=CARTESIAN_POINT('Ctrl Pts',(0.683270033662761,-38.1140019200491,
-7.94976096659087));
#68096=CARTESIAN_POINT('Ctrl Pts',(0.690667797597331,-38.097643441461,-7.94973017875777));
#68097=CARTESIAN_POINT('Ctrl Pts',(0.697978168202641,-38.081478213417,-7.94969975463609));
#68098=CARTESIAN_POINT('Ctrl Pts',(0.703849790613318,-38.0646625836195,
-7.94966978700977));
#68099=CARTESIAN_POINT('Ctrl Pts',(0.708187802634565,-38.0474587849797,
-7.94964018198505));
#68100=CARTESIAN_POINT('Ctrl Pts',(0.712435492937246,-38.0306131865135,
-7.94961119336634));
#68101=CARTESIAN_POINT('Ctrl Pts',(0.715212568059503,-38.0133958472847,
-7.94958255936925));
#68102=CARTESIAN_POINT('Ctrl Pts',(0.71647780862749,-37.9960669200146,-7.94955357367437));
#68103=CARTESIAN_POINT('Ctrl Pts',(0.717008189396048,-37.9888027443343,
-7.94954142305612));
#68104=CARTESIAN_POINT('Ctrl Pts',(0.717273508649237,-37.9815190941805,
-7.94952920247982));
#68105=CARTESIAN_POINT('Ctrl Pts',(0.717273438258802,-37.9742356128,-7.94951682263062));
#68106=CARTESIAN_POINT('Ctrl Pts',(2.02820898725,-37.9742356128,-9.02284995699));
#68107=CARTESIAN_POINT('Ctrl Pts',(2.02820898725,-36.2942356128,-9.02284995699));
#68108=CARTESIAN_POINT('Ctrl Pts',(1.64860914359,-37.9742356128,-9.09702477361));
#68109=CARTESIAN_POINT('Ctrl Pts',(1.64860914359,-36.2942356128,-9.09702477361));
#68110=CARTESIAN_POINT('Ctrl Pts',(1.23586688919,-37.9742356128,-9.00518418336));
#68111=CARTESIAN_POINT('Ctrl Pts',(1.23586688919,-36.2942356128,-9.00518418336));
#68112=CARTESIAN_POINT('Ctrl Pts',(0.890959353803,-37.9742356128,-8.72278991704));
#68113=CARTESIAN_POINT('Ctrl Pts',(0.890959353803,-36.2942356128,-8.72278991704));
#68114=CARTESIAN_POINT('Ctrl Pts',(0.719470863523,-37.9742356128,-8.33628951564));
#68115=CARTESIAN_POINT('Ctrl Pts',(0.719470863523,-36.2942356128,-8.33628951564));
#68116=CARTESIAN_POINT('Ctrl Pts',(0.717273426056,-37.9742356128,-7.9495168227));
#68117=CARTESIAN_POINT('Ctrl Pts',(0.717273426056,-36.2942356128,-7.9495168227));
#68118=CARTESIAN_POINT('',(0.717273426056,-37.2742356128,-7.9495168227));
#68119=CARTESIAN_POINT('Origin',(0.417273426056,-36.5742356128,0.915007091638));
#68120=CARTESIAN_POINT('',(0.717273426056,-36.5742356128,-3.28965091665));
#68121=CARTESIAN_POINT('Origin',(0.41939471766068,-36.5721143212087,-3.28965091665326));
#68122=CARTESIAN_POINT('',(0.717273426056,-36.5742356128,-5.61958386968));
#68123=CARTESIAN_POINT('Origin',(0.417273426056,-37.9742356128,0.916320001688));
#68124=CARTESIAN_POINT('',(0.717273426056,-37.9742356128,-3.28965091665));
#68125=CARTESIAN_POINT('',(0.717273426056,-37.9742356128,-5.61958386968));
#68126=CARTESIAN_POINT('Origin',(0.419394717187198,-37.9763569039297,-3.28965091667348));
#68127=CARTESIAN_POINT('Origin',(0.717273426056,-38.2742356128,-7.9495168227));
#68128=CARTESIAN_POINT('',(0.717273426056,-37.2742356128,-3.28965091665));
#68129=CARTESIAN_POINT('Ctrl Pts',(0.417273426056,-36.2742356128,-3.28965091665));
#68130=CARTESIAN_POINT('Ctrl Pts',(0.511521205664,-36.2742356128,-3.28965091665));
#68131=CARTESIAN_POINT('Ctrl Pts',(0.605768985271,-36.3112466293,-3.28965091665));
#68132=CARTESIAN_POINT('Ctrl Pts',(0.680262409552,-36.3857400536,-3.28965091665));
#68133=CARTESIAN_POINT('Ctrl Pts',(0.717273426056,-36.4799878332,-3.28965091665));
#68134=CARTESIAN_POINT('Ctrl Pts',(0.717273426056,-36.5742356128,-3.28965091665));
#68135=CARTESIAN_POINT('Ctrl Pts',(0.417273426056,-36.2742356128,-3.16524611306));
#68136=CARTESIAN_POINT('Ctrl Pts',(0.511521205664,-36.2742356128,-3.18000729667));
#68137=CARTESIAN_POINT('Ctrl Pts',(0.605768985271,-36.3112466293,-3.19476848028));
#68138=CARTESIAN_POINT('Ctrl Pts',(0.680262408262,-36.3857400536,-3.20643571855));
#68139=CARTESIAN_POINT('Ctrl Pts',(0.717273426056,-36.4799878332,-3.21223241981));
#68140=CARTESIAN_POINT('Ctrl Pts',(0.717273426056,-36.5742356128,-3.21223241981));
#68141=CARTESIAN_POINT('Ctrl Pts',(0.441599544527,-36.2742356128,-3.04112730047));
#68142=CARTESIAN_POINT('Ctrl Pts',(0.532969569844,-36.2742356128,-3.07035582302));
#68143=CARTESIAN_POINT('Ctrl Pts',(0.624339595161,-36.3112466293,-3.09958434558));
#68144=CARTESIAN_POINT('Ctrl Pts',(0.696558447571,-36.3857400536,-3.12268655792));
#68145=CARTESIAN_POINT('Ctrl Pts',(0.73243936812,-36.4799878332,-3.13416457735));
#68146=CARTESIAN_POINT('Ctrl Pts',(0.73243936812,-36.5742356128,-3.13416457735));
#68147=CARTESIAN_POINT('Ctrl Pts',(0.48971071229,-36.2742356128,-2.92311263468));
#68148=CARTESIAN_POINT('Ctrl Pts',(0.575439222257,-36.2742356128,-2.96626059864));
#68149=CARTESIAN_POINT('Ctrl Pts',(0.661167732224,-36.3112466293,-3.0094085626));
#68150=CARTESIAN_POINT('Ctrl Pts',(0.728928155046,-36.3857400536,-3.04351258121));
#68151=CARTESIAN_POINT('Ctrl Pts',(0.762593034794,-36.4799878332,-3.06045686966));
#68152=CARTESIAN_POINT('Ctrl Pts',(0.762593034794,-36.5742356128,-3.06045686966));
#68153=CARTESIAN_POINT('Ctrl Pts',(0.613174121579,-36.2742356128,-2.73656462166));
#68154=CARTESIAN_POINT('Ctrl Pts',(0.68434190078,-36.2742356128,-2.8017427822));
#68155=CARTESIAN_POINT('Ctrl Pts',(0.755509679981,-36.3112466293,-2.86692094274));
#68156=CARTESIAN_POINT('Ctrl Pts',(0.811760201326,-36.3857400536,-2.91843783481));
#68157=CARTESIAN_POINT('Ctrl Pts',(0.839708198554,-36.4799878332,-2.94403315029));
#68158=CARTESIAN_POINT('Ctrl Pts',(0.839708198554,-36.5742356128,-2.94403315029));
#68159=CARTESIAN_POINT('Ctrl Pts',(0.790505416227,-36.2742356128,-2.60290926659));
#68160=CARTESIAN_POINT('Ctrl Pts',(0.84074776272,-36.2742356128,-2.68383943279));
#68161=CARTESIAN_POINT('Ctrl Pts',(0.890990109212,-36.3112466293,-2.76476959899));
#68162=CARTESIAN_POINT('Ctrl Pts',(0.930702009443,-36.3857400536,-2.82873672124));
#68163=CARTESIAN_POINT('Ctrl Pts',(0.950431772163,-36.4799878332,-2.86051798652));
#68164=CARTESIAN_POINT('Ctrl Pts',(0.950431772163,-36.5742356128,-2.86051798652));
#68165=CARTESIAN_POINT('Ctrl Pts',(0.875558654279,-36.2742356128,-2.55689129959));
#68166=CARTESIAN_POINT('Ctrl Pts',(0.915879301025,-36.2742356128,-2.64319398283));
#68167=CARTESIAN_POINT('Ctrl Pts',(0.956199947771,-36.3112466293,-2.72949666608));
#68168=CARTESIAN_POINT('Ctrl Pts',(0.988067915893,-36.3857400536,-2.79771056105));
#68169=CARTESIAN_POINT('Ctrl Pts',(1.00390325904,-36.4799878332,-2.83160127239));
#68170=CARTESIAN_POINT('Ctrl Pts',(1.00390325904,-36.5742356128,-2.83160127239));
#68171=CARTESIAN_POINT('Ctrl Pts',(0.966362779946,-36.2742356128,-2.52404170312));
#68172=CARTESIAN_POINT('Ctrl Pts',(0.995964836957,-36.2742356128,-2.61422938163));
#68173=CARTESIAN_POINT('Ctrl Pts',(1.02556689397,-36.3112466293,-2.70441706013));
#68174=CARTESIAN_POINT('Ctrl Pts',(1.04896532681,-36.3857400536,-2.77570120058));
#68175=CARTESIAN_POINT('Ctrl Pts',(1.06058905392,-36.4799878332,-2.81111799992));
#68176=CARTESIAN_POINT('Ctrl Pts',(1.06058905392,-36.5742356128,-2.81111799992));
#68177=CARTESIAN_POINT('Ctrl Pts',(1.05996676265,-36.2742356128,-2.50526930112));
#68178=CARTESIAN_POINT('Ctrl Pts',(1.07849866849,-36.2742356128,-2.59767714375));
#68179=CARTESIAN_POINT('Ctrl Pts',(1.09703057432,-36.3112466293,-2.69008498638));
#68180=CARTESIAN_POINT('Ctrl Pts',(1.11167818862,-36.3857400536,-2.76312412488));
#68181=CARTESIAN_POINT('Ctrl Pts',(1.11895565102,-36.4799878332,-2.79941259982));
#68182=CARTESIAN_POINT('Ctrl Pts',(1.11895565102,-36.5742356128,-2.79941259982));
#68183=CARTESIAN_POINT('',(1.11895565834,-36.5742356128,-2.79941259037));
#68184=CARTESIAN_POINT('Origin',(1.06038498235599,-36.5721142080809,-2.50734904525943));
#68185=CARTESIAN_POINT('Ctrl Pts',(0.717273426056,-36.5742356128,-3.28965091665));
#68186=CARTESIAN_POINT('Ctrl Pts',(0.717273426056,-36.5742356128,-3.15236381141));
#68187=CARTESIAN_POINT('Ctrl Pts',(0.764935707726,-36.5742356128,-3.0142516443));
#68188=CARTESIAN_POINT('Ctrl Pts',(0.858305199948,-36.5742356128,-2.90029762813));
#68189=CARTESIAN_POINT('Ctrl Pts',(0.984348856958,-36.5742356128,-2.82640811382));
#68190=CARTESIAN_POINT('Ctrl Pts',(1.11895565834,-36.5742356128,-2.79941259037));
#68191=CARTESIAN_POINT('Ctrl Pts',(1.11895565835,-37.9742356128,-2.79941259036));
#68192=CARTESIAN_POINT('Ctrl Pts',(1.11895565835,-38.0684833924,-2.79941259036));
#68193=CARTESIAN_POINT('Ctrl Pts',(1.11167797924,-38.1627311721,-2.7631241524));
#68194=CARTESIAN_POINT('Ctrl Pts',(1.09702992877,-38.2372245963,-2.69008508834));
#68195=CARTESIAN_POINT('Ctrl Pts',(1.0784974711,-38.2742356128,-2.59767733988));
#68196=CARTESIAN_POINT('Ctrl Pts',(1.05996501343,-38.2742356128,-2.50526959142));
#68197=CARTESIAN_POINT('Ctrl Pts',(1.05079714613,-37.9742356128,-2.81308183852));
#68198=CARTESIAN_POINT('Ctrl Pts',(1.05079714459,-38.0684833915,-2.81308183883));
#68199=CARTESIAN_POINT('Ctrl Pts',(1.03842294874,-38.1627311702,-2.77781551551));
#68200=CARTESIAN_POINT('Ctrl Pts',(1.01350086203,-38.2372245936,-2.7068369058));
#68201=CARTESIAN_POINT('Ctrl Pts',(0.981976632903,-38.2742356114,-2.61703465975));
#68202=CARTESIAN_POINT('Ctrl Pts',(0.950452403813,-38.2742356128,-2.52723241358));
#68203=CARTESIAN_POINT('Ctrl Pts',(0.984545966087,-37.9742356128,-2.83883463086));
#68204=CARTESIAN_POINT('Ctrl Pts',(0.98454601951,-38.0684833954,-2.83883463094));
#68205=CARTESIAN_POINT('Ctrl Pts',(0.96732248259,-38.1627311779,-2.80547148767));
#68206=CARTESIAN_POINT('Ctrl Pts',(0.932680120997,-38.2372246041,-2.73831545226));
#68207=CARTESIAN_POINT('Ctrl Pts',(0.888841036929,-38.2742356175,-2.65335283513));
#68208=CARTESIAN_POINT('Ctrl Pts',(0.845001933072,-38.2742356128,-2.56839021887));
#68209=CARTESIAN_POINT('Ctrl Pts',(0.923689095375,-37.9742356128,-2.8760099825));
#68210=CARTESIAN_POINT('Ctrl Pts',(0.923689119028,-38.0684833919,-2.87600994329));
#68211=CARTESIAN_POINT('Ctrl Pts',(0.901979860215,-38.162731171,-2.84536674598));
#68212=CARTESIAN_POINT('Ctrl Pts',(0.858278675606,-38.237224595,-2.78369427505));
#68213=CARTESIAN_POINT('Ctrl Pts',(0.802991263748,-38.274235612,-2.70566561619));
#68214=CARTESIAN_POINT('Ctrl Pts',(0.747703842309,-38.2742356128,-2.62763697264));
#68215=CARTESIAN_POINT('Ctrl Pts',(0.819317393776,-37.9742356128,-2.96776730531));
#68216=CARTESIAN_POINT('Ctrl Pts',(0.819317370869,-38.068483393,-2.96776734328));
#68217=CARTESIAN_POINT('Ctrl Pts',(0.789854337745,-38.1627311731,-2.94394296668));
#68218=CARTESIAN_POINT('Ctrl Pts',(0.7305590039,-38.2372245976,-2.89598667512));
#68219=CARTESIAN_POINT('Ctrl Pts',(0.655537093063,-38.2742356137,-2.83531489222));
#68220=CARTESIAN_POINT('Ctrl Pts',(0.580515191511,-38.2742356128,-2.77464309447));
#68221=CARTESIAN_POINT('Ctrl Pts',(0.751652775661,-37.9742356128,-3.08946794145));
#68222=CARTESIAN_POINT('Ctrl Pts',(0.751652797847,-38.0684833919,-3.08946790467));
#68223=CARTESIAN_POINT('Ctrl Pts',(0.717171967169,-38.162731171,-3.07467132905));
#68224=CARTESIAN_POINT('Ctrl Pts',(0.647765324546,-38.2372245951,-3.04489371052));
#68225=CARTESIAN_POINT('Ctrl Pts',(0.559955670297,-38.274235612,-3.00721795236));
#68226=CARTESIAN_POINT('Ctrl Pts',(0.472146007049,-38.2742356128,-2.96954220859));
#68227=CARTESIAN_POINT('Ctrl Pts',(0.728810629724,-37.9742356128,-3.15397751799));
#68228=CARTESIAN_POINT('Ctrl Pts',(0.728810613963,-38.0684833915,-3.15397750075));
#68229=CARTESIAN_POINT('Ctrl Pts',(0.692660998557,-38.1627311702,-3.14394628549));
#68230=CARTESIAN_POINT('Ctrl Pts',(0.619901810784,-38.2372245934,-3.12374493319));
#68231=CARTESIAN_POINT('Ctrl Pts',(0.527847978649,-38.2742356114,-3.09819124184));
#68232=CARTESIAN_POINT('Ctrl Pts',(0.435794152725,-38.2742356128,-3.07263755644));
#68233=CARTESIAN_POINT('Ctrl Pts',(0.717273426056,-37.9742356128,-3.22232941308));
#68234=CARTESIAN_POINT('Ctrl Pts',(0.717273426056,-38.0684833924,-3.22232941308));
#68235=CARTESIAN_POINT('Ctrl Pts',(0.680262508937,-38.1627311721,-3.21728624585));
#68236=CARTESIAN_POINT('Ctrl Pts',(0.605768984872,-38.2372245968,-3.20714313748));
#68237=CARTESIAN_POINT('Ctrl Pts',(0.511521205664,-38.2742356128,-3.19430712084));
#68238=CARTESIAN_POINT('Ctrl Pts',(0.417273426056,-38.2742356128,-3.1814711047));
#68239=CARTESIAN_POINT('Ctrl Pts',(0.717273426056,-37.9742356128,-3.28965091665));
#68240=CARTESIAN_POINT('Ctrl Pts',(0.717273426056,-38.0684833924,-3.28965091665));
#68241=CARTESIAN_POINT('Ctrl Pts',(0.680262409552,-38.1627311721,-3.28965091665));
#68242=CARTESIAN_POINT('Ctrl Pts',(0.605768985271,-38.2372245963,-3.28965091665));
#68243=CARTESIAN_POINT('Ctrl Pts',(0.511521205664,-38.2742356128,-3.28965091665));
#68244=CARTESIAN_POINT('Ctrl Pts',(0.417273426056,-38.2742356128,-3.28965091665));
#68245=CARTESIAN_POINT('',(1.11895565834,-37.9742356128,-2.79941259037));
#68246=CARTESIAN_POINT('Ctrl Pts',(0.717273426056,-37.9742356128,-3.28965091665));
#68247=CARTESIAN_POINT('Ctrl Pts',(0.717273426056,-37.9742356128,-3.22232941308));
#68248=CARTESIAN_POINT('Ctrl Pts',(0.728810629724,-37.9742356128,-3.15397751799));
#68249=CARTESIAN_POINT('Ctrl Pts',(0.751652775661,-37.9742356128,-3.08946794145));
#68250=CARTESIAN_POINT('Ctrl Pts',(0.819317393776,-37.9742356128,-2.96776730531));
#68251=CARTESIAN_POINT('Ctrl Pts',(0.923689095375,-37.9742356128,-2.8760099825));
#68252=CARTESIAN_POINT('Ctrl Pts',(0.984545966087,-37.9742356128,-2.83883463086));
#68253=CARTESIAN_POINT('Ctrl Pts',(1.05079714613,-37.9742356128,-2.81308183852));
#68254=CARTESIAN_POINT('Ctrl Pts',(1.11895565834,-37.9742356128,-2.79941259037));
#68255=CARTESIAN_POINT('Origin',(1.06038213453216,-37.9763569039054,-2.50734946784708));
#68256=CARTESIAN_POINT('Ctrl Pts',(0.717273426056,-37.9742356128,-3.28965091665));
#68257=CARTESIAN_POINT('Ctrl Pts',(0.717273426056,-36.2942356128,-3.28965091665));
#68258=CARTESIAN_POINT('Ctrl Pts',(0.717273426056,-37.9742356128,-3.15236381141));
#68259=CARTESIAN_POINT('Ctrl Pts',(0.717273426056,-36.2942356128,-3.15236381141));
#68260=CARTESIAN_POINT('Ctrl Pts',(0.764935707726,-37.9742356128,-3.0142516443));
#68261=CARTESIAN_POINT('Ctrl Pts',(0.764935707726,-36.2942356128,-3.0142516443));
#68262=CARTESIAN_POINT('Ctrl Pts',(0.858305199948,-37.9742356128,-2.90029762813));
#68263=CARTESIAN_POINT('Ctrl Pts',(0.858305199948,-36.2942356128,-2.90029762813));
#68264=CARTESIAN_POINT('Ctrl Pts',(0.984348856958,-37.9742356128,-2.82640811382));
#68265=CARTESIAN_POINT('Ctrl Pts',(0.984348856958,-36.2942356128,-2.82640811382));
#68266=CARTESIAN_POINT('Ctrl Pts',(1.11895565834,-37.9742356128,-2.79941259037));
#68267=CARTESIAN_POINT('Ctrl Pts',(1.11895565834,-36.2942356128,-2.79941259037));
#68268=CARTESIAN_POINT('',(1.11895565834,-37.2742356128,-2.79941259037));
#68269=CARTESIAN_POINT('Ctrl Pts',(1.05996499772,-36.2742356128,-2.50526959461));
#68270=CARTESIAN_POINT('Ctrl Pts',(1.07849746032,-36.2742356128,-2.59767734207));
#68271=CARTESIAN_POINT('Ctrl Pts',(1.09702992293,-36.3112466293,-2.69008508953));
#68272=CARTESIAN_POINT('Ctrl Pts',(1.1116779773,-36.3857400536,-2.7631241528));
#68273=CARTESIAN_POINT('Ctrl Pts',(1.11895565834,-36.4799878332,-2.79941259037));
#68274=CARTESIAN_POINT('Ctrl Pts',(1.11895565834,-36.5742356128,-2.79941259037));
#68275=CARTESIAN_POINT('Ctrl Pts',(1.18794302831,-36.2742356128,-2.47960347752));
#68276=CARTESIAN_POINT('Ctrl Pts',(1.20872454331,-36.2742356128,-2.57156017536));
#68277=CARTESIAN_POINT('Ctrl Pts',(1.22950605832,-36.3112466293,-2.66351687319));
#68278=CARTESIAN_POINT('Ctrl Pts',(1.24593176322,-36.3857400536,-2.73619942694));
#68279=CARTESIAN_POINT('Ctrl Pts',(1.25409264508,-36.4799878332,-2.77231073775));
#68280=CARTESIAN_POINT('Ctrl Pts',(1.25409264508,-36.5742356128,-2.77231073775));
#68281=CARTESIAN_POINT('Ctrl Pts',(1.31515278454,-36.2742356128,-2.45004137538));
#68282=CARTESIAN_POINT('Ctrl Pts',(1.33816133022,-36.2742356128,-2.54148026436));
#68283=CARTESIAN_POINT('Ctrl Pts',(1.36116987589,-36.3112466293,-2.63291915334));
#68284=CARTESIAN_POINT('Ctrl Pts',(1.37935582534,-36.3857400536,-2.70519243109));
#68285=CARTESIAN_POINT('Ctrl Pts',(1.3883912601,-36.4799878332,-2.74110039882));
#68286=CARTESIAN_POINT('Ctrl Pts',(1.3883912601,-36.5742356128,-2.74110039882));
#68287=CARTESIAN_POINT('Ctrl Pts',(1.44143362741,-36.2742356128,-2.41663560271));
#68288=CARTESIAN_POINT('Ctrl Pts',(1.46665027818,-36.2742356128,-2.50748956127));
#68289=CARTESIAN_POINT('Ctrl Pts',(1.49186692895,-36.3112466293,-2.59834351983));
#68290=CARTESIAN_POINT('Ctrl Pts',(1.51179810201,-36.3857400536,-2.67015449813));
#68291=CARTESIAN_POINT('Ctrl Pts',(1.52170071978,-36.4799878332,-2.70583273481));
#68292=CARTESIAN_POINT('Ctrl Pts',(1.52170071978,-36.5742356128,-2.70583273481));
#68293=CARTESIAN_POINT('Ctrl Pts',(1.69185428337,-36.2742356128,-2.34222503069));
#68294=CARTESIAN_POINT('Ctrl Pts',(1.72143190971,-36.2742356128,-2.43178423883));
#68295=CARTESIAN_POINT('Ctrl Pts',(1.75100953605,-36.3112466293,-2.52134344697));
#68296=CARTESIAN_POINT('Ctrl Pts',(1.77438774757,-36.3857400536,-2.59213099598));
#68297=CARTESIAN_POINT('Ctrl Pts',(1.7860027921,-36.4799878332,-2.62730084419));
#68298=CARTESIAN_POINT('Ctrl Pts',(1.7860027921,-36.5742356128,-2.62730084419));
#68299=CARTESIAN_POINT('Ctrl Pts',(1.93730960461,-36.2742356128,-2.25284977591));
#68300=CARTESIAN_POINT('Ctrl Pts',(1.97117385257,-36.2742356128,-2.34084746769));
#68301=CARTESIAN_POINT('Ctrl Pts',(2.00503810053,-36.3112466293,-2.42884515947));
#68302=CARTESIAN_POINT('Ctrl Pts',(2.0318043325,-36.3857400536,-2.49839854512));
#68303=CARTESIAN_POINT('Ctrl Pts',(2.04510285375,-36.4799878332,-2.53295512846));
#68304=CARTESIAN_POINT('Ctrl Pts',(2.04510285375,-36.5742356128,-2.53295512846));
#68305=CARTESIAN_POINT('Ctrl Pts',(2.05867417483,-36.2742356128,-2.20445670509));
#68306=CARTESIAN_POINT('Ctrl Pts',(2.09464235556,-36.2742356128,-2.29161676797));
#68307=CARTESIAN_POINT('Ctrl Pts',(2.13061053629,-36.3112466293,-2.37877683084));
#68308=CARTESIAN_POINT('Ctrl Pts',(2.15904002711,-36.3857400536,-2.44766800768));
#68309=CARTESIAN_POINT('Ctrl Pts',(2.17316444997,-36.4799878332,-2.48189580202));
#68310=CARTESIAN_POINT('Ctrl Pts',(2.17316444997,-36.5742356128,-2.48189580202));
#68311=CARTESIAN_POINT('Ctrl Pts',(2.17843292253,-36.2742356128,-2.15245040014));
#68312=CARTESIAN_POINT('Ctrl Pts',(2.21651835677,-36.2742356128,-2.23869055108));
#68313=CARTESIAN_POINT('Ctrl Pts',(2.25460379102,-36.3112466293,-2.32493070202));
#68314=CARTESIAN_POINT('Ctrl Pts',(2.28470634408,-36.3857400536,-2.39309497682));
#68315=CARTESIAN_POINT('Ctrl Pts',(2.29966262492,-36.4799878332,-2.42696132644));
#68316=CARTESIAN_POINT('Ctrl Pts',(2.29966262492,-36.5742356128,-2.42696132644));
#68317=CARTESIAN_POINT('Ctrl Pts',(2.29653436395,-36.2742356128,-2.09683572989));
#68318=CARTESIAN_POINT('Ctrl Pts',(2.3366869803,-36.2742356128,-2.18210243716));
#68319=CARTESIAN_POINT('Ctrl Pts',(2.37683959666,-36.3112466293,-2.26736914443));
#68320=CARTESIAN_POINT('Ctrl Pts',(2.40857621579,-36.3857400536,-2.33476393111));
#68321=CARTESIAN_POINT('Ctrl Pts',(2.42434411136,-36.4799878332,-2.36824808876));
#68322=CARTESIAN_POINT('Ctrl Pts',(2.42434411136,-36.5742356128,-2.36824808876));
#68323=CARTESIAN_POINT('',(2.42434411094,-36.5742356128,-2.36824808793));
#68324=CARTESIAN_POINT('Origin',(2.2974382266538,-36.5721143196987,-2.09875482216244));
#68325=CARTESIAN_POINT('Origin',(0.445434424817657,-36.5742356128,1.43140361501688));
#68326=CARTESIAN_POINT('Ctrl Pts',(2.42434410765,-37.9742356128,-2.36824808142));
#68327=CARTESIAN_POINT('Ctrl Pts',(2.42434410765,-38.0684833925,-2.36824808142));
#68328=CARTESIAN_POINT('Ctrl Pts',(2.4085761387,-38.1627311721,-2.33476395847));
#68329=CARTESIAN_POINT('Ctrl Pts',(2.37683937187,-38.2372245964,-2.26736924161));
#68330=CARTESIAN_POINT('Ctrl Pts',(2.33668656866,-38.2742356129,-2.1821026227));
#68331=CARTESIAN_POINT('Ctrl Pts',(2.29653376547,-38.2742356128,-2.0968360038));
#68332=CARTESIAN_POINT('Ctrl Pts',(2.29966569663,-37.9742356128,-2.42695994895));
#68333=CARTESIAN_POINT('Ctrl Pts',(2.29966569667,-38.0684833925,-2.42695994893));
#68334=CARTESIAN_POINT('Ctrl Pts',(2.28470854164,-38.1627311723,-2.39309400964));
#68335=CARTESIAN_POINT('Ctrl Pts',(2.25460410565,-38.2372245966,-2.32493061899));
#68336=CARTESIAN_POINT('Ctrl Pts',(2.21651634095,-38.274235613,-2.23869156224));
#68337=CARTESIAN_POINT('Ctrl Pts',(2.17842857626,-38.2742356128,-2.15245250557));
#68338=CARTESIAN_POINT('Ctrl Pts',(2.17315794346,-37.9742356128,-2.48189872286));
#68339=CARTESIAN_POINT('Ctrl Pts',(2.17315794944,-38.0684833917,-2.48189872001));
#68340=CARTESIAN_POINT('Ctrl Pts',(2.15903493648,-38.1627311705,-2.44767026483));
#68341=CARTESIAN_POINT('Ctrl Pts',(2.13060846119,-38.2372245946,-2.37877767407));
#68342=CARTESIAN_POINT('Ctrl Pts',(2.09464401419,-38.2742356116,-2.29161586047));
#68343=CARTESIAN_POINT('Ctrl Pts',(2.05867956465,-38.2742356128,-2.20445404757));
#68344=CARTESIAN_POINT('Ctrl Pts',(2.04510265844,-37.9742356128,-2.53295494804));
#68345=CARTESIAN_POINT('Ctrl Pts',(2.04510267392,-38.068483392,-2.53295494205));
#68346=CARTESIAN_POINT('Ctrl Pts',(2.03180403214,-38.1627311711,-2.49839847555));
#68347=CARTESIAN_POINT('Ctrl Pts',(2.005037321,-38.2372245952,-2.42884538862));
#68348=CARTESIAN_POINT('Ctrl Pts',(1.97117254874,-38.2742356121,-2.3408480546));
#68349=CARTESIAN_POINT('Ctrl Pts',(1.9373077703,-38.2742356128,-2.25285072267));
#68350=CARTESIAN_POINT('Ctrl Pts',(1.78600167486,-37.9742356128,-2.62730149119));
#68351=CARTESIAN_POINT('Ctrl Pts',(1.78600169488,-38.0684833923,-2.62730148454));
#68352=CARTESIAN_POINT('Ctrl Pts',(1.77438683171,-38.1627311718,-2.59213150305));
#68353=CARTESIAN_POINT('Ctrl Pts',(1.75100917837,-38.2372245961,-2.5213436377));
#68354=CARTESIAN_POINT('Ctrl Pts',(1.72143215468,-38.2742356127,-2.43178405694));
#68355=CARTESIAN_POINT('Ctrl Pts',(1.69185512312,-38.2742356128,-2.34222447873));
#68356=CARTESIAN_POINT('Ctrl Pts',(1.52170151672,-37.9742356128,-2.70583218602));
#68357=CARTESIAN_POINT('Ctrl Pts',(1.52170152953,-38.0684833931,-2.70583218274));
#68358=CARTESIAN_POINT('Ctrl Pts',(1.51179878238,-38.1627311734,-2.67015406859));
#68359=CARTESIAN_POINT('Ctrl Pts',(1.49186711563,-38.2372245979,-2.59834339715));
#68360=CARTESIAN_POINT('Ctrl Pts',(1.46664992394,-38.2742356139,-2.50748980544));
#68361=CARTESIAN_POINT('Ctrl Pts',(1.44143272734,-38.2742356128,-2.41663621543));
#68362=CARTESIAN_POINT('Ctrl Pts',(1.38839422114,-37.9742356128,-2.74109975505));
#68363=CARTESIAN_POINT('Ctrl Pts',(1.38839422089,-38.0684833925,-2.74109975528));
#68364=CARTESIAN_POINT('Ctrl Pts',(1.37935818392,-38.1627311721,-2.70519190943));
#68365=CARTESIAN_POINT('Ctrl Pts',(1.36117170821,-38.2372245964,-2.63291873908));
#68366=CARTESIAN_POINT('Ctrl Pts',(1.33816220899,-38.2742356129,-2.5414800437));
#68367=CARTESIAN_POINT('Ctrl Pts',(1.31515270986,-38.2742356128,-2.45004134821));
#68368=CARTESIAN_POINT('Ctrl Pts',(1.25409290934,-37.9742356128,-2.77231068475));
#68369=CARTESIAN_POINT('Ctrl Pts',(1.25409290934,-38.0684833924,-2.77231068475));
#68370=CARTESIAN_POINT('Ctrl Pts',(1.24593217744,-38.1627311721,-2.73619934385));
#68371=CARTESIAN_POINT('Ctrl Pts',(1.22950631738,-38.2372245963,-2.66351682126));
#68372=CARTESIAN_POINT('Ctrl Pts',(1.20872479797,-38.2742356128,-2.57156012428));
#68373=CARTESIAN_POINT('Ctrl Pts',(1.18794327857,-38.2742356128,-2.47960342733));
#68374=CARTESIAN_POINT('Ctrl Pts',(1.11895565834,-37.9742356128,-2.79941259037));
#68375=CARTESIAN_POINT('Ctrl Pts',(1.11895565834,-38.0684833924,-2.79941259037));
#68376=CARTESIAN_POINT('Ctrl Pts',(1.1116779773,-38.1627311721,-2.7631241528));
#68377=CARTESIAN_POINT('Ctrl Pts',(1.09702992293,-38.2372245963,-2.69008508953));
#68378=CARTESIAN_POINT('Ctrl Pts',(1.07849746032,-38.2742356128,-2.59767734207));
#68379=CARTESIAN_POINT('Ctrl Pts',(1.05996499772,-38.2742356128,-2.50526959461));
#68380=CARTESIAN_POINT('',(2.42434411094,-37.9742356128,-2.36824808793));
#68381=CARTESIAN_POINT('Origin',(0.445434424817657,-37.9742356128,1.43140361501688));
#68382=CARTESIAN_POINT('Origin',(2.29743725625794,-37.9763568917663,-2.09875525922514));
#68383=CARTESIAN_POINT('Ctrl Pts',(1.11895565834,-37.9742356128,-2.79941259037));
#68384=CARTESIAN_POINT('Ctrl Pts',(1.11895565834,-36.2942356128,-2.79941259037));
#68385=CARTESIAN_POINT('Ctrl Pts',(1.38919794322,-37.9742356128,-2.7452152403));
#68386=CARTESIAN_POINT('Ctrl Pts',(1.38919794322,-36.2942356128,-2.7452152403));
#68387=CARTESIAN_POINT('Ctrl Pts',(1.65613520407,-37.9742356128,-2.67457823688));
#68388=CARTESIAN_POINT('Ctrl Pts',(1.65613520407,-36.2942356128,-2.67457823688));
#68389=CARTESIAN_POINT('Ctrl Pts',(1.91849016776,-37.9742356128,-2.58792345825));
#68390=CARTESIAN_POINT('Ctrl Pts',(1.91849016776,-36.2942356128,-2.58792345825));
#68391=CARTESIAN_POINT('Ctrl Pts',(2.1749855611,-37.9742356128,-2.48567278256));
#68392=CARTESIAN_POINT('Ctrl Pts',(2.1749855611,-36.2942356128,-2.48567278256));
#68393=CARTESIAN_POINT('Ctrl Pts',(2.42434411094,-37.9742356128,-2.36824808793));
#68394=CARTESIAN_POINT('Ctrl Pts',(2.42434411094,-36.2942356128,-2.36824808793));
#68395=CARTESIAN_POINT('',(2.42434411094,-37.2742356128,-2.36824808793));
#68396=CARTESIAN_POINT('Ctrl Pts',(2.29653416635,-36.2742356128,-2.09683582206));
#68397=CARTESIAN_POINT('Ctrl Pts',(2.33668684465,-36.2742356128,-2.18210250012));
#68398=CARTESIAN_POINT('Ctrl Pts',(2.37683952295,-36.3112466293,-2.26736917817));
#68399=CARTESIAN_POINT('Ctrl Pts',(2.40857619105,-36.3857400536,-2.33476394176));
#68400=CARTESIAN_POINT('Ctrl Pts',(2.42434411094,-36.4799878332,-2.36824808793));
#68401=CARTESIAN_POINT('Ctrl Pts',(2.42434411094,-36.5742356128,-2.36824808793));
#68402=CARTESIAN_POINT('Ctrl Pts',(2.95453073399,-36.2742356128,-1.78698061128));
#68403=CARTESIAN_POINT('Ctrl Pts',(3.00083493027,-36.2742356128,-1.86935049626));
#68404=CARTESIAN_POINT('Ctrl Pts',(3.04713912654,-36.3112466293,-1.95172038124));
#68405=CARTESIAN_POINT('Ctrl Pts',(3.08373795336,-36.3857400536,-2.01682552));
#68406=CARTESIAN_POINT('Ctrl Pts',(3.10192156845,-36.4799878332,-2.04917209841));
#68407=CARTESIAN_POINT('Ctrl Pts',(3.10192156845,-36.5742356128,-2.04917209841));
#68408=CARTESIAN_POINT('Ctrl Pts',(3.5952546957,-36.2742356128,-1.41294917537));
#68409=CARTESIAN_POINT('Ctrl Pts',(3.64373574115,-36.2742356128,-1.49338900213));
#68410=CARTESIAN_POINT('Ctrl Pts',(3.6922167866,-36.3112466293,-1.5738288289));
#68411=CARTESIAN_POINT('Ctrl Pts',(3.73053619354,-36.3857400536,-1.63740845094));
#68412=CARTESIAN_POINT('Ctrl Pts',(3.7495746563,-36.4799878332,-1.6689970964));
#68413=CARTESIAN_POINT('Ctrl Pts',(3.7495746563,-36.5742356128,-1.6689970964));
#68414=CARTESIAN_POINT('Ctrl Pts',(4.24448534634,-36.2742356128,-1.01869348797));
#68415=CARTESIAN_POINT('Ctrl Pts',(4.29909048777,-36.2742356128,-1.09736282407));
#68416=CARTESIAN_POINT('Ctrl Pts',(4.35369562921,-36.3112466293,-1.17603216016));
#68417=CARTESIAN_POINT('Ctrl Pts',(4.39685551792,-36.3857400536,-1.23821239064));
#68418=CARTESIAN_POINT('Ctrl Pts',(4.41829890989,-36.4799878332,-1.26910576216));
#68419=CARTESIAN_POINT('Ctrl Pts',(4.41829890989,-36.5742356128,-1.26910576216));
#68420=CARTESIAN_POINT('Ctrl Pts',(4.92993816697,-36.2742356128,-0.405284473542));
#68421=CARTESIAN_POINT('Ctrl Pts',(4.99982900549,-36.2742356128,-0.471480723113));
#68422=CARTESIAN_POINT('Ctrl Pts',(5.06971984401,-36.3112466293,-0.537676972684));
#68423=CARTESIAN_POINT('Ctrl Pts',(5.12496154763,-36.3857400536,-0.589998473204));
#68424=CARTESIAN_POINT('Ctrl Pts',(5.15240761552,-36.4799878332,-0.615993680209));
#68425=CARTESIAN_POINT('Ctrl Pts',(5.15240761552,-36.5742356128,-0.615993680209));
#68426=CARTESIAN_POINT('Ctrl Pts',(5.39693231373,-36.2742356128,0.342016557109));
#68427=CARTESIAN_POINT('Ctrl Pts',(5.4787021914,-36.2742356128,0.2948529986));
#68428=CARTESIAN_POINT('Ctrl Pts',(5.56047206907,-36.3112466293,0.247689440091));
#68429=CARTESIAN_POINT('Ctrl Pts',(5.62510296248,-36.3857400536,0.210411373802));
#68430=CARTESIAN_POINT('Ctrl Pts',(5.65721391827,-36.4799878332,0.191890287698));
#68431=CARTESIAN_POINT('Ctrl Pts',(5.65721391827,-36.5742356128,0.191890287698));
#68432=CARTESIAN_POINT('Ctrl Pts',(5.4810890824,-36.2742356128,0.496036554802));
#68433=CARTESIAN_POINT('Ctrl Pts',(5.56496873272,-36.2742356128,0.452739908435));
#68434=CARTESIAN_POINT('Ctrl Pts',(5.64884838304,-36.3112466293,0.409443262069));
#68435=CARTESIAN_POINT('Ctrl Pts',(5.71514684025,-36.3857400536,0.375221601448));
#68436=CARTESIAN_POINT('Ctrl Pts',(5.74808630186,-36.4799878332,0.358219049031));
#68437=CARTESIAN_POINT('Ctrl Pts',(5.74808630186,-36.5742356128,0.358219049031));
#68438=CARTESIAN_POINT('Ctrl Pts',(5.60372131748,-36.2742356128,0.754858335755));
#68439=CARTESIAN_POINT('Ctrl Pts',(5.69047130637,-36.2742356128,0.717714053116));
#68440=CARTESIAN_POINT('Ctrl Pts',(5.77722129526,-36.3112466293,0.680569770476));
#68441=CARTESIAN_POINT('Ctrl Pts',(5.84578846738,-36.3857400536,0.651210937785));
#68442=CARTESIAN_POINT('Ctrl Pts',(5.87985510838,-36.4799878332,0.636624411961));
#68443=CARTESIAN_POINT('Ctrl Pts',(5.87985510838,-36.5742356128,0.636624411961));
#68444=CARTESIAN_POINT('Ctrl Pts',(5.70660931534,-36.2742356128,1.02615041344));
#68445=CARTESIAN_POINT('Ctrl Pts',(5.79530810838,-36.2742356128,0.994188908045));
#68446=CARTESIAN_POINT('Ctrl Pts',(5.88400690142,-36.3112466293,0.962227402652));
#68447=CARTESIAN_POINT('Ctrl Pts',(5.95411440796,-36.3857400536,0.936965035973));
#68448=CARTESIAN_POINT('Ctrl Pts',(5.98894634251,-36.4799878332,0.924413781998));
#68449=CARTESIAN_POINT('Ctrl Pts',(5.98894634251,-36.5742356128,0.924413781998));
#68450=CARTESIAN_POINT('Ctrl Pts',(5.74376248036,-36.2742356128,1.13296600714));
#68451=CARTESIAN_POINT('Ctrl Pts',(5.83306897758,-36.2742356128,1.10277988931));
#68452=CARTESIAN_POINT('Ctrl Pts',(5.92237547479,-36.3112466293,1.07259377148));
#68453=CARTESIAN_POINT('Ctrl Pts',(5.99296331053,-36.3857400536,1.04873466986));
#68454=CARTESIAN_POINT('Ctrl Pts',(6.02803389001,-36.4799878332,1.03688060983));
#68455=CARTESIAN_POINT('Ctrl Pts',(6.02803389001,-36.5742356128,1.03688060983));
#68456=CARTESIAN_POINT('Ctrl Pts',(5.79918814733,-36.2742356128,1.3044656396));
#68457=CARTESIAN_POINT('Ctrl Pts',(5.88927282406,-36.2742356128,1.276721735));
#68458=CARTESIAN_POINT('Ctrl Pts',(5.97935750079,-36.3112466293,1.24897783041));
#68459=CARTESIAN_POINT('Ctrl Pts',(6.0505604095,-36.3857400536,1.22704905448));
#68460=CARTESIAN_POINT('Ctrl Pts',(6.08593657929,-36.4799878332,1.21615404846));
#68461=CARTESIAN_POINT('Ctrl Pts',(6.08593657929,-36.5742356128,1.21615404846));
#68462=CARTESIAN_POINT('Ctrl Pts',(5.85112053171,-36.2742356128,1.48092066179));
#68463=CARTESIAN_POINT('Ctrl Pts',(5.94165101522,-36.2742356128,1.45470447779));
#68464=CARTESIAN_POINT('Ctrl Pts',(6.03218149873,-36.3112466293,1.42848829379));
#68465=CARTESIAN_POINT('Ctrl Pts',(6.10373677297,-36.3857400536,1.40776702777));
#68466=CARTESIAN_POINT('Ctrl Pts',(6.13928801073,-36.4799878332,1.39747195633));
#68467=CARTESIAN_POINT('Ctrl Pts',(6.13928801073,-36.5742356128,1.39747195633));
#68468=CARTESIAN_POINT('Ctrl Pts',(5.86993279335,-36.2742356128,1.54652856629));
#68469=CARTESIAN_POINT('Ctrl Pts',(5.96057340692,-36.2742356128,1.52070063308));
#68470=CARTESIAN_POINT('Ctrl Pts',(6.05121402049,-36.3112466293,1.49487269988));
#68471=CARTESIAN_POINT('Ctrl Pts',(6.12285634131,-36.3857400536,1.47445830642));
#68472=CARTESIAN_POINT('Ctrl Pts',(6.15845082724,-36.4799878332,1.4643157015));
#68473=CARTESIAN_POINT('Ctrl Pts',(6.15845082724,-36.5742356128,1.4643157015));
#68474=CARTESIAN_POINT('Ctrl Pts',(5.90547870352,-36.2742356128,1.67276409439));
#68475=CARTESIAN_POINT('Ctrl Pts',(5.99629775732,-36.2742356128,1.6475719299));
#68476=CARTESIAN_POINT('Ctrl Pts',(6.08711681113,-36.3112466293,1.62237976542));
#68477=CARTESIAN_POINT('Ctrl Pts',(6.15890017139,-36.3857400536,1.60246788439));
#68478=CARTESIAN_POINT('Ctrl Pts',(6.19456473032,-36.4799878332,1.59257494429));
#68479=CARTESIAN_POINT('Ctrl Pts',(6.19456473032,-36.5742356128,1.59257494429));
#68480=CARTESIAN_POINT('Ctrl Pts',(5.94051748703,-36.2742356128,1.79907562584));
#68481=CARTESIAN_POINT('Ctrl Pts',(6.03131527525,-36.2742356128,1.77381004956));
#68482=CARTESIAN_POINT('Ctrl Pts',(6.12211306348,-36.3112466293,1.74854447327));
#68483=CARTESIAN_POINT('Ctrl Pts',(6.19387961533,-36.3857400536,1.72857456759));
#68484=CARTESIAN_POINT('Ctrl Pts',(6.22953582338,-36.4799878332,1.71865279873));
#68485=CARTESIAN_POINT('Ctrl Pts',(6.22953582338,-36.5742356128,1.71865279873));
#68486=CARTESIAN_POINT('Ctrl Pts',(5.95837521227,-36.2742356128,1.86312440916));
#68487=CARTESIAN_POINT('Ctrl Pts',(6.04910326111,-36.2742356128,1.8376090522));
#68488=CARTESIAN_POINT('Ctrl Pts',(6.13983130995,-36.3112466293,1.81209369523));
#68489=CARTESIAN_POINT('Ctrl Pts',(6.21154274281,-36.3857400536,1.79192636818));
#68490=CARTESIAN_POINT('Ctrl Pts',(6.24717156127,-36.4799878332,1.78190650545));
#68491=CARTESIAN_POINT('Ctrl Pts',(6.24717156127,-36.5742356128,1.78190650545));
#68492=CARTESIAN_POINT('Ctrl Pts',(6.01765623996,-36.2742356128,2.07213314299));
#68493=CARTESIAN_POINT('Ctrl Pts',(6.10806285924,-36.2742356128,2.04545736833));
#68494=CARTESIAN_POINT('Ctrl Pts',(6.19846947852,-36.3112466293,2.01878159367));
#68495=CARTESIAN_POINT('Ctrl Pts',(6.26992684338,-36.3857400536,1.99769705348));
#68496=CARTESIAN_POINT('Ctrl Pts',(6.30542944689,-36.4799878332,1.98722151502));
#68497=CARTESIAN_POINT('Ctrl Pts',(6.30542944689,-36.5742356128,1.98722151502));
#68498=CARTESIAN_POINT('Ctrl Pts',(6.08567485884,-36.2742356128,2.29020798204));
#68499=CARTESIAN_POINT('Ctrl Pts',(6.17503220776,-36.2742356128,2.26008450139));
#68500=CARTESIAN_POINT('Ctrl Pts',(6.26438955668,-36.3112466293,2.22996102075));
#68501=CARTESIAN_POINT('Ctrl Pts',(6.33501760237,-36.3857400536,2.20615146186));
#68502=CARTESIAN_POINT('Ctrl Pts',(6.37010813448,-36.4799878332,2.19432196508));
#68503=CARTESIAN_POINT('Ctrl Pts',(6.37010813448,-36.5742356128,2.19432196508));
#68504=CARTESIAN_POINT('Ctrl Pts',(6.13676392343,-36.2742356128,2.43482563093));
#68505=CARTESIAN_POINT('Ctrl Pts',(6.2249876692,-36.2742356128,2.40121723527));
#68506=CARTESIAN_POINT('Ctrl Pts',(6.31321141497,-36.3112466293,2.3676088396));
#68507=CARTESIAN_POINT('Ctrl Pts',(6.38294338684,-36.3857400536,2.34104466316));
#68508=CARTESIAN_POINT('Ctrl Pts',(6.41758882819,-36.4799878332,2.32784678495));
#68509=CARTESIAN_POINT('Ctrl Pts',(6.41758882819,-36.5742356128,2.32784678495));
#68510=CARTESIAN_POINT('Ctrl Pts',(6.19859174917,-36.2742356128,2.58091129692));
#68511=CARTESIAN_POINT('Ctrl Pts',(6.28484385346,-36.2742356128,2.54230495555));
#68512=CARTESIAN_POINT('Ctrl Pts',(6.37109595776,-36.3112466293,2.50369861417));
#68513=CARTESIAN_POINT('Ctrl Pts',(6.43926964058,-36.3857400536,2.47318424312));
#68514=CARTESIAN_POINT('Ctrl Pts',(6.47314072418,-36.4799878332,2.45802349563));
#68515=CARTESIAN_POINT('Ctrl Pts',(6.47314072418,-36.5742356128,2.45802349563));
#68516=CARTESIAN_POINT('Ctrl Pts',(6.27496287808,-36.2742356128,2.72284550202));
#68517=CARTESIAN_POINT('Ctrl Pts',(6.35795875815,-36.2742356128,2.67818760544));
#68518=CARTESIAN_POINT('Ctrl Pts',(6.44095463823,-36.3112466293,2.63352970885));
#68519=CARTESIAN_POINT('Ctrl Pts',(6.50655456359,-36.3857400536,2.59823211721));
#68520=CARTESIAN_POINT('Ctrl Pts',(6.53914696948,-36.4799878332,2.58069500223));
#68521=CARTESIAN_POINT('Ctrl Pts',(6.53914696948,-36.5742356128,2.58069500223));
#68522=CARTESIAN_POINT('Ctrl Pts',(2.42434411094,-36.5742356128,-2.36824808793));
#68523=CARTESIAN_POINT('Ctrl Pts',(2.54136162563,-36.5742356128,-2.31314371739));
#68524=CARTESIAN_POINT('Ctrl Pts',(2.65752099957,-36.5742356128,-2.25621686612));
#68525=CARTESIAN_POINT('Ctrl Pts',(2.77407974247,-36.5742356128,-2.1971394748));
#68526=CARTESIAN_POINT('Ctrl Pts',(3.24315352432,-36.5742356128,-1.95213056688));
#68527=CARTESIAN_POINT('Ctrl Pts',(3.70906725491,-36.5742356128,-1.67871445412));
#68528=CARTESIAN_POINT('Ctrl Pts',(4.05512009518,-36.5742356128,-1.45762154475));
#68529=CARTESIAN_POINT('Ctrl Pts',(4.83098837637,-36.5742356128,-0.890342468227));
#68530=CARTESIAN_POINT('Ctrl Pts',(5.472362609,-36.5742356128,-0.180892800224));
#68531=CARTESIAN_POINT('Ctrl Pts',(5.76642241654,-36.5742356128,0.2786624797));
#68532=CARTESIAN_POINT('Ctrl Pts',(6.00694923868,-36.5742356128,0.922077058536));
#68533=CARTESIAN_POINT('Ctrl Pts',(6.19138019969,-36.5742356128,1.57972239002));
#68534=CARTESIAN_POINT('Ctrl Pts',(6.22058475326,-36.5742356128,1.68729406867));
#68535=CARTESIAN_POINT('Ctrl Pts',(6.29416488239538,-36.5742356128,1.9543061191784));
#68536=CARTESIAN_POINT('Ctrl Pts',(6.37839829623924,-36.5742356128,2.2167883668313));
#68537=CARTESIAN_POINT('Ctrl Pts',(6.4240234576883,-36.5742356128,2.3426643448704));
#68538=CARTESIAN_POINT('Ctrl Pts',(6.47656234367984,-36.5742356128,2.46438238106866));
#68539=CARTESIAN_POINT('Ctrl Pts',(6.53914700243265,-36.5742356128,2.58069506476114));
#68540=CARTESIAN_POINT('Ctrl Pts',(6.53914703241,-37.9742356128,2.58069512031));
#68541=CARTESIAN_POINT('Ctrl Pts',(6.5391470324,-38.0684833925,2.58069512029));
#68542=CARTESIAN_POINT('Ctrl Pts',(6.50655461068,-38.1627311721,2.59823220638));
#68543=CARTESIAN_POINT('Ctrl Pts',(6.44095465346,-38.2372245963,2.63352973988));
#68544=CARTESIAN_POINT('Ctrl Pts',(6.35795873309,-38.2742356128,2.67818756293));
#68545=CARTESIAN_POINT('Ctrl Pts',(6.27496281272,-38.2742356128,2.72284538598));
#68546=CARTESIAN_POINT('Ctrl Pts',(6.47749928031,-37.9742356128,2.46612372063));
#68547=CARTESIAN_POINT('Ctrl Pts',(6.47749928325,-38.0684833921,2.46612372592));
#68548=CARTESIAN_POINT('Ctrl Pts',(6.44371355209,-38.1627311714,2.4814430712));
#68549=CARTESIAN_POINT('Ctrl Pts',(6.37571165731,-38.2372245955,2.51227664714));
#68550=CARTESIAN_POINT('Ctrl Pts',(6.2896768948,-38.2742356123,2.55128684019));
#68551=CARTESIAN_POINT('Ctrl Pts',(6.20364213078,-38.2742356128,2.59029703093));
#68552=CARTESIAN_POINT('Ctrl Pts',(6.4250505295,-37.9742356128,2.34529109436));
#68553=CARTESIAN_POINT('Ctrl Pts',(6.4250505205,-38.0684834574,2.34529107738));
#68554=CARTESIAN_POINT('Ctrl Pts',(6.39050752202,-38.1627313021,2.35875081294));
#68555=CARTESIAN_POINT('Ctrl Pts',(6.3209817521,-38.2372247495,2.38584206978));
#68556=CARTESIAN_POINT('Ctrl Pts',(6.23301891757,-38.2742357149,2.4201173123));
#68557=CARTESIAN_POINT('Ctrl Pts',(6.14505612298,-38.2742356128,2.45439254437));
#68558=CARTESIAN_POINT('Ctrl Pts',(6.37923785733,-37.9742356128,2.21935750204));
#68559=CARTESIAN_POINT('Ctrl Pts',(6.37923785229,-38.0684834205,2.21935748159));
#68560=CARTESIAN_POINT('Ctrl Pts',(6.34424285411,-38.1627312282,2.23147400682));
#68561=CARTESIAN_POINT('Ctrl Pts',(6.27380710482,-38.2372246625,2.25586132033));
#68562=CARTESIAN_POINT('Ctrl Pts',(6.18469305765,-38.274235657,2.28671576875));
#68563=CARTESIAN_POINT('Ctrl Pts',(6.09557902928,-38.2742356128,2.31757022073));
#68564=CARTESIAN_POINT('Ctrl Pts',(6.29255842824,-37.9742356128,1.94958030449));
#68565=CARTESIAN_POINT('Ctrl Pts',(6.29255843379,-38.0684833616,1.94958032698));
#68566=CARTESIAN_POINT('Ctrl Pts',(6.25694629473,-38.1627311103,1.95971958966));
#68567=CARTESIAN_POINT('Ctrl Pts',(6.18526848373,-38.2372245236,1.98012731791));
#68568=CARTESIAN_POINT('Ctrl Pts',(6.09458293312,-38.2742355643,2.00594677005));
#68569=CARTESIAN_POINT('Ctrl Pts',(6.00389736185,-38.2742356128,2.03176621828));
#68570=CARTESIAN_POINT('Ctrl Pts',(6.21629158074,-37.9742356128,1.67179392517));
#68571=CARTESIAN_POINT('Ctrl Pts',(6.21629157465,-38.0684834264,1.67179390044));
#68572=CARTESIAN_POINT('Ctrl Pts',(6.18059131343,-38.16273124,1.68154041674));
#68573=CARTESIAN_POINT('Ctrl Pts',(6.10873604958,-38.2372246763,1.70115751673));
#68574=CARTESIAN_POINT('Ctrl Pts',(6.01782606333,-38.2742356662,1.72597678277));
#68575=CARTESIAN_POINT('Ctrl Pts',(5.92691609981,-38.2742356128,1.75079605312));
#68576=CARTESIAN_POINT('Ctrl Pts',(6.18335047849,-37.9742356128,1.55015139283));
#68577=CARTESIAN_POINT('Ctrl Pts',(6.18335048466,-38.068483409,1.55015141338));
#68578=CARTESIAN_POINT('Ctrl Pts',(6.1476764427,-38.1627312051,1.56001197253));
#68579=CARTESIAN_POINT('Ctrl Pts',(6.07587398952,-38.2372246353,1.57985865724));
#68580=CARTESIAN_POINT('Ctrl Pts',(5.98503078164,-38.2742356388,1.60496832085));
#68581=CARTESIAN_POINT('Ctrl Pts',(5.89418758109,-38.2742356128,1.63007797337));
#68582=CARTESIAN_POINT('Ctrl Pts',(6.10683421874,-37.9742356128,1.27934110155));
#68583=CARTESIAN_POINT('Ctrl Pts',(6.10683421362,-38.0684833787,1.2793410845));
#68584=CARTESIAN_POINT('Ctrl Pts',(6.07133589713,-38.1627311446,1.28985606578));
#68585=CARTESIAN_POINT('Ctrl Pts',(5.99988714566,-38.237224564,1.31101997322));
#68586=CARTESIAN_POINT('Ctrl Pts',(5.90949143082,-38.2742355913,1.33779619135));
#68587=CARTESIAN_POINT('Ctrl Pts',(5.81909570989,-38.2742356128,1.36457241864));
#68588=CARTESIAN_POINT('Ctrl Pts',(6.02154757341,-37.9742356128,1.0171856396));
#68589=CARTESIAN_POINT('Ctrl Pts',(6.02154757766,-38.0684834038,1.01718565375));
#68590=CARTESIAN_POINT('Ctrl Pts',(5.98651519,-38.1627311948,1.02915949851));
#68591=CARTESIAN_POINT('Ctrl Pts',(5.91600421823,-38.2372246232,1.05325967438));
#68592=CARTESIAN_POINT('Ctrl Pts',(5.82679497009,-38.2742356307,1.08375078668));
#68593=CARTESIAN_POINT('Ctrl Pts',(5.737585727,-38.2742356128,1.11424189141));
#68594=CARTESIAN_POINT('Ctrl Pts',(5.97900661099,-37.9742356128,0.896224423713));
#68595=CARTESIAN_POINT('Ctrl Pts',(5.97900661569,-38.0684834269,0.896224436759));
#68596=CARTESIAN_POINT('Ctrl Pts',(5.94423871805,-38.162731241,0.908957424316));
#68597=CARTESIAN_POINT('Ctrl Pts',(5.87426009442,-38.2372246775,0.934585556151));
#68598=CARTESIAN_POINT('Ctrl Pts',(5.78572437213,-38.274235667,0.967009808905));
#68599=CARTESIAN_POINT('Ctrl Pts',(5.69718866798,-38.2742356128,0.999434049256));
#68600=CARTESIAN_POINT('Ctrl Pts',(5.88756297838,-37.9742356128,0.659856731438));
#68601=CARTESIAN_POINT('Ctrl Pts',(5.88756298491,-38.0684834275,0.659856746387));
#68602=CARTESIAN_POINT('Ctrl Pts',(5.85345466069,-38.1627312422,0.674306677198));
#68603=CARTESIAN_POINT('Ctrl Pts',(5.78480358285,-38.2372246789,0.703390562944));
#68604=CARTESIAN_POINT('Ctrl Pts',(5.69794744689,-38.2742356679,0.740186972418));
#68605=CARTESIAN_POINT('Ctrl Pts',(5.61109132821,-38.2742356128,0.776983367386));
#68606=CARTESIAN_POINT('Ctrl Pts',(5.78044949711,-37.9742356128,0.430172441648));
#68607=CARTESIAN_POINT('Ctrl Pts',(5.78044950152,-38.0684834047,0.430172449852));
#68608=CARTESIAN_POINT('Ctrl Pts',(5.74724282873,-38.1627311966,0.44656967303));
#68609=CARTESIAN_POINT('Ctrl Pts',(5.68040654018,-38.2372246253,0.47957295341));
#68610=CARTESIAN_POINT('Ctrl Pts',(5.59584643675,-38.2742356321,0.521328119811));
#68611=CARTESIAN_POINT('Ctrl Pts',(5.51128633822,-38.2742356128,0.56308327929));
#68612=CARTESIAN_POINT('Ctrl Pts',(5.7226529197,-37.9742356128,0.317367361304));
#68613=CARTESIAN_POINT('Ctrl Pts',(5.72265292242,-38.068483393,0.317367365818));
#68614=CARTESIAN_POINT('Ctrl Pts',(5.68995600371,-38.1627311732,0.334765690655));
#68615=CARTESIAN_POINT('Ctrl Pts',(5.62414571793,-38.2372245977,0.369783928543));
#68616=CARTESIAN_POINT('Ctrl Pts',(5.54088369215,-38.2742356138,0.414088388794));
#68617=CARTESIAN_POINT('Ctrl Pts',(5.4576216655,-38.2742356128,0.458392846952));
#68618=CARTESIAN_POINT('Ctrl Pts',(5.56080084046,-37.9742356128,0.0295320933249));
#68619=CARTESIAN_POINT('Ctrl Pts',(5.56080083609,-38.0684833915,0.0295320860792));
#68620=CARTESIAN_POINT('Ctrl Pts',(5.52957060213,-38.1627311702,0.0495393442441));
#68621=CARTESIAN_POINT('Ctrl Pts',(5.46671237524,-38.2372245941,0.089808691663));
#68622=CARTESIAN_POINT('Ctrl Pts',(5.38718524665,-38.2742356113,0.140756771766));
#68623=CARTESIAN_POINT('Ctrl Pts',(5.30765811944,-38.2742356128,0.191704855228));
#68624=CARTESIAN_POINT('Ctrl Pts',(5.37029202866,-37.9742356128,-0.241067403666));
#68625=CARTESIAN_POINT('Ctrl Pts',(5.37029203567,-38.068483394,-0.241067392035));
#68626=CARTESIAN_POINT('Ctrl Pts',(5.34079929298,-38.1627311751,-0.218590865746));
#68627=CARTESIAN_POINT('Ctrl Pts',(5.2814381653,-38.2372245999,-0.17335155271));
#68628=CARTESIAN_POINT('Ctrl Pts',(5.2063354988,-38.2742356152,-0.116115572303));
#68629=CARTESIAN_POINT('Ctrl Pts',(5.13123283009,-38.2742356128,-0.0588795972884));
#68630=CARTESIAN_POINT('Ctrl Pts',(5.24251980415,-37.9742356128,-0.400329171328));
#68631=CARTESIAN_POINT('Ctrl Pts',(5.24251981319,-38.0684833825,-0.400329163319));
#68632=CARTESIAN_POINT('Ctrl Pts',(5.21414835053,-38.1627311521,-0.376472093618));
#68633=CARTESIAN_POINT('Ctrl Pts',(5.15704406285,-38.2372245728,-0.328454107043));
#68634=CARTESIAN_POINT('Ctrl Pts',(5.08479670601,-38.2742355971,-0.267702591492));
#68635=CARTESIAN_POINT('Ctrl Pts',(5.01254934105,-38.2742356128,-0.206951074935));
#68636=CARTESIAN_POINT('Ctrl Pts',(4.6934087233,-37.9742356128,-1.00944907659));
#68637=CARTESIAN_POINT('Ctrl Pts',(4.6934086961,-38.0684834225,-1.00944910069));
#68638=CARTESIAN_POINT('Ctrl Pts',(4.66949795797,-38.1627312322,-0.980685909202));
#68639=CARTESIAN_POINT('Ctrl Pts',(4.6213719682,-38.2372246672,-0.922793157139));
#68640=CARTESIAN_POINT('Ctrl Pts',(4.56048383437,-38.2742356601,-0.84954825045));
#68641=CARTESIAN_POINT('Ctrl Pts',(4.49959572501,-38.2742356128,-0.776303346788));
#68642=CARTESIAN_POINT('Ctrl Pts',(4.02409822752,-37.9742356128,-1.50218108799));
#68643=CARTESIAN_POINT('Ctrl Pts',(4.02409830939,-38.0684833019,-1.50218101545));
#68644=CARTESIAN_POINT('Ctrl Pts',(4.00389313666,-38.1627309911,-1.47102303591));
#68645=CARTESIAN_POINT('Ctrl Pts',(3.96322537228,-38.2372243831,-1.40831031261));
#68646=CARTESIAN_POINT('Ctrl Pts',(3.91177314147,-38.2742354707,-1.3289672931));
#68647=CARTESIAN_POINT('Ctrl Pts',(3.860320837,-38.2742356128,-1.24962426449));
#68648=CARTESIAN_POINT('Ctrl Pts',(3.49329943878,-37.9742356128,-1.81694867414));
#68649=CARTESIAN_POINT('Ctrl Pts',(3.49329940337,-38.0684833917,-1.81694869081));
#68650=CARTESIAN_POINT('Ctrl Pts',(3.4746893405,-38.1627311706,-1.78496313544));
#68651=CARTESIAN_POINT('Ctrl Pts',(3.43723215534,-38.2372245946,-1.72058465543));
#68652=CARTESIAN_POINT('Ctrl Pts',(3.38984202793,-38.2742356117,-1.63913410317));
#68653=CARTESIAN_POINT('Ctrl Pts',(3.34245191658,-38.2742356128,-1.55768354279));
#68654=CARTESIAN_POINT('Ctrl Pts',(2.96849813462,-37.9742356128,-2.11200213165));
#68655=CARTESIAN_POINT('Ctrl Pts',(2.96849813462,-38.0684833924,-2.11200213165));
#68656=CARTESIAN_POINT('Ctrl Pts',(2.9507901825,-38.1627311721,-2.07943156023));
#68657=CARTESIAN_POINT('Ctrl Pts',(2.91514879128,-38.2372245963,-2.01387555828));
#68658=CARTESIAN_POINT('Ctrl Pts',(2.8700559069,-38.2742356128,-1.93093525801));
#68659=CARTESIAN_POINT('Ctrl Pts',(2.82496302107,-38.2742356128,-1.84799495842));
#68660=CARTESIAN_POINT('Ctrl Pts',(2.42434411094,-37.9742356128,-2.36824808793));
#68661=CARTESIAN_POINT('Ctrl Pts',(2.42434411094,-38.0684833924,-2.36824808793));
#68662=CARTESIAN_POINT('Ctrl Pts',(2.40857619105,-38.1627311721,-2.33476394176));
#68663=CARTESIAN_POINT('Ctrl Pts',(2.37683952295,-38.2372245963,-2.26736917817));
#68664=CARTESIAN_POINT('Ctrl Pts',(2.33668684465,-38.2742356128,-2.18210250012));
#68665=CARTESIAN_POINT('Ctrl Pts',(2.29653416635,-38.2742356128,-2.09683582206));
#68666=CARTESIAN_POINT('Ctrl Pts',(2.42434411094,-37.9742356128,-2.36824808793));
#68667=CARTESIAN_POINT('Ctrl Pts',(2.96849813462,-37.9742356128005,-2.11200213165));
#68668=CARTESIAN_POINT('Ctrl Pts',(3.49329943878,-37.9742356128005,-1.81694867414));
#68669=CARTESIAN_POINT('Ctrl Pts',(4.02409822752,-37.9742356128005,-1.50218108799));
#68670=CARTESIAN_POINT('Ctrl Pts',(4.6934087233,-37.9742356128005,-1.00944907659));
#68671=CARTESIAN_POINT('Ctrl Pts',(5.24251980415,-37.9742356128005,-0.400329171328));
#68672=CARTESIAN_POINT('Ctrl Pts',(5.37029202866,-37.9742356128005,-0.241067403666));
#68673=CARTESIAN_POINT('Ctrl Pts',(5.56080084046,-37.9742356128005,0.0295320933249));
#68674=CARTESIAN_POINT('Ctrl Pts',(5.7226529197,-37.9742356128005,0.317367361304));
#68675=CARTESIAN_POINT('Ctrl Pts',(5.78044949711,-37.9742356128005,0.430172441648));
#68676=CARTESIAN_POINT('Ctrl Pts',(5.88756297838,-37.9742356128005,0.659856731438));
#68677=CARTESIAN_POINT('Ctrl Pts',(5.97900661099,-37.9742356128005,0.896224423713));
#68678=CARTESIAN_POINT('Ctrl Pts',(6.02154757341,-37.9742356128005,1.0171856396));
#68679=CARTESIAN_POINT('Ctrl Pts',(6.10683421874,-37.9742356128005,1.27934110155));
#68680=CARTESIAN_POINT('Ctrl Pts',(6.18335047849,-37.9742356128005,1.55015139283));
#68681=CARTESIAN_POINT('Ctrl Pts',(6.21629158074,-37.9742356128005,1.67179392517));
#68682=CARTESIAN_POINT('Ctrl Pts',(6.29255842824,-37.9742356128005,1.94958030449));
#68683=CARTESIAN_POINT('Ctrl Pts',(6.37923785733,-37.9742356128005,2.21935750204));
#68684=CARTESIAN_POINT('Ctrl Pts',(6.4250505295,-37.9742356128005,2.34529109436));
#68685=CARTESIAN_POINT('Ctrl Pts',(6.47749928031,-37.9742356128005,2.46612372063));
#68686=CARTESIAN_POINT('Ctrl Pts',(6.53914701908,-37.9742356128,2.5806950957));
#68687=CARTESIAN_POINT('Ctrl Pts',(2.42434411094,-37.9742356128,-2.36824808793));
#68688=CARTESIAN_POINT('Ctrl Pts',(2.42434411094,-36.2942356128,-2.36824808793));
#68689=CARTESIAN_POINT('Ctrl Pts',(2.54136162563,-37.9742356128,-2.31314371739));
#68690=CARTESIAN_POINT('Ctrl Pts',(2.54136162563,-36.2942356128,-2.31314371739));
#68691=CARTESIAN_POINT('Ctrl Pts',(2.65752099957,-37.9742356128,-2.25621686612));
#68692=CARTESIAN_POINT('Ctrl Pts',(2.65752099957,-36.2942356128,-2.25621686612));
#68693=CARTESIAN_POINT('Ctrl Pts',(2.77407974247,-37.9742356128,-2.1971394748));
#68694=CARTESIAN_POINT('Ctrl Pts',(2.77407974247,-36.2942356128,-2.1971394748));
#68695=CARTESIAN_POINT('Ctrl Pts',(3.24315352432,-37.9742356128,-1.95213056688));
#68696=CARTESIAN_POINT('Ctrl Pts',(3.24315352432,-36.2942356128,-1.95213056688));
#68697=CARTESIAN_POINT('Ctrl Pts',(3.70906725491,-37.9742356128,-1.67871445412));
#68698=CARTESIAN_POINT('Ctrl Pts',(3.70906725491,-36.2942356128,-1.67871445412));
#68699=CARTESIAN_POINT('Ctrl Pts',(4.05512009518,-37.9742356128,-1.45762154475));
#68700=CARTESIAN_POINT('Ctrl Pts',(4.05512009518,-36.2942356128,-1.45762154475));
#68701=CARTESIAN_POINT('Ctrl Pts',(4.83098837637,-37.9742356128,-0.890342468227));
#68702=CARTESIAN_POINT('Ctrl Pts',(4.83098837637,-36.2942356128,-0.890342468227));
#68703=CARTESIAN_POINT('Ctrl Pts',(5.472362609,-37.9742356128,-0.180892800224));
#68704=CARTESIAN_POINT('Ctrl Pts',(5.472362609,-36.2942356128,-0.180892800224));
#68705=CARTESIAN_POINT('Ctrl Pts',(5.76642241654,-37.9742356128,0.2786624797));
#68706=CARTESIAN_POINT('Ctrl Pts',(5.76642241654,-36.2942356128,0.2786624797));
#68707=CARTESIAN_POINT('Ctrl Pts',(6.00694923868,-37.9742356128,0.922077058536));
#68708=CARTESIAN_POINT('Ctrl Pts',(6.00694923868,-36.2942356128,0.922077058536));
#68709=CARTESIAN_POINT('Ctrl Pts',(6.19138019969,-37.9742356128,1.57972239002));
#68710=CARTESIAN_POINT('Ctrl Pts',(6.19138019969,-36.2942356128,1.57972239002));
#68711=CARTESIAN_POINT('Ctrl Pts',(6.22058475326,-37.9742356128,1.68729406867));
#68712=CARTESIAN_POINT('Ctrl Pts',(6.22058475326,-36.2942356128,1.68729406867));
#68713=CARTESIAN_POINT('Ctrl Pts',(6.2941648843,-37.9742356128,1.95430612609));
#68714=CARTESIAN_POINT('Ctrl Pts',(6.2941648843,-36.2942356128,1.95430612609));
#68715=CARTESIAN_POINT('Ctrl Pts',(6.3783983006,-37.9742356128,2.21678838042));
#68716=CARTESIAN_POINT('Ctrl Pts',(6.3783983006,-36.2942356128,2.21678838042));
#68717=CARTESIAN_POINT('Ctrl Pts',(6.42402346497,-37.9742356128,2.34266436496));
#68718=CARTESIAN_POINT('Ctrl Pts',(6.42402346497,-36.2942356128,2.34266436496));
#68719=CARTESIAN_POINT('Ctrl Pts',(6.47656235486,-37.9742356128,2.46438240697));
#68720=CARTESIAN_POINT('Ctrl Pts',(6.47656235486,-36.2942356128,2.46438240697));
#68721=CARTESIAN_POINT('Ctrl Pts',(6.53914701908,-37.9742356128,2.5806950957));
#68722=CARTESIAN_POINT('Ctrl Pts',(6.53914701908,-36.2942356128,2.5806950957));
#68723=CARTESIAN_POINT('Ctrl Pts',(6.62478636278,-36.5742356128,4.12129363314));
#68724=CARTESIAN_POINT('Ctrl Pts',(6.62478636278,-36.4799878332,4.12129363314));
#68725=CARTESIAN_POINT('Ctrl Pts',(6.64533881083,-36.3857400536,4.09051357105));
#68726=CARTESIAN_POINT('Ctrl Pts',(6.68670547342,-36.3112466293,4.02856141623));
#68727=CARTESIAN_POINT('Ctrl Pts',(6.7390418526,-36.2742356128,3.95018063176));
#68728=CARTESIAN_POINT('Ctrl Pts',(6.79137823178,-36.2742356128,3.87179984728));
#68729=CARTESIAN_POINT('Ctrl Pts',(6.98489076396,-36.5742356128,4.36174236824));
#68730=CARTESIAN_POINT('Ctrl Pts',(6.98489076396,-36.4799878332,4.36174236824));
#68731=CARTESIAN_POINT('Ctrl Pts',(7.00065080016,-36.3857400536,4.3277623195));
#68732=CARTESIAN_POINT('Ctrl Pts',(7.03237160049,-36.3112466293,4.25936943399));
#68733=CARTESIAN_POINT('Ctrl Pts',(7.07250420315,-36.2742356128,4.17283994981));
#68734=CARTESIAN_POINT('Ctrl Pts',(7.11263680581,-36.2742356128,4.08631046562));
#68735=CARTESIAN_POINT('Ctrl Pts',(7.39717344286,-36.5742356128,4.53703336491));
#68736=CARTESIAN_POINT('Ctrl Pts',(7.39717342808,-36.4799878254,4.53703335475));
#68737=CARTESIAN_POINT('Ctrl Pts',(7.40695489431,-36.385740038,4.50036897905));
#68738=CARTESIAN_POINT('Ctrl Pts',(7.42664242728,-36.3112466109,4.42657326421));
#68739=CARTESIAN_POINT('Ctrl Pts',(7.45155075762,-36.2742356005,4.33320822323));
#68740=CARTESIAN_POINT('Ctrl Pts',(7.47645909178,-36.2742356128,4.23984319062));
#68741=CARTESIAN_POINT('Ctrl Pts',(7.85671042359,-36.5742356128,4.61558616292));
#68742=CARTESIAN_POINT('Ctrl Pts',(7.85671043413,-36.4799878271,4.61558615243));
#68743=CARTESIAN_POINT('Ctrl Pts',(7.85903775873,-36.3857400413,4.57747578228));
#68744=CARTESIAN_POINT('Ctrl Pts',(7.86372203974,-36.3112466149,4.50076965772));
#68745=CARTESIAN_POINT('Ctrl Pts',(7.86964850582,-36.2742356032,4.40372241788));
#68746=CARTESIAN_POINT('Ctrl Pts',(7.87557497252,-36.2742356128,4.30667518455));
#68747=CARTESIAN_POINT('Ctrl Pts',(8.54369953399,-36.5742356128,4.54933608482));
#68748=CARTESIAN_POINT('Ctrl Pts',(8.54369952872,-36.4799878363,4.54933609007));
#68749=CARTESIAN_POINT('Ctrl Pts',(8.53475132294,-36.3857400598,4.51242231126));
#68750=CARTESIAN_POINT('Ctrl Pts',(8.51674094895,-36.3112466366,4.43812459524));
#68751=CARTESIAN_POINT('Ctrl Pts',(8.49395453991,-36.2742356177,4.34412441801));
#68752=CARTESIAN_POINT('Ctrl Pts',(8.47116813057,-36.2742356128,4.25012423752));
#68753=CARTESIAN_POINT('Ctrl Pts',(9.14546603834,-36.5742356128,4.26313835988));
#68754=CARTESIAN_POINT('Ctrl Pts',(9.14546604097,-36.4799878317,4.26313835725));
#68755=CARTESIAN_POINT('Ctrl Pts',(9.12717740792,-36.3857400506,4.2306861245));
#68756=CARTESIAN_POINT('Ctrl Pts',(9.09036720445,-36.3112466257,4.16536833407));
#68757=CARTESIAN_POINT('Ctrl Pts',(9.04379557728,-36.2742356104,4.08272940811));
#68758=CARTESIAN_POINT('Ctrl Pts',(8.99722395025,-36.2742356128,4.00009048378));
#68759=CARTESIAN_POINT('Ctrl Pts',(9.33430629029,-36.5742356128,4.1449615154));
#68760=CARTESIAN_POINT('Ctrl Pts',(9.33430624684,-36.4799878386,4.14496156749));
#68761=CARTESIAN_POINT('Ctrl Pts',(9.31320927896,-36.3857400644,4.11430294877));
#68762=CARTESIAN_POINT('Ctrl Pts',(9.27074665566,-36.311246642,4.05259522538));
#68763=CARTESIAN_POINT('Ctrl Pts',(9.21702372832,-36.2742356213,3.97452363113));
#68764=CARTESIAN_POINT('Ctrl Pts',(9.16330081692,-36.2742356128,3.89645201289));
#68765=CARTESIAN_POINT('Ctrl Pts',(9.68898808689,-36.5742356128,3.86407647413));
#68766=CARTESIAN_POINT('Ctrl Pts',(9.68898813284,-36.4799878275,3.86407641904));
#68767=CARTESIAN_POINT('Ctrl Pts',(9.66297620974,-36.3857400423,3.83738683986));
#68768=CARTESIAN_POINT('Ctrl Pts',(9.61062104631,-36.3112466159,3.7836677505));
#68769=CARTESIAN_POINT('Ctrl Pts',(9.54438216355,-36.2742356039,3.7157033607));
#68770=CARTESIAN_POINT('Ctrl Pts',(9.47814326392,-36.2742356128,3.64773899629));
#68771=CARTESIAN_POINT('Ctrl Pts',(9.97409371558,-36.5742356128,3.5368417215));
#68772=CARTESIAN_POINT('Ctrl Pts',(9.97409366698,-36.4799878392,3.53684177977));
#68773=CARTESIAN_POINT('Ctrl Pts',(9.94505212424,-36.3857400657,3.51373460238));
#68774=CARTESIAN_POINT('Ctrl Pts',(9.88659916874,-36.3112466435,3.46722594263));
#68775=CARTESIAN_POINT('Ctrl Pts',(9.81264555648,-36.2742356223,3.40838393028));
#68776=CARTESIAN_POINT('Ctrl Pts',(9.73869196204,-36.2742356128,3.34954189108));
#68777=CARTESIAN_POINT('Ctrl Pts',(10.1029300816,-36.5742356128,3.36222205123));
#68778=CARTESIAN_POINT('Ctrl Pts',(10.1029301671,-36.4799878807,3.36222190496));
#68779=CARTESIAN_POINT('Ctrl Pts',(10.0727204671,-36.3857401486,3.34076368711));
#68780=CARTESIAN_POINT('Ctrl Pts',(10.0119163664,-36.3112467413,3.29757384942));
#68781=CARTESIAN_POINT('Ctrl Pts',(9.93498794039,-36.2742356875,3.24293101687));
#68782=CARTESIAN_POINT('Ctrl Pts',(9.85805945703,-36.2742356128,3.18828822444));
#68783=CARTESIAN_POINT('Ctrl Pts',(10.2192706083,-36.5742356128,3.18776254463));
#68784=CARTESIAN_POINT('Ctrl Pts',(10.2192705627,-36.4799878336,3.18776261966));
#68785=CARTESIAN_POINT('Ctrl Pts',(10.1883194918,-36.3857400544,3.16743138786));
#68786=CARTESIAN_POINT('Ctrl Pts',(10.1260230843,-36.3112466302,3.12651006944));
#68787=CARTESIAN_POINT('Ctrl Pts',(10.0472068327,-36.2742356134,3.07473700749));
#68788=CARTESIAN_POINT('Ctrl Pts',(9.96839059861,-36.2742356128,3.02296391637));
#68789=CARTESIAN_POINT('Ctrl Pts',(10.3257938388,-36.5742356128,3.01323063831));
#68790=CARTESIAN_POINT('Ctrl Pts',(10.3257938435,-36.4799878332,3.01323063056));
#68791=CARTESIAN_POINT('Ctrl Pts',(10.2942021431,-36.3857400536,2.99394903723));
#68792=CARTESIAN_POINT('Ctrl Pts',(10.2306163683,-36.3112466293,2.9551402798));
#68793=CARTESIAN_POINT('Ctrl Pts',(10.1501687536,-36.2742356128,2.90604012229));
#68794=CARTESIAN_POINT('Ctrl Pts',(10.0697211371,-36.2742356128,2.85693996784));
#68795=CARTESIAN_POINT('',(6.6247863622675,-36.5742356128,4.121293632315));
#68796=CARTESIAN_POINT('Origin',(6.79020000386945,-36.572114293675,3.87356387873257));
#68797=CARTESIAN_POINT('',(10.3257952821,-36.5742356128,3.01322822759));
#68798=CARTESIAN_POINT('Ctrl Pts',(6.62478636278,-36.5742356128,4.12129363314));
#68799=CARTESIAN_POINT('Ctrl Pts',(6.98489076396,-36.5742356127964,4.36174236824));
#68800=CARTESIAN_POINT('Ctrl Pts',(7.39717344286,-36.5742356127964,4.53703336491));
#68801=CARTESIAN_POINT('Ctrl Pts',(7.85671042359,-36.5742356127964,4.61558616292));
#68802=CARTESIAN_POINT('Ctrl Pts',(8.54369953399,-36.5742356127964,4.54933608482));
#68803=CARTESIAN_POINT('Ctrl Pts',(9.14546603834001,-36.5742356127964,4.26313835988));
#68804=CARTESIAN_POINT('Ctrl Pts',(9.33430629029,-36.5742356127964,4.1449615154));
#68805=CARTESIAN_POINT('Ctrl Pts',(9.68898808689,-36.5742356127964,3.86407647413));
#68806=CARTESIAN_POINT('Ctrl Pts',(9.97409371558,-36.5742356127964,3.5368417215));
#68807=CARTESIAN_POINT('Ctrl Pts',(10.1029300816,-36.5742356127964,3.36222205123));
#68808=CARTESIAN_POINT('Ctrl Pts',(10.2192706083,-36.5742356127964,3.18776254463));
#68809=CARTESIAN_POINT('Ctrl Pts',(10.3257952821,-36.5742356128,3.01322822759));
#68810=CARTESIAN_POINT('Origin',(10.0715309146271,-36.5721142827529,2.85804663423425));
#68811=CARTESIAN_POINT('Ctrl Pts',(10.0697226343,-38.2742356128,2.85693747561));
#68812=CARTESIAN_POINT('Ctrl Pts',(10.1501702339,-38.2742356128,2.9060376555));
#68813=CARTESIAN_POINT('Ctrl Pts',(10.2306178336,-38.2372245963,2.95513783538));
#68814=CARTESIAN_POINT('Ctrl Pts',(10.2942035987,-38.1627311721,2.99394660677));
#68815=CARTESIAN_POINT('Ctrl Pts',(10.3257952972,-38.0684833924,3.01322820232));
#68816=CARTESIAN_POINT('Ctrl Pts',(10.3257952972,-37.9742356128,3.01322820232));
#68817=CARTESIAN_POINT('Ctrl Pts',(9.96239262302,-38.2742356128,3.03279125873));
#68818=CARTESIAN_POINT('Ctrl Pts',(10.0411275292,-38.2742356128,3.08469759446));
#68819=CARTESIAN_POINT('Ctrl Pts',(10.1198624354,-38.2372245963,3.13660393018));
#68820=CARTESIAN_POINT('Ctrl Pts',(10.1820945837,-38.1627311721,3.17763052871));
#68821=CARTESIAN_POINT('Ctrl Pts',(10.2130136133,-38.0684833924,3.19801425689));
#68822=CARTESIAN_POINT('Ctrl Pts',(10.2130136133,-37.9742356128,3.19801425689));
#68823=CARTESIAN_POINT('Ctrl Pts',(9.84476270741,-38.2742356128,3.20806595154));
#68824=CARTESIAN_POINT('Ctrl Pts',(9.92144376871,-38.2742356128,3.26308291366));
#68825=CARTESIAN_POINT('Ctrl Pts',(9.99812483001,-38.2372245963,3.31809987579));
#68826=CARTESIAN_POINT('Ctrl Pts',(10.0587333807,-38.1627311721,3.36158550664));
#68827=CARTESIAN_POINT('Ctrl Pts',(10.0888461064,-38.0684833924,3.38319038106));
#68828=CARTESIAN_POINT('Ctrl Pts',(10.0888461064,-37.9742356128,3.38319038106));
#68829=CARTESIAN_POINT('Ctrl Pts',(9.71703247101,-38.2742356128,3.37827910506));
#68830=CARTESIAN_POINT('Ctrl Pts',(9.79053204643,-38.2742356128,3.43778793927));
#68831=CARTESIAN_POINT('Ctrl Pts',(9.86403162186,-38.2372245963,3.49729677347));
#68832=CARTESIAN_POINT('Ctrl Pts',(9.92212570714,-38.1627311721,3.54433248183));
#68833=CARTESIAN_POINT('Ctrl Pts',(9.9509888859,-38.0684833924,3.56770160749));
#68834=CARTESIAN_POINT('Ctrl Pts',(9.9509888859,-37.9742356128,3.56770160749));
#68835=CARTESIAN_POINT('Ctrl Pts',(9.4465153344,-38.2742356128,3.67954908967));
#68836=CARTESIAN_POINT('Ctrl Pts',(9.51165483329,-38.2742356128,3.74868285322));
#68837=CARTESIAN_POINT('Ctrl Pts',(9.57679433219,-38.2372245963,3.81781661678));
#68838=CARTESIAN_POINT('Ctrl Pts',(9.62828054625,-38.1627311721,3.87245998019));
#68839=CARTESIAN_POINT('Ctrl Pts',(9.65386079919,-38.0684833924,3.89960869375));
#68840=CARTESIAN_POINT('Ctrl Pts',(9.65386079919,-37.9742356128,3.89960869375));
#68841=CARTESIAN_POINT('Ctrl Pts',(9.11961907684,-38.2742356128,3.92493521278));
#68842=CARTESIAN_POINT('Ctrl Pts',(9.17143121953,-38.2742356128,4.00428974878));
#68843=CARTESIAN_POINT('Ctrl Pts',(9.22324336223,-38.2372245963,4.08364428479));
#68844=CARTESIAN_POINT('Ctrl Pts',(9.26419569527,-38.1627311721,4.14636604856));
#68845=CARTESIAN_POINT('Ctrl Pts',(9.28454224928,-38.0684833924,4.17752854602));
#68846=CARTESIAN_POINT('Ctrl Pts',(9.28454224928,-37.9742356128,4.17752854602));
#68847=CARTESIAN_POINT('Ctrl Pts',(8.95439425436,-38.2742356128,4.02292606705));
#68848=CARTESIAN_POINT('Ctrl Pts',(8.99905838483,-38.2742356128,4.10659587218));
#68849=CARTESIAN_POINT('Ctrl Pts',(9.04372251529,-38.2372245963,4.19026567732));
#68850=CARTESIAN_POINT('Ctrl Pts',(9.07902498138,-38.1627311721,4.25639823777));
#68851=CARTESIAN_POINT('Ctrl Pts',(9.09656459722,-38.0684833924,4.28925532855));
#68852=CARTESIAN_POINT('Ctrl Pts',(9.09656459722,-37.9742356128,4.28925532855));
#68853=CARTESIAN_POINT('Ctrl Pts',(8.43375423048,-38.2742356128,4.25670358831));
#68854=CARTESIAN_POINT('Ctrl Pts',(8.45474053418,-38.2742356128,4.35103499499));
#68855=CARTESIAN_POINT('Ctrl Pts',(8.47572683789,-38.2372245963,4.44536640166));
#68856=CARTESIAN_POINT('Ctrl Pts',(8.49231451374,-38.1627311721,4.51992599457));
#68857=CARTESIAN_POINT('Ctrl Pts',(8.50055570992,-38.0684833924,4.55696978154));
#68858=CARTESIAN_POINT('Ctrl Pts',(8.50055570992,-37.9742356128,4.55696978154));
#68859=CARTESIAN_POINT('Ctrl Pts',(7.85070473056,-38.2742356128,4.30204442107));
#68860=CARTESIAN_POINT('Ctrl Pts',(7.84356701002,-38.2742356128,4.39888585549));
#68861=CARTESIAN_POINT('Ctrl Pts',(7.83642928948,-38.2372245963,4.49572728991));
#68862=CARTESIAN_POINT('Ctrl Pts',(7.83078742393,-38.1627311721,4.57227059967));
#68863=CARTESIAN_POINT('Ctrl Pts',(7.82798466043,-38.0684833924,4.61030028076));
#68864=CARTESIAN_POINT('Ctrl Pts',(7.82798466043,-37.9742356128,4.61030028076));
#68865=CARTESIAN_POINT('Ctrl Pts',(7.46124971174,-38.2742356128,4.23337366135));
#68866=CARTESIAN_POINT('Ctrl Pts',(7.43569930686,-38.2742356128,4.32644610908));
#68867=CARTESIAN_POINT('Ctrl Pts',(7.41014890199,-38.2372245963,4.41951855682));
#68868=CARTESIAN_POINT('Ctrl Pts',(7.38995471066,-38.1627311721,4.49308356189));
#68869=CARTESIAN_POINT('Ctrl Pts',(7.37992024706,-38.0684833924,4.5296324638));
#68870=CARTESIAN_POINT('Ctrl Pts',(7.37992024706,-37.9742356128,4.5296324638));
#68871=CARTESIAN_POINT('Ctrl Pts',(7.10590026383,-38.2742356128,4.0818123451));
#68872=CARTESIAN_POINT('Ctrl Pts',(7.06551175748,-38.2742356128,4.1681709574));
#68873=CARTESIAN_POINT('Ctrl Pts',(7.02512325114,-38.2372245963,4.25452956969));
#68874=CARTESIAN_POINT('Ctrl Pts',(6.99319962237,-38.1627311721,4.32278702275));
#68875=CARTESIAN_POINT('Ctrl Pts',(6.97733965525,-38.0684833924,4.35670034561));
#68876=CARTESIAN_POINT('Ctrl Pts',(6.97733965525,-37.9742356128,4.35670034561));
#68877=CARTESIAN_POINT('Ctrl Pts',(6.79137823178,-38.2742356128,3.87179984728));
#68878=CARTESIAN_POINT('Ctrl Pts',(6.7390418526,-38.2742356128,3.95018063176));
#68879=CARTESIAN_POINT('Ctrl Pts',(6.68670547342,-38.2372245963,4.02856141623));
#68880=CARTESIAN_POINT('Ctrl Pts',(6.64533881083,-38.1627311721,4.09051357105));
#68881=CARTESIAN_POINT('Ctrl Pts',(6.62478636278,-38.0684833924,4.12129363314));
#68882=CARTESIAN_POINT('Ctrl Pts',(6.62478636278,-37.9742356128,4.12129363314));
#68883=CARTESIAN_POINT('',(6.62478636196,-37.9742356128,4.121293631845));
#68884=CARTESIAN_POINT('Origin',(6.79019999558982,-37.9763569532443,3.87356390622112));
#68885=CARTESIAN_POINT('',(10.3257952821,-37.9742356128,3.01322822759));
#68886=CARTESIAN_POINT('Origin',(10.0715333086021,-37.9763569039709,2.85804261568983));
#68887=CARTESIAN_POINT('Ctrl Pts',(6.62478636278,-37.9742356128,4.12129363314));
#68888=CARTESIAN_POINT('Ctrl Pts',(6.77209862642,-37.9742356128,4.21965690596));
#68889=CARTESIAN_POINT('Ctrl Pts',(6.92865784201,-37.9742356128,4.30723684413));
#68890=CARTESIAN_POINT('Ctrl Pts',(7.09318322917,-37.9742356128,4.3815910145));
#68891=CARTESIAN_POINT('Ctrl Pts',(7.35028595871,-37.9742356128,4.47075138071));
#68892=CARTESIAN_POINT('Ctrl Pts',(7.61904353259,-37.9742356128,4.52294971153));
#68893=CARTESIAN_POINT('Ctrl Pts',(7.71036083894,-37.9742356128,4.53610818987));
#68894=CARTESIAN_POINT('Ctrl Pts',(7.98526439172,-37.9742356128,4.56199873534));
#68895=CARTESIAN_POINT('Ctrl Pts',(8.26232955523,-37.9742356128,4.54692356056));
#68896=CARTESIAN_POINT('Ctrl Pts',(8.44551261186,-37.9742356128,4.51817058272));
#68897=CARTESIAN_POINT('Ctrl Pts',(8.80081499429,-37.9742356128,4.42491856124));
#68898=CARTESIAN_POINT('Ctrl Pts',(9.12906626269,-37.9742356128,4.26637622783));
#68899=CARTESIAN_POINT('Ctrl Pts',(9.28446203337,-37.9742356128,4.17257256592));
#68900=CARTESIAN_POINT('Ctrl Pts',(9.50104385578,-37.9742356128,4.01328807602));
#68901=CARTESIAN_POINT('Ctrl Pts',(9.69216005671,-37.9742356128,3.83525523444));
#68902=CARTESIAN_POINT('Ctrl Pts',(9.75297759191,-37.9742356128,3.77433260224));
#68903=CARTESIAN_POINT('Ctrl Pts',(9.92328269257,-37.9742356128,3.5920488793));
#68904=CARTESIAN_POINT('Ctrl Pts',(10.0727130885,-37.9742356128,3.39989142333));
#68905=CARTESIAN_POINT('Ctrl Pts',(10.163703376,-37.9742356128,3.27006200044));
#68906=CARTESIAN_POINT('Ctrl Pts',(10.24741676,-37.9742356128,3.14164655991));
#68907=CARTESIAN_POINT('Ctrl Pts',(10.3257952821,-37.9742356128,3.01322822759));
#68908=CARTESIAN_POINT('Ctrl Pts',(10.3257952821,-37.9742356128,3.01322822759));
#68909=CARTESIAN_POINT('Ctrl Pts',(10.3257952821,-36.2942356128,3.01322822759));
#68910=CARTESIAN_POINT('Ctrl Pts',(10.24741676,-37.9742356128,3.14164655991));
#68911=CARTESIAN_POINT('Ctrl Pts',(10.24741676,-36.2942356128,3.14164655991));
#68912=CARTESIAN_POINT('Ctrl Pts',(10.163703376,-37.9742356128,3.27006200044));
#68913=CARTESIAN_POINT('Ctrl Pts',(10.163703376,-36.2942356128,3.27006200044));
#68914=CARTESIAN_POINT('Ctrl Pts',(10.0727130885,-37.9742356128,3.39989142333));
#68915=CARTESIAN_POINT('Ctrl Pts',(10.0727130885,-36.2942356128,3.39989142333));
#68916=CARTESIAN_POINT('Ctrl Pts',(9.92328269257,-37.9742356128,3.5920488793));
#68917=CARTESIAN_POINT('Ctrl Pts',(9.92328269257,-36.2942356128,3.5920488793));
#68918=CARTESIAN_POINT('Ctrl Pts',(9.75297759191,-37.9742356128,3.77433260224));
#68919=CARTESIAN_POINT('Ctrl Pts',(9.75297759191,-36.2942356128,3.77433260224));
#68920=CARTESIAN_POINT('Ctrl Pts',(9.69216005671,-37.9742356128,3.83525523444));
#68921=CARTESIAN_POINT('Ctrl Pts',(9.69216005671,-36.2942356128,3.83525523444));
#68922=CARTESIAN_POINT('Ctrl Pts',(9.50104385578,-37.9742356128,4.01328807602));
#68923=CARTESIAN_POINT('Ctrl Pts',(9.50104385578,-36.2942356128,4.01328807602));
#68924=CARTESIAN_POINT('Ctrl Pts',(9.28446203337,-37.9742356128,4.17257256592));
#68925=CARTESIAN_POINT('Ctrl Pts',(9.28446203337,-36.2942356128,4.17257256592));
#68926=CARTESIAN_POINT('Ctrl Pts',(9.12906626269,-37.9742356128,4.26637622783));
#68927=CARTESIAN_POINT('Ctrl Pts',(9.12906626269,-36.2942356128,4.26637622783));
#68928=CARTESIAN_POINT('Ctrl Pts',(8.80081499429,-37.9742356128,4.42491856124));
#68929=CARTESIAN_POINT('Ctrl Pts',(8.80081499429,-36.2942356128,4.42491856124));
#68930=CARTESIAN_POINT('Ctrl Pts',(8.44551261186,-37.9742356128,4.51817058272));
#68931=CARTESIAN_POINT('Ctrl Pts',(8.44551261186,-36.2942356128,4.51817058272));
#68932=CARTESIAN_POINT('Ctrl Pts',(8.26232955523,-37.9742356128,4.54692356056));
#68933=CARTESIAN_POINT('Ctrl Pts',(8.26232955523,-36.2942356128,4.54692356056));
#68934=CARTESIAN_POINT('Ctrl Pts',(7.98526439172,-37.9742356128,4.56199873534));
#68935=CARTESIAN_POINT('Ctrl Pts',(7.98526439172,-36.2942356128,4.56199873534));
#68936=CARTESIAN_POINT('Ctrl Pts',(7.71036083894,-37.9742356128,4.53610818987));
#68937=CARTESIAN_POINT('Ctrl Pts',(7.71036083894,-36.2942356128,4.53610818987));
#68938=CARTESIAN_POINT('Ctrl Pts',(7.61904353259,-37.9742356128,4.52294971153));
#68939=CARTESIAN_POINT('Ctrl Pts',(7.61904353259,-36.2942356128,4.52294971153));
#68940=CARTESIAN_POINT('Ctrl Pts',(7.35028595871,-37.9742356128,4.47075138071));
#68941=CARTESIAN_POINT('Ctrl Pts',(7.35028595871,-36.2942356128,4.47075138071));
#68942=CARTESIAN_POINT('Ctrl Pts',(7.09318322917,-37.9742356128,4.3815910145));
#68943=CARTESIAN_POINT('Ctrl Pts',(7.09318322917,-36.2942356128,4.3815910145));
#68944=CARTESIAN_POINT('Ctrl Pts',(6.92865784201,-37.9742356128,4.30723684413));
#68945=CARTESIAN_POINT('Ctrl Pts',(6.92865784201,-36.2942356128,4.30723684413));
#68946=CARTESIAN_POINT('Ctrl Pts',(6.77209862642,-37.9742356128,4.21965690596));
#68947=CARTESIAN_POINT('Ctrl Pts',(6.77209862642,-36.2942356128,4.21965690596));
#68948=CARTESIAN_POINT('Ctrl Pts',(6.62478636278,-37.9742356128,4.12129363314));
#68949=CARTESIAN_POINT('Ctrl Pts',(6.62478636278,-36.2942356128,4.12129363314));
#68950=CARTESIAN_POINT('',(10.3257952821,-37.2742356128,3.01322822759));
#68951=CARTESIAN_POINT('',(6.62478636278,-37.2742356128,4.12129363314));
#68952=CARTESIAN_POINT('Ctrl Pts',(6.16208308783,-36.5742356128,4.4189333977));
#68953=CARTESIAN_POINT('Ctrl Pts',(6.16208308783,-36.4799878332,4.4189333977));
#68954=CARTESIAN_POINT('Ctrl Pts',(6.12555180739,-36.3857400536,4.42487316974));
#68955=CARTESIAN_POINT('Ctrl Pts',(6.0520239654,-36.3112466293,4.4368283658));
#68956=CARTESIAN_POINT('Ctrl Pts',(5.95899782364,-36.2742356128,4.45195387109));
#68957=CARTESIAN_POINT('Ctrl Pts',(5.86597168188,-36.2742356128,4.46707937639));
#68958=CARTESIAN_POINT('Ctrl Pts',(6.15238298742,-36.5742356128,4.35927503269));
#68959=CARTESIAN_POINT('Ctrl Pts',(6.15238298742,-36.4799878332,4.35927503269));
#68960=CARTESIAN_POINT('Ctrl Pts',(6.11466577784,-36.3857400536,4.35792099922));
#68961=CARTESIAN_POINT('Ctrl Pts',(6.03875096538,-36.3112466293,4.35519565622));
#68962=CARTESIAN_POINT('Ctrl Pts',(5.94270487345,-36.2742356128,4.35174761258));
#68963=CARTESIAN_POINT('Ctrl Pts',(5.84665878152,-36.2742356128,4.34829956896));
#68964=CARTESIAN_POINT('Ctrl Pts',(6.15762307668,-36.5742356128,4.29742569118));
#68965=CARTESIAN_POINT('Ctrl Pts',(6.15762309009,-36.4799878341,4.29742572463));
#68966=CARTESIAN_POINT('Ctrl Pts',(6.12052271305,-36.3857400553,4.28842649608));
#68967=CARTESIAN_POINT('Ctrl Pts',(6.04584940666,-36.3112466313,4.27031343988));
#68968=CARTESIAN_POINT('Ctrl Pts',(5.95137403766,-36.2742356142,4.24739707171));
#68969=CARTESIAN_POINT('Ctrl Pts',(5.85689866288,-36.2742356128,4.22448069029));
#68970=CARTESIAN_POINT('Ctrl Pts',(6.1785485954,-36.5742356128,4.23847486966));
#68971=CARTESIAN_POINT('Ctrl Pts',(6.17854857015,-36.4799878332,4.23847488615));
#68972=CARTESIAN_POINT('Ctrl Pts',(6.14407261188,-36.3857400535,4.22209265639));
#68973=CARTESIAN_POINT('Ctrl Pts',(6.07468029561,-36.3112466293,4.1891186584));
#68974=CARTESIAN_POINT('Ctrl Pts',(5.98688692179,-36.2742356128,4.14740088542));
#68975=CARTESIAN_POINT('Ctrl Pts',(5.89909355815,-36.2742356128,4.10568310582));
#68976=CARTESIAN_POINT('Ctrl Pts',(6.25923171959,-36.5742356128,4.11978495173));
#68977=CARTESIAN_POINT('Ctrl Pts',(6.25923175272,-36.4799878333,4.11978493009));
#68978=CARTESIAN_POINT('Ctrl Pts',(6.23474842569,-36.3857400538,4.08878629998));
#68979=CARTESIAN_POINT('Ctrl Pts',(6.1854715852,-36.3112466295,4.02639543407));
#68980=CARTESIAN_POINT('Ctrl Pts',(6.12312665839,-36.2742356129,3.94745911673));
#68981=CARTESIAN_POINT('Ctrl Pts',(6.06078171822,-36.2742356128,3.86852280807));
#68982=CARTESIAN_POINT('Ctrl Pts',(6.39414337331,-36.5742356128,4.06099492613));
#68983=CARTESIAN_POINT('Ctrl Pts',(6.39414332985,-36.4799878331,4.06099495453));
#68984=CARTESIAN_POINT('Ctrl Pts',(6.38612870308,-36.3857400534,4.02281971522));
#68985=CARTESIAN_POINT('Ctrl Pts',(6.369995284,-36.3112466292,3.9459813705));
#68986=CARTESIAN_POINT('Ctrl Pts',(6.34958448959,-36.2742356127,3.84876749811));
#68987=CARTESIAN_POINT('Ctrl Pts',(6.32917371276,-36.2742356128,3.75155361429));
#68988=CARTESIAN_POINT('Ctrl Pts',(6.47897493351,-36.5742356128,4.05513069729));
#68989=CARTESIAN_POINT('Ctrl Pts',(6.47897491719,-36.4799878312,4.05513067751));
#68990=CARTESIAN_POINT('Ctrl Pts',(6.48151319419,-36.3857400495,4.01612595006));
#68991=CARTESIAN_POINT('Ctrl Pts',(6.48663098039,-36.3112466242,3.93762581777));
#68992=CARTESIAN_POINT('Ctrl Pts',(6.49310219221,-36.2742356096,3.83830627934));
#68993=CARTESIAN_POINT('Ctrl Pts',(6.49957341023,-36.2742356128,3.73898674982));
#68994=CARTESIAN_POINT('Ctrl Pts',(6.55876184042,-36.5742356128,4.07720779466));
#68995=CARTESIAN_POINT('Ctrl Pts',(6.55876183658,-36.4799878345,4.07720779208));
#68996=CARTESIAN_POINT('Ctrl Pts',(6.57126454019,-36.3857400562,4.04105280425));
#68997=CARTESIAN_POINT('Ctrl Pts',(6.59642328625,-36.3112466325,3.96827827511));
#68998=CARTESIAN_POINT('Ctrl Pts',(6.62825617609,-36.2742356148,3.87620692129));
#68999=CARTESIAN_POINT('Ctrl Pts',(6.66008906758,-36.2742356128,3.78413556779));
#69000=CARTESIAN_POINT('Ctrl Pts',(6.62478636073,-36.5742356128,4.12129362984));
#69001=CARTESIAN_POINT('Ctrl Pts',(6.62478636078,-36.4799878332,4.12129362988));
#69002=CARTESIAN_POINT('Ctrl Pts',(6.64533878987,-36.3857400535,4.09051355751));
#69003=CARTESIAN_POINT('Ctrl Pts',(6.68670541424,-36.3112466292,4.02856138193));
#69004=CARTESIAN_POINT('Ctrl Pts',(6.73904174502,-36.2742356128,3.95018057117));
#69005=CARTESIAN_POINT('Ctrl Pts',(6.79137807575,-36.2742356128,3.87179976043));
#69006=CARTESIAN_POINT('',(6.16208308816031,-36.5742356128,4.41893339764629));
#69007=CARTESIAN_POINT('Origin',(5.8680654705604,-36.5721143212264,4.46673889588175));
#69008=CARTESIAN_POINT('Ctrl Pts',(6.16208308783,-36.5742356128,4.4189333977));
#69009=CARTESIAN_POINT('Ctrl Pts',(6.13973650651,-36.5742356128,4.28149559307));
#69010=CARTESIAN_POINT('Ctrl Pts',(6.19622108576,-36.5742356128,4.13004365321));
#69011=CARTESIAN_POINT('Ctrl Pts',(6.34774592774,-36.5742356128,4.03257337207));
#69012=CARTESIAN_POINT('Ctrl Pts',(6.50898576372,-36.5742356128,4.04397131362));
#69013=CARTESIAN_POINT('Ctrl Pts',(6.62478636278,-36.5742356128,4.12129363314));
#69014=CARTESIAN_POINT('Ctrl Pts',(6.79137807329,-38.2742356128,3.87179977251));
#69015=CARTESIAN_POINT('Ctrl Pts',(6.73904174287,-38.2742356128,3.95018057885));
#69016=CARTESIAN_POINT('Ctrl Pts',(6.68670541245,-38.2372245963,4.02856138519));
#69017=CARTESIAN_POINT('Ctrl Pts',(6.6453387884,-38.1627311721,4.09051355729));
#69018=CARTESIAN_POINT('Ctrl Pts',(6.6247863595,-38.0684833924,4.12129362796));
#69019=CARTESIAN_POINT('Ctrl Pts',(6.6247863595,-37.9742356128,4.12129362796));
#69020=CARTESIAN_POINT('Ctrl Pts',(6.67468686061,-38.2742356128,3.79388274471));
#69021=CARTESIAN_POINT('Ctrl Pts',(6.64057040577,-38.2742356128,3.88442933328));
#69022=CARTESIAN_POINT('Ctrl Pts',(6.60645395093,-38.2372245963,3.97497592186));
#69023=CARTESIAN_POINT('Ctrl Pts',(6.57948981739,-38.1627311721,4.04654496794));
#69024=CARTESIAN_POINT('Ctrl Pts',(6.56609081204,-38.0684833924,4.08210148774));
#69025=CARTESIAN_POINT('Ctrl Pts',(6.56609081204,-37.9742356128,4.08210148774));
#69026=CARTESIAN_POINT('Ctrl Pts',(6.53492809075,-38.2742356128,3.7495789243));
#69027=CARTESIAN_POINT('Ctrl Pts',(6.52286609392,-38.2742356128,3.84720752091));
#69028=CARTESIAN_POINT('Ctrl Pts',(6.51080409709,-38.2372245963,3.94483611753));
#69029=CARTESIAN_POINT('Ctrl Pts',(6.50126803274,-38.1627311721,4.0220001801));
#69030=CARTESIAN_POINT('Ctrl Pts',(6.49653356236,-38.0684833924,4.06034039907));
#69031=CARTESIAN_POINT('Ctrl Pts',(6.49653356236,-37.9742356128,4.06034039907));
#69032=CARTESIAN_POINT('Ctrl Pts',(6.38553386058,-38.2742356128,3.74945814774));
#69033=CARTESIAN_POINT('Ctrl Pts',(6.39707418027,-38.2742356128,3.84703544696));
#69034=CARTESIAN_POINT('Ctrl Pts',(6.40861449997,-38.2372245963,3.94461274618));
#69035=CARTESIAN_POINT('Ctrl Pts',(6.41773671293,-38.1627311721,4.02173930641));
#69036=CARTESIAN_POINT('Ctrl Pts',(6.42226783906,-38.0684833924,4.06005633783));
#69037=CARTESIAN_POINT('Ctrl Pts',(6.42226783906,-37.9742356128,4.06005633783));
#69038=CARTESIAN_POINT('Ctrl Pts',(6.10848563002,-38.2742356128,3.83467286799));
#69039=CARTESIAN_POINT('Ctrl Pts',(6.16340332634,-38.2742356128,3.91886622309));
#69040=CARTESIAN_POINT('Ctrl Pts',(6.21832102267,-38.2372245963,4.00305957819));
#69041=CARTESIAN_POINT('Ctrl Pts',(6.26172720453,-38.1627311721,4.06960454208));
#69042=CARTESIAN_POINT('Ctrl Pts',(6.28329408668,-38.0684833924,4.10266864079));
#69043=CARTESIAN_POINT('Ctrl Pts',(6.28329408668,-37.9742356128,4.10266864079));
#69044=CARTESIAN_POINT('Ctrl Pts',(5.91969829593,-38.2742356128,4.0541842541));
#69045=CARTESIAN_POINT('Ctrl Pts',(6.00421162703,-38.2742356128,4.10402542076));
#69046=CARTESIAN_POINT('Ctrl Pts',(6.08872495813,-38.2372245963,4.15386658741));
#69047=CARTESIAN_POINT('Ctrl Pts',(6.15552503566,-38.1627311721,4.19326244205));
#69048=CARTESIAN_POINT('Ctrl Pts',(6.18871258397,-38.0684833924,4.21283361496));
#69049=CARTESIAN_POINT('Ctrl Pts',(6.18871258397,-37.9742356128,4.21283361496));
#69050=CARTESIAN_POINT('Ctrl Pts',(5.86049982571,-38.2742356128,4.18805332395));
#69051=CARTESIAN_POINT('Ctrl Pts',(5.95442429429,-38.2742356128,4.21671667916));
#69052=CARTESIAN_POINT('Ctrl Pts',(6.04834876288,-38.2372245963,4.24538003438));
#69053=CARTESIAN_POINT('Ctrl Pts',(6.12258586761,-38.1627311721,4.26803136845));
#69054=CARTESIAN_POINT('Ctrl Pts',(6.15947069476,-38.0684833924,4.27929161731));
#69055=CARTESIAN_POINT('Ctrl Pts',(6.15947069476,-37.9742356128,4.27929161731));
#69056=CARTESIAN_POINT('Ctrl Pts',(5.84384347146,-38.2742356128,4.33098461465));
#69057=CARTESIAN_POINT('Ctrl Pts',(5.94032979225,-38.2742356128,4.33714019046));
#69058=CARTESIAN_POINT('Ctrl Pts',(6.03681611303,-38.2372245963,4.34329576626));
#69059=CARTESIAN_POINT('Ctrl Pts',(6.11307940101,-38.1627311721,4.34816391257));
#69060=CARTESIAN_POINT('Ctrl Pts',(6.15096896934,-38.0684833924,4.35057842098));
#69061=CARTESIAN_POINT('Ctrl Pts',(6.15096896934,-37.9742356128,4.35057842098));
#69062=CARTESIAN_POINT('Ctrl Pts',(5.86597168188,-38.2742356128,4.46707937639));
#69063=CARTESIAN_POINT('Ctrl Pts',(5.95899782364,-38.2742356128,4.45195387109));
#69064=CARTESIAN_POINT('Ctrl Pts',(6.0520239654,-38.2372245963,4.4368283658));
#69065=CARTESIAN_POINT('Ctrl Pts',(6.12555180739,-38.1627311721,4.42487316974));
#69066=CARTESIAN_POINT('Ctrl Pts',(6.16208308783,-38.0684833924,4.4189333977));
#69067=CARTESIAN_POINT('Ctrl Pts',(6.16208308783,-37.9742356128,4.4189333977));
#69068=CARTESIAN_POINT('',(6.16208308783,-37.9742356128,4.4189333977));
#69069=CARTESIAN_POINT('Origin',(5.86806547685312,-37.9763569039045,4.46673893760219));
#69070=CARTESIAN_POINT('Ctrl Pts',(6.16208308783,-37.9742356128,4.4189333977));
#69071=CARTESIAN_POINT('Ctrl Pts',(6.15919261847849,-37.9742356128,4.40115619248035));
#69072=CARTESIAN_POINT('Ctrl Pts',(6.1578958682542,-37.9742356128,4.38312498437982));
#69073=CARTESIAN_POINT('Ctrl Pts',(6.15821910283257,-37.9742356128,4.365132913013));
#69074=CARTESIAN_POINT('Ctrl Pts',(6.15854192725494,-37.9742356128,4.34716367198903));
#69075=CARTESIAN_POINT('Ctrl Pts',(6.16048059072391,-37.9742356128,4.32923373168325));
#69076=CARTESIAN_POINT('Ctrl Pts',(6.16401008069579,-37.9742356128,4.31162615872299));
#69077=CARTESIAN_POINT('Ctrl Pts',(6.16753519147487,-37.9742356128,4.29404043224978));
#69078=CARTESIAN_POINT('Ctrl Pts',(6.17264712597345,-37.9742356128,4.2767765339022));
#69079=CARTESIAN_POINT('Ctrl Pts',(6.17927059085163,-37.9742356128,4.2601036138989));
#69080=CARTESIAN_POINT('Ctrl Pts',(6.185882474244,-37.9742356128,4.24345984739608));
#69081=CARTESIAN_POINT('Ctrl Pts',(6.19400052518591,-37.9742356128,4.22740524746908));
#69082=CARTESIAN_POINT('Ctrl Pts',(6.20350066431033,-37.9742356128,4.21219088469382));
#69083=CARTESIAN_POINT('Ctrl Pts',(6.212990313481,-37.9742356128,4.196993321458));
#69084=CARTESIAN_POINT('Ctrl Pts',(6.22385890537373,-37.9742356128,4.18263438843155));
#69085=CARTESIAN_POINT('Ctrl Pts',(6.2359349706977,-37.9742356128,4.16934392349151));
#69086=CARTESIAN_POINT('Ctrl Pts',(6.24799262158315,-37.9742356128,4.1560737247924));
#69087=CARTESIAN_POINT('Ctrl Pts',(6.2612539503332,-37.9742356128,4.14386897449315));
#69088=CARTESIAN_POINT('Ctrl Pts',(6.27550217470401,-37.9742356128,4.13293448634083));
#69089=CARTESIAN_POINT('Ctrl Pts',(6.28129678738945,-37.9742356128,4.12848753757673));
#69090=CARTESIAN_POINT('Ctrl Pts',(6.2872541085728,-37.9742356128,4.12425039027964));
#69091=CARTESIAN_POINT('Ctrl Pts',(6.29335744170626,-37.9742356128,4.12023554862129));
#69092=CARTESIAN_POINT('Ctrl Pts',(6.30811707445383,-37.9742356128,4.11052649504004));
#69093=CARTESIAN_POINT('Ctrl Pts',(6.32373132640604,-37.9742356128,4.1021214113779));
#69094=CARTESIAN_POINT('Ctrl Pts',(6.33994605204457,-37.9742356128,4.09515243205252));
#69095=CARTESIAN_POINT('Ctrl Pts',(6.35637472997303,-37.9742356128,4.08809149748113));
#69096=CARTESIAN_POINT('Ctrl Pts',(6.3734193219789,-37.9742356128,4.08250481550582));
#69097=CARTESIAN_POINT('Ctrl Pts',(6.39080390205361,-37.9742356128,4.07847709763709));
#69098=CARTESIAN_POINT('Ctrl Pts',(6.40837174310293,-37.9742356128,4.07440692125058));
#69099=CARTESIAN_POINT('Ctrl Pts',(6.42628621839665,-37.9742356128,4.07192870130141));
#69100=CARTESIAN_POINT('Ctrl Pts',(6.44425897825834,-37.9742356128,4.07107677316466));
#69101=CARTESIAN_POINT('Ctrl Pts',(6.46238597578069,-37.9742356128,4.070217533997));
#69102=CARTESIAN_POINT('Ctrl Pts',(6.48057166961878,-37.9742356128,4.07101252700654));
#69103=CARTESIAN_POINT('Ctrl Pts',(6.49852532361879,-37.9742356128,4.0734443564819));
#69104=CARTESIAN_POINT('Ctrl Pts',(6.51648139915476,-37.9742356128,4.07587651395527));
#69105=CARTESIAN_POINT('Ctrl Pts',(6.53420479100214,-37.9742356128,4.07994576358515));
#69106=CARTESIAN_POINT('Ctrl Pts',(6.55141856220953,-37.9742356128,4.08558449609217));
#69107=CARTESIAN_POINT('Ctrl Pts',(6.56853351254586,-37.9742356128,4.09119085774616));
#69108=CARTESIAN_POINT('Ctrl Pts',(6.58514414635111,-37.9742356128,4.09834849003559));
#69109=CARTESIAN_POINT('Ctrl Pts',(6.60100030737395,-37.9742356128,4.10694459823105));
#69110=CARTESIAN_POINT('Ctrl Pts',(6.60913757342369,-37.9742356128,4.11135605818519));
#69111=CARTESIAN_POINT('Ctrl Pts',(6.61707654315828,-37.9742356128,4.11614563605583));
#69112=CARTESIAN_POINT('Ctrl Pts',(6.6247863595,-37.9742356128,4.12129362796));
#69113=CARTESIAN_POINT('Ctrl Pts',(6.62478636278,-37.9742356128,4.12129363314));
#69114=CARTESIAN_POINT('Ctrl Pts',(6.62478636278,-36.2942356128,4.12129363314));
#69115=CARTESIAN_POINT('Ctrl Pts',(6.50898576372,-37.9742356128,4.04397131362));
#69116=CARTESIAN_POINT('Ctrl Pts',(6.50898576372,-36.2942356128,4.04397131362));
#69117=CARTESIAN_POINT('Ctrl Pts',(6.34774592774,-37.9742356128,4.03257337207));
#69118=CARTESIAN_POINT('Ctrl Pts',(6.34774592774,-36.2942356128,4.03257337207));
#69119=CARTESIAN_POINT('Ctrl Pts',(6.19622108576,-37.9742356128,4.13004365321));
#69120=CARTESIAN_POINT('Ctrl Pts',(6.19622108576,-36.2942356128,4.13004365321));
#69121=CARTESIAN_POINT('Ctrl Pts',(6.13973650651,-37.9742356128,4.28149559307));
#69122=CARTESIAN_POINT('Ctrl Pts',(6.13973650651,-36.2942356128,4.28149559307));
#69123=CARTESIAN_POINT('Ctrl Pts',(6.16208308783,-37.9742356128,4.4189333977));
#69124=CARTESIAN_POINT('Ctrl Pts',(6.16208308783,-36.2942356128,4.4189333977));
#69125=CARTESIAN_POINT('',(6.16208308783,-37.2742356128,4.4189333977));
#69126=CARTESIAN_POINT('Ctrl Pts',(-4.4408920985E-16,-36.5742356128,11.6643459897));
#69127=CARTESIAN_POINT('Ctrl Pts',(0.,-36.4799878332,11.6643459897));
#69128=CARTESIAN_POINT('Ctrl Pts',(-2.4666821874E-6,-36.3857400536,11.6273349733));
#69129=CARTESIAN_POINT('Ctrl Pts',(-7.43146349125E-6,-36.3112466293,11.5528415491));
#69130=CARTESIAN_POINT('Ctrl Pts',(-1.37128181037E-5,-36.2742356128,11.4585937697));
#69131=CARTESIAN_POINT('Ctrl Pts',(-1.99941727144E-5,-36.2742356128,11.3643459904));
#69132=CARTESIAN_POINT('Ctrl Pts',(1.22322324235,-36.5742356128,11.6642644652));
#69133=CARTESIAN_POINT('Ctrl Pts',(1.22322324235,-36.4799878332,11.6642644652));
#69134=CARTESIAN_POINT('Ctrl Pts',(1.21599829202,-36.3857400536,11.6272539302));
#69135=CARTESIAN_POINT('Ctrl Pts',(1.20145637047,-36.3112466293,11.5527614749));
#69136=CARTESIAN_POINT('Ctrl Pts',(1.18305818534,-36.2742356128,11.4585149213));
#69137=CARTESIAN_POINT('Ctrl Pts',(1.16466000022,-36.2742356128,11.3642683676));
#69138=CARTESIAN_POINT('Ctrl Pts',(2.4473136708,-36.5742356128,11.3659246093));
#69139=CARTESIAN_POINT('Ctrl Pts',(2.44731353996,-36.4799878304,11.3659245634));
#69140=CARTESIAN_POINT('Ctrl Pts',(2.43279023211,-36.385740048,11.3306770417));
#69141=CARTESIAN_POINT('Ctrl Pts',(2.40355880045,-36.3112466227,11.2597331237));
#69142=CARTESIAN_POINT('Ctrl Pts',(2.36657578312,-36.2742356084,11.1699761465));
#69143=CARTESIAN_POINT('Ctrl Pts',(2.32959281761,-36.2742356128,11.080219189));
#69144=CARTESIAN_POINT('Ctrl Pts',(3.57166410201,-36.5742356128,10.7642929822));
#69145=CARTESIAN_POINT('Ctrl Pts',(3.57166393324,-36.4799878332,10.7642932734));
#69146=CARTESIAN_POINT('Ctrl Pts',(3.55046878885,-36.3857400536,10.7326400178));
#69147=CARTESIAN_POINT('Ctrl Pts',(3.50780873346,-36.3112466293,10.6689298739));
#69148=CARTESIAN_POINT('Ctrl Pts',(3.45383608788,-36.2742356128,10.5883247871));
#69149=CARTESIAN_POINT('Ctrl Pts',(3.39986350918,-36.2742356128,10.5077195847));
#69150=CARTESIAN_POINT('Ctrl Pts',(5.21608381041,-36.5742356128,9.26358008756));
#69151=CARTESIAN_POINT('Ctrl Pts',(5.21608394001,-36.4799878332,9.26357986393));
#69152=CARTESIAN_POINT('Ctrl Pts',(5.1851705575,-36.3857400536,9.24078655442));
#69153=CARTESIAN_POINT('Ctrl Pts',(5.12294992148,-36.3112466293,9.1949099969));
#69154=CARTESIAN_POINT('Ctrl Pts',(5.04422937351,-36.2742356128,9.13686787374));
#69155=CARTESIAN_POINT('Ctrl Pts',(4.96550877419,-36.2742356128,9.07882583933));
#69156=CARTESIAN_POINT('Ctrl Pts',(6.08439879036,-36.5742356128,7.24167411427));
#69157=CARTESIAN_POINT('Ctrl Pts',(6.08439869084,-36.4799878332,7.24167428599));
#69158=CARTESIAN_POINT('Ctrl Pts',(6.04833274366,-36.3857400536,7.23086825093));
#69159=CARTESIAN_POINT('Ctrl Pts',(5.97574160406,-36.3112466293,7.20911826662));
#69160=CARTESIAN_POINT('Ctrl Pts',(5.88390062773,-36.2742356128,7.1816004922));
#69161=CARTESIAN_POINT('Ctrl Pts',(5.79205969084,-36.2742356128,7.15408264964));
#69162=CARTESIAN_POINT('Ctrl Pts',(6.28999565278,-36.5742356128,6.30194108143));
#69163=CARTESIAN_POINT('Ctrl Pts',(6.28999570655,-36.4799878425,6.30194140801));
#69164=CARTESIAN_POINT('Ctrl Pts',(6.25270268299,-36.3857400722,6.29672322672));
#69165=CARTESIAN_POINT('Ctrl Pts',(6.1776416364,-36.3112466512,6.28622029667));
#69166=CARTESIAN_POINT('Ctrl Pts',(6.08267565391,-36.2742356274,6.27293185144));
#69167=CARTESIAN_POINT('Ctrl Pts',(5.98770964456,-36.2742356128,6.25964327781));
#69168=CARTESIAN_POINT('Ctrl Pts',(6.31282662857,-36.5742356128,5.34605335178));
#69169=CARTESIAN_POINT('Ctrl Pts',(6.31282662838,-36.479987833,5.34605335063));
#69170=CARTESIAN_POINT('Ctrl Pts',(6.27540577927,-36.3857400531,5.34652194592));
#69171=CARTESIAN_POINT('Ctrl Pts',(6.20008743734,-36.3112466287,5.34746491082));
#69172=CARTESIAN_POINT('Ctrl Pts',(6.10479600032,-36.2742356124,5.34865801627));
#69173=CARTESIAN_POINT('Ctrl Pts',(6.00950456354,-36.2742356128,5.34985112215));
#69174=CARTESIAN_POINT('Ctrl Pts',(6.1620830891,-36.5742356128,4.41893339717));
#69175=CARTESIAN_POINT('Ctrl Pts',(6.1620830891,-36.4799878332,4.41893339717));
#69176=CARTESIAN_POINT('Ctrl Pts',(6.12555180773,-36.3857400536,4.42487316367));
#69177=CARTESIAN_POINT('Ctrl Pts',(6.05202396388,-36.3112466293,4.43682834856));
#69178=CARTESIAN_POINT('Ctrl Pts',(5.95899781977,-36.2742356128,4.45195383973));
#69179=CARTESIAN_POINT('Ctrl Pts',(5.86597167565,-36.2742356128,4.4670793309));
#69180=CARTESIAN_POINT('',(-2.26207941267376E-14,-36.5742356128,11.664345990025));
#69181=CARTESIAN_POINT('Origin',(1.98978387159151E-5,-36.5721143212387,
11.3664672830582));
#69182=CARTESIAN_POINT('Ctrl Pts',(-8.881784197E-16,-36.5742356128,11.6643459897));
#69183=CARTESIAN_POINT('Ctrl Pts',(1.22322324235,-36.5742356127992,11.6642644652));
#69184=CARTESIAN_POINT('Ctrl Pts',(2.4473136708,-36.5742356127992,11.3659246093));
#69185=CARTESIAN_POINT('Ctrl Pts',(3.57166410201,-36.5742356127992,10.7642929822));
#69186=CARTESIAN_POINT('Ctrl Pts',(5.21608381041,-36.5742356127992,9.26358008756));
#69187=CARTESIAN_POINT('Ctrl Pts',(6.08439879036,-36.5742356127992,7.24167411427));
#69188=CARTESIAN_POINT('Ctrl Pts',(6.28999565278,-36.5742356127992,6.30194108143));
#69189=CARTESIAN_POINT('Ctrl Pts',(6.31282662857,-36.5742356127992,5.34605335178));
#69190=CARTESIAN_POINT('Ctrl Pts',(6.16208308783,-36.5742356128,4.4189333977));
#69191=CARTESIAN_POINT('Ctrl Pts',(5.86597173001,-38.2742356128,4.46707975784));
#69192=CARTESIAN_POINT('Ctrl Pts',(5.95899785196,-38.2742356128,4.45195413465));
#69193=CARTESIAN_POINT('Ctrl Pts',(6.05202397392,-38.2372245963,4.43682851147));
#69194=CARTESIAN_POINT('Ctrl Pts',(6.12555180026,-38.1627311721,4.42487322222));
#69195=CARTESIAN_POINT('Ctrl Pts',(6.16208307292,-38.0684833924,4.41893340389));
#69196=CARTESIAN_POINT('Ctrl Pts',(6.16208307292,-37.9742356128,4.41893340389));
#69197=CARTESIAN_POINT('Ctrl Pts',(6.01420213304,-38.2742356128,5.37874078181));
#69198=CARTESIAN_POINT('Ctrl Pts',(6.10956494828,-38.2742356128,5.37798657976));
#69199=CARTESIAN_POINT('Ctrl Pts',(6.20492776352,-38.2372245963,5.37723237772));
#69200=CARTESIAN_POINT('Ctrl Pts',(6.28030251857,-38.1627311721,5.37663629724));
#69201=CARTESIAN_POINT('Ctrl Pts',(6.3177514017,-38.0684833924,5.37634008214));
#69202=CARTESIAN_POINT('Ctrl Pts',(6.3177514017,-37.9742356128,5.37634008214));
#69203=CARTESIAN_POINT('Ctrl Pts',(5.98610106079,-38.2742356128,6.31912512184));
#69204=CARTESIAN_POINT('Ctrl Pts',(6.08104726414,-38.2742356128,6.3333863194));
#69205=CARTESIAN_POINT('Ctrl Pts',(6.17599346749,-38.2372245963,6.34764751696));
#69206=CARTESIAN_POINT('Ctrl Pts',(6.25103891549,-38.1627311721,6.35891950337));
#69207=CARTESIAN_POINT('Ctrl Pts',(6.28832421261,-38.0684833924,6.36451992356));
#69208=CARTESIAN_POINT('Ctrl Pts',(6.28832421261,-37.9742356128,6.36451992356));
#69209=CARTESIAN_POINT('Ctrl Pts',(5.77227970857,-38.2742356128,7.24175688045));
#69210=CARTESIAN_POINT('Ctrl Pts',(5.86379821772,-38.2742356128,7.27066611408));
#69211=CARTESIAN_POINT('Ctrl Pts',(5.95531672688,-38.2372245963,7.2995753477));
#69212=CARTESIAN_POINT('Ctrl Pts',(6.02765295993,-38.1627311721,7.32242521478));
#69213=CARTESIAN_POINT('Ctrl Pts',(6.06359217089,-38.0684833924,7.3337778291));
#69214=CARTESIAN_POINT('Ctrl Pts',(6.06359217089,-37.9742356128,7.3337778291));
#69215=CARTESIAN_POINT('Ctrl Pts',(4.90899024491,-38.2742356128,9.15302960102));
#69216=CARTESIAN_POINT('Ctrl Pts',(4.98682586563,-38.2742356128,9.21224464762));
#69217=CARTESIAN_POINT('Ctrl Pts',(5.06466148636,-38.2372245963,9.27145969422));
#69218=CARTESIAN_POINT('Ctrl Pts',(5.126182715,-38.1627311721,9.31826323529));
#69219=CARTESIAN_POINT('Ctrl Pts',(5.15674872066,-38.0684833924,9.34151694846));
#69220=CARTESIAN_POINT('Ctrl Pts',(5.15674872066,-37.9742356128,9.34151694846));
#69221=CARTESIAN_POINT('Ctrl Pts',(3.31894855665,-38.2742356128,10.5503954389));
#69222=CARTESIAN_POINT('Ctrl Pts',(3.37162983501,-38.2742356128,10.631675793));
#69223=CARTESIAN_POINT('Ctrl Pts',(3.42431111337,-38.2372245963,10.7129561472));
#69224=CARTESIAN_POINT('Ctrl Pts',(3.46595041963,-38.1627311721,10.7772001444));
#69225=CARTESIAN_POINT('Ctrl Pts',(3.48663827384,-38.0684833924,10.8091188417));
#69226=CARTESIAN_POINT('Ctrl Pts',(3.48663827384,-37.9742356128,10.8091188417));
#69227=CARTESIAN_POINT('Ctrl Pts',(2.2714472695,-38.2742356128,11.0941425407));
#69228=CARTESIAN_POINT('Ctrl Pts',(2.30749032166,-38.2742356128,11.1841227887));
#69229=CARTESIAN_POINT('Ctrl Pts',(2.34353337383,-38.2372245963,11.2741030367));
#69230=CARTESIAN_POINT('Ctrl Pts',(2.3720216678,-38.1627311721,11.3452234049));
#69231=CARTESIAN_POINT('Ctrl Pts',(2.38617586782,-38.0684833924,11.3805585656));
#69232=CARTESIAN_POINT('Ctrl Pts',(2.38617586782,-37.9742356128,11.3805585656));
#69233=CARTESIAN_POINT('Ctrl Pts',(1.13551567819,-38.2742356128,11.36427031));
#69234=CARTESIAN_POINT('Ctrl Pts',(1.15345363427,-38.2742356128,11.4585168943));
#69235=CARTESIAN_POINT('Ctrl Pts',(1.17139159035,-38.2372245963,11.5527634786));
#69236=CARTESIAN_POINT('Ctrl Pts',(1.18556983122,-38.1627311721,11.6272559581));
#69237=CARTESIAN_POINT('Ctrl Pts',(1.19261396576,-38.0684833924,11.6642665053));
#69238=CARTESIAN_POINT('Ctrl Pts',(1.19261396576,-37.9742356128,11.6642665053));
#69239=CARTESIAN_POINT('Ctrl Pts',(-1.99941727153E-5,-38.2742356128,11.3643459904));
#69240=CARTESIAN_POINT('Ctrl Pts',(-1.37128181037E-5,-38.2742356128,11.4585937697));
#69241=CARTESIAN_POINT('Ctrl Pts',(-7.43146349169E-6,-38.2372245963,11.5528415491));
#69242=CARTESIAN_POINT('Ctrl Pts',(-2.46668218784E-6,-38.1627311721,11.6273349733));
#69243=CARTESIAN_POINT('Ctrl Pts',(0.,-38.0684833924,11.6643459897));
#69244=CARTESIAN_POINT('Ctrl Pts',(4.4408920985E-16,-37.9742356128,11.6643459897));
#69245=CARTESIAN_POINT('',(-9.29855414889283E-10,-37.9742356128,11.664345985775));
#69246=CARTESIAN_POINT('Origin',(1.94712553347615E-5,-37.9763569038603,
11.3664672676817));
#69247=CARTESIAN_POINT('Ctrl Pts',(-8.881784197E-16,-37.9742356128,11.6643459897));
#69248=CARTESIAN_POINT('Ctrl Pts',(2.16261462464,-37.9742356128,11.6642018574));
#69249=CARTESIAN_POINT('Ctrl Pts',(4.32870534526,-37.9742356128,10.7314087249));
#69250=CARTESIAN_POINT('Ctrl Pts',(5.93623245773,-37.9742356128,8.8412691379));
#69251=CARTESIAN_POINT('Ctrl Pts',(6.5091537474,-37.9742356128,6.55351625923));
#69252=CARTESIAN_POINT('Ctrl Pts',(6.16208308783,-37.9742356128,4.4189333977));
#69253=CARTESIAN_POINT('Ctrl Pts',(6.16208308783,-37.9742356128,4.4189333977));
#69254=CARTESIAN_POINT('Ctrl Pts',(6.16208308783,-36.2942356128,4.4189333977));
#69255=CARTESIAN_POINT('Ctrl Pts',(6.5091537474,-37.9742356128,6.55351625923));
#69256=CARTESIAN_POINT('Ctrl Pts',(6.5091537474,-36.2942356128,6.55351625923));
#69257=CARTESIAN_POINT('Ctrl Pts',(5.93623245773,-37.9742356128,8.8412691379));
#69258=CARTESIAN_POINT('Ctrl Pts',(5.93623245773,-36.2942356128,8.8412691379));
#69259=CARTESIAN_POINT('Ctrl Pts',(4.32870534526,-37.9742356128,10.7314087249));
#69260=CARTESIAN_POINT('Ctrl Pts',(4.32870534526,-36.2942356128,10.7314087249));
#69261=CARTESIAN_POINT('Ctrl Pts',(2.16261462464,-37.9742356128,11.6642018574));
#69262=CARTESIAN_POINT('Ctrl Pts',(2.16261462464,-36.2942356128,11.6642018574));
#69263=CARTESIAN_POINT('Ctrl Pts',(-3.33066907388E-16,-37.9742356128,11.6643459897));
#69264=CARTESIAN_POINT('Ctrl Pts',(-3.33066907388E-16,-36.2942356128,11.6643459897));
#69265=CARTESIAN_POINT('',(-8.881784197E-16,-37.2742356128,11.6643459897));
#69266=CARTESIAN_POINT('Ctrl Pts',(-6.16208308783,-36.5742356128,4.4189333977));
#69267=CARTESIAN_POINT('Ctrl Pts',(-6.16208308783,-36.4799878332,4.4189333977));
#69268=CARTESIAN_POINT('Ctrl Pts',(-6.12555180739,-36.3857400536,4.42487316974));
#69269=CARTESIAN_POINT('Ctrl Pts',(-6.0520239654,-36.3112466293,4.4368283658));
#69270=CARTESIAN_POINT('Ctrl Pts',(-5.95899782364,-36.2742356128,4.45195387109));
#69271=CARTESIAN_POINT('Ctrl Pts',(-5.86597168188,-36.2742356128,4.46707937639));
#69272=CARTESIAN_POINT('Ctrl Pts',(-6.35839402215,-36.5742356128,5.62630124733));
#69273=CARTESIAN_POINT('Ctrl Pts',(-6.35839402215,-36.4799878332,5.62630124733));
#69274=CARTESIAN_POINT('Ctrl Pts',(-6.32070362989,-36.3857400536,5.6251121534));
#69275=CARTESIAN_POINT('Ctrl Pts',(-6.24484280119,-36.3112466293,5.6227188204));
#69276=CARTESIAN_POINT('Ctrl Pts',(-6.1488650054,-36.2742356128,5.61969081738));
#69277=CARTESIAN_POINT('Ctrl Pts',(-6.05288720961,-36.2742356128,5.61666281436));
#69278=CARTESIAN_POINT('Ctrl Pts',(-6.26045506318,-36.5742356128,6.88241111792));
#69279=CARTESIAN_POINT('Ctrl Pts',(-6.26045499686,-36.4799878304,6.88241099615));
#69280=CARTESIAN_POINT('Ctrl Pts',(-6.22333297826,-36.385740048,6.87373516796));
#69281=CARTESIAN_POINT('Ctrl Pts',(-6.14861621702,-36.3112466227,6.85627316104));
#69282=CARTESIAN_POINT('Ctrl Pts',(-6.0540859168,-36.2742356084,6.83418060869));
#69283=CARTESIAN_POINT('Ctrl Pts',(-5.95955564435,-36.2742356128,6.81208810432));
#69284=CARTESIAN_POINT('Ctrl Pts',(-5.84714534581,-36.5742356128,8.08876910145));
#69285=CARTESIAN_POINT('Ctrl Pts',(-5.84714560615,-36.4799878332,8.08876888811));
#69286=CARTESIAN_POINT('Ctrl Pts',(-5.8125000472,-36.3857400536,8.07293070699));
#69287=CARTESIAN_POINT('Ctrl Pts',(-5.74276722117,-36.3112466293,8.04105288192));
#69288=CARTESIAN_POINT('Ctrl Pts',(-5.65454236156,-36.2742356128,8.00072174454));
#69289=CARTESIAN_POINT('Ctrl Pts',(-5.56631739861,-36.2742356128,7.96039069172));
#69290=CARTESIAN_POINT('Ctrl Pts',(-4.62991621251,-36.5742356128,9.95279930682));
#69291=CARTESIAN_POINT('Ctrl Pts',(-4.6299160126,-36.4799878332,9.95279947064));
#69292=CARTESIAN_POINT('Ctrl Pts',(-4.60245517626,-36.3857400536,9.92594663756));
#69293=CARTESIAN_POINT('Ctrl Pts',(-4.54718408945,-36.3112466293,9.87189876027));
#69294=CARTESIAN_POINT('Ctrl Pts',(-4.47725615686,-36.2742356128,9.80351822959));
#69295=CARTESIAN_POINT('Ctrl Pts',(-4.40732830362,-36.2742356128,9.73513763396));
#69296=CARTESIAN_POINT('Ctrl Pts',(-2.77364981049,-36.5742356128,11.1344717293));
#69297=CARTESIAN_POINT('Ctrl Pts',(-2.77364996401,-36.4799878332,11.1344716035));
#69298=CARTESIAN_POINT('Ctrl Pts',(-2.75719363855,-36.3857400536,11.1006084628));
#69299=CARTESIAN_POINT('Ctrl Pts',(-2.72407112966,-36.3112466293,11.0324510365));
#69300=CARTESIAN_POINT('Ctrl Pts',(-2.68216504727,-36.2742356128,10.9462195277));
#69301=CARTESIAN_POINT('Ctrl Pts',(-2.64025890396,-36.2742356128,10.8599880688));
#69302=CARTESIAN_POINT('Ctrl Pts',(-1.87911669731,-36.5742356128,11.4882778234));
#69303=CARTESIAN_POINT('Ctrl Pts',(-1.87911702828,-36.4799878425,11.4882778241));
#69304=CARTESIAN_POINT('Ctrl Pts',(-1.86797905714,-36.3857400722,11.4523063823));
#69305=CARTESIAN_POINT('Ctrl Pts',(-1.84556114865,-36.3112466512,11.379905349));
#69306=CARTESIAN_POINT('Ctrl Pts',(-1.81719807576,-36.2742356274,11.2883048211));
#69307=CARTESIAN_POINT('Ctrl Pts',(-1.78883487183,-36.2742356128,11.1967042873));
#69308=CARTESIAN_POINT('Ctrl Pts',(-0.939294959167,-36.5742356128,11.664282669));
#69309=CARTESIAN_POINT('Ctrl Pts',(-0.939294958001,-36.479987833,11.664282669));
#69310=CARTESIAN_POINT('Ctrl Pts',(-0.933749468027,-36.3857400531,11.6272720345));
#69311=CARTESIAN_POINT('Ctrl Pts',(-0.922587661188,-36.3112466287,11.5527793779));
#69312=CARTESIAN_POINT('Ctrl Pts',(-0.908466021992,-36.2742356124,11.4585325701));
#69313=CARTESIAN_POINT('Ctrl Pts',(-0.894344383251,-36.2742356128,11.3642857625));
#69314=CARTESIAN_POINT('Ctrl Pts',(3.1926341727E-10,-36.5742356128,11.664345991));
#69315=CARTESIAN_POINT('Ctrl Pts',(3.15680505525E-10,-36.4799878332,11.664345991));
#69316=CARTESIAN_POINT('Ctrl Pts',(2.47261842083E-6,-36.3857400536,11.6273349746));
#69317=CARTESIAN_POINT('Ctrl Pts',(7.44871679598E-6,-36.3112466293,11.5528415504));
#69318=CARTESIAN_POINT('Ctrl Pts',(1.37443917449E-5,-36.2742356128,11.458593771));
#69319=CARTESIAN_POINT('Ctrl Pts',(2.00400681003E-5,-36.2742356128,11.3643459915));
#69320=CARTESIAN_POINT('',(-6.162083087295,-36.5742356128,4.41893339689));
#69321=CARTESIAN_POINT('Origin',(-5.86806546560554,-36.5721142937107,4.4667386455464));
#69322=CARTESIAN_POINT('Ctrl Pts',(-6.16208308783,-36.5742356128,4.4189333977));
#69323=CARTESIAN_POINT('Ctrl Pts',(-6.35839402215,-36.5742356127992,5.62630124733));
#69324=CARTESIAN_POINT('Ctrl Pts',(-6.26045506318,-36.5742356127992,6.88241111792));
#69325=CARTESIAN_POINT('Ctrl Pts',(-5.84714534581,-36.5742356127992,8.08876910145));
#69326=CARTESIAN_POINT('Ctrl Pts',(-4.62991621251,-36.5742356127992,9.95279930682));
#69327=CARTESIAN_POINT('Ctrl Pts',(-2.77364981049,-36.5742356127992,11.1344717293));
#69328=CARTESIAN_POINT('Ctrl Pts',(-1.87911669731,-36.5742356127992,11.4882778234));
#69329=CARTESIAN_POINT('Ctrl Pts',(-0.939294959167,-36.5742356127992,11.664282669));
#69330=CARTESIAN_POINT('Ctrl Pts',(-8.881784197E-16,-36.5742356128,11.6643459897));
#69331=CARTESIAN_POINT('Ctrl Pts',(1.96099429597E-5,-38.2742356128,11.3643459766));
#69332=CARTESIAN_POINT('Ctrl Pts',(1.34481291951E-5,-38.2742356128,11.4585937554));
#69333=CARTESIAN_POINT('Ctrl Pts',(7.2863154319E-6,-38.2372245963,11.5528415342));
#69334=CARTESIAN_POINT('Ctrl Pts',(2.41601918738E-6,-38.1627311721,11.6273349578));
#69335=CARTESIAN_POINT('Ctrl Pts',(-3.71941810684E-9,-38.0684833924,11.664345974));
#69336=CARTESIAN_POINT('Ctrl Pts',(-3.71941899502E-9,-37.9742356128,11.664345974));
#69337=CARTESIAN_POINT('Ctrl Pts',(-0.923613472615,-38.2742356128,11.3642840884));
#69338=CARTESIAN_POINT('Ctrl Pts',(-0.938179781412,-38.2742356128,11.4585308814));
#69339=CARTESIAN_POINT('Ctrl Pts',(-0.952746090209,-38.2372245963,11.5527776745));
#69340=CARTESIAN_POINT('Ctrl Pts',(-0.964259338702,-38.1627311721,11.6272703192));
#69341=CARTESIAN_POINT('Ctrl Pts',(-0.969979473568,-38.0684833924,11.6642809481));
#69342=CARTESIAN_POINT('Ctrl Pts',(-0.969979473568,-37.9742356128,11.6642809481));
#69343=CARTESIAN_POINT('Ctrl Pts',(-1.8472868151,-38.2742356128,11.1855666197));
#69344=CARTESIAN_POINT('Ctrl Pts',(-1.87660684553,-38.2742356128,11.2769914473));
#69345=CARTESIAN_POINT('Ctrl Pts',(-1.90592687595,-38.2372245963,11.3684162749));
#69346=CARTESIAN_POINT('Ctrl Pts',(-1.9291013597,-38.1627311721,11.4406784382));
#69347=CARTESIAN_POINT('Ctrl Pts',(-1.94061537058,-38.0684833924,11.4765808844));
#69348=CARTESIAN_POINT('Ctrl Pts',(-1.94061537058,-37.9742356128,11.4765808844));
#69349=CARTESIAN_POINT('Ctrl Pts',(-2.72362004199,-38.2742356128,10.8263883796));
#69350=CARTESIAN_POINT('Ctrl Pts',(-2.76684775976,-38.2742356128,10.9120782024));
#69351=CARTESIAN_POINT('Ctrl Pts',(-2.81007547753,-38.2372245963,10.9977680251));
#69352=CARTESIAN_POINT('Ctrl Pts',(-2.84424267491,-38.1627311721,11.065497263));
#69353=CARTESIAN_POINT('Ctrl Pts',(-2.86121814123,-38.0684833924,11.0991475569));
#69354=CARTESIAN_POINT('Ctrl Pts',(-2.86121814123,-37.9742356128,11.0991475569));
#69355=CARTESIAN_POINT('Ctrl Pts',(-4.47149525948,-38.2742356128,9.66743871091));
#69356=CARTESIAN_POINT('Ctrl Pts',(-4.54243882238,-38.2742356128,9.73475747859));
#69357=CARTESIAN_POINT('Ctrl Pts',(-4.61338238528,-38.2372245963,9.80207624627));
#69358=CARTESIAN_POINT('Ctrl Pts',(-4.66945613866,-38.1627311721,9.85528495994));
#69359=CARTESIAN_POINT('Ctrl Pts',(-4.69731563381,-38.0684833924,9.88172100368));
#69360=CARTESIAN_POINT('Ctrl Pts',(-4.69731563381,-37.9742356128,9.88172100368));
#69361=CARTESIAN_POINT('Ctrl Pts',(-5.5954485446,-38.2742356128,7.87367371291));
#69362=CARTESIAN_POINT('Ctrl Pts',(-5.68413257942,-38.2742356128,7.91262181979));
#69363=CARTESIAN_POINT('Ctrl Pts',(-5.77281661423,-38.2372245963,7.95156992668));
#69364=CARTESIAN_POINT('Ctrl Pts',(-5.84291248439,-38.1627311721,7.98235453304));
#69365=CARTESIAN_POINT('Ctrl Pts',(-5.87773859488,-38.0684833924,7.9976493876));
#69366=CARTESIAN_POINT('Ctrl Pts',(-5.87773859488,-37.9742356128,7.9976493876));
#69367=CARTESIAN_POINT('Ctrl Pts',(-5.96396296691,-38.2742356128,6.75246143244));
#69368=CARTESIAN_POINT('Ctrl Pts',(-6.05856272782,-38.2742356128,6.77359036684));
#69369=CARTESIAN_POINT('Ctrl Pts',(-6.15316248873,-38.2372245963,6.79471930124));
#69370=CARTESIAN_POINT('Ctrl Pts',(-6.22793409869,-38.1627311721,6.81141948144));
#69371=CARTESIAN_POINT('Ctrl Pts',(-6.2650833582,-38.0684833924,6.81971691948));
#69372=CARTESIAN_POINT('Ctrl Pts',(-6.2650833582,-37.9742356128,6.81971691948));
#69373=CARTESIAN_POINT('Ctrl Pts',(-6.04820993657,-38.2742356128,5.58789626039));
#69374=CARTESIAN_POINT('Ctrl Pts',(-6.14411387177,-38.2742356128,5.59046999984));
#69375=CARTESIAN_POINT('Ctrl Pts',(-6.24001780696,-38.2372245963,5.59304373929));
#69376=CARTESIAN_POINT('Ctrl Pts',(-6.31582026979,-38.1627311721,5.59507810563));
#69377=CARTESIAN_POINT('Ctrl Pts',(-6.35348164354,-38.0684833924,5.59608872751));
#69378=CARTESIAN_POINT('Ctrl Pts',(-6.35348164354,-37.9742356128,5.59608872751));
#69379=CARTESIAN_POINT('Ctrl Pts',(-5.86597168188,-38.2742356128,4.46707937639));
#69380=CARTESIAN_POINT('Ctrl Pts',(-5.95899782364,-38.2742356128,4.45195387109));
#69381=CARTESIAN_POINT('Ctrl Pts',(-6.0520239654,-38.2372245963,4.4368283658));
#69382=CARTESIAN_POINT('Ctrl Pts',(-6.12555180739,-38.1627311721,4.42487316974));
#69383=CARTESIAN_POINT('Ctrl Pts',(-6.16208308783,-38.0684833924,4.4189333977));
#69384=CARTESIAN_POINT('Ctrl Pts',(-6.16208308783,-37.9742356128,4.4189333977));
#69385=CARTESIAN_POINT('',(-6.1620830869925,-37.9742356128,4.418933396415));
#69386=CARTESIAN_POINT('Origin',(-5.86806549401996,-37.9763569532034,4.46673864924859));
#69387=CARTESIAN_POINT('Ctrl Pts',(-6.16208308783,-37.9742356128,4.4189333977));
#69388=CARTESIAN_POINT('Ctrl Pts',(-6.5091537474,-37.9742356128,6.55351625923));
#69389=CARTESIAN_POINT('Ctrl Pts',(-5.93623245773,-37.9742356128,8.8412691379));
#69390=CARTESIAN_POINT('Ctrl Pts',(-4.32870534526,-37.9742356128,10.7314087249));
#69391=CARTESIAN_POINT('Ctrl Pts',(-2.16261462464,-37.9742356128,11.6642018574));
#69392=CARTESIAN_POINT('Ctrl Pts',(-8.881784197E-16,-37.9742356128,11.6643459897));
#69393=CARTESIAN_POINT('Ctrl Pts',(-8.881784197E-16,-37.9742356128,11.6643459897));
#69394=CARTESIAN_POINT('Ctrl Pts',(-8.881784197E-16,-36.2942356128,11.6643459897));
#69395=CARTESIAN_POINT('Ctrl Pts',(-2.16261462464,-37.9742356128,11.6642018574));
#69396=CARTESIAN_POINT('Ctrl Pts',(-2.16261462464,-36.2942356128,11.6642018574));
#69397=CARTESIAN_POINT('Ctrl Pts',(-4.32870534526,-37.9742356128,10.7314087249));
#69398=CARTESIAN_POINT('Ctrl Pts',(-4.32870534526,-36.2942356128,10.7314087249));
#69399=CARTESIAN_POINT('Ctrl Pts',(-5.93623245773,-37.9742356128,8.8412691379));
#69400=CARTESIAN_POINT('Ctrl Pts',(-5.93623245773,-36.2942356128,8.8412691379));
#69401=CARTESIAN_POINT('Ctrl Pts',(-6.5091537474,-37.9742356128,6.55351625923));
#69402=CARTESIAN_POINT('Ctrl Pts',(-6.5091537474,-36.2942356128,6.55351625923));
#69403=CARTESIAN_POINT('Ctrl Pts',(-6.16208308783,-37.9742356128,4.4189333977));
#69404=CARTESIAN_POINT('Ctrl Pts',(-6.16208308783,-36.2942356128,4.4189333977));
#69405=CARTESIAN_POINT('',(-6.16208308783,-37.2742356128,4.4189333977));
#69406=CARTESIAN_POINT('Ctrl Pts',(-6.62478636278,-36.5742356128,4.12129363314));
#69407=CARTESIAN_POINT('Ctrl Pts',(-6.62478636278,-36.4799878332,4.12129363314));
#69408=CARTESIAN_POINT('Ctrl Pts',(-6.64533881083,-36.3857400536,4.09051357105));
#69409=CARTESIAN_POINT('Ctrl Pts',(-6.68670547342,-36.3112466293,4.02856141623));
#69410=CARTESIAN_POINT('Ctrl Pts',(-6.7390418526,-36.2742356128,3.95018063176));
#69411=CARTESIAN_POINT('Ctrl Pts',(-6.79137823178,-36.2742356128,3.87179984728));
#69412=CARTESIAN_POINT('Ctrl Pts',(-6.57452017565,-36.5742356128,4.08772991919));
#69413=CARTESIAN_POINT('Ctrl Pts',(-6.57452017565,-36.4799878332,4.08772991919));
#69414=CARTESIAN_POINT('Ctrl Pts',(-6.58892710136,-36.3857400536,4.05284637296));
#69415=CARTESIAN_POINT('Ctrl Pts',(-6.61792442226,-36.3112466293,3.98263496631));
#69416=CARTESIAN_POINT('Ctrl Pts',(-6.65461133659,-36.2742356128,3.89380472879));
#69417=CARTESIAN_POINT('Ctrl Pts',(-6.69129825092,-36.2742356128,3.80497449128));
#69418=CARTESIAN_POINT('Ctrl Pts',(-6.5160654267,-36.5742356128,4.06685309219));
#69419=CARTESIAN_POINT('Ctrl Pts',(-6.51606545157,-36.4799878341,4.06685311826));
#69420=CARTESIAN_POINT('Ctrl Pts',(-6.52325959788,-36.3857400553,4.0293608744));
#69421=CARTESIAN_POINT('Ctrl Pts',(-6.53773954623,-36.3112466313,3.95389885357));
#69422=CARTESIAN_POINT('Ctrl Pts',(-6.55605928475,-36.2742356142,3.85842559837));
#69423=CARTESIAN_POINT('Ctrl Pts',(-6.57437901362,-36.2742356128,3.76295233242));
#69424=CARTESIAN_POINT('Ctrl Pts',(-6.45374447685,-36.5742356128,4.06145161999));
#69425=CARTESIAN_POINT('Ctrl Pts',(-6.45374450233,-36.4799878332,4.06145160386));
#69426=CARTESIAN_POINT('Ctrl Pts',(-6.45313203559,-36.3857400535,4.02328625262));
#69427=CARTESIAN_POINT('Ctrl Pts',(-6.45189903265,-36.3112466293,3.94646790973));
#69428=CARTESIAN_POINT('Ctrl Pts',(-6.45033914294,-36.2742356128,3.84927935169));
#69429=CARTESIAN_POINT('Ctrl Pts',(-6.448779243,-36.2742356128,3.75209080017));
#69430=CARTESIAN_POINT('Ctrl Pts',(-6.31228390912,-36.5742356128,4.0856584563));
#69431=CARTESIAN_POINT('Ctrl Pts',(-6.31228387569,-36.4799878333,4.08565847747));
#69432=CARTESIAN_POINT('Ctrl Pts',(-6.29422735035,-36.3857400538,4.05052572546));
#69433=CARTESIAN_POINT('Ctrl Pts',(-6.25788474007,-36.3112466295,3.97981475152));
#69434=CARTESIAN_POINT('Ctrl Pts',(-6.21190456653,-36.2742356129,3.89035159857));
#69435=CARTESIAN_POINT('Ctrl Pts',(-6.16592440644,-36.2742356128,3.80088843706));
#69436=CARTESIAN_POINT('Ctrl Pts',(-6.20284603213,-36.5742356128,4.18404937306));
#69437=CARTESIAN_POINT('Ctrl Pts',(-6.202846076,-36.4799878331,4.18404934528));
#69438=CARTESIAN_POINT('Ctrl Pts',(-6.17143035383,-36.3857400534,4.16092715811));
#69439=CARTESIAN_POINT('Ctrl Pts',(-6.10819814971,-36.3112466292,4.1143857057));
#69440=CARTESIAN_POINT('Ctrl Pts',(-6.02819808562,-36.2742356127,4.05550338866));
#69441=CARTESIAN_POINT('Ctrl Pts',(-5.94819800384,-36.2742356128,3.99662108289));
#69442=CARTESIAN_POINT('Ctrl Pts',(-6.16233508317,-36.5742356128,4.25881330688));
#69443=CARTESIAN_POINT('Ctrl Pts',(-6.16233507193,-36.4799878312,4.25881328382));
#69444=CARTESIAN_POINT('Ctrl Pts',(-6.12578886815,-36.3857400495,4.24495014557));
#69445=CARTESIAN_POINT('Ctrl Pts',(-6.05223285478,-36.3112466242,4.21705793513));
#69446=CARTESIAN_POINT('Ctrl Pts',(-5.95917030134,-36.2742356096,4.1817647567));
#69447=CARTESIAN_POINT('Ctrl Pts',(-5.86610775343,-36.2742356128,4.14647158762));
#69448=CARTESIAN_POINT('Ctrl Pts',(-6.14934204931,-36.5742356128,4.34057228077));
#69449=CARTESIAN_POINT('Ctrl Pts',(-6.14934204855,-36.4799878345,4.34057227621));
#69450=CARTESIAN_POINT('Ctrl Pts',(-6.11125741298,-36.3857400562,4.33695823749));
#69451=CARTESIAN_POINT('Ctrl Pts',(-6.03460182449,-36.3112466325,4.32967707355));
#69452=CARTESIAN_POINT('Ctrl Pts',(-5.93761903844,-36.2742356148,4.32046804105));
#69453=CARTESIAN_POINT('Ctrl Pts',(-5.840636252,-36.2742356128,4.31125901017));
#69454=CARTESIAN_POINT('Ctrl Pts',(-6.16208308569,-36.5742356128,4.41893339446));
#69455=CARTESIAN_POINT('Ctrl Pts',(-6.1620830857,-36.4799878332,4.41893339453));
#69456=CARTESIAN_POINT('Ctrl Pts',(-6.12555180375,-36.3857400535,4.42487314505));
#69457=CARTESIAN_POINT('Ctrl Pts',(-6.05202395871,-36.3112466292,4.43682829772));
#69458=CARTESIAN_POINT('Ctrl Pts',(-5.95899781312,-36.2742356128,4.45195374807));
#69459=CARTESIAN_POINT('Ctrl Pts',(-5.86597166755,-36.2742356128,4.4670791984));
#69460=CARTESIAN_POINT('',(-6.62478636300403,-36.5742356128,4.12129363280448));
#69461=CARTESIAN_POINT('Origin',(-6.7901996463368,-36.5721143211899,3.87356359757439));
#69462=CARTESIAN_POINT('Ctrl Pts',(-6.62478636278,-36.5742356128,4.12129363314));
#69463=CARTESIAN_POINT('Ctrl Pts',(-6.50898576372,-36.5742356128,4.04397131362));
#69464=CARTESIAN_POINT('Ctrl Pts',(-6.34774592774,-36.5742356128,4.03257337207));
#69465=CARTESIAN_POINT('Ctrl Pts',(-6.19622108576,-36.5742356128,4.13004365321));
#69466=CARTESIAN_POINT('Ctrl Pts',(-6.13973650651,-36.5742356128,4.28149559307));
#69467=CARTESIAN_POINT('Ctrl Pts',(-6.16208308783,-36.5742356128,4.4189333977));
#69468=CARTESIAN_POINT('Ctrl Pts',(-5.86597167956,-38.2742356128,4.46707920117));
#69469=CARTESIAN_POINT('Ctrl Pts',(-5.95899782099,-38.2742356128,4.4519537493));
#69470=CARTESIAN_POINT('Ctrl Pts',(-6.05202396243,-38.2372245963,4.43682829744));
#69471=CARTESIAN_POINT('Ctrl Pts',(-6.12555180416,-38.1627311721,4.42487314362));
#69472=CARTESIAN_POINT('Ctrl Pts',(-6.16208308448,-38.0684833924,4.41893339256));
#69473=CARTESIAN_POINT('Ctrl Pts',(-6.16208308448,-37.9742356128,4.41893339256));
#69474=CARTESIAN_POINT('Ctrl Pts',(-5.84345320673,-38.2742356128,4.32858436112));
#69475=CARTESIAN_POINT('Ctrl Pts',(-5.93999533685,-38.2742356128,4.33508315368));
#69476=CARTESIAN_POINT('Ctrl Pts',(-6.03653746697,-38.2372245963,4.34158194625));
#69477=CARTESIAN_POINT('Ctrl Pts',(-6.11284466996,-38.1627311721,4.34672039209));
#69478=CARTESIAN_POINT('Ctrl Pts',(-6.15075635123,-38.0684833924,4.34927066034));
#69479=CARTESIAN_POINT('Ctrl Pts',(-6.15075635123,-37.9742356128,4.34927066034));
#69480=CARTESIAN_POINT('Ctrl Pts',(-5.86108700083,-38.2742356128,4.1830357728));
#69481=CARTESIAN_POINT('Ctrl Pts',(-5.9549289869,-38.2742356128,4.21254028592));
#69482=CARTESIAN_POINT('Ctrl Pts',(-6.04877097298,-38.2372245963,4.24204479904));
#69483=CARTESIAN_POINT('Ctrl Pts',(-6.12294317876,-38.1627311721,4.26536245256));
#69484=CARTESIAN_POINT('Ctrl Pts',(-6.1597953199,-38.0684833924,4.27695155493));
#69485=CARTESIAN_POINT('Ctrl Pts',(-6.1597953199,-37.9742356128,4.27695155493));
#69486=CARTESIAN_POINT('Ctrl Pts',(-5.92292196944,-38.2742356128,4.04703912854));
#69487=CARTESIAN_POINT('Ctrl Pts',(-6.00693080322,-38.2742356128,4.09800013468));
#69488=CARTESIAN_POINT('Ctrl Pts',(-6.09093963701,-38.2372245963,4.14896114082));
#69489=CARTESIAN_POINT('Ctrl Pts',(-6.15734124187,-38.1627311721,4.18924200394));
#69490=CARTESIAN_POINT('Ctrl Pts',(-6.19033039264,-38.0684833924,4.20925304918));
#69491=CARTESIAN_POINT('Ctrl Pts',(-6.19033039264,-37.9742356128,4.20925304918));
#69492=CARTESIAN_POINT('Ctrl Pts',(-6.11534148986,-38.2742356128,3.83026274895));
#69493=CARTESIAN_POINT('Ctrl Pts',(-6.16918512024,-38.2742356128,3.91514701063));
#69494=CARTESIAN_POINT('Ctrl Pts',(-6.22302875062,-38.2372245963,4.00003127231));
#69495=CARTESIAN_POINT('Ctrl Pts',(-6.26558574119,-38.1627311721,4.0671224893));
#69496=CARTESIAN_POINT('Ctrl Pts',(-6.28673108844,-38.0684833924,4.10045774569));
#69497=CARTESIAN_POINT('Ctrl Pts',(-6.28673108844,-37.9742356128,4.10045774569));
#69498=CARTESIAN_POINT('Ctrl Pts',(-6.39337248546,-38.2742356128,3.74948730929));
#69499=CARTESIAN_POINT('Ctrl Pts',(-6.40368458266,-38.2742356128,3.84705936306));
#69500=CARTESIAN_POINT('Ctrl Pts',(-6.41399667986,-38.2372245963,3.94463141684));
#69501=CARTESIAN_POINT('Ctrl Pts',(-6.4221483252,-38.1627311721,4.02175362115));
#69502=CARTESIAN_POINT('Ctrl Pts',(-6.42619691032,-38.0684833924,4.0600688026));
#69503=CARTESIAN_POINT('Ctrl Pts',(-6.42619691032,-37.9742356128,4.0600688026));
#69504=CARTESIAN_POINT('Ctrl Pts',(-6.53973745527,-38.2742356128,3.75112508254));
#69505=CARTESIAN_POINT('Ctrl Pts',(-6.52687581649,-38.2742356128,3.84847995905));
#69506=CARTESIAN_POINT('Ctrl Pts',(-6.51401417772,-38.2372245963,3.94583483556));
#69507=CARTESIAN_POINT('Ctrl Pts',(-6.50384486271,-38.1627311721,4.02278167233));
#69508=CARTESIAN_POINT('Ctrl Pts',(-6.49879758752,-38.0684833924,4.06101527916));
#69509=CARTESIAN_POINT('Ctrl Pts',(-6.49879758752,-37.9742356128,4.06101527916));
#69510=CARTESIAN_POINT('Ctrl Pts',(-6.67670923675,-38.2742356128,3.79523312185));
#69511=CARTESIAN_POINT('Ctrl Pts',(-6.64230360047,-38.2742356128,3.88558661323));
#69512=CARTESIAN_POINT('Ctrl Pts',(-6.60789796419,-38.2372245963,3.97594010461));
#69513=CARTESIAN_POINT('Ctrl Pts',(-6.58070607097,-38.1627311721,4.04735711157));
#69514=CARTESIAN_POINT('Ctrl Pts',(-6.56719269506,-38.0684833924,4.08283721742));
#69515=CARTESIAN_POINT('Ctrl Pts',(-6.56719269506,-37.9742356128,4.08283721742));
#69516=CARTESIAN_POINT('Ctrl Pts',(-6.79137823178,-38.2742356128,3.87179984728));
#69517=CARTESIAN_POINT('Ctrl Pts',(-6.7390418526,-38.2742356128,3.95018063176));
#69518=CARTESIAN_POINT('Ctrl Pts',(-6.68670547342,-38.2372245963,4.02856141623));
#69519=CARTESIAN_POINT('Ctrl Pts',(-6.64533881083,-38.1627311721,4.09051357105));
#69520=CARTESIAN_POINT('Ctrl Pts',(-6.62478636278,-38.0684833924,4.12129363314));
#69521=CARTESIAN_POINT('Ctrl Pts',(-6.62478636278,-37.9742356128,4.12129363314));
#69522=CARTESIAN_POINT('',(-6.62478636278,-37.9742356128,4.12129363314));
#69523=CARTESIAN_POINT('Origin',(-6.79020165742271,-37.9763569229,3.87356496908019));
#69524=CARTESIAN_POINT('Ctrl Pts',(-6.62478636278,-37.9742356128,4.12129363314));
#69525=CARTESIAN_POINT('Ctrl Pts',(-6.60980787112068,-37.9742356128,4.11129220199465));
#69526=CARTESIAN_POINT('Ctrl Pts',(-6.59393742031848,-37.9742356128,4.10263571211049));
#69527=CARTESIAN_POINT('Ctrl Pts',(-6.57743087233442,-37.9742356128,4.09546961237743));
#69528=CARTESIAN_POINT('Ctrl Pts',(-6.56094526970541,-37.9742356128,4.08831260579356));
#69529=CARTESIAN_POINT('Ctrl Pts',(-6.54382543811632,-37.9742356128,4.08264228477619));
#69530=CARTESIAN_POINT('Ctrl Pts',(-6.52633933526977,-37.9742356128,4.0785532591173));
#69531=CARTESIAN_POINT('Ctrl Pts',(-6.5088749281894,-37.9742356128,4.07446930688987));
#69532=CARTESIAN_POINT('Ctrl Pts',(-6.49104541888437,-37.9742356128,4.07196278396557));
#69533=CARTESIAN_POINT('Ctrl Pts',(-6.47312694977236,-37.9742356128,4.07107677504198));
#69534=CARTESIAN_POINT('Ctrl Pts',(-6.45523981202579,-37.9742356128,4.0701923153506));
#69535=CARTESIAN_POINT('Ctrl Pts',(-6.4372642894345,-37.9742356128,4.07092273833882));
#69536=CARTESIAN_POINT('Ctrl Pts',(-6.4194803008611,-37.9742356128,4.07325923758356));
#69537=CARTESIAN_POINT('Ctrl Pts',(-6.401715949138,-37.9742356128,4.07559315689604));
#69538=CARTESIAN_POINT('Ctrl Pts',(-6.38414297337429,-37.9742356128,4.07952962384662));
#69539=CARTESIAN_POINT('Ctrl Pts',(-6.36704162076337,-37.9742356128,4.0850079039406));
#69540=CARTESIAN_POINT('Ctrl Pts',(-6.34996634542379,-37.9742356128,4.09047783039147));
#69541=CARTESIAN_POINT('Ctrl Pts',(-6.33336151916574,-37.9742356128,4.09748486400625));
#69542=CARTESIAN_POINT('Ctrl Pts',(-6.31750340617419,-37.9742356128,4.10591666015032));
#69543=CARTESIAN_POINT('Ctrl Pts',(-6.31105406776151,-37.9742356128,4.10934578862159));
#69544=CARTESIAN_POINT('Ctrl Pts',(-6.30472818010765,-37.9742356128,4.11300997159109));
#69545=CARTESIAN_POINT('Ctrl Pts',(-6.29854404488772,-37.9742356128,4.11689920017885));
#69546=CARTESIAN_POINT('Ctrl Pts',(-6.28358900896551,-37.9742356128,4.12630448502001));
#69547=CARTESIAN_POINT('Ctrl Pts',(-6.2694662070212,-37.9742356128,4.13702813937559));
#69548=CARTESIAN_POINT('Ctrl Pts',(-6.25640125842688,-37.9742356128,4.14889368279589));
#69549=CARTESIAN_POINT('Ctrl Pts',(-6.2431639186608,-37.9742356128,4.16091579131242));
#69550=CARTESIAN_POINT('Ctrl Pts',(-6.23101274439312,-37.9742356128,4.1741096572297));
#69551=CARTESIAN_POINT('Ctrl Pts',(-6.22013923191321,-37.9742356128,4.18825931672047));
#69552=CARTESIAN_POINT('Ctrl Pts',(-6.20915109541951,-37.9742356128,4.20255813599449));
#69553=CARTESIAN_POINT('Ctrl Pts',(-6.19946788747794,-37.9742356128,4.21783247671418));
#69554=CARTESIAN_POINT('Ctrl Pts',(-6.19124041418449,-37.9742356128,4.23383418171913));
#69555=CARTESIAN_POINT('Ctrl Pts',(-6.18294233481706,-37.9742356128,4.24997320926858));
#69556=CARTESIAN_POINT('Ctrl Pts',(-6.17612524468972,-37.9742356128,4.26685156098772));
#69557=CARTESIAN_POINT('Ctrl Pts',(-6.17089386489525,-37.9742356128,4.28419745826298));
#69558=CARTESIAN_POINT('Ctrl Pts',(-6.16566177951222,-37.9742356128,4.30154569508676));
#69559=CARTESIAN_POINT('Ctrl Pts',(-6.1620159041005,-37.9742356128,4.31936099759098));
#69560=CARTESIAN_POINT('Ctrl Pts',(-6.16000954443398,-37.9742356128,4.33736332366485));
#69561=CARTESIAN_POINT('Ctrl Pts',(-6.15801470288541,-37.9742356128,4.35526230191006));
#69562=CARTESIAN_POINT('Ctrl Pts',(-6.15764060490737,-37.9742356128,4.37334557885617));
#69563=CARTESIAN_POINT('Ctrl Pts',(-6.1588883338163,-37.9742356128,4.39133874672889));
#69564=CARTESIAN_POINT('Ctrl Pts',(-6.15952865917384,-37.9742356128,4.40057270898534));
#69565=CARTESIAN_POINT('Ctrl Pts',(-6.16059528794716,-37.9742356128,4.4097830074333));
#69566=CARTESIAN_POINT('Ctrl Pts',(-6.16208308448,-37.9742356128,4.41893339256));
#69567=CARTESIAN_POINT('Ctrl Pts',(-6.16208308783,-37.9742356128,4.4189333977));
#69568=CARTESIAN_POINT('Ctrl Pts',(-6.16208308783,-36.2942356128,4.4189333977));
#69569=CARTESIAN_POINT('Ctrl Pts',(-6.13973650651,-37.9742356128,4.28149559307));
#69570=CARTESIAN_POINT('Ctrl Pts',(-6.13973650651,-36.2942356128,4.28149559307));
#69571=CARTESIAN_POINT('Ctrl Pts',(-6.19622108576,-37.9742356128,4.13004365321));
#69572=CARTESIAN_POINT('Ctrl Pts',(-6.19622108576,-36.2942356128,4.13004365321));
#69573=CARTESIAN_POINT('Ctrl Pts',(-6.34774592774,-37.9742356128,4.03257337207));
#69574=CARTESIAN_POINT('Ctrl Pts',(-6.34774592774,-36.2942356128,4.03257337207));
#69575=CARTESIAN_POINT('Ctrl Pts',(-6.50898576372,-37.9742356128,4.04397131362));
#69576=CARTESIAN_POINT('Ctrl Pts',(-6.50898576372,-36.2942356128,4.04397131362));
#69577=CARTESIAN_POINT('Ctrl Pts',(-6.62478636278,-37.9742356128,4.12129363314));
#69578=CARTESIAN_POINT('Ctrl Pts',(-6.62478636278,-36.2942356128,4.12129363314));
#69579=CARTESIAN_POINT('',(-6.62478636278,-37.2742356128,4.12129363314));
#69580=CARTESIAN_POINT('Ctrl Pts',(-10.3257952821,-36.5742356128,3.01322822759));
#69581=CARTESIAN_POINT('Ctrl Pts',(-10.3257952821,-36.4799878332,3.01322822759));
#69582=CARTESIAN_POINT('Ctrl Pts',(-10.2942035846,-36.3857400536,2.99394663035));
#69583=CARTESIAN_POINT('Ctrl Pts',(-10.2306178216,-36.3112466293,2.95513785557));
#69584=CARTESIAN_POINT('Ctrl Pts',(-10.1501702245,-36.2742356128,2.90603767139));
#69585=CARTESIAN_POINT('Ctrl Pts',(-10.0697226274,-36.2742356128,2.85693748721));
#69586=CARTESIAN_POINT('Ctrl Pts',(-10.2120403388,-36.5742356128,3.19960862508));
#69587=CARTESIAN_POINT('Ctrl Pts',(-10.2120403388,-36.4799878332,3.19960862508));
#69588=CARTESIAN_POINT('Ctrl Pts',(-10.1811264858,-36.3857400536,3.17921642189));
#69589=CARTESIAN_POINT('Ctrl Pts',(-10.1189050443,-36.3112466293,3.13817229103));
#69590=CARTESIAN_POINT('Ctrl Pts',(-10.0401835634,-36.2742356128,3.08624397291));
#69591=CARTESIAN_POINT('Ctrl Pts',(-9.9614620825,-36.2742356128,3.0343156548));
#69592=CARTESIAN_POINT('Ctrl Pts',(-10.0867279364,-36.5742356128,3.38639921292));
#69593=CARTESIAN_POINT('Ctrl Pts',(-10.0867279138,-36.4799877817,3.38639925793));
#69594=CARTESIAN_POINT('Ctrl Pts',(-10.056625897,-36.3857399505,3.36477264615));
#69595=CARTESIAN_POINT('Ctrl Pts',(-9.99603849534,-36.3112465078,3.32124392015));
#69596=CARTESIAN_POINT('Ctrl Pts',(-9.91938440381,-36.2742355318,3.26617212038));
#69597=CARTESIAN_POINT('Ctrl Pts',(-9.84273034735,-36.2742356128,3.21110032106));
#69598=CARTESIAN_POINT('Ctrl Pts',(-9.94731298405,-36.5742356128,3.57262583962));
#69599=CARTESIAN_POINT('Ctrl Pts',(-9.94731297208,-36.4799878487,3.57262583568));
#69600=CARTESIAN_POINT('Ctrl Pts',(-9.91847739878,-36.3857400847,3.54921512866));
#69601=CARTESIAN_POINT('Ctrl Pts',(-9.86043899652,-36.3112466659,3.50209555723));
#69602=CARTESIAN_POINT('Ctrl Pts',(-9.78700982899,-36.2742356372,3.44248069278));
#69603=CARTESIAN_POINT('Ctrl Pts',(-9.7135806598,-36.2742356128,3.38286582323));
#69604=CARTESIAN_POINT('Ctrl Pts',(-9.66551121862,-36.5742356128,3.88595497216));
#69605=CARTESIAN_POINT('Ctrl Pts',(-9.66551122768,-36.4799878215,3.88595497515));
#69606=CARTESIAN_POINT('Ctrl Pts',(-9.63981184426,-36.3857400301,3.85895077503));
#69607=CARTESIAN_POINT('Ctrl Pts',(-9.58808574642,-36.3112466017,3.80459843069));
#69608=CARTESIAN_POINT('Ctrl Pts',(-9.52264278801,-36.2742355944,3.73583279562));
#69609=CARTESIAN_POINT('Ctrl Pts',(-9.45719983084,-36.2742356128,3.66706716442));
#69610=CARTESIAN_POINT('Ctrl Pts',(-9.3190883522,-36.5742356128,4.15054175699));
#69611=CARTESIAN_POINT('Ctrl Pts',(-9.31908834533,-36.4799878421,4.15054175473));
#69612=CARTESIAN_POINT('Ctrl Pts',(-9.29825794524,-36.3857400714,4.11976487501));
#69613=CARTESIAN_POINT('Ctrl Pts',(-9.2563318491,-36.3112466503,4.05781912505));
#69614=CARTESIAN_POINT('Ctrl Pts',(-9.20328768523,-36.2742356268,3.97944644413));
#69615=CARTESIAN_POINT('Ctrl Pts',(-9.15024352041,-36.2742356128,3.9010737603));
#69616=CARTESIAN_POINT('Ctrl Pts',(-9.15760248753,-36.5742356128,4.25148215543));
#69617=CARTESIAN_POINT('Ctrl Pts',(-9.15760248541,-36.4799878223,4.2514821194));
#69618=CARTESIAN_POINT('Ctrl Pts',(-9.13915536063,-36.3857400317,4.2191945066));
#69619=CARTESIAN_POINT('Ctrl Pts',(-9.10202619378,-36.3112466035,4.15420811433));
#69620=CARTESIAN_POINT('Ctrl Pts',(-9.05505101001,-36.2742355956,4.07198848278));
#69621=CARTESIAN_POINT('Ctrl Pts',(-9.00807582956,-36.2742356128,3.98976887128));
#69622=CARTESIAN_POINT('Ctrl Pts',(-8.57636643433,-36.5742356128,4.53983021603));
#69623=CARTESIAN_POINT('Ctrl Pts',(-8.57636643948,-36.4799878598,4.53983030324));
#69624=CARTESIAN_POINT('Ctrl Pts',(-8.56686869878,-36.3857401067,4.50309713161));
#69625=CARTESIAN_POINT('Ctrl Pts',(-8.54775216416,-36.3112466919,4.42916277982));
#69626=CARTESIAN_POINT('Ctrl Pts',(-8.52356628354,-36.2742356545,4.33562228694));
#69627=CARTESIAN_POINT('Ctrl Pts',(-8.49938039487,-36.2742356128,4.24208174555));
#69628=CARTESIAN_POINT('Ctrl Pts',(-7.90756140161,-36.5742356128,4.62319204336));
#69629=CARTESIAN_POINT('Ctrl Pts',(-7.90756138915,-36.479987769,4.62319183227));
#69630=CARTESIAN_POINT('Ctrl Pts',(-7.90907281157,-36.3857399251,4.58492140719));
#69631=CARTESIAN_POINT('Ctrl Pts',(-7.91211511531,-36.3112464779,4.50789350029));
#69632=CARTESIAN_POINT('Ctrl Pts',(-7.91596412286,-36.2742355119,4.41043924037));
#69633=CARTESIAN_POINT('Ctrl Pts',(-7.91981314987,-36.2742356128,4.31298509787));
#69634=CARTESIAN_POINT('Ctrl Pts',(-7.427051153,-36.5742356128,4.54976665456));
#69635=CARTESIAN_POINT('Ctrl Pts',(-7.42705185339,-36.4799878489,4.54976712257));
#69636=CARTESIAN_POINT('Ctrl Pts',(-7.43643206769,-36.3857400849,4.512928851));
#69637=CARTESIAN_POINT('Ctrl Pts',(-7.4553103639,-36.3112466662,4.43878203837));
#69638=CARTESIAN_POINT('Ctrl Pts',(-7.47919473941,-36.2742356374,4.34497270415));
#69639=CARTESIAN_POINT('Ctrl Pts',(-7.50307884797,-36.2742356128,4.25116318014));
#69640=CARTESIAN_POINT('Ctrl Pts',(-6.99795842984,-36.5742356128,4.37046697706));
#69641=CARTESIAN_POINT('Ctrl Pts',(-6.99795797817,-36.4799878293,4.37046667454));
#69642=CARTESIAN_POINT('Ctrl Pts',(-7.01351947686,-36.3857400458,4.33635407281));
#69643=CARTESIAN_POINT('Ctrl Pts',(-7.04484172418,-36.3112466201,4.26769510081));
#69644=CARTESIAN_POINT('Ctrl Pts',(-7.08447015303,-36.2742356067,4.18082901477));
#69645=CARTESIAN_POINT('Ctrl Pts',(-7.1240987555,-36.2742356128,4.09396304787));
#69646=CARTESIAN_POINT('Ctrl Pts',(-6.62478625212,-36.5742356128,4.12129355731));
#69647=CARTESIAN_POINT('Ctrl Pts',(-6.6247862495,-36.4799878332,4.12129355555));
#69648=CARTESIAN_POINT('Ctrl Pts',(-6.64533862663,-36.3857400536,4.0905134461));
#69649=CARTESIAN_POINT('Ctrl Pts',(-6.68670514971,-36.3112466293,4.02856119812));
#69650=CARTESIAN_POINT('Ctrl Pts',(-6.73904135397,-36.2742356128,3.95018029684));
#69651=CARTESIAN_POINT('Ctrl Pts',(-6.79137755926,-36.2742356128,3.87179939627));
#69652=CARTESIAN_POINT('',(-10.3257952821,-36.5742356128,3.01322822759));
#69653=CARTESIAN_POINT('Origin',(-10.0715345021286,-36.5721143191909,2.85804066652907));
#69654=CARTESIAN_POINT('Ctrl Pts',(-10.3257952821,-36.5742356128,3.01322822759));
#69655=CARTESIAN_POINT('Ctrl Pts',(-10.24741676,-36.5742356128,3.14164655991));
#69656=CARTESIAN_POINT('Ctrl Pts',(-10.163703376,-36.5742356128,3.27006200044));
#69657=CARTESIAN_POINT('Ctrl Pts',(-10.0727130885,-36.5742356128,3.39989142333));
#69658=CARTESIAN_POINT('Ctrl Pts',(-9.92328269257,-36.5742356128,3.5920488793));
#69659=CARTESIAN_POINT('Ctrl Pts',(-9.75297759192,-36.5742356128,3.77433260224));
#69660=CARTESIAN_POINT('Ctrl Pts',(-9.69216005671,-36.5742356128,3.83525523444));
#69661=CARTESIAN_POINT('Ctrl Pts',(-9.50104385577,-36.5742356128,4.01328807602));
#69662=CARTESIAN_POINT('Ctrl Pts',(-9.28446203337,-36.5742356128,4.17257256592));
#69663=CARTESIAN_POINT('Ctrl Pts',(-9.12906626269,-36.5742356128,4.26637622783));
#69664=CARTESIAN_POINT('Ctrl Pts',(-8.80081499429,-36.5742356128,4.42491856124));
#69665=CARTESIAN_POINT('Ctrl Pts',(-8.44551261186,-36.5742356128,4.51817058272));
#69666=CARTESIAN_POINT('Ctrl Pts',(-8.26232955523,-36.5742356128,4.54692356056));
#69667=CARTESIAN_POINT('Ctrl Pts',(-7.98526439172,-36.5742356128,4.56199873534));
#69668=CARTESIAN_POINT('Ctrl Pts',(-7.71036083894,-36.5742356128,4.53610818987));
#69669=CARTESIAN_POINT('Ctrl Pts',(-7.61904353259,-36.5742356128,4.52294971153));
#69670=CARTESIAN_POINT('Ctrl Pts',(-7.35028595871,-36.5742356128,4.47075138071));
#69671=CARTESIAN_POINT('Ctrl Pts',(-7.09318322917,-36.5742356128,4.3815910145));
#69672=CARTESIAN_POINT('Ctrl Pts',(-6.92865784201,-36.5742356128,4.30723684413));
#69673=CARTESIAN_POINT('Ctrl Pts',(-6.77209862643,-36.5742356128,4.21965690596));
#69674=CARTESIAN_POINT('Ctrl Pts',(-6.62478636278,-36.5742356128,4.12129363314));
#69675=CARTESIAN_POINT('Ctrl Pts',(-6.79137909539,-38.2742356128,3.87180043587));
#69676=CARTESIAN_POINT('Ctrl Pts',(-6.73904267861,-38.2742356128,3.95018119693));
#69677=CARTESIAN_POINT('Ctrl Pts',(-6.68670626183,-38.2372245963,4.02856195799));
#69678=CARTESIAN_POINT('Ctrl Pts',(-6.64533956952,-38.1627311721,4.0905140943));
#69679=CARTESIAN_POINT('Ctrl Pts',(-6.62478710671,-38.0684833924,4.12129414719));
#69680=CARTESIAN_POINT('Ctrl Pts',(-6.62478710671,-37.9742356128,4.12129414719));
#69681=CARTESIAN_POINT('Ctrl Pts',(-7.1049579039,-38.2742356128,4.08118318573));
#69682=CARTESIAN_POINT('Ctrl Pts',(-7.06458024318,-38.2742356128,4.16754907896));
#69683=CARTESIAN_POINT('Ctrl Pts',(-7.02420258246,-38.2372245963,4.2539149722));
#69684=CARTESIAN_POINT('Ctrl Pts',(-6.99228789916,-38.1627311721,4.32217842764));
#69685=CARTESIAN_POINT('Ctrl Pts',(-6.97643181802,-38.0684833924,4.35609436218));
#69686=CARTESIAN_POINT('Ctrl Pts',(-6.97643181802,-37.9742356128,4.35609436218));
#69687=CARTESIAN_POINT('Ctrl Pts',(-7.45951427977,-38.2742356128,4.2326662718));
#69688=CARTESIAN_POINT('Ctrl Pts',(-7.43382029577,-38.2742356128,4.32566174563));
#69689=CARTESIAN_POINT('Ctrl Pts',(-7.40812631176,-38.2372245963,4.41865721947));
#69690=CARTESIAN_POINT('Ctrl Pts',(-7.38781807594,-38.1627311721,4.49216101308));
#69691=CARTESIAN_POINT('Ctrl Pts',(-7.37772778853,-38.0684833924,4.52868005872));
#69692=CARTESIAN_POINT('Ctrl Pts',(-7.37772778853,-37.9742356128,4.52868005872));
#69693=CARTESIAN_POINT('Ctrl Pts',(-7.84730605121,-38.2742356128,4.30154970059));
#69694=CARTESIAN_POINT('Ctrl Pts',(-7.84002374033,-38.2742356128,4.39837872821));
#69695=CARTESIAN_POINT('Ctrl Pts',(-7.83274142945,-38.2372245963,4.49520775584));
#69696=CARTESIAN_POINT('Ctrl Pts',(-7.82698541779,-38.1627311721,4.57174135372));
#69697=CARTESIAN_POINT('Ctrl Pts',(-7.82412573574,-38.0684833924,4.60976606821));
#69698=CARTESIAN_POINT('Ctrl Pts',(-7.82412573574,-37.9742356128,4.60976606821));
#69699=CARTESIAN_POINT('Ctrl Pts',(-8.42919235133,-38.2742356128,4.25742949913));
#69700=CARTESIAN_POINT('Ctrl Pts',(-8.44994916242,-38.2742356128,4.35179273091));
#69701=CARTESIAN_POINT('Ctrl Pts',(-8.4707059735,-38.2372245963,4.4461559627));
#69702=CARTESIAN_POINT('Ctrl Pts',(-8.4871121894,-38.1627311721,4.52074066283));
#69703=CARTESIAN_POINT('Ctrl Pts',(-8.49526333308,-38.0684833924,4.55779699483));
#69704=CARTESIAN_POINT('Ctrl Pts',(-8.49526333308,-37.9742356128,4.55779699483));
#69705=CARTESIAN_POINT('Ctrl Pts',(-8.948859956,-38.2742356128,4.02576580976));
#69706=CARTESIAN_POINT('Ctrl Pts',(-8.99328098916,-38.2742356128,4.10956686635));
#69707=CARTESIAN_POINT('Ctrl Pts',(-9.03770202233,-38.2372245963,4.19336792295));
#69708=CARTESIAN_POINT('Ctrl Pts',(-9.07281237888,-38.1627311721,4.25960424824));
#69709=CARTESIAN_POINT('Ctrl Pts',(-9.0902564961,-38.0684833924,4.29251285762));
#69710=CARTESIAN_POINT('Ctrl Pts',(-9.0902564961,-37.9742356128,4.29251285762));
#69711=CARTESIAN_POINT('Ctrl Pts',(-9.11396067931,-38.2742356128,3.92853263445));
#69712=CARTESIAN_POINT('Ctrl Pts',(-9.16552913778,-38.2742356128,4.00804487662));
#69713=CARTESIAN_POINT('Ctrl Pts',(-9.21709759625,-38.2372245963,4.0875571188));
#69714=CARTESIAN_POINT('Ctrl Pts',(-9.2578573361,-38.1627311721,4.1504035075));
#69715=CARTESIAN_POINT('Ctrl Pts',(-9.27810818078,-38.0684833924,4.18162796201));
#69716=CARTESIAN_POINT('Ctrl Pts',(-9.27810818078,-37.9742356128,4.18162796201));
#69717=CARTESIAN_POINT('Ctrl Pts',(-9.44245605888,-38.2742356128,3.68354837841));
#69718=CARTESIAN_POINT('Ctrl Pts',(-9.50744911367,-38.2742356128,3.7528343336));
#69719=CARTESIAN_POINT('Ctrl Pts',(-9.57244216847,-38.2372245963,3.82212028879));
#69720=CARTESIAN_POINT('Ctrl Pts',(-9.62381261275,-38.1627311721,3.87688397742));
#69721=CARTESIAN_POINT('Ctrl Pts',(-9.64933537762,-38.0684833924,3.90409242352));
#69722=CARTESIAN_POINT('Ctrl Pts',(-9.64933537762,-37.9742356128,3.90409242352));
#69723=CARTESIAN_POINT('Ctrl Pts',(-9.71422494881,-38.2742356128,3.38199158831));
#69724=CARTESIAN_POINT('Ctrl Pts',(-9.78766313637,-38.2742356128,3.44159039714));
#69725=CARTESIAN_POINT('Ctrl Pts',(-9.86110132392,-38.2372245963,3.50118920597));
#69726=CARTESIAN_POINT('Ctrl Pts',(-9.91914691568,-38.1627311721,3.54829598872));
#69727=CARTESIAN_POINT('Ctrl Pts',(-9.94798596003,-38.0684833924,3.57170048887));
#69728=CARTESIAN_POINT('Ctrl Pts',(-9.94798596003,-37.9742356128,3.57170048887));
#69729=CARTESIAN_POINT('Ctrl Pts',(-9.84307440206,-38.2742356128,3.21058575408));
#69730=CARTESIAN_POINT('Ctrl Pts',(-9.91972289161,-38.2742356128,3.26565161277));
#69731=CARTESIAN_POINT('Ctrl Pts',(-9.99637138116,-38.2372245963,3.32071747146));
#69732=CARTESIAN_POINT('Ctrl Pts',(-10.0569540934,-38.1627311721,3.36424190319));
#69733=CARTESIAN_POINT('Ctrl Pts',(-10.0870541219,-38.0684833924,3.3858658262));
#69734=CARTESIAN_POINT('Ctrl Pts',(-10.0870541219,-37.9742356128,3.3858658262));
#69735=CARTESIAN_POINT('Ctrl Pts',(-9.96162763734,-38.2742356128,3.03404440349));
#69736=CARTESIAN_POINT('Ctrl Pts',(-10.0403517579,-38.2742356128,3.08596839674));
#69737=CARTESIAN_POINT('Ctrl Pts',(-10.1190758784,-38.2372245963,3.13789239));
#69738=CARTESIAN_POINT('Ctrl Pts',(-10.181299565,-38.1627311721,3.17893284235));
#69739=CARTESIAN_POINT('Ctrl Pts',(-10.2122142958,-38.0684833924,3.19932360733));
#69740=CARTESIAN_POINT('Ctrl Pts',(-10.2122142958,-37.9742356128,3.19932360733));
#69741=CARTESIAN_POINT('Ctrl Pts',(-10.0697226274,-38.2742356128,2.85693748721));
#69742=CARTESIAN_POINT('Ctrl Pts',(-10.1501702245,-38.2742356128,2.90603767139));
#69743=CARTESIAN_POINT('Ctrl Pts',(-10.2306178216,-38.2372245963,2.95513785557));
#69744=CARTESIAN_POINT('Ctrl Pts',(-10.2942035846,-38.1627311721,2.99394663035));
#69745=CARTESIAN_POINT('Ctrl Pts',(-10.3257952821,-38.0684833924,3.01322822759));
#69746=CARTESIAN_POINT('Ctrl Pts',(-10.3257952821,-37.9742356128,3.01322822759));
#69747=CARTESIAN_POINT('',(-10.3257952821,-37.9742356128,3.01322822759));
#69748=CARTESIAN_POINT('Origin',(-10.0715328873088,-37.9763569037572,2.85804330597835));
#69749=CARTESIAN_POINT('Ctrl Pts',(-10.3257952821,-37.9742356128,3.01322822759));
#69750=CARTESIAN_POINT('Ctrl Pts',(-10.24741676,-37.9742356128,3.14164655991));
#69751=CARTESIAN_POINT('Ctrl Pts',(-10.163703376,-37.9742356128,3.27006200044));
#69752=CARTESIAN_POINT('Ctrl Pts',(-10.0727130885,-37.9742356128,3.39989142333));
#69753=CARTESIAN_POINT('Ctrl Pts',(-9.92328269257,-37.9742356128,3.5920488793));
#69754=CARTESIAN_POINT('Ctrl Pts',(-9.75297759192,-37.9742356128,3.77433260224));
#69755=CARTESIAN_POINT('Ctrl Pts',(-9.69216005671,-37.9742356128,3.83525523444));
#69756=CARTESIAN_POINT('Ctrl Pts',(-9.50104385577,-37.9742356128,4.01328807602));
#69757=CARTESIAN_POINT('Ctrl Pts',(-9.28446203337,-37.9742356128,4.17257256592));
#69758=CARTESIAN_POINT('Ctrl Pts',(-9.12906626269,-37.9742356128,4.26637622783));
#69759=CARTESIAN_POINT('Ctrl Pts',(-8.80081499429,-37.9742356128,4.42491856124));
#69760=CARTESIAN_POINT('Ctrl Pts',(-8.44551261186,-37.9742356128,4.51817058272));
#69761=CARTESIAN_POINT('Ctrl Pts',(-8.26232955523,-37.9742356128,4.54692356056));
#69762=CARTESIAN_POINT('Ctrl Pts',(-7.98526439172,-37.9742356128,4.56199873534));
#69763=CARTESIAN_POINT('Ctrl Pts',(-7.71036083894,-37.9742356128,4.53610818987));
#69764=CARTESIAN_POINT('Ctrl Pts',(-7.61904353259,-37.9742356128,4.52294971153));
#69765=CARTESIAN_POINT('Ctrl Pts',(-7.35028595871,-37.9742356128,4.47075138071));
#69766=CARTESIAN_POINT('Ctrl Pts',(-7.09318322917,-37.9742356128,4.3815910145));
#69767=CARTESIAN_POINT('Ctrl Pts',(-6.92865784201,-37.9742356128,4.30723684413));
#69768=CARTESIAN_POINT('Ctrl Pts',(-6.77209862643,-37.9742356128,4.21965690596));
#69769=CARTESIAN_POINT('Ctrl Pts',(-6.62478636278,-37.9742356128,4.12129363314));
#69770=CARTESIAN_POINT('Ctrl Pts',(-6.62478636278,-37.9742356128,4.12129363314));
#69771=CARTESIAN_POINT('Ctrl Pts',(-6.62478636278,-36.2942356128,4.12129363314));
#69772=CARTESIAN_POINT('Ctrl Pts',(-6.77209862643,-37.9742356128,4.21965690596));
#69773=CARTESIAN_POINT('Ctrl Pts',(-6.77209862643,-36.2942356128,4.21965690596));
#69774=CARTESIAN_POINT('Ctrl Pts',(-6.92865784201,-37.9742356128,4.30723684413));
#69775=CARTESIAN_POINT('Ctrl Pts',(-6.92865784201,-36.2942356128,4.30723684413));
#69776=CARTESIAN_POINT('Ctrl Pts',(-7.09318322917,-37.9742356128,4.3815910145));
#69777=CARTESIAN_POINT('Ctrl Pts',(-7.09318322917,-36.2942356128,4.3815910145));
#69778=CARTESIAN_POINT('Ctrl Pts',(-7.35028595871,-37.9742356128,4.47075138071));
#69779=CARTESIAN_POINT('Ctrl Pts',(-7.35028595871,-36.2942356128,4.47075138071));
#69780=CARTESIAN_POINT('Ctrl Pts',(-7.61904353259,-37.9742356128,4.52294971153));
#69781=CARTESIAN_POINT('Ctrl Pts',(-7.61904353259,-36.2942356128,4.52294971153));
#69782=CARTESIAN_POINT('Ctrl Pts',(-7.71036083894,-37.9742356128,4.53610818987));
#69783=CARTESIAN_POINT('Ctrl Pts',(-7.71036083894,-36.2942356128,4.53610818987));
#69784=CARTESIAN_POINT('Ctrl Pts',(-7.98526439172,-37.9742356128,4.56199873534));
#69785=CARTESIAN_POINT('Ctrl Pts',(-7.98526439172,-36.2942356128,4.56199873534));
#69786=CARTESIAN_POINT('Ctrl Pts',(-8.26232955523,-37.9742356128,4.54692356056));
#69787=CARTESIAN_POINT('Ctrl Pts',(-8.26232955523,-36.2942356128,4.54692356056));
#69788=CARTESIAN_POINT('Ctrl Pts',(-8.44551261186,-37.9742356128,4.51817058272));
#69789=CARTESIAN_POINT('Ctrl Pts',(-8.44551261186,-36.2942356128,4.51817058272));
#69790=CARTESIAN_POINT('Ctrl Pts',(-8.80081499429,-37.9742356128,4.42491856124));
#69791=CARTESIAN_POINT('Ctrl Pts',(-8.80081499429,-36.2942356128,4.42491856124));
#69792=CARTESIAN_POINT('Ctrl Pts',(-9.12906626269,-37.9742356128,4.26637622783));
#69793=CARTESIAN_POINT('Ctrl Pts',(-9.12906626269,-36.2942356128,4.26637622783));
#69794=CARTESIAN_POINT('Ctrl Pts',(-9.28446203337,-37.9742356128,4.17257256592));
#69795=CARTESIAN_POINT('Ctrl Pts',(-9.28446203337,-36.2942356128,4.17257256592));
#69796=CARTESIAN_POINT('Ctrl Pts',(-9.50104385577,-37.9742356128,4.01328807602));
#69797=CARTESIAN_POINT('Ctrl Pts',(-9.50104385577,-36.2942356128,4.01328807602));
#69798=CARTESIAN_POINT('Ctrl Pts',(-9.69216005671,-37.9742356128,3.83525523444));
#69799=CARTESIAN_POINT('Ctrl Pts',(-9.69216005671,-36.2942356128,3.83525523444));
#69800=CARTESIAN_POINT('Ctrl Pts',(-9.75297759192,-37.9742356128,3.77433260224));
#69801=CARTESIAN_POINT('Ctrl Pts',(-9.75297759192,-36.2942356128,3.77433260224));
#69802=CARTESIAN_POINT('Ctrl Pts',(-9.92328269257,-37.9742356128,3.5920488793));
#69803=CARTESIAN_POINT('Ctrl Pts',(-9.92328269257,-36.2942356128,3.5920488793));
#69804=CARTESIAN_POINT('Ctrl Pts',(-10.0727130885,-37.9742356128,3.39989142333));
#69805=CARTESIAN_POINT('Ctrl Pts',(-10.0727130885,-36.2942356128,3.39989142333));
#69806=CARTESIAN_POINT('Ctrl Pts',(-10.163703376,-37.9742356128,3.27006200044));
#69807=CARTESIAN_POINT('Ctrl Pts',(-10.163703376,-36.2942356128,3.27006200044));
#69808=CARTESIAN_POINT('Ctrl Pts',(-10.24741676,-37.9742356128,3.14164655991));
#69809=CARTESIAN_POINT('Ctrl Pts',(-10.24741676,-36.2942356128,3.14164655991));
#69810=CARTESIAN_POINT('Ctrl Pts',(-10.3257952821,-37.9742356128,3.01322822759));
#69811=CARTESIAN_POINT('Ctrl Pts',(-10.3257952821,-36.2942356128,3.01322822759));
#69812=CARTESIAN_POINT('',(-10.3257952821,-37.2742356128,3.01322822759));
#69813=CARTESIAN_POINT('Ctrl Pts',(-11.0450673741,-36.5742356128,0.800650704934));
#69814=CARTESIAN_POINT('Ctrl Pts',(-11.0450673741,-36.4799878332,0.800650704934));
#69815=CARTESIAN_POINT('Ctrl Pts',(-11.008502755,-36.3857400536,0.794919738554));
#69816=CARTESIAN_POINT('Ctrl Pts',(-10.9349078112,-36.3112466293,0.783384813269));
#69817=CARTESIAN_POINT('Ctrl Pts',(-10.8417967734,-36.2742356128,0.768791027219));
#69818=CARTESIAN_POINT('Ctrl Pts',(-10.7486857355,-36.2742356128,0.75419724117));
#69819=CARTESIAN_POINT('Ctrl Pts',(-11.0356958718,-36.5742356128,0.860442612609));
#69820=CARTESIAN_POINT('Ctrl Pts',(-11.0356958718,-36.4799878332,0.860442612609));
#69821=CARTESIAN_POINT('Ctrl Pts',(-10.9991532809,-36.3857400536,0.854571102129));
#69822=CARTESIAN_POINT('Ctrl Pts',(-10.9256026745,-36.3112466293,0.842753296288));
#69823=CARTESIAN_POINT('Ctrl Pts',(-10.8325477313,-36.2742356128,0.827801615647));
#69824=CARTESIAN_POINT('Ctrl Pts',(-10.7394927882,-36.2742356128,0.812849935018));
#69825=CARTESIAN_POINT('Ctrl Pts',(-11.026134227,-36.5742356128,0.919561027699));
#69826=CARTESIAN_POINT('Ctrl Pts',(-11.0261342139,-36.4799878338,0.919561111138));
#69827=CARTESIAN_POINT('Ctrl Pts',(-10.9896137808,-36.3857400548,0.913553049122));
#69828=CARTESIAN_POINT('Ctrl Pts',(-10.9161077872,-36.3112466308,0.901460304345));
#69829=CARTESIAN_POINT('Ctrl Pts',(-10.8231092957,-36.2742356138,0.886160722879));
#69830=CARTESIAN_POINT('Ctrl Pts',(-10.7301108089,-36.2742356128,0.870861108564));
#69831=CARTESIAN_POINT('Ctrl Pts',(-11.0156765092,-36.5742356128,0.982678343196));
#69832=CARTESIAN_POINT('Ctrl Pts',(-11.0156765148,-36.4799878335,0.982678307492));
#69833=CARTESIAN_POINT('Ctrl Pts',(-10.9791715737,-36.3857400541,0.976578280666));
#69834=CARTESIAN_POINT('Ctrl Pts',(-10.9056967395,-36.3112466299,0.964300575476));
#69835=CARTESIAN_POINT('Ctrl Pts',(-10.8127376585,-36.2742356132,0.9487670598));
#69836=CARTESIAN_POINT('Ctrl Pts',(-10.7197785752,-36.2742356128,0.933233558116));
#69837=CARTESIAN_POINT('Ctrl Pts',(-10.9943063871,-36.5742356128,1.10902865463));
#69838=CARTESIAN_POINT('Ctrl Pts',(-10.9943063815,-36.479987833,1.10902869053));
#69839=CARTESIAN_POINT('Ctrl Pts',(-10.957836371,-36.3857400532,1.10271910297));
#69840=CARTESIAN_POINT('Ctrl Pts',(-10.884431856,-36.3112466288,1.0900195227));
#69841=CARTESIAN_POINT('Ctrl Pts',(-10.791561749,-36.2742356125,1.07395221337));
#69842=CARTESIAN_POINT('Ctrl Pts',(-10.6986916443,-36.2742356128,1.05788488998));
#69843=CARTESIAN_POINT('Ctrl Pts',(-10.9728702198,-36.5742356128,1.22868657788));
#69844=CARTESIAN_POINT('Ctrl Pts',(-10.9728702255,-36.4799878335,1.2286865418));
#69845=CARTESIAN_POINT('Ctrl Pts',(-10.9364628515,-36.3857400541,1.22202580029));
#69846=CARTESIAN_POINT('Ctrl Pts',(-10.8631843933,-36.3112466299,1.20861952714));
#69847=CARTESIAN_POINT('Ctrl Pts',(-10.7704737642,-36.2742356132,1.19165816618));
#69848=CARTESIAN_POINT('Ctrl Pts',(-10.6777631327,-36.2742356128,1.17469681936));
#69849=CARTESIAN_POINT('Ctrl Pts',(-10.9617509373,-36.5742356128,1.28871328879));
#69850=CARTESIAN_POINT('Ctrl Pts',(-10.9617509376,-36.4799878316,1.28871328613));
#69851=CARTESIAN_POINT('Ctrl Pts',(-10.9253775233,-36.3857400503,1.28186748201));
#69852=CARTESIAN_POINT('Ctrl Pts',(-10.8521674238,-36.3112466254,1.26808868559));
#69853=CARTESIAN_POINT('Ctrl Pts',(-10.7595432847,-36.2742356102,1.2506559946));
#69854=CARTESIAN_POINT('Ctrl Pts',(-10.6669191464,-36.2742356128,1.23322330483));
#69855=CARTESIAN_POINT('Ctrl Pts',(-10.9262749306,-36.5742356128,1.47265339473));
#69856=CARTESIAN_POINT('Ctrl Pts',(-10.9262749299,-36.4799878366,1.47265340004));
#69857=CARTESIAN_POINT('Ctrl Pts',(-10.8900377752,-36.3857400603,1.46509591619));
#69858=CARTESIAN_POINT('Ctrl Pts',(-10.8171019319,-36.3112466372,1.44988468551));
#69859=CARTESIAN_POINT('Ctrl Pts',(-10.7248247757,-36.2742356181,1.43063969881));
#69860=CARTESIAN_POINT('Ctrl Pts',(-10.6325476177,-36.2742356128,1.41139470965));
#69861=CARTESIAN_POINT('Ctrl Pts',(-10.8845365863,-36.5742356128,1.66051012485));
#69862=CARTESIAN_POINT('Ctrl Pts',(-10.8845365878,-36.4799878265,1.66051011422));
#69863=CARTESIAN_POINT('Ctrl Pts',(-10.8485236903,-36.3857400402,1.65192611838));
#69864=CARTESIAN_POINT('Ctrl Pts',(-10.7760392139,-36.3112466136,1.6346488105));
#69865=CARTESIAN_POINT('Ctrl Pts',(-10.6843331221,-36.2742356023,1.61278986878));
#69866=CARTESIAN_POINT('Ctrl Pts',(-10.5926270337,-36.2742356128,1.59093093198));
#69867=CARTESIAN_POINT('Ctrl Pts',(-10.8528256956,-36.5742356128,1.78779287908));
#69868=CARTESIAN_POINT('Ctrl Pts',(-10.8528257075,-36.4799878307,1.78779285781));
#69869=CARTESIAN_POINT('Ctrl Pts',(-10.8170223835,-36.3857400485,1.77834284407));
#69870=CARTESIAN_POINT('Ctrl Pts',(-10.7449597336,-36.3112466233,1.75932244652));
#69871=CARTESIAN_POINT('Ctrl Pts',(-10.6537873116,-36.2742356088,1.73525820021));
#69872=CARTESIAN_POINT('Ctrl Pts',(-10.5626148864,-36.2742356128,1.71119396292));
#69873=CARTESIAN_POINT('Ctrl Pts',(-10.7586931318,-36.5742356128,2.11943860448));
#69874=CARTESIAN_POINT('Ctrl Pts',(-10.758693113,-36.4799878373,2.11943863814));
#69875=CARTESIAN_POINT('Ctrl Pts',(-10.7235741006,-36.3857400617,2.10755898422));
#69876=CARTESIAN_POINT('Ctrl Pts',(-10.6528887702,-36.3112466389,2.08364838728));
#69877=CARTESIAN_POINT('Ctrl Pts',(-10.5634589492,-36.2742356192,2.05339707211));
#69878=CARTESIAN_POINT('Ctrl Pts',(-10.4740291333,-36.2742356128,2.02314574267));
#69879=CARTESIAN_POINT('Ctrl Pts',(-10.6310539149,-36.5742356128,2.44887196143));
#69880=CARTESIAN_POINT('Ctrl Pts',(-10.6310539447,-36.4799878268,2.44887190815));
#69881=CARTESIAN_POINT('Ctrl Pts',(-10.5970339308,-36.3857400409,2.43409852045));
#69882=CARTESIAN_POINT('Ctrl Pts',(-10.5285606254,-36.3112466143,2.40436355679));
#69883=CARTESIAN_POINT('Ctrl Pts',(-10.4419293559,-36.2742356028,2.36674347238));
#69884=CARTESIAN_POINT('Ctrl Pts',(-10.3552980782,-36.2742356128,2.32912341055));
#69885=CARTESIAN_POINT('Ctrl Pts',(-10.5407851495,-36.5742356128,2.64396902292));
#69886=CARTESIAN_POINT('Ctrl Pts',(-10.5407850384,-36.4799878442,2.64396920253));
#69887=CARTESIAN_POINT('Ctrl Pts',(-10.5075973283,-36.3857400755,2.62740472217));
#69888=CARTESIAN_POINT('Ctrl Pts',(-10.440799126,-36.3112466551,2.59406493039));
#69889=CARTESIAN_POINT('Ctrl Pts',(-10.3562873645,-36.27423563,2.55188374368));
#69890=CARTESIAN_POINT('Ctrl Pts',(-10.2717756404,-36.2742356128,2.50970248388));
#69891=CARTESIAN_POINT('Ctrl Pts',(-10.4329248475,-36.5742356128,2.83770348479));
#69892=CARTESIAN_POINT('Ctrl Pts',(-10.432924939,-36.4799878331,2.83770333584));
#69893=CARTESIAN_POINT('Ctrl Pts',(-10.4006746925,-36.3857400534,2.81950071793));
#69894=CARTESIAN_POINT('Ctrl Pts',(-10.3357634803,-36.3112466291,2.78286358468));
#69895=CARTESIAN_POINT('Ctrl Pts',(-10.2536388298,-36.2742356127,2.73651111612));
#69896=CARTESIAN_POINT('Ctrl Pts',(-10.1715141437,-36.2742356128,2.69015870569));
#69897=CARTESIAN_POINT('Ctrl Pts',(-10.3257953578,-36.5742356128,3.01322810549));
#69898=CARTESIAN_POINT('Ctrl Pts',(-10.3257953569,-36.4799878332,3.01322810703));
#69899=CARTESIAN_POINT('Ctrl Pts',(-10.2942037404,-36.3857400536,2.99394637711));
#69900=CARTESIAN_POINT('Ctrl Pts',(-10.2306181415,-36.3112466294,2.9551373334));
#69901=CARTESIAN_POINT('Ctrl Pts',(-10.1501707528,-36.2742356129,2.90603680802));
#69902=CARTESIAN_POINT('Ctrl Pts',(-10.0697233643,-36.2742356128,2.85693628205));
#69903=CARTESIAN_POINT('',(-11.0450673734813,-36.5742356128,0.800650704837023));
#69904=CARTESIAN_POINT('Origin',(-10.7507814379643,-36.5721143212036,0.754525737239802));
#69905=CARTESIAN_POINT('Ctrl Pts',(-11.0450673741,-36.5742356128,0.800650704934));
#69906=CARTESIAN_POINT('Ctrl Pts',(-11.0322998283,-36.5742356128,0.882109994357));
#69907=CARTESIAN_POINT('Ctrl Pts',(-11.0192230843,-36.5742356128,0.962056438391));
#69908=CARTESIAN_POINT('Ctrl Pts',(-11.0034487645,-36.5742356128,1.05599081));
#69909=CARTESIAN_POINT('Ctrl Pts',(-10.9747007144,-36.5742356128,1.22147170177));
#69910=CARTESIAN_POINT('Ctrl Pts',(-10.9420747597,-36.5742356128,1.39194060497));
#69911=CARTESIAN_POINT('Ctrl Pts',(-10.9239906907,-36.5742356128,1.48074082922));
#69912=CARTESIAN_POINT('Ctrl Pts',(-10.8740649015,-36.5742356128,1.70707199422));
#69913=CARTESIAN_POINT('Ctrl Pts',(-10.8111933802,-36.5742356128,1.9383801789));
#69914=CARTESIAN_POINT('Ctrl Pts',(-10.7670166783,-36.5742356128,2.08017125701));
#69915=CARTESIAN_POINT('Ctrl Pts',(-10.6667840474,-36.5742356128,2.35918484011));
#69916=CARTESIAN_POINT('Ctrl Pts',(-10.5420136,-36.5742356128,2.63031881231));
#69917=CARTESIAN_POINT('Ctrl Pts',(-10.4735263391,-36.5742356128,2.76337956772));
#69918=CARTESIAN_POINT('Ctrl Pts',(-10.3992001828,-36.5742356128,2.89295886461));
#69919=CARTESIAN_POINT('Ctrl Pts',(-10.3257952821,-36.5742356128,3.01322822759));
#69920=CARTESIAN_POINT('Ctrl Pts',(-10.0697223221,-38.2742356128,2.85693798735));
#69921=CARTESIAN_POINT('Ctrl Pts',(-10.1501700117,-38.2742356128,2.90603801994));
#69922=CARTESIAN_POINT('Ctrl Pts',(-10.2306177012,-38.2372245963,2.95513805253));
#69923=CARTESIAN_POINT('Ctrl Pts',(-10.2942035374,-38.1627311721,2.9939467075));
#69924=CARTESIAN_POINT('Ctrl Pts',(-10.3257952712,-38.0684833924,3.01322824521));
#69925=CARTESIAN_POINT('Ctrl Pts',(-10.3257952712,-37.9742356128,3.01322824521));
#69926=CARTESIAN_POINT('Ctrl Pts',(-10.1868233028,-38.2742356128,2.66507503056));
#69927=CARTESIAN_POINT('Ctrl Pts',(-10.2691930709,-38.2742356128,2.71102584437));
#69928=CARTESIAN_POINT('Ctrl Pts',(-10.3515628389,-38.2372245963,2.75697665817));
#69929=CARTESIAN_POINT('Ctrl Pts',(-10.4166677835,-38.1627311721,2.79329633777));
#69930=CARTESIAN_POINT('Ctrl Pts',(-10.4490144177,-38.0684833924,2.81134101369));
#69931=CARTESIAN_POINT('Ctrl Pts',(-10.4490144177,-37.9742356128,2.81134101369));
#69932=CARTESIAN_POINT('Ctrl Pts',(-10.301618245,-38.2742356128,2.45520417407));
#69933=CARTESIAN_POINT('Ctrl Pts',(-10.3868740365,-38.2742356128,2.49608900873));
#69934=CARTESIAN_POINT('Ctrl Pts',(-10.472129828,-38.2372245963,2.5369738434));
#69935=CARTESIAN_POINT('Ctrl Pts',(-10.5395161398,-38.1627311721,2.56928895818));
#69936=CARTESIAN_POINT('Ctrl Pts',(-10.5729958579,-38.0684833924,2.58534464476));
#69937=CARTESIAN_POINT('Ctrl Pts',(-10.5729958579,-37.9742356128,2.58534464476));
#69938=CARTESIAN_POINT('Ctrl Pts',(-10.3925251896,-38.2742356128,2.24714722347));
#69939=CARTESIAN_POINT('Ctrl Pts',(-10.4800958587,-38.2742356128,2.28265349733));
#69940=CARTESIAN_POINT('Ctrl Pts',(-10.5676665277,-38.2372245963,2.31815977119));
#69941=CARTESIAN_POINT('Ctrl Pts',(-10.6368823272,-38.1627311721,2.34622398605));
#69942=CARTESIAN_POINT('Ctrl Pts',(-10.6712712865,-38.0684833924,2.36016720339));
#69943=CARTESIAN_POINT('Ctrl Pts',(-10.6712712865,-37.9742356128,2.36016720339));
#69944=CARTESIAN_POINT('Ctrl Pts',(-10.4951845718,-38.2742356128,1.95707474872));
#69945=CARTESIAN_POINT('Ctrl Pts',(-10.5850671643,-38.2742356128,1.98585046507));
#69946=CARTESIAN_POINT('Ctrl Pts',(-10.6749497569,-38.2372245963,2.01462618141));
#69947=CARTESIAN_POINT('Ctrl Pts',(-10.7459929506,-38.1627311721,2.03737048094));
#69948=CARTESIAN_POINT('Ctrl Pts',(-10.7812897498,-38.0684833924,2.04867069867));
#69949=CARTESIAN_POINT('Ctrl Pts',(-10.7812897498,-37.9742356128,2.04867069867));
#69950=CARTESIAN_POINT('Ctrl Pts',(-10.5724029544,-38.2742356128,1.66744116868));
#69951=CARTESIAN_POINT('Ctrl Pts',(-10.6637262076,-38.2742356128,1.69079424142));
#69952=CARTESIAN_POINT('Ctrl Pts',(-10.7550494608,-38.2372245963,1.71414731415));
#69953=CARTESIAN_POINT('Ctrl Pts',(-10.8272313361,-38.1627311721,1.7326055842));
#69954=CARTESIAN_POINT('Ctrl Pts',(-10.8630938978,-38.0684833924,1.74177630792));
#69955=CARTESIAN_POINT('Ctrl Pts',(-10.8630938978,-37.9742356128,1.74177630792));
#69956=CARTESIAN_POINT('Ctrl Pts',(-10.5899310768,-38.2742356128,1.59685627097));
#69957=CARTESIAN_POINT('Ctrl Pts',(-10.6815562054,-38.2742356128,1.61898136728));
#69958=CARTESIAN_POINT('Ctrl Pts',(-10.7731813341,-38.2372245963,1.64110646359));
#69959=CARTESIAN_POINT('Ctrl Pts',(-10.8456018157,-38.1627311721,1.65859413501));
#69960=CARTESIAN_POINT('Ctrl Pts',(-10.8815829196,-38.0684833924,1.66728263986));
#69961=CARTESIAN_POINT('Ctrl Pts',(-10.8815829196,-37.9742356128,1.66728263986));
#69962=CARTESIAN_POINT('Ctrl Pts',(-10.6184801248,-38.2742356128,1.47356398205));
#69963=CARTESIAN_POINT('Ctrl Pts',(-10.7105472499,-38.2742356128,1.49376689715));
#69964=CARTESIAN_POINT('Ctrl Pts',(-10.802614375,-38.2372245963,1.51396981225));
#69965=CARTESIAN_POINT('Ctrl Pts',(-10.8753842104,-38.1627311721,1.52993819193));
#69966=CARTESIAN_POINT('Ctrl Pts',(-10.9115388859,-38.0684833924,1.53787185811));
#69967=CARTESIAN_POINT('Ctrl Pts',(-10.9115388859,-37.9742356128,1.53787185811));
#69968=CARTESIAN_POINT('Ctrl Pts',(-10.6439064683,-38.2742356128,1.35095545652));
#69969=CARTESIAN_POINT('Ctrl Pts',(-10.7362898376,-38.2742356128,1.36962561802));
#69970=CARTESIAN_POINT('Ctrl Pts',(-10.828673207,-38.2372245963,1.38829577952));
#69971=CARTESIAN_POINT('Ctrl Pts',(-10.9016930018,-38.1627311721,1.40305267094));
#69972=CARTESIAN_POINT('Ctrl Pts',(-10.9379718661,-38.0684833924,1.41038442635));
#69973=CARTESIAN_POINT('Ctrl Pts',(-10.9379718661,-37.9742356128,1.41038442635));
#69974=CARTESIAN_POINT('Ctrl Pts',(-10.6541976648,-38.2742356128,1.29920325109));
#69975=CARTESIAN_POINT('Ctrl Pts',(-10.7466984979,-38.2742356128,1.31727486189));
#69976=CARTESIAN_POINT('Ctrl Pts',(-10.8391993311,-38.2372245963,1.33534647269));
#69977=CARTESIAN_POINT('Ctrl Pts',(-10.9123119707,-38.1627311721,1.34963026042));
#69978=CARTESIAN_POINT('Ctrl Pts',(-10.9486369615,-38.0684833924,1.35672697486));
#69979=CARTESIAN_POINT('Ctrl Pts',(-10.9486369615,-37.9742356128,1.35672697486));
#69980=CARTESIAN_POINT('Ctrl Pts',(-10.6809317668,-38.2742356128,1.15917604429));
#69981=CARTESIAN_POINT('Ctrl Pts',(-10.7736762576,-38.2742356128,1.17597190018));
#69982=CARTESIAN_POINT('Ctrl Pts',(-10.8664207484,-38.2372245963,1.19276775608));
#69983=CARTESIAN_POINT('Ctrl Pts',(-10.9397259711,-38.1627311721,1.20604321247));
#69984=CARTESIAN_POINT('Ctrl Pts',(-10.9761466498,-38.0684833924,1.21263891407));
#69985=CARTESIAN_POINT('Ctrl Pts',(-10.9761466498,-37.9742356128,1.21263891407));
#69986=CARTESIAN_POINT('Ctrl Pts',(-10.7044770632,-38.2742356128,1.02478825138));
#69987=CARTESIAN_POINT('Ctrl Pts',(-10.7973834123,-38.2742356128,1.0406433192));
#69988=CARTESIAN_POINT('Ctrl Pts',(-10.8902897614,-38.2372245963,1.05649838701));
#69989=CARTESIAN_POINT('Ctrl Pts',(-10.9637229232,-38.1627311721,1.06903020348));
#69990=CARTESIAN_POINT('Ctrl Pts',(-11.0002071572,-38.0684833924,1.0752564997));
#69991=CARTESIAN_POINT('Ctrl Pts',(-11.0002071572,-37.9742356128,1.0752564997));
#69992=CARTESIAN_POINT('Ctrl Pts',(-10.7213509628,-38.2742356128,0.924627136137));
#69993=CARTESIAN_POINT('Ctrl Pts',(-10.8143014058,-38.2742356128,0.940218025264));
#69994=CARTESIAN_POINT('Ctrl Pts',(-10.9072518487,-38.2372245963,0.955808914391));
#69995=CARTESIAN_POINT('Ctrl Pts',(-10.9807198422,-38.1627311721,0.968132053039));
#69996=CARTESIAN_POINT('Ctrl Pts',(-11.017221412,-38.0684833924,0.974254477573));
#69997=CARTESIAN_POINT('Ctrl Pts',(-11.017221412,-37.9742356128,0.974254477573));
#69998=CARTESIAN_POINT('Ctrl Pts',(-10.7352098055,-38.2742356128,0.840176151798));
#69999=CARTESIAN_POINT('Ctrl Pts',(-10.8282386142,-38.2742356128,0.855294575063));
#70000=CARTESIAN_POINT('Ctrl Pts',(-10.9212674229,-38.2372245963,0.870412998329));
#70001=CARTESIAN_POINT('Ctrl Pts',(-10.9947973836,-38.1627311721,0.882362527918));
#70002=CARTESIAN_POINT('Ctrl Pts',(-11.0313297006,-38.0684833924,0.888299587687));
#70003=CARTESIAN_POINT('Ctrl Pts',(-11.0313297006,-37.9742356128,0.888299587687));
#70004=CARTESIAN_POINT('Ctrl Pts',(-10.7486857355,-38.2742356128,0.75419724117));
#70005=CARTESIAN_POINT('Ctrl Pts',(-10.8417967734,-38.2742356128,0.768791027219));
#70006=CARTESIAN_POINT('Ctrl Pts',(-10.9349078112,-38.2372245963,0.783384813269));
#70007=CARTESIAN_POINT('Ctrl Pts',(-11.008502755,-38.1627311721,0.794919738554));
#70008=CARTESIAN_POINT('Ctrl Pts',(-11.0450673741,-38.0684833924,0.800650704934));
#70009=CARTESIAN_POINT('Ctrl Pts',(-11.0450673741,-37.9742356128,0.800650704934));
#70010=CARTESIAN_POINT('',(-11.0450673741,-37.9742356128,0.800650704934));
#70011=CARTESIAN_POINT('Origin',(-10.750781440652,-37.9763569039346,0.754525717032591));
#70012=CARTESIAN_POINT('Ctrl Pts',(-11.0450673741,-37.9742356128,0.800650704934));
#70013=CARTESIAN_POINT('Ctrl Pts',(-11.043029714617,-37.9742356128,0.813651347081446));
#70014=CARTESIAN_POINT('Ctrl Pts',(-11.0409811405816,-37.9742356128,0.826614446398853));
#70015=CARTESIAN_POINT('Ctrl Pts',(-11.0389082501465,-37.9742356128,0.83962956698804));
#70016=CARTESIAN_POINT('Ctrl Pts',(-11.0367226177714,-37.9742356128,0.853352563844801));
#70017=CARTESIAN_POINT('Ctrl Pts',(-11.0345100122603,-37.9742356128,0.867133053722408));
#70018=CARTESIAN_POINT('Ctrl Pts',(-11.0322638259458,-37.9742356128,0.881017973437018));
#70019=CARTESIAN_POINT('Ctrl Pts',(-11.0298438478065,-37.9742356128,0.895977196525099));
#70020=CARTESIAN_POINT('Ctrl Pts',(-11.0273849786507,-37.9742356128,0.911057150600489));
#70021=CARTESIAN_POINT('Ctrl Pts',(-11.0248881319546,-37.9742356128,0.926257079775398));
#70022=CARTESIAN_POINT('Ctrl Pts',(-11.0220231838727,-37.9742356128,0.943697881408424));
#70023=CARTESIAN_POINT('Ctrl Pts',(-11.0191083835626,-37.9742356128,0.961295875046121));
#70024=CARTESIAN_POINT('Ctrl Pts',(-11.0161550530303,-37.9742356128,0.978983247293589));
#70025=CARTESIAN_POINT('Ctrl Pts',(-11.0123390721258,-37.9742356128,1.00183699630861));
#70026=CARTESIAN_POINT('Ctrl Pts',(-11.0084595370333,-37.9742356128,1.02483590282602));
#70027=CARTESIAN_POINT('Ctrl Pts',(-11.004549929836,-37.9742356128,1.04776199688937));
#70028=CARTESIAN_POINT('Ctrl Pts',(-11.001617724438,-37.9742356128,1.06495656743688));
#70029=CARTESIAN_POINT('Ctrl Pts',(-10.9986689929647,-37.9742356128,1.08210742911664));
#70030=CARTESIAN_POINT('Ctrl Pts',(-10.9957140569788,-37.9742356128,1.09913879058753));
#70031=CARTESIAN_POINT('Ctrl Pts',(-10.993046538305,-37.9742356128,1.1145135651959));
#70032=CARTESIAN_POINT('Ctrl Pts',(-10.9903741100481,-37.9742356128,1.12978998947176));
#70033=CARTESIAN_POINT('Ctrl Pts',(-10.9876978418533,-37.9742356128,1.14494777879044));
#70034=CARTESIAN_POINT('Ctrl Pts',(-10.9851896023423,-37.9742356128,1.15915389092199));
#70035=CARTESIAN_POINT('Ctrl Pts',(-10.9826780825886,-37.9742356128,1.17325519845599));
#70036=CARTESIAN_POINT('Ctrl Pts',(-10.9801565078912,-37.9742356128,1.18727837430054));
#70037=CARTESIAN_POINT('Ctrl Pts',(-10.9781789138184,-37.9742356128,1.19827632310602));
#70038=CARTESIAN_POINT('Ctrl Pts',(-10.9761951318328,-37.9742356128,1.20922624618161));
#70039=CARTESIAN_POINT('Ctrl Pts',(-10.9741973505613,-37.9742356128,1.22016709300421));
#70040=CARTESIAN_POINT('Ctrl Pts',(-10.9724279672361,-37.9742356128,1.22985711873791));
#70041=CARTESIAN_POINT('Ctrl Pts',(-10.9706468302445,-37.9742356128,1.23954425009291));
#70042=CARTESIAN_POINT('Ctrl Pts',(-10.9688458050707,-37.9742356128,1.24927114147751));
#70043=CARTESIAN_POINT('Ctrl Pts',(-10.9658441595318,-37.9742356128,1.26548228641616));
#70044=CARTESIAN_POINT('Ctrl Pts',(-10.9627873829675,-37.9742356128,1.28180320816873));
#70045=CARTESIAN_POINT('Ctrl Pts',(-10.959680869317,-37.9742356128,1.29817179412848));
#70046=CARTESIAN_POINT('Ctrl Pts',(-10.9561464184371,-37.9742356128,1.31679523170439));
#70047=CARTESIAN_POINT('Ctrl Pts',(-10.952547477265,-37.9742356128,1.3354810217601));
#70048=CARTESIAN_POINT('Ctrl Pts',(-10.9488799948937,-37.9742356128,1.35420754643654));
#70049=CARTESIAN_POINT('Ctrl Pts',(-10.9435234773383,-37.9742356128,1.38155845041511));
#70050=CARTESIAN_POINT('Ctrl Pts',(-10.9380201984635,-37.9742356128,1.4089997435351));
#70051=CARTESIAN_POINT('Ctrl Pts',(-10.9323355373801,-37.9742356128,1.43658969318583));
#70052=CARTESIAN_POINT('Ctrl Pts',(-10.9283455568722,-37.9742356128,1.45595467549586));
#70053=CARTESIAN_POINT('Ctrl Pts',(-10.9242655286716,-37.9742356128,1.47539686828966));
#70054=CARTESIAN_POINT('Ctrl Pts',(-10.9200861694079,-37.9742356128,1.4949189254137));
#70055=CARTESIAN_POINT('Ctrl Pts',(-10.9183110532267,-37.9742356128,1.5032106077761));
#70056=CARTESIAN_POINT('Ctrl Pts',(-10.9165181002464,-37.9742356128,1.51151619372324));
#70057=CARTESIAN_POINT('Ctrl Pts',(-10.9147071085259,-37.9742356128,1.51983280126634));
#70058=CARTESIAN_POINT('Ctrl Pts',(-10.9058971470908,-37.9742356128,1.56029073980552));
#70059=CARTESIAN_POINT('Ctrl Pts',(-10.8966600534637,-37.9742356128,1.60100258738621));
#70060=CARTESIAN_POINT('Ctrl Pts',(-10.8869322989095,-37.9742356128,1.64190711298157));
#70061=CARTESIAN_POINT('Ctrl Pts',(-10.8816541363127,-37.9742356128,1.66410141649091));
#70062=CARTESIAN_POINT('Ctrl Pts',(-10.876231590757,-37.9742356128,1.68635379921446));
#70063=CARTESIAN_POINT('Ctrl Pts',(-10.8706519617309,-37.9742356128,1.70866956482949));
#70064=CARTESIAN_POINT('Ctrl Pts',(-10.8566733630686,-37.9742356128,1.76457706870001));
#70065=CARTESIAN_POINT('Ctrl Pts',(-10.8417157749528,-37.9742356128,1.82086392811176));
#70066=CARTESIAN_POINT('Ctrl Pts',(-10.8256187306821,-37.9742356128,1.87740688019527));
#70067=CARTESIAN_POINT('Ctrl Pts',(-10.8242461843505,-37.9742356128,1.88222812688856));
#70068=CARTESIAN_POINT('Ctrl Pts',(-10.8228653339238,-37.9742356128,1.88705120681551));
#70069=CARTESIAN_POINT('Ctrl Pts',(-10.8214760666396,-37.9742356128,1.89187602345432));
#70070=CARTESIAN_POINT('Ctrl Pts',(-10.8097618302743,-37.9742356128,1.93255865031043));
#70071=CARTESIAN_POINT('Ctrl Pts',(-10.7974509858169,-37.9742356128,1.9733604688576));
#70072=CARTESIAN_POINT('Ctrl Pts',(-10.7845441296016,-37.9742356128,2.01414918818009));
#70073=CARTESIAN_POINT('Ctrl Pts',(-10.7702538208126,-37.9742356128,2.0593099449518));
#70074=CARTESIAN_POINT('Ctrl Pts',(-10.7552320337685,-37.9742356128,2.10445505521447));
#70075=CARTESIAN_POINT('Ctrl Pts',(-10.7394592387859,-37.9742356128,2.14946507846607));
#70076=CARTESIAN_POINT('Ctrl Pts',(-10.7259378847107,-37.9742356128,2.18805027924931));
#70077=CARTESIAN_POINT('Ctrl Pts',(-10.7118637692977,-37.9742356128,2.22653783742124));
#70078=CARTESIAN_POINT('Ctrl Pts',(-10.6972233120527,-37.9742356128,2.26487617500612));
#70079=CARTESIAN_POINT('Ctrl Pts',(-10.6877543902685,-37.9742356128,2.28967203444221));
#70080=CARTESIAN_POINT('Ctrl Pts',(-10.6780485763058,-37.9742356128,2.31440587708767));
#70081=CARTESIAN_POINT('Ctrl Pts',(-10.6681039614208,-37.9742356128,2.33906617952837));
#70082=CARTESIAN_POINT('Ctrl Pts',(-10.6597404312459,-37.9742356128,2.35980576431583));
#70083=CARTESIAN_POINT('Ctrl Pts',(-10.6512078054758,-37.9742356128,2.3804940542434));
#70084=CARTESIAN_POINT('Ctrl Pts',(-10.6425013497725,-37.9742356128,2.40113574775587));
#70085=CARTESIAN_POINT('Ctrl Pts',(-10.6241726688637,-37.9742356128,2.44459028616991));
#70086=CARTESIAN_POINT('Ctrl Pts',(-10.605076119422,-37.9742356128,2.48782579272503));
#70087=CARTESIAN_POINT('Ctrl Pts',(-10.5852407699418,-37.9742356128,2.53076593827548));
#70088=CARTESIAN_POINT('Ctrl Pts',(-10.5671928447555,-37.9742356128,2.56983661535895));
#70089=CARTESIAN_POINT('Ctrl Pts',(-10.5485330177449,-37.9742356128,2.60866350649996));
#70090=CARTESIAN_POINT('Ctrl Pts',(-10.5293221190785,-37.9742356128,2.64716762097847));
#70091=CARTESIAN_POINT('Ctrl Pts',(-10.511707986674,-37.9742356128,2.68247136091912));
#70092=CARTESIAN_POINT('Ctrl Pts',(-10.4936305798116,-37.9742356128,2.71750404672932));
#70093=CARTESIAN_POINT('Ctrl Pts',(-10.4751726224105,-37.9742356128,2.7521792368075));
#70094=CARTESIAN_POINT('Ctrl Pts',(-10.4573434347709,-37.9742356128,2.78567321758267));
#70095=CARTESIAN_POINT('Ctrl Pts',(-10.4391590047372,-37.9742356128,2.81883397269397));
#70096=CARTESIAN_POINT('Ctrl Pts',(-10.4207304827102,-37.9742356128,2.85155406272029));
#70097=CARTESIAN_POINT('Ctrl Pts',(-10.4030434198708,-37.9742356128,2.88295768193392));
#70098=CARTESIAN_POINT('Ctrl Pts',(-10.3851314693061,-37.9742356128,2.91395554916307));
#70099=CARTESIAN_POINT('Ctrl Pts',(-10.367128661443,-37.9742356128,2.94442155879934));
#70100=CARTESIAN_POINT('Ctrl Pts',(-10.3533782097523,-37.9742356128,2.96769133965221));
#70101=CARTESIAN_POINT('Ctrl Pts',(-10.3395754397378,-37.9742356128,2.99065025975012));
#70102=CARTESIAN_POINT('Ctrl Pts',(-10.3257952819937,-37.9742356128,3.01322822752513));
#70103=CARTESIAN_POINT('Ctrl Pts',(-10.3257952821,-37.9742356128,3.01322822759));
#70104=CARTESIAN_POINT('Ctrl Pts',(-10.3257952821,-36.2942356128,3.01322822759));
#70105=CARTESIAN_POINT('Ctrl Pts',(-10.3992001828,-37.9742356128,2.89295886461));
#70106=CARTESIAN_POINT('Ctrl Pts',(-10.3992001828,-36.2942356128,2.89295886461));
#70107=CARTESIAN_POINT('Ctrl Pts',(-10.4735263391,-37.9742356128,2.76337956772));
#70108=CARTESIAN_POINT('Ctrl Pts',(-10.4735263391,-36.2942356128,2.76337956772));
#70109=CARTESIAN_POINT('Ctrl Pts',(-10.5420136,-37.9742356128,2.63031881231));
#70110=CARTESIAN_POINT('Ctrl Pts',(-10.5420136,-36.2942356128,2.63031881231));
#70111=CARTESIAN_POINT('Ctrl Pts',(-10.6667840474,-37.9742356128,2.35918484011));
#70112=CARTESIAN_POINT('Ctrl Pts',(-10.6667840474,-36.2942356128,2.35918484011));
#70113=CARTESIAN_POINT('Ctrl Pts',(-10.7670166783,-37.9742356128,2.08017125701));
#70114=CARTESIAN_POINT('Ctrl Pts',(-10.7670166783,-36.2942356128,2.08017125701));
#70115=CARTESIAN_POINT('Ctrl Pts',(-10.8111933802,-37.9742356128,1.9383801789));
#70116=CARTESIAN_POINT('Ctrl Pts',(-10.8111933802,-36.2942356128,1.9383801789));
#70117=CARTESIAN_POINT('Ctrl Pts',(-10.8740649015,-37.9742356128,1.70707199422));
#70118=CARTESIAN_POINT('Ctrl Pts',(-10.8740649015,-36.2942356128,1.70707199422));
#70119=CARTESIAN_POINT('Ctrl Pts',(-10.9239906907,-37.9742356128,1.48074082922));
#70120=CARTESIAN_POINT('Ctrl Pts',(-10.9239906907,-36.2942356128,1.48074082922));
#70121=CARTESIAN_POINT('Ctrl Pts',(-10.9420747597,-37.9742356128,1.39194060497));
#70122=CARTESIAN_POINT('Ctrl Pts',(-10.9420747597,-36.2942356128,1.39194060497));
#70123=CARTESIAN_POINT('Ctrl Pts',(-10.9747007144,-37.9742356128,1.22147170177));
#70124=CARTESIAN_POINT('Ctrl Pts',(-10.9747007144,-36.2942356128,1.22147170177));
#70125=CARTESIAN_POINT('Ctrl Pts',(-11.0034487645,-37.9742356128,1.05599081));
#70126=CARTESIAN_POINT('Ctrl Pts',(-11.0034487645,-36.2942356128,1.05599081));
#70127=CARTESIAN_POINT('Ctrl Pts',(-11.0192230843,-37.9742356128,0.962056438391));
#70128=CARTESIAN_POINT('Ctrl Pts',(-11.0192230843,-36.2942356128,0.962056438391));
#70129=CARTESIAN_POINT('Ctrl Pts',(-11.0322998283,-37.9742356128,0.882109994357));
#70130=CARTESIAN_POINT('Ctrl Pts',(-11.0322998283,-36.2942356128,0.882109994357));
#70131=CARTESIAN_POINT('Ctrl Pts',(-11.0450673741,-37.9742356128,0.800650704934));
#70132=CARTESIAN_POINT('Ctrl Pts',(-11.0450673741,-36.2942356128,0.800650704934));
#70133=CARTESIAN_POINT('',(-11.0450673741,-37.2742356128,0.800650704934));
#70134=CARTESIAN_POINT('Ctrl Pts',(-1.38699292008,-36.5742356128,-10.1328356959));
#70135=CARTESIAN_POINT('Ctrl Pts',(-1.38699292008,-36.4799878332,-10.1328356959));
#70136=CARTESIAN_POINT('Ctrl Pts',(-1.38185951829,-36.3857400536,-10.0961824078));
#70137=CARTESIAN_POINT('Ctrl Pts',(-1.37152733308,-36.3112466293,-10.0224089965));
#70138=CARTESIAN_POINT('Ctrl Pts',(-1.35845523278,-36.2742356128,-9.92907216478));
#70139=CARTESIAN_POINT('Ctrl Pts',(-1.34538313247,-36.2742356128,-9.83573533307));
#70140=CARTESIAN_POINT('Ctrl Pts',(-1.51152029043,-36.5742356128,-10.1153952681));
#70141=CARTESIAN_POINT('Ctrl Pts',(-1.51152029043,-36.4799878332,-10.1153952681));
#70142=CARTESIAN_POINT('Ctrl Pts',(-1.50631651992,-36.3857400536,-10.0787518353));
#70143=CARTESIAN_POINT('Ctrl Pts',(-1.4958427008,-36.3112466293,-10.0049982603));
#70144=CARTESIAN_POINT('Ctrl Pts',(-1.48259140782,-36.2742356128,-9.91168652503));
#70145=CARTESIAN_POINT('Ctrl Pts',(-1.46934011484,-36.2742356128,-9.81837478978));
#70146=CARTESIAN_POINT('Ctrl Pts',(-1.63096792048,-36.5742356128,-10.098359414));
#70147=CARTESIAN_POINT('Ctrl Pts',(-1.63096797981,-36.4799878326,-10.0983594061));
#70148=CARTESIAN_POINT('Ctrl Pts',(-1.62565332197,-36.3857400523,-10.061731723));
#70149=CARTESIAN_POINT('Ctrl Pts',(-1.61495624423,-36.3112466278,-9.98800985755));
#70150=CARTESIAN_POINT('Ctrl Pts',(-1.60142245201,-36.2742356118,-9.89473824575));
#70151=CARTESIAN_POINT('Ctrl Pts',(-1.58788863653,-36.2742356128,-9.80146663746));
#70152=CARTESIAN_POINT('Ctrl Pts',(-1.75323704933,-36.5742356128,-10.0804678237));
#70153=CARTESIAN_POINT('Ctrl Pts',(-1.75323702948,-36.4799878327,-10.0804678262));
#70154=CARTESIAN_POINT('Ctrl Pts',(-1.74780800354,-36.3857400526,-10.0438567886));
#70155=CARTESIAN_POINT('Ctrl Pts',(-1.73688082988,-36.3112466281,-9.97016841334));
#70156=CARTESIAN_POINT('Ctrl Pts',(-1.72305597232,-36.274235612,-9.87693916651));
#70157=CARTESIAN_POINT('Ctrl Pts',(-1.70923112261,-36.2742356128,-9.78370991904));
#70158=CARTESIAN_POINT('Ctrl Pts',(-1.98588197209,-36.5742356128,-10.0450377979));
#70159=CARTESIAN_POINT('Ctrl Pts',(-1.98588199194,-36.4799878338,-10.0450377955));
#70160=CARTESIAN_POINT('Ctrl Pts',(-1.98006948849,-36.3857400547,-10.0084834252));
#70161=CARTESIAN_POINT('Ctrl Pts',(-1.96837042637,-36.3112466306,-9.93490911225));
#70162=CARTESIAN_POINT('Ctrl Pts',(-1.95356896515,-36.2742356137,-9.84182417757));
#70163=CARTESIAN_POINT('Ctrl Pts',(-1.93876749608,-36.2742356128,-9.74873924352));
#70164=CARTESIAN_POINT('Ctrl Pts',(-2.19293659404,-36.5742356128,-10.0096459663));
#70165=CARTESIAN_POINT('Ctrl Pts',(-2.1929365742,-36.4799878327,-10.0096459687));
#70166=CARTESIAN_POINT('Ctrl Pts',(-2.18644879041,-36.3857400526,-9.97320546397));
#70167=CARTESIAN_POINT('Ctrl Pts',(-2.17339061443,-36.3112466281,-9.89986032655));
#70168=CARTESIAN_POINT('Ctrl Pts',(-2.15686965068,-36.274235612,-9.80706533814));
#70169=CARTESIAN_POINT('Ctrl Pts',(-2.14034869478,-36.2742356128,-9.7142703491));
#70170=CARTESIAN_POINT('Ctrl Pts',(-2.29885537085,-36.5742356128,-9.99032970039));
#70171=CARTESIAN_POINT('Ctrl Pts',(-2.29885536708,-36.4799878331,-9.99032970104));
#70172=CARTESIAN_POINT('Ctrl Pts',(-2.29206280416,-36.3857400534,-9.95394533749));
#70173=CARTESIAN_POINT('Ctrl Pts',(-2.27839116924,-36.3112466291,-9.88071319968));
#70174=CARTESIAN_POINT('Ctrl Pts',(-2.26109405783,-36.2742356127,-9.78806117733));
#70175=CARTESIAN_POINT('Ctrl Pts',(-2.24379694792,-36.2742356128,-9.69540915479));
#70176=CARTESIAN_POINT('Ctrl Pts',(-2.69693922631,-36.5742356128,-9.91335054502));
#70177=CARTESIAN_POINT('Ctrl Pts',(-2.69693923691,-36.4799878335,-9.91335054317));
#70178=CARTESIAN_POINT('Ctrl Pts',(-2.6889563496,-36.3857400542,-9.87719590648));
#70179=CARTESIAN_POINT('Ctrl Pts',(-2.67288888841,-36.31124663,-9.80442615135));
#70180=CARTESIAN_POINT('Ctrl Pts',(-2.65256061041,-36.2742356133,-9.71235912888));
#70181=CARTESIAN_POINT('Ctrl Pts',(-2.6322323282,-36.2742356128,-9.62029210697));
#70182=CARTESIAN_POINT('Ctrl Pts',(-3.0919938661,-36.5742356128,-9.81991318886));
#70183=CARTESIAN_POINT('Ctrl Pts',(-3.09199383639,-36.4799878324,-9.81991319404));
#70184=CARTESIAN_POINT('Ctrl Pts',(-3.08278784534,-36.385740052,-9.78404777523));
#70185=CARTESIAN_POINT('Ctrl Pts',(-3.0642586456,-36.3112466275,-9.71186013107));
#70186=CARTESIAN_POINT('Ctrl Pts',(-3.04081584451,-36.2742356116,-9.62052958129));
#70187=CARTESIAN_POINT('Ctrl Pts',(-3.01737305521,-36.2742356128,-9.52919902996));
#70188=CARTESIAN_POINT('Ctrl Pts',(-3.38040989704,-36.5742356128,-9.7419516802));
#70189=CARTESIAN_POINT('Ctrl Pts',(-3.38040989405,-36.4799878327,-9.74195168123));
#70190=CARTESIAN_POINT('Ctrl Pts',(-3.37029179636,-36.3857400526,-9.70633130336));
#70191=CARTESIAN_POINT('Ctrl Pts',(-3.34992673534,-36.3112466282,-9.634636867));
#70192=CARTESIAN_POINT('Ctrl Pts',(-3.32416121766,-36.274235612,-9.54393031759));
#70193=CARTESIAN_POINT('Ctrl Pts',(-3.29839570127,-36.2742356128,-9.45322376807));
#70194=CARTESIAN_POINT('Ctrl Pts',(-3.87968490278,-36.5742356128,-9.58959720128));
#70195=CARTESIAN_POINT('Ctrl Pts',(-3.87968490502,-36.4799878336,-9.58959720052));
#70196=CARTESIAN_POINT('Ctrl Pts',(-3.86796253504,-36.3857400544,-9.55446591569));
#70197=CARTESIAN_POINT('Ctrl Pts',(-3.84436849025,-36.3112466302,-9.48375589692));
#70198=CARTESIAN_POINT('Ctrl Pts',(-3.81451771536,-36.2742356134,-9.39429481622));
#70199=CARTESIAN_POINT('Ctrl Pts',(-3.78466693948,-36.2742356128,-9.30483373562));
#70200=CARTESIAN_POINT('Ctrl Pts',(-4.36855122677,-36.5742356128,-9.40939629264));
#70201=CARTESIAN_POINT('Ctrl Pts',(-4.36855122509,-36.4799878329,-9.40939629322));
#70202=CARTESIAN_POINT('Ctrl Pts',(-4.35523621791,-36.3857400531,-9.37485180944));
#70203=CARTESIAN_POINT('Ctrl Pts',(-4.32843661881,-36.3112466287,-9.30532286492));
#70204=CARTESIAN_POINT('Ctrl Pts',(-4.29453023508,-36.2742356124,-9.21735605819));
#70205=CARTESIAN_POINT('Ctrl Pts',(-4.26062385208,-36.2742356128,-9.12938925139));
#70206=CARTESIAN_POINT('Ctrl Pts',(-4.5760187763,-36.5742356128,-9.32706183536));
#70207=CARTESIAN_POINT('Ctrl Pts',(-4.5760187745,-36.4799878338,-9.3270618362));
#70208=CARTESIAN_POINT('Ctrl Pts',(-4.56202665041,-36.3857400547,-9.29278602584));
#70209=CARTESIAN_POINT('Ctrl Pts',(-4.53386419357,-36.3112466306,-9.22379784981));
#70210=CARTESIAN_POINT('Ctrl Pts',(-4.49823354595,-36.2742356137,-9.13651521345));
#70211=CARTESIAN_POINT('Ctrl Pts',(-4.46260289891,-36.2742356128,-9.04923257645));
#70212=CARTESIAN_POINT('Ctrl Pts',(-5.19275926061,-36.5742356128,-9.06462215196));
#70213=CARTESIAN_POINT('Ctrl Pts',(-5.19275926422,-36.4799878322,-9.06462215026));
#70214=CARTESIAN_POINT('Ctrl Pts',(-5.17675952444,-36.3857400515,-9.03120113486));
#70215=CARTESIAN_POINT('Ctrl Pts',(-5.14455625961,-36.3112466268,-8.96393343893));
#70216=CARTESIAN_POINT('Ctrl Pts',(-5.10381324925,-36.2742356112,-8.87882752609));
#70217=CARTESIAN_POINT('Ctrl Pts',(-5.06307023773,-36.2742356128,-8.79372161452));
#70218=CARTESIAN_POINT('Ctrl Pts',(-5.78834049125,-36.5742356128,-8.75798298595));
#70219=CARTESIAN_POINT('Ctrl Pts',(-5.788340484,-36.4799878354,-8.75798298935));
#70220=CARTESIAN_POINT('Ctrl Pts',(-5.77044437661,-36.3857400579,-8.72553988322));
#70221=CARTESIAN_POINT('Ctrl Pts',(-5.73442423661,-36.3112466344,-8.66024045486));
#70222=CARTESIAN_POINT('Ctrl Pts',(-5.68885218855,-36.2742356162,-8.57762475546));
#70223=CARTESIAN_POINT('Ctrl Pts',(-5.64328014279,-36.2742356128,-8.49500905351));
#70224=CARTESIAN_POINT('Ctrl Pts',(-6.17544881684,-36.5742356128,-8.53471177464));
#70225=CARTESIAN_POINT('Ctrl Pts',(-6.1754488205,-36.4799878347,-8.53471177187));
#70226=CARTESIAN_POINT('Ctrl Pts',(-6.15635088894,-36.3857400565,-8.5029666931));
#70227=CARTESIAN_POINT('Ctrl Pts',(-6.11791178011,-36.3112466328,-8.43907221751));
#70228=CARTESIAN_POINT('Ctrl Pts',(-6.06927928827,-36.2742356151,-8.35823404393));
#70229=CARTESIAN_POINT('Ctrl Pts',(-6.02064679434,-36.2742356128,-8.27739587081));
#70230=CARTESIAN_POINT('Ctrl Pts',(-6.92915280215,-36.5742356128,-8.05308379561));
#70231=CARTESIAN_POINT('Ctrl Pts',(-6.92915279847,-36.4799878318,-8.05308379839));
#70232=CARTESIAN_POINT('Ctrl Pts',(-6.90785214448,-36.3857400507,-8.02275557517));
#70233=CARTESIAN_POINT('Ctrl Pts',(-6.86497954496,-36.3112466259,-7.96171284949));
#70234=CARTESIAN_POINT('Ctrl Pts',(-6.81073788334,-36.2742356106,-7.88448265761));
#70235=CARTESIAN_POINT('Ctrl Pts',(-6.75649622382,-36.2742356128,-7.80725246527));
#70236=CARTESIAN_POINT('Ctrl Pts',(-7.64600571687,-36.5742356128,-7.5075764295));
#70237=CARTESIAN_POINT('Ctrl Pts',(-7.64600572057,-36.4799878347,-7.50757642669));
#70238=CARTESIAN_POINT('Ctrl Pts',(-7.62292488665,-36.3857400566,-7.47861327484));
#70239=CARTESIAN_POINT('Ctrl Pts',(-7.57646924515,-36.3112466328,-7.42031808495));
#70240=CARTESIAN_POINT('Ctrl Pts',(-7.51769437599,-36.2742356151,-7.34656402996));
#70241=CARTESIAN_POINT('Ctrl Pts',(-7.45891950471,-36.2742356128,-7.27280997543));
#70242=CARTESIAN_POINT('Ctrl Pts',(-7.99980083252,-36.5742356128,-7.21703589238));
#70243=CARTESIAN_POINT('Ctrl Pts',(-7.99980082858,-36.4799878295,-7.21703589554));
#70244=CARTESIAN_POINT('Ctrl Pts',(-7.97586366783,-36.3857400462,-7.18878251664));
#70245=CARTESIAN_POINT('Ctrl Pts',(-7.92768447517,-36.3112466206,-7.13191590546));
#70246=CARTESIAN_POINT('Ctrl Pts',(-7.86672900529,-36.274235607,-7.05996926121));
#70247=CARTESIAN_POINT('Ctrl Pts',(-7.80577353846,-36.2742356128,-6.9880226175));
#70248=CARTESIAN_POINT('Ctrl Pts',(-8.84905353168,-36.5742356128,-6.46450747752));
#70249=CARTESIAN_POINT('Ctrl Pts',(-8.84905353743,-36.4799878387,-6.46450747292));
#70250=CARTESIAN_POINT('Ctrl Pts',(-8.82295393196,-36.3857400645,-6.43813308402));
#70251=CARTESIAN_POINT('Ctrl Pts',(-8.77042229601,-36.3112466421,-6.38504839428));
#70252=CARTESIAN_POINT('Ctrl Pts',(-8.70396018261,-36.2742356214,-6.31788657283));
#70253=CARTESIAN_POINT('Ctrl Pts',(-8.63749806478,-36.2742356128,-6.25072475062));
#70254=CARTESIAN_POINT('Ctrl Pts',(-9.61892143257,-36.5742356128,-5.61595506741));
#70255=CARTESIAN_POINT('Ctrl Pts',(-9.61892142418,-36.4799878253,-5.61595507411));
#70256=CARTESIAN_POINT('Ctrl Pts',(-9.59030674766,-36.3857400378,-5.59233308488));
#70257=CARTESIAN_POINT('Ctrl Pts',(-9.53271295384,-36.3112466107,-5.544788236));
#70258=CARTESIAN_POINT('Ctrl Pts',(-9.45984629869,-36.2742356004,-5.48463532196));
#70259=CARTESIAN_POINT('Ctrl Pts',(-9.38697965001,-36.2742356128,-5.42448240903));
#70260=CARTESIAN_POINT('Ctrl Pts',(-10.0435276565,-36.5742356128,-5.07402143134));
#70261=CARTESIAN_POINT('Ctrl Pts',(-10.0435276316,-36.4799878177,-5.07402148559));
#70262=CARTESIAN_POINT('Ctrl Pts',(-10.0130849077,-36.3857400225,-5.05250152625));
#70263=CARTESIAN_POINT('Ctrl Pts',(-9.95181175627,-36.3112465927,-5.00918745144));
#70264=CARTESIAN_POINT('Ctrl Pts',(-9.87429005612,-36.2742355884,-4.95438720865));
#70265=CARTESIAN_POINT('Ctrl Pts',(-9.79676837504,-36.2742356128,-4.89958694614));
#70266=CARTESIAN_POINT('Ctrl Pts',(-10.6579518564,-36.5742356128,-4.04641144733));
#70267=CARTESIAN_POINT('Ctrl Pts',(-10.6579518746,-36.4799878446,-4.04641140784));
#70268=CARTESIAN_POINT('Ctrl Pts',(-10.6240592807,-36.3857400763,-4.03054004281));
#70269=CARTESIAN_POINT('Ctrl Pts',(-10.5558423977,-36.311246656,-3.99859521531));
#70270=CARTESIAN_POINT('Ctrl Pts',(-10.469535573,-36.2742356306,-3.95817920057));
#70271=CARTESIAN_POINT('Ctrl Pts',(-10.3832287344,-36.2742356128,-3.91776320018));
#70272=CARTESIAN_POINT('Ctrl Pts',(-11.0188703723,-36.5742356128,-2.91552801853));
#70273=CARTESIAN_POINT('Ctrl Pts',(-11.0188703591,-36.479987825,-2.91552804728));
#70274=CARTESIAN_POINT('Ctrl Pts',(-10.9828310738,-36.3857400371,-2.90637408447));
#70275=CARTESIAN_POINT('Ctrl Pts',(-10.9102935043,-36.3112466099,-2.88794953427));
#70276=CARTESIAN_POINT('Ctrl Pts',(-10.8185202492,-36.2742355999,-2.86463909812));
#70277=CARTESIAN_POINT('Ctrl Pts',(-10.7267470043,-36.2742356128,-2.84132865151));
#70278=CARTESIAN_POINT('Ctrl Pts',(-11.1211124249,-36.5742356128,-2.42831608424));
#70279=CARTESIAN_POINT('Ctrl Pts',(-11.1211124689,-36.4799878553,-2.42831638526));
#70280=CARTESIAN_POINT('Ctrl Pts',(-11.0844967792,-36.3857400977,-2.42201094849));
#70281=CARTESIAN_POINT('Ctrl Pts',(-11.010798996,-36.3112466813,-2.40931943624));
#70282=CARTESIAN_POINT('Ctrl Pts',(-10.9175578094,-36.2742356474,-2.39326215592));
#70283=CARTESIAN_POINT('Ctrl Pts',(-10.8243165921,-36.2742356128,-2.37720475576));
#70284=CARTESIAN_POINT('Ctrl Pts',(-11.2315884468,-36.5742356128,-1.47511926274));
#70285=CARTESIAN_POINT('Ctrl Pts',(-11.2315884056,-36.4799878126,-1.47511898088));
#70286=CARTESIAN_POINT('Ctrl Pts',(-11.1944459333,-36.3857400124,-1.47378416589));
#70287=CARTESIAN_POINT('Ctrl Pts',(-11.1196879677,-36.3112465807,-1.47109784338));
#70288=CARTESIAN_POINT('Ctrl Pts',(-11.0251055307,-36.2742355804,-1.46769934297));
#70289=CARTESIAN_POINT('Ctrl Pts',(-10.9305231225,-36.2742356128,-1.46430095477));
#70290=CARTESIAN_POINT('Ctrl Pts',(-11.2043755329,-36.5742356128,-0.530546116159));
#70291=CARTESIAN_POINT('Ctrl Pts',(-11.2043755715,-36.4799878525,-0.53054638008));
#70292=CARTESIAN_POINT('Ctrl Pts',(-11.1673834471,-36.3857400923,-0.532820991327));
#70293=CARTESIAN_POINT('Ctrl Pts',(-11.0929280062,-36.3112466749,-0.537398895803));
#70294=CARTESIAN_POINT('Ctrl Pts',(-10.9987282489,-36.2742356432,-0.54319060461));
#70295=CARTESIAN_POINT('Ctrl Pts',(-10.9045284647,-36.2742356128,-0.548982208346));
#70296=CARTESIAN_POINT('Ctrl Pts',(-11.1665128558,-36.5742356128,-0.077344330525));
#70297=CARTESIAN_POINT('Ctrl Pts',(-11.1665126991,-36.4799878387,-0.0773433425996));
#70298=CARTESIAN_POINT('Ctrl Pts',(-11.1296536904,-36.3857400646,-0.0809244862498));
#70299=CARTESIAN_POINT('Ctrl Pts',(-11.055466388,-36.3112466423,-0.0881334573585));
#70300=CARTESIAN_POINT('Ctrl Pts',(-10.9616060106,-36.2742356215,-0.0972547802524));
#70301=CARTESIAN_POINT('Ctrl Pts',(-10.8677456912,-36.2742356128,-0.106376490674));
#70302=CARTESIAN_POINT('Ctrl Pts',(-11.1136931672,-36.5742356128,0.362811362875));
#70303=CARTESIAN_POINT('Ctrl Pts',(-11.113693272,-36.4799878329,0.362810700302));
#70304=CARTESIAN_POINT('Ctrl Pts',(-11.0769608227,-36.385740053,0.358150436098));
#70305=CARTESIAN_POINT('Ctrl Pts',(-11.0030279669,-36.3112466286,0.348771272008));
#70306=CARTESIAN_POINT('Ctrl Pts',(-10.9094893391,-36.2742356123,0.336905358648));
#70307=CARTESIAN_POINT('Ctrl Pts',(-10.8159506704,-36.2742356128,0.325039704942));
#70308=CARTESIAN_POINT('Ctrl Pts',(-11.0450672445,-36.5742356128,0.800651515617));
#70309=CARTESIAN_POINT('Ctrl Pts',(-11.045067244,-36.4799878332,0.800651518699));
#70310=CARTESIAN_POINT('Ctrl Pts',(-11.0085026394,-36.3857400536,0.794920460492));
#70311=CARTESIAN_POINT('Ctrl Pts',(-10.9349077252,-36.3112466293,0.783385346618));
#70312=CARTESIAN_POINT('Ctrl Pts',(-10.8417967252,-36.2742356128,0.768791320097));
#70313=CARTESIAN_POINT('Ctrl Pts',(-10.7486857254,-36.2742356128,0.754197292365));
#70314=CARTESIAN_POINT('',(-1.38699292015031,-36.5742356128,-10.1328356964021));
#70315=CARTESIAN_POINT('Origin',(-1.34567758431402,-36.5721143209619,-9.8378360912598));
#70316=CARTESIAN_POINT('Ctrl Pts',(-1.38699292008,-36.5742356128,-10.1328356959));
#70317=CARTESIAN_POINT('Ctrl Pts',(-1.54048434157,-36.5742356128,-10.1113387667));
#70318=CARTESIAN_POINT('Ctrl Pts',(-1.68405004862,-36.5742356128,-10.0907690318));
#70319=CARTESIAN_POINT('Ctrl Pts',(-1.83768542132,-36.5742356128,-10.0680136807));
#70320=CARTESIAN_POINT('Ctrl Pts',(-2.0472685103,-36.5742356128,-10.0350233698));
#70321=CARTESIAN_POINT('Ctrl Pts',(-2.24744160945,-36.5742356128,-9.99950190736));
#70322=CARTESIAN_POINT('Ctrl Pts',(-2.32512404463,-36.5742356128,-9.9850708371));
#70323=CARTESIAN_POINT('Ctrl Pts',(-2.47861794583,-36.5742356128,-9.95531796778));
#70324=CARTESIAN_POINT('Ctrl Pts',(-2.63158870593,-36.5742356128,-9.9231347794));
#70325=CARTESIAN_POINT('Ctrl Pts',(-2.70802102444,-36.5742356128,-9.90641220658));
#70326=CARTESIAN_POINT('Ctrl Pts',(-3.01253146542,-36.5742356128,-9.83720045464));
#70327=CARTESIAN_POINT('Ctrl Pts',(-3.31446912355,-36.5742356128,-9.75814914822));
#70328=CARTESIAN_POINT('Ctrl Pts',(-3.53901439175,-36.5742356128,-9.69332241166));
#70329=CARTESIAN_POINT('Ctrl Pts',(-4.06616678433,-36.5742356128,-9.5265559109));
#70330=CARTESIAN_POINT('Ctrl Pts',(-4.58136980211,-36.5742356128,-9.32859973654));
#70331=CARTESIAN_POINT('Ctrl Pts',(-4.87486658275,-36.5742356128,-9.20377818652));
#70332=CARTESIAN_POINT('Ctrl Pts',(-5.45178039505,-36.5742356128,-8.9342344636));
#70333=CARTESIAN_POINT('Ctrl Pts',(-6.0085344695,-36.5742356128,-8.62630121912));
#70334=CARTESIAN_POINT('Ctrl Pts',(-6.28153293631,-36.5742356128,-8.46325996649));
#70335=CARTESIAN_POINT('Ctrl Pts',(-6.68293897529,-36.5742356128,-8.20578167081));
#70336=CARTESIAN_POINT('Ctrl Pts',(-7.07391925375,-36.5742356128,-7.9296599837));
#70337=CARTESIAN_POINT('Ctrl Pts',(-7.20312714751,-36.5742356128,-7.83561707231));
#70338=CARTESIAN_POINT('Ctrl Pts',(-7.71835943346,-36.5742356128,-7.44951290203));
#70339=CARTESIAN_POINT('Ctrl Pts',(-8.21985964705,-36.5742356128,-7.02884209138));
#70340=CARTESIAN_POINT('Ctrl Pts',(-8.58741395083,-36.5742356128,-6.694450027));
#70341=CARTESIAN_POINT('Ctrl Pts',(-9.23922565915,-36.5742356128,-6.04471661443));
#70342=CARTESIAN_POINT('Ctrl Pts',(-9.82149842759,-36.5742356128,-5.3259548207));
#70343=CARTESIAN_POINT('Ctrl Pts',(-10.0721843915,-36.5742356128,-4.97806710989));
#70344=CARTESIAN_POINT('Ctrl Pts',(-10.6524574839,-36.5742356128,-4.03375119461));
#70345=CARTESIAN_POINT('Ctrl Pts',(-11.0291793988,-36.5742356128,-2.98459593108));
#70346=CARTESIAN_POINT('Ctrl Pts',(-11.1622899814,-36.5742356128,-2.31636115633));
#70347=CARTESIAN_POINT('Ctrl Pts',(-11.2336540706,-36.5742356128,-1.36618233642));
#70348=CARTESIAN_POINT('Ctrl Pts',(-11.1889875368,-36.5742356128,-0.434883867537));
#70349=CARTESIAN_POINT('Ctrl Pts',(-11.1677658434,-36.5742356128,-0.163547364276));
#70350=CARTESIAN_POINT('Ctrl Pts',(-11.1309935407,-36.5742356128,0.191196052966));
#70351=CARTESIAN_POINT('Ctrl Pts',(-11.0837537732,-36.5742356128,0.541839826065));
#70352=CARTESIAN_POINT('Ctrl Pts',(-11.0714556362,-36.5742356128,0.62831585634));
#70353=CARTESIAN_POINT('Ctrl Pts',(-11.0585597994,-36.5742356128,0.714566551426));
#70354=CARTESIAN_POINT('Ctrl Pts',(-11.0450673741,-36.5742356128,0.800650704934));
#70355=CARTESIAN_POINT('Ctrl Pts',(-10.7486857339,-38.2742356128,0.754197251045));
#70356=CARTESIAN_POINT('Ctrl Pts',(-10.8417967716,-38.2742356128,0.768791038108));
#70357=CARTESIAN_POINT('Ctrl Pts',(-10.9349078093,-38.2372245963,0.783384825171));
#70358=CARTESIAN_POINT('Ctrl Pts',(-11.008502753,-38.1627311721,0.794919751257));
#70359=CARTESIAN_POINT('Ctrl Pts',(-11.045067372,-38.0684833924,0.800650718035));
#70360=CARTESIAN_POINT('Ctrl Pts',(-11.045067372,-37.9742356128,0.800650718035));
#70361=CARTESIAN_POINT('Ctrl Pts',(-10.8644820124,-38.2742356128,0.015396349477));
#70362=CARTESIAN_POINT('Ctrl Pts',(-10.95831508,-38.2742356128,0.0253834674463));
#70363=CARTESIAN_POINT('Ctrl Pts',(-11.0521481476,-38.2372245963,0.0353705854157));
#70364=CARTESIAN_POINT('Ctrl Pts',(-11.1263136449,-38.1627311721,0.0432652827677));
#70365=CARTESIAN_POINT('Ctrl Pts',(-11.1631619431,-38.0684833924,0.0471863333183));
#70366=CARTESIAN_POINT('Ctrl Pts',(-11.1631619431,-37.9742356128,0.0471863333183));
#70367=CARTESIAN_POINT('Ctrl Pts',(-10.9353869016,-38.2742356128,-0.736346737241));
#70368=CARTESIAN_POINT('Ctrl Pts',(-11.0296310539,-38.2742356128,-0.731109451787));
#70369=CARTESIAN_POINT('Ctrl Pts',(-11.1238752062,-38.2372245963,-0.725872166333));
#70370=CARTESIAN_POINT('Ctrl Pts',(-11.1983659715,-38.1627311721,-0.721733939256));
#70371=CARTESIAN_POINT('Ctrl Pts',(-11.2353753555,-38.0684833924,-0.719675939874));
#70372=CARTESIAN_POINT('Ctrl Pts',(-11.2353753555,-37.9742356128,-0.719675939874));
#70373=CARTESIAN_POINT('Ctrl Pts',(-10.9581033367,-38.2742356128,-1.51216421625));
#70374=CARTESIAN_POINT('Ctrl Pts',(-11.0532569791,-38.2742356128,-1.51543079532));
#70375=CARTESIAN_POINT('Ctrl Pts',(-11.1484106216,-38.2372245963,-1.51869737439));
#70376=CARTESIAN_POINT('Ctrl Pts',(-11.2236199878,-38.1627311721,-1.52127894667));
#70377=CARTESIAN_POINT('Ctrl Pts',(-11.2609867877,-38.0684833924,-1.52256206037));
#70378=CARTESIAN_POINT('Ctrl Pts',(-11.2609867877,-37.9742356128,-1.52256206037));
#70379=CARTESIAN_POINT('Ctrl Pts',(-10.831079727,-38.2742356128,-2.52840849741));
#70380=CARTESIAN_POINT('Ctrl Pts',(-10.9245012349,-38.2742356128,-2.54681170763));
#70381=CARTESIAN_POINT('Ctrl Pts',(-11.0179227428,-38.2372245963,-2.56521491785));
#70382=CARTESIAN_POINT('Ctrl Pts',(-11.0917630994,-38.1627311721,-2.57976092087));
#70383=CARTESIAN_POINT('Ctrl Pts',(-11.1284496225,-38.0684833924,-2.58698773492));
#70384=CARTESIAN_POINT('Ctrl Pts',(-11.1284496225,-37.9742356128,-2.58698773492));
#70385=CARTESIAN_POINT('Ctrl Pts',(-10.4997203395,-38.2742356128,-3.49265676226));
#70386=CARTESIAN_POINT('Ctrl Pts',(-10.5879306786,-38.2742356128,-3.52619793269));
#70387=CARTESIAN_POINT('Ctrl Pts',(-10.6761410178,-38.2372245963,-3.55973910313));
#70388=CARTESIAN_POINT('Ctrl Pts',(-10.7458624447,-38.1627311721,-3.58625000051));
#70389=CARTESIAN_POINT('Ctrl Pts',(-10.7805025696,-38.0684833924,-3.59942162369));
#70390=CARTESIAN_POINT('Ctrl Pts',(-10.7805025696,-37.9742356128,-3.59942162369));
#70391=CARTESIAN_POINT('Ctrl Pts',(-10.4039697378,-38.2742356128,-3.72874327308));
#70392=CARTESIAN_POINT('Ctrl Pts',(-10.4906791962,-38.2742356128,-3.76598554153));
#70393=CARTESIAN_POINT('Ctrl Pts',(-10.5773886547,-38.2372245963,-3.80322780998));
#70394=CARTESIAN_POINT('Ctrl Pts',(-10.6459237916,-38.1627311721,-3.83266409077));
#70395=CARTESIAN_POINT('Ctrl Pts',(-10.6799745163,-38.0684833924,-3.8472890954));
#70396=CARTESIAN_POINT('Ctrl Pts',(-10.6799745163,-37.9742356128,-3.8472890954));
#70397=CARTESIAN_POINT('Ctrl Pts',(-10.0688223315,-38.2742356128,-4.4465666977));
#70398=CARTESIAN_POINT('Ctrl Pts',(-10.1503858218,-38.2742356128,-4.49478078091));
#70399=CARTESIAN_POINT('Ctrl Pts',(-10.231949312,-38.2372245963,-4.54299486411));
#70400=CARTESIAN_POINT('Ctrl Pts',(-10.2964170767,-38.1627311721,-4.58110326484));
#70401=CARTESIAN_POINT('Ctrl Pts',(-10.3284469844,-38.0684833924,-4.60003689108));
#70402=CARTESIAN_POINT('Ctrl Pts',(-10.3284469844,-37.9742356128,-4.60003689108));
#70403=CARTESIAN_POINT('Ctrl Pts',(-9.62301691076,-38.2742356128,-5.11189798418));
#70404=CARTESIAN_POINT('Ctrl Pts',(-9.69858882439,-38.2742356128,-5.16881938559));
#70405=CARTESIAN_POINT('Ctrl Pts',(-9.77416073802,-38.2372245963,-5.22574078701));
#70406=CARTESIAN_POINT('Ctrl Pts',(-9.83389276175,-38.1627311721,-5.27073145039));
#70407=CARTESIAN_POINT('Ctrl Pts',(-9.86356978302,-38.0684833924,-5.29308443223));
#70408=CARTESIAN_POINT('Ctrl Pts',(-9.86356978302,-37.9742356128,-5.29308443223));
#70409=CARTESIAN_POINT('Ctrl Pts',(-9.28042553493,-38.2742356128,-5.53648144054));
#70410=CARTESIAN_POINT('Ctrl Pts',(-9.35246734892,-38.2742356128,-5.59750992502));
#70411=CARTESIAN_POINT('Ctrl Pts',(-9.42450916291,-38.2372245963,-5.65853840949));
#70412=CARTESIAN_POINT('Ctrl Pts',(-9.4814509968,-38.1627311721,-5.70677531028));
#70413=CARTESIAN_POINT('Ctrl Pts',(-9.50974175105,-38.0684833924,-5.73074114001));
#70414=CARTESIAN_POINT('Ctrl Pts',(-9.50974175105,-37.9742356128,-5.73074114001));
#70415=CARTESIAN_POINT('Ctrl Pts',(-8.60018141119,-38.2742356128,-6.27983264313));
#70416=CARTESIAN_POINT('Ctrl Pts',(-8.66640539804,-38.2742356128,-6.34716877797));
#70417=CARTESIAN_POINT('Ctrl Pts',(-8.73262938489,-38.2372245963,-6.4145049128));
#70418=CARTESIAN_POINT('Ctrl Pts',(-8.78497280955,-38.1627311721,-6.46772737895));
#70419=CARTESIAN_POINT('Ctrl Pts',(-8.81097890835,-38.0684833924,-6.49417021728));
#70420=CARTESIAN_POINT('Ctrl Pts',(-8.81097890835,-37.9742356128,-6.49417021728));
#70421=CARTESIAN_POINT('Ctrl Pts',(-7.85121695461,-38.2742356128,-6.95010363271));
#70422=CARTESIAN_POINT('Ctrl Pts',(-7.91247104152,-38.2742356128,-7.02180601188));
#70423=CARTESIAN_POINT('Ctrl Pts',(-7.97372512843,-38.2372245963,-7.09350839104));
#70424=CARTESIAN_POINT('Ctrl Pts',(-8.02214034526,-38.1627311721,-7.15018193575));
#70425=CARTESIAN_POINT('Ctrl Pts',(-8.04619476894,-38.0684833924,-7.17833939422));
#70426=CARTESIAN_POINT('Ctrl Pts',(-8.04619476894,-37.9742356128,-7.17833939422));
#70427=CARTESIAN_POINT('Ctrl Pts',(-7.49651322649,-38.2742356128,-7.24338281986));
#70428=CARTESIAN_POINT('Ctrl Pts',(-7.55552872191,-38.2742356128,-7.3169478207));
#70429=CARTESIAN_POINT('Ctrl Pts',(-7.61454421733,-38.2372245963,-7.39051282155));
#70430=CARTESIAN_POINT('Ctrl Pts',(-7.66119005191,-38.1627311721,-7.44865858205));
#70431=CARTESIAN_POINT('Ctrl Pts',(-7.68436538279,-38.0684833924,-7.47754749032));
#70432=CARTESIAN_POINT('Ctrl Pts',(-7.68436538279,-37.9742356128,-7.47754749032));
#70433=CARTESIAN_POINT('Ctrl Pts',(-6.78245213327,-38.2742356128,-7.7898018263));
#70434=CARTESIAN_POINT('Ctrl Pts',(-6.83688001526,-38.2742356128,-7.86690543711));
#70435=CARTESIAN_POINT('Ctrl Pts',(-6.89130789724,-38.2372245963,-7.94400904792));
#70436=CARTESIAN_POINT('Ctrl Pts',(-6.93432768319,-38.1627311721,-8.00495172497));
#70437=CARTESIAN_POINT('Ctrl Pts',(-6.95570146247,-38.0684833924,-8.03523024212));
#70438=CARTESIAN_POINT('Ctrl Pts',(-6.95570146247,-37.9742356128,-8.03523024212));
#70439=CARTESIAN_POINT('Ctrl Pts',(-6.03422296673,-38.2742356128,-8.26953898084));
#70440=CARTESIAN_POINT('Ctrl Pts',(-6.08296773524,-38.2742356128,-8.35031143298));
#70441=CARTESIAN_POINT('Ctrl Pts',(-6.13171250375,-38.2372245963,-8.43108388512));
#70442=CARTESIAN_POINT('Ctrl Pts',(-6.1702403581,-38.1627311721,-8.49492641351));
#70443=CARTESIAN_POINT('Ctrl Pts',(-6.1893823839,-38.0684833924,-8.52664568131));
#70444=CARTESIAN_POINT('Ctrl Pts',(-6.1893823839,-37.9742356128,-8.52664568131));
#70445=CARTESIAN_POINT('Ctrl Pts',(-5.65254018915,-38.2742356128,-8.4902387588));
#70446=CARTESIAN_POINT('Ctrl Pts',(-5.69818840924,-38.2742356128,-8.57281530405));
#70447=CARTESIAN_POINT('Ctrl Pts',(-5.74383662934,-38.2372245963,-8.65539184929));
#70448=CARTESIAN_POINT('Ctrl Pts',(-5.77991697251,-38.1627311721,-8.72066033248));
#70449=CARTESIAN_POINT('Ctrl Pts',(-5.79784298659,-38.0684833924,-8.75308806599));
#70450=CARTESIAN_POINT('Ctrl Pts',(-5.79784298659,-37.9742356128,-8.75308806599));
#70451=CARTESIAN_POINT('Ctrl Pts',(-5.06785956151,-38.2742356128,-8.79168353687));
#70452=CARTESIAN_POINT('Ctrl Pts',(-5.10864378738,-38.2742356128,-8.87677178634));
#70453=CARTESIAN_POINT('Ctrl Pts',(-5.14942801325,-38.2372245963,-8.96186003582));
#70454=CARTESIAN_POINT('Ctrl Pts',(-5.1816638564,-38.1627311721,-9.0291137695));
#70455=CARTESIAN_POINT('Ctrl Pts',(-5.19767978446,-38.0684833924,-9.06252784693));
#70456=CARTESIAN_POINT('Ctrl Pts',(-5.19767978446,-37.9742356128,-9.06252784693));
#70457=CARTESIAN_POINT('Ctrl Pts',(-4.46260362429,-38.2742356128,-9.04923232877));
#70458=CARTESIAN_POINT('Ctrl Pts',(-4.49823406166,-38.2742356128,-9.1365151112));
#70459=CARTESIAN_POINT('Ctrl Pts',(-4.53386449903,-38.2372245963,-9.22379789362));
#70460=CARTESIAN_POINT('Ctrl Pts',(-4.56202678889,-38.1627311721,-9.29278618567));
#70461=CARTESIAN_POINT('Ctrl Pts',(-4.57601882892,-38.0684833924,-9.32706205417));
#70462=CARTESIAN_POINT('Ctrl Pts',(-4.57601882892,-37.9742356128,-9.32706205417));
#70463=CARTESIAN_POINT('Ctrl Pts',(-4.26062386225,-38.2742356128,-9.12938925058));
#70464=CARTESIAN_POINT('Ctrl Pts',(-4.29453024428,-38.2742356128,-9.21735605705));
#70465=CARTESIAN_POINT('Ctrl Pts',(-4.3284366263,-38.2372245963,-9.30532286352));
#70466=CARTESIAN_POINT('Ctrl Pts',(-4.3552362232,-38.1627311721,-9.37485180801));
#70467=CARTESIAN_POINT('Ctrl Pts',(-4.36855122828,-38.0684833924,-9.40939629213));
#70468=CARTESIAN_POINT('Ctrl Pts',(-4.36855122828,-37.9742356128,-9.40939629213));
#70469=CARTESIAN_POINT('Ctrl Pts',(-3.7846669259,-38.2742356128,-9.30483373669));
#70470=CARTESIAN_POINT('Ctrl Pts',(-3.81451770308,-38.2742356128,-9.39429481774));
#70471=CARTESIAN_POINT('Ctrl Pts',(-3.84436848026,-38.2372245963,-9.4837558988));
#70472=CARTESIAN_POINT('Ctrl Pts',(-3.86796252798,-38.1627311721,-9.55446591759));
#70473=CARTESIAN_POINT('Ctrl Pts',(-3.87968490077,-38.0684833924,-9.58959720197));
#70474=CARTESIAN_POINT('Ctrl Pts',(-3.87968490077,-37.9742356128,-9.58959720197));
#70475=CARTESIAN_POINT('Ctrl Pts',(-3.29839571939,-38.2742356128,-9.45322376664));
#70476=CARTESIAN_POINT('Ctrl Pts',(-3.32416123403,-38.2742356128,-9.54393031556));
#70477=CARTESIAN_POINT('Ctrl Pts',(-3.34992674868,-38.2372245963,-9.63463686449));
#70478=CARTESIAN_POINT('Ctrl Pts',(-3.37029180577,-38.1627311721,-9.70633130082));
#70479=CARTESIAN_POINT('Ctrl Pts',(-3.38040989972,-38.0684833924,-9.74195167929));
#70480=CARTESIAN_POINT('Ctrl Pts',(-3.38040989972,-37.9742356128,-9.74195167929));
#70481=CARTESIAN_POINT('Ctrl Pts',(-3.01737322736,-38.2742356128,-9.52919900757));
#70482=CARTESIAN_POINT('Ctrl Pts',(-3.04081598292,-38.2742356128,-9.6205295628));
#70483=CARTESIAN_POINT('Ctrl Pts',(-3.06425873847,-38.2372245963,-9.71186011804));
#70484=CARTESIAN_POINT('Ctrl Pts',(-3.08278788744,-38.1627311721,-9.78404776885));
#70485=CARTESIAN_POINT('Ctrl Pts',(-3.09199383589,-38.0684833924,-9.81991319399));
#70486=CARTESIAN_POINT('Ctrl Pts',(-3.09199383589,-37.9742356128,-9.81991319399));
#70487=CARTESIAN_POINT('Ctrl Pts',(-2.63223226683,-38.2742356128,-9.62029211495));
#70488=CARTESIAN_POINT('Ctrl Pts',(-2.65256056107,-38.2742356128,-9.71235913547));
#70489=CARTESIAN_POINT('Ctrl Pts',(-2.67288885531,-38.2372245963,-9.804426156));
#70490=CARTESIAN_POINT('Ctrl Pts',(-2.68895633456,-38.1627311721,-9.87719590877));
#70491=CARTESIAN_POINT('Ctrl Pts',(-2.69693923708,-38.0684833924,-9.91335054319));
#70492=CARTESIAN_POINT('Ctrl Pts',(-2.69693923708,-37.9742356128,-9.91335054319));
#70493=CARTESIAN_POINT('Ctrl Pts',(-2.24379696979,-38.2742356128,-9.69540915194));
#70494=CARTESIAN_POINT('Ctrl Pts',(-2.26109407541,-38.2742356128,-9.78806117498));
#70495=CARTESIAN_POINT('Ctrl Pts',(-2.27839118104,-38.2372245963,-9.88071319803));
#70496=CARTESIAN_POINT('Ctrl Pts',(-2.29206280953,-38.1627311721,-9.95394533667));
#70497=CARTESIAN_POINT('Ctrl Pts',(-2.29885536701,-38.0684833924,-9.99032970104));
#70498=CARTESIAN_POINT('Ctrl Pts',(-2.29885536701,-37.9742356128,-9.99032970104));
#70499=CARTESIAN_POINT('Ctrl Pts',(-2.14030551313,-38.2742356128,-9.71427636052));
#70500=CARTESIAN_POINT('Ctrl Pts',(-2.15683710444,-38.2742356128,-9.80706985748));
#70501=CARTESIAN_POINT('Ctrl Pts',(-2.17336869575,-38.2372245963,-9.89986335443));
#70502=CARTESIAN_POINT('Ctrl Pts',(-2.18643526145,-38.1627311721,-9.97320731411));
#70503=CARTESIAN_POINT('Ctrl Pts',(-2.19292720261,-38.0684833924,-10.0096472351));
#70504=CARTESIAN_POINT('Ctrl Pts',(-2.19292720261,-37.9742356128,-10.0096472351));
#70505=CARTESIAN_POINT('Ctrl Pts',(-1.93885306926,-38.2742356128,-9.74872598301));
#70506=CARTESIAN_POINT('Ctrl Pts',(-1.95364426813,-38.2742356128,-9.84181234766));
#70507=CARTESIAN_POINT('Ctrl Pts',(-1.968435467,-38.2372245963,-9.93489871231));
#70508=CARTESIAN_POINT('Ctrl Pts',(-1.98012642784,-38.1627311721,-10.0084741544));
#70509=CARTESIAN_POINT('Ctrl Pts',(-1.98593491754,-38.0684833924,-10.0450290844));
#70510=CARTESIAN_POINT('Ctrl Pts',(-1.98593491754,-37.9742356128,-10.0450290844));
#70511=CARTESIAN_POINT('Ctrl Pts',(-1.70928454097,-38.2742356128,-9.78370121332));
#70512=CARTESIAN_POINT('Ctrl Pts',(-1.72312043005,-38.2742356128,-9.87692890895));
#70513=CARTESIAN_POINT('Ctrl Pts',(-1.73695631912,-38.2372245963,-9.97015660458));
#70514=CARTESIAN_POINT('Ctrl Pts',(-1.74789220221,-38.1627311721,-10.0438437548));
#70515=CARTESIAN_POINT('Ctrl Pts',(-1.75332554374,-38.0684833924,-10.0804541852));
#70516=CARTESIAN_POINT('Ctrl Pts',(-1.75332554374,-37.9742356128,-10.0804541852));
#70517=CARTESIAN_POINT('Ctrl Pts',(-1.58829686019,-38.2742356128,-9.80140839538));
#70518=CARTESIAN_POINT('Ctrl Pts',(-1.6018000959,-38.2742356128,-9.89468428557));
#70519=CARTESIAN_POINT('Ctrl Pts',(-1.61530333161,-38.2372245963,-9.98796017577));
#70520=CARTESIAN_POINT('Ctrl Pts',(-1.62597628817,-38.1627311721,-10.0616854186));
#70521=CARTESIAN_POINT('Ctrl Pts',(-1.6312789944,-38.0684833924,-10.0983147753));
#70522=CARTESIAN_POINT('Ctrl Pts',(-1.6312789944,-37.9742356128,-10.0983147753));
#70523=CARTESIAN_POINT('Ctrl Pts',(-1.46928796479,-38.2742356128,-9.81838209355));
#70524=CARTESIAN_POINT('Ctrl Pts',(-1.48253918237,-38.2742356128,-9.91169383936));
#70525=CARTESIAN_POINT('Ctrl Pts',(-1.49579039996,-38.2372245963,-10.0050055852));
#70526=CARTESIAN_POINT('Ctrl Pts',(-1.50626415805,-38.1627311721,-10.0787591687));
#70527=CARTESIAN_POINT('Ctrl Pts',(-1.51146790041,-38.0684833924,-10.1154026054));
#70528=CARTESIAN_POINT('Ctrl Pts',(-1.51146790041,-37.9742356128,-10.1154026054));
#70529=CARTESIAN_POINT('Ctrl Pts',(-1.34538313247,-38.2742356128,-9.83573533307));
#70530=CARTESIAN_POINT('Ctrl Pts',(-1.35845523278,-38.2742356128,-9.92907216478));
#70531=CARTESIAN_POINT('Ctrl Pts',(-1.37152733308,-38.2372245963,-10.0224089965));
#70532=CARTESIAN_POINT('Ctrl Pts',(-1.38185951829,-38.1627311721,-10.0961824078));
#70533=CARTESIAN_POINT('Ctrl Pts',(-1.38699292008,-38.0684833924,-10.1328356959));
#70534=CARTESIAN_POINT('Ctrl Pts',(-1.38699292008,-37.9742356128,-10.1328356959));
#70535=CARTESIAN_POINT('',(-1.38699292008,-37.9742356128,-10.1328356959));
#70536=CARTESIAN_POINT('Origin',(-1.34567653659528,-37.9763568755272,-9.83783619861542));
#70537=CARTESIAN_POINT('Ctrl Pts',(-1.38699292008,-37.9742356128,-10.1328356959));
#70538=CARTESIAN_POINT('Ctrl Pts',(-1.54048434157,-37.9742356128,-10.1113387667));
#70539=CARTESIAN_POINT('Ctrl Pts',(-1.68405004862,-37.9742356128,-10.0907690318));
#70540=CARTESIAN_POINT('Ctrl Pts',(-1.83768542132,-37.9742356128,-10.0680136807));
#70541=CARTESIAN_POINT('Ctrl Pts',(-2.0472685103,-37.9742356128,-10.0350233698));
#70542=CARTESIAN_POINT('Ctrl Pts',(-2.24744160945,-37.9742356128,-9.99950190736));
#70543=CARTESIAN_POINT('Ctrl Pts',(-2.32512404463,-37.9742356128,-9.9850708371));
#70544=CARTESIAN_POINT('Ctrl Pts',(-2.47861794583,-37.9742356128,-9.95531796778));
#70545=CARTESIAN_POINT('Ctrl Pts',(-2.63158870593,-37.9742356128,-9.9231347794));
#70546=CARTESIAN_POINT('Ctrl Pts',(-2.70802102444,-37.9742356128,-9.90641220658));
#70547=CARTESIAN_POINT('Ctrl Pts',(-3.01253146542,-37.9742356128,-9.83720045464));
#70548=CARTESIAN_POINT('Ctrl Pts',(-3.31446912355,-37.9742356128,-9.75814914822));
#70549=CARTESIAN_POINT('Ctrl Pts',(-3.53901439175,-37.9742356128,-9.69332241166));
#70550=CARTESIAN_POINT('Ctrl Pts',(-4.06616678433,-37.9742356128,-9.5265559109));
#70551=CARTESIAN_POINT('Ctrl Pts',(-4.58136980211,-37.9742356128,-9.32859973654));
#70552=CARTESIAN_POINT('Ctrl Pts',(-4.87486658275,-37.9742356128,-9.20377818652));
#70553=CARTESIAN_POINT('Ctrl Pts',(-5.45178039505,-37.9742356128,-8.9342344636));
#70554=CARTESIAN_POINT('Ctrl Pts',(-6.0085344695,-37.9742356128,-8.62630121912));
#70555=CARTESIAN_POINT('Ctrl Pts',(-6.28153293631,-37.9742356128,-8.46325996649));
#70556=CARTESIAN_POINT('Ctrl Pts',(-6.68293897529,-37.9742356128,-8.20578167081));
#70557=CARTESIAN_POINT('Ctrl Pts',(-7.07391925375,-37.9742356128,-7.9296599837));
#70558=CARTESIAN_POINT('Ctrl Pts',(-7.20312714751,-37.9742356128,-7.83561707231));
#70559=CARTESIAN_POINT('Ctrl Pts',(-7.71835943346,-37.9742356128,-7.44951290203));
#70560=CARTESIAN_POINT('Ctrl Pts',(-8.21985964705,-37.9742356128,-7.02884209138));
#70561=CARTESIAN_POINT('Ctrl Pts',(-8.58741395083,-37.9742356128,-6.694450027));
#70562=CARTESIAN_POINT('Ctrl Pts',(-9.23922565915,-37.9742356128,-6.04471661443));
#70563=CARTESIAN_POINT('Ctrl Pts',(-9.82149842759,-37.9742356128,-5.3259548207));
#70564=CARTESIAN_POINT('Ctrl Pts',(-10.0721843915,-37.9742356128,-4.97806710989));
#70565=CARTESIAN_POINT('Ctrl Pts',(-10.6524574839,-37.9742356128,-4.03375119461));
#70566=CARTESIAN_POINT('Ctrl Pts',(-11.0291793988,-37.9742356128,-2.98459593108));
#70567=CARTESIAN_POINT('Ctrl Pts',(-11.1622899814,-37.9742356128,-2.31636115633));
#70568=CARTESIAN_POINT('Ctrl Pts',(-11.2336540706,-37.9742356128,-1.36618233642));
#70569=CARTESIAN_POINT('Ctrl Pts',(-11.1889875368,-37.9742356128,-0.434883867537));
#70570=CARTESIAN_POINT('Ctrl Pts',(-11.1677658434,-37.9742356128,-0.163547364276));
#70571=CARTESIAN_POINT('Ctrl Pts',(-11.1309935407,-37.9742356128,0.191196052966));
#70572=CARTESIAN_POINT('Ctrl Pts',(-11.0837537732,-37.9742356128,0.541839826065));
#70573=CARTESIAN_POINT('Ctrl Pts',(-11.0714556362,-37.9742356128,0.62831585634));
#70574=CARTESIAN_POINT('Ctrl Pts',(-11.0585597994,-37.9742356128,0.714566551426));
#70575=CARTESIAN_POINT('Ctrl Pts',(-11.0450673741,-37.9742356128,0.800650704934));
#70576=CARTESIAN_POINT('Ctrl Pts',(-11.0450673741,-37.9742356128,0.800650704934));
#70577=CARTESIAN_POINT('Ctrl Pts',(-11.0450673741,-36.2942356128,0.800650704934));
#70578=CARTESIAN_POINT('Ctrl Pts',(-11.0585597994,-37.9742356128,0.714566551426));
#70579=CARTESIAN_POINT('Ctrl Pts',(-11.0585597994,-36.2942356128,0.714566551426));
#70580=CARTESIAN_POINT('Ctrl Pts',(-11.0714556362,-37.9742356128,0.62831585634));
#70581=CARTESIAN_POINT('Ctrl Pts',(-11.0714556362,-36.2942356128,0.62831585634));
#70582=CARTESIAN_POINT('Ctrl Pts',(-11.0837537732,-37.9742356128,0.541839826065));
#70583=CARTESIAN_POINT('Ctrl Pts',(-11.0837537732,-36.2942356128,0.541839826065));
#70584=CARTESIAN_POINT('Ctrl Pts',(-11.1309935407,-37.9742356128,0.191196052966));
#70585=CARTESIAN_POINT('Ctrl Pts',(-11.1309935407,-36.2942356128,0.191196052966));
#70586=CARTESIAN_POINT('Ctrl Pts',(-11.1677658434,-37.9742356128,-0.163547364276));
#70587=CARTESIAN_POINT('Ctrl Pts',(-11.1677658434,-36.2942356128,-0.163547364276));
#70588=CARTESIAN_POINT('Ctrl Pts',(-11.1889875368,-37.9742356128,-0.434883867537));
#70589=CARTESIAN_POINT('Ctrl Pts',(-11.1889875368,-36.2942356128,-0.434883867537));
#70590=CARTESIAN_POINT('Ctrl Pts',(-11.2336540706,-37.9742356128,-1.36618233642));
#70591=CARTESIAN_POINT('Ctrl Pts',(-11.2336540706,-36.2942356128,-1.36618233642));
#70592=CARTESIAN_POINT('Ctrl Pts',(-11.1622899814,-37.9742356128,-2.31636115633));
#70593=CARTESIAN_POINT('Ctrl Pts',(-11.1622899814,-36.2942356128,-2.31636115633));
#70594=CARTESIAN_POINT('Ctrl Pts',(-11.0291793988,-37.9742356128,-2.98459593108));
#70595=CARTESIAN_POINT('Ctrl Pts',(-11.0291793988,-36.2942356128,-2.98459593108));
#70596=CARTESIAN_POINT('Ctrl Pts',(-10.6524574839,-37.9742356128,-4.03375119461));
#70597=CARTESIAN_POINT('Ctrl Pts',(-10.6524574839,-36.2942356128,-4.03375119461));
#70598=CARTESIAN_POINT('Ctrl Pts',(-10.0721843915,-37.9742356128,-4.97806710989));
#70599=CARTESIAN_POINT('Ctrl Pts',(-10.0721843915,-36.2942356128,-4.97806710989));
#70600=CARTESIAN_POINT('Ctrl Pts',(-9.82149842759,-37.9742356128,-5.3259548207));
#70601=CARTESIAN_POINT('Ctrl Pts',(-9.82149842759,-36.2942356128,-5.3259548207));
#70602=CARTESIAN_POINT('Ctrl Pts',(-9.23922565915,-37.9742356128,-6.04471661443));
#70603=CARTESIAN_POINT('Ctrl Pts',(-9.23922565915,-36.2942356128,-6.04471661443));
#70604=CARTESIAN_POINT('Ctrl Pts',(-8.58741395083,-37.9742356128,-6.694450027));
#70605=CARTESIAN_POINT('Ctrl Pts',(-8.58741395083,-36.2942356128,-6.694450027));
#70606=CARTESIAN_POINT('Ctrl Pts',(-8.21985964705,-37.9742356128,-7.02884209138));
#70607=CARTESIAN_POINT('Ctrl Pts',(-8.21985964705,-36.2942356128,-7.02884209138));
#70608=CARTESIAN_POINT('Ctrl Pts',(-7.71835943346,-37.9742356128,-7.44951290203));
#70609=CARTESIAN_POINT('Ctrl Pts',(-7.71835943346,-36.2942356128,-7.44951290203));
#70610=CARTESIAN_POINT('Ctrl Pts',(-7.20312714751,-37.9742356128,-7.83561707231));
#70611=CARTESIAN_POINT('Ctrl Pts',(-7.20312714751,-36.2942356128,-7.83561707231));
#70612=CARTESIAN_POINT('Ctrl Pts',(-7.07391925375,-37.9742356128,-7.9296599837));
#70613=CARTESIAN_POINT('Ctrl Pts',(-7.07391925375,-36.2942356128,-7.9296599837));
#70614=CARTESIAN_POINT('Ctrl Pts',(-6.68293897529,-37.9742356128,-8.20578167081));
#70615=CARTESIAN_POINT('Ctrl Pts',(-6.68293897529,-36.2942356128,-8.20578167081));
#70616=CARTESIAN_POINT('Ctrl Pts',(-6.28153293631,-37.9742356128,-8.46325996649));
#70617=CARTESIAN_POINT('Ctrl Pts',(-6.28153293631,-36.2942356128,-8.46325996649));
#70618=CARTESIAN_POINT('Ctrl Pts',(-6.0085344695,-37.9742356128,-8.62630121912));
#70619=CARTESIAN_POINT('Ctrl Pts',(-6.0085344695,-36.2942356128,-8.62630121912));
#70620=CARTESIAN_POINT('Ctrl Pts',(-5.45178039505,-37.9742356128,-8.9342344636));
#70621=CARTESIAN_POINT('Ctrl Pts',(-5.45178039505,-36.2942356128,-8.9342344636));
#70622=CARTESIAN_POINT('Ctrl Pts',(-4.87486658275,-37.9742356128,-9.20377818652));
#70623=CARTESIAN_POINT('Ctrl Pts',(-4.87486658275,-36.2942356128,-9.20377818652));
#70624=CARTESIAN_POINT('Ctrl Pts',(-4.58136980211,-37.9742356128,-9.32859973654));
#70625=CARTESIAN_POINT('Ctrl Pts',(-4.58136980211,-36.2942356128,-9.32859973654));
#70626=CARTESIAN_POINT('Ctrl Pts',(-4.06616678433,-37.9742356128,-9.5265559109));
#70627=CARTESIAN_POINT('Ctrl Pts',(-4.06616678433,-36.2942356128,-9.5265559109));
#70628=CARTESIAN_POINT('Ctrl Pts',(-3.53901439175,-37.9742356128,-9.69332241166));
#70629=CARTESIAN_POINT('Ctrl Pts',(-3.53901439175,-36.2942356128,-9.69332241166));
#70630=CARTESIAN_POINT('Ctrl Pts',(-3.31446912355,-37.9742356128,-9.75814914822));
#70631=CARTESIAN_POINT('Ctrl Pts',(-3.31446912355,-36.2942356128,-9.75814914822));
#70632=CARTESIAN_POINT('Ctrl Pts',(-3.01253146542,-37.9742356128,-9.83720045464));
#70633=CARTESIAN_POINT('Ctrl Pts',(-3.01253146542,-36.2942356128,-9.83720045464));
#70634=CARTESIAN_POINT('Ctrl Pts',(-2.70802102444,-37.9742356128,-9.90641220658));
#70635=CARTESIAN_POINT('Ctrl Pts',(-2.70802102444,-36.2942356128,-9.90641220658));
#70636=CARTESIAN_POINT('Ctrl Pts',(-2.63158870593,-37.9742356128,-9.9231347794));
#70637=CARTESIAN_POINT('Ctrl Pts',(-2.63158870593,-36.2942356128,-9.9231347794));
#70638=CARTESIAN_POINT('Ctrl Pts',(-2.47861794583,-37.9742356128,-9.95531796778));
#70639=CARTESIAN_POINT('Ctrl Pts',(-2.47861794583,-36.2942356128,-9.95531796778));
#70640=CARTESIAN_POINT('Ctrl Pts',(-2.32512404463,-37.9742356128,-9.9850708371));
#70641=CARTESIAN_POINT('Ctrl Pts',(-2.32512404463,-36.2942356128,-9.9850708371));
#70642=CARTESIAN_POINT('Ctrl Pts',(-2.24744160945,-37.9742356128,-9.99950190736));
#70643=CARTESIAN_POINT('Ctrl Pts',(-2.24744160945,-36.2942356128,-9.99950190736));
#70644=CARTESIAN_POINT('Ctrl Pts',(-2.0472685103,-37.9742356128,-10.0350233698));
#70645=CARTESIAN_POINT('Ctrl Pts',(-2.0472685103,-36.2942356128,-10.0350233698));
#70646=CARTESIAN_POINT('Ctrl Pts',(-1.83768542132,-37.9742356128,-10.0680136807));
#70647=CARTESIAN_POINT('Ctrl Pts',(-1.83768542132,-36.2942356128,-10.0680136807));
#70648=CARTESIAN_POINT('Ctrl Pts',(-1.68405004862,-37.9742356128,-10.0907690318));
#70649=CARTESIAN_POINT('Ctrl Pts',(-1.68405004862,-36.2942356128,-10.0907690318));
#70650=CARTESIAN_POINT('Ctrl Pts',(-1.54048434157,-37.9742356128,-10.1113387667));
#70651=CARTESIAN_POINT('Ctrl Pts',(-1.54048434157,-36.2942356128,-10.1113387667));
#70652=CARTESIAN_POINT('Ctrl Pts',(-1.38699292008,-37.9742356128,-10.1328356959));
#70653=CARTESIAN_POINT('Ctrl Pts',(-1.38699292008,-36.2942356128,-10.1328356959));
#70654=CARTESIAN_POINT('',(-1.38699292008,-37.2742356128,-10.1328356959));
#70655=CARTESIAN_POINT('Ctrl Pts',(1.38699292008,-36.5742356128,-10.1328356959));
#70656=CARTESIAN_POINT('Ctrl Pts',(1.38699292008,-36.4799878332,-10.1328356959));
#70657=CARTESIAN_POINT('Ctrl Pts',(1.38185951829,-36.3857400536,-10.0961824078));
#70658=CARTESIAN_POINT('Ctrl Pts',(1.37152733308,-36.3112466293,-10.0224089965));
#70659=CARTESIAN_POINT('Ctrl Pts',(1.35845523278,-36.2742356128,-9.92907216478));
#70660=CARTESIAN_POINT('Ctrl Pts',(1.34538313247,-36.2742356128,-9.83573533307));
#70661=CARTESIAN_POINT('Ctrl Pts',(1.11136534535,-36.5742356128,-10.1714381558));
#70662=CARTESIAN_POINT('Ctrl Pts',(1.11136534535,-36.4799878332,-10.1714381558));
#70663=CARTESIAN_POINT('Ctrl Pts',(1.1072586023,-36.3857400536,-10.1346410811));
#70664=CARTESIAN_POINT('Ctrl Pts',(1.09899281062,-36.3112466293,-10.0605782652));
#70665=CARTESIAN_POINT('Ctrl Pts',(1.08853507531,-36.2742356128,-9.96687528396));
#70666=CARTESIAN_POINT('Ctrl Pts',(1.07807734001,-36.2742356128,-9.87317230266));
#70667=CARTESIAN_POINT('Ctrl Pts',(0.834409330039,-36.5742356128,-10.2003869648));
#70668=CARTESIAN_POINT('Ctrl Pts',(0.834409340739,-36.4799878342,-10.2003869633));
#70669=CARTESIAN_POINT('Ctrl Pts',(0.831329379193,-36.3857400556,-10.1634827365));
#70670=CARTESIAN_POINT('Ctrl Pts',(0.825130215053,-36.3112466317,-10.0892042535));
#70671=CARTESIAN_POINT('Ctrl Pts',(0.817287134283,-36.2742356144,-9.99522841452));
#70672=CARTESIAN_POINT('Ctrl Pts',(0.809444049232,-36.2742356128,-9.90125257547));
#70673=CARTESIAN_POINT('Ctrl Pts',(0.556562377033,-36.5742356128,-10.2196842577));
#70674=CARTESIAN_POINT('Ctrl Pts',(0.556562398806,-36.4799878341,-10.2196842562));
#70675=CARTESIAN_POINT('Ctrl Pts',(0.554510558535,-36.3857400553,-10.1827090256));
#70676=CARTESIAN_POINT('Ctrl Pts',(0.550380660272,-36.3112466314,-10.1082876224));
#70677=CARTESIAN_POINT('Ctrl Pts',(0.545155596145,-36.2742356142,-10.0141309667));
#70678=CARTESIAN_POINT('Ctrl Pts',(0.539930523441,-36.2742356128,-9.91997431098));
#70679=CARTESIAN_POINT('Ctrl Pts',(5.42079519942E-6,-36.5742356128,-10.2389842343));
#70680=CARTESIAN_POINT('Ctrl Pts',(5.4533884471E-6,-36.4799878334,-10.2389842343));
#70681=CARTESIAN_POINT('Ctrl Pts',(4.06209988914E-6,-36.3857400539,-10.2019373985));
#70682=CARTESIAN_POINT('Ctrl Pts',(1.27978273706E-6,-36.3112466296,-10.1273718877));
#70683=CARTESIAN_POINT('Ctrl Pts',(-2.28441439194E-6,-36.274235613,-10.033032902));
#70684=CARTESIAN_POINT('Ctrl Pts',(-5.86138357242E-6,-36.2742356128,-9.93869391623));
#70685=CARTESIAN_POINT('Ctrl Pts',(-0.556573758695,-36.5742356128,-10.2196842429));
#70686=CARTESIAN_POINT('Ctrl Pts',(-0.556573737115,-36.4799878321,-10.2196842444));
#70687=CARTESIAN_POINT('Ctrl Pts',(-0.554519003891,-36.3857400514,-10.1827090156));
#70688=CARTESIAN_POINT('Ctrl Pts',(-0.550383451506,-36.3112466267,-10.1082876123));
#70689=CARTESIAN_POINT('Ctrl Pts',(-0.545151211684,-36.2742356111,-10.0141309554));
#70690=CARTESIAN_POINT('Ctrl Pts',(-0.539918980363,-36.2742356128,-9.91997429864));
#70691=CARTESIAN_POINT('Ctrl Pts',(-0.83438718174,-36.5742356128,-10.2003905389));
#70692=CARTESIAN_POINT('Ctrl Pts',(-0.834387171416,-36.4799878328,-10.2003905404));
#70693=CARTESIAN_POINT('Ctrl Pts',(-0.831312895645,-36.3857400527,-10.1634855111));
#70694=CARTESIAN_POINT('Ctrl Pts',(-0.825124969885,-36.3112466283,-10.0892054421));
#70695=CARTESIAN_POINT('Ctrl Pts',(-0.817296217687,-36.2742356121,-9.99522758151));
#70696=CARTESIAN_POINT('Ctrl Pts',(-0.809467469578,-36.2742356128,-9.90124972058));
#70697=CARTESIAN_POINT('Ctrl Pts',(-1.11138042468,-36.5742356128,-10.1714357354));
#70698=CARTESIAN_POINT('Ctrl Pts',(-1.11138042478,-36.4799878329,-10.1714357354));
#70699=CARTESIAN_POINT('Ctrl Pts',(-1.10726985602,-36.385740053,-10.1346391998));
#70700=CARTESIAN_POINT('Ctrl Pts',(-1.09899651827,-36.3112466286,-10.0605774471));
#70701=CARTESIAN_POINT('Ctrl Pts',(-1.08852917102,-36.2742356123,-9.96687582026));
#70702=CARTESIAN_POINT('Ctrl Pts',(-1.07806182375,-36.2742356128,-9.87317419359));
#70703=CARTESIAN_POINT('Ctrl Pts',(-1.38699292042,-36.5742356128,-10.1328356979));
#70704=CARTESIAN_POINT('Ctrl Pts',(-1.38699292042,-36.4799878332,-10.1328356979));
#70705=CARTESIAN_POINT('Ctrl Pts',(-1.3818595472,-36.3857400536,-10.0961824057));
#70706=CARTESIAN_POINT('Ctrl Pts',(-1.37152741947,-36.3112466294,-10.0224089864));
#70707=CARTESIAN_POINT('Ctrl Pts',(-1.3584553919,-36.2742356128,-9.92907214443));
#70708=CARTESIAN_POINT('Ctrl Pts',(-1.34538336432,-36.2742356128,-9.83573530247));
#70709=CARTESIAN_POINT('',(1.38699292008,-36.5742356128,-10.1328356959));
#70710=CARTESIAN_POINT('Origin',(1.34567723997399,-36.5721143211205,-9.83783613747388));
#70711=CARTESIAN_POINT('Origin',(1.27675647831893E-14,-36.5742356128,-2.72395521665914));
#70712=CARTESIAN_POINT('Ctrl Pts',(-1.34538263085,-38.2742356128,-9.83573538825));
#70713=CARTESIAN_POINT('Ctrl Pts',(-1.35845488787,-38.2742356128,-9.92907219763));
#70714=CARTESIAN_POINT('Ctrl Pts',(-1.37152714489,-38.2372245963,-10.022409007));
#70715=CARTESIAN_POINT('Ctrl Pts',(-1.38185945397,-38.1627311721,-10.0961824006));
#70716=CARTESIAN_POINT('Ctrl Pts',(-1.3869929173,-38.0684833924,-10.13283568));
#70717=CARTESIAN_POINT('Ctrl Pts',(-1.3869929173,-37.9742356128,-10.13283568));
#70718=CARTESIAN_POINT('Ctrl Pts',(-1.07805458856,-38.2742356128,-9.87317534285));
#70719=CARTESIAN_POINT('Ctrl Pts',(-1.08852516046,-38.2742356128,-9.96687652205));
#70720=CARTESIAN_POINT('Ctrl Pts',(-1.09899573236,-38.2372245963,-10.0605777012));
#70721=CARTESIAN_POINT('Ctrl Pts',(-1.10727163244,-38.1627311721,-10.1346390981));
#70722=CARTESIAN_POINT('Ctrl Pts',(-1.11138345406,-38.0684833924,-10.1714354597));
#70723=CARTESIAN_POINT('Ctrl Pts',(-1.11138345406,-37.9742356128,-10.1714354597));
#70724=CARTESIAN_POINT('Ctrl Pts',(-0.809472541664,-38.2742356128,-9.90124868745));
#70725=CARTESIAN_POINT('Ctrl Pts',(-0.817296138563,-38.2742356128,-9.99522725993));
#70726=CARTESIAN_POINT('Ctrl Pts',(-0.825119735463,-38.2372245963,-10.0892058324));
#70727=CARTESIAN_POINT('Ctrl Pts',(-0.83130356121,-38.1627311721,-10.1634864674));
#70728=CARTESIAN_POINT('Ctrl Pts',(-0.83437582405,-38.0684833924,-10.2003917745));
#70729=CARTESIAN_POINT('Ctrl Pts',(-0.83437582405,-37.9742356128,-10.2003917745));
#70730=CARTESIAN_POINT('Ctrl Pts',(-0.539912794952,-38.2742356128,-9.91997481745));
#70731=CARTESIAN_POINT('Ctrl Pts',(-0.545145819039,-38.2742356128,-10.0141312189));
#70732=CARTESIAN_POINT('Ctrl Pts',(-0.550378843126,-38.2372245963,-10.1082876203));
#70733=CARTESIAN_POINT('Ctrl Pts',(-0.554515025793,-38.1627311721,-10.1827088234));
#70734=CARTESIAN_POINT('Ctrl Pts',(-0.556570027967,-38.0684833924,-10.2196839516));
#70735=CARTESIAN_POINT('Ctrl Pts',(-0.556570027967,-37.9742356128,-10.2196839516));
#70736=CARTESIAN_POINT('Ctrl Pts',(-6.58122985814E-6,-38.2742356128,-9.93869363588));
#70737=CARTESIAN_POINT('Ctrl Pts',(-2.11071485614E-6,-38.2742356128,-10.0330328354));
#70738=CARTESIAN_POINT('Ctrl Pts',(2.35980014682E-6,-38.2372245963,-10.1273720349));
#70739=CARTESIAN_POINT('Ctrl Pts',(5.89487381069E-6,-38.1627311721,-10.2019377133));
#70740=CARTESIAN_POINT('Ctrl Pts',(7.64886135792E-6,-38.0684833924,-10.2389846345));
#70741=CARTESIAN_POINT('Ctrl Pts',(7.64886135792E-6,-37.9742356128,-10.2389846345));
#70742=CARTESIAN_POINT('Ctrl Pts',(0.539931096955,-38.2742356128,-9.91997471322));
#70743=CARTESIAN_POINT('Ctrl Pts',(0.545155312685,-38.2742356128,-10.0141311006));
#70744=CARTESIAN_POINT('Ctrl Pts',(0.550379528416,-38.2372245963,-10.1082874879));
#70745=CARTESIAN_POINT('Ctrl Pts',(0.554508745802,-38.1627311721,-10.18270868));
#70746=CARTESIAN_POINT('Ctrl Pts',(0.556560292102,-38.0684833924,-10.2196838026));
#70747=CARTESIAN_POINT('Ctrl Pts',(0.556560292102,-37.9742356128,-10.2196838026));
#70748=CARTESIAN_POINT('Ctrl Pts',(0.809437211467,-38.2742356128,-9.90125321466));
#70749=CARTESIAN_POINT('Ctrl Pts',(0.817279129002,-38.2742356128,-9.99522921039));
#70750=CARTESIAN_POINT('Ctrl Pts',(0.825121046537,-38.2372245963,-10.0892052061));
#70751=CARTESIAN_POINT('Ctrl Pts',(0.831319359229,-38.1627311721,-10.1634838037));
#70752=CARTESIAN_POINT('Ctrl Pts',(0.834398810248,-38.0684833924,-10.2003880997));
#70753=CARTESIAN_POINT('Ctrl Pts',(0.834398810248,-37.9742356128,-10.2003880997));
#70754=CARTESIAN_POINT('Ctrl Pts',(1.07807579453,-38.2742356128,-9.87317251911));
#70755=CARTESIAN_POINT('Ctrl Pts',(1.08853351472,-38.2742356128,-9.96687550252));
#70756=CARTESIAN_POINT('Ctrl Pts',(1.09899123491,-38.2372245963,-10.0605784859));
#70757=CARTESIAN_POINT('Ctrl Pts',(1.10725697278,-38.1627311721,-10.1346413093));
#70758=CARTESIAN_POINT('Ctrl Pts',(1.11136375176,-38.0684833924,-10.171438379));
#70759=CARTESIAN_POINT('Ctrl Pts',(1.11136375176,-37.9742356128,-10.171438379));
#70760=CARTESIAN_POINT('Ctrl Pts',(1.34538313247,-38.2742356128,-9.83573533307));
#70761=CARTESIAN_POINT('Ctrl Pts',(1.35845523278,-38.2742356128,-9.92907216478));
#70762=CARTESIAN_POINT('Ctrl Pts',(1.37152733308,-38.2372245963,-10.0224089965));
#70763=CARTESIAN_POINT('Ctrl Pts',(1.38185951829,-38.1627311721,-10.0961824078));
#70764=CARTESIAN_POINT('Ctrl Pts',(1.38699292008,-38.0684833924,-10.1328356959));
#70765=CARTESIAN_POINT('Ctrl Pts',(1.38699292008,-37.9742356128,-10.1328356959));
#70766=CARTESIAN_POINT('',(1.38700644577,-37.9742356128,-10.1328338118));
#70767=CARTESIAN_POINT('Origin',(1.34569970434081,-37.9763569227614,-9.83783301687873));
#70768=CARTESIAN_POINT('Origin',(0.,-37.9742356128,-2.72395521670843));
#70769=CARTESIAN_POINT('Ctrl Pts',(-1.38699292008,-37.9742356128,-10.1328356959));
#70770=CARTESIAN_POINT('Ctrl Pts',(-1.38699292008,-36.2942356128,-10.1328356959));
#70771=CARTESIAN_POINT('Ctrl Pts',(-0.835781068554,-37.9742356128,-10.2100345517));
#70772=CARTESIAN_POINT('Ctrl Pts',(-0.835781068554,-36.2942356128,-10.2100345517));
#70773=CARTESIAN_POINT('Ctrl Pts',(-0.27919124227,-37.9742356128,-10.2486339796));
#70774=CARTESIAN_POINT('Ctrl Pts',(-0.27919124227,-36.2942356128,-10.2486339796));
#70775=CARTESIAN_POINT('Ctrl Pts',(0.27919124227,-37.9742356128,-10.2486339796));
#70776=CARTESIAN_POINT('Ctrl Pts',(0.27919124227,-36.2942356128,-10.2486339796));
#70777=CARTESIAN_POINT('Ctrl Pts',(0.835781068554,-37.9742356128,-10.2100345517));
#70778=CARTESIAN_POINT('Ctrl Pts',(0.835781068554,-36.2942356128,-10.2100345517));
#70779=CARTESIAN_POINT('Ctrl Pts',(1.38699292008,-37.9742356128,-10.1328356959));
#70780=CARTESIAN_POINT('Ctrl Pts',(1.38699292008,-36.2942356128,-10.1328356959));
#70781=CARTESIAN_POINT('',(1.38699292008,-37.2742356128,-10.1328356959));
#70782=CARTESIAN_POINT('Ctrl Pts',(11.0450673604,-36.5742356128,0.80065078572));
#70783=CARTESIAN_POINT('Ctrl Pts',(11.045067361,-36.4799878332,0.800650781683));
#70784=CARTESIAN_POINT('Ctrl Pts',(11.0085027593,-36.3857400536,0.794919704988));
#70785=CARTESIAN_POINT('Ctrl Pts',(10.9349078496,-36.3112466293,0.783384562601));
#70786=CARTESIAN_POINT('Ctrl Pts',(10.8417968545,-36.2742356128,0.768790504329));
#70787=CARTESIAN_POINT('Ctrl Pts',(10.7486858592,-36.2742356128,0.754196447643));
#70788=CARTESIAN_POINT('Ctrl Pts',(11.1590945635,-36.5742356128,0.0731427823434));
#70789=CARTESIAN_POINT('Ctrl Pts',(11.1590943539,-36.4799878336,0.0731441086594));
#70790=CARTESIAN_POINT('Ctrl Pts',(11.122250057,-36.3857400543,0.0691974113034));
#70791=CARTESIAN_POINT('Ctrl Pts',(11.0480924687,-36.3112466301,0.0612520226421));
#70792=CARTESIAN_POINT('Ctrl Pts',(10.9542697034,-36.2742356134,0.051198890854));
#70793=CARTESIAN_POINT('Ctrl Pts',(10.8604470201,-36.2742356128,0.0411452401641));
#70794=CARTESIAN_POINT('Ctrl Pts',(11.2300205496,-36.5742356128,-0.665529030045));
#70795=CARTESIAN_POINT('Ctrl Pts',(11.2300208596,-36.4799878483,-0.66553104165));
#70796=CARTESIAN_POINT('Ctrl Pts',(11.1930302198,-36.3857400837,-0.667764985107));
#70797=CARTESIAN_POINT('Ctrl Pts',(11.1185774042,-36.3112466648,-0.672258707664));
#70798=CARTESIAN_POINT('Ctrl Pts',(11.0243808176,-36.2742356365,-0.677942925129));
#70799=CARTESIAN_POINT('Ctrl Pts',(10.9301841004,-36.2742356128,-0.683626353818));
#70800=CARTESIAN_POINT('Ctrl Pts',(11.2586691615,-36.5742356128,-1.43857902297));
#70801=CARTESIAN_POINT('Ctrl Pts',(11.2586691082,-36.4799878202,-1.43857844952));
#70802=CARTESIAN_POINT('Ctrl Pts',(11.2213359158,-36.3857400276,-1.43764120566));
#70803=CARTESIAN_POINT('Ctrl Pts',(11.1461941074,-36.3112465987,-1.43575552205));
#70804=CARTESIAN_POINT('Ctrl Pts',(11.0511260388,-36.2742355924,-1.43337012132));
#70805=CARTESIAN_POINT('Ctrl Pts',(10.956057999,-36.2742356128,-1.43098494596));
#70806=CARTESIAN_POINT('Ctrl Pts',(11.1287255199,-36.5742356128,-2.62842434011));
#70807=CARTESIAN_POINT('Ctrl Pts',(11.1287255488,-36.4799878403,-2.62842465101));
#70808=CARTESIAN_POINT('Ctrl Pts',(11.0920269838,-36.3857400677,-2.62101538779));
#70809=CARTESIAN_POINT('Ctrl Pts',(11.0181624037,-36.311246646,-2.60610209162));
#70810=CARTESIAN_POINT('Ctrl Pts',(10.9247102077,-36.2742356239,-2.5872338689));
#70811=CARTESIAN_POINT('Ctrl Pts',(10.831257996,-36.2742356128,-2.56836552398));
#70812=CARTESIAN_POINT('Ctrl Pts',(10.7310385841,-36.5742356128,-3.75973072379));
#70813=CARTESIAN_POINT('Ctrl Pts',(10.7310385684,-36.4799878294,-3.75973055523));
#70814=CARTESIAN_POINT('Ctrl Pts',(10.6966894642,-36.385740046,-3.74560929459));
#70815=CARTESIAN_POINT('Ctrl Pts',(10.6275537888,-36.3112466203,-3.71718713519));
#70816=CARTESIAN_POINT('Ctrl Pts',(10.54008455,-36.2742356068,-3.68122801356));
#70817=CARTESIAN_POINT('Ctrl Pts',(10.4526153195,-36.2742356128,-3.64526895817));
#70818=CARTESIAN_POINT('Ctrl Pts',(10.5562244357,-36.5742356128,-4.14577572839));
#70819=CARTESIAN_POINT('Ctrl Pts',(10.5562244337,-36.4799878354,-4.14577573503));
#70820=CARTESIAN_POINT('Ctrl Pts',(10.5229141043,-36.385740058,-4.12938259431));
#70821=CARTESIAN_POINT('Ctrl Pts',(10.4558691905,-36.3112466344,-4.09638751326));
#70822=CARTESIAN_POINT('Ctrl Pts',(10.3710451368,-36.2742356162,-4.05464270841));
#70823=CARTESIAN_POINT('Ctrl Pts',(10.2862210827,-36.2742356128,-4.01289790025));
#70824=CARTESIAN_POINT('Ctrl Pts',(10.1185165315,-36.5742356128,-4.93605874865));
#70825=CARTESIAN_POINT('Ctrl Pts',(10.1185165338,-36.4799878308,-4.93605874107));
#70826=CARTESIAN_POINT('Ctrl Pts',(10.0876389665,-36.3857400487,-4.9153527052));
#70827=CARTESIAN_POINT('Ctrl Pts',(10.0254905563,-36.3112466235,-4.8736769201));
#70828=CARTESIAN_POINT('Ctrl Pts',(9.94686147247,-36.274235609,-4.82094944962));
#70829=CARTESIAN_POINT('Ctrl Pts',(9.868232389,-36.2742356128,-4.76822198291));
#70830=CARTESIAN_POINT('Ctrl Pts',(9.56890441447,-36.5742356128,-5.65332240208));
#70831=CARTESIAN_POINT('Ctrl Pts',(9.56890441181,-36.4799878361,-5.65332241073));
#70832=CARTESIAN_POINT('Ctrl Pts',(9.54035667914,-36.3857400593,-5.62965790004));
#70833=CARTESIAN_POINT('Ctrl Pts',(9.48289761876,-36.311246636,-5.5820274647));
#70834=CARTESIAN_POINT('Ctrl Pts',(9.41020141946,-36.2742356173,-5.52176626379));
#70835=CARTESIAN_POINT('Ctrl Pts',(9.33750521971,-36.2742356128,-5.46150505857));
#70836=CARTESIAN_POINT('Ctrl Pts',(9.25594847982,-36.5742356128,-6.01159034787));
#70837=CARTESIAN_POINT('Ctrl Pts',(9.2559484841,-36.4799878361,-6.01159034444));
#70838=CARTESIAN_POINT('Ctrl Pts',(9.22850758179,-36.3857400593,-5.98668964763));
#70839=CARTESIAN_POINT('Ctrl Pts',(9.17327627072,-36.311246636,-5.93657111006));
#70840=CARTESIAN_POINT('Ctrl Pts',(9.10339857703,-36.2742356173,-5.87316201272));
#70841=CARTESIAN_POINT('Ctrl Pts',(9.03352088058,-36.2742356128,-5.80975291532));
#70842=CARTESIAN_POINT('Ctrl Pts',(8.60187015157,-36.5742356128,-6.68997127933));
#70843=CARTESIAN_POINT('Ctrl Pts',(8.60187014738,-36.4799878305,-6.68997128269));
#70844=CARTESIAN_POINT('Ctrl Pts',(8.57641889755,-36.3857400481,-6.66302157178));
#70845=CARTESIAN_POINT('Ctrl Pts',(8.52519224274,-36.3112466228,-6.60877890052));
#70846=CARTESIAN_POINT('Ctrl Pts',(8.46038117687,-36.2742356085,-6.54015201885));
#70847=CARTESIAN_POINT('Ctrl Pts',(8.39557011371,-36.2742356128,-6.47152513724));
#70848=CARTESIAN_POINT('Ctrl Pts',(7.89889535824,-36.5742356128,-7.30184497632));
#70849=CARTESIAN_POINT('Ctrl Pts',(7.89889536235,-36.479987836,-7.30184497303));
#70850=CARTESIAN_POINT('Ctrl Pts',(7.87520178124,-36.3857400591,-7.27338138171));
#70851=CARTESIAN_POINT('Ctrl Pts',(7.82751284046,-36.3112466358,-7.21609167633));
#70852=CARTESIAN_POINT('Ctrl Pts',(7.76717762213,-36.2742356171,-7.14360974255));
#70853=CARTESIAN_POINT('Ctrl Pts',(7.70684240115,-36.2742356128,-7.07112780873));
#70854=CARTESIAN_POINT('Ctrl Pts',(7.54206117235,-36.5742356128,-7.58966580122));
#70855=CARTESIAN_POINT('Ctrl Pts',(7.5420611681,-36.4799878303,-7.58966580444));
#70856=CARTESIAN_POINT('Ctrl Pts',(7.51923353688,-36.3857400477,-7.56050216317));
#70857=CARTESIAN_POINT('Ctrl Pts',(7.47328753544,-36.3112466223,-7.50180343345));
#70858=CARTESIAN_POINT('Ctrl Pts',(7.41515745994,-36.2742356082,-7.42753882464));
#70859=CARTESIAN_POINT('Ctrl Pts',(7.35702738724,-36.2742356128,-7.35327421602));
#70860=CARTESIAN_POINT('Ctrl Pts',(6.81974100977,-36.5742356128,-8.12924918963));
#70861=CARTESIAN_POINT('Ctrl Pts',(6.81974101401,-36.4799878362,-8.12924918643));
#70862=CARTESIAN_POINT('Ctrl Pts',(6.79873299015,-36.3857400596,-8.09871470869));
#70863=CARTESIAN_POINT('Ctrl Pts',(6.75644936833,-36.3112466363,-8.03725685438));
#70864=CARTESIAN_POINT('Ctrl Pts',(6.70295286504,-36.2742356175,-7.95950145129));
#70865=CARTESIAN_POINT('Ctrl Pts',(6.64945635896,-36.2742356128,-7.88174604801));
#70866=CARTESIAN_POINT('Ctrl Pts',(6.05811766031,-36.5742356128,-8.60451307516));
#70867=CARTESIAN_POINT('Ctrl Pts',(6.05811765609,-36.4799878303,-8.60451307836));
#70868=CARTESIAN_POINT('Ctrl Pts',(6.03938391395,-36.3857400477,-8.57254968367));
#70869=CARTESIAN_POINT('Ctrl Pts',(6.00167783198,-36.3112466224,-8.50821578835));
#70870=CARTESIAN_POINT('Ctrl Pts',(5.95397275891,-36.2742356082,-8.42682166631));
#70871=CARTESIAN_POINT('Ctrl Pts',(5.90626768861,-36.2742356128,-8.34542754446));
#70872=CARTESIAN_POINT('Ctrl Pts',(5.66726526532,-36.5742356128,-8.82396239702));
#70873=CARTESIAN_POINT('Ctrl Pts',(5.66726527346,-36.4799878325,-8.82396239323));
#70874=CARTESIAN_POINT('Ctrl Pts',(5.64974730298,-36.3857400521,-8.79131270234));
#70875=CARTESIAN_POINT('Ctrl Pts',(5.6144882341,-36.3112466275,-8.72559748206));
#70876=CARTESIAN_POINT('Ctrl Pts',(5.56987907103,-36.2742356116,-8.64245573545));
#70877=CARTESIAN_POINT('Ctrl Pts',(5.52526990488,-36.2742356128,-8.5593139908));
#70878=CARTESIAN_POINT('Ctrl Pts',(5.06534643699,-36.5742356128,-9.12478048112));
#70879=CARTESIAN_POINT('Ctrl Pts',(5.06534643293,-36.4799878336,-9.12478048301));
#70880=CARTESIAN_POINT('Ctrl Pts',(5.04976009616,-36.3857400544,-9.09116389237));
#70881=CARTESIAN_POINT('Ctrl Pts',(5.01838891207,-36.3112466303,-9.02350255063));
#70882=CARTESIAN_POINT('Ctrl Pts',(4.97869864017,-36.2742356134,-8.93789860125));
#70883=CARTESIAN_POINT('Ctrl Pts',(4.93900836982,-36.2742356128,-8.8522946509));
#70884=CARTESIAN_POINT('Ctrl Pts',(4.44254377917,-36.5742356128,-9.38061203627));
#70885=CARTESIAN_POINT('Ctrl Pts',(4.44254378121,-36.479987833,-9.38061203532));
#70886=CARTESIAN_POINT('Ctrl Pts',(4.42898621881,-36.3857400532,-9.3461619704));
#70887=CARTESIAN_POINT('Ctrl Pts',(4.40169841545,-36.3112466289,-9.27682306804));
#70888=CARTESIAN_POINT('Ctrl Pts',(4.36717436193,-36.2742356125,-9.18909670022));
#70889=CARTESIAN_POINT('Ctrl Pts',(4.33265030764,-36.2742356128,-9.10137033288));
#70890=CARTESIAN_POINT('Ctrl Pts',(4.23279656972,-36.5742356128,-9.46077263537));
#70891=CARTESIAN_POINT('Ctrl Pts',(4.23279657536,-36.4799878331,-9.46077263319));
#70892=CARTESIAN_POINT('Ctrl Pts',(4.21992355351,-36.3857400533,-9.42606097103));
#70893=CARTESIAN_POINT('Ctrl Pts',(4.19401354548,-36.3112466289,-9.35619554385));
#70894=CARTESIAN_POINT('Ctrl Pts',(4.16123265235,-36.2742356126,-9.26780302676));
#70895=CARTESIAN_POINT('Ctrl Pts',(4.12845175702,-36.2742356128,-9.17941051062));
#70896=CARTESIAN_POINT('Ctrl Pts',(3.80923512589,-36.5742356128,-9.61074441909));
#70897=CARTESIAN_POINT('Ctrl Pts',(3.80923513444,-36.4799878343,-9.61074441627));
#70898=CARTESIAN_POINT('Ctrl Pts',(3.79773947086,-36.3857400557,-9.57554539274));
#70899=CARTESIAN_POINT('Ctrl Pts',(3.77460171857,-36.3112466318,-9.50469903632));
#70900=CARTESIAN_POINT('Ctrl Pts',(3.74532823308,-36.2742356145,-9.4150654646));
#70901=CARTESIAN_POINT('Ctrl Pts',(3.716054744,-36.2742356128,-9.32543189337));
#70902=CARTESIAN_POINT('Ctrl Pts',(3.37823722599,-36.5742356128,-9.73997950077));
#70903=CARTESIAN_POINT('Ctrl Pts',(3.37823723183,-36.4799878348,-9.73997949916));
#70904=CARTESIAN_POINT('Ctrl Pts',(3.36812208699,-36.3857400568,-9.7043667315));
#70905=CARTESIAN_POINT('Ctrl Pts',(3.34776295853,-36.3112466331,-9.63268761569));
#70906=CARTESIAN_POINT('Ctrl Pts',(3.32200494097,-36.2742356153,-9.54200045039));
#70907=CARTESIAN_POINT('Ctrl Pts',(3.29624692084,-36.2742356128,-9.45131328477));
#70908=CARTESIAN_POINT('Ctrl Pts',(3.16149193513,-36.5742356128,-9.79931128721));
#70909=CARTESIAN_POINT('Ctrl Pts',(3.16149192019,-36.4799878339,-9.7993112903));
#70910=CARTESIAN_POINT('Ctrl Pts',(3.15207526541,-36.3857400549,-9.76350879732));
#70911=CARTESIAN_POINT('Ctrl Pts',(3.13312203699,-36.3112466308,-9.69144780897));
#70912=CARTESIAN_POINT('Ctrl Pts',(3.10914275311,-36.2742356138,-9.60027750259));
#70913=CARTESIAN_POINT('Ctrl Pts',(3.085163475,-36.2742356128,-9.50910719462));
#70914=CARTESIAN_POINT('Ctrl Pts',(2.82069093435,-36.5742356128,-9.88383207656));
#70915=CARTESIAN_POINT('Ctrl Pts',(2.82069094264,-36.4799878329,-9.88383207485));
#70916=CARTESIAN_POINT('Ctrl Pts',(2.81231719671,-36.3857400529,-9.84777000922));
#70917=CARTESIAN_POINT('Ctrl Pts',(2.79546304335,-36.3112466285,-9.77518657496));
#70918=CARTESIAN_POINT('Ctrl Pts',(2.77413945741,-36.2742356123,-9.68335528262));
#70919=CARTESIAN_POINT('Ctrl Pts',(2.75281586826,-36.2742356128,-9.59152399117));
#70920=CARTESIAN_POINT('Ctrl Pts',(2.4779858176,-36.5742356128,-9.95579014891));
#70921=CARTESIAN_POINT('Ctrl Pts',(2.47798581299,-36.4799878334,-9.95579014986));
#70922=CARTESIAN_POINT('Ctrl Pts',(2.47066165835,-36.385740054,-9.91950820283));
#70923=CARTESIAN_POINT('Ctrl Pts',(2.45592006997,-36.3112466298,-9.84648220223));
#70924=CARTESIAN_POINT('Ctrl Pts',(2.43726927277,-36.2742356132,-9.75409098075));
#70925=CARTESIAN_POINT('Ctrl Pts',(2.41861847736,-36.2742356128,-9.66169975877));
#70926=CARTESIAN_POINT('Ctrl Pts',(2.35465529944,-36.5742356128,-9.98006182258));
#70927=CARTESIAN_POINT('Ctrl Pts',(2.35465523153,-36.4799878333,-9.98006183247));
#70928=CARTESIAN_POINT('Ctrl Pts',(2.34769194242,-36.3857400538,-9.94370911603));
#70929=CARTESIAN_POINT('Ctrl Pts',(2.33367676219,-36.3112466296,-9.87054066385));
#70930=CARTESIAN_POINT('Ctrl Pts',(2.31594504154,-36.274235613,-9.77796920984));
#70931=CARTESIAN_POINT('Ctrl Pts',(2.29821334717,-36.2742356128,-9.68539775193));
#70932=CARTESIAN_POINT('Ctrl Pts',(2.10245396246,-36.5742356128,-10.0263413789));
#70933=CARTESIAN_POINT('Ctrl Pts',(2.10245403384,-36.4799878331,-10.0263413685));
#70934=CARTESIAN_POINT('Ctrl Pts',(2.09626771326,-36.3857400534,-9.98984574067));
#70935=CARTESIAN_POINT('Ctrl Pts',(2.08381618659,-36.3112466291,-9.91638967147));
#70936=CARTESIAN_POINT('Ctrl Pts',(2.06806269103,-36.2742356127,-9.82345434149));
#70937=CARTESIAN_POINT('Ctrl Pts',(2.05230916782,-36.2742356128,-9.73051901561));
#70938=CARTESIAN_POINT('Ctrl Pts',(1.84363587601,-36.5742356128,-10.0671337109));
#70939=CARTESIAN_POINT('Ctrl Pts',(1.84363580098,-36.4799878334,-10.0671337218));
#70940=CARTESIAN_POINT('Ctrl Pts',(1.8381321438,-36.3857400539,-10.0305323548));
#70941=CARTESIAN_POINT('Ctrl Pts',(1.82705483329,-36.3112466296,-9.95686343242));
#70942=CARTESIAN_POINT('Ctrl Pts',(1.8130400557,-36.274235613,-9.863658792));
#70943=CARTESIAN_POINT('Ctrl Pts',(1.79902530718,-36.2742356128,-9.77045414726));
#70944=CARTESIAN_POINT('Ctrl Pts',(1.68657601118,-36.5742356128,-10.090407293));
#70945=CARTESIAN_POINT('Ctrl Pts',(1.68657610781,-36.4799878388,-10.0904072805));
#70946=CARTESIAN_POINT('Ctrl Pts',(1.68120354795,-36.3857400648,-10.0537882489));
#70947=CARTESIAN_POINT('Ctrl Pts',(1.67038985815,-36.3112466425,-9.98008380584));
#70948=CARTESIAN_POINT('Ctrl Pts',(1.65670851502,-36.2742356216,-9.88683423583));
#70949=CARTESIAN_POINT('Ctrl Pts',(1.643027135,-36.2742356128,-9.79358466713));
#70950=CARTESIAN_POINT('Ctrl Pts',(1.54071990404,-36.5742356128,-10.1113057482));
#70951=CARTESIAN_POINT('Ctrl Pts',(1.54071964237,-36.4799878332,-10.1113057849));
#70952=CARTESIAN_POINT('Ctrl Pts',(1.53549875184,-36.3857400535,-10.0746647498));
#70953=CARTESIAN_POINT('Ctrl Pts',(1.52499081167,-36.3112466292,-10.0009159536));
#70954=CARTESIAN_POINT('Ctrl Pts',(1.51169650293,-36.2742356128,-9.90761024282));
#70955=CARTESIAN_POINT('Ctrl Pts',(1.49840229593,-36.2742356128,-9.81430451786));
#70956=CARTESIAN_POINT('Ctrl Pts',(1.38699270387,-36.5742356128,-10.132835726));
#70957=CARTESIAN_POINT('Ctrl Pts',(1.38699270126,-36.4799878332,-10.1328357264));
#70958=CARTESIAN_POINT('Ctrl Pts',(1.38185929484,-36.3857400536,-10.0961824389));
#70959=CARTESIAN_POINT('Ctrl Pts',(1.37152710348,-36.3112466293,-10.0224090285));
#70960=CARTESIAN_POINT('Ctrl Pts',(1.35845499699,-36.2742356128,-9.92907219764));
#70961=CARTESIAN_POINT('Ctrl Pts',(1.34538289151,-36.2742356128,-9.83573536665));
#70962=CARTESIAN_POINT('',(11.0450673741,-36.5742356128,0.800650704934));
#70963=CARTESIAN_POINT('Origin',(10.7507791129301,-36.5721142936209,0.754540830736387));
#70964=CARTESIAN_POINT('Ctrl Pts',(11.0450673741,-36.5742356128,0.800650704934));
#70965=CARTESIAN_POINT('Ctrl Pts',(11.0585597994,-36.5742356128,0.714566551433));
#70966=CARTESIAN_POINT('Ctrl Pts',(11.0714556362,-36.5742356128,0.628315856355));
#70967=CARTESIAN_POINT('Ctrl Pts',(11.0837537732,-36.5742356128,0.541839826087));
#70968=CARTESIAN_POINT('Ctrl Pts',(11.1309935407,-36.5742356128,0.191196052993));
#70969=CARTESIAN_POINT('Ctrl Pts',(11.1677658434,-36.5742356128,-0.163547364245));
#70970=CARTESIAN_POINT('Ctrl Pts',(11.1889875368,-36.5742356128,-0.434883867498));
#70971=CARTESIAN_POINT('Ctrl Pts',(11.2336540706,-36.5742356128,-1.36618233638));
#70972=CARTESIAN_POINT('Ctrl Pts',(11.1622899815,-36.5742356128,-2.31636115629));
#70973=CARTESIAN_POINT('Ctrl Pts',(11.0291793988,-36.5742356128,-2.98459593105));
#70974=CARTESIAN_POINT('Ctrl Pts',(10.6524574839,-36.5742356128,-4.03375119457));
#70975=CARTESIAN_POINT('Ctrl Pts',(10.0721843915,-36.5742356128,-4.97806710985));
#70976=CARTESIAN_POINT('Ctrl Pts',(9.82149842762,-36.5742356128,-5.32595482066));
#70977=CARTESIAN_POINT('Ctrl Pts',(9.23922565917,-36.5742356128,-6.0447166144));
#70978=CARTESIAN_POINT('Ctrl Pts',(8.58741395086,-36.5742356128,-6.69445002697));
#70979=CARTESIAN_POINT('Ctrl Pts',(8.21985964708,-36.5742356128,-7.02884209136));
#70980=CARTESIAN_POINT('Ctrl Pts',(7.71835943349,-36.5742356128,-7.44951290201));
#70981=CARTESIAN_POINT('Ctrl Pts',(7.20312714754,-36.5742356128,-7.83561707229));
#70982=CARTESIAN_POINT('Ctrl Pts',(7.07391925378,-36.5742356128,-7.92965998368));
#70983=CARTESIAN_POINT('Ctrl Pts',(6.68293897532,-36.5742356128,-8.20578167079));
#70984=CARTESIAN_POINT('Ctrl Pts',(6.28153293634,-36.5742356128,-8.46325996647));
#70985=CARTESIAN_POINT('Ctrl Pts',(6.00853446953,-36.5742356128,-8.62630121911));
#70986=CARTESIAN_POINT('Ctrl Pts',(5.45178039508,-36.5742356128,-8.93423446359));
#70987=CARTESIAN_POINT('Ctrl Pts',(4.87486658279,-36.5742356128,-9.2037781865));
#70988=CARTESIAN_POINT('Ctrl Pts',(4.58136980215,-36.5742356128,-9.32859973652));
#70989=CARTESIAN_POINT('Ctrl Pts',(4.06616678437,-36.5742356128,-9.52655591089));
#70990=CARTESIAN_POINT('Ctrl Pts',(3.53901439179,-36.5742356128,-9.69332241165));
#70991=CARTESIAN_POINT('Ctrl Pts',(3.31446912359,-36.5742356128,-9.75814914821));
#70992=CARTESIAN_POINT('Ctrl Pts',(3.01253146546,-36.5742356128,-9.83720045464));
#70993=CARTESIAN_POINT('Ctrl Pts',(2.70802102447,-36.5742356128,-9.90641220657));
#70994=CARTESIAN_POINT('Ctrl Pts',(2.63158870596,-36.5742356128,-9.92313477939));
#70995=CARTESIAN_POINT('Ctrl Pts',(2.47861794588,-36.5742356128,-9.95531796777));
#70996=CARTESIAN_POINT('Ctrl Pts',(2.32512404468,-36.5742356128,-9.98507083709));
#70997=CARTESIAN_POINT('Ctrl Pts',(2.24744160945,-36.5742356128,-9.99950190736));
#70998=CARTESIAN_POINT('Ctrl Pts',(2.04726851031,-36.5742356128,-10.0350233698));
#70999=CARTESIAN_POINT('Ctrl Pts',(1.83768542134,-36.5742356128,-10.0680136806));
#71000=CARTESIAN_POINT('Ctrl Pts',(1.68405004863,-36.5742356128,-10.0907690318));
#71001=CARTESIAN_POINT('Ctrl Pts',(1.54048434157,-36.5742356128,-10.1113387667));
#71002=CARTESIAN_POINT('Ctrl Pts',(1.38699292008,-36.5742356128,-10.1328356959));
#71003=CARTESIAN_POINT('Ctrl Pts',(1.3453969549,-38.2742356128,-9.83573340734));
#71004=CARTESIAN_POINT('Ctrl Pts',(1.35846896198,-38.2742356128,-9.92907025215));
#71005=CARTESIAN_POINT('Ctrl Pts',(1.37154096907,-38.2372245963,-10.022407097));
#71006=CARTESIAN_POINT('Ctrl Pts',(1.38187308059,-38.1627311721,-10.0961805186));
#71007=CARTESIAN_POINT('Ctrl Pts',(1.38700644577,-38.0684833924,-10.1328338118));
#71008=CARTESIAN_POINT('Ctrl Pts',(1.38700644577,-37.9742356128,-10.1328338118));
#71009=CARTESIAN_POINT('Ctrl Pts',(1.48744214824,-38.2742356128,-9.81583956161));
#71010=CARTESIAN_POINT('Ctrl Pts',(1.50072194506,-38.2742356128,-9.9091473051));
#71011=CARTESIAN_POINT('Ctrl Pts',(1.51400174188,-38.2372245963,-10.0024550486));
#71012=CARTESIAN_POINT('Ctrl Pts',(1.52449808981,-38.1627311721,-10.0762054686));
#71013=CARTESIAN_POINT('Ctrl Pts',(1.52971305438,-38.0684833924,-10.1128473337));
#71014=CARTESIAN_POINT('Ctrl Pts',(1.52971305438,-37.9742356128,-10.1128473337));
#71015=CARTESIAN_POINT('Ctrl Pts',(1.62218880952,-38.2742356128,-9.79656548787));
#71016=CARTESIAN_POINT('Ctrl Pts',(1.63581885953,-38.2742356128,-9.88982281252));
#71017=CARTESIAN_POINT('Ctrl Pts',(1.64944890954,-38.2372245963,-9.98308013716));
#71018=CARTESIAN_POINT('Ctrl Pts',(1.66022209833,-38.1627311721,-10.056790706));
#71019=CARTESIAN_POINT('Ctrl Pts',(1.66557460619,-38.0684833924,-10.0934127718));
#71020=CARTESIAN_POINT('Ctrl Pts',(1.66557460619,-37.9742356128,-10.0934127718));
#71021=CARTESIAN_POINT('Ctrl Pts',(1.76414135208,-38.2742356128,-9.77563578571));
#71022=CARTESIAN_POINT('Ctrl Pts',(1.77805006872,-38.2742356128,-9.86885473404));
#71023=CARTESIAN_POINT('Ctrl Pts',(1.79195878537,-38.2372245963,-9.96207368237));
#71024=CARTESIAN_POINT('Ctrl Pts',(1.80295222999,-38.1627311721,-10.0357539189));
#71025=CARTESIAN_POINT('Ctrl Pts',(1.8084141722,-38.0684833924,-10.072360914));
#71026=CARTESIAN_POINT('Ctrl Pts',(1.8084141722,-37.9742356128,-10.072360914));
#71027=CARTESIAN_POINT('Ctrl Pts',(1.99446361947,-38.2742356128,-9.73983610905));
#71028=CARTESIAN_POINT('Ctrl Pts',(2.00973240206,-38.2742356128,-9.83284844843));
#71029=CARTESIAN_POINT('Ctrl Pts',(2.02500118465,-38.2372245963,-9.92586078781));
#71030=CARTESIAN_POINT('Ctrl Pts',(2.03706962731,-38.1627311721,-9.99937772036));
#71031=CARTESIAN_POINT('Ctrl Pts',(2.04306566395,-38.0684833924,-10.0359035807));
#71032=CARTESIAN_POINT('Ctrl Pts',(2.04306566395,-37.9742356128,-10.0359035807));
#71033=CARTESIAN_POINT('Ctrl Pts',(2.20684905707,-38.2742356128,-9.70218717363));
#71034=CARTESIAN_POINT('Ctrl Pts',(2.22389967294,-38.2742356128,-9.79488512123));
#71035=CARTESIAN_POINT('Ctrl Pts',(2.2409502888,-38.2372245963,-9.88758306883));
#71036=CARTESIAN_POINT('Ctrl Pts',(2.25442709278,-38.1627311721,-9.96085150608));
#71037=CARTESIAN_POINT('Ctrl Pts',(2.26112285302,-38.0684833924,-9.99725390513));
#71038=CARTESIAN_POINT('Ctrl Pts',(2.26112285302,-37.9742356128,-9.99725390513));
#71039=CARTESIAN_POINT('Ctrl Pts',(2.30711395977,-38.2742356128,-9.6833625585));
#71040=CARTESIAN_POINT('Ctrl Pts',(2.32490006217,-38.2742356128,-9.77592170898));
#71041=CARTESIAN_POINT('Ctrl Pts',(2.34268616457,-38.2372245963,-9.86848085947));
#71042=CARTESIAN_POINT('Ctrl Pts',(2.35674429625,-38.1627311721,-9.94163959163));
#71043=CARTESIAN_POINT('Ctrl Pts',(2.36372888208,-38.0684833924,-9.97798748507));
#71044=CARTESIAN_POINT('Ctrl Pts',(2.36372888208,-37.9742356128,-9.97798748507));
#71045=CARTESIAN_POINT('Ctrl Pts',(2.62538537067,-38.2742356128,-9.62013145829));
#71046=CARTESIAN_POINT('Ctrl Pts',(2.64567868831,-38.2742356128,-9.71219319788));
#71047=CARTESIAN_POINT('Ctrl Pts',(2.66597200595,-38.2372245963,-9.80425493747));
#71048=CARTESIAN_POINT('Ctrl Pts',(2.68201183923,-38.1627311721,-9.87702051628));
#71049=CARTESIAN_POINT('Ctrl Pts',(2.68998100695,-38.0684833924,-9.9131730768));
#71050=CARTESIAN_POINT('Ctrl Pts',(2.68998100695,-37.9742356128,-9.9131730768));
#71051=CARTESIAN_POINT('Ctrl Pts',(2.94353985871,-38.2742356128,-9.54564367384));
#71052=CARTESIAN_POINT('Ctrl Pts',(2.96637211727,-38.2742356128,-9.63711021518));
#71053=CARTESIAN_POINT('Ctrl Pts',(2.98920437583,-38.2372245963,-9.72857675651));
#71054=CARTESIAN_POINT('Ctrl Pts',(3.00725098901,-38.1627311721,-9.80087189053));
#71055=CARTESIAN_POINT('Ctrl Pts',(3.01621719496,-38.0684833924,-9.83679071747));
#71056=CARTESIAN_POINT('Ctrl Pts',(3.01621719496,-37.9742356128,-9.83679071747));
#71057=CARTESIAN_POINT('Ctrl Pts',(3.1599790764,-38.2742356128,-9.48926500243));
#71058=CARTESIAN_POINT('Ctrl Pts',(3.18460764997,-38.2742356128,-9.58026655999));
#71059=CARTESIAN_POINT('Ctrl Pts',(3.20923622353,-38.2372245963,-9.67126811755));
#71060=CARTESIAN_POINT('Ctrl Pts',(3.22870264265,-38.1627311721,-9.74319572864));
#71061=CARTESIAN_POINT('Ctrl Pts',(3.23837426089,-38.0684833924,-9.77893195672));
#71062=CARTESIAN_POINT('Ctrl Pts',(3.23837426089,-37.9742356128,-9.77893195672));
#71063=CARTESIAN_POINT('Ctrl Pts',(3.8074159761,-38.2742356128,-9.30368354848));
#71064=CARTESIAN_POINT('Ctrl Pts',(3.83743195198,-38.2742356128,-9.39314222695));
#71065=CARTESIAN_POINT('Ctrl Pts',(3.86744792787,-38.2372245963,-9.48260090542));
#71066=CARTESIAN_POINT('Ctrl Pts',(3.89117254863,-38.1627311721,-9.55330902521));
#71067=CARTESIAN_POINT('Ctrl Pts',(3.90295979477,-38.0684833924,-9.5884393661));
#71068=CARTESIAN_POINT('Ctrl Pts',(3.90295979477,-37.9742356128,-9.5884393661));
#71069=CARTESIAN_POINT('Ctrl Pts',(4.43772493193,-38.2742356128,-9.0706422086));
#71070=CARTESIAN_POINT('Ctrl Pts',(4.4731429426,-38.2742356128,-9.15810966487));
#71071=CARTESIAN_POINT('Ctrl Pts',(4.50856095327,-38.2372245963,-9.24557712114));
#71072=CARTESIAN_POINT('Ctrl Pts',(4.53655534108,-38.1627311721,-9.31471137936));
#71073=CARTESIAN_POINT('Ctrl Pts',(4.55046396139,-38.0684833924,-9.3490597691));
#71074=CARTESIAN_POINT('Ctrl Pts',(4.55046396139,-37.9742356128,-9.3490597691));
#71075=CARTESIAN_POINT('Ctrl Pts',(4.84930849374,-38.2742356128,-8.89395004026));
#71076=CARTESIAN_POINT('Ctrl Pts',(4.88828590441,-38.2742356128,-8.97987882553));
#71077=CARTESIAN_POINT('Ctrl Pts',(4.92726331508,-38.2372245963,-9.0658076108));
#71078=CARTESIAN_POINT('Ctrl Pts',(4.95807105191,-38.1627311721,-9.13372570379));
#71079=CARTESIAN_POINT('Ctrl Pts',(4.97337744528,-38.0684833924,-9.16746985886));
#71080=CARTESIAN_POINT('Ctrl Pts',(4.97337744528,-37.9742356128,-9.16746985886));
#71081=CARTESIAN_POINT('Ctrl Pts',(5.85544401236,-38.2742356128,-8.40100946237));
#71082=CARTESIAN_POINT('Ctrl Pts',(5.90280719326,-38.2742356128,-8.48282686114));
#71083=CARTESIAN_POINT('Ctrl Pts',(5.95017037416,-38.2372245963,-8.56464425991));
#71084=CARTESIAN_POINT('Ctrl Pts',(5.98760622193,-38.1627311721,-8.62931271392));
#71085=CARTESIAN_POINT('Ctrl Pts',(6.00620569958,-38.0684833924,-8.66144233128));
#71086=CARTESIAN_POINT('Ctrl Pts',(6.00620569958,-37.9742356128,-8.66144233128));
#71087=CARTESIAN_POINT('Ctrl Pts',(6.79666807074,-38.2742356128,-7.78925125486));
#71088=CARTESIAN_POINT('Ctrl Pts',(6.85133327952,-38.2742356128,-7.86627345027));
#71089=CARTESIAN_POINT('Ctrl Pts',(6.9059984883,-38.2372245963,-7.94329564567));
#71090=CARTESIAN_POINT('Ctrl Pts',(6.94920585732,-38.1627311721,-8.00417397196));
#71091=CARTESIAN_POINT('Ctrl Pts',(6.97067283459,-38.0684833924,-8.03442051739));
#71092=CARTESIAN_POINT('Ctrl Pts',(6.97067283459,-37.9742356128,-8.03442051739));
#71093=CARTESIAN_POINT('Ctrl Pts',(7.33820201297,-38.2742356128,-7.38433102414));
#71094=CARTESIAN_POINT('Ctrl Pts',(7.39620233991,-38.2742356128,-7.45876186455));
#71095=CARTESIAN_POINT('Ctrl Pts',(7.45420266686,-38.2372245963,-7.53319270496));
#71096=CARTESIAN_POINT('Ctrl Pts',(7.50004611258,-38.1627311721,-7.5920228247));
#71097=CARTESIAN_POINT('Ctrl Pts',(7.52282278764,-38.0684833924,-7.62125174753));
#71098=CARTESIAN_POINT('Ctrl Pts',(7.52282278764,-37.9742356128,-7.62125174753));
#71099=CARTESIAN_POINT('Ctrl Pts',(8.10467751429,-38.2742356128,-6.74809011842));
#71100=CARTESIAN_POINT('Ctrl Pts',(8.16739900498,-38.2742356128,-6.81870393688));
#71101=CARTESIAN_POINT('Ctrl Pts',(8.23012049567,-38.2372245963,-6.88931775534));
#71102=CARTESIAN_POINT('Ctrl Pts',(8.27969554811,-38.1627311721,-6.94513090196));
#71103=CARTESIAN_POINT('Ctrl Pts',(8.30432621991,-38.0684833924,-6.9728608836));
#71104=CARTESIAN_POINT('Ctrl Pts',(8.30432621991,-37.9742356128,-6.9728608836));
#71105=CARTESIAN_POINT('Ctrl Pts',(8.80837603922,-38.2742356128,-6.03968780603));
#71106=CARTESIAN_POINT('Ctrl Pts',(8.87649577319,-38.2742356128,-6.10488334472));
#71107=CARTESIAN_POINT('Ctrl Pts',(8.94461550716,-38.2372245963,-6.17007888341));
#71108=CARTESIAN_POINT('Ctrl Pts',(8.9984573299,-38.1627311721,-6.22160942286));
#71109=CARTESIAN_POINT('Ctrl Pts',(9.02520788688,-38.0684833924,-6.24721165103));
#71110=CARTESIAN_POINT('Ctrl Pts',(9.02520788688,-37.9742356128,-6.24721165103));
#71111=CARTESIAN_POINT('Ctrl Pts',(9.01511576881,-38.2742356128,-5.81836032423));
#71112=CARTESIAN_POINT('Ctrl Pts',(9.08496935084,-38.2742356128,-5.88172164813));
#71113=CARTESIAN_POINT('Ctrl Pts',(9.15482293286,-38.2372245963,-5.94508297203));
#71114=CARTESIAN_POINT('Ctrl Pts',(9.21003518872,-38.1627311721,-5.9951637485));
#71115=CARTESIAN_POINT('Ctrl Pts',(9.23746662625,-38.0684833924,-6.02004568222));
#71116=CARTESIAN_POINT('Ctrl Pts',(9.23746662625,-37.9742356128,-6.02004568222));
#71117=CARTESIAN_POINT('Ctrl Pts',(9.57792489155,-38.2742356128,-5.17020745095));
#71118=CARTESIAN_POINT('Ctrl Pts',(9.65303226325,-38.2742356128,-5.22756135993));
#71119=CARTESIAN_POINT('Ctrl Pts',(9.72813963496,-38.2372245963,-5.28491526891));
#71120=CARTESIAN_POINT('Ctrl Pts',(9.78750448504,-38.1627311721,-5.33024778594));
#71121=CARTESIAN_POINT('Ctrl Pts',(9.81699908093,-38.0684833924,-5.35277061336));
#71122=CARTESIAN_POINT('Ctrl Pts',(9.81699908093,-37.9742356128,-5.35277061336));
#71123=CARTESIAN_POINT('Ctrl Pts',(10.0628691567,-38.2742356128,-4.45793107296));
#71124=CARTESIAN_POINT('Ctrl Pts',(10.1440778097,-38.2742356128,-4.50658435893));
#71125=CARTESIAN_POINT('Ctrl Pts',(10.2252864627,-38.2372245963,-4.55523764491));
#71126=CARTESIAN_POINT('Ctrl Pts',(10.2894737642,-38.1627311721,-4.59369319157));
#71127=CARTESIAN_POINT('Ctrl Pts',(10.3213643277,-38.0684833924,-4.61279929216));
#71128=CARTESIAN_POINT('Ctrl Pts',(10.3213643277,-37.9742356128,-4.61279929216));
#71129=CARTESIAN_POINT('Ctrl Pts',(10.3284955409,-38.2742356128,-3.96990195467));
#71130=CARTESIAN_POINT('Ctrl Pts',(10.4140079048,-38.2742356128,-4.01100462119));
#71131=CARTESIAN_POINT('Ctrl Pts',(10.4995202688,-38.2372245963,-4.05210728771));
#71132=CARTESIAN_POINT('Ctrl Pts',(10.567109215,-38.1627311721,-4.08459477936));
#71133=CARTESIAN_POINT('Ctrl Pts',(10.6006898492,-38.0684833924,-4.10073580569));
#71134=CARTESIAN_POINT('Ctrl Pts',(10.6006898492,-37.9742356128,-4.10073580569));
#71135=CARTESIAN_POINT('Ctrl Pts',(10.8077466192,-38.2742356128,-2.75452466443));
#71136=CARTESIAN_POINT('Ctrl Pts',(10.9008597457,-38.2742356128,-2.77619835249));
#71137=CARTESIAN_POINT('Ctrl Pts',(10.9939728721,-38.2372245963,-2.79787204055));
#71138=CARTESIAN_POINT('Ctrl Pts',(11.0675694769,-38.1627311721,-2.81500298289));
#71139=CARTESIAN_POINT('Ctrl Pts',(11.104134906,-38.0684833924,-2.82351415623));
#71140=CARTESIAN_POINT('Ctrl Pts',(11.104134906,-37.9742356128,-2.82351415623));
#71141=CARTESIAN_POINT('Ctrl Pts',(10.9568356572,-38.2742356128,-1.46082431358));
#71142=CARTESIAN_POINT('Ctrl Pts',(11.0519582595,-38.2742356128,-1.46349516331));
#71143=CARTESIAN_POINT('Ctrl Pts',(11.1470808617,-38.2372245963,-1.46616601304));
#71144=CARTESIAN_POINT('Ctrl Pts',(11.2222657318,-38.1627311721,-1.46827696463));
#71145=CARTESIAN_POINT('Ctrl Pts',(11.2596203042,-38.0684833924,-1.46932589231));
#71146=CARTESIAN_POINT('Ctrl Pts',(11.2596203042,-37.9742356128,-1.46932589231));
#71147=CARTESIAN_POINT('Ctrl Pts',(10.9320266615,-38.2742356128,-0.702352458466));
#71148=CARTESIAN_POINT('Ctrl Pts',(11.0262542838,-38.2742356128,-0.696917360674));
#71149=CARTESIAN_POINT('Ctrl Pts',(11.1204819061,-38.2372245963,-0.691482262882));
#71150=CARTESIAN_POINT('Ctrl Pts',(11.1949594534,-38.1627311721,-0.68718671173));
#71151=CARTESIAN_POINT('Ctrl Pts',(11.2319624987,-38.0684833924,-0.68505200487));
#71152=CARTESIAN_POINT('Ctrl Pts',(11.2319624987,-37.9742356128,-0.68505200487));
#71153=CARTESIAN_POINT('Ctrl Pts',(10.861915737,-38.2742356128,0.0317722973303));
#71154=CARTESIAN_POINT('Ctrl Pts',(10.9557329316,-38.2742356128,0.041860744283));
#71155=CARTESIAN_POINT('Ctrl Pts',(11.0495501263,-38.2372245963,0.0519491912357));
#71156=CARTESIAN_POINT('Ctrl Pts',(11.1237031794,-38.1627311721,0.0599233301614));
#71157=CARTESIAN_POINT('Ctrl Pts',(11.1605451425,-38.0684833924,0.0638848213432));
#71158=CARTESIAN_POINT('Ctrl Pts',(11.1605451425,-37.9742356128,0.0638848213432));
#71159=CARTESIAN_POINT('Ctrl Pts',(10.7486857138,-38.2742356128,0.754197377643));
#71160=CARTESIAN_POINT('Ctrl Pts',(10.8417967511,-38.2742356128,0.768791167183));
#71161=CARTESIAN_POINT('Ctrl Pts',(10.9349077884,-38.2372245963,0.783384956722));
#71162=CARTESIAN_POINT('Ctrl Pts',(11.0085027318,-38.1627311721,0.794919884766));
#71163=CARTESIAN_POINT('Ctrl Pts',(11.0450673507,-38.0684833924,0.800650852517));
#71164=CARTESIAN_POINT('Ctrl Pts',(11.0450673507,-37.9742356128,0.800650852517));
#71165=CARTESIAN_POINT('',(11.0450673664881,-37.9742356128,0.800650755926446));
#71166=CARTESIAN_POINT('Origin',(10.7507817353365,-37.9763569060012,0.754523858996911));
#71167=CARTESIAN_POINT('Ctrl Pts',(11.045067373838,-37.9742356128,0.800650704892936));
#71168=CARTESIAN_POINT('Ctrl Pts',(11.0576661427342,-37.9742356128,0.720268620987917));
#71169=CARTESIAN_POINT('Ctrl Pts',(11.0696392766439,-37.9742356128,0.639700888506689));
#71170=CARTESIAN_POINT('Ctrl Pts',(11.0809742041238,-37.9742356128,0.558892739368612));
#71171=CARTESIAN_POINT('Ctrl Pts',(11.0875830790094,-37.9742356128,0.511777224220254));
#71172=CARTESIAN_POINT('Ctrl Pts',(11.093974504389,-37.9742356128,0.464580392649293));
#71173=CARTESIAN_POINT('Ctrl Pts',(11.1001422093536,-37.9742356128,0.417294686478159));
#71174=CARTESIAN_POINT('Ctrl Pts',(11.1055449723429,-37.9742356128,0.375873531496338));
#71175=CARTESIAN_POINT('Ctrl Pts',(11.1107759171709,-37.9742356128,0.334385408520878));
#71176=CARTESIAN_POINT('Ctrl Pts',(11.1158312696378,-37.9742356128,0.292809025903721));
#71177=CARTESIAN_POINT('Ctrl Pts',(11.1278544247113,-37.9742356128,0.19392783040354));
#71178=CARTESIAN_POINT('Ctrl Pts',(11.1388834873982,-37.9742356128,0.0945699250618215));
#71179=CARTESIAN_POINT('Ctrl Pts',(11.1488040792331,-37.9742356128,-0.00525704534534066));
#71180=CARTESIAN_POINT('Ctrl Pts',(11.1592276051179,-37.9742356128,-0.110144841089314));
#71181=CARTESIAN_POINT('Ctrl Pts',(11.1684269371819,-37.9742356128,-0.21555045358533));
#71182=CARTESIAN_POINT('Ctrl Pts',(11.1762317393997,-37.9742356128,-0.321420936240089));
#71183=CARTESIAN_POINT('Ctrl Pts',(11.1846838595737,-37.9742356128,-0.436072149340684));
#71184=CARTESIAN_POINT('Ctrl Pts',(11.1914997918907,-37.9742356128,-0.551268619946787));
#71185=CARTESIAN_POINT('Ctrl Pts',(11.1964295589341,-37.9742356128,-0.666891713681186));
#71186=CARTESIAN_POINT('Ctrl Pts',(11.1994520258282,-37.9742356128,-0.737780859136654));
#71187=CARTESIAN_POINT('Ctrl Pts',(11.2017648735253,-37.9742356128,-0.808829359655462));
#71188=CARTESIAN_POINT('Ctrl Pts',(11.2033071963304,-37.9742356128,-0.880001550581649));
#71189=CARTESIAN_POINT('Ctrl Pts',(11.2048492854098,-37.9742356128,-0.951162955976867));
#71190=CARTESIAN_POINT('Ctrl Pts',(11.2056211223806,-37.9742356128,-1.02244172630779));
#71191=CARTESIAN_POINT('Ctrl Pts',(11.2055609332167,-37.9742356128,-1.09383517988263));
#71192=CARTESIAN_POINT('Ctrl Pts',(11.2054459298545,-37.9742356128,-1.23024656479139));
#71193=CARTESIAN_POINT('Ctrl Pts',(11.2022909838307,-37.9742356128,-1.36706187880045));
#71194=CARTESIAN_POINT('Ctrl Pts',(11.1956647789511,-37.9742356128,-1.50402455513197));
#71195=CARTESIAN_POINT('Ctrl Pts',(11.1895754817146,-37.9742356128,-1.62988942976902));
#71196=CARTESIAN_POINT('Ctrl Pts',(11.1805531072994,-37.9742356128,-1.75587729149789));
#71197=CARTESIAN_POINT('Ctrl Pts',(11.1682938698613,-37.9742356128,-1.88176142786058));
#71198=CARTESIAN_POINT('Ctrl Pts',(11.1571777445444,-37.9742356128,-1.99590750279133));
#71199=CARTESIAN_POINT('Ctrl Pts',(11.1433996715383,-37.9742356128,-2.10996747829517));
#71200=CARTESIAN_POINT('Ctrl Pts',(11.1267731665591,-37.9742356128,-2.22376344203655));
#71201=CARTESIAN_POINT('Ctrl Pts',(11.1110191505116,-37.9742356128,-2.33158787303733));
#71202=CARTESIAN_POINT('Ctrl Pts',(11.092707316135,-37.9742356128,-2.43917480080161));
#71203=CARTESIAN_POINT('Ctrl Pts',(11.0717243336485,-37.9742356128,-2.54637308638286));
#71204=CARTESIAN_POINT('Ctrl Pts',(11.0520129790026,-37.9742356128,-2.64707485391739));
#71205=CARTESIAN_POINT('Ctrl Pts',(11.0299442382527,-37.9742356128,-2.74743336288688));
#71206=CARTESIAN_POINT('Ctrl Pts',(11.0054696943795,-37.9742356128,-2.84732875965493));
#71207=CARTESIAN_POINT('Ctrl Pts',(10.9925223436773,-37.9742356128,-2.90017471838646));
#71208=CARTESIAN_POINT('Ctrl Pts',(10.9789025174646,-37.9742356128,-2.95289119232652));
#71209=CARTESIAN_POINT('Ctrl Pts',(10.9646089566338,-37.9742356128,-3.00546151299019));
#71210=CARTESIAN_POINT('Ctrl Pts',(10.9388145384853,-37.9742356128,-3.10033086356308));
#71211=CARTESIAN_POINT('Ctrl Pts',(10.9108232164818,-37.9742356128,-3.19472254000091));
#71212=CARTESIAN_POINT('Ctrl Pts',(10.88061675586,-37.9742356128,-3.28848712616045));
#71213=CARTESIAN_POINT('Ctrl Pts',(10.8496041039679,-37.9742356128,-3.38475422963813));
#71214=CARTESIAN_POINT('Ctrl Pts',(10.8162567039116,-37.9742356128,-3.48036028663188));
#71215=CARTESIAN_POINT('Ctrl Pts',(10.7806034744716,-37.9742356128,-3.57516864650273));
#71216=CARTESIAN_POINT('Ctrl Pts',(10.7432639703021,-37.9742356128,-3.67446111465515));
#71217=CARTESIAN_POINT('Ctrl Pts',(10.703395501285,-37.9742356128,-3.77287851876867));
#71218=CARTESIAN_POINT('Ctrl Pts',(10.6610814766523,-37.9742356128,-3.87029239545888));
#71219=CARTESIAN_POINT('Ctrl Pts',(10.6187243454886,-37.9742356128,-3.96780551050643));
#71220=CARTESIAN_POINT('Ctrl Pts',(10.5739172222098,-37.9742356128,-4.06431314334558));
#71221=CARTESIAN_POINT('Ctrl Pts',(10.5267870850518,-37.9742356128,-4.15971429500487));
#71222=CARTESIAN_POINT('Ctrl Pts',(10.4878597234772,-37.9742356128,-4.23851133123732));
#71223=CARTESIAN_POINT('Ctrl Pts',(10.4473483600161,-37.9742356128,-4.316554711738));
#71224=CARTESIAN_POINT('Ctrl Pts',(10.4053370662145,-37.9742356128,-4.39381058626197));
#71225=CARTESIAN_POINT('Ctrl Pts',(10.3474952495324,-37.9742356128,-4.50017770156528));
#71226=CARTESIAN_POINT('Ctrl Pts',(10.2868118157629,-37.9742356128,-4.60504448980234));
#71227=CARTESIAN_POINT('Ctrl Pts',(10.2235623322584,-37.9742356128,-4.7083274604292));
#71228=CARTESIAN_POINT('Ctrl Pts',(10.1574136573687,-37.9742356128,-4.81634465309378));
#71229=CARTESIAN_POINT('Ctrl Pts',(10.0884593000215,-37.9742356128,-4.9226293675133));
#71230=CARTESIAN_POINT('Ctrl Pts',(10.0170520252819,-37.9742356128,-5.02713305669034));
#71231=CARTESIAN_POINT('Ctrl Pts',(9.94157132886643,-37.9742356128,-5.1375981495793));
#71232=CARTESIAN_POINT('Ctrl Pts',(9.86335135573855,-37.9742356128,-5.24607301541748));
#71233=CARTESIAN_POINT('Ctrl Pts',(9.78283033969483,-37.9742356128,-5.35255452647816));
#71234=CARTESIAN_POINT('Ctrl Pts',(9.73480989402804,-37.9742356128,-5.41605707360986));
#71235=CARTESIAN_POINT('Ctrl Pts',(9.68597136550832,-37.9742356128,-5.47885171054048));
#71236=CARTESIAN_POINT('Ctrl Pts',(9.6364074829053,-37.9742356128,-5.54094653469057));
#71237=CARTESIAN_POINT('Ctrl Pts',(9.55705149948688,-37.9742356128,-5.64036561925043));
#71238=CARTESIAN_POINT('Ctrl Pts',(9.47583217163434,-37.9742356128,-5.73799546041952));
#71239=CARTESIAN_POINT('Ctrl Pts',(9.39295246670258,-37.9742356128,-5.83397638243802));
#71240=CARTESIAN_POINT('Ctrl Pts',(9.34842440213017,-37.9742356128,-5.88554322497057));
#71241=CARTESIAN_POINT('Ctrl Pts',(9.30341933348068,-37.9742356128,-5.93663173824686));
#71242=CARTESIAN_POINT('Ctrl Pts',(9.25796679639709,-37.9742356128,-5.98726452990667));
#71243=CARTESIAN_POINT('Ctrl Pts',(9.16705589418052,-37.9742356128,-6.08853660550218));
#71244=CARTESIAN_POINT('Ctrl Pts',(9.0743387174743,-37.9742356128,-6.1880080646955));
#71245=CARTESIAN_POINT('Ctrl Pts',(8.98008824482996,-37.9742356128,-6.28577047569799));
#71246=CARTESIAN_POINT('Ctrl Pts',(8.90029866668485,-37.9742356128,-6.36853315384152));
#71247=CARTESIAN_POINT('Ctrl Pts',(8.8194114197026,-37.9742356128,-6.45007008726216));
#71248=CARTESIAN_POINT('Ctrl Pts',(8.73756131692268,-37.9742356128,-6.53041646823511));
#71249=CARTESIAN_POINT('Ctrl Pts',(8.68636996822059,-37.9742356128,-6.58066734716676));
#71250=CARTESIAN_POINT('Ctrl Pts',(8.63480131053765,-37.9742356128,-6.63045217403649));
#71251=CARTESIAN_POINT('Ctrl Pts',(8.58287807592455,-37.9742356128,-6.67977647996842));
#71252=CARTESIAN_POINT('Ctrl Pts',(8.50456388436919,-37.9742356128,-6.75417078864104));
#71253=CARTESIAN_POINT('Ctrl Pts',(8.42544574969429,-37.9742356128,-6.82751663928241));
#71254=CARTESIAN_POINT('Ctrl Pts',(8.34567252955157,-37.9742356128,-6.8997996171541));
#71255=CARTESIAN_POINT('Ctrl Pts',(8.26266734472803,-37.9742356128,-6.97501109698531));
#71256=CARTESIAN_POINT('Ctrl Pts',(8.17895266977429,-37.9742356128,-7.04907193014341));
#71257=CARTESIAN_POINT('Ctrl Pts',(8.09463951602057,-37.9742356128,-7.12197066509028));
#71258=CARTESIAN_POINT('Ctrl Pts',(8.0029222082522,-37.9742356128,-7.20127117054375));
#71259=CARTESIAN_POINT('Ctrl Pts',(7.91049666065247,-37.9742356128,-7.27919663775101));
#71260=CARTESIAN_POINT('Ctrl Pts',(7.81744159254399,-37.9742356128,-7.35573617280705));
#71261=CARTESIAN_POINT('Ctrl Pts',(7.71969237318238,-37.9742356128,-7.43613673512038));
#71262=CARTESIAN_POINT('Ctrl Pts',(7.62124779569011,-37.9742356128,-7.5150082397789));
#71263=CARTESIAN_POINT('Ctrl Pts',(7.52213761733522,-37.9742356128,-7.59233927662337));
#71264=CARTESIAN_POINT('Ctrl Pts',(7.48114563527072,-37.9742356128,-7.62432340305695));
#71265=CARTESIAN_POINT('Ctrl Pts',(7.44003642245277,-37.9742356128,-7.65604603818923));
#71266=CARTESIAN_POINT('Ctrl Pts',(7.39882688005116,-37.9742356128,-7.68749334749781));
#71267=CARTESIAN_POINT('Ctrl Pts',(7.28758125498532,-37.9742356128,-7.77238571409046));
#71268=CARTESIAN_POINT('Ctrl Pts',(7.17557863982231,-37.9742356128,-7.85529688978051));
#71269=CARTESIAN_POINT('Ctrl Pts',(7.06265199352647,-37.9742356128,-7.93630090391787));
#71270=CARTESIAN_POINT('Ctrl Pts',(6.98391249723267,-37.9742356128,-7.99278195139573));
#71271=CARTESIAN_POINT('Ctrl Pts',(6.90472242863274,-37.9742356128,-8.04833530896636));
#71272=CARTESIAN_POINT('Ctrl Pts',(6.82501533972286,-37.9742356128,-8.10297764790911));
#71273=CARTESIAN_POINT('Ctrl Pts',(6.68910314957339,-37.9742356128,-8.19615079050117));
#71274=CARTESIAN_POINT('Ctrl Pts',(6.55169566021097,-37.9742356128,-8.28666925523598));
#71275=CARTESIAN_POINT('Ctrl Pts',(6.41265719431847,-37.9742356128,-8.37444381217628));
#71276=CARTESIAN_POINT('Ctrl Pts',(6.3053066284567,-37.9742356128,-8.44221389504739));
#71277=CARTESIAN_POINT('Ctrl Pts',(6.19698246692728,-37.9742356128,-8.50834800082493));
#71278=CARTESIAN_POINT('Ctrl Pts',(6.08764898154051,-37.9742356128,-8.57278393309764));
#71279=CARTESIAN_POINT('Ctrl Pts',(5.98836838379676,-37.9742356128,-8.63129517372608));
#71280=CARTESIAN_POINT('Ctrl Pts',(5.88825509703659,-37.9742356128,-8.68840608318665));
#71281=CARTESIAN_POINT('Ctrl Pts',(5.7873158382133,-37.9742356128,-8.74405315587561));
#71282=CARTESIAN_POINT('Ctrl Pts',(5.62003536011473,-37.9742356128,-8.83627365593388));
#71283=CARTESIAN_POINT('Ctrl Pts',(5.45049527652575,-37.9742356128,-8.92446710527229));
#71284=CARTESIAN_POINT('Ctrl Pts',(5.27878630562228,-37.9742356128,-9.00845329983273));
#71285=CARTESIAN_POINT('Ctrl Pts',(5.11226631012109,-37.9742356128,-9.08990146568441));
#71286=CARTESIAN_POINT('Ctrl Pts',(4.94370656192245,-37.9742356128,-9.16739135702801));
#71287=CARTESIAN_POINT('Ctrl Pts',(4.77325954530881,-37.9742356128,-9.24076338864954));
#71288=CARTESIAN_POINT('Ctrl Pts',(4.61325613185901,-37.9742356128,-9.30963978053032));
#71289=CARTESIAN_POINT('Ctrl Pts',(4.45159154314567,-37.9742356128,-9.37488596251091));
#71290=CARTESIAN_POINT('Ctrl Pts',(4.28841412642254,-37.9742356128,-9.4364074687214));
#71291=CARTESIAN_POINT('Ctrl Pts',(4.21192131899931,-37.9742356128,-9.46524695411987));
#71292=CARTESIAN_POINT('Ctrl Pts',(4.13509623384778,-37.9742356128,-9.49326864559091));
#71293=CARTESIAN_POINT('Ctrl Pts',(4.0579543036934,-37.9742356128,-9.52046726498404));
#71294=CARTESIAN_POINT('Ctrl Pts',(4.00538316554377,-37.9742356128,-9.53900274075881));
#71295=CARTESIAN_POINT('Ctrl Pts',(3.95266776619419,-37.9742356128,-9.55715511842427));
#71296=CARTESIAN_POINT('Ctrl Pts',(3.89979238982722,-37.9742356128,-9.57493036523837));
#71297=CARTESIAN_POINT('Ctrl Pts',(3.82665212994116,-37.9742356128,-9.59951810835909));
#71298=CARTESIAN_POINT('Ctrl Pts',(3.75321493143739,-37.9742356128,-9.62338071508881));
#71299=CARTESIAN_POINT('Ctrl Pts',(3.67950687086322,-37.9742356128,-9.64651331815322));
#71300=CARTESIAN_POINT('Ctrl Pts',(3.61652703617181,-37.9742356128,-9.66627896529724));
#71301=CARTESIAN_POINT('Ctrl Pts',(3.55335456166025,-37.9742356128,-9.68551083921918));
#71302=CARTESIAN_POINT('Ctrl Pts',(3.49002949975775,-37.9742356128,-9.70420212536654));
#71303=CARTESIAN_POINT('Ctrl Pts',(3.40965967613772,-37.9742356128,-9.72792441360065));
#71304=CARTESIAN_POINT('Ctrl Pts',(3.32904208220192,-37.9742356128,-9.7507761888097));
#71305=CARTESIAN_POINT('Ctrl Pts',(3.2481676520397,-37.9742356128,-9.77276406314082));
#71306=CARTESIAN_POINT('Ctrl Pts',(3.1749308511008,-37.9742356128,-9.79267544393483));
#71307=CARTESIAN_POINT('Ctrl Pts',(3.10147823214554,-37.9742356128,-9.81187941582968));
#71308=CARTESIAN_POINT('Ctrl Pts',(3.02780135377895,-37.9742356128,-9.83038392558351));
#71309=CARTESIAN_POINT('Ctrl Pts',(2.97692025161001,-37.9742356128,-9.84316310233806));
#71310=CARTESIAN_POINT('Ctrl Pts',(2.92593218832356,-37.9742356128,-9.85560874262589));
#71311=CARTESIAN_POINT('Ctrl Pts',(2.87485126513147,-37.9742356128,-9.86772100278545));
#71312=CARTESIAN_POINT('Ctrl Pts',(2.8467281991402,-37.9742356128,-9.874389517575));
#71313=CARTESIAN_POINT('Ctrl Pts',(2.81857376808186,-37.9742356128,-9.88095778691781));
#71314=CARTESIAN_POINT('Ctrl Pts',(2.79038631636844,-37.9742356128,-9.88742682636709));
#71315=CARTESIAN_POINT('Ctrl Pts',(2.73551854970118,-37.9742356128,-9.90001901634839));
#71316=CARTESIAN_POINT('Ctrl Pts',(2.68053097377708,-37.9742356128,-9.91223375160826));
#71317=CARTESIAN_POINT('Ctrl Pts',(2.62549899348512,-37.9742356128,-9.92406002398358));
#71318=CARTESIAN_POINT('Ctrl Pts',(2.60518339835759,-37.9742356128,-9.92842580839057));
#71319=CARTESIAN_POINT('Ctrl Pts',(2.58486223162589,-37.9742356128,-9.93273857235789));
#71320=CARTESIAN_POINT('Ctrl Pts',(2.56454112002745,-37.9742356128,-9.93699744921689));
#71321=CARTESIAN_POINT('Ctrl Pts',(2.54041972653535,-37.9742356128,-9.94205278509517));
#71322=CARTESIAN_POINT('Ctrl Pts',(2.51629397351212,-37.9742356128,-9.94703300268813));
#71323=CARTESIAN_POINT('Ctrl Pts',(2.49212731680301,-37.9742356128,-9.95194519152246));
#71324=CARTESIAN_POINT('Ctrl Pts',(2.4713374613571,-37.9742356128,-9.95617100136525));
#71325=CARTESIAN_POINT('Ctrl Pts',(2.45051702575423,-37.9742356128,-9.96034657813116));
#71326=CARTESIAN_POINT('Ctrl Pts',(2.42965942383348,-37.9742356128,-9.96447343814513));
#71327=CARTESIAN_POINT('Ctrl Pts',(2.39359814483382,-37.9742356128,-9.97160847940834));
#71328=CARTESIAN_POINT('Ctrl Pts',(2.35743385663318,-37.9742356128,-9.9785963109437));
#71329=CARTESIAN_POINT('Ctrl Pts',(2.32123184643125,-37.9742356128,-9.98542552600865));
#71330=CARTESIAN_POINT('Ctrl Pts',(2.29491518968168,-37.9742356128,-9.99038994946831));
#71331=CARTESIAN_POINT('Ctrl Pts',(2.26858128058276,-37.9742356128,-9.99527006010204));
#71332=CARTESIAN_POINT('Ctrl Pts',(2.24223429025926,-37.9742356128,-10.0000650689695));
#71333=CARTESIAN_POINT('Ctrl Pts',(2.21853740664891,-37.9742356128,-10.0043777728362));
#71334=CARTESIAN_POINT('Ctrl Pts',(2.1948308803507,-37.9742356128,-10.008621462852));
#71335=CARTESIAN_POINT('Ctrl Pts',(2.17107873562539,-37.9742356128,-10.0128024884733));
#71336=CARTESIAN_POINT('Ctrl Pts',(2.15245143750088,-37.9742356128,-10.0160814012458));
#71337=CARTESIAN_POINT('Ctrl Pts',(2.13379556879273,-37.9742356128,-10.0193218644102));
#71338=CARTESIAN_POINT('Ctrl Pts',(2.11506900102166,-37.9742356128,-10.0225313604444));
#71339=CARTESIAN_POINT('Ctrl Pts',(2.09995902895158,-37.9742356128,-10.025121017878));
#71340=CARTESIAN_POINT('Ctrl Pts',(2.08480873377376,-37.9742356128,-10.027689584587));
#71341=CARTESIAN_POINT('Ctrl Pts',(2.06954473665795,-37.9742356128,-10.0302496637803));
#71342=CARTESIAN_POINT('Ctrl Pts',(2.06589127481877,-37.9742356128,-10.0308624227822));
#71343=CARTESIAN_POINT('Ctrl Pts',(2.06223161231065,-37.9742356128,-10.031474641092));
#71344=CARTESIAN_POINT('Ctrl Pts',(2.05856513736635,-37.9742356128,-10.0320864240192));
#71345=CARTESIAN_POINT('Ctrl Pts',(2.0385286174435,-37.9742356128,-10.0354296899615));
#71346=CARTESIAN_POINT('Ctrl Pts',(2.01828403398492,-37.9742356128,-10.0387606184883));
#71347=CARTESIAN_POINT('Ctrl Pts',(1.99776023211584,-37.9742356128,-10.0420924842183));
#71348=CARTESIAN_POINT('Ctrl Pts',(1.9761101819271,-37.9742356128,-10.045607186842));
#71349=CARTESIAN_POINT('Ctrl Pts',(1.95414977844573,-37.9742356128,-10.0491228843939));
#71350=CARTESIAN_POINT('Ctrl Pts',(1.93185281336172,-37.9742356128,-10.0526469463018));
#71351=CARTESIAN_POINT('Ctrl Pts',(1.90630644189858,-37.9742356128,-10.0566845807608));
#71352=CARTESIAN_POINT('Ctrl Pts',(1.88031839144298,-37.9742356128,-10.0607331823361));
#71353=CARTESIAN_POINT('Ctrl Pts',(1.85392023551879,-37.9742356128,-10.0647936010473));
#71354=CARTESIAN_POINT('Ctrl Pts',(1.82217491673056,-37.9742356128,-10.069676490851));
#71355=CARTESIAN_POINT('Ctrl Pts',(1.78983837541185,-37.9742356128,-10.0745762225125));
#71356=CARTESIAN_POINT('Ctrl Pts',(1.757049426948,-37.9742356128,-10.0794819772469));
#71357=CARTESIAN_POINT('Ctrl Pts',(1.7270948216314,-37.9742356128,-10.0839636686013));
#71358=CARTESIAN_POINT('Ctrl Pts',(1.69676713389206,-37.9742356128,-10.0884497474174));
#71359=CARTESIAN_POINT('Ctrl Pts',(1.66618126682606,-37.9742356128,-10.0929303149498));
#71360=CARTESIAN_POINT('Ctrl Pts',(1.64013828901344,-37.9742356128,-10.0967453881202));
#71361=CARTESIAN_POINT('Ctrl Pts',(1.61390964456225,-37.9742356128,-10.1005562459663));
#71362=CARTESIAN_POINT('Ctrl Pts',(1.58753817424305,-37.9742356128,-10.1043605387549));
#71363=CARTESIAN_POINT('Ctrl Pts',(1.56338079239737,-37.9742356128,-10.1078454318016));
#71364=CARTESIAN_POINT('Ctrl Pts',(1.53910435580598,-37.9742356128,-10.1113247014488));
#71365=CARTESIAN_POINT('Ctrl Pts',(1.5147016560395,-37.9742356128,-10.1148020695187));
#71366=CARTESIAN_POINT('Ctrl Pts',(1.49244002770215,-37.9742356128,-10.1179743363705));
#71367=CARTESIAN_POINT('Ctrl Pts',(1.47007358539911,-37.9742356128,-10.121144981694));
#71368=CARTESIAN_POINT('Ctrl Pts',(1.44755531188353,-37.9742356128,-10.124322600884));
#71369=CARTESIAN_POINT('Ctrl Pts',(1.42751533029559,-37.9742356128,-10.1271505010788));
#71370=CARTESIAN_POINT('Ctrl Pts',(1.40735494258601,-37.9742356128,-10.1299839452806));
#71371=CARTESIAN_POINT('Ctrl Pts',(1.38700644577,-37.9742356128,-10.1328338118));
#71372=CARTESIAN_POINT('Ctrl Pts',(1.38699292008,-37.9742356128,-10.1328356959));
#71373=CARTESIAN_POINT('Ctrl Pts',(1.38699292008,-36.2942356128,-10.1328356959));
#71374=CARTESIAN_POINT('Ctrl Pts',(1.54048434157,-37.9742356128,-10.1113387667));
#71375=CARTESIAN_POINT('Ctrl Pts',(1.54048434157,-36.2942356128,-10.1113387667));
#71376=CARTESIAN_POINT('Ctrl Pts',(1.68405004863,-37.9742356128,-10.0907690318));
#71377=CARTESIAN_POINT('Ctrl Pts',(1.68405004863,-36.2942356128,-10.0907690318));
#71378=CARTESIAN_POINT('Ctrl Pts',(1.83768542134,-37.9742356128,-10.0680136806));
#71379=CARTESIAN_POINT('Ctrl Pts',(1.83768542134,-36.2942356128,-10.0680136806));
#71380=CARTESIAN_POINT('Ctrl Pts',(2.04726851031,-37.9742356128,-10.0350233698));
#71381=CARTESIAN_POINT('Ctrl Pts',(2.04726851031,-36.2942356128,-10.0350233698));
#71382=CARTESIAN_POINT('Ctrl Pts',(2.24744160945,-37.9742356128,-9.99950190736));
#71383=CARTESIAN_POINT('Ctrl Pts',(2.24744160945,-36.2942356128,-9.99950190736));
#71384=CARTESIAN_POINT('Ctrl Pts',(2.32512404468,-37.9742356128,-9.98507083709));
#71385=CARTESIAN_POINT('Ctrl Pts',(2.32512404468,-36.2942356128,-9.98507083709));
#71386=CARTESIAN_POINT('Ctrl Pts',(2.47861794588,-37.9742356128,-9.95531796777));
#71387=CARTESIAN_POINT('Ctrl Pts',(2.47861794588,-36.2942356128,-9.95531796777));
#71388=CARTESIAN_POINT('Ctrl Pts',(2.63158870596,-37.9742356128,-9.92313477939));
#71389=CARTESIAN_POINT('Ctrl Pts',(2.63158870596,-36.2942356128,-9.92313477939));
#71390=CARTESIAN_POINT('Ctrl Pts',(2.70802102447,-37.9742356128,-9.90641220657));
#71391=CARTESIAN_POINT('Ctrl Pts',(2.70802102447,-36.2942356128,-9.90641220657));
#71392=CARTESIAN_POINT('Ctrl Pts',(3.01253146546,-37.9742356128,-9.83720045464));
#71393=CARTESIAN_POINT('Ctrl Pts',(3.01253146546,-36.2942356128,-9.83720045464));
#71394=CARTESIAN_POINT('Ctrl Pts',(3.31446912359,-37.9742356128,-9.75814914821));
#71395=CARTESIAN_POINT('Ctrl Pts',(3.31446912359,-36.2942356128,-9.75814914821));
#71396=CARTESIAN_POINT('Ctrl Pts',(3.53901439179,-37.9742356128,-9.69332241165));
#71397=CARTESIAN_POINT('Ctrl Pts',(3.53901439179,-36.2942356128,-9.69332241165));
#71398=CARTESIAN_POINT('Ctrl Pts',(4.06616678437,-37.9742356128,-9.52655591089));
#71399=CARTESIAN_POINT('Ctrl Pts',(4.06616678437,-36.2942356128,-9.52655591089));
#71400=CARTESIAN_POINT('Ctrl Pts',(4.58136980215,-37.9742356128,-9.32859973652));
#71401=CARTESIAN_POINT('Ctrl Pts',(4.58136980215,-36.2942356128,-9.32859973652));
#71402=CARTESIAN_POINT('Ctrl Pts',(4.87486658279,-37.9742356128,-9.2037781865));
#71403=CARTESIAN_POINT('Ctrl Pts',(4.87486658279,-36.2942356128,-9.2037781865));
#71404=CARTESIAN_POINT('Ctrl Pts',(5.45178039508,-37.9742356128,-8.93423446359));
#71405=CARTESIAN_POINT('Ctrl Pts',(5.45178039508,-36.2942356128,-8.93423446359));
#71406=CARTESIAN_POINT('Ctrl Pts',(6.00853446953,-37.9742356128,-8.62630121911));
#71407=CARTESIAN_POINT('Ctrl Pts',(6.00853446953,-36.2942356128,-8.62630121911));
#71408=CARTESIAN_POINT('Ctrl Pts',(6.28153293634,-37.9742356128,-8.46325996647));
#71409=CARTESIAN_POINT('Ctrl Pts',(6.28153293634,-36.2942356128,-8.46325996647));
#71410=CARTESIAN_POINT('Ctrl Pts',(6.68293897532,-37.9742356128,-8.20578167079));
#71411=CARTESIAN_POINT('Ctrl Pts',(6.68293897532,-36.2942356128,-8.20578167079));
#71412=CARTESIAN_POINT('Ctrl Pts',(7.07391925378,-37.9742356128,-7.92965998368));
#71413=CARTESIAN_POINT('Ctrl Pts',(7.07391925378,-36.2942356128,-7.92965998368));
#71414=CARTESIAN_POINT('Ctrl Pts',(7.20312714754,-37.9742356128,-7.83561707229));
#71415=CARTESIAN_POINT('Ctrl Pts',(7.20312714754,-36.2942356128,-7.83561707229));
#71416=CARTESIAN_POINT('Ctrl Pts',(7.71835943349,-37.9742356128,-7.44951290201));
#71417=CARTESIAN_POINT('Ctrl Pts',(7.71835943349,-36.2942356128,-7.44951290201));
#71418=CARTESIAN_POINT('Ctrl Pts',(8.21985964708,-37.9742356128,-7.02884209136));
#71419=CARTESIAN_POINT('Ctrl Pts',(8.21985964708,-36.2942356128,-7.02884209136));
#71420=CARTESIAN_POINT('Ctrl Pts',(8.58741395086,-37.9742356128,-6.69445002697));
#71421=CARTESIAN_POINT('Ctrl Pts',(8.58741395086,-36.2942356128,-6.69445002697));
#71422=CARTESIAN_POINT('Ctrl Pts',(9.23922565917,-37.9742356128,-6.0447166144));
#71423=CARTESIAN_POINT('Ctrl Pts',(9.23922565917,-36.2942356128,-6.0447166144));
#71424=CARTESIAN_POINT('Ctrl Pts',(9.82149842762,-37.9742356128,-5.32595482066));
#71425=CARTESIAN_POINT('Ctrl Pts',(9.82149842762,-36.2942356128,-5.32595482066));
#71426=CARTESIAN_POINT('Ctrl Pts',(10.0721843915,-37.9742356128,-4.97806710985));
#71427=CARTESIAN_POINT('Ctrl Pts',(10.0721843915,-36.2942356128,-4.97806710985));
#71428=CARTESIAN_POINT('Ctrl Pts',(10.6524574839,-37.9742356128,-4.03375119457));
#71429=CARTESIAN_POINT('Ctrl Pts',(10.6524574839,-36.2942356128,-4.03375119457));
#71430=CARTESIAN_POINT('Ctrl Pts',(11.0291793988,-37.9742356128,-2.98459593105));
#71431=CARTESIAN_POINT('Ctrl Pts',(11.0291793988,-36.2942356128,-2.98459593105));
#71432=CARTESIAN_POINT('Ctrl Pts',(11.1622899815,-37.9742356128,-2.31636115629));
#71433=CARTESIAN_POINT('Ctrl Pts',(11.1622899815,-36.2942356128,-2.31636115629));
#71434=CARTESIAN_POINT('Ctrl Pts',(11.2336540706,-37.9742356128,-1.36618233638));
#71435=CARTESIAN_POINT('Ctrl Pts',(11.2336540706,-36.2942356128,-1.36618233638));
#71436=CARTESIAN_POINT('Ctrl Pts',(11.1889875368,-37.9742356128,-0.434883867498));
#71437=CARTESIAN_POINT('Ctrl Pts',(11.1889875368,-36.2942356128,-0.434883867498));
#71438=CARTESIAN_POINT('Ctrl Pts',(11.1677658434,-37.9742356128,-0.163547364245));
#71439=CARTESIAN_POINT('Ctrl Pts',(11.1677658434,-36.2942356128,-0.163547364245));
#71440=CARTESIAN_POINT('Ctrl Pts',(11.1309935407,-37.9742356128,0.191196052993));
#71441=CARTESIAN_POINT('Ctrl Pts',(11.1309935407,-36.2942356128,0.191196052993));
#71442=CARTESIAN_POINT('Ctrl Pts',(11.0837537732,-37.9742356128,0.541839826087));
#71443=CARTESIAN_POINT('Ctrl Pts',(11.0837537732,-36.2942356128,0.541839826087));
#71444=CARTESIAN_POINT('Ctrl Pts',(11.0714556362,-37.9742356128,0.628315856355));
#71445=CARTESIAN_POINT('Ctrl Pts',(11.0714556362,-36.2942356128,0.628315856355));
#71446=CARTESIAN_POINT('Ctrl Pts',(11.0585597994,-37.9742356128,0.714566551433));
#71447=CARTESIAN_POINT('Ctrl Pts',(11.0585597994,-36.2942356128,0.714566551433));
#71448=CARTESIAN_POINT('Ctrl Pts',(11.0450673741,-37.9742356128,0.800650704934));
#71449=CARTESIAN_POINT('Ctrl Pts',(11.0450673741,-36.2942356128,0.800650704934));
#71450=CARTESIAN_POINT('',(11.0450673741,-37.2742356128,0.800650704934));
#71451=CARTESIAN_POINT('Ctrl Pts',(10.3257952821,-36.5742356128,3.01322822759));
#71452=CARTESIAN_POINT('Ctrl Pts',(10.3257952821,-36.4799878332,3.01322822759));
#71453=CARTESIAN_POINT('Ctrl Pts',(10.2942035846,-36.3857400536,2.99394663035));
#71454=CARTESIAN_POINT('Ctrl Pts',(10.2306178216,-36.3112466293,2.95513785557));
#71455=CARTESIAN_POINT('Ctrl Pts',(10.1501702245,-36.2742356128,2.90603767139));
#71456=CARTESIAN_POINT('Ctrl Pts',(10.0697226274,-36.2742356128,2.85693748721));
#71457=CARTESIAN_POINT('Ctrl Pts',(10.3937468068,-36.5742356128,2.90189388187));
#71458=CARTESIAN_POINT('Ctrl Pts',(10.3937468068,-36.4799878332,2.90189388187));
#71459=CARTESIAN_POINT('Ctrl Pts',(10.361743269,-36.3857400536,2.88328705955));
#71460=CARTESIAN_POINT('Ctrl Pts',(10.2973285787,-36.3112466293,2.84583643038));
#71461=CARTESIAN_POINT('Ctrl Pts',(10.2158322378,-36.2742356128,2.79845454767));
#71462=CARTESIAN_POINT('Ctrl Pts',(10.1343358969,-36.2742356128,2.75107266497));
#71463=CARTESIAN_POINT('Ctrl Pts',(10.4620487356,-36.5742356128,2.78329337524));
#71464=CARTESIAN_POINT('Ctrl Pts',(10.4620487075,-36.4799878222,2.78329342192));
#71465=CARTESIAN_POINT('Ctrl Pts',(10.4295091719,-36.3857400315,2.76560455904));
#71466=CARTESIAN_POINT('Ctrl Pts',(10.3640156965,-36.3112466033,2.7300014792));
#71467=CARTESIAN_POINT('Ctrl Pts',(10.2811545152,-36.2742355955,2.68495705923));
#71468=CARTESIAN_POINT('Ctrl Pts',(10.1982933508,-36.2742356128,2.63991262435));
#71469=CARTESIAN_POINT('Ctrl Pts',(10.5258464853,-36.5742356128,2.66146373578));
#71470=CARTESIAN_POINT('Ctrl Pts',(10.5258464925,-36.4799878342,2.66146372337));
#71471=CARTESIAN_POINT('Ctrl Pts',(10.49275753,-36.3857400555,2.64481822146));
#71472=CARTESIAN_POINT('Ctrl Pts',(10.4261581581,-36.3112466315,2.61131522692));
#71473=CARTESIAN_POINT('Ctrl Pts',(10.3418977911,-36.2742356143,2.5689278305));
#71474=CARTESIAN_POINT('Ctrl Pts',(10.257637421,-36.2742356128,2.52654043836));
#71475=CARTESIAN_POINT('Ctrl Pts',(10.6432548222,-36.5742356128,2.41313758791));
#71476=CARTESIAN_POINT('Ctrl Pts',(10.643254815,-36.4799878323,2.41313760034));
#71477=CARTESIAN_POINT('Ctrl Pts',(10.6091443507,-36.3857400518,2.39865283441));
#71478=CARTESIAN_POINT('Ctrl Pts',(10.5404889831,-36.3112466272,2.36949880159));
#71479=CARTESIAN_POINT('Ctrl Pts',(10.4536274153,-36.2742356114,2.33261362134));
#71480=CARTESIAN_POINT('Ctrl Pts',(10.3667658506,-36.2742356128,2.29572843681));
#71481=CARTESIAN_POINT('Ctrl Pts',(10.7398872019,-36.5742356128,2.15784469508));
#71482=CARTESIAN_POINT('Ctrl Pts',(10.7398872091,-36.4799878342,2.15784468263));
#71483=CARTESIAN_POINT('Ctrl Pts',(10.7049465072,-36.3857400555,2.1455561634));
#71484=CARTESIAN_POINT('Ctrl Pts',(10.6346200712,-36.3112466315,2.12082262831));
#71485=CARTESIAN_POINT('Ctrl Pts',(10.5456442881,-36.2742356143,2.08953019835));
#71486=CARTESIAN_POINT('Ctrl Pts',(10.4566685018,-36.2742356128,2.05823777268));
#71487=CARTESIAN_POINT('Ctrl Pts',(10.7831182422,-36.5742356128,2.02819080292));
#71488=CARTESIAN_POINT('Ctrl Pts',(10.7831182402,-36.479987836,2.02819080957));
#71489=CARTESIAN_POINT('Ctrl Pts',(10.7478302137,-36.3857400592,2.0169555735));
#71490=CARTESIAN_POINT('Ctrl Pts',(10.6768047166,-36.311246636,1.9943419946));
#71491=CARTESIAN_POINT('Ctrl Pts',(10.5869444982,-36.2742356173,1.96573168544));
#71492=CARTESIAN_POINT('Ctrl Pts',(10.4970842789,-36.2742356128,1.93712137311));
#71493=CARTESIAN_POINT('Ctrl Pts',(10.8542127323,-36.5742356128,1.78659505536));
#71494=CARTESIAN_POINT('Ctrl Pts',(10.8542127341,-36.4799878308,1.78659504957));
#71495=CARTESIAN_POINT('Ctrl Pts',(10.818391418,-36.3857400487,1.77719284878));
#71496=CARTESIAN_POINT('Ctrl Pts',(10.746292545,-36.3112466236,1.75826870283));
#71497=CARTESIAN_POINT('Ctrl Pts',(10.6550743098,-36.274235609,1.73432620773));
#71498=CARTESIAN_POINT('Ctrl Pts',(10.5638560753,-36.2742356128,1.71038371539));
#71499=CARTESIAN_POINT('Ctrl Pts',(10.9096968315,-36.5742356128,1.5493422145));
#71500=CARTESIAN_POINT('Ctrl Pts',(10.9096968299,-36.4799878354,1.54934221954));
#71501=CARTESIAN_POINT('Ctrl Pts',(10.8735444913,-36.3857400579,1.54137680968));
#71502=CARTESIAN_POINT('Ctrl Pts',(10.8007793611,-36.3112466344,1.52534453328));
#71503=CARTESIAN_POINT('Ctrl Pts',(10.7087181892,-36.2742356162,1.50506077338));
#71504=CARTESIAN_POINT('Ctrl Pts',(10.6166570167,-36.2742356128,1.48477701108));
#71505=CARTESIAN_POINT('Ctrl Pts',(10.9325897702,-36.5742356128,1.44085989855));
#71506=CARTESIAN_POINT('Ctrl Pts',(10.9325897728,-36.4799878363,1.44085988415));
#71507=CARTESIAN_POINT('Ctrl Pts',(10.8963180592,-36.3857400597,1.43348398822));
#71508=CARTESIAN_POINT('Ctrl Pts',(10.8233126521,-36.3112466366,1.41863827973));
#71509=CARTESIAN_POINT('Ctrl Pts',(10.7309474837,-36.2742356176,1.3998557533));
#71510=CARTESIAN_POINT('Ctrl Pts',(10.6385823125,-36.2742356128,1.38107323223));
#71511=CARTESIAN_POINT('Ctrl Pts',(10.9702924284,-36.5742356128,1.24661939192));
#71512=CARTESIAN_POINT('Ctrl Pts',(10.9702924263,-36.4799878308,1.24661940331));
#71513=CARTESIAN_POINT('Ctrl Pts',(10.9338862965,-36.3857400488,1.23993800485));
#71514=CARTESIAN_POINT('Ctrl Pts',(10.8606103532,-36.3112466236,1.22649008978));
#71515=CARTESIAN_POINT('Ctrl Pts',(10.7679029112,-36.274235609,1.20947601848));
#71516=CARTESIAN_POINT('Ctrl Pts',(10.6751954713,-36.2742356128,1.19246194295));
#71517=CARTESIAN_POINT('Ctrl Pts',(11.0025979433,-36.5742356128,1.06106603291));
#71518=CARTESIAN_POINT('Ctrl Pts',(11.0025979449,-36.4799878351,1.0610660239));
#71519=CARTESIAN_POINT('Ctrl Pts',(10.9661101376,-36.3857400575,1.05486169103));
#71520=CARTESIAN_POINT('Ctrl Pts',(10.8926697928,-36.3112466339,1.04237401943));
#71521=CARTESIAN_POINT('Ctrl Pts',(10.7997543496,-36.2742356158,1.02657483871));
#71522=CARTESIAN_POINT('Ctrl Pts',(10.7068389045,-36.2742356128,1.01077566133));
#71523=CARTESIAN_POINT('Ctrl Pts',(11.0186198552,-36.5742356128,0.965719195611));
#71524=CARTESIAN_POINT('Ctrl Pts',(11.0186198914,-36.4799878336,0.965718974446));
#71525=CARTESIAN_POINT('Ctrl Pts',(10.9821161692,-36.3857400544,0.959609890492));
#71526=CARTESIAN_POINT('Ctrl Pts',(10.9086437537,-36.3112466303,0.947314164305));
#71527=CARTESIAN_POINT('Ctrl Pts',(10.8156877131,-36.2742356135,0.931757969109));
#71528=CARTESIAN_POINT('Ctrl Pts',(10.722731658,-36.2742356128,0.916201860672));
#71529=CARTESIAN_POINT('Ctrl Pts',(11.0320114918,-36.5742356128,0.883950471231));
#71530=CARTESIAN_POINT('Ctrl Pts',(11.0320115123,-36.4799878331,0.883950339438));
#71531=CARTESIAN_POINT('Ctrl Pts',(10.9954782575,-36.3857400535,0.878019250857));
#71532=CARTESIAN_POINT('Ctrl Pts',(10.9219464145,-36.3112466291,0.866081706745));
#71533=CARTESIAN_POINT('Ctrl Pts',(10.828915199,-36.2742356127,0.85097860876));
#71534=CARTESIAN_POINT('Ctrl Pts',(10.7358839755,-36.2742356128,0.835875562575));
#71535=CARTESIAN_POINT('Ctrl Pts',(11.0450658874,-36.5742356128,0.800660309528));
#71536=CARTESIAN_POINT('Ctrl Pts',(11.0450658931,-36.4799878332,0.800660273261));
#71537=CARTESIAN_POINT('Ctrl Pts',(11.0085012867,-36.3857400536,0.794929224556));
#71538=CARTESIAN_POINT('Ctrl Pts',(10.9349063615,-36.3112466293,0.783394177901));
#71539=CARTESIAN_POINT('Ctrl Pts',(10.8417953438,-36.2742356128,0.768800260322));
#71540=CARTESIAN_POINT('Ctrl Pts',(10.7486843238,-36.2742356128,0.754206356986));
#71541=CARTESIAN_POINT('Ctrl Pts',(10.3257952821,-36.5742356128,3.01322822759));
#71542=CARTESIAN_POINT('Ctrl Pts',(10.3992001828,-36.5742356128,2.89295886461));
#71543=CARTESIAN_POINT('Ctrl Pts',(10.4735263391,-36.5742356128,2.76337956773));
#71544=CARTESIAN_POINT('Ctrl Pts',(10.5420136,-36.5742356128,2.63031881231));
#71545=CARTESIAN_POINT('Ctrl Pts',(10.6667840474,-36.5742356128,2.3591848401));
#71546=CARTESIAN_POINT('Ctrl Pts',(10.7670166783,-36.5742356128,2.08017125701));
#71547=CARTESIAN_POINT('Ctrl Pts',(10.8111933802,-36.5742356128,1.9383801789));
#71548=CARTESIAN_POINT('Ctrl Pts',(10.8740649015,-36.5742356128,1.70707199422));
#71549=CARTESIAN_POINT('Ctrl Pts',(10.9239906907,-36.5742356128,1.48074082922));
#71550=CARTESIAN_POINT('Ctrl Pts',(10.9420747597,-36.5742356128,1.39194060496));
#71551=CARTESIAN_POINT('Ctrl Pts',(10.9747007143,-36.5742356128,1.22147170256));
#71552=CARTESIAN_POINT('Ctrl Pts',(11.0034487643,-36.5742356128,1.05599081154));
#71553=CARTESIAN_POINT('Ctrl Pts',(11.0192230845,-36.5742356128,0.962056436866));
#71554=CARTESIAN_POINT('Ctrl Pts',(11.0322998284,-36.5742356128,0.882109993579));
#71555=CARTESIAN_POINT('Ctrl Pts',(11.0450673741,-36.5742356128,0.800650704934));
#71556=CARTESIAN_POINT('Ctrl Pts',(10.7486858853,-38.2742356128,0.75419629452));
#71557=CARTESIAN_POINT('Ctrl Pts',(10.8417968709,-38.2742356128,0.768790414629));
#71558=CARTESIAN_POINT('Ctrl Pts',(10.9349078565,-38.2372245963,0.783384534738));
#71559=CARTESIAN_POINT('Ctrl Pts',(11.0085027591,-38.1627311721,0.794919724064));
#71560=CARTESIAN_POINT('Ctrl Pts',(11.0450673576,-38.0684833924,0.800650821629));
#71561=CARTESIAN_POINT('Ctrl Pts',(11.0450673576,-37.9742356128,0.800650821629));
#71562=CARTESIAN_POINT('Ctrl Pts',(10.7357744891,-38.2742356128,0.836572947324));
#71563=CARTESIAN_POINT('Ctrl Pts',(10.8288041791,-38.2742356128,0.851685759842));
#71564=CARTESIAN_POINT('Ctrl Pts',(10.9218338691,-38.2372245963,0.86679857236));
#71565=CARTESIAN_POINT('Ctrl Pts',(10.9953645154,-38.1627311721,0.878743737491));
#71566=CARTESIAN_POINT('Ctrl Pts',(11.0318971895,-38.0684833924,0.884678523649));
#71567=CARTESIAN_POINT('Ctrl Pts',(11.0318971895,-37.9742356128,0.884678523649));
#71568=CARTESIAN_POINT('Ctrl Pts',(10.722464663,-38.2742356128,0.917844462815));
#71569=CARTESIAN_POINT('Ctrl Pts',(10.8154219344,-38.2742356128,0.933393309198));
#71570=CARTESIAN_POINT('Ctrl Pts',(10.9083792058,-38.2372245963,0.948942155581));
#71571=CARTESIAN_POINT('Ctrl Pts',(10.9818526127,-38.1627311721,0.961231959982));
#71572=CARTESIAN_POINT('Ctrl Pts',(11.0183568478,-38.0684833924,0.96733797804));
#71573=CARTESIAN_POINT('Ctrl Pts',(11.0183568478,-37.9742356128,0.96733797804));
#71574=CARTESIAN_POINT('Ctrl Pts',(10.7064160578,-38.2742356128,1.01327576595));
#71575=CARTESIAN_POINT('Ctrl Pts',(10.7993296705,-38.2742356128,1.02908657461));
#71576=CARTESIAN_POINT('Ctrl Pts',(10.8922432832,-38.2372245963,1.04489738327));
#71577=CARTESIAN_POINT('Ctrl Pts',(10.9656821815,-38.1627311721,1.05739424674));
#71578=CARTESIAN_POINT('Ctrl Pts',(11.0021692726,-38.0684833924,1.06360313301));
#71579=CARTESIAN_POINT('Ctrl Pts',(11.0021692726,-37.9742356128,1.06360313301));
#71580=CARTESIAN_POINT('Ctrl Pts',(10.6699861172,-38.2742356128,1.22225589069));
#71581=CARTESIAN_POINT('Ctrl Pts',(10.7626589385,-38.2742356128,1.23947073278));
#71582=CARTESIAN_POINT('Ctrl Pts',(10.8553317597,-38.2372245963,1.25668557487));
#71583=CARTESIAN_POINT('Ctrl Pts',(10.9285803371,-38.1627311721,1.27029218249));
#71584=CARTESIAN_POINT('Ctrl Pts',(10.964972869,-38.0684833924,1.27705243495));
#71585=CARTESIAN_POINT('Ctrl Pts',(10.964972869,-37.9742356128,1.27705243495));
#71586=CARTESIAN_POINT('Ctrl Pts',(10.6268374654,-38.2742356128,1.44080864883));
#71587=CARTESIAN_POINT('Ctrl Pts',(10.7190870973,-38.2742356128,1.46018401586));
#71588=CARTESIAN_POINT('Ctrl Pts',(10.8113367292,-38.2372245963,1.4795593829));
#71589=CARTESIAN_POINT('Ctrl Pts',(10.8842508199,-38.1627311721,1.49487365862));
#71590=CARTESIAN_POINT('Ctrl Pts',(10.9204771637,-38.0684833924,1.50248235758));
#71591=CARTESIAN_POINT('Ctrl Pts',(10.9204771637,-37.9742356128,1.50248235758));
#71592=CARTESIAN_POINT('Ctrl Pts',(10.5978372142,-38.2742356128,1.57143060617));
#71593=CARTESIAN_POINT('Ctrl Pts',(10.689631737,-38.2742356128,1.59298148681));
#71594=CARTESIAN_POINT('Ctrl Pts',(10.7814262599,-38.2372245963,1.61453236745));
#71595=CARTESIAN_POINT('Ctrl Pts',(10.8539806029,-38.1627311721,1.63156622296));
#71596=CARTESIAN_POINT('Ctrl Pts',(10.8900282554,-38.0684833924,1.64002918981));
#71597=CARTESIAN_POINT('Ctrl Pts',(10.8900282554,-37.9742356128,1.64002918981));
#71598=CARTESIAN_POINT('Ctrl Pts',(10.5099314906,-38.2742356128,1.91769651998));
#71599=CARTESIAN_POINT('Ctrl Pts',(10.6001579466,-38.2742356128,1.94553878808));
#71600=CARTESIAN_POINT('Ctrl Pts',(10.6903844027,-38.2372245963,1.97338105617));
#71601=CARTESIAN_POINT('Ctrl Pts',(10.761699418,-38.1627311721,1.9953875076));
#71602=CARTESIAN_POINT('Ctrl Pts',(10.7971312201,-38.0684833924,2.00632121187));
#71603=CARTESIAN_POINT('Ctrl Pts',(10.7971312201,-37.9742356128,2.00632121187));
#71604=CARTESIAN_POINT('Ctrl Pts',(10.3851598454,-38.2742356128,2.26389944964));
#71605=CARTESIAN_POINT('Ctrl Pts',(10.4725421188,-38.2742356128,2.29983157374));
#71606=CARTESIAN_POINT('Ctrl Pts',(10.5599243922,-38.2372245963,2.33576369785));
#71607=CARTESIAN_POINT('Ctrl Pts',(10.628991251,-38.1627311721,2.36416455541));
#71608=CARTESIAN_POINT('Ctrl Pts',(10.6633062605,-38.0684833924,2.37827495298));
#71609=CARTESIAN_POINT('Ctrl Pts',(10.6633062605,-37.9742356128,2.37827495298));
#71610=CARTESIAN_POINT('Ctrl Pts',(10.2956098407,-38.2742356128,2.46622288607));
#71611=CARTESIAN_POINT('Ctrl Pts',(10.3807463521,-38.2742356128,2.50731926973));
#71612=CARTESIAN_POINT('Ctrl Pts',(10.4658828634,-38.2372245963,2.54841565339));
#71613=CARTESIAN_POINT('Ctrl Pts',(10.5331750304,-38.1627311721,2.58089775529));
#71614=CARTESIAN_POINT('Ctrl Pts',(10.5666077732,-38.0684833924,2.59703673813));
#71615=CARTESIAN_POINT('Ctrl Pts',(10.5666077732,-37.9742356128,2.59703673813));
#71616=CARTESIAN_POINT('Ctrl Pts',(10.1838372262,-38.2742356128,2.66996781664));
#71617=CARTESIAN_POINT('Ctrl Pts',(10.2661370276,-38.2742356128,2.71603327924));
#71618=CARTESIAN_POINT('Ctrl Pts',(10.348436829,-38.2372245963,2.76209874184));
#71619=CARTESIAN_POINT('Ctrl Pts',(10.4134863826,-38.1627311721,2.79850918724));
#71620=CARTESIAN_POINT('Ctrl Pts',(10.4458056304,-38.0684833924,2.8165987382));
#71621=CARTESIAN_POINT('Ctrl Pts',(10.4458056304,-37.9742356128,2.8165987382));
#71622=CARTESIAN_POINT('Ctrl Pts',(10.0697226274,-38.2742356128,2.85693748721));
#71623=CARTESIAN_POINT('Ctrl Pts',(10.1501702245,-38.2742356128,2.90603767139));
#71624=CARTESIAN_POINT('Ctrl Pts',(10.2306178216,-38.2372245963,2.95513785557));
#71625=CARTESIAN_POINT('Ctrl Pts',(10.2942035846,-38.1627311721,2.99394663035));
#71626=CARTESIAN_POINT('Ctrl Pts',(10.3257952821,-38.0684833924,3.01322822759));
#71627=CARTESIAN_POINT('Ctrl Pts',(10.3257952821,-37.9742356128,3.01322822759));
#71628=CARTESIAN_POINT('Ctrl Pts',(10.3257952821,-37.9742356128,3.01322822759));
#71629=CARTESIAN_POINT('Ctrl Pts',(10.3435108770889,-37.9742356128,2.98420232735513));
#71630=CARTESIAN_POINT('Ctrl Pts',(10.3612660726275,-37.9742356128,2.95454361401332));
#71631=CARTESIAN_POINT('Ctrl Pts',(10.3789029130837,-37.9742356128,2.92440130957732));
#71632=CARTESIAN_POINT('Ctrl Pts',(10.3970692021044,-37.9742356128,2.89335414920351));
#71633=CARTESIAN_POINT('Ctrl Pts',(10.4151099921331,-37.9742356128,2.86179373744858));
#71634=CARTESIAN_POINT('Ctrl Pts',(10.4328934056652,-37.9742356128,2.82984504858017));
#71635=CARTESIAN_POINT('Ctrl Pts',(10.4513725247225,-37.9742356128,2.7966464939688));
#71636=CARTESIAN_POINT('Ctrl Pts',(10.4695738352306,-37.9742356128,2.76302842606344));
#71637=CARTESIAN_POINT('Ctrl Pts',(10.4873915130274,-37.9742356128,2.72909395600771));
#71638=CARTESIAN_POINT('Ctrl Pts',(10.506746145179,-37.9742356128,2.69223229576914));
#71639=CARTESIAN_POINT('Ctrl Pts',(10.5256480261522,-37.9742356128,2.65499706078238));
#71640=CARTESIAN_POINT('Ctrl Pts',(10.5440106698345,-37.9742356128,2.61748093307006));
#71641=CARTESIAN_POINT('Ctrl Pts',(10.5638797850415,-37.9742356128,2.57688698175579));
#71642=CARTESIAN_POINT('Ctrl Pts',(10.5831177873975,-37.9742356128,2.53596344249259));
#71643=CARTESIAN_POINT('Ctrl Pts',(10.6016693303391,-37.9742356128,2.49479084421754));
#71644=CARTESIAN_POINT('Ctrl Pts',(10.6162942510062,-37.9742356128,2.46233284407569));
#71645=CARTESIAN_POINT('Ctrl Pts',(10.6304938506889,-37.9742356128,2.42971906581169));
#71646=CARTESIAN_POINT('Ctrl Pts',(10.6442593718278,-37.9742356128,2.39698023320332));
#71647=CARTESIAN_POINT('Ctrl Pts',(10.6569750338918,-37.9742356128,2.36673830283123));
#71648=CARTESIAN_POINT('Ctrl Pts',(10.6693194231973,-37.9742356128,2.33639290955639));
#71649=CARTESIAN_POINT('Ctrl Pts',(10.6813046418276,-37.9742356128,2.30593898856114));
#71650=CARTESIAN_POINT('Ctrl Pts',(10.7005865729481,-37.9742356128,2.25694443743201));
#71651=CARTESIAN_POINT('Ctrl Pts',(10.718933686294,-37.9742356128,2.2076779701046));
#71652=CARTESIAN_POINT('Ctrl Pts',(10.7363740820652,-37.9742356128,2.15823655988335));
#71653=CARTESIAN_POINT('Ctrl Pts',(10.7508645620954,-37.9742356128,2.11715780359402));
#71654=CARTESIAN_POINT('Ctrl Pts',(10.7647302536249,-37.9742356128,2.07595786403464));
#71655=CARTESIAN_POINT('Ctrl Pts',(10.7779838592388,-37.9742356128,2.03472677202854));
#71656=CARTESIAN_POINT('Ctrl Pts',(10.7900447242869,-37.9742356128,1.99720621717286));
#71657=CARTESIAN_POINT('Ctrl Pts',(10.8015991768384,-37.9742356128,1.95965960974327));
#71658=CARTESIAN_POINT('Ctrl Pts',(10.8126441119714,-37.9742356128,1.92219040368875));
#71659=CARTESIAN_POINT('Ctrl Pts',(10.8236166119916,-37.9742356128,1.88496692892495));
#71660=CARTESIAN_POINT('Ctrl Pts',(10.8340837193902,-37.9742356128,1.84782839628653));
#71661=CARTESIAN_POINT('Ctrl Pts',(10.8440841088843,-37.9742356128,1.81083470663686));
#71662=CARTESIAN_POINT('Ctrl Pts',(10.8559248749312,-37.9742356128,1.76703305025062));
#71663=CARTESIAN_POINT('Ctrl Pts',(10.8671115731973,-37.9742356128,1.72343299507352));
#71664=CARTESIAN_POINT('Ctrl Pts',(10.8777255157072,-37.9742356128,1.68005510341546));
#71665=CARTESIAN_POINT('Ctrl Pts',(10.8816732452895,-37.9742356128,1.66392121292609));
#71666=CARTESIAN_POINT('Ctrl Pts',(10.8855420335377,-37.9742356128,1.64781665780391));
#71667=CARTESIAN_POINT('Ctrl Pts',(10.88933297735,-37.9742356128,1.63175608320554));
#71668=CARTESIAN_POINT('Ctrl Pts',(10.8993385050894,-37.9742356128,1.58936702849724));
#71669=CARTESIAN_POINT('Ctrl Pts',(10.9088091071911,-37.9742356128,1.54725502348625));
#71670=CARTESIAN_POINT('Ctrl Pts',(10.9178378693608,-37.9742356128,1.50538883341575));
#71671=CARTESIAN_POINT('Ctrl Pts',(10.9255930579366,-37.9742356128,1.46942817869433));
#71672=CARTESIAN_POINT('Ctrl Pts',(10.9330224352445,-37.9742356128,1.43364757364882));
#71673=CARTESIAN_POINT('Ctrl Pts',(10.9401770982342,-37.9742356128,1.39806231067591));
#71674=CARTESIAN_POINT('Ctrl Pts',(10.9465294246673,-37.9742356128,1.36646764200538));
#71675=CARTESIAN_POINT('Ctrl Pts',(10.9526652330497,-37.9742356128,1.33502659574014));
#71676=CARTESIAN_POINT('Ctrl Pts',(10.9586123994879,-37.9742356128,1.30378932417771));
#71677=CARTESIAN_POINT('Ctrl Pts',(10.9632698278339,-37.9742356128,1.2793263542004));
#71678=CARTESIAN_POINT('Ctrl Pts',(10.9678114424312,-37.9742356128,1.25498893556002));
#71679=CARTESIAN_POINT('Ctrl Pts',(10.9722463818661,-37.9742356128,1.23082335732336));
#71680=CARTESIAN_POINT('Ctrl Pts',(10.9744000643225,-37.9742356128,1.2190881391401));
#71681=CARTESIAN_POINT('Ctrl Pts',(10.9765290742772,-37.9742356128,1.20739061189226));
#71682=CARTESIAN_POINT('Ctrl Pts',(10.9786472561583,-37.9742356128,1.19565808724385));
#71683=CARTESIAN_POINT('Ctrl Pts',(10.981079762963,-37.9742356128,1.1821845294256));
#71684=CARTESIAN_POINT('Ctrl Pts',(10.9834978391073,-37.9742356128,1.16866563142089));
#71685=CARTESIAN_POINT('Ctrl Pts',(10.98591187279,-37.9742356128,1.15505222871516));
#71686=CARTESIAN_POINT('Ctrl Pts',(10.9886383738725,-37.9742356128,1.13967673603612));
#71687=CARTESIAN_POINT('Ctrl Pts',(10.9913597243006,-37.9742356128,1.12418073304783));
#71688=CARTESIAN_POINT('Ctrl Pts',(10.9940787041515,-37.9742356128,1.10856313499871));
#71689=CARTESIAN_POINT('Ctrl Pts',(10.9972032177,-37.9742356128,1.09061618453343));
#71690=CARTESIAN_POINT('Ctrl Pts',(11.0003244602367,-37.9742356128,1.07250966807065));
#71691=CARTESIAN_POINT('Ctrl Pts',(11.0034323169338,-37.9742356128,1.05432169160246));
#71692=CARTESIAN_POINT('Ctrl Pts',(11.0072388611408,-37.9742356128,1.03204481618283));
#71693=CARTESIAN_POINT('Ctrl Pts',(11.0110245978049,-37.9742356128,1.00965060914404));
#71694=CARTESIAN_POINT('Ctrl Pts',(11.0147570943917,-37.9742356128,0.987350997854593));
#71695=CARTESIAN_POINT('Ctrl Pts',(11.017586140657,-37.9742356128,0.97044900462676));
#71696=CARTESIAN_POINT('Ctrl Pts',(11.0203841001757,-37.9742356128,0.953604041000246));
#71697=CARTESIAN_POINT('Ctrl Pts',(11.0231387163433,-37.9742356128,0.936890599639805));
#71698=CARTESIAN_POINT('Ctrl Pts',(11.0256260652016,-37.9742356128,0.921798784026464));
#71699=CARTESIAN_POINT('Ctrl Pts',(11.0280779020287,-37.9742356128,0.906815173063734));
#71700=CARTESIAN_POINT('Ctrl Pts',(11.0304906336531,-37.9742356128,0.891957832231274));
#71701=CARTESIAN_POINT('Ctrl Pts',(11.0327503987612,-37.9742356128,0.878042442690342));
#71702=CARTESIAN_POINT('Ctrl Pts',(11.0349757566118,-37.9742356128,0.864238410878224));
#71703=CARTESIAN_POINT('Ctrl Pts',(11.0371706175412,-37.9742356128,0.850516112005006));
#71704=CARTESIAN_POINT('Ctrl Pts',(11.039226797446,-37.9742356128,0.837660848688127));
#71705=CARTESIAN_POINT('Ctrl Pts',(11.0412561654325,-37.9742356128,0.824877574458748));
#71706=CARTESIAN_POINT('Ctrl Pts',(11.0432691636105,-37.9742356128,0.812095953182369));
#71707=CARTESIAN_POINT('Ctrl Pts',(11.0438698244563,-37.9742356128,0.80828203048223));
#71708=CARTESIAN_POINT('Ctrl Pts',(11.0444690817224,-37.9742356128,0.804467913923509));
#71709=CARTESIAN_POINT('Ctrl Pts',(11.0450673576,-37.9742356128,0.800650821629));
#71710=CARTESIAN_POINT('Ctrl Pts',(11.0450673741,-37.9742356128,0.800650704934));
#71711=CARTESIAN_POINT('Ctrl Pts',(11.0450673741,-36.2942356128,0.800650704934));
#71712=CARTESIAN_POINT('Ctrl Pts',(11.0322998284,-37.9742356128,0.882109993579));
#71713=CARTESIAN_POINT('Ctrl Pts',(11.0322998284,-36.2942356128,0.882109993579));
#71714=CARTESIAN_POINT('Ctrl Pts',(11.0192230845,-37.9742356128,0.962056436866));
#71715=CARTESIAN_POINT('Ctrl Pts',(11.0192230845,-36.2942356128,0.962056436866));
#71716=CARTESIAN_POINT('Ctrl Pts',(11.0034487643,-37.9742356128,1.05599081154));
#71717=CARTESIAN_POINT('Ctrl Pts',(11.0034487643,-36.2942356128,1.05599081154));
#71718=CARTESIAN_POINT('Ctrl Pts',(10.9747007143,-37.9742356128,1.22147170256));
#71719=CARTESIAN_POINT('Ctrl Pts',(10.9747007143,-36.2942356128,1.22147170256));
#71720=CARTESIAN_POINT('Ctrl Pts',(10.9420747597,-37.9742356128,1.39194060496));
#71721=CARTESIAN_POINT('Ctrl Pts',(10.9420747597,-36.2942356128,1.39194060496));
#71722=CARTESIAN_POINT('Ctrl Pts',(10.9239906907,-37.9742356128,1.48074082922));
#71723=CARTESIAN_POINT('Ctrl Pts',(10.9239906907,-36.2942356128,1.48074082922));
#71724=CARTESIAN_POINT('Ctrl Pts',(10.8740649015,-37.9742356128,1.70707199422));
#71725=CARTESIAN_POINT('Ctrl Pts',(10.8740649015,-36.2942356128,1.70707199422));
#71726=CARTESIAN_POINT('Ctrl Pts',(10.8111933802,-37.9742356128,1.9383801789));
#71727=CARTESIAN_POINT('Ctrl Pts',(10.8111933802,-36.2942356128,1.9383801789));
#71728=CARTESIAN_POINT('Ctrl Pts',(10.7670166783,-37.9742356128,2.08017125701));
#71729=CARTESIAN_POINT('Ctrl Pts',(10.7670166783,-36.2942356128,2.08017125701));
#71730=CARTESIAN_POINT('Ctrl Pts',(10.6667840474,-37.9742356128,2.3591848401));
#71731=CARTESIAN_POINT('Ctrl Pts',(10.6667840474,-36.2942356128,2.3591848401));
#71732=CARTESIAN_POINT('Ctrl Pts',(10.5420136,-37.9742356128,2.63031881231));
#71733=CARTESIAN_POINT('Ctrl Pts',(10.5420136,-36.2942356128,2.63031881231));
#71734=CARTESIAN_POINT('Ctrl Pts',(10.4735263391,-37.9742356128,2.76337956773));
#71735=CARTESIAN_POINT('Ctrl Pts',(10.4735263391,-36.2942356128,2.76337956773));
#71736=CARTESIAN_POINT('Ctrl Pts',(10.3992001828,-37.9742356128,2.89295886461));
#71737=CARTESIAN_POINT('Ctrl Pts',(10.3992001828,-36.2942356128,2.89295886461));
#71738=CARTESIAN_POINT('Ctrl Pts',(10.3257952821,-37.9742356128,3.01322822759));
#71739=CARTESIAN_POINT('Ctrl Pts',(10.3257952821,-36.2942356128,3.01322822759));
#71740=CARTESIAN_POINT('',(0.,0.,0.));
#71741=CARTESIAN_POINT('Origin',(-3.35265884719E-30,-42.6742356128,3.15283103411E-22));
#71742=CARTESIAN_POINT('',(0.77958411848117,-42.6742356128,-4.94563407380883));
#71743=CARTESIAN_POINT('',(6.75287820063378,-42.6742356128,2.63899277819224));
#71744=CARTESIAN_POINT('Ctrl Pts',(0.779584195372,-42.6742356128,-4.94563441411));
#71745=CARTESIAN_POINT('Ctrl Pts',(0.783019505297316,-42.6742356128,-4.96062388339205));
#71746=CARTESIAN_POINT('Ctrl Pts',(0.786509971280464,-42.6742356128,-4.97559800551016));
#71747=CARTESIAN_POINT('Ctrl Pts',(0.790056389615954,-42.6742356128,-4.99056023421706));
#71748=CARTESIAN_POINT('Ctrl Pts',(0.829308383727368,-42.6742356128,-5.15616317711285));
#71749=CARTESIAN_POINT('Ctrl Pts',(0.875381467538884,-42.6742356128,-5.32014544362963));
#71750=CARTESIAN_POINT('Ctrl Pts',(0.928124152698679,-42.6742356127999,
-5.48195135268744));
#71751=CARTESIAN_POINT('Ctrl Pts',(0.981494143503791,-42.6742356127999,
-5.64568173259634));
#71752=CARTESIAN_POINT('Ctrl Pts',(1.04169323701819,-42.6742356127997,-5.80718344510452));
#71753=CARTESIAN_POINT('Ctrl Pts',(1.1085137075534,-42.6742356127992,-5.96589766472136));
#71754=CARTESIAN_POINT('Ctrl Pts',(1.17574469865151,-42.6742356127987,-6.12558696652868));
#71755=CARTESIAN_POINT('Ctrl Pts',(1.24967852311599,-42.6742356127978,-6.28245419176864));
#71756=CARTESIAN_POINT('Ctrl Pts',(1.33005445375074,-42.6742356127966,-6.43595063967566));
#71757=CARTESIAN_POINT('Ctrl Pts',(1.41084070525712,-42.6742356127954,-6.59023069028317));
#71758=CARTESIAN_POINT('Ctrl Pts',(1.49813483665254,-42.6742356127938,-6.74110522701633));
#71759=CARTESIAN_POINT('Ctrl Pts',(1.59162503957232,-42.674235612792,-6.88804121025148));
#71760=CARTESIAN_POINT('Ctrl Pts',(1.68547908635635,-42.6742356127902,-7.03554903689125));
#71761=CARTESIAN_POINT('Ctrl Pts',(1.78557734186053,-42.6742356127882,-7.17908735951526));
#71762=CARTESIAN_POINT('Ctrl Pts',(1.89155970140233,-42.6742356127863,-7.31814464429339));
#71763=CARTESIAN_POINT('Ctrl Pts',(1.99789293179152,-42.6742356127845,-7.45766229952898));
#71764=CARTESIAN_POINT('Ctrl Pts',(2.11014909709696,-42.6742356127828,-7.5926689596614));
#71765=CARTESIAN_POINT('Ctrl Pts',(2.22792250961881,-42.6742356127818,-7.72267943330251));
#71766=CARTESIAN_POINT('Ctrl Pts',(2.34573059330044,-42.6742356127807,-7.8527281805557));
#71767=CARTESIAN_POINT('Ctrl Pts',(2.46905895621691,-42.6742356127804,-7.97777757592768));
#71768=CARTESIAN_POINT('Ctrl Pts',(2.59746272145967,-42.674235612781,-8.09737684660448));
#71769=CARTESIAN_POINT('Ctrl Pts',(2.72562676191173,-42.6742356127816,-8.21675283013642));
#71770=CARTESIAN_POINT('Ctrl Pts',(2.85884704246923,-42.6742356127832,-8.33069881216825));
#71771=CARTESIAN_POINT('Ctrl Pts',(2.99664585191555,-42.6742356127857,-8.4388044646528));
#71772=CARTESIAN_POINT('Ctrl Pts',(3.11571505661626,-42.6742356127878,-8.53221640425306));
#71773=CARTESIAN_POINT('Ctrl Pts',(3.23820210993358,-42.6742356127905,-8.62126826774772));
#71774=CARTESIAN_POINT('Ctrl Pts',(3.363779477155,-42.6742356127932,-8.70572001193011));
#71775=CARTESIAN_POINT('Ctrl Pts',(3.50872753999223,-42.6742356127963,-8.80319869772609));
#71776=CARTESIAN_POINT('Ctrl Pts',(3.65779162004941,-42.6742356127977,-8.89454681427974));
#71777=CARTESIAN_POINT('Ctrl Pts',(3.81044289926437,-42.6742356127985,-8.97943725563266));
#71778=CARTESIAN_POINT('Ctrl Pts',(3.96182994811744,-42.6742356127994,-9.06362464966135));
#71779=CARTESIAN_POINT('Ctrl Pts',(4.11674479055607,-42.6742356127997,-9.14146074594292));
#71780=CARTESIAN_POINT('Ctrl Pts',(4.27464700945189,-42.6742356127998,-9.21267133077376));
#71781=CARTESIAN_POINT('Ctrl Pts',(4.43163594214289,-42.6742356128,-9.28347004270492));
#71782=CARTESIAN_POINT('Ctrl Pts',(4.59157758029576,-42.6742356128,-9.34771951000529));
#71783=CARTESIAN_POINT('Ctrl Pts',(4.75391970062592,-42.6742356128,-9.4051969786154));
#71784=CARTESIAN_POINT('Ctrl Pts',(4.91468786119625,-42.6742356128,-9.46211718443686));
#71785=CARTESIAN_POINT('Ctrl Pts',(5.07780996923672,-42.6742356128,-9.51239595479921));
#71786=CARTESIAN_POINT('Ctrl Pts',(5.24273211710097,-42.6742356128,-9.55586484972988));
#71787=CARTESIAN_POINT('Ctrl Pts',(5.32221123857816,-42.6742356128,-9.57681333739765));
#71788=CARTESIAN_POINT('Ctrl Pts',(5.40210816909334,-42.6742356128,-9.59618098515424));
#71789=CARTESIAN_POINT('Ctrl Pts',(5.48235965328664,-42.6742356128,-9.61395309319581));
#71790=CARTESIAN_POINT('Ctrl Pts',(5.64903325566381,-42.6742356128,-9.65086382822956));
#71791=CARTESIAN_POINT('Ctrl Pts',(5.8172324747726,-42.6742356128,-9.68088796096779));
#71792=CARTESIAN_POINT('Ctrl Pts',(5.9863825361148,-42.6742356128,-9.70391857948388));
#71793=CARTESIAN_POINT('Ctrl Pts',(6.15680323563844,-42.6742356128,-9.72712220168082));
#71794=CARTESIAN_POINT('Ctrl Pts',(6.32818887600278,-42.6742356128,-9.74322687290936));
#71795=CARTESIAN_POINT('Ctrl Pts',(6.4999462288075,-42.6742356128,-9.75217621766798));
#71796=CARTESIAN_POINT('Ctrl Pts',(6.67284585238956,-42.6742356128,-9.7611850799659));
#71797=CARTESIAN_POINT('Ctrl Pts',(6.84612189524726,-42.6742356128,-9.76294316381342));
#71798=CARTESIAN_POINT('Ctrl Pts',(7.01916749716638,-42.6742356128,-9.75744593352396));
#71799=CARTESIAN_POINT('Ctrl Pts',(7.19318017371352,-42.6742356128,-9.75191798166816));
#71800=CARTESIAN_POINT('Ctrl Pts',(7.3669595611434,-42.6742356128,-9.73905344497));
#71801=CARTESIAN_POINT('Ctrl Pts',(7.53989075903008,-42.6742356128,-9.71890043121172));
#71802=CARTESIAN_POINT('Ctrl Pts',(7.71357133496519,-42.6742356128,-9.69866008661722));
#71803=CARTESIAN_POINT('Ctrl Pts',(7.88639608023403,-42.6742356128,-9.67106802306371));
#71804=CARTESIAN_POINT('Ctrl Pts',(8.05774833885344,-42.6742356128,-9.63622514593106));
#71805=CARTESIAN_POINT('Ctrl Pts',(8.23576088873995,-42.6742356128,-9.60002796094069));
#71806=CARTESIAN_POINT('Ctrl Pts',(8.41218387461858,-42.6742356128,-9.5560050970399));
#71807=CARTESIAN_POINT('Ctrl Pts',(8.5863377901713,-42.6742356128,-9.50432770550163));
#71808=CARTESIAN_POINT('Ctrl Pts',(8.75375175092122,-42.6742356128,-9.45465028784963));
#71809=CARTESIAN_POINT('Ctrl Pts',(8.91907037676882,-42.6742356128,-9.39789907292805));
#71810=CARTESIAN_POINT('Ctrl Pts',(9.08169780495813,-42.6742356128,-9.33427897488519));
#71811=CARTESIAN_POINT('Ctrl Pts',(9.24517506010802,-42.6742356128,-9.27032642323869));
#71812=CARTESIAN_POINT('Ctrl Pts',(9.4059329078901,-42.6742356128,-9.19943320191932));
#71813=CARTESIAN_POINT('Ctrl Pts',(9.56339297670855,-42.6742356128,-9.12185394747491));
#71814=CARTESIAN_POINT('Ctrl Pts',(9.72049523523666,-42.6742356128,-9.04445098315768));
#71815=CARTESIAN_POINT('Ctrl Pts',(9.87431442098647,-42.6742356128,-8.96039245709044));
#71816=CARTESIAN_POINT('Ctrl Pts',(10.0242991772771,-42.6742356128,-8.86997765445494));
#71817=CARTESIAN_POINT('Ctrl Pts',(10.1737494126108,-42.6742356128,-8.77988507527749));
#71818=CARTESIAN_POINT('Ctrl Pts',(10.3193922472071,-42.6742356128,-8.68348157024173));
#71819=CARTESIAN_POINT('Ctrl Pts',(10.4607090001088,-42.6742356128,-8.58110749092089));
#71820=CARTESIAN_POINT('Ctrl Pts',(10.6009930196497,-42.6742356128,-8.47948155451174));
#71821=CARTESIAN_POINT('Ctrl Pts',(10.737013731518,-42.6742356128,-8.37197213719144));
#71822=CARTESIAN_POINT('Ctrl Pts',(10.8682937302911,-42.6742356128,-8.25895379645599));
#71823=CARTESIAN_POINT('Ctrl Pts',(10.9988863407824,-42.6742356128,-8.14652722509724));
#71824=CARTESIAN_POINT('Ctrl Pts',(11.124787528533,-42.6742356128,-8.02864939656428));
#71825=CARTESIAN_POINT('Ctrl Pts',(11.2455604901236,-42.6742356128,-7.90572832483952));
#71826=CARTESIAN_POINT('Ctrl Pts',(11.3653029051114,-42.6742356128,-7.78385612937986));
#71827=CARTESIAN_POINT('Ctrl Pts',(11.4800040444459,-42.6742356128,-7.65702653237569));
#71828=CARTESIAN_POINT('Ctrl Pts',(11.5892739367748,-42.6742356128,-7.52567390389989));
#71829=CARTESIAN_POINT('Ctrl Pts',(11.6246642014889,-42.6742356128,-7.48313149634753));
#71830=CARTESIAN_POINT('Ctrl Pts',(11.659485033899,-42.6742356128,-7.44011491296741));
#71831=CARTESIAN_POINT('Ctrl Pts',(11.6937240507251,-42.6742356128,-7.39663970957412));
#71832=CARTESIAN_POINT('Ctrl Pts',(11.7994911640488,-42.6742356128,-7.26234126323053));
#71833=CARTESIAN_POINT('Ctrl Pts',(11.8997014351145,-42.6742356128,-7.12366634871067));
#71834=CARTESIAN_POINT('Ctrl Pts',(11.994008150501,-42.6742356128,-6.98108829107189));
#71835=CARTESIAN_POINT('Ctrl Pts',(12.0890003774915,-42.6742356128,-6.83747383944364));
#71836=CARTESIAN_POINT('Ctrl Pts',(12.1780028286506,-42.6742356128,-6.68989952409289));
#71837=CARTESIAN_POINT('Ctrl Pts',(12.2607064520845,-42.6742356128,-6.53887699905973));
#71838=CARTESIAN_POINT('Ctrl Pts',(12.3439374138085,-42.6742356128,-6.38689151790917));
#71839=CARTESIAN_POINT('Ctrl Pts',(12.420788886891,-42.6742356128,-6.23141395914406));
#71840=CARTESIAN_POINT('Ctrl Pts',(12.4909927754262,-42.6742356128,-6.07299041838974));
#71841=CARTESIAN_POINT('Ctrl Pts',(12.5615678727858,-42.6742356128,-5.91372920015702));
#71842=CARTESIAN_POINT('Ctrl Pts',(12.6254248272806,-42.6742356128,-5.75149102399791));
#71843=CARTESIAN_POINT('Ctrl Pts',(12.6823396578243,-42.6742356128,-5.58685163845662));
#71844=CARTESIAN_POINT('Ctrl Pts',(12.7394829364501,-42.6742356128,-5.42155141370174));
#71845=CARTESIAN_POINT('Ctrl Pts',(12.7896281850343,-42.6742356128,-5.25383093843157));
#71846=CARTESIAN_POINT('Ctrl Pts',(12.8325983909053,-42.6742356128,-5.08428994230337));
#71847=CARTESIAN_POINT('Ctrl Pts',(12.87720466428,-42.6742356128,-4.90829376382998));
#71848=CARTESIAN_POINT('Ctrl Pts',(12.9140787347158,-42.6742356128,-4.73033603312672));
#71849=CARTESIAN_POINT('Ctrl Pts',(12.9430798859501,-42.6742356128,-4.55110211074482));
#71850=CARTESIAN_POINT('Ctrl Pts',(12.9710073007924,-42.6742356128,-4.37850413131527));
#71851=CARTESIAN_POINT('Ctrl Pts',(12.9916343265915,-42.6742356128,-4.20472180630914));
#71852=CARTESIAN_POINT('Ctrl Pts',(13.0048866885129,-42.6742356128,-4.03038094709754));
#71853=CARTESIAN_POINT('Ctrl Pts',(13.0181761619694,-42.6742356128,-3.85555186873162));
#71854=CARTESIAN_POINT('Ctrl Pts',(13.0240497216501,-42.6742356128,-3.68016120196708));
#71855=CARTESIAN_POINT('Ctrl Pts',(13.0224853990129,-42.6742356128,-3.50483862976804));
#71856=CARTESIAN_POINT('Ctrl Pts',(13.0209250079126,-42.6742356128,-3.32995668735456));
#71857=CARTESIAN_POINT('Ctrl Pts',(13.0119640639272,-42.6742356128,-3.15514278510275));
#71858=CARTESIAN_POINT('Ctrl Pts',(12.9956325370699,-42.6742356128,-2.9810213883885));
#71859=CARTESIAN_POINT('Ctrl Pts',(12.9793624016983,-42.6742356128,-2.80755452761145));
#71860=CARTESIAN_POINT('Ctrl Pts',(12.9557769932041,-42.6742356128,-2.63477525560034));
#71861=CARTESIAN_POINT('Ctrl Pts',(12.9249574485041,-42.6742356128,-2.46329630674595));
#71862=CARTESIAN_POINT('Ctrl Pts',(12.8943693323404,-42.6742356128,-2.29310501877498));
#71863=CARTESIAN_POINT('Ctrl Pts',(12.8566553491569,-42.6742356128,-2.12419486156537));
#71864=CARTESIAN_POINT('Ctrl Pts',(12.8119453525895,-42.6742356128,-1.95715618241776));
#71865=CARTESIAN_POINT('Ctrl Pts',(12.7674725431208,-42.6742356128,-1.79100364558063));
#71866=CARTESIAN_POINT('Ctrl Pts',(12.7160777651395,-42.6742356128,-1.62670303780744));
#71867=CARTESIAN_POINT('Ctrl Pts',(12.6579386831089,-42.6742356128,-1.46482287587078));
#71868=CARTESIAN_POINT('Ctrl Pts',(12.6002987770892,-42.6742356128,-1.30433259988757));
#71869=CARTESIAN_POINT('Ctrl Pts',(12.5360299222692,-42.6742356128,-1.14622161782475));
#71870=CARTESIAN_POINT('Ctrl Pts',(12.4653539433873,-42.6742356128,-0.991028010976763));
#71871=CARTESIAN_POINT('Ctrl Pts',(12.4420672694898,-42.6742356128,-0.939894047630111));
#71872=CARTESIAN_POINT('Ctrl Pts',(12.4180854288606,-42.6742356128,-0.889076651319818));
#71873=CARTESIAN_POINT('Ctrl Pts',(12.3934175172357,-42.6742356128,-0.838594619595771));
#71874=CARTESIAN_POINT('Ctrl Pts',(12.3185024105953,-42.6742356128,-0.685283433487476));
#71875=CARTESIAN_POINT('Ctrl Pts',(12.2372578125187,-42.6742356128,-0.535070520939901));
#71876=CARTESIAN_POINT('Ctrl Pts',(12.1499565739039,-42.6742356128,-0.388469222689598));
#71877=CARTESIAN_POINT('Ctrl Pts',(12.061958185551,-42.6742356128,-0.240697230205108));
#71878=CARTESIAN_POINT('Ctrl Pts',(11.9678062121948,-42.6742356128,-0.0965949378574854));
#71879=CARTESIAN_POINT('Ctrl Pts',(11.8678252730607,-42.6742356128,0.0433402117257184));
#71880=CARTESIAN_POINT('Ctrl Pts',(11.7671342669587,-42.6742356128,0.184269184013886));
#71881=CARTESIAN_POINT('Ctrl Pts',(11.660531396595,-42.6742356128,0.320971434223083));
#71882=CARTESIAN_POINT('Ctrl Pts',(11.5483911271814,-42.6742356128,0.452970093455365));
#71883=CARTESIAN_POINT('Ctrl Pts',(11.4355782693087,-42.6742356128,0.585760446655333));
#71884=CARTESIAN_POINT('Ctrl Pts',(11.3171615973516,-42.6742356128,0.713790436676404));
#71885=CARTESIAN_POINT('Ctrl Pts',(11.1935625752031,-42.6742356128,0.836608787067195));
#71886=CARTESIAN_POINT('Ctrl Pts',(11.0693854080758,-42.6742356128,0.960001630777979));
#71887=CARTESIAN_POINT('Ctrl Pts',(10.9399775204536,-42.6742356128,1.0781337847633));
#71888=CARTESIAN_POINT('Ctrl Pts',(10.805803514957,-42.6742356128,1.1905847691352));
#71889=CARTESIAN_POINT('Ctrl Pts',(10.6669174748723,-42.6742356128,1.30698490092859));
#71890=CARTESIAN_POINT('Ctrl Pts',(10.5229247523534,-42.6742356128,1.41729739891248));
#71891=CARTESIAN_POINT('Ctrl Pts',(10.3743783545598,-42.6742356128,1.52110055406783));
#71892=CARTESIAN_POINT('Ctrl Pts',(10.2308082149157,-42.6742356128,1.62142633579327));
#71893=CARTESIAN_POINT('Ctrl Pts',(10.0829839466795,-42.6742356128,1.71567215095053));
#71894=CARTESIAN_POINT('Ctrl Pts',(9.93143848173256,-42.6742356128,1.80349800771626));
#71895=CARTESIAN_POINT('Ctrl Pts',(9.77978308346317,-42.6742356128,1.89138757465791));
#71896=CARTESIAN_POINT('Ctrl Pts',(9.62440150387112,-42.6742356128,1.97284768977086));
#71897=CARTESIAN_POINT('Ctrl Pts',(9.46585194695658,-42.6742356128,2.04758417096211));
#71898=CARTESIAN_POINT('Ctrl Pts',(9.30767676126653,-42.6742356128,2.12214418248343));
#71899=CARTESIAN_POINT('Ctrl Pts',(9.14634881129091,-42.6742356128,2.19001213657793));
#71900=CARTESIAN_POINT('Ctrl Pts',(8.98244418750696,-42.6742356128,2.25094289839676));
#71901=CARTESIAN_POINT('Ctrl Pts',(8.81914713258895,-42.6742356128,2.31164779938869));
#71902=CARTESIAN_POINT('Ctrl Pts',(8.65329273944362,-42.6742356128,2.36546671959078));
#71903=CARTESIAN_POINT('Ctrl Pts',(8.48546838207095,-42.6742356128,2.41220585261861));
#71904=CARTESIAN_POINT('Ctrl Pts',(8.31891495058699,-42.6742356128,2.45859103241158));
#71905=CARTESIAN_POINT('Ctrl Pts',(8.15042154522815,-42.6742356128,2.49800316356433));
#71906=CARTESIAN_POINT('Ctrl Pts',(7.98057573186983,-42.6742356128,2.53030228157987));
#71907=CARTESIAN_POINT('Ctrl Pts',(7.8116501798998,-42.6742356128,2.56242639598126));
#71908=CARTESIAN_POINT('Ctrl Pts',(7.64138708606372,-42.6742356128,2.58751427080524));
#71909=CARTESIAN_POINT('Ctrl Pts',(7.47037401862466,-42.6742356128,2.60547871329712));
#71910=CARTESIAN_POINT('Ctrl Pts',(7.30086061566379,-42.6742356128,2.62328562024696));
#71911=CARTESIAN_POINT('Ctrl Pts',(7.13061057599309,-42.6742356128,2.63409341996058));
#71912=CARTESIAN_POINT('Ctrl Pts',(6.96020184664722,-42.6742356128,2.63786809596414));
#71913=CARTESIAN_POINT('Ctrl Pts',(6.90647999391455,-42.6742356128,2.63905807366748));
#71914=CARTESIAN_POINT('Ctrl Pts',(6.85274239824904,-42.6742356128,2.63954945473006));
#71915=CARTESIAN_POINT('Ctrl Pts',(6.79900722782363,-42.6742356128,2.63934225086415));
#71916=CARTESIAN_POINT('Ctrl Pts',(6.78363056283946,-42.6742356128,2.63928295814387));
#71917=CARTESIAN_POINT('Ctrl Pts',(6.76825498579667,-42.6742356128,2.63916647454667));
#71918=CARTESIAN_POINT('Ctrl Pts',(6.75287834563,-42.6742356128,2.63899277983));
#71919=CARTESIAN_POINT('',(5.94384247274,-42.6742356128,3.43894307771));
#71920=CARTESIAN_POINT('Ctrl Pts',(6.75287805523922,-42.6742356128,2.63899277654992));
#71921=CARTESIAN_POINT('Ctrl Pts',(6.71005222967492,-42.6742356128,2.63850906375133));
#71922=CARTESIAN_POINT('Ctrl Pts',(6.66724147238406,-42.6742356127937,2.64150712921468));
#71923=CARTESIAN_POINT('Ctrl Pts',(6.62496447000998,-42.6742356127904,2.64789261444747));
#71924=CARTESIAN_POINT('Ctrl Pts',(6.60814536827622,-42.674235612789,2.65043295836305));
#71925=CARTESIAN_POINT('Ctrl Pts',(6.59141084641839,-42.6742356127902,2.65350887060177));
#71926=CARTESIAN_POINT('Ctrl Pts',(6.57479370413688,-42.6742356127937,2.65711208455179));
#71927=CARTESIAN_POINT('Ctrl Pts',(6.53437461602468,-42.6742356128024,2.66587644485308));
#71928=CARTESIAN_POINT('Ctrl Pts',(6.49464930529023,-42.6742356128,2.67776791556408));
#71929=CARTESIAN_POINT('Ctrl Pts',(6.45607632377881,-42.6742356128,2.69263942998386));
#71930=CARTESIAN_POINT('Ctrl Pts',(6.4387274004743,-42.6742356128,2.69932817306207));
#71931=CARTESIAN_POINT('Ctrl Pts',(6.42161145731401,-42.6742356128,2.70661910716981));
#71932=CARTESIAN_POINT('Ctrl Pts',(6.40476925681742,-42.6742356128,2.71449546272456));
#71933=CARTESIAN_POINT('Ctrl Pts',(6.37094623967965,-42.6742356128,2.73031299850116));
#71934=CARTESIAN_POINT('Ctrl Pts',(6.33822887458183,-42.6742356128,2.74849417854391));
#71935=CARTESIAN_POINT('Ctrl Pts',(6.30693936358219,-42.6742356128,2.76887107730016));
#71936=CARTESIAN_POINT('Ctrl Pts',(6.27647408768983,-42.6742356128,2.7887112033554));
#71937=CARTESIAN_POINT('Ctrl Pts',(6.2473622386234,-42.6742356128,2.81063362727969));
#71938=CARTESIAN_POINT('Ctrl Pts',(6.21988117165712,-42.6742356128,2.8344393996307));
#71939=CARTESIAN_POINT('Ctrl Pts',(6.19315655162769,-42.6742356128,2.85758989161735));
#71940=CARTESIAN_POINT('Ctrl Pts',(6.16797397175328,-42.6742356128,2.88252167936477));
#71941=CARTESIAN_POINT('Ctrl Pts',(6.14455644811797,-42.6742356128,2.90901447161481));
#71942=CARTESIAN_POINT('Ctrl Pts',(6.13747930837076,-42.6742356128,2.91702100535285));
#71943=CARTESIAN_POINT('Ctrl Pts',(6.13056316699852,-42.6742356128,2.92516982658604));
#71944=CARTESIAN_POINT('Ctrl Pts',(6.12381360086615,-42.6742356128,2.93345409605156));
#71945=CARTESIAN_POINT('Ctrl Pts',(6.10030182744432,-42.6742356128,2.96231193118036));
#71946=CARTESIAN_POINT('Ctrl Pts',(6.07881363705799,-42.6742356128,2.99281698557839));
#71947=CARTESIAN_POINT('Ctrl Pts',(6.05955270585133,-42.6742356127995,3.02466607617447));
#71948=CARTESIAN_POINT('Ctrl Pts',(6.04782749794023,-42.6742356127992,3.04405440195226));
#71949=CARTESIAN_POINT('Ctrl Pts',(6.0369266122408,-42.6742356127987,3.06394048669793));
#71950=CARTESIAN_POINT('Ctrl Pts',(6.02688710892239,-42.6742356127981,3.08425307204228));
#71951=CARTESIAN_POINT('Ctrl Pts',(6.00904145899223,-42.674235612797,3.12035956812436));
#71952=CARTESIAN_POINT('Ctrl Pts',(5.99392153004012,-42.6742356127982,3.15781104852967));
#71953=CARTESIAN_POINT('Ctrl Pts',(5.98169008790022,-42.6742356127991,3.19619179415814));
#71954=CARTESIAN_POINT('Ctrl Pts',(5.97574243389594,-42.6742356127994,3.21485479340334));
#71955=CARTESIAN_POINT('Ctrl Pts',(5.97047696570253,-42.6742356127997,3.23373721697366));
#71956=CARTESIAN_POINT('Ctrl Pts',(5.96590837847632,-42.6742356127998,3.25278961905919));
#71957=CARTESIAN_POINT('Ctrl Pts',(5.95476050483813,-42.6742356128001,3.29927965206879));
#71958=CARTESIAN_POINT('Ctrl Pts',(5.94776475136862,-42.6742356128,3.34678324157907));
#71959=CARTESIAN_POINT('Ctrl Pts',(5.94508590943863,-42.6742356128,3.39458200052585));
#71960=CARTESIAN_POINT('Ctrl Pts',(5.94440568849322,-42.6742356128,3.40671922916792));
#71961=CARTESIAN_POINT('Ctrl Pts',(5.9440036024013,-42.6742356128,3.4188753187901));
#71962=CARTESIAN_POINT('Ctrl Pts',(5.94388199529069,-42.6742356128,3.43103814870507));
#71963=CARTESIAN_POINT('Ctrl Pts',(5.9438556543113,-42.6742356128,3.4336727056029));
#71964=CARTESIAN_POINT('Ctrl Pts',(5.94384247124667,-42.6742356128,3.43630890719333));
#71965=CARTESIAN_POINT('Ctrl Pts',(5.94384247373,-42.6742356128,3.43894307771));
#71966=CARTESIAN_POINT('',(5.94384247076,-42.6742356128,6.92091963994));
#71967=CARTESIAN_POINT('',(5.94384247076,-42.6742356128,1.43032185727));
#71968=CARTESIAN_POINT('',(-1.17395376824544E-6,-42.6742356128,12.8643459956148));
#71969=CARTESIAN_POINT('Ctrl Pts',(5.94384247076,-42.6742356128,6.92091963994));
#71970=CARTESIAN_POINT('Ctrl Pts',(5.94384247076,-42.6742356128,7.08559459645875));
#71971=CARTESIAN_POINT('Ctrl Pts',(5.9370146386167,-42.6742356128,7.25027218802812));
#71972=CARTESIAN_POINT('Ctrl Pts',(5.92336859551397,-42.6742356128,7.41437712494407));
#71973=CARTESIAN_POINT('Ctrl Pts',(5.90973331659169,-42.6742356128,7.57835261370136));
#71974=CARTESIAN_POINT('Ctrl Pts',(5.88929072702028,-42.6742356128,7.74175617845836));
#71975=CARTESIAN_POINT('Ctrl Pts',(5.86210332732502,-42.6742356128,7.90402225667837));
#71976=CARTESIAN_POINT('Ctrl Pts',(5.8347466327406,-42.6742356128,8.06729875950804));
#71977=CARTESIAN_POINT('Ctrl Pts',(5.8005609575781,-42.6742356128,8.2294233768324));
#71978=CARTESIAN_POINT('Ctrl Pts',(5.75966185673292,-42.6742356128,8.38983112480323));
#71979=CARTESIAN_POINT('Ctrl Pts',(5.71852924283062,-42.6742356128,8.55115471940251));
#71980=CARTESIAN_POINT('Ctrl Pts',(5.67060642398137,-42.6742356128,8.71074158795276));
#71981=CARTESIAN_POINT('Ctrl Pts',(5.61606181116267,-42.6742356128,8.86803122028198));
#71982=CARTESIAN_POINT('Ctrl Pts',(5.56110091309423,-42.6742356128,9.02652128929028));
#71983=CARTESIAN_POINT('Ctrl Pts',(5.49941685038436,-42.6742356128,9.18267871222936));
#71984=CARTESIAN_POINT('Ctrl Pts',(5.43123200188617,-42.6742356128,9.33594751367258));
#71985=CARTESIAN_POINT('Ctrl Pts',(5.36281588859205,-42.6742356128,9.48973616195672));
#71986=CARTESIAN_POINT('Ctrl Pts',(5.28785494664489,-42.6742356128,9.64061635566827));
#71987=CARTESIAN_POINT('Ctrl Pts',(5.20662234382798,-42.6742356128,9.78804708151671));
#71988=CARTESIAN_POINT('Ctrl Pts',(5.12505400163844,-42.6742356128,9.93608714767537));
#71989=CARTESIAN_POINT('Ctrl Pts',(5.03716217715285,-42.6742356128,10.0806489597359));
#71990=CARTESIAN_POINT('Ctrl Pts',(4.94327034299726,-42.6742356128,10.2212087007409));
#71991=CARTESIAN_POINT('Ctrl Pts',(4.85945762028116,-42.6742356128,10.3466796184606));
#71992=CARTESIAN_POINT('Ctrl Pts',(4.77086463695177,-42.6742356128,10.4689618047329));
#71993=CARTESIAN_POINT('Ctrl Pts',(4.67775153908735,-42.6742356128,10.5877007524186));
#71994=CARTESIAN_POINT('Ctrl Pts',(4.57326078712055,-42.6742356128,10.7209486221168));
#71995=CARTESIAN_POINT('Ctrl Pts',(4.46307651478612,-42.6742356128,10.8497345855174));
#71996=CARTESIAN_POINT('Ctrl Pts',(4.3476020380169,-42.6742356128,10.9735884555489));
#71997=CARTESIAN_POINT('Ctrl Pts',(4.2318482698802,-42.6742356128,11.0977418836965));
#71998=CARTESIAN_POINT('Ctrl Pts',(4.11077889784178,-42.6742356128,11.2169391224151));
#71999=CARTESIAN_POINT('Ctrl Pts',(3.98483832342394,-42.6742356128,11.3307424063621));
#72000=CARTESIAN_POINT('Ctrl Pts',(3.85880408066675,-42.6742356128,11.4446303315351));
#72001=CARTESIAN_POINT('Ctrl Pts',(3.72789162138932,-42.6742356128,11.5531160747408));
#72002=CARTESIAN_POINT('Ctrl Pts',(3.5925810591973,-42.6742356128,11.6557998098278));
#72003=CARTESIAN_POINT('Ctrl Pts',(3.45755287962789,-42.6742356128,11.7582692519435));
#72004=CARTESIAN_POINT('Ctrl Pts',(3.3181451832739,-42.6742356128,11.8549606973954));
#72005=CARTESIAN_POINT('Ctrl Pts',(3.17486600574486,-42.6742356128,11.9455183814792));
#72006=CARTESIAN_POINT('Ctrl Pts',(3.03203906481474,-42.6742356128,12.035790235481));
#72007=CARTESIAN_POINT('Ctrl Pts',(2.88536529209994,-42.6742356128,12.1199668191166));
#72008=CARTESIAN_POINT('Ctrl Pts',(2.73537496462231,-42.6742356128,12.1977396617275));
#72009=CARTESIAN_POINT('Ctrl Pts',(2.58605108794698,-42.6742356128,12.2751669368992));
#72010=CARTESIAN_POINT('Ctrl Pts',(2.43344031083315,-42.6742356128,12.3462470988987));
#72011=CARTESIAN_POINT('Ctrl Pts',(2.27808900582438,-42.6742356128,12.4107217696588));
#72012=CARTESIAN_POINT('Ctrl Pts',(2.12360328779087,-42.6742356128,12.4748372002102));
#72013=CARTESIAN_POINT('Ctrl Pts',(1.96640773805164,-42.6742356128,12.5324204058701));
#72014=CARTESIAN_POINT('Ctrl Pts',(1.80705892470451,-42.6742356128,12.583265045202));
#72015=CARTESIAN_POINT('Ctrl Pts',(1.64933517642864,-42.6742356128,12.6335911626466));
#72016=CARTESIAN_POINT('Ctrl Pts',(1.48950209987098,-42.6742356128,12.6773153642981));
#72017=CARTESIAN_POINT('Ctrl Pts',(1.32811474567441,-42.6742356128,12.7142860970285));
#72018=CARTESIAN_POINT('Ctrl Pts',(1.16777537817361,-42.6742356128,12.7510167562027));
#72019=CARTESIAN_POINT('Ctrl Pts',(1.00590207237904,-42.6742356128,12.7810812575043));
#72020=CARTESIAN_POINT('Ctrl Pts',(0.843050953735733,-42.6742356128,12.8043806957307));
#72021=CARTESIAN_POINT('Ctrl Pts',(0.681964641973335,-42.6742356128,12.8274276394748));
#72022=CARTESIAN_POINT('Ctrl Pts',(0.519921807453605,-42.6742356128,12.8438552832061));
#72023=CARTESIAN_POINT('Ctrl Pts',(0.357469083900356,-42.6742356128,12.8536179859801));
#72024=CARTESIAN_POINT('Ctrl Pts',(0.246023068049313,-42.6742356128,12.8603154072625));
#72025=CARTESIAN_POINT('Ctrl Pts',(0.134384321199348,-42.6742356128,12.8638771742974));
#72026=CARTESIAN_POINT('Ctrl Pts',(0.0227308830019703,-42.6742356128,12.8643026885943));
#72027=CARTESIAN_POINT('Ctrl Pts',(0.015153784542996,-42.6742356128,12.8643315651231));
#72028=CARTESIAN_POINT('Ctrl Pts',(0.00757664450181249,-42.6742356128,12.8643459888667));
#72029=CARTESIAN_POINT('Ctrl Pts',(-1.17395376619811E-6,-42.6742356128,
12.8643459882));
#72030=CARTESIAN_POINT('',(-5.94384246090667,-42.6742356128,6.92091847055));
#72031=CARTESIAN_POINT('Ctrl Pts',(-1.17395377015422E-6,-42.6742356128,
12.8643460035999));
#72032=CARTESIAN_POINT('Ctrl Pts',(-0.164706854594312,-42.6742356128,12.8643460048832));
#72033=CARTESIAN_POINT('Ctrl Pts',(-0.329412989973873,-42.6742356128,12.8575186542237));
#72034=CARTESIAN_POINT('Ctrl Pts',(-0.493544656307221,-42.6742356128,12.8438731963528));
#72035=CARTESIAN_POINT('Ctrl Pts',(-0.657503591528626,-42.6742356128,12.8302420988741));
#72036=CARTESIAN_POINT('Ctrl Pts',(-0.820889093836288,-42.6742356128,12.8098073874254));
#72037=CARTESIAN_POINT('Ctrl Pts',(-0.983136337600976,-42.6742356128,12.7826312009108));
#72038=CARTESIAN_POINT('Ctrl Pts',(-1.14639445651254,-42.6742356128,12.7552856942221));
#72039=CARTESIAN_POINT('Ctrl Pts',(-1.30849990009775,-42.6742356128,12.721114535931));
#72040=CARTESIAN_POINT('Ctrl Pts',(-1.46888834825522,-42.6742356128,12.6802329315353));
#72041=CARTESIAN_POINT('Ctrl Pts',(-1.63019316272522,-42.6742356128,12.6391177534285));
#72042=CARTESIAN_POINT('Ctrl Pts',(-1.78976110989173,-42.6742356128,12.5912153307976));
#72043=CARTESIAN_POINT('Ctrl Pts',(-1.94703226892316,-42.6742356128,12.536693743442));
#72044=CARTESIAN_POINT('Ctrl Pts',(-2.10550497071265,-42.6742356128,12.4817556142433));
#72045=CARTESIAN_POINT('Ctrl Pts',(-2.26164544450545,-42.6742356128,12.4200968838488));
#72046=CARTESIAN_POINT('Ctrl Pts',(-2.41489822703504,-42.6742356128,12.3519396246491));
#72047=CARTESIAN_POINT('Ctrl Pts',(-2.56867137509239,-42.6742356128,12.2835509393861));
#72048=CARTESIAN_POINT('Ctrl Pts',(-2.71953698323308,-42.6742356128,12.2086196487733));
#72049=CARTESIAN_POINT('Ctrl Pts',(-2.86695447501242,-42.6742356128,12.1274186462476));
#72050=CARTESIAN_POINT('Ctrl Pts',(-3.01498232800051,-42.6742356128,12.045881442492));
#72051=CARTESIAN_POINT('Ctrl Pts',(-3.15953323881548,-42.6742356128,11.9580226293889));
#72052=CARTESIAN_POINT('Ctrl Pts',(-3.30008374997782,-42.6742356128,11.8641654454777));
#72053=CARTESIAN_POINT('Ctrl Pts',(-3.42578603376579,-42.6742356128,11.7802236492509));
#72054=CARTESIAN_POINT('Ctrl Pts',(-3.54828872501526,-42.6742356128,11.6914846190643));
#72055=CARTESIAN_POINT('Ctrl Pts',(-3.66723551076089,-42.6742356128,11.5982098808653));
#72056=CARTESIAN_POINT('Ctrl Pts',(-3.80048768009197,-42.6742356128,11.4937172614902));
#72057=CARTESIAN_POINT('Ctrl Pts',(-3.92927735398716,-42.6742356128,11.3835310608653));
#72058=CARTESIAN_POINT('Ctrl Pts',(-4.05313446008693,-42.6742356128,11.268054647639));
#72059=CARTESIAN_POINT('Ctrl Pts',(-4.17729331738431,-42.6742356128,11.1522969009706));
#72060=CARTESIAN_POINT('Ctrl Pts',(-4.29649533405885,-42.6742356128,11.031223354757));
#72061=CARTESIAN_POINT('Ctrl Pts',(-4.41030279594079,-42.6742356128,10.905278524681));
#72062=CARTESIAN_POINT('Ctrl Pts',(-4.52419722051319,-42.6742356128,10.7792374574946));
#72063=CARTESIAN_POINT('Ctrl Pts',(-4.632688642205,-42.6742356128,10.6483178932861));
#72064=CARTESIAN_POINT('Ctrl Pts',(-4.73537722156243,-42.6742356128,10.5130001325075));
#72065=CARTESIAN_POINT('Ctrl Pts',(-4.83785496840781,-42.6742356128,10.3779601960362));
#72066=CARTESIAN_POINT('Ctrl Pts',(-4.93455349622713,-42.6742356128,10.2385403525583));
#72067=CARTESIAN_POINT('Ctrl Pts',(-5.02511695345455,-42.6742356128,10.0952489230484));
#72068=CARTESIAN_POINT('Ctrl Pts',(-5.11539650363132,-42.6742356128,9.95240669731646));
#72069=CARTESIAN_POINT('Ctrl Pts',(-5.19957922013242,-42.6742356128,9.80571736998885));
#72070=CARTESIAN_POINT('Ctrl Pts',(-5.27735649408011,-42.6742356128,9.65571158802438));
#72071=CARTESIAN_POINT('Ctrl Pts',(-5.35478979332208,-42.6742356128,9.50636921571785));
#72072=CARTESIAN_POINT('Ctrl Pts',(-5.42587402836502,-42.6742356128,9.35373990520833));
#72073=CARTESIAN_POINT('Ctrl Pts',(-5.49035064036701,-42.6742356128,9.1983704838353));
#72074=CARTESIAN_POINT('Ctrl Pts',(-5.55446924847197,-42.6742356128,9.04386374517158));
#72075=CARTESIAN_POINT('Ctrl Pts',(-5.61205326919096,-42.6742356128,8.88664748173921));
#72076=CARTESIAN_POINT('Ctrl Pts',(-5.66289614742354,-42.6742356128,8.72727879847535));
#72077=CARTESIAN_POINT('Ctrl Pts',(-5.7132219012526,-42.6742356128,8.56953105875636));
#72078=CARTESIAN_POINT('Ctrl Pts',(-5.75694285303024,-42.6742356128,8.40967470181282));
#72079=CARTESIAN_POINT('Ctrl Pts',(-5.79390721110658,-42.6742356128,8.24826540145233));
#72080=CARTESIAN_POINT('Ctrl Pts',(-5.83063199617447,-42.6742356128,8.08790222535021));
#72081=CARTESIAN_POINT('Ctrl Pts',(-5.86068737210952,-42.6742356128,7.92600638961922));
#72082=CARTESIAN_POINT('Ctrl Pts',(-5.88397418321587,-42.6742356128,7.76313470857918));
#72083=CARTESIAN_POINT('Ctrl Pts',(-5.90700909826615,-42.6742356128,7.60202482884));
#72084=CARTESIAN_POINT('Ctrl Pts',(-5.92342102136939,-42.6742356128,7.43996031329963));
#72085=CARTESIAN_POINT('Ctrl Pts',(-5.93316405737334,-42.6742356128,7.27748855031532));
#72086=CARTESIAN_POINT('Ctrl Pts',(-5.93983232068902,-42.6742356128,7.16629071665196));
#72087=CARTESIAN_POINT('Ctrl Pts',(-5.94337776755146,-42.6742356128,7.05490229328725));
#72088=CARTESIAN_POINT('Ctrl Pts',(-5.94379970723532,-42.6742356128,6.94350032657215));
#72089=CARTESIAN_POINT('Ctrl Pts',(-5.9438282162108,-42.6742356128,6.93597328880065));
#72090=CARTESIAN_POINT('Ctrl Pts',(-5.94384245634447,-42.6742356128,6.9284462137));
#72091=CARTESIAN_POINT('Ctrl Pts',(-5.94384245598,-42.6742356128,6.92091847055));
#72092=CARTESIAN_POINT('',(-5.94384247076,-42.6742356128,3.43894174696));
#72093=CARTESIAN_POINT('',(-5.94384247076,-42.6742356128,1.43032185727));
#72094=CARTESIAN_POINT('',(-6.7528793859,-42.6742356128,2.63899279271));
#72095=CARTESIAN_POINT('Ctrl Pts',(-5.94384247076,-42.6742356128,3.43894174696));
#72096=CARTESIAN_POINT('Ctrl Pts',(-5.94384247076,-42.6742356128,3.39614059129875));
#72097=CARTESIAN_POINT('Ctrl Pts',(-5.94731942992889,-42.6742356127938,
3.3533935597809));
#72098=CARTESIAN_POINT('Ctrl Pts',(-5.95417334989511,-42.6742356127904,
3.31121746702997));
#72099=CARTESIAN_POINT('Ctrl Pts',(-5.95690615429115,-42.674235612789,3.29440095731788));
#72100=CARTESIAN_POINT('Ctrl Pts',(-5.96017526355245,-42.6742356127902,
3.27767531133813));
#72101=CARTESIAN_POINT('Ctrl Pts',(-5.96397199512074,-42.6742356127937,
3.26107340308066));
#72102=CARTESIAN_POINT('Ctrl Pts',(-5.97319230916015,-42.6742356128024,
3.22075588127698));
#72103=CARTESIAN_POINT('Ctrl Pts',(-5.98553169840033,-42.6742356128,3.1811674117174));
#72104=CARTESIAN_POINT('Ctrl Pts',(-6.00083792640887,-42.6742356128,3.14276485597422));
#72105=CARTESIAN_POINT('Ctrl Pts',(-6.00772218970423,-42.6742356128,3.12549258583667));
#72106=CARTESIAN_POINT('Ctrl Pts',(-6.0152059741815,-42.6742356128,3.10846008240039));
#72107=CARTESIAN_POINT('Ctrl Pts',(-6.02327205093866,-42.6742356128,3.09170791617586));
#72108=CARTESIAN_POINT('Ctrl Pts',(-6.03947059121232,-42.6742356128,3.05806570727695));
#72109=CARTESIAN_POINT('Ctrl Pts',(-6.05802013722139,-42.6742356128,3.02555577603168));
#72110=CARTESIAN_POINT('Ctrl Pts',(-6.07874913502031,-42.6742356128,2.99449840731163));
#72111=CARTESIAN_POINT('Ctrl Pts',(-6.09893208502231,-42.6742356128,2.96425915859585));
#72112=CARTESIAN_POINT('Ctrl Pts',(-6.12118191381689,-42.6742356128,2.93539676884652));
#72113=CARTESIAN_POINT('Ctrl Pts',(-6.14529655206815,-42.6742356128,2.90818632861611));
#72114=CARTESIAN_POINT('Ctrl Pts',(-6.16874740818222,-42.6742356128,2.88172488590256));
#72115=CARTESIAN_POINT('Ctrl Pts',(-6.19396202990645,-42.6742356128,2.85682550380557));
#72116=CARTESIAN_POINT('Ctrl Pts',(-6.22071762118132,-42.6742356128,2.83370869611102));
#72117=CARTESIAN_POINT('Ctrl Pts',(-6.22880357679397,-42.6742356128,2.82672243746309));
#72118=CARTESIAN_POINT('Ctrl Pts',(-6.2370299924312,-42.6742356128,2.81989877398227));
#72119=CARTESIAN_POINT('Ctrl Pts',(-6.24538996627878,-42.6742356128,2.8132432049317));
#72120=CARTESIAN_POINT('Ctrl Pts',(-6.27451151430862,-42.6742356128,2.79005886520695));
#72121=CARTESIAN_POINT('Ctrl Pts',(-6.30525732125456,-42.6742356128,2.76891658397484));
#72122=CARTESIAN_POINT('Ctrl Pts',(-6.33732192296069,-42.6742356127995,
2.75001660009913));
#72123=CARTESIAN_POINT('Ctrl Pts',(-6.35684144186036,-42.6742356127992,
2.73851112138318));
#72124=CARTESIAN_POINT('Ctrl Pts',(-6.37684937766888,-42.6742356127987,
2.72783553419962));
#72125=CARTESIAN_POINT('Ctrl Pts',(-6.39727405799141,-42.6742356127981,
2.71802609152613));
#72126=CARTESIAN_POINT('Ctrl Pts',(-6.43357980892323,-42.674235612797,2.70058938373633));
#72127=CARTESIAN_POINT('Ctrl Pts',(-6.47119967282077,-42.6742356127982,
2.68589341404767));
#72128=CARTESIAN_POINT('Ctrl Pts',(-6.50971611872968,-42.6742356127991,
2.67409624258505));
#72129=CARTESIAN_POINT('Ctrl Pts',(-6.5284451026621,-42.6742356127994,2.66835975705121));
#72130=CARTESIAN_POINT('Ctrl Pts',(-6.54738579197464,-42.6742356127997,
2.66330789205722));
#72131=CARTESIAN_POINT('Ctrl Pts',(-6.56648857804215,-42.6742356127998,
2.65895478335595));
#72132=CARTESIAN_POINT('Ctrl Pts',(-6.61310155549509,-42.6742356128001,
2.64833270147608));
#72133=CARTESIAN_POINT('Ctrl Pts',(-6.66068112877502,-42.6742356128,2.64187392258124));
#72134=CARTESIAN_POINT('Ctrl Pts',(-6.70850709539224,-42.6742356128,2.63973511372826));
#72135=CARTESIAN_POINT('Ctrl Pts',(-6.72065123224425,-42.6742356128,2.63919201989768));
#72136=CARTESIAN_POINT('Ctrl Pts',(-6.73281108748355,-42.6742356128,2.63892725618837));
#72137=CARTESIAN_POINT('Ctrl Pts',(-6.74497451472132,-42.6742356128,2.63894302968162));
#72138=CARTESIAN_POINT('Ctrl Pts',(-6.7476092010827,-42.6742356128,2.63894644633441));
#72139=CARTESIAN_POINT('Ctrl Pts',(-6.75024538341664,-42.6742356128,2.63896303862909));
#72140=CARTESIAN_POINT('Ctrl Pts',(-6.7528793859,-42.6742356128,2.63899279271));
#72141=CARTESIAN_POINT('',(-0.779583726501,-42.6742356128,-4.94563238948));
#72142=CARTESIAN_POINT('Ctrl Pts',(-6.7528793859,-42.6742356128,2.63899279271));
#72143=CARTESIAN_POINT('Ctrl Pts',(-6.92377102533431,-42.6742356128,2.64092304741057));
#72144=CARTESIAN_POINT('Ctrl Pts',(-7.09474113659899,-42.6742356128,2.63578350248769));
#72145=CARTESIAN_POINT('Ctrl Pts',(-7.26520473277953,-42.6742356128,2.62358798817555));
#72146=CARTESIAN_POINT('Ctrl Pts',(-7.43683936146178,-42.6742356128,2.61130869442924));
#72147=CARTESIAN_POINT('Ctrl Pts',(-7.60796025492586,-42.6742356128,2.59187623037914));
#72148=CARTESIAN_POINT('Ctrl Pts',(-7.77797524513836,-42.6742356128,2.56535760473604));
#72149=CARTESIAN_POINT('Ctrl Pts',(-7.94902508875408,-42.6742356128,2.53867756456142));
#72150=CARTESIAN_POINT('Ctrl Pts',(-8.11895527770663,-42.6742356128,2.50482492446711));
#72151=CARTESIAN_POINT('Ctrl Pts',(-8.28717142756282,-42.6742356128,2.46392001704393));
#72152=CARTESIAN_POINT('Ctrl Pts',(-8.45663566918383,-42.6742356128,2.42271161273214));
#72153=CARTESIAN_POINT('Ctrl Pts',(-8.62436007967723,-42.6742356128,2.37434598658467));
#72154=CARTESIAN_POINT('Ctrl Pts',(-8.78974957389737,-42.6742356128,2.31899759320297));
#72155=CARTESIAN_POINT('Ctrl Pts',(-8.95563157807734,-42.6742356128,2.26348437898347));
#72156=CARTESIAN_POINT('Ctrl Pts',(-9.11916447820672,-42.6742356128,2.20094687292207));
#72157=CARTESIAN_POINT('Ctrl Pts',(-9.27976444923896,-42.6742356128,2.13161100458411));
#72158=CARTESIAN_POINT('Ctrl Pts',(-9.44080179314795,-42.6742356128,2.06208630913739));
#72159=CARTESIAN_POINT('Ctrl Pts',(-9.59888994577529,-42.6742356128,1.98572630214571));
#72160=CARTESIAN_POINT('Ctrl Pts',(-9.75346091790575,-42.6742356128,1.90280695099595));
#72161=CARTESIAN_POINT('Ctrl Pts',(-9.85690152582706,-42.6742356128,1.84731640207106));
#72162=CARTESIAN_POINT('Ctrl Pts',(-9.95876741745598,-42.6742356128,1.78888928526941));
#72163=CARTESIAN_POINT('Ctrl Pts',(-10.0588943984393,-42.6742356128,1.72761986311077));
#72164=CARTESIAN_POINT('Ctrl Pts',(-10.2085963618408,-42.6742356128,1.63601465636686));
#72165=CARTESIAN_POINT('Ctrl Pts',(-10.3544080750074,-42.6742356128,1.53805489504499));
#72166=CARTESIAN_POINT('Ctrl Pts',(-10.4958044832224,-42.6742356128,1.43409260848261));
#72167=CARTESIAN_POINT('Ctrl Pts',(-10.6368847189839,-42.6742356128,1.3303627890078));
#72168=CARTESIAN_POINT('Ctrl Pts',(-10.7735691317831,-42.6742356128,1.22065742461589));
#72169=CARTESIAN_POINT('Ctrl Pts',(-10.9053668778309,-42.6742356128,1.10536790176509));
#72170=CARTESIAN_POINT('Ctrl Pts',(-11.0366971527523,-42.6742356128,0.990487297311773));
#72171=CARTESIAN_POINT('Ctrl Pts',(-11.1631751349909,-42.6742356128,0.870062247857544));
#72172=CARTESIAN_POINT('Ctrl Pts',(-11.2843492080509,-42.6742356128,0.744518921524571));
#72173=CARTESIAN_POINT('Ctrl Pts',(-11.4046009580189,-42.6742356128,0.619931175094103));
#72174=CARTESIAN_POINT('Ctrl Pts',(-11.5196290385353,-42.6742356128,0.490302959907881));
#72175=CARTESIAN_POINT('Ctrl Pts',(-11.6290287556409,-42.6742356128,0.356086480044981));
#72176=CARTESIAN_POINT('Ctrl Pts',(-11.7378494261036,-42.6742356128,0.222580400575742));
#72177=CARTESIAN_POINT('Ctrl Pts',(-11.8411009566513,-42.6742356128,0.0845346663024816));
#72178=CARTESIAN_POINT('Ctrl Pts',(-11.9384244464344,-42.6742356128,-0.0575728384140106));
#72179=CARTESIAN_POINT('Ctrl Pts',(-12.0348336088766,-42.6742356128,-0.198345282322419));
#72180=CARTESIAN_POINT('Ctrl Pts',(-12.1254254315195,-42.6742356128,-0.343103357163285));
#72181=CARTESIAN_POINT('Ctrl Pts',(-12.2098924354945,-42.6742356128,-0.491352838062098));
#72182=CARTESIAN_POINT('Ctrl Pts',(-12.268639735316,-42.6742356128,-0.594461227053108));
#72183=CARTESIAN_POINT('Ctrl Pts',(-12.3244251412665,-42.6742356128,-0.699257892387985));
#72184=CARTESIAN_POINT('Ctrl Pts',(-12.3771578279306,-42.6742356128,-0.805568642615839));
#72185=CARTESIAN_POINT('Ctrl Pts',(-12.4532257315113,-42.6742356128,-0.958923922035363));
#72186=CARTESIAN_POINT('Ctrl Pts',(-12.5229376336484,-42.6742356128,-1.11542736371576));
#72187=CARTESIAN_POINT('Ctrl Pts',(-12.5860515296792,-42.6742356128,-1.27454370014428));
#72188=CARTESIAN_POINT('Ctrl Pts',(-12.6496267367883,-42.6742356128,-1.43482304715101));
#72189=CARTESIAN_POINT('Ctrl Pts',(-12.7065070981696,-42.6742356128,-1.597753382621));
#72190=CARTESIAN_POINT('Ctrl Pts',(-12.7564952320637,-42.6742356128,-1.76276934411767));
#72191=CARTESIAN_POINT('Ctrl Pts',(-12.8068026288887,-42.6742356128,-1.92883922532304));
#72192=CARTESIAN_POINT('Ctrl Pts',(-12.8501294506246,-42.6742356128,-2.09702120108295));
#72193=CARTESIAN_POINT('Ctrl Pts',(-12.8863254015399,-42.6742356128,-2.26672434958655));
#72194=CARTESIAN_POINT('Ctrl Pts',(-12.9227119363533,-42.6742356128,-2.43732104244341));
#72195=CARTESIAN_POINT('Ctrl Pts',(-12.9518922903244,-42.6742356128,-2.60945469813757));
#72196=CARTESIAN_POINT('Ctrl Pts',(-12.9737653933523,-42.6742356128,-2.78251424103995));
#72197=CARTESIAN_POINT('Ctrl Pts',(-12.9957250456641,-42.6742356128,-2.95625856010277));
#72198=CARTESIAN_POINT('Ctrl Pts',(-13.0103194960362,-42.6742356128,-3.13093582595532));
#72199=CARTESIAN_POINT('Ctrl Pts',(-13.0174985506679,-42.6742356128,-3.30592102821733));
#72200=CARTESIAN_POINT('Ctrl Pts',(-13.0249406122865,-42.6742356128,-3.48731686992664));
#72201=CARTESIAN_POINT('Ctrl Pts',(-13.0244136769526,-42.6742356128,-3.66904331228793));
#72202=CARTESIAN_POINT('Ctrl Pts',(-13.0159205917797,-42.6742356128,-3.85040149710429));
#72203=CARTESIAN_POINT('Ctrl Pts',(-13.0077589161263,-42.6742356128,-4.02468288619295));
#72204=CARTESIAN_POINT('Ctrl Pts',(-12.9922406788355,-42.6742356128,-4.19862603527503));
#72205=CARTESIAN_POINT('Ctrl Pts',(-12.9694214754203,-42.6742356128,-4.37160392560452));
#72206=CARTESIAN_POINT('Ctrl Pts',(-12.9464802820924,-42.6742356128,-4.54550654399528));
#72207=CARTESIAN_POINT('Ctrl Pts',(-12.9161600388264,-42.6742356128,-4.71843359904739));
#72208=CARTESIAN_POINT('Ctrl Pts',(-12.8785687783075,-42.6742356128,-4.8897636315973));
#72209=CARTESIAN_POINT('Ctrl Pts',(-12.8410768237495,-42.6742356128,-5.06064105645925));
#72210=CARTESIAN_POINT('Ctrl Pts',(-12.7963522654434,-42.6742356128,-5.2299296012495));
#72211=CARTESIAN_POINT('Ctrl Pts',(-12.7445528469835,-42.6742356128,-5.39702377187447));
#72212=CARTESIAN_POINT('Ctrl Pts',(-12.692955085043,-42.6742356128,-5.56346744043058));
#72213=CARTESIAN_POINT('Ctrl Pts',(-12.6343374980566,-42.6742356128,-5.72773351285106));
#72214=CARTESIAN_POINT('Ctrl Pts',(-12.5689054311692,-42.6742356128,-5.88923868726432));
#72215=CARTESIAN_POINT('Ctrl Pts',(-12.5039776015438,-42.6742356128,-6.04949925898035));
#72216=CARTESIAN_POINT('Ctrl Pts',(-12.4323400011397,-42.6742356128,-6.20704107056944));
#72217=CARTESIAN_POINT('Ctrl Pts',(-12.3542409292231,-42.6742356128,-6.36131303593145));
#72218=CARTESIAN_POINT('Ctrl Pts',(-12.2765647547587,-42.6742356128,-6.51474963642295));
#72219=CARTESIAN_POINT('Ctrl Pts',(-12.1924969600612,-42.6742356128,-6.66495145996804));
#72220=CARTESIAN_POINT('Ctrl Pts',(-12.1023280783887,-42.6742356128,-6.81139873697023));
#72221=CARTESIAN_POINT('Ctrl Pts',(-12.0129470463386,-42.6742356128,-6.95656643248342));
#72222=CARTESIAN_POINT('Ctrl Pts',(-11.9175711644125,-42.6742356128,-7.09804468603061));
#72223=CARTESIAN_POINT('Ctrl Pts',(-11.8165278203223,-42.6742356128,-7.23535275773844));
#72224=CARTESIAN_POINT('Ctrl Pts',(-11.7830752393437,-42.6742356128,-7.28081155989094));
#72225=CARTESIAN_POINT('Ctrl Pts',(-11.7490018150758,-42.6742356128,-7.32581349837004));
#72226=CARTESIAN_POINT('Ctrl Pts',(-11.7143204894683,-42.6742356128,-7.37034181538974));
#72227=CARTESIAN_POINT('Ctrl Pts',(-11.6090374799616,-42.6742356128,-7.50551759491913));
#72228=CARTESIAN_POINT('Ctrl Pts',(-11.4981515428722,-42.6742356128,-7.63632322849263));
#72229=CARTESIAN_POINT('Ctrl Pts',(-11.3820409767117,-42.6742356128,-7.76230784158382));
#72230=CARTESIAN_POINT('Ctrl Pts',(-11.2650896267103,-42.6742356128,-7.88920473880554));
#72231=CARTESIAN_POINT('Ctrl Pts',(-11.1428379117467,-42.6742356128,-8.01121040408434));
#72232=CARTESIAN_POINT('Ctrl Pts',(-11.0157106099601,-42.6742356128,-8.12790111131797));
#72233=CARTESIAN_POINT('Ctrl Pts',(-10.8877834955309,-42.6742356128,-8.24532597008016));
#72234=CARTESIAN_POINT('Ctrl Pts',(-10.7549194727002,-42.6742356128,-8.35736864419994));
#72235=CARTESIAN_POINT('Ctrl Pts',(-10.6175867190644,-42.6742356128,-8.46363679340583));
#72236=CARTESIAN_POINT('Ctrl Pts',(-10.4795477508587,-42.6742356128,-8.57045141177738));
#72237=CARTESIAN_POINT('Ctrl Pts',(-10.3369942102914,-42.6742356128,-8.67143182642991));
#72238=CARTESIAN_POINT('Ctrl Pts',(-10.1904336618126,-42.6742356128,-8.76622139845801));
#72239=CARTESIAN_POINT('Ctrl Pts',(-10.0433150051289,-42.6742356128,-8.86137193282168));
#72240=CARTESIAN_POINT('Ctrl Pts',(-9.89215901548288,-42.6742356128,-8.95028425309374));
#72241=CARTESIAN_POINT('Ctrl Pts',(-9.73750768486439,-42.6742356128,-9.03264163716008));
#72242=CARTESIAN_POINT('Ctrl Pts',(-9.57733278527883,-42.6742356128,-9.11794051994497));
#72243=CARTESIAN_POINT('Ctrl Pts',(-9.41340855055791,-42.6742356128,-9.19620745294721));
#72244=CARTESIAN_POINT('Ctrl Pts',(-9.24636493029186,-42.6742356128,-9.26714220767078));
#72245=CARTESIAN_POINT('Ctrl Pts',(-9.10197090675754,-42.6742356128,-9.32845885434453));
#72246=CARTESIAN_POINT('Ctrl Pts',(-8.95524480384927,-42.6742356128,-9.38429823234259));
#72247=CARTESIAN_POINT('Ctrl Pts',(-8.80661470177786,-42.6742356128,-9.43449693353395));
#72248=CARTESIAN_POINT('Ctrl Pts',(-8.64045654990412,-42.6742356128,-9.49061560196096));
#72249=CARTESIAN_POINT('Ctrl Pts',(-8.47191949133974,-42.6742356128,-9.5396838161239));
#72250=CARTESIAN_POINT('Ctrl Pts',(-8.30160860483715,-42.6742356128,-9.5815245018864));
#72251=CARTESIAN_POINT('Ctrl Pts',(-8.13175340326074,-42.6742356128,-9.62325323843535));
#72252=CARTESIAN_POINT('Ctrl Pts',(-7.960134129673,-42.6742356128,-9.65779298871373));
#72253=CARTESIAN_POINT('Ctrl Pts',(-7.78736340133293,-42.6742356128,-9.68501834033365));
#72254=CARTESIAN_POINT('Ctrl Pts',(-7.61527114017249,-42.6742356128,-9.71213677854465));
#72255=CARTESIAN_POINT('Ctrl Pts',(-7.44203672137731,-42.6742356128,-9.7319980826045));
#72256=CARTESIAN_POINT('Ctrl Pts',(-7.26827378018691,-42.6742356128,-9.74452934705639));
#72257=CARTESIAN_POINT('Ctrl Pts',(-7.09587297012232,-42.6742356128,-9.7569623786789));
#72258=CARTESIAN_POINT('Ctrl Pts',(-6.92295215394564,-42.6742356128,-9.76217980786957));
#72259=CARTESIAN_POINT('Ctrl Pts',(-6.75011476368856,-42.6742356128,-9.7601614805935));
#72260=CARTESIAN_POINT('Ctrl Pts',(-6.57821936998901,-42.6742356128,-9.75815415358388));
#72261=CARTESIAN_POINT('Ctrl Pts',(-6.40640674483326,-42.6742356128,-9.74898967690743));
#72262=CARTESIAN_POINT('Ctrl Pts',(-6.2352707865071,-42.6742356128,-9.73269957300655));
#72263=CARTESIAN_POINT('Ctrl Pts',(-6.06567484140039,-42.6742356128,-9.71655606001268));
#72264=CARTESIAN_POINT('Ctrl Pts',(-5.89674367410256,-42.6742356128,-9.69341456947751));
#72265=CARTESIAN_POINT('Ctrl Pts',(-5.72905197408973,-42.6742356128,-9.66335680406608));
#72266=CARTESIAN_POINT('Ctrl Pts',(-5.65633979088631,-42.6742356128,-9.65032356661238));
#72267=CARTESIAN_POINT('Ctrl Pts',(-5.58386058221207,-42.6742356128,-9.63599062406029));
#72268=CARTESIAN_POINT('Ctrl Pts',(-5.51166083356658,-42.6742356128,-9.62036767336498));
#72269=CARTESIAN_POINT('Ctrl Pts',(-5.34553008021385,-42.6742356128,-9.58441945169806));
#72270=CARTESIAN_POINT('Ctrl Pts',(-5.18088487182742,-42.6742356128,-9.54163888505871));
#72271=CARTESIAN_POINT('Ctrl Pts',(-5.01828069868697,-42.6742356128,-9.49216531343611));
#72272=CARTESIAN_POINT('Ctrl Pts',(-4.85368753416137,-42.6742356128,-9.44208657587067));
#72273=CARTESIAN_POINT('Ctrl Pts',(-4.69118586381926,-42.6742356128,-9.38515019160763));
#72274=CARTESIAN_POINT('Ctrl Pts',(-4.53133558518016,-42.6742356127989,
-9.32155164731861));
#72275=CARTESIAN_POINT('Ctrl Pts',(-4.37049551713942,-42.6742356127977,
-9.25755930224529));
#72276=CARTESIAN_POINT('Ctrl Pts',(-4.21233999388847,-42.6742356127957,
-9.18682219542086));
#72277=CARTESIAN_POINT('Ctrl Pts',(-4.05741975468309,-42.6742356127869,
-9.10958874043621));
#72278=CARTESIAN_POINT('Ctrl Pts',(-3.9012794912673,-42.674235612778,-9.03174705837019));
#72279=CARTESIAN_POINT('Ctrl Pts',(-3.74842590424833,-42.6742356127626,
-8.94730645802646));
#72280=CARTESIAN_POINT('Ctrl Pts',(-3.59939955038934,-42.6742356127243,
-8.85656883986676));
#72281=CARTESIAN_POINT('Ctrl Pts',(-3.52827949945173,-42.6742356127061,
-8.81326600209095));
#72282=CARTESIAN_POINT('Ctrl Pts',(-3.45803073797694,-42.6742356126824,
-8.76852969966192));
#72283=CARTESIAN_POINT('Ctrl Pts',(-3.38870993135324,-42.67423561265,-8.7223963607209));
#72284=CARTESIAN_POINT('Ctrl Pts',(-3.24323874551504,-42.6742356125822,
-8.62558456857231));
#72285=CARTESIAN_POINT('Ctrl Pts',(-3.10185699243564,-42.6742356125117,
-8.52261712902016));
#72286=CARTESIAN_POINT('Ctrl Pts',(-2.96506951706885,-42.6742356124598,
-8.41386451273636));
#72287=CARTESIAN_POINT('Ctrl Pts',(-2.82781328827125,-42.6742356124077,
-8.30473921494896));
#72288=CARTESIAN_POINT('Ctrl Pts',(-2.69518312142502,-42.6742356123738,
-8.18978922737835));
#72289=CARTESIAN_POINT('Ctrl Pts',(-2.56765662468396,-42.6742356123612,
-8.06943004369615));
#72290=CARTESIAN_POINT('Ctrl Pts',(-2.44012637314771,-42.6742356123487,
-7.94906731624778));
#72291=CARTESIAN_POINT('Ctrl Pts',(-2.31770031683979,-42.6742356123569,
-7.82329530435268));
#72292=CARTESIAN_POINT('Ctrl Pts',(-2.20082023554204,-42.6742356123795,
-7.69256736730877));
#72293=CARTESIAN_POINT('Ctrl Pts',(-2.08412128240898,-42.674235612402,-7.5620420183453));
#72294=CARTESIAN_POINT('Ctrl Pts',(-1.97295134094947,-42.6742356124384,
-7.42657633123456));
#72295=CARTESIAN_POINT('Ctrl Pts',(-1.86771112173087,-42.6742356124791,
-7.28665574540306));
#72296=CARTESIAN_POINT('Ctrl Pts',(-1.76279308389599,-42.6742356125197,
-7.14716351109238));
#72297=CARTESIAN_POINT('Ctrl Pts',(-1.6637687149937,-42.6742356125643,-7.00324385547099));
#72298=CARTESIAN_POINT('Ctrl Pts',(-1.57099319647258,-42.6742356126051,
-6.85540816315929));
#72299=CARTESIAN_POINT('Ctrl Pts',(-1.47891116550525,-42.6742356126455,
-6.7086775275938));
#72300=CARTESIAN_POINT('Ctrl Pts',(-1.39298507142996,-42.674235612682,-6.55808943413321));
#72301=CARTESIAN_POINT('Ctrl Pts',(-1.31351830313044,-42.6742356127107,
-6.40417013889175));
#72302=CARTESIAN_POINT('Ctrl Pts',(-1.23447264371694,-42.6742356127392,
-6.25106649004366));
#72303=CARTESIAN_POINT('Ctrl Pts',(-1.16181819676399,-42.67423561276,-6.09466708554217));
#72304=CARTESIAN_POINT('Ctrl Pts',(-1.09580756166894,-42.6742356127736,
-5.9355123158406));
#72305=CARTESIAN_POINT('Ctrl Pts',(-1.0304709446788,-42.6742356127871,-5.77798263573418));
#72306=CARTESIAN_POINT('Ctrl Pts',(-0.971643269281571,-42.6742356127937,
-5.61775380907576));
#72307=CARTESIAN_POINT('Ctrl Pts',(-0.919522300230464,-42.6742356127969,
-5.45536837298743));
#72308=CARTESIAN_POINT('Ctrl Pts',(-0.867847187573667,-42.6742356128,-5.29437202436889));
#72309=CARTESIAN_POINT('Ctrl Pts',(-0.822764645901731,-42.6742356128,-5.13125602266412));
#72310=CARTESIAN_POINT('Ctrl Pts',(-0.78441907782484,-42.6742356128,-4.96656404596631));
#72311=CARTESIAN_POINT('Ctrl Pts',(-0.782795283673876,-42.6742356128,-4.95958994486716));
#72312=CARTESIAN_POINT('Ctrl Pts',(-0.781183576258786,-42.6742356128,-4.95261299441384));
#72313=CARTESIAN_POINT('Ctrl Pts',(-0.779583726501,-42.6742356128,-4.94563238948));
#72314=CARTESIAN_POINT('',(-1.92001921505849E-7,-42.6742356128,-4.32434669440466));
#72315=CARTESIAN_POINT('Ctrl Pts',(-0.779583726501,-42.6742356128,-4.94563238948));
#72316=CARTESIAN_POINT('Ctrl Pts',(-0.770339586016146,-42.6742356128,-4.90529749155185));
#72317=CARTESIAN_POINT('Ctrl Pts',(-0.757952557321631,-42.6742356128,-4.86571925121627));
#72318=CARTESIAN_POINT('Ctrl Pts',(-0.742592335257283,-42.6742356128,-4.82734087116641));
#72319=CARTESIAN_POINT('Ctrl Pts',(-0.727732731079844,-42.6742356128,-4.79021331310618));
#72320=CARTESIAN_POINT('Ctrl Pts',(-0.71009068241812,-42.6742356128,-4.75420963049573));
#72321=CARTESIAN_POINT('Ctrl Pts',(-0.689867037474384,-42.6742356128,-4.71972195099769));
#72322=CARTESIAN_POINT('Ctrl Pts',(-0.67972492593344,-42.6742356128,-4.7024264588532));
#72323=CARTESIAN_POINT('Ctrl Pts',(-0.668934286154698,-42.6742356128,-4.6855120087769));
#72324=CARTESIAN_POINT('Ctrl Pts',(-0.657525035376213,-42.6742356128,-4.66902604106184));
#72325=CARTESIAN_POINT('Ctrl Pts',(-0.636024130235446,-42.6742356128,-4.63795798629844));
#72326=CARTESIAN_POINT('Ctrl Pts',(-0.612323425048321,-42.6742356128,-4.60841296301403));
#72327=CARTESIAN_POINT('Ctrl Pts',(-0.586653996613761,-42.6742356128,-4.5806891190954));
#72328=CARTESIAN_POINT('Ctrl Pts',(-0.577855991671729,-42.6742356128,-4.57118697858495));
#72329=CARTESIAN_POINT('Ctrl Pts',(-0.568827070431133,-42.6742356128,-4.56189851480791));
#72330=CARTESIAN_POINT('Ctrl Pts',(-0.559577658427724,-42.6742356128,-4.55283483251327));
#72331=CARTESIAN_POINT('Ctrl Pts',(-0.53393557106704,-42.6742356128,-4.52770764246886));
#72332=CARTESIAN_POINT('Ctrl Pts',(-0.506597397053191,-42.6742356128,-4.50431172009628));
#72333=CARTESIAN_POINT('Ctrl Pts',(-0.477809692424286,-42.6742356128,-4.48286055934883));
#72334=CARTESIAN_POINT('Ctrl Pts',(-0.465912990238111,-42.6742356128,-4.47399573062247));
#72335=CARTESIAN_POINT('Ctrl Pts',(-0.453769151708002,-42.6742356128,-4.46546260164222));
#72336=CARTESIAN_POINT('Ctrl Pts',(-0.44139735549178,-42.6742356128,-4.45727428681099));
#72337=CARTESIAN_POINT('Ctrl Pts',(-0.410257347175726,-42.6742356128,-4.43666416783696));
#72338=CARTESIAN_POINT('Ctrl Pts',(-0.377671015886976,-42.6742356128001,
-4.41824161902664));
#72339=CARTESIAN_POINT('Ctrl Pts',(-0.343960679444774,-42.6742356127991,
-4.40218302518042));
#72340=CARTESIAN_POINT('Ctrl Pts',(-0.331872099374508,-42.6742356127987,
-4.39642438797848));
#72341=CARTESIAN_POINT('Ctrl Pts',(-0.319639082799004,-42.6742356127982,
-4.39096925555829));
#72342=CARTESIAN_POINT('Ctrl Pts',(-0.30727685469933,-42.6742356127976,
-4.3858242042423));
#72343=CARTESIAN_POINT('Ctrl Pts',(-0.270146176475813,-42.6742356127959,
-4.37037074040737));
#72344=CARTESIAN_POINT('Ctrl Pts',(-0.23185666760706,-42.6742356127962,
-4.35772125484493));
#72345=CARTESIAN_POINT('Ctrl Pts',(-0.192827890891106,-42.6742356127974,
-4.3480119902983));
#72346=CARTESIAN_POINT('Ctrl Pts',(-0.151055129146623,-42.6742356127986,
-4.33762009926949));
#72347=CARTESIAN_POINT('Ctrl Pts',(-0.108435042767796,-42.6742356127998,
-4.33059591170187));
#72348=CARTESIAN_POINT('Ctrl Pts',(-0.0655037400434273,-42.6742356127999,
-4.32705002118447));
#72349=CARTESIAN_POINT('Ctrl Pts',(-0.0473517386002392,-42.6742356128,-4.32555076526385));
#72350=CARTESIAN_POINT('Ctrl Pts',(-0.0291443943596306,-42.6742356128,-4.32467272136695));
#72351=CARTESIAN_POINT('Ctrl Pts',(-0.0109235923233173,-42.6742356128,-4.32442189871929));
#72352=CARTESIAN_POINT('Ctrl Pts',(-0.0072829618668721,-42.6742356128,-4.32437178278211));
#72353=CARTESIAN_POINT('Ctrl Pts',(-0.00364100425362554,-42.6742356128,
-4.32434670023877));
#72354=CARTESIAN_POINT('Ctrl Pts',(-3.83477804066779E-7,-42.6742356128,
-4.32434669416));
#72355=CARTESIAN_POINT('Ctrl Pts',(-6.27276008913E-15,-42.6742356128,-4.32434669465));
#72356=CARTESIAN_POINT('Ctrl Pts',(0.0418710994610801,-42.6742356128,-4.32434671500355));
#72357=CARTESIAN_POINT('Ctrl Pts',(0.0837043788816997,-42.6742356128,-4.3276623402763));
#72358=CARTESIAN_POINT('Ctrl Pts',(0.125013272835771,-42.6742356128,-4.33422057793384));
#72359=CARTESIAN_POINT('Ctrl Pts',(0.164771346375193,-42.6742356128,-4.34053260592876));
#72360=CARTESIAN_POINT('Ctrl Pts',(0.204042705126419,-42.6742356128,-4.34984847391554));
#72361=CARTESIAN_POINT('Ctrl Pts',(0.242392380067074,-42.6742356128,-4.362055492168));
#72362=CARTESIAN_POINT('Ctrl Pts',(0.260743896289878,-42.6742356128,-4.36789693134157));
#72363=CARTESIAN_POINT('Ctrl Pts',(0.278884424047291,-42.6742356128,-4.37439969445921));
#72364=CARTESIAN_POINT('Ctrl Pts',(0.296767143629254,-42.6742356128,-4.38154722137599));
#72365=CARTESIAN_POINT('Ctrl Pts',(0.331742254434663,-42.6742356128,-4.39552638963131));
#72366=CARTESIAN_POINT('Ctrl Pts',(0.365730473692324,-42.6742356128,-4.4119749533356));
#72367=CARTESIAN_POINT('Ctrl Pts',(0.39839280384516,-42.6742356128,-4.43073575255324));
#72368=CARTESIAN_POINT('Ctrl Pts',(0.429691506349557,-42.6742356128,-4.44871330255381));
#72369=CARTESIAN_POINT('Ctrl Pts',(0.459772353724042,-42.6742356128,-4.46881415672584));
#72370=CARTESIAN_POINT('Ctrl Pts',(0.48835644570818,-42.6742356128,-4.49085721429512));
#72371=CARTESIAN_POINT('Ctrl Pts',(0.510283685623865,-42.6742356128,-4.50776673907783));
#72372=CARTESIAN_POINT('Ctrl Pts',(0.531330750563295,-42.6742356128,-4.52581851907484));
#72373=CARTESIAN_POINT('Ctrl Pts',(0.551383898576014,-42.6742356128,-4.54491381005563));
#72374=CARTESIAN_POINT('Ctrl Pts',(0.578386538937482,-42.6742356128,-4.57062664450061));
#72375=CARTESIAN_POINT('Ctrl Pts',(0.603585765744263,-42.6742356128001,
-4.59823263562595));
#72376=CARTESIAN_POINT('Ctrl Pts',(0.62673854776236,-42.6742356127992,-4.62745825901451));
#72377=CARTESIAN_POINT('Ctrl Pts',(0.635091421482877,-42.6742356127989,
-4.63800204340195));
#72378=CARTESIAN_POINT('Ctrl Pts',(0.643178393391744,-42.6742356127985,
-4.64875641850709));
#72379=CARTESIAN_POINT('Ctrl Pts',(0.650989517822355,-42.674235612798,-4.65970782242662));
#72380=CARTESIAN_POINT('Ctrl Pts',(0.674231624148513,-42.6742356127964,
-4.69229387281917));
#72381=CARTESIAN_POINT('Ctrl Pts',(0.695023442466847,-42.6742356127966,
-4.72661905129764));
#72382=CARTESIAN_POINT('Ctrl Pts',(0.713142368797677,-42.6742356127976,
-4.76230994089147));
#72383=CARTESIAN_POINT('Ctrl Pts',(0.732451655575785,-42.6742356127987,
-4.80034561750661));
#72384=CARTESIAN_POINT('Ctrl Pts',(0.748725829968211,-42.6742356127998,
-4.83993264972833));
#72385=CARTESIAN_POINT('Ctrl Pts',(0.761745590136327,-42.6742356127999,
-4.88058615396062));
#72386=CARTESIAN_POINT('Ctrl Pts',(0.767488735920299,-42.6742356128,-4.89851881926478));
#72387=CARTESIAN_POINT('Ctrl Pts',(0.772599221477852,-42.6742356128,-4.91665855611848));
#72388=CARTESIAN_POINT('Ctrl Pts',(0.777060571531673,-42.6742356128,-4.93496167066254));
#72389=CARTESIAN_POINT('Ctrl Pts',(0.777815731721221,-42.6742356128,-4.93805978743923));
#72390=CARTESIAN_POINT('Ctrl Pts',(0.778552314305808,-42.6742356128,-4.94116264967606));
#72391=CARTESIAN_POINT('Ctrl Pts',(0.779270224014823,-42.6742356128,-4.94426996798293));
#72392=CARTESIAN_POINT('Ctrl Pts',(0.779375237689296,-42.6742356128,-4.94472449716545));
#72393=CARTESIAN_POINT('Ctrl Pts',(0.779479851147667,-42.6742356128,-4.94517911900667));
#72394=CARTESIAN_POINT('Ctrl Pts',(0.779584041801,-42.6742356128,-4.94563373444));
#72395=CARTESIAN_POINT('',(5.54384247000667,-42.6742356128,3.12351053169));
#72396=CARTESIAN_POINT('',(5.54384245881164,-42.6742356128,6.92091963994));
#72397=CARTESIAN_POINT('',(5.54384247076,-42.6742356128,1.77756718468));
#72398=CARTESIAN_POINT('',(4.98144931501833,-42.6742356128,2.35961165425857));
#72399=CARTESIAN_POINT('Ctrl Pts',(4.98144948316736,-42.6742356128,2.35961170656036));
#72400=CARTESIAN_POINT('Ctrl Pts',(5.02061454614235,-42.6742356128,2.37179381057219));
#72401=CARTESIAN_POINT('Ctrl Pts',(5.05880901067664,-42.6742356128,2.38699634304257));
#72402=CARTESIAN_POINT('Ctrl Pts',(5.0956106138185,-42.6742356128,2.40502524049932));
#72403=CARTESIAN_POINT('Ctrl Pts',(5.13126969987241,-42.6742356128,2.4224944252897));
#72404=CARTESIAN_POINT('Ctrl Pts',(5.16562018730549,-42.6742356128,2.44261704816507));
#72405=CARTESIAN_POINT('Ctrl Pts',(5.19829190310246,-42.6742356128,2.4651700559157));
#72406=CARTESIAN_POINT('Ctrl Pts',(5.21049951593566,-42.6742356128,2.47359686730678));
#72407=CARTESIAN_POINT('Ctrl Pts',(5.22247296352245,-42.6742356128,2.48236252078492));
#72408=CARTESIAN_POINT('Ctrl Pts',(5.23419382990894,-42.6742356128,2.49145370342273));
#72409=CARTESIAN_POINT('Ctrl Pts',(5.26403643920578,-42.6742356128,2.51460084993566));
#72410=CARTESIAN_POINT('Ctrl Pts',(5.29223950540321,-42.6742356128,2.53986119092365));
#72411=CARTESIAN_POINT('Ctrl Pts',(5.31851865739924,-42.6742356128,2.5669873519108));
#72412=CARTESIAN_POINT('Ctrl Pts',(5.32550593200998,-42.6742356128,2.57419983486996));
#72413=CARTESIAN_POINT('Ctrl Pts',(5.33235737434974,-42.6742356128,2.58154400578135));
#72414=CARTESIAN_POINT('Ctrl Pts',(5.33906805847429,-42.6742356128,2.58901473966406));
#72415=CARTESIAN_POINT('Ctrl Pts',(5.36318747049904,-42.6742356128,2.61586590793544));
#72416=CARTESIAN_POINT('Ctrl Pts',(5.38548485109696,-42.6742356128,2.64435374065739));
#72417=CARTESIAN_POINT('Ctrl Pts',(5.40575467525082,-42.6742356128,2.67421842643644));
#72418=CARTESIAN_POINT('Ctrl Pts',(5.41233781008693,-42.6742356128,2.6839177337333));
#72419=CARTESIAN_POINT('Ctrl Pts',(5.41870738243033,-42.6742356128,2.69376200286744));
#72420=CARTESIAN_POINT('Ctrl Pts',(5.42485727315772,-42.6742356128,2.70374155831051));
#72421=CARTESIAN_POINT('Ctrl Pts',(5.4444023437645,-42.6742356128,2.73545775041947));
#72422=CARTESIAN_POINT('Ctrl Pts',(5.46172526525044,-42.6742356128,2.76854259355569));
#72423=CARTESIAN_POINT('Ctrl Pts',(5.4766603444294,-42.6742356127988,2.80266885969859));
#72424=CARTESIAN_POINT('Ctrl Pts',(5.49214926650727,-42.6742356127975,2.83806064241109));
#72425=CARTESIAN_POINT('Ctrl Pts',(5.50507023096377,-42.674235612795,2.87457310110306));
#72426=CARTESIAN_POINT('Ctrl Pts',(5.51529386257496,-42.6742356127955,2.91183085727209));
#72427=CARTESIAN_POINT('Ctrl Pts',(5.52051739832013,-42.6742356127958,2.93086687387907));
#72428=CARTESIAN_POINT('Ctrl Pts',(5.52503765376591,-42.674235612797,2.95009722852049));
#72429=CARTESIAN_POINT('Ctrl Pts',(5.52884225515805,-42.6742356127983,2.96947009082168));
#72430=CARTESIAN_POINT('Ctrl Pts',(5.53697901810226,-42.6742356128011,3.01090212846463));
#72431=CARTESIAN_POINT('Ctrl Pts',(5.54183789209737,-42.6742356128,3.05298314735757));
#72432=CARTESIAN_POINT('Ctrl Pts',(5.54333924500842,-42.6742356128,3.09520879650193));
#72433=CARTESIAN_POINT('Ctrl Pts',(5.54364552076626,-42.6742356128,3.10382282228966));
#72434=CARTESIAN_POINT('Ctrl Pts',(5.54381218081857,-42.6742356128,3.11244273439275));
#72435=CARTESIAN_POINT('Ctrl Pts',(5.54383870476508,-42.6742356128,3.12106402816618));
#72436=CARTESIAN_POINT('Ctrl Pts',(5.54384121393877,-42.6742356128,3.12187960527063));
#72437=CARTESIAN_POINT('Ctrl Pts',(5.54384246876333,-42.6742356128,3.12269520399));
#72438=CARTESIAN_POINT('Ctrl Pts',(5.54384246963,-42.6742356128,3.12351053169));
#72439=CARTESIAN_POINT('',(0.7797602054102,-42.6742356128,-2.1748213248982));
#72440=CARTESIAN_POINT('Ctrl Pts',(0.779760433538598,-42.6742356128,-2.17482033007699));
#72441=CARTESIAN_POINT('Ctrl Pts',(0.82008088638103,-42.6742356128,-1.99899136424202));
#72442=CARTESIAN_POINT('Ctrl Pts',(0.868120974796676,-42.6742356128,-1.82488581137916));
#72443=CARTESIAN_POINT('Ctrl Pts',(0.923660857455244,-42.6742356128,-1.65320006696145));
#72444=CARTESIAN_POINT('Ctrl Pts',(0.978754958155079,-42.6742356128,-1.48289233063035));
#72445=CARTESIAN_POINT('Ctrl Pts',(1.04122908190946,-42.6742356128,-1.31496565181674));
#72446=CARTESIAN_POINT('Ctrl Pts',(1.11083180500875,-42.6742356128,-1.15006455618185));
#72447=CARTESIAN_POINT('Ctrl Pts',(1.17987810904471,-42.6742356128,-0.986481715194041));
#72448=CARTESIAN_POINT('Ctrl Pts',(1.25593962112789,-42.6742356128,-0.825876216584327));
#72449=CARTESIAN_POINT('Ctrl Pts',(1.33873253370372,-42.6742356128,-0.668843344668419));
#72450=CARTESIAN_POINT('Ctrl Pts',(1.42051548793609,-42.6742356128,-0.513726055309701));
#72451=CARTESIAN_POINT('Ctrl Pts',(1.50886670645572,-42.6742356128,-0.36209468242655));
#72452=CARTESIAN_POINT('Ctrl Pts',(1.60347348717891,-42.6742356128,-0.214490841091055));
#72453=CARTESIAN_POINT('Ctrl Pts',(1.69744929431954,-42.6742356128,-0.067871433681505));
#72454=CARTESIAN_POINT('Ctrl Pts',(1.79759761771214,-42.6742356128,0.0747740334099692));
#72455=CARTESIAN_POINT('Ctrl Pts',(1.90357150485393,-42.6742356128,0.212945727140077));
#72456=CARTESIAN_POINT('Ctrl Pts',(2.00841817475825,-42.6742356128,0.349647723767401));
#72457=CARTESIAN_POINT('Ctrl Pts',(2.11896721928139,-42.6742356128,0.481970679030743));
#72458=CARTESIAN_POINT('Ctrl Pts',(2.23484145936028,-42.6742356128,0.609460133745291));
#72459=CARTESIAN_POINT('Ctrl Pts',(2.33817498809426,-42.6742356128,0.723151798286571));
#72460=CARTESIAN_POINT('Ctrl Pts',(2.445742944833,-42.6742356128,0.832999982031719));
#72461=CARTESIAN_POINT('Ctrl Pts',(2.55724886492688,-42.6742356128,0.938702013268061));
#72462=CARTESIAN_POINT('Ctrl Pts',(2.68199902176198,-42.6742356128,1.05695891804424));
#72463=CARTESIAN_POINT('Ctrl Pts',(2.81167944725901,-42.6742356128,1.17002607613155));
#72464=CARTESIAN_POINT('Ctrl Pts',(2.94584550454677,-42.6742356128,1.27751782547255));
#72465=CARTESIAN_POINT('Ctrl Pts',(3.08194386060407,-42.6742356128,1.38655770240398));
#72466=CARTESIAN_POINT('Ctrl Pts',(3.22265784039016,-42.6742356128,1.48986042507482));
#72467=CARTESIAN_POINT('Ctrl Pts',(3.36748660588292,-42.6742356128,1.58706255794715));
#72468=CARTESIAN_POINT('Ctrl Pts',(3.51565498560908,-42.6742356128,1.68650607998932));
#72469=CARTESIAN_POINT('Ctrl Pts',(3.6681299835651,-42.6742356128,1.77956437899082));
#72470=CARTESIAN_POINT('Ctrl Pts',(3.82433912948244,-42.6742356128,1.86588929707841));
#72471=CARTESIAN_POINT('Ctrl Pts',(3.98280673611594,-42.6742356128,1.95346229468901));
#72472=CARTESIAN_POINT('Ctrl Pts',(4.14511704822198,-42.6742356128,2.03410582589879));
#72473=CARTESIAN_POINT('Ctrl Pts',(4.31063811976049,-42.6742356128,2.1074981892179));
#72474=CARTESIAN_POINT('Ctrl Pts',(4.47978318815511,-42.6742356128,2.18249743975359));
#72475=CARTESIAN_POINT('Ctrl Pts',(4.65228095758631,-42.6742356128,2.24992450648734));
#72476=CARTESIAN_POINT('Ctrl Pts',(4.82742445854302,-42.6742356128,2.30947944587345));
#72477=CARTESIAN_POINT('Ctrl Pts',(4.86342784939903,-42.6742356128,2.32172186279678));
#72478=CARTESIAN_POINT('Ctrl Pts',(4.8995429390839,-42.6742356128,2.33363177089508));
#72479=CARTESIAN_POINT('Ctrl Pts',(4.9357634328988,-42.6742356128,2.34520678581771));
#72480=CARTESIAN_POINT('Ctrl Pts',(4.9509736781236,-42.6742356128,2.35006753720209));
#72481=CARTESIAN_POINT('Ctrl Pts',(4.96620142604667,-42.6742356128,2.35486889455));
#72482=CARTESIAN_POINT('Ctrl Pts',(4.98144914733,-42.6742356128,2.3596116021));
#72483=CARTESIAN_POINT('',(-0.779760475483967,-42.6742356128,-2.17482015902982));
#72484=CARTESIAN_POINT('Ctrl Pts',(-0.779760436124172,-42.6742356128,-2.1748203306699));
#72485=CARTESIAN_POINT('Ctrl Pts',(-0.771882386024557,-42.6742356128,-2.2091747844539));
#72486=CARTESIAN_POINT('Ctrl Pts',(-0.761743310786152,-42.6742356127436,
-2.24303459797053));
#72487=CARTESIAN_POINT('Ctrl Pts',(-0.749417245972666,-42.6742356121532,
-2.27609427848163));
#72488=CARTESIAN_POINT('Ctrl Pts',(-0.743947277564191,-42.6742356118913,
-2.29076525504441));
#72489=CARTESIAN_POINT('Ctrl Pts',(-0.738047224848478,-42.6742356115623,
-2.30527902661246));
#72490=CARTESIAN_POINT('Ctrl Pts',(-0.731726287300169,-42.6742356113417,
-2.31961063905224));
#72491=CARTESIAN_POINT('Ctrl Pts',(-0.71748704598615,-42.6742356108449,
-2.35189561044918));
#72492=CARTESIAN_POINT('Ctrl Pts',(-0.701108863892468,-42.6742356109896,
-2.38325168854725));
#72493=CARTESIAN_POINT('Ctrl Pts',(-0.682724258933874,-42.6742356115095,
-2.41339155273195));
#72494=CARTESIAN_POINT('Ctrl Pts',(-0.674556959324613,-42.6742356117405,
-2.42678108715671));
#72495=CARTESIAN_POINT('Ctrl Pts',(-0.665994299629919,-42.6742356120229,
-2.43993092853152));
#72496=CARTESIAN_POINT('Ctrl Pts',(-0.657050718113802,-42.6742356122661,
-2.45281754922215));
#72497=CARTESIAN_POINT('Ctrl Pts',(-0.636448244523914,-42.6742356128262,
-2.48250322514104));
#72498=CARTESIAN_POINT('Ctrl Pts',(-0.613815845819897,-42.6742356127802,
-2.5107827227237));
#72499=CARTESIAN_POINT('Ctrl Pts',(-0.589368331375716,-42.6742356127938,
-2.53739155422732));
#72500=CARTESIAN_POINT('Ctrl Pts',(-0.567203612838432,-42.6742356128062,
-2.56151577602625));
#72501=CARTESIAN_POINT('Ctrl Pts',(-0.543547753181066,-42.6742356128,-2.58426707716386));
#72502=CARTESIAN_POINT('Ctrl Pts',(-0.518587085338794,-42.6742356128,-2.60547441341678));
#72503=CARTESIAN_POINT('Ctrl Pts',(-0.4900008751542,-42.6742356128,-2.62976211979596));
#72504=CARTESIAN_POINT('Ctrl Pts',(-0.459703825368212,-42.6742356128016,
-2.6520234184038));
#72505=CARTESIAN_POINT('Ctrl Pts',(-0.428000961425894,-42.6742356127984,
-2.67204333218478));
#72506=CARTESIAN_POINT('Ctrl Pts',(-0.396135658604291,-42.6742356127953,
-2.69216582383898));
#72507=CARTESIAN_POINT('Ctrl Pts',(-0.362850627609383,-42.6742356128003,
-2.71002365359072));
#72508=CARTESIAN_POINT('Ctrl Pts',(-0.328481739610751,-42.6742356126976,
-2.72544414029683));
#72509=CARTESIAN_POINT('Ctrl Pts',(-0.302412698880465,-42.6742356126197,
-2.73714068677917));
#72510=CARTESIAN_POINT('Ctrl Pts',(-0.275720672999424,-42.674235612482,
-2.74743585589414));
#72511=CARTESIAN_POINT('Ctrl Pts',(-0.248559329784468,-42.6742356120918,
-2.75627299220266));
#72512=CARTESIAN_POINT('Ctrl Pts',(-0.213345963022923,-42.6742356115859,
-2.76772991167425));
#72513=CARTESIAN_POINT('Ctrl Pts',(-0.177343992087915,-42.6742356115549,
-2.77674513901392));
#72514=CARTESIAN_POINT('Ctrl Pts',(-0.140897295835687,-42.6742356118431,
-2.7832338109811));
#72515=CARTESIAN_POINT('Ctrl Pts',(-0.105167926379445,-42.6742356121256,
-2.78959477594734));
#72516=CARTESIAN_POINT('Ctrl Pts',(-0.0690116959894625,-42.6742356125303,
-2.79352757273382));
#72517=CARTESIAN_POINT('Ctrl Pts',(-0.0327575959623081,-42.6742356126816,
-2.79500142010586));
#72518=CARTESIAN_POINT('Ctrl Pts',(-0.00125856507985131,-42.674235612813,
-2.79628195841334));
#72519=CARTESIAN_POINT('Ctrl Pts',(0.0303140671195736,-42.6742356128,-2.79570693363651));
#72520=CARTESIAN_POINT('Ctrl Pts',(0.0617459707272592,-42.6742356128,-2.7932881369414));
#72521=CARTESIAN_POINT('Ctrl Pts',(0.0975001652207659,-42.6742356128,-2.79053672460072));
#72522=CARTESIAN_POINT('Ctrl Pts',(0.133074926050902,-42.6742356128188,
-2.78539779724224));
#72523=CARTESIAN_POINT('Ctrl Pts',(0.168152094213755,-42.6742356125744,
-2.77790104853703));
#72524=CARTESIAN_POINT('Ctrl Pts',(0.203937242420985,-42.674235612325,-2.77025298919988));
#72525=CARTESIAN_POINT('Ctrl Pts',(0.239204002026126,-42.6742356117404,
-2.76015111489368));
#72526=CARTESIAN_POINT('Ctrl Pts',(0.273621672102003,-42.6742356113681,
-2.74768128575085));
#72527=CARTESIAN_POINT('Ctrl Pts',(0.303967810871832,-42.6742356110398,
-2.73668660875005));
#72528=CARTESIAN_POINT('Ctrl Pts',(0.333653760938991,-42.6742356110113,
-2.72385202374141));
#72529=CARTESIAN_POINT('Ctrl Pts',(0.362462032603895,-42.6742356115161,
-2.70926867569233));
#72530=CARTESIAN_POINT('Ctrl Pts',(0.395399194544457,-42.6742356120931,
-2.69259519725825));
#72531=CARTESIAN_POINT('Ctrl Pts',(0.427186062002718,-42.6742356125277,
-2.67362882788146));
#72532=CARTESIAN_POINT('Ctrl Pts',(0.457510957670161,-42.6742356126845,
-2.65254442199209));
#72533=CARTESIAN_POINT('Ctrl Pts',(0.483644635797922,-42.6742356128196,
-2.63437410137267));
#72534=CARTESIAN_POINT('Ctrl Pts',(0.508692612723636,-42.6742356128,-2.61463163103994));
#72535=CARTESIAN_POINT('Ctrl Pts',(0.532470455680955,-42.6742356128,-2.59345610321658));
#72536=CARTESIAN_POINT('Ctrl Pts',(0.559653617309548,-42.6742356128,-2.56924794453598));
#72537=CARTESIAN_POINT('Ctrl Pts',(0.585178113150637,-42.674235612815,-2.54316956742759));
#72538=CARTESIAN_POINT('Ctrl Pts',(0.608798795510751,-42.6742356127792,
-2.51546647952722));
#72539=CARTESIAN_POINT('Ctrl Pts',(0.618869569523831,-42.6742356127639,
-2.50365515530484));
#72540=CARTESIAN_POINT('Ctrl Pts',(0.628594706907684,-42.6742356127371,
-2.4915489628781));
#72541=CARTESIAN_POINT('Ctrl Pts',(0.637957296244174,-42.6742356126657,
-2.47916894035594));
#72542=CARTESIAN_POINT('Ctrl Pts',(0.65952394751115,-42.6742356125014,-2.45065165535956));
#72543=CARTESIAN_POINT('Ctrl Pts',(0.679165969277145,-42.6742356121484,
-2.42068246401955));
#72544=CARTESIAN_POINT('Ctrl Pts',(0.696711688177922,-42.6742356119776,
-2.38954124508249));
#72545=CARTESIAN_POINT('Ctrl Pts',(0.704648211534099,-42.6742356119004,
-2.37545501625189));
#72546=CARTESIAN_POINT('Ctrl Pts',(0.712156407805598,-42.6742356118675,
-2.36112935270655));
#72547=CARTESIAN_POINT('Ctrl Pts',(0.719223465086762,-42.6742356119079,
-2.34659188406283));
#72548=CARTESIAN_POINT('Ctrl Pts',(0.734743304322684,-42.6742356119965,
-2.31466640684203));
#72549=CARTESIAN_POINT('Ctrl Pts',(0.748133092456025,-42.6742356124825,
-2.28172010730082));
#72550=CARTESIAN_POINT('Ctrl Pts',(0.759286157002397,-42.6742356126654,
-2.24805003279359));
#72551=CARTESIAN_POINT('Ctrl Pts',(0.764654983546271,-42.6742356127534,
-2.23184204000406));
#72552=CARTESIAN_POINT('Ctrl Pts',(0.76950616314712,-42.6742356127875,-2.21546668989043));
#72553=CARTESIAN_POINT('Ctrl Pts',(0.773831693881399,-42.6742356127965,
-2.19895906143653));
#72554=CARTESIAN_POINT('Ctrl Pts',(0.775495494440411,-42.6742356127999,
-2.19260945877808));
#72555=CARTESIAN_POINT('Ctrl Pts',(0.777081584877396,-42.6742356128,-2.18623986325737));
#72556=CARTESIAN_POINT('Ctrl Pts',(0.77858938947441,-42.6742356128,-2.17985291185987));
#72557=CARTESIAN_POINT('Ctrl Pts',(0.778985012316415,-42.6742356128,-2.17817708206825));
#72558=CARTESIAN_POINT('Ctrl Pts',(0.779375249835899,-42.6742356128,-2.17650001824316));
#72559=CARTESIAN_POINT('Ctrl Pts',(0.77975997749,-42.6742356128,-2.17482231881));
#72560=CARTESIAN_POINT('',(-4.9814499490356,-42.6742356128,2.35961185030861));
#72561=CARTESIAN_POINT('Ctrl Pts',(-4.98144948349564,-42.6742356128,2.35961170550494));
#72562=CARTESIAN_POINT('Ctrl Pts',(-4.80919836505199,-42.6742356128,2.30603390147258));
#72563=CARTESIAN_POINT('Ctrl Pts',(-4.63925280032748,-42.6742356128,2.24489003529727));
#72564=CARTESIAN_POINT('Ctrl Pts',(-4.47229043758232,-42.6742356128,2.17645227217075));
#72565=CARTESIAN_POINT('Ctrl Pts',(-4.30666840647509,-42.6742356128,2.10856391010469));
#72566=CARTESIAN_POINT('Ctrl Pts',(-4.1439818210772,-42.6742356128,2.03349814638391));
#72567=CARTESIAN_POINT('Ctrl Pts',(-3.9848542066517,-42.6742356128,1.95155469208076));
#72568=CARTESIAN_POINT('Ctrl Pts',(-3.82699882905798,-42.6742356128,1.87026638164477));
#72569=CARTESIAN_POINT('Ctrl Pts',(-3.67264569158656,-42.6742356128,1.78220978388477));
#72570=CARTESIAN_POINT('Ctrl Pts',(-3.52236675719064,-42.6742356128,1.68771315474634));
#72571=CARTESIAN_POINT('Ctrl Pts',(-3.37392108171852,-42.6742356128,1.59436929388734));
#72572=CARTESIAN_POINT('Ctrl Pts',(-3.22945074026306,-42.6742356128,1.49474147234454));
#72573=CARTESIAN_POINT('Ctrl Pts',(-3.08947198433951,-42.6742356128,1.38918267495346));
#72574=CARTESIAN_POINT('Ctrl Pts',(-2.95042677891965,-42.6742356128,1.28432787344963));
#72575=CARTESIAN_POINT('Ctrl Pts',(-2.81581340943447,-42.6742356128,1.17362082121951));
#72576=CARTESIAN_POINT('Ctrl Pts',(-2.68610386179253,-42.6742356128,1.05744547667766));
#72577=CARTESIAN_POINT('Ctrl Pts',(-2.55777390003295,-42.6742356128,0.942505768741767));
#72578=CARTESIAN_POINT('Ctrl Pts',(-2.43424394217692,-42.6742356128,0.822213384451512));
#72579=CARTESIAN_POINT('Ctrl Pts',(-2.31593843360122,-42.6742356128,0.696978970869958));
#72580=CARTESIAN_POINT('Ctrl Pts',(-2.21042894038762,-42.6742356128,0.585290008378093));
#72581=CARTESIAN_POINT('Ctrl Pts',(-2.10907441450449,-42.6742356128,0.469670718927621));
#72582=CARTESIAN_POINT('Ctrl Pts',(-2.01215415618858,-42.6742356128,0.35043979706303));
#72583=CARTESIAN_POINT('Ctrl Pts',(-1.9037090267106,-42.6742356128,0.217031023870963));
#72584=CARTESIAN_POINT('Ctrl Pts',(-1.80081569189617,-42.6742356128,0.0790993529284168));
#72585=CARTESIAN_POINT('Ctrl Pts',(-1.70382506592654,-42.6742356128,-0.062882265463112));
#72586=CARTESIAN_POINT('Ctrl Pts',(-1.60543636915258,-42.6742356128,-0.206910477053096));
#72587=CARTESIAN_POINT('Ctrl Pts',(-1.51312175751413,-42.6742356128,-0.355106089171734));
#72588=CARTESIAN_POINT('Ctrl Pts',(-1.42720569724974,-42.6742356128,-0.506941748698572));
#72589=CARTESIAN_POINT('Ctrl Pts',(-1.33928851382052,-42.6742356128,-0.662313904831416));
#72590=CARTESIAN_POINT('Ctrl Pts',(-1.25807145212962,-42.6742356128,-0.821497524831694));
#72591=CARTESIAN_POINT('Ctrl Pts',(-1.18385847761663,-42.6742356128,-0.983894534460413));
#72592=CARTESIAN_POINT('Ctrl Pts',(-1.10857063815684,-42.6742356128,-1.14864362408946));
#72593=CARTESIAN_POINT('Ctrl Pts',(-1.04049120426499,-42.6742356128,-1.31669966268174));
#72594=CARTESIAN_POINT('Ctrl Pts',(-0.979893200082159,-42.6742356128,-1.48740715124177));
#72595=CARTESIAN_POINT('Ctrl Pts',(-0.939948615418486,-42.6742356128,-1.59993296494573));
#72596=CARTESIAN_POINT('Ctrl Pts',(-0.903253871668043,-42.6742356128,-1.71361022529542));
#72597=CARTESIAN_POINT('Ctrl Pts',(-0.869877025508678,-42.6742356128,-1.82824463543011));
#72598=CARTESIAN_POINT('Ctrl Pts',(-0.85185246901731,-42.6742356128,-1.8901508560317));
#72599=CARTESIAN_POINT('Ctrl Pts',(-0.834795388868271,-42.6742356128,-1.95233612918722));
#72600=CARTESIAN_POINT('Ctrl Pts',(-0.81871556018869,-42.6742356128,-2.01476928736231));
#72601=CARTESIAN_POINT('Ctrl Pts',(-0.807621905288932,-42.6742356128,-2.05784262631996));
#72602=CARTESIAN_POINT('Ctrl Pts',(-0.796993187080195,-42.6742356128,-2.10103480337359));
#72603=CARTESIAN_POINT('Ctrl Pts',(-0.786833098471183,-42.6742356128,-2.14433263155088));
#72604=CARTESIAN_POINT('Ctrl Pts',(-0.784449857609889,-42.6742356128,-2.15448895570202));
#72605=CARTESIAN_POINT('Ctrl Pts',(-0.78209237975105,-42.6742356128,-2.16465117321392));
#72606=CARTESIAN_POINT('Ctrl Pts',(-0.779760514736,-42.6742356128,-2.17481998786));
#72607=CARTESIAN_POINT('',(-5.54384247076,-42.6742356128,3.12351150632));
#72608=CARTESIAN_POINT('Ctrl Pts',(-5.54384247076,-42.6742356128,3.12351150632));
#72609=CARTESIAN_POINT('Ctrl Pts',(-5.54384247076,-42.6742356128,3.08277773492765));
#72610=CARTESIAN_POINT('Ctrl Pts',(-5.54071360078215,-42.6742356128,3.04207318197935));
#72611=CARTESIAN_POINT('Ctrl Pts',(-5.53451433673871,-42.6742356128,3.00184928981549));
#72612=CARTESIAN_POINT('Ctrl Pts',(-5.52845684412169,-42.6742356128,2.96254528080684));
#72613=CARTESIAN_POINT('Ctrl Pts',(-5.51946761052196,-42.6742356128,2.92370108139371));
#72614=CARTESIAN_POINT('Ctrl Pts',(-5.50764984198096,-42.6742356128,2.88573839093141));
#72615=CARTESIAN_POINT('Ctrl Pts',(-5.49633599201714,-42.6742356128,2.84939445826564));
#72616=CARTESIAN_POINT('Ctrl Pts',(-5.48242970534344,-42.6742356128,2.81385906698573));
#72617=CARTESIAN_POINT('Ctrl Pts',(-5.46606736204047,-42.6742356128,2.77949183965844));
#72618=CARTESIAN_POINT('Ctrl Pts',(-5.45540608526423,-42.6742356128,2.75709904934816));
#72619=CARTESIAN_POINT('Ctrl Pts',(-5.44370303413002,-42.6742356128,2.73520201301567));
#72620=CARTESIAN_POINT('Ctrl Pts',(-5.43100715596564,-42.6742356128,2.71389584592905));
#72621=CARTESIAN_POINT('Ctrl Pts',(-5.41253132965188,-42.6742356128,2.68288979519291));
#72622=CARTESIAN_POINT('Ctrl Pts',(-5.39195153436773,-42.6742356128,2.65313745264134));
#72623=CARTESIAN_POINT('Ctrl Pts',(-5.36945481472739,-42.6742356128,2.62491223520097));
#72624=CARTESIAN_POINT('Ctrl Pts',(-5.36214844037038,-42.6742356128,2.61574538740164));
#72625=CARTESIAN_POINT('Ctrl Pts',(-5.3546402157141,-42.6742356128,2.60673941007348));
#72626=CARTESIAN_POINT('Ctrl Pts',(-5.34693756224094,-42.6742356128,2.59790301992746));
#72627=CARTESIAN_POINT('Ctrl Pts',(-5.32245762826908,-42.6742356128,2.56981993815857));
#72628=CARTESIAN_POINT('Ctrl Pts',(-5.29601080618723,-42.6742356128,2.54345222915515));
#72629=CARTESIAN_POINT('Ctrl Pts',(-5.26786034544883,-42.6742356127988,
2.519055298754));
#72630=CARTESIAN_POINT('Ctrl Pts',(-5.23866597118581,-42.6742356127975,
2.49375364832564));
#72631=CARTESIAN_POINT('Ctrl Pts',(-5.20763878578798,-42.674235612795,2.47057122522464));
#72632=CARTESIAN_POINT('Ctrl Pts',(-5.17509880313699,-42.6742356127955,
2.44974305729505));
#72633=CARTESIAN_POINT('Ctrl Pts',(-5.15847322776628,-42.6742356127958,
2.43910137135866));
#72634=CARTESIAN_POINT('Ctrl Pts',(-5.14145320351809,-42.674235612797,2.42907350989681));
#72635=CARTESIAN_POINT('Ctrl Pts',(-5.1240845467918,-42.6742356127983,2.41968668236892));
#72636=CARTESIAN_POINT('Ctrl Pts',(-5.08693883187455,-42.6742356128011,
2.39961141547735));
#72637=CARTESIAN_POINT('Ctrl Pts',(-5.04819985954546,-42.6742356128,2.38247336856776));
#72638=CARTESIAN_POINT('Ctrl Pts',(-5.00832557034011,-42.6742356128,2.36849837699853));
#72639=CARTESIAN_POINT('Ctrl Pts',(-5.00019121922974,-42.6742356128,2.36564748008089));
#72640=CARTESIAN_POINT('Ctrl Pts',(-4.99200978031334,-42.6742356128,2.36292815045189));
#72641=CARTESIAN_POINT('Ctrl Pts',(-4.98378540040244,-42.6742356128,2.36034222294903));
#72642=CARTESIAN_POINT('Ctrl Pts',(-4.98300737166342,-42.6742356128,2.36009759345282));
#72643=CARTESIAN_POINT('Ctrl Pts',(-4.98222894973333,-42.6742356128,2.35985415528));
#72644=CARTESIAN_POINT('Ctrl Pts',(-4.98145041415,-42.6742356128,2.35961199498));
#72645=CARTESIAN_POINT('',(-5.54384247374,-42.6742356128,6.92092019865));
#72646=CARTESIAN_POINT('',(-5.54384247076,-42.6742356128,1.77756718468));
#72647=CARTESIAN_POINT('',(1.46955156614709E-7,-42.6742356128,12.4643460018));
#72648=CARTESIAN_POINT('Ctrl Pts',(2.6645352591E-15,-42.6742356128,12.4643460018));
#72649=CARTESIAN_POINT('Ctrl Pts',(-0.152934422951822,-42.6742356128,12.4643459942906));
#72650=CARTESIAN_POINT('Ctrl Pts',(-0.305879899778285,-42.6742356128,12.4580345127897));
#72651=CARTESIAN_POINT('Ctrl Pts',(-0.458305068588312,-42.6742356128,12.4454167663129));
#72652=CARTESIAN_POINT('Ctrl Pts',(-0.612162616952914,-42.6742356128,12.4326804475411));
#72653=CARTESIAN_POINT('Ctrl Pts',(-0.765489828123542,-42.6742356128,12.4135188817167));
#72654=CARTESIAN_POINT('Ctrl Pts',(-0.917747353463392,-42.6742356128,12.3879900366151));
#72655=CARTESIAN_POINT('Ctrl Pts',(-1.07200490475462,-42.6742356128,12.3621258494502));
#72656=CARTESIAN_POINT('Ctrl Pts',(-1.22516425528739,-42.6742356128,12.3297260830963));
#72657=CARTESIAN_POINT('Ctrl Pts',(-1.37667510471216,-42.6742356128,12.2909034822149));
#72658=CARTESIAN_POINT('Ctrl Pts',(-1.52925372735887,-42.6742356128,12.2518072789229));
#72659=CARTESIAN_POINT('Ctrl Pts',(-1.68016030056891,-42.6742356128,12.2061975321192));
#72660=CARTESIAN_POINT('Ctrl Pts',(-1.82884693378749,-42.6742356128,12.15424051866));
#72661=CARTESIAN_POINT('Ctrl Pts',(-1.97886109712591,-42.6742356128,12.1018196134655));
#72662=CARTESIAN_POINT('Ctrl Pts',(-2.12661525264074,-42.6742356128,12.0429377287266));
#72663=CARTESIAN_POINT('Ctrl Pts',(-2.27156468105575,-42.6742356128,11.9778154451136));
#72664=CARTESIAN_POINT('Ctrl Pts',(-2.30699184911197,-42.6742356128,11.9618988726166));
#72665=CARTESIAN_POINT('Ctrl Pts',(-2.34225156607063,-42.6742356128,11.9456097462612));
#72666=CARTESIAN_POINT('Ctrl Pts',(-2.37733606672488,-42.6742356128,11.9289517189297));
#72667=CARTESIAN_POINT('Ctrl Pts',(-2.52218856563558,-42.6742356128,11.8601761388049));
#72668=CARTESIAN_POINT('Ctrl Pts',(-2.66405185080705,-42.6742356128,11.7851089263726));
#72669=CARTESIAN_POINT('Ctrl Pts',(-2.8023946521394,-42.6742356128,11.7040363137361));
#72670=CARTESIAN_POINT('Ctrl Pts',(-2.94501320772194,-42.6742356128,11.6204579937933));
#72671=CARTESIAN_POINT('Ctrl Pts',(-3.08388989194594,-42.6742356128,11.5304973181011));
#72672=CARTESIAN_POINT('Ctrl Pts',(-3.21847226185907,-42.6742356128,11.4345172231166));
#72673=CARTESIAN_POINT('Ctrl Pts',(-3.3499760674468,-42.6742356128,11.3407326675371));
#72674=CARTESIAN_POINT('Ctrl Pts',(-3.47737964611668,-42.6742356128,11.2412013333675));
#72675=CARTESIAN_POINT('Ctrl Pts',(-3.60019907306528,-42.6742356128,11.1363045235771));
#72676=CARTESIAN_POINT('Ctrl Pts',(-3.7273313885791,-42.6742356128,11.0277241902375));
#72677=CARTESIAN_POINT('Ctrl Pts',(-3.84955145038418,-42.6742356128,10.9133949502508));
#72678=CARTESIAN_POINT('Ctrl Pts',(-3.96636185003895,-42.6742356128,10.7937834186627));
#72679=CARTESIAN_POINT('Ctrl Pts',(-4.08317224969372,-42.6742356128,10.6741718870745));
#72680=CARTESIAN_POINT('Ctrl Pts',(-4.19457269676896,-42.6742356128,10.5492783343306));
#72681=CARTESIAN_POINT('Ctrl Pts',(-4.30011007911526,-42.6742356128,10.4196098288233));
#72682=CARTESIAN_POINT('Ctrl Pts',(-4.40180740998025,-42.6742356128,10.2946594025935));
#72683=CARTESIAN_POINT('Ctrl Pts',(-4.49805952609308,-42.6742356128,10.1652770827442));
#72684=CARTESIAN_POINT('Ctrl Pts',(-4.58849736625876,-42.6742356128,10.031953943456));
#72685=CARTESIAN_POINT('Ctrl Pts',(-4.67853934273498,-42.6742356128,9.89921438499756));
#72686=CARTESIAN_POINT('Ctrl Pts',(-4.76281768342982,-42.6742356128,9.76256862347885));
#72687=CARTESIAN_POINT('Ctrl Pts',(-4.84101173146805,-42.6742356128,9.62252848262185));
#72688=CARTESIAN_POINT('Ctrl Pts',(-4.9188015286105,-42.6742356128,9.48321232720629));
#72689=CARTESIAN_POINT('Ctrl Pts',(-4.9905696427724,-42.6742356128,9.34053698753787));
#72690=CARTESIAN_POINT('Ctrl Pts',(-5.05604571341481,-42.6742356128,9.19503049048107));
#72691=CARTESIAN_POINT('Ctrl Pts',(-5.12113898989817,-42.6742356128,9.05037467118533));
#72692=CARTESIAN_POINT('Ctrl Pts',(-5.18001345232591,-42.6742356128,8.90292088539472));
#72693=CARTESIAN_POINT('Ctrl Pts',(-5.23245034475332,-42.6742356128,8.75320905292079));
#72694=CARTESIAN_POINT('Ctrl Pts',(-5.28435356154415,-42.6742356128,8.60502091023473));
#72695=CARTESIAN_POINT('Ctrl Pts',(-5.32994949468892,-42.6742356128,8.4546206362449));
#72696=CARTESIAN_POINT('Ctrl Pts',(-5.3690735764806,-42.6742356128,8.30254979313354));
#72697=CARTESIAN_POINT('Ctrl Pts',(-5.4079616738089,-42.6742356128,8.15139619471301));
#72698=CARTESIAN_POINT('Ctrl Pts',(-5.440455646721,-42.6742356128,7.99859228485633));
#72699=CARTESIAN_POINT('Ctrl Pts',(-5.46644261980943,-42.6742356128,7.8446851206844));
#72700=CARTESIAN_POINT('Ctrl Pts',(-5.49215843779819,-42.6742356128,7.69238386545387));
#72701=CARTESIAN_POINT('Ctrl Pts',(-5.5115022728444,-42.6742356128,7.53900242459925));
#72702=CARTESIAN_POINT('Ctrl Pts',(-5.52441386329599,-42.6742356128,7.3850834002636));
#72703=CARTESIAN_POINT('Ctrl Pts',(-5.53701510708161,-42.6742356128,7.23486401744098));
#72704=CARTESIAN_POINT('Ctrl Pts',(-5.54348965896334,-42.6742356128,7.0841327522232));
#72705=CARTESIAN_POINT('Ctrl Pts',(-5.54382843698574,-42.6742356128,6.93340348714827));
#72706=CARTESIAN_POINT('Ctrl Pts',(-5.54383778962934,-42.6742356128,6.92924230489017));
#72707=CARTESIAN_POINT('Ctrl Pts',(-5.54384246875505,-42.6742356128,6.92508112888333));
#72708=CARTESIAN_POINT('Ctrl Pts',(-5.54384247523,-42.6742356128,6.92092019865));
#72709=CARTESIAN_POINT('Ctrl Pts',(5.54384244762,-42.6742356128,6.92091963994));
#72710=CARTESIAN_POINT('Ctrl Pts',(5.54384243194334,-42.6742356128,6.92966373948699));
#72711=CARTESIAN_POINT('Ctrl Pts',(5.54382181063784,-42.6742356128,6.93840868167453));
#72712=CARTESIAN_POINT('Ctrl Pts',(5.5437805349069,-42.6742356128,6.94715314260851));
#72713=CARTESIAN_POINT('Ctrl Pts',(5.54305520621443,-42.6742356128,7.10081749384282));
#72714=CARTESIAN_POINT('Ctrl Pts',(5.53595215261845,-42.6742356128,7.25446554541178));
#72715=CARTESIAN_POINT('Ctrl Pts',(5.52248273569997,-42.6742356128,7.40755466122751));
#72716=CARTESIAN_POINT('Ctrl Pts',(5.50836100597807,-42.6742356128,7.56805775724128));
#72717=CARTESIAN_POINT('Ctrl Pts',(5.48724107786514,-42.6742356128,7.72794619824574));
#72718=CARTESIAN_POINT('Ctrl Pts',(5.45919555961385,-42.6742356128,7.88660567787795));
#72719=CARTESIAN_POINT('Ctrl Pts',(5.43185920864886,-42.6742356128,8.04125324688654));
#72720=CARTESIAN_POINT('Ctrl Pts',(5.39794349973922,-42.6742356128,8.19473309461251));
#72721=CARTESIAN_POINT('Ctrl Pts',(5.35756863797163,-42.6742356128,8.34648936004158));
#72722=CARTESIAN_POINT('Ctrl Pts',(5.31689946083409,-42.6742356128,8.49935186334855));
#72723=CARTESIAN_POINT('Ctrl Pts',(5.26967674106624,-42.6742356128,8.65046536546907));
#72724=CARTESIAN_POINT('Ctrl Pts',(5.21607418264677,-42.6742356128,8.79927766128295));
#72725=CARTESIAN_POINT('Ctrl Pts',(5.16211508332785,-42.6742356128,8.94907979174951));
#72726=CARTESIAN_POINT('Ctrl Pts',(5.10169112673359,-42.6742356128,9.0965497937351));
#72727=CARTESIAN_POINT('Ctrl Pts',(5.03502889143353,-42.6742356128,9.24114349268404));
#72728=CARTESIAN_POINT('Ctrl Pts',(4.9666514619051,-42.6742356128,9.3894575330944));
#72729=CARTESIAN_POINT('Ctrl Pts',(4.89171060292642,-42.6742356128,9.53474504778954));
#72730=CARTESIAN_POINT('Ctrl Pts',(4.81050183666432,-42.6742356128,9.67644283944644));
#72731=CARTESIAN_POINT('Ctrl Pts',(4.7303262629303,-42.6742356128,9.8163378565222));
#72732=CARTESIAN_POINT('Ctrl Pts',(4.64404156366582,-42.6742356128,9.9527337636317));
#72733=CARTESIAN_POINT('Ctrl Pts',(4.55197842717089,-42.6742356128,10.0851149237367));
#72734=CARTESIAN_POINT('Ctrl Pts',(4.45813571604418,-42.6742356128,10.2200550033312));
#72735=CARTESIAN_POINT('Ctrl Pts',(4.35828908770674,-42.6742356128,10.3508233132124));
#72736=CARTESIAN_POINT('Ctrl Pts',(4.25283467714301,-42.6742356128,10.4769049601158));
#72737=CARTESIAN_POINT('Ctrl Pts',(4.14738026657929,-42.6742356128,10.6029866070193));
#72738=CARTESIAN_POINT('Ctrl Pts',(4.03631829777995,-42.6742356128,10.7243813702904));
#72739=CARTESIAN_POINT('Ctrl Pts',(3.92008790027254,-42.6742356128,10.8406091727226));
#72740=CARTESIAN_POINT('Ctrl Pts',(3.80548814794816,-42.6742356128,10.9552063663791));
#72741=CARTESIAN_POINT('Ctrl Pts',(3.68586534857264,-42.6742356128,11.0647793545833));
#72742=CARTESIAN_POINT('Ctrl Pts',(3.56167933530323,-42.6742356128,11.1689068773146));
#72743=CARTESIAN_POINT('Ctrl Pts',(3.4379919014801,-42.6742356128,11.2726163510141));
#72744=CARTESIAN_POINT('Ctrl Pts',(3.309778046148,-42.6742356128,11.3709238168171));
#72745=CARTESIAN_POINT('Ctrl Pts',(3.17752456376651,-42.6742356128,11.4634531338962));
#72746=CARTESIAN_POINT('Ctrl Pts',(3.04581089145029,-42.6742356128,11.5556047803401));
#72747=CARTESIAN_POINT('Ctrl Pts',(2.91009072040676,-42.6742356128,11.6420251771074));
#72748=CARTESIAN_POINT('Ctrl Pts',(2.77087386987523,-42.6742356128,11.7223852197934));
#72749=CARTESIAN_POINT('Ctrl Pts',(2.63237555232269,-42.6742356128,11.8023305042037));
#72750=CARTESIAN_POINT('Ctrl Pts',(2.49041677304819,-42.6742356128,11.8762776720779));
#72751=CARTESIAN_POINT('Ctrl Pts',(2.34552496533561,-42.6742356128,11.9439472520736));
#72752=CARTESIAN_POINT('Ctrl Pts',(2.20151495801616,-42.6742356128,12.0112050002121));
#72753=CARTESIAN_POINT('Ctrl Pts',(2.05460772523369,-42.6742356128,12.0722611930782));
#72754=CARTESIAN_POINT('Ctrl Pts',(1.90534316243217,-42.6742356128,12.1268878184385));
#72755=CARTESIAN_POINT('Ctrl Pts',(1.75315419905355,-42.6742356128,12.1825846920327));
#72756=CARTESIAN_POINT('Ctrl Pts',(1.59851476541057,-42.6742356128,12.2315972208754));
#72757=CARTESIAN_POINT('Ctrl Pts',(1.4420176011676,-42.6742356128,12.273736305035));
#72758=CARTESIAN_POINT('Ctrl Pts',(1.29127071052453,-42.6742356128,12.3143270463583));
#72759=CARTESIAN_POINT('Ctrl Pts',(1.1388003798863,-42.6742356128,12.3485403027653));
#72760=CARTESIAN_POINT('Ctrl Pts',(0.985151863989862,-42.6742356128,12.3762563568521));
#72761=CARTESIAN_POINT('Ctrl Pts',(0.832564790435014,-42.6742356128,12.4037809415116));
#72762=CARTESIAN_POINT('Ctrl Pts',(0.678815934744325,-42.6742356128,12.4248976698191));
#72763=CARTESIAN_POINT('Ctrl Pts',(0.524451633473361,-42.6742356128,12.4395390775479));
#72764=CARTESIAN_POINT('Ctrl Pts',(0.43730184594899,-42.6742356128,12.4478052087849));
#72765=CARTESIAN_POINT('Ctrl Pts',(0.349956098267065,-42.6742356128,12.454008297127));
#72766=CARTESIAN_POINT('Ctrl Pts',(0.262514127733032,-42.6742356128,12.4581434972064));
#72767=CARTESIAN_POINT('Ctrl Pts',(0.212960826973561,-42.6742356128,12.4604869120676));
#72768=CARTESIAN_POINT('Ctrl Pts',(0.163376641704469,-42.6742356128,12.4621663256812));
#72769=CARTESIAN_POINT('Ctrl Pts',(0.113779847635199,-42.6742356128,12.4631816295884));
#72770=CARTESIAN_POINT('Ctrl Pts',(0.0806814244047195,-42.6742356128,12.4638591927063));
#72771=CARTESIAN_POINT('Ctrl Pts',(0.047577387565802,-42.6742356128,12.4642410020864));
#72772=CARTESIAN_POINT('Ctrl Pts',(0.0144731887327847,-42.6742356128,12.4643271664958));
#72773=CARTESIAN_POINT('Ctrl Pts',(0.0096488453239203,-42.6742356128,12.4643397234135));
#72774=CARTESIAN_POINT('Ctrl Pts',(0.00482444203328454,-42.6742356128,12.4643460015574));
#72775=CARTESIAN_POINT('Ctrl Pts',(2.93507693704953E-7,-42.6742356128,12.4643460018));
#72776=CARTESIAN_POINT('',(1.02290383517,-42.6742356128,-3.56061176027));
#72777=CARTESIAN_POINT('Origin',(6.82290383517,-42.6742356128,-3.56061176027));
#72778=CARTESIAN_POINT('',(-1.02290383517,-42.6742356128,-3.56061176027));
#72779=CARTESIAN_POINT('Origin',(-6.82290383517,-42.6742356128,-3.56061176027));
#72780=CARTESIAN_POINT('Origin',(-3.35265884719E-30,-40.6742356128,3.15283103411E-22));
#72781=CARTESIAN_POINT('',(6.74948971107,-40.6742356128,2.9389736393));
#72782=CARTESIAN_POINT('',(6.24384247076,-40.6742356128,3.43894174696));
#72783=CARTESIAN_POINT('Ctrl Pts',(6.74948971107,-40.6742356128,2.9389736393));
#72784=CARTESIAN_POINT('Ctrl Pts',(6.59129069763,-40.6742356128,2.93718674963));
#72785=CARTESIAN_POINT('Ctrl Pts',(6.43081292755,-40.6742356128,2.99918925876));
#72786=CARTESIAN_POINT('Ctrl Pts',(6.30765353814,-40.6742356128,3.12096539428));
#72787=CARTESIAN_POINT('Ctrl Pts',(6.24384247076,-40.6742356128,3.28073264221));
#72788=CARTESIAN_POINT('Ctrl Pts',(6.24384247076,-40.6742356128,3.43894174696));
#72789=CARTESIAN_POINT('',(0.4871654368,-40.6742356128,-5.0126513422));
#72790=CARTESIAN_POINT('Ctrl Pts',(0.4871654368,-40.6742356128,-5.0126513422));
#72791=CARTESIAN_POINT('Ctrl Pts',(0.813757598474,-40.6742356128,-6.43768308726));
#72792=CARTESIAN_POINT('Ctrl Pts',(1.54099672242,-40.6742356128,-7.77089360944));
#72793=CARTESIAN_POINT('Ctrl Pts',(2.63582398808,-40.6742356128,-8.86093046307));
#72794=CARTESIAN_POINT('Ctrl Pts',(5.30859738244,-40.6742356128,-10.303702289));
#72795=CARTESIAN_POINT('Ctrl Pts',(8.3416246802,-40.6742356128,-10.1422911046));
#72796=CARTESIAN_POINT('Ctrl Pts',(9.79740146658,-40.6742356128,-9.62504741726));
#72797=CARTESIAN_POINT('Ctrl Pts',(12.2523240225,-40.6742356128,-7.83656666427));
#72798=CARTESIAN_POINT('Ctrl Pts',(13.4155860878,-40.6742356128,-5.03083511496));
#72799=CARTESIAN_POINT('Ctrl Pts',(13.5772083053,-40.6742356128,-3.49437641304));
#72800=CARTESIAN_POINT('Ctrl Pts',(13.0232255151,-40.6742356128,-0.50800550047));
#72801=CARTESIAN_POINT('Ctrl Pts',(10.9941845663,-40.6742356128,1.75214958001));
#72802=CARTESIAN_POINT('Ctrl Pts',(9.67790042305,-40.6742356128,2.56099019349));
#72803=CARTESIAN_POINT('Ctrl Pts',(8.21137385808,-40.6742356128,2.95548591471));
#72804=CARTESIAN_POINT('Ctrl Pts',(6.74948971107,-40.6742356128,2.9389736393));
#72805=CARTESIAN_POINT('',(-6.66133814775E-16,-40.6742356128,-4.62434669465));
#72806=CARTESIAN_POINT('Ctrl Pts',(-6.66133814775E-16,-40.6742356128,-4.62434669465));
#72807=CARTESIAN_POINT('Ctrl Pts',(0.134351406801,-40.6742356128,-4.62434669465));
#72808=CARTESIAN_POINT('Ctrl Pts',(0.269654391195,-40.6742356128,-4.67008903963));
#72809=CARTESIAN_POINT('Ctrl Pts',(0.38229629568,-40.6742356128,-4.75983578098));
#72810=CARTESIAN_POINT('Ctrl Pts',(0.457108114206,-40.6742356128,-4.88150110685));
#72811=CARTESIAN_POINT('Ctrl Pts',(0.4871654368,-40.6742356128,-5.0126513422));
#72812=CARTESIAN_POINT('',(-0.4871654368,-40.6742356128,-5.0126513422));
#72813=CARTESIAN_POINT('Ctrl Pts',(-0.4871654368,-40.6742356128,-5.0126513422));
#72814=CARTESIAN_POINT('Ctrl Pts',(-0.457108114206,-40.6742356128,-4.88150110685));
#72815=CARTESIAN_POINT('Ctrl Pts',(-0.38229629568,-40.6742356128,-4.75983578098));
#72816=CARTESIAN_POINT('Ctrl Pts',(-0.269654391195,-40.6742356128,-4.67008903963));
#72817=CARTESIAN_POINT('Ctrl Pts',(-0.134351406801,-40.6742356128,-4.62434669465));
#72818=CARTESIAN_POINT('Ctrl Pts',(-6.66133814775E-16,-40.6742356128,-4.62434669465));
#72819=CARTESIAN_POINT('',(-6.74948971107,-40.6742356128,2.9389736393));
#72820=CARTESIAN_POINT('Ctrl Pts',(-6.74948971107,-40.6742356128,2.9389736393));
#72821=CARTESIAN_POINT('Ctrl Pts',(-8.21137385808,-40.6742356128,2.95548591471));
#72822=CARTESIAN_POINT('Ctrl Pts',(-9.67790042305,-40.6742356128,2.56099019349));
#72823=CARTESIAN_POINT('Ctrl Pts',(-10.9941845663,-40.6742356128,1.75214958001));
#72824=CARTESIAN_POINT('Ctrl Pts',(-13.0232255151,-40.6742356128,-0.50800550047));
#72825=CARTESIAN_POINT('Ctrl Pts',(-13.5772083053,-40.6742356128,-3.49437641304));
#72826=CARTESIAN_POINT('Ctrl Pts',(-13.4155860878,-40.6742356128,-5.03083511496));
#72827=CARTESIAN_POINT('Ctrl Pts',(-12.2523240225,-40.6742356128,-7.83656666427));
#72828=CARTESIAN_POINT('Ctrl Pts',(-9.79740146658,-40.6742356128,-9.62504741726));
#72829=CARTESIAN_POINT('Ctrl Pts',(-8.3416246802,-40.6742356128,-10.1422911046));
#72830=CARTESIAN_POINT('Ctrl Pts',(-5.30859738244,-40.6742356128,-10.303702289));
#72831=CARTESIAN_POINT('Ctrl Pts',(-2.63582398808,-40.6742356128,-8.86093046307));
#72832=CARTESIAN_POINT('Ctrl Pts',(-1.54099672242,-40.6742356128,-7.77089360944));
#72833=CARTESIAN_POINT('Ctrl Pts',(-0.813757598474,-40.6742356128,-6.43768308726));
#72834=CARTESIAN_POINT('Ctrl Pts',(-0.4871654368,-40.6742356128,-5.0126513422));
#72835=CARTESIAN_POINT('',(-6.24384247076,-40.6742356128,3.43894174696));
#72836=CARTESIAN_POINT('Ctrl Pts',(-6.24384247076,-40.6742356128,3.43894174696));
#72837=CARTESIAN_POINT('Ctrl Pts',(-6.24384247076,-40.6742356128,3.28073264221));
#72838=CARTESIAN_POINT('Ctrl Pts',(-6.30765353814,-40.6742356128,3.12096539428));
#72839=CARTESIAN_POINT('Ctrl Pts',(-6.43081292755,-40.6742356128,2.99918925876));
#72840=CARTESIAN_POINT('Ctrl Pts',(-6.59129069763,-40.6742356128,2.93718674963));
#72841=CARTESIAN_POINT('Ctrl Pts',(-6.74948971107,-40.6742356128,2.9389736393));
#72842=CARTESIAN_POINT('',(-6.24384247076,-40.6742356128,6.92091963994));
#72843=CARTESIAN_POINT('',(-6.24384247076,-40.6742356128,5.17993069345));
#72844=CARTESIAN_POINT('',(3.5527136788E-15,-40.6742356128,13.1643460036));
#72845=CARTESIAN_POINT('Ctrl Pts',(3.5527136788E-15,-40.6742356128,13.1643460036));
#72846=CARTESIAN_POINT('Ctrl Pts',(-1.96184634686,-40.6742356128,13.1643460036));
#72847=CARTESIAN_POINT('Ctrl Pts',(-3.92510661379,-40.6742356128,12.3963108842));
#72848=CARTESIAN_POINT('Ctrl Pts',(-5.47580735138,-40.6742356128,10.8456101466));
#72849=CARTESIAN_POINT('Ctrl Pts',(-6.24384247076,-40.6742356128,8.88234987966));
#72850=CARTESIAN_POINT('Ctrl Pts',(-6.24384247076,-40.6742356128,6.92091963994));
#72851=CARTESIAN_POINT('',(6.24384247076,-40.6742356128,6.92091963994));
#72852=CARTESIAN_POINT('Ctrl Pts',(6.24384247076,-40.6742356128,6.92091963994));
#72853=CARTESIAN_POINT('Ctrl Pts',(6.24384247076,-40.6742356128,8.88234987966));
#72854=CARTESIAN_POINT('Ctrl Pts',(5.47580735138,-40.6742356128,10.8456101466));
#72855=CARTESIAN_POINT('Ctrl Pts',(3.92510661379,-40.6742356128,12.3963108842));
#72856=CARTESIAN_POINT('Ctrl Pts',(1.96184634686,-40.6742356128,13.1643460036));
#72857=CARTESIAN_POINT('Ctrl Pts',(3.5527136788E-15,-40.6742356128,13.1643460036));
#72858=CARTESIAN_POINT('',(6.24384247076,-40.6742356128,5.17993069345));
#72859=CARTESIAN_POINT('',(-1.32290383517,-40.6742356128,-3.56061176027));
#72860=CARTESIAN_POINT('Origin',(-6.82290383517,-40.6742356128,-3.56061176027));
#72861=CARTESIAN_POINT('',(1.32290383517,-40.6742356128,-3.56061176027));
#72862=CARTESIAN_POINT('Origin',(6.82290383517,-40.6742356128,-3.56061176027));
#72863=CARTESIAN_POINT('',(4.89234685393,-40.6742356128,2.64607413014));
#72864=CARTESIAN_POINT('',(5.24384247076,-40.6742356128,3.12351150632));
#72865=CARTESIAN_POINT('Ctrl Pts',(4.89234685393,-40.6742356128,2.64607413014));
#72866=CARTESIAN_POINT('Ctrl Pts',(5.01354316676,-40.6742356128,2.6837716054));
#72867=CARTESIAN_POINT('Ctrl Pts',(5.12322496214,-40.6742356128,2.76042445737));
#72868=CARTESIAN_POINT('Ctrl Pts',(5.20322505246,-40.6742356128,2.86908878029));
#72869=CARTESIAN_POINT('Ctrl Pts',(5.24384247076,-40.6742356128,2.9965877265));
#72870=CARTESIAN_POINT('Ctrl Pts',(5.24384247076,-40.6742356128,3.12351150632));
#72871=CARTESIAN_POINT('',(5.24384247076,-40.6742356128,6.92091963994));
#72872=CARTESIAN_POINT('',(5.24384247076,-40.6742356128,5.02221557313));
#72873=CARTESIAN_POINT('',(3.10862446895E-15,-40.6742356128,12.1643460036));
#72874=CARTESIAN_POINT('Ctrl Pts',(5.24384247076,-40.6742356128,6.92091963994));
#72875=CARTESIAN_POINT('Ctrl Pts',(5.24384247076,-40.6742356128,8.5681906143));
#72876=CARTESIAN_POINT('Ctrl Pts',(4.59882235543,-40.6742356128,10.2169985032));
#72877=CARTESIAN_POINT('Ctrl Pts',(3.29649497043,-40.6742356128,11.5193258882));
#72878=CARTESIAN_POINT('Ctrl Pts',(1.64768708151,-40.6742356128,12.1643460036));
#72879=CARTESIAN_POINT('Ctrl Pts',(3.10862446895E-15,-40.6742356128,12.1643460036));
#72880=CARTESIAN_POINT('',(-5.24384247076,-40.6742356128,6.92091963994));
#72881=CARTESIAN_POINT('Ctrl Pts',(3.10862446895E-15,-40.6742356128,12.1643460036));
#72882=CARTESIAN_POINT('Ctrl Pts',(-1.64768708151,-40.6742356128,12.1643460036));
#72883=CARTESIAN_POINT('Ctrl Pts',(-3.29649497043,-40.6742356128,11.5193258882));
#72884=CARTESIAN_POINT('Ctrl Pts',(-4.59882235543,-40.6742356128,10.2169985032));
#72885=CARTESIAN_POINT('Ctrl Pts',(-5.24384247076,-40.6742356128,8.5681906143));
#72886=CARTESIAN_POINT('Ctrl Pts',(-5.24384247076,-40.6742356128,6.92091963994));
#72887=CARTESIAN_POINT('',(-5.24384247076,-40.6742356128,3.12351150632));
#72888=CARTESIAN_POINT('',(-5.24384247076,-40.6742356128,5.02221557313));
#72889=CARTESIAN_POINT('',(-4.89234685393,-40.6742356128,2.64607413014));
#72890=CARTESIAN_POINT('Ctrl Pts',(-5.24384247076,-40.6742356128,3.12351150632));
#72891=CARTESIAN_POINT('Ctrl Pts',(-5.24384247076,-40.6742356128,2.9965877265));
#72892=CARTESIAN_POINT('Ctrl Pts',(-5.20322505246,-40.6742356128,2.86908878029));
#72893=CARTESIAN_POINT('Ctrl Pts',(-5.12322496214,-40.6742356128,2.76042445737));
#72894=CARTESIAN_POINT('Ctrl Pts',(-5.01354316676,-40.6742356128,2.6837716054));
#72895=CARTESIAN_POINT('Ctrl Pts',(-4.89234685393,-40.6742356128,2.64607413014));
#72896=CARTESIAN_POINT('',(-0.48735027394,-40.6742356128,-2.10776590718));
#72897=CARTESIAN_POINT('Ctrl Pts',(-4.89234685393,-40.6742356128,2.64607413014));
#72898=CARTESIAN_POINT('Ctrl Pts',(-3.59661572838,-40.6742356128,2.2430437828));
#72899=CARTESIAN_POINT('Ctrl Pts',(-2.40362850687,-40.6742356128,1.49964984368));
#72900=CARTESIAN_POINT('Ctrl Pts',(-1.44114622406,-40.6742356128,0.46094601538));
#72901=CARTESIAN_POINT('Ctrl Pts',(-0.790651846747,-40.6742356128,-0.785131881257));
#72902=CARTESIAN_POINT('Ctrl Pts',(-0.48735027394,-40.6742356128,-2.10776590718));
#72903=CARTESIAN_POINT('',(0.48735027394,-40.6742356128,-2.10776590718));
#72904=CARTESIAN_POINT('Ctrl Pts',(-0.48735027394,-40.6742356128,-2.10776590718));
#72905=CARTESIAN_POINT('Ctrl Pts',(-0.427207937888,-40.6742356128,-2.37003391761));
#72906=CARTESIAN_POINT('Ctrl Pts',(-0.191539291907,-40.6742356128,-2.59726293898));
#72907=CARTESIAN_POINT('Ctrl Pts',(0.191539291907,-40.6742356128,-2.59726293898));
#72908=CARTESIAN_POINT('Ctrl Pts',(0.427207937888,-40.6742356128,-2.37003391761));
#72909=CARTESIAN_POINT('Ctrl Pts',(0.48735027394,-40.6742356128,-2.10776590718));
#72910=CARTESIAN_POINT('Ctrl Pts',(0.48735027394,-40.6742356128,-2.10776590718));
#72911=CARTESIAN_POINT('Ctrl Pts',(0.790651846747,-40.6742356128,-0.785131881257001));
#72912=CARTESIAN_POINT('Ctrl Pts',(1.44114622406,-40.6742356128,0.46094601538));
#72913=CARTESIAN_POINT('Ctrl Pts',(2.40362850687,-40.6742356128,1.49964984368));
#72914=CARTESIAN_POINT('Ctrl Pts',(3.59661572838,-40.6742356128,2.2430437828));
#72915=CARTESIAN_POINT('Ctrl Pts',(4.89234685393,-40.6742356128,2.64607413014));
#72916=CARTESIAN_POINT('Origin',(-6.82290383517,-42.3742356128,-3.56061176027));
#72917=CARTESIAN_POINT('',(-1.32290383517,-42.3742356128,-3.56061176027));
#72918=CARTESIAN_POINT('Origin',(-6.82290383517,-42.3742356128,-3.56061176027));
#72919=CARTESIAN_POINT('Origin',(-1.02290383517,-42.3742356128,-3.56061176027));
#72920=CARTESIAN_POINT('Origin',(-6.82290383517,-41.6742356128,-3.56061176027));
#72921=CARTESIAN_POINT('',(-1.32290383517,-41.6742356128,-3.56061176027));
#72922=CARTESIAN_POINT('Origin',(6.82290383517,-42.3742356128,-3.56061176027));
#72923=CARTESIAN_POINT('',(1.32290383517,-42.3742356128,-3.56061176027));
#72924=CARTESIAN_POINT('Origin',(6.82290383517,-42.3742356128,-3.56061176027));
#72925=CARTESIAN_POINT('Origin',(1.02290383517,-42.3742356128,-3.56061176027));
#72926=CARTESIAN_POINT('Origin',(6.82290383517,-41.6742356128,-3.56061176027));
#72927=CARTESIAN_POINT('',(1.32290383517,-41.6742356128,-3.56061176027));
#72928=CARTESIAN_POINT('Ctrl Pts',(4.98144948383,-42.6742356128,2.35961170443));
#72929=CARTESIAN_POINT('Ctrl Pts',(4.95345706708,-42.6742356128,2.44960652964));
#72930=CARTESIAN_POINT('Ctrl Pts',(4.92546465033,-42.6372245963,2.53960135485));
#72931=CARTESIAN_POINT('Ctrl Pts',(4.90333945028,-42.5627311721,2.61073324492));
#72932=CARTESIAN_POINT('Ctrl Pts',(4.89234685393,-42.4684833924,2.64607413014));
#72933=CARTESIAN_POINT('Ctrl Pts',(4.89234685393,-42.3742356128,2.64607413014));
#72934=CARTESIAN_POINT('Ctrl Pts',(5.0910703557,-42.6742356128,2.3937086997));
#72935=CARTESIAN_POINT('Ctrl Pts',(5.05009495057,-42.6742356128,2.4796652347));
#72936=CARTESIAN_POINT('Ctrl Pts',(5.00911954543,-42.6372245963,2.56562176971));
#72937=CARTESIAN_POINT('Ctrl Pts',(4.97673259252,-42.5627311721,2.63356179455));
#72938=CARTESIAN_POINT('Ctrl Pts',(4.96064159025,-42.4684833924,2.66731684844));
#72939=CARTESIAN_POINT('Ctrl Pts',(4.96064159025,-42.3742356128,2.66731684844));
#72940=CARTESIAN_POINT('Ctrl Pts',(5.19436346575,-42.6742356128,2.44749827577));
#72941=CARTESIAN_POINT('Ctrl Pts',(5.14132273239,-42.6742356128,2.52714226629));
#72942=CARTESIAN_POINT('Ctrl Pts',(5.08828199902,-42.6372245963,2.60678625681));
#72943=CARTESIAN_POINT('Ctrl Pts',(5.04635861923,-42.5627311721,2.6697368545));
#72944=CARTESIAN_POINT('Ctrl Pts',(5.02552956775,-42.4684833924,2.70101297135));
#72945=CARTESIAN_POINT('Ctrl Pts',(5.02552956775,-42.3742356128,2.70101297135));
#72946=CARTESIAN_POINT('Ctrl Pts',(5.28701136621,-42.6742356128,2.51927061523));
#72947=CARTESIAN_POINT('Ctrl Pts',(5.223039768,-42.6742356128,2.59047432619));
#72948=CARTESIAN_POINT('Ctrl Pts',(5.15906816979,-42.6372245963,2.66167803715));
#72949=CARTESIAN_POINT('Ctrl Pts',(5.10850502722,-42.5627311721,2.7179585308));
#72950=CARTESIAN_POINT('Ctrl Pts',(5.08338344476,-42.4684833924,2.74591906654));
#72951=CARTESIAN_POINT('Ctrl Pts',(5.08338344476,-42.3742356128,2.74591906654));
#72952=CARTESIAN_POINT('Ctrl Pts',(5.42454853942,-42.6742356128,2.67302418893));
#72953=CARTESIAN_POINT('Ctrl Pts',(5.34434320211,-42.6742356128,2.72608989891));
#72954=CARTESIAN_POINT('Ctrl Pts',(5.26413786481,-42.6372245963,2.77915560888));
#72955=CARTESIAN_POINT('Ctrl Pts',(5.20074359189,-42.5627311721,2.82109789633));
#72956=CARTESIAN_POINT('Ctrl Pts',(5.16924702152,-42.4684833924,2.84193758995));
#72957=CARTESIAN_POINT('Ctrl Pts',(5.16924702152,-42.3742356128,2.84193758995));
#72958=CARTESIAN_POINT('Ctrl Pts',(5.50717689409,-42.6742356128,2.86060629363));
#72959=CARTESIAN_POINT('Ctrl Pts',(5.41723711426,-42.6742356128,2.89155356331));
#72960=CARTESIAN_POINT('Ctrl Pts',(5.32729733443,-42.6372245963,2.92250083298));
#72961=CARTESIAN_POINT('Ctrl Pts',(5.25620894302,-42.5627311721,2.9469621888));
#72962=CARTESIAN_POINT('Ctrl Pts',(5.22088968328,-42.4684833924,2.95911451251));
#72963=CARTESIAN_POINT('Ctrl Pts',(5.22088968328,-42.3742356128,2.95911451251));
#72964=CARTESIAN_POINT('Ctrl Pts',(5.53155282798,-42.6742356128,2.94664996334));
#72965=CARTESIAN_POINT('Ctrl Pts',(5.43875945884,-42.6742356128,2.96752341897));
#72966=CARTESIAN_POINT('Ctrl Pts',(5.3459660897,-42.6372245963,2.9883968746));
#72967=CARTESIAN_POINT('Ctrl Pts',(5.27262225435,-42.5627311721,3.0048926648));
#72968=CARTESIAN_POINT('Ctrl Pts',(5.23618236028,-42.4684833924,3.0130922362));
#72969=CARTESIAN_POINT('Ctrl Pts',(5.23618236028,-42.3742356128,3.0130922362));
#72970=CARTESIAN_POINT('Ctrl Pts',(5.54384237615,-42.6742356128,3.03508099123));
#72971=CARTESIAN_POINT('Ctrl Pts',(5.44959461136,-42.6742356128,3.04553329529));
#72972=CARTESIAN_POINT('Ctrl Pts',(5.35534684657,-42.6372245963,3.05598559935));
#72973=CARTESIAN_POINT('Ctrl Pts',(5.28085341767,-42.5627311721,3.06424881978));
#72974=CARTESIAN_POINT('Ctrl Pts',(5.24384242331,-42.4684833924,3.06835170839));
#72975=CARTESIAN_POINT('Ctrl Pts',(5.24384242331,-42.3742356128,3.06835170839));
#72976=CARTESIAN_POINT('Ctrl Pts',(5.54384246963,-42.6742356128,3.12351053169));
#72977=CARTESIAN_POINT('Ctrl Pts',(5.44959469032,-42.6742356128,3.12351083782));
#72978=CARTESIAN_POINT('Ctrl Pts',(5.35534691101,-42.6372245963,3.12351114396));
#72979=CARTESIAN_POINT('Ctrl Pts',(5.28085348696,-42.5627311721,3.12351138593));
#72980=CARTESIAN_POINT('Ctrl Pts',(5.24384247058,-42.4684833924,3.12351150615));
#72981=CARTESIAN_POINT('Ctrl Pts',(5.24384247058,-42.3742356128,3.12351150615));
#72982=CARTESIAN_POINT('',(4.89234685374928,-42.3742356128,2.646074130721));
#72983=CARTESIAN_POINT('Origin',(4.980818894668,-42.3763569082249,2.36163710735502));
#72984=CARTESIAN_POINT('',(5.24384247076,-42.3742356128,3.12351150632));
#72985=CARTESIAN_POINT('Origin',(5.5417211288869,-42.3763569535561,3.1235105385842));
#72986=CARTESIAN_POINT('Ctrl Pts',(4.89234685393,-42.3742356128,2.64607413014));
#72987=CARTESIAN_POINT('Ctrl Pts',(5.01354316676,-42.3742356128,2.6837716054));
#72988=CARTESIAN_POINT('Ctrl Pts',(5.12322496214,-42.3742356128,2.76042445737));
#72989=CARTESIAN_POINT('Ctrl Pts',(5.20322505246,-42.3742356128,2.86908878029));
#72990=CARTESIAN_POINT('Ctrl Pts',(5.24384247076,-42.3742356128,2.9965877265));
#72991=CARTESIAN_POINT('Ctrl Pts',(5.24384247076,-42.3742356128,3.12351150632));
#72992=CARTESIAN_POINT('Ctrl Pts',(4.89234685393,-40.6742356128,2.64607413014));
#72993=CARTESIAN_POINT('Ctrl Pts',(4.89234685393,-42.7142356128,2.64607413014));
#72994=CARTESIAN_POINT('Ctrl Pts',(5.01354316676,-40.6742356128,2.6837716054));
#72995=CARTESIAN_POINT('Ctrl Pts',(5.01354316676,-42.7142356128,2.6837716054));
#72996=CARTESIAN_POINT('Ctrl Pts',(5.12322496214,-40.6742356128,2.76042445737));
#72997=CARTESIAN_POINT('Ctrl Pts',(5.12322496214,-42.7142356128,2.76042445737));
#72998=CARTESIAN_POINT('Ctrl Pts',(5.20322505246,-40.6742356128,2.86908878029));
#72999=CARTESIAN_POINT('Ctrl Pts',(5.20322505246,-42.7142356128,2.86908878029));
#73000=CARTESIAN_POINT('Ctrl Pts',(5.24384247076,-40.6742356128,2.9965877265));
#73001=CARTESIAN_POINT('Ctrl Pts',(5.24384247076,-42.7142356128,2.9965877265));
#73002=CARTESIAN_POINT('Ctrl Pts',(5.24384247076,-40.6742356128,3.12351150632));
#73003=CARTESIAN_POINT('Ctrl Pts',(5.24384247076,-42.7142356128,3.12351150632));
#73004=CARTESIAN_POINT('',(5.24384247076,-41.5242356128,3.12351150632));
#73005=CARTESIAN_POINT('',(4.89234685393,-41.6742356128,2.64607413014));
#73006=CARTESIAN_POINT('Origin',(5.54384247076,-42.3742356128,1.77756718468));
#73007=CARTESIAN_POINT('',(5.24384247076,-42.3742356128,6.92091964038719));
#73008=CARTESIAN_POINT('Origin',(5.54384247076,-42.3742356128,6.92091963994));
#73009=CARTESIAN_POINT('',(5.24384247076,-42.3742356128,5.02221557313));
#73010=CARTESIAN_POINT('Origin',(5.24384247076,-40.6742356128,3.12351150632));
#73011=CARTESIAN_POINT('',(5.24384247076,-41.6742356128,6.92091963994));
#73012=CARTESIAN_POINT('Ctrl Pts',(5.54384244762,-42.6742356128,6.92091961486));
#73013=CARTESIAN_POINT('Ctrl Pts',(5.44959466918,-42.6742356128,6.92091962424));
#73014=CARTESIAN_POINT('Ctrl Pts',(5.35534689074,-42.6372245963,6.92091963362));
#73015=CARTESIAN_POINT('Ctrl Pts',(5.28085346739,-42.5627311721,6.92091964103));
#73016=CARTESIAN_POINT('Ctrl Pts',(5.24384245134,-42.4684833924,6.92091964471));
#73017=CARTESIAN_POINT('Ctrl Pts',(5.24384245134,-42.3742356128,6.92091964471));
#73018=CARTESIAN_POINT('Ctrl Pts',(5.54384242174,-42.6742356128,7.79164279162));
#73019=CARTESIAN_POINT('Ctrl Pts',(5.44959464312,-42.6742356128,7.77690267016));
#73020=CARTESIAN_POINT('Ctrl Pts',(5.35534686449,-42.6372245963,7.76216254869));
#73021=CARTESIAN_POINT('Ctrl Pts',(5.28085344062,-42.5627311721,7.75051190074));
#73022=CARTESIAN_POINT('Ctrl Pts',(5.24384242488,-42.4684833924,7.74472352777));
#73023=CARTESIAN_POINT('Ctrl Pts',(5.24384242488,-42.3742356128,7.74472352777));
#73024=CARTESIAN_POINT('Ctrl Pts',(5.37333591464,-42.6742356128,8.66281176035));
#73025=CARTESIAN_POINT('Ctrl Pts',(5.28197913873,-42.6742356128,8.63316176369));
#73026=CARTESIAN_POINT('Ctrl Pts',(5.19062236283,-42.6372245963,8.60351176703));
#73027=CARTESIAN_POINT('Ctrl Pts',(5.11841398777,-42.5627311721,8.580076505));
#73028=CARTESIAN_POINT('Ctrl Pts',(5.08253826524,-42.4684833924,8.56843288973));
#73029=CARTESIAN_POINT('Ctrl Pts',(5.08253826524,-42.3742356128,8.56843288973));
#73030=CARTESIAN_POINT('Ctrl Pts',(5.03080493437,-42.6742356128,9.48834807329));
#73031=CARTESIAN_POINT('Ctrl Pts',(4.94530723737,-42.6742356128,9.44467844814));
#73032=CARTESIAN_POINT('Ctrl Pts',(4.85980954038,-42.6372245963,9.40100882299));
#73033=CARTESIAN_POINT('Ctrl Pts',(4.79223215539,-42.5627311721,9.36649233861));
#73034=CARTESIAN_POINT('Ctrl Pts',(4.75865731238,-42.4684833924,9.34934333918));
#73035=CARTESIAN_POINT('Ctrl Pts',(4.75865731238,-42.3742356128,9.34934333918));
#73036=CARTESIAN_POINT('Ctrl Pts',(4.04085177536,-42.6742356128,10.9614284297));
#73037=CARTESIAN_POINT('Ctrl Pts',(3.9721502684,-42.6742356128,10.8927236182));
#73038=CARTESIAN_POINT('Ctrl Pts',(3.90344876143,-42.6372245963,10.8240188068));
#73039=CARTESIAN_POINT('Ctrl Pts',(3.84914712943,-42.5627311721,10.7697145612));
#73040=CARTESIAN_POINT('Ctrl Pts',(3.82216808673,-42.4684833924,10.7427342225));
#73041=CARTESIAN_POINT('Ctrl Pts',(3.82216808673,-42.3742356128,10.7427342225));
#73042=CARTESIAN_POINT('Ctrl Pts',(2.56772513466,-42.6742356128,11.9513497364));
#73043=CARTESIAN_POINT('Ctrl Pts',(2.5240578489,-42.6742356128,11.8658510287));
#73044=CARTESIAN_POINT('Ctrl Pts',(2.48039056315,-42.6372245963,11.7803523209));
#73045=CARTESIAN_POINT('Ctrl Pts',(2.44587592617,-42.5627311721,11.7127741387));
#73046=CARTESIAN_POINT('Ctrl Pts',(2.42872784707,-42.4684833924,11.6791988971));
#73047=CARTESIAN_POINT('Ctrl Pts',(2.42872784707,-42.3742356128,11.6791988971));
#73048=CARTESIAN_POINT('Ctrl Pts',(1.74211448794,-42.6742356128,12.2938681423));
#73049=CARTESIAN_POINT('Ctrl Pts',(1.71247115576,-42.6742356128,12.2025094799));
#73050=CARTESIAN_POINT('Ctrl Pts',(1.68282782357,-42.6372245963,12.1111508175));
#73051=CARTESIAN_POINT('Ctrl Pts',(1.65939783581,-42.5627311721,12.0389409514));
#73052=CARTESIAN_POINT('Ctrl Pts',(1.647756831,-42.4684833924,12.003064488));
#73053=CARTESIAN_POINT('Ctrl Pts',(1.647756831,-42.3742356128,12.003064488));
#73054=CARTESIAN_POINT('Ctrl Pts',(0.870857634643,-42.6742356128,12.464345958));
#73055=CARTESIAN_POINT('Ctrl Pts',(0.856121049032,-42.6742356128,12.3700981819));
#73056=CARTESIAN_POINT('Ctrl Pts',(0.841384463421,-42.6372245963,12.2758504058));
#73057=CARTESIAN_POINT('Ctrl Pts',(0.829736605758,-42.5627311721,12.2013569839));
#73058=CARTESIAN_POINT('Ctrl Pts',(0.823949625757,-42.4684833924,12.1643459692));
#73059=CARTESIAN_POINT('Ctrl Pts',(0.823949625757,-42.3742356128,12.1643459692));
#73060=CARTESIAN_POINT('Ctrl Pts',(2.93507693705E-7,-42.6742356128,12.4643460018));
#73061=CARTESIAN_POINT('Ctrl Pts',(2.01415953693E-7,-42.6742356128,12.3700982223));
#73062=CARTESIAN_POINT('Ctrl Pts',(1.09324215014E-7,-42.6372245963,12.2758504427));
#73063=CARTESIAN_POINT('Ctrl Pts',(3.65349244191E-8,-42.5627311721,12.2013570185));
#73064=CARTESIAN_POINT('Ctrl Pts',(3.70582231568E-10,-42.4684833924,12.164346002));
#73065=CARTESIAN_POINT('Ctrl Pts',(3.70582675657E-10,-42.3742356128,12.164346002));
#73066=CARTESIAN_POINT('',(9.26471538767733E-11,-42.3742356128,12.1643460032));
#73067=CARTESIAN_POINT('Origin',(4.74561210871912E-7,-42.3763569069502,
12.4622247083968));
#73068=CARTESIAN_POINT('Ctrl Pts',(5.24384247076,-42.3742356128,6.92091963994));
#73069=CARTESIAN_POINT('Ctrl Pts',(5.24384247076,-42.3742356128,8.5681906143));
#73070=CARTESIAN_POINT('Ctrl Pts',(4.59882235543,-42.3742356128,10.2169985032));
#73071=CARTESIAN_POINT('Ctrl Pts',(3.29649497043,-42.3742356128,11.5193258882));
#73072=CARTESIAN_POINT('Ctrl Pts',(1.64768708151,-42.3742356128,12.1643460036));
#73073=CARTESIAN_POINT('Ctrl Pts',(3.10862446895E-15,-42.3742356128,12.1643460036));
#73074=CARTESIAN_POINT('Ctrl Pts',(5.24384247076,-40.6742356128,6.92091963994));
#73075=CARTESIAN_POINT('Ctrl Pts',(5.24384247076,-42.7142356128,6.92091963994));
#73076=CARTESIAN_POINT('Ctrl Pts',(5.24384247076,-40.6742356128,8.5681906143));
#73077=CARTESIAN_POINT('Ctrl Pts',(5.24384247076,-42.7142356128,8.5681906143));
#73078=CARTESIAN_POINT('Ctrl Pts',(4.59882235543,-40.6742356128,10.2169985032));
#73079=CARTESIAN_POINT('Ctrl Pts',(4.59882235543,-42.7142356128,10.2169985032));
#73080=CARTESIAN_POINT('Ctrl Pts',(3.29649497043,-40.6742356128,11.5193258882));
#73081=CARTESIAN_POINT('Ctrl Pts',(3.29649497043,-42.7142356128,11.5193258882));
#73082=CARTESIAN_POINT('Ctrl Pts',(1.64768708151,-40.6742356128,12.1643460036));
#73083=CARTESIAN_POINT('Ctrl Pts',(1.64768708151,-42.7142356128,12.1643460036));
#73084=CARTESIAN_POINT('Ctrl Pts',(1.66533453694E-15,-40.6742356128,12.1643460036));
#73085=CARTESIAN_POINT('Ctrl Pts',(1.66533453694E-15,-42.7142356128,12.1643460036));
#73086=CARTESIAN_POINT('',(1.7763568394E-15,-41.6742356128,12.1643460036));
#73087=CARTESIAN_POINT('Ctrl Pts',(2.6645352591E-15,-42.6742356128,12.4643460036));
#73088=CARTESIAN_POINT('Ctrl Pts',(2.6645352591E-15,-42.6742356128,12.3700982239));
#73089=CARTESIAN_POINT('Ctrl Pts',(3.99680288865E-15,-42.6372245963,12.2758504443));
#73090=CARTESIAN_POINT('Ctrl Pts',(3.99680288865E-15,-42.5627311721,12.2013570201));
#73091=CARTESIAN_POINT('Ctrl Pts',(3.5527136788E-15,-42.4684833924,12.1643460036));
#73092=CARTESIAN_POINT('Ctrl Pts',(3.5527136788E-15,-42.3742356128,12.1643460036));
#73093=CARTESIAN_POINT('Ctrl Pts',(-0.98432408905,-42.6742356128,12.4643460036));
#73094=CARTESIAN_POINT('Ctrl Pts',(-0.967642424377,-42.6742356128,12.3700982239));
#73095=CARTESIAN_POINT('Ctrl Pts',(-0.950960759704,-42.6372245963,12.2758504443));
#73096=CARTESIAN_POINT('Ctrl Pts',(-0.937775575531,-42.5627311721,12.20135702));
#73097=CARTESIAN_POINT('Ctrl Pts',(-0.931224701216,-42.4684833924,12.1643460036));
#73098=CARTESIAN_POINT('Ctrl Pts',(-0.931224701216,-42.3742356128,12.1643460036));
#73099=CARTESIAN_POINT('Ctrl Pts',(-1.96903536838,-42.6742356128,12.2466179469));
#73100=CARTESIAN_POINT('Ctrl Pts',(-1.9355445799,-42.6742356128,12.1560629127));
#73101=CARTESIAN_POINT('Ctrl Pts',(-1.90205379142,-42.6372245963,12.0655078786));
#73102=CARTESIAN_POINT('Ctrl Pts',(-1.87558267973,-42.5627311721,11.9939331994));
#73103=CARTESIAN_POINT('Ctrl Pts',(-1.86243087769,-42.4684833924,11.9583723207));
#73104=CARTESIAN_POINT('Ctrl Pts',(-1.86243087769,-42.3742356128,11.9583723207));
#73105=CARTESIAN_POINT('Ctrl Pts',(-2.88824914665,-42.6742356128,11.8085576616));
#73106=CARTESIAN_POINT('Ctrl Pts',(-2.83912141015,-42.6742356128,11.7255036705));
#73107=CARTESIAN_POINT('Ctrl Pts',(-2.78999367365,-42.6372245963,11.6424496795));
#73108=CARTESIAN_POINT('Ctrl Pts',(-2.75116312141,-42.5627311721,11.5768037983));
#73109=CARTESIAN_POINT('Ctrl Pts',(-2.7318707045,-42.4684833924,11.5441885971));
#73110=CARTESIAN_POINT('Ctrl Pts',(-2.7318707045,-42.3742356128,11.5441885971));
#73111=CARTESIAN_POINT('Ctrl Pts',(-4.2870492691,-42.6742356128,10.7016671976));
#73112=CARTESIAN_POINT('Ctrl Pts',(-4.214184775,-42.6742356128,10.6373567994));
#73113=CARTESIAN_POINT('Ctrl Pts',(-4.14132028091,-42.6372245963,10.5730464011));
#73114=CARTESIAN_POINT('Ctrl Pts',(-4.08372820096,-42.5627311721,10.5222154955));
#73115=CARTESIAN_POINT('Ctrl Pts',(-4.05511438087,-42.4684833924,10.4969608421));
#73116=CARTESIAN_POINT('Ctrl Pts',(-4.05511438087,-42.3742356128,10.4969608421));
#73117=CARTESIAN_POINT('Ctrl Pts',(-5.1560065879,-42.6742356128,9.16334308768));
#73118=CARTESIAN_POINT('Ctrl Pts',(-5.06836283571,-42.6742356128,9.12520886355));
#73119=CARTESIAN_POINT('Ctrl Pts',(-4.98071908353,-42.6372245963,9.08707463943));
#73120=CARTESIAN_POINT('Ctrl Pts',(-4.91144548089,-42.5627311721,9.05693334249));
#73121=CARTESIAN_POINT('Ctrl Pts',(-4.87702786008,-42.4684833924,9.04195808227));
#73122=CARTESIAN_POINT('Ctrl Pts',(-4.87702786008,-42.3742356128,9.04195808227));
#73123=CARTESIAN_POINT('Ctrl Pts',(-5.4148883553,-42.6742356128,8.4357571418));
#73124=CARTESIAN_POINT('Ctrl Pts',(-5.3228269536,-42.6742356128,8.40996790687));
#73125=CARTESIAN_POINT('Ctrl Pts',(-5.2307655519,-42.6372245963,8.38417867195));
#73126=CARTESIAN_POINT('Ctrl Pts',(-5.15800024067,-42.5627311721,8.36379492493));
#73127=CARTESIAN_POINT('Ctrl Pts',(-5.12184781233,-42.4684833924,8.35366745746));
#73128=CARTESIAN_POINT('Ctrl Pts',(-5.12184781233,-42.3742356128,8.35366745746));
#73129=CARTESIAN_POINT('Ctrl Pts',(-5.5438412969,-42.6742356128,7.67813852663));
#73130=CARTESIAN_POINT('Ctrl Pts',(-5.44959357541,-42.6742356128,7.66532863316));
#73131=CARTESIAN_POINT('Ctrl Pts',(-5.35534585392,-42.6372245963,7.65251873968));
#73132=CARTESIAN_POINT('Ctrl Pts',(-5.28085247527,-42.5627311721,7.64239376366));
#73133=CARTESIAN_POINT('Ctrl Pts',(-5.2438414819,-42.4684833924,7.6373633693));
#73134=CARTESIAN_POINT('Ctrl Pts',(-5.2438414819,-42.3742356128,7.6373633693));
#73135=CARTESIAN_POINT('Ctrl Pts',(-5.54384247523,-42.6742356128,6.92092019865));
#73136=CARTESIAN_POINT('Ctrl Pts',(-5.44959469539,-42.6742356128,6.92092002284));
#73137=CARTESIAN_POINT('Ctrl Pts',(-5.35534691555,-42.6372245963,6.92091984703));
#73138=CARTESIAN_POINT('Ctrl Pts',(-5.28085349108,-42.5627311721,6.92091970806));
#73139=CARTESIAN_POINT('Ctrl Pts',(-5.24384247449,-42.4684833924,6.92091963902));
#73140=CARTESIAN_POINT('Ctrl Pts',(-5.24384247449,-42.3742356128,6.92091963902));
#73141=CARTESIAN_POINT('',(-5.243842472625,-42.3742356128,6.92091963994));
#73142=CARTESIAN_POINT('Origin',(-5.54172113446363,-42.3763569535662,6.92092019624449));
#73143=CARTESIAN_POINT('Ctrl Pts',(2.94224766596691E-15,-42.3742356128,
12.1643460036));
#73144=CARTESIAN_POINT('Ctrl Pts',(-0.147449922720393,-42.3742356128,12.1643460036));
#73145=CARTESIAN_POINT('Ctrl Pts',(-0.294900815063498,-42.3742356128,12.1581447470062));
#73146=CARTESIAN_POINT('Ctrl Pts',(-0.441824896475511,-42.3742356128,12.145748963406));
#73147=CARTESIAN_POINT('Ctrl Pts',(-0.590135191421333,-42.3742356128,12.1332362268678));
#73148=CARTESIAN_POINT('Ctrl Pts',(-0.737908469878102,-42.3742356128,12.1144116091439));
#73149=CARTESIAN_POINT('Ctrl Pts',(-0.884608151694916,-42.3742356128,12.0893347773405));
#73150=CARTESIAN_POINT('Ctrl Pts',(-1.03930642893801,-42.3742356128,12.0628906662787));
#73151=CARTESIAN_POINT('Ctrl Pts',(-1.19281049201319,-42.3742356128,12.0294936516789));
#73152=CARTESIAN_POINT('Ctrl Pts',(-1.34450258526901,-42.3742356128,11.9892743993845));
#73153=CARTESIAN_POINT('Ctrl Pts',(-1.49136324514781,-42.3742356128,11.9503361409359));
#73154=CARTESIAN_POINT('Ctrl Pts',(-1.63652535204734,-42.3742356128,11.9050037934466));
#73155=CARTESIAN_POINT('Ctrl Pts',(-1.77944242181759,-42.3742356128,11.8534486481863));
#73156=CARTESIAN_POINT('Ctrl Pts',(-1.92321237006314,-42.3742356128,11.8015858400712));
#73157=CARTESIAN_POINT('Ctrl Pts',(-2.0647101495172,-42.3742356128,11.7434258871945));
#73158=CARTESIAN_POINT('Ctrl Pts',(-2.20339722846304,-42.3742356128,11.6791931653637));
#73159=CARTESIAN_POINT('Ctrl Pts',(-2.34273810420776,-42.3742356128,11.6146576384826));
#73160=CARTESIAN_POINT('Ctrl Pts',(-2.479241454579,-42.3742356128,11.543992114104));
#73161=CARTESIAN_POINT('Ctrl Pts',(-2.61238291383962,-42.3742356128,11.4674721362935));
#73162=CARTESIAN_POINT('Ctrl Pts',(-2.75114825234043,-42.3742356128,11.3877199638153));
#73163=CARTESIAN_POINT('Ctrl Pts',(-2.88626120444508,-42.3742356128,11.3016081914638));
#73164=CARTESIAN_POINT('Ctrl Pts',(-3.01715771894491,-42.3742356128,11.2095008346905));
#73165=CARTESIAN_POINT('Ctrl Pts',(-3.1434013231585,-42.3742356128,11.1206675701983));
#73166=CARTESIAN_POINT('Ctrl Pts',(-3.26572284156763,-42.3742356128,11.026257876475));
#73167=CARTESIAN_POINT('Ctrl Pts',(-3.38364680560608,-42.3742356128,10.9266419252746));
#73168=CARTESIAN_POINT('Ctrl Pts',(-3.50150366185979,-42.3742356128,10.8270826631947));
#73169=CARTESIAN_POINT('Ctrl Pts',(-3.61496771838722,-42.3742356128,10.7223232785427));
#73170=CARTESIAN_POINT('Ctrl Pts',(-3.72359807694681,-42.3742356128,10.6127729063755));
#73171=CARTESIAN_POINT('Ctrl Pts',(-3.83193116474364,-42.3742356128,10.5035223226202));
#73172=CARTESIAN_POINT('Ctrl Pts',(-3.93545674116179,-42.3742356128,10.3895071587474));
#73173=CARTESIAN_POINT('Ctrl Pts',(-4.03377468497118,-42.3742356128,10.271169329208));
#73174=CARTESIAN_POINT('Ctrl Pts',(-4.04506377902863,-42.3742356128,10.2575815054959));
#73175=CARTESIAN_POINT('Ctrl Pts',(-4.05628425744536,-42.3742356128,10.2439367281876));
#73176=CARTESIAN_POINT('Ctrl Pts',(-4.06743554813384,-42.3742356128,10.2302356948108));
#73177=CARTESIAN_POINT('Ctrl Pts',(-4.16409419458107,-42.3742356128,10.1114760482251));
#73178=CARTESIAN_POINT('Ctrl Pts',(-4.25555110734879,-42.3742356128,9.98848713576328));
#73179=CARTESIAN_POINT('Ctrl Pts',(-4.34145194270822,-42.3742356128,9.86173891404879));
#73180=CARTESIAN_POINT('Ctrl Pts',(-4.42735924310164,-42.3742356128,9.73498115306081));
#73181=CARTESIAN_POINT('Ctrl Pts',(-4.50770946494624,-42.3742356128,9.60446378646192));
#73182=CARTESIAN_POINT('Ctrl Pts',(-4.58219157674198,-42.3742356128,9.47068578032751));
#73183=CARTESIAN_POINT('Ctrl Pts',(-4.65656344968784,-42.3742356128,9.33710577520543));
#73184=CARTESIAN_POINT('Ctrl Pts',(-4.72508441832579,-42.3742356128,9.20027505005788));
#73185=CARTESIAN_POINT('Ctrl Pts',(-4.78749044755381,-42.3742356128,9.06071508722799));
#73186=CARTESIAN_POINT('Ctrl Pts',(-4.84971102952993,-42.3742356128,8.92156984412792));
#73187=CARTESIAN_POINT('Ctrl Pts',(-4.90585282355185,-42.3742356128,8.77971183518736));
#73188=CARTESIAN_POINT('Ctrl Pts',(-4.9557016653129,-42.3742356128,8.63567838517432));
#73189=CARTESIAN_POINT('Ctrl Pts',(-5.00519016121833,-42.3742356128,8.49268611997015));
#73190=CARTESIAN_POINT('Ctrl Pts',(-5.04847625992148,-42.3742356128,8.3475500284784));
#73191=CARTESIAN_POINT('Ctrl Pts',(-5.085399006776,-42.3742356128,8.20081194497571));
#73192=CARTESIAN_POINT('Ctrl Pts',(-5.12213010100009,-42.3742356128,8.05483552581506));
#73193=CARTESIAN_POINT('Ctrl Pts',(-5.15256362407304,-42.3742356128,7.90727396260646));
#73194=CARTESIAN_POINT('Ctrl Pts',(-5.17659093071025,-42.3742356128,7.75867267407153));
#73195=CARTESIAN_POINT('Ctrl Pts',(-5.20038237069215,-42.3742356128,7.61153014616394));
#73196=CARTESIAN_POINT('Ctrl Pts',(-5.2178926901178,-42.3742356128,7.46336845857782));
#73197=CARTESIAN_POINT('Ctrl Pts',(-5.22906657671221,-42.3742356128,7.31472507751491));
#73198=CARTESIAN_POINT('Ctrl Pts',(-5.23891552865557,-42.3742356128,7.18370696627698));
#73199=CARTESIAN_POINT('Ctrl Pts',(-5.24384229242681,-42.3742356128,7.05231483928685));
#73200=CARTESIAN_POINT('Ctrl Pts',(-5.24384247449,-42.3742356128,6.92091963994));
#73201=CARTESIAN_POINT('Ctrl Pts',(1.55431223448E-15,-40.6742356128,12.1643460036));
#73202=CARTESIAN_POINT('Ctrl Pts',(1.55431223448E-15,-42.7142356128,12.1643460036));
#73203=CARTESIAN_POINT('Ctrl Pts',(-1.64768708151,-40.6742356128,12.1643460036));
#73204=CARTESIAN_POINT('Ctrl Pts',(-1.64768708151,-42.7142356128,12.1643460036));
#73205=CARTESIAN_POINT('Ctrl Pts',(-3.29649497043,-40.6742356128,11.5193258882));
#73206=CARTESIAN_POINT('Ctrl Pts',(-3.29649497043,-42.7142356128,11.5193258882));
#73207=CARTESIAN_POINT('Ctrl Pts',(-4.59882235543,-40.6742356128,10.2169985032));
#73208=CARTESIAN_POINT('Ctrl Pts',(-4.59882235543,-42.7142356128,10.2169985032));
#73209=CARTESIAN_POINT('Ctrl Pts',(-5.24384247076,-40.6742356128,8.5681906143));
#73210=CARTESIAN_POINT('Ctrl Pts',(-5.24384247076,-42.7142356128,8.5681906143));
#73211=CARTESIAN_POINT('Ctrl Pts',(-5.24384247076,-40.6742356128,6.92091963994));
#73212=CARTESIAN_POINT('Ctrl Pts',(-5.24384247076,-42.7142356128,6.92091963994));
#73213=CARTESIAN_POINT('',(-5.24384247076,-41.5242356128,6.92091963994));
#73214=CARTESIAN_POINT('Origin',(-5.54384247076,-42.3742356128,1.77756718468));
#73215=CARTESIAN_POINT('',(-5.24384247076,-42.3742356128,3.12351150632));
#73216=CARTESIAN_POINT('Origin',(-5.54172117965729,-42.3763569039027,3.12351150632264));
#73217=CARTESIAN_POINT('',(-5.24384247076,-42.3742356128,5.02221557313));
#73218=CARTESIAN_POINT('Origin',(-5.24384247076,-40.6742356128,6.92091963994));
#73219=CARTESIAN_POINT('',(-5.24384247076,-41.6742356128,3.12351150632));
#73220=CARTESIAN_POINT('Ctrl Pts',(-5.54384247076,-42.6742356128,3.12351150632));
#73221=CARTESIAN_POINT('Ctrl Pts',(-5.44959469115,-42.6742356128,3.12351150632));
#73222=CARTESIAN_POINT('Ctrl Pts',(-5.35534691154,-42.6372245963,3.12351150632));
#73223=CARTESIAN_POINT('Ctrl Pts',(-5.28085348726,-42.5627311721,3.12351150632));
#73224=CARTESIAN_POINT('Ctrl Pts',(-5.24384247076,-42.4684833924,3.12351150632));
#73225=CARTESIAN_POINT('Ctrl Pts',(-5.24384247076,-42.3742356128,3.12351150632));
#73226=CARTESIAN_POINT('Ctrl Pts',(-5.54384247076,-42.6742356128,3.00871019694));
#73227=CARTESIAN_POINT('Ctrl Pts',(-5.44959469115,-42.6742356128,3.02230673235));
#73228=CARTESIAN_POINT('Ctrl Pts',(-5.35534691154,-42.6372245963,3.03590326776));
#73229=CARTESIAN_POINT('Ctrl Pts',(-5.28085348822,-42.5627311721,3.04664996844));
#73230=CARTESIAN_POINT('Ctrl Pts',(-5.24384247076,-42.4684833924,3.05198931333));
#73231=CARTESIAN_POINT('Ctrl Pts',(-5.24384247076,-42.3742356128,3.05198931333));
#73232=CARTESIAN_POINT('Ctrl Pts',(-5.52315912182,-42.6742356128,2.89410223843));
#73233=CARTESIAN_POINT('Ctrl Pts',(-5.43135552331,-42.6742356128,2.9210945322));
#73234=CARTESIAN_POINT('Ctrl Pts',(-5.3395519248,-42.6372245963,2.94808682596));
#73235=CARTESIAN_POINT('Ctrl Pts',(-5.26699037711,-42.5627311721,2.9694215235));
#73236=CARTESIAN_POINT('Ctrl Pts',(-5.23093919189,-42.4684833924,2.980021378));
#73237=CARTESIAN_POINT('Ctrl Pts',(-5.23093919189,-42.3742356128,2.980021378));
#73238=CARTESIAN_POINT('Ctrl Pts',(-5.48214276556,-42.6742356128,2.78431808342));
#73239=CARTESIAN_POINT('Ctrl Pts',(-5.39515201423,-42.6742356128,2.82425482107));
#73240=CARTESIAN_POINT('Ctrl Pts',(-5.30816126289,-42.6372245963,2.86419155871));
#73241=CARTESIAN_POINT('Ctrl Pts',(-5.23940274386,-42.5627311721,2.89575722697));
#73242=CARTESIAN_POINT('Ctrl Pts',(-5.205242604,-42.4684833924,2.91144066757));
#73243=CARTESIAN_POINT('Ctrl Pts',(-5.205242604,-42.3742356128,2.91144066757));
#73244=CARTESIAN_POINT('Ctrl Pts',(-5.3761771061,-42.6742356128,2.60732114997));
#73245=CARTESIAN_POINT('Ctrl Pts',(-5.30168431114,-42.6742356128,2.66814622051));
#73246=CARTESIAN_POINT('Ctrl Pts',(-5.22719151618,-42.6372245963,2.72897129106));
#73247=CARTESIAN_POINT('Ctrl Pts',(-5.16831323005,-42.5627311721,2.77704765466));
#73248=CARTESIAN_POINT('Ctrl Pts',(-5.13905917525,-42.4684833924,2.80093336279));
#73249=CARTESIAN_POINT('Ctrl Pts',(-5.13905917525,-42.3742356128,2.80093336279));
#73250=CARTESIAN_POINT('Ctrl Pts',(-5.221601036,-42.6742356128,2.47270789076));
#73251=CARTESIAN_POINT('Ctrl Pts',(-5.16533736648,-42.6742356128,2.54939750536));
#73252=CARTESIAN_POINT('Ctrl Pts',(-5.10907369696,-42.6372245963,2.62608711997));
#73253=CARTESIAN_POINT('Ctrl Pts',(-5.06460229045,-42.5627311721,2.686702393));
#73254=CARTESIAN_POINT('Ctrl Pts',(-5.04250821359,-42.4684833924,2.71681851572));
#73255=CARTESIAN_POINT('Ctrl Pts',(-5.04250821359,-42.3742356128,2.71681851572));
#73256=CARTESIAN_POINT('Ctrl Pts',(-5.14667997426,-42.6742356128,2.42387620273));
#73257=CARTESIAN_POINT('Ctrl Pts',(-5.09918799439,-42.6742356128,2.5062826488));
#73258=CARTESIAN_POINT('Ctrl Pts',(-5.05169601452,-42.6372245963,2.58868909488));
#73259=CARTESIAN_POINT('Ctrl Pts',(-5.01416083888,-42.5627311721,2.6538238772));
#73260=CARTESIAN_POINT('Ctrl Pts',(-4.99550830718,-42.4684833924,2.68618406744));
#73261=CARTESIAN_POINT('Ctrl Pts',(-4.99550830718,-42.3742356128,2.68618406744));
#73262=CARTESIAN_POINT('Ctrl Pts',(-5.06588952194,-42.6742356128,2.38587643296));
#73263=CARTESIAN_POINT('Ctrl Pts',(-5.02791646833,-42.6742356128,2.47276681809));
#73264=CARTESIAN_POINT('Ctrl Pts',(-4.98994341473,-42.6372245963,2.55965720322));
#73265=CARTESIAN_POINT('Ctrl Pts',(-4.95992787275,-42.5627311721,2.62833484879));
#73266=CARTESIAN_POINT('Ctrl Pts',(-4.94501753823,-42.4684833924,2.66245711898));
#73267=CARTESIAN_POINT('Ctrl Pts',(-4.94501753823,-42.3742356128,2.66245711898));
#73268=CARTESIAN_POINT('Ctrl Pts',(-4.98145041415,-42.6742356128,2.35961199498));
#73269=CARTESIAN_POINT('Ctrl Pts',(-4.95345770517,-42.6742356128,2.44960672899));
#73270=CARTESIAN_POINT('Ctrl Pts',(-4.92546499618,-42.6372245963,2.53960146299));
#73271=CARTESIAN_POINT('Ctrl Pts',(-4.90333956515,-42.5627311721,2.61073328096));
#73272=CARTESIAN_POINT('Ctrl Pts',(-4.89234685404,-42.4684833924,2.64607413036));
#73273=CARTESIAN_POINT('Ctrl Pts',(-4.89234685404,-42.3742356128,2.64607413036));
#73274=CARTESIAN_POINT('',(-4.89234685393,-42.3742356128,2.64607413014));
#73275=CARTESIAN_POINT('Origin',(-4.98082094568694,-42.3763569061133,2.36163774248594));
#73276=CARTESIAN_POINT('Ctrl Pts',(-5.24384247076,-42.3742356128,3.12351150632));
#73277=CARTESIAN_POINT('Ctrl Pts',(-5.24384247076,-42.3742356128,2.9965877265));
#73278=CARTESIAN_POINT('Ctrl Pts',(-5.20322505246,-42.3742356128,2.86908878029));
#73279=CARTESIAN_POINT('Ctrl Pts',(-5.12322496214,-42.3742356128,2.76042445737));
#73280=CARTESIAN_POINT('Ctrl Pts',(-5.01354316676,-42.3742356128,2.6837716054));
#73281=CARTESIAN_POINT('Ctrl Pts',(-4.89234685393,-42.3742356128,2.64607413014));
#73282=CARTESIAN_POINT('Ctrl Pts',(-5.24384247076,-40.6742356128,3.12351150632));
#73283=CARTESIAN_POINT('Ctrl Pts',(-5.24384247076,-42.7142356128,3.12351150632));
#73284=CARTESIAN_POINT('Ctrl Pts',(-5.24384247076,-40.6742356128,2.9965877265));
#73285=CARTESIAN_POINT('Ctrl Pts',(-5.24384247076,-42.7142356128,2.9965877265));
#73286=CARTESIAN_POINT('Ctrl Pts',(-5.20322505246,-40.6742356128,2.86908878029));
#73287=CARTESIAN_POINT('Ctrl Pts',(-5.20322505246,-42.7142356128,2.86908878029));
#73288=CARTESIAN_POINT('Ctrl Pts',(-5.12322496214,-40.6742356128,2.76042445737));
#73289=CARTESIAN_POINT('Ctrl Pts',(-5.12322496214,-42.7142356128,2.76042445737));
#73290=CARTESIAN_POINT('Ctrl Pts',(-5.01354316676,-40.6742356128,2.6837716054));
#73291=CARTESIAN_POINT('Ctrl Pts',(-5.01354316676,-42.7142356128,2.6837716054));
#73292=CARTESIAN_POINT('Ctrl Pts',(-4.89234685393,-40.6742356128,2.64607413014));
#73293=CARTESIAN_POINT('Ctrl Pts',(-4.89234685393,-42.7142356128,2.64607413014));
#73294=CARTESIAN_POINT('',(-4.89234685393,-41.6742356128,2.64607413014));
#73295=CARTESIAN_POINT('Ctrl Pts',(-4.98144948383,-42.6742356128,2.35961170443));
#73296=CARTESIAN_POINT('Ctrl Pts',(-4.95345706708,-42.6742356128,2.44960652964));
#73297=CARTESIAN_POINT('Ctrl Pts',(-4.92546465033,-42.6372245963,2.53960135485));
#73298=CARTESIAN_POINT('Ctrl Pts',(-4.90333945028,-42.5627311721,2.61073324492));
#73299=CARTESIAN_POINT('Ctrl Pts',(-4.89234685393,-42.4684833924,2.64607413014));
#73300=CARTESIAN_POINT('Ctrl Pts',(-4.89234685393,-42.3742356128,2.64607413014));
#73301=CARTESIAN_POINT('Ctrl Pts',(-4.28684551132,-42.6742356128,2.14355879439));
#73302=CARTESIAN_POINT('Ctrl Pts',(-4.24825002553,-42.6742356128,2.23025559078));
#73303=CARTESIAN_POINT('Ctrl Pts',(-4.20965453974,-42.6372245963,2.31695238717));
#73304=CARTESIAN_POINT('Ctrl Pts',(-4.17914867624,-42.5627311721,2.38547751597));
#73305=CARTESIAN_POINT('Ctrl Pts',(-4.16399226443,-42.4684833924,2.41952326831));
#73306=CARTESIAN_POINT('Ctrl Pts',(-4.16399226443,-42.3742356128,2.41952326831));
#73307=CARTESIAN_POINT('Ctrl Pts',(-3.62343950079,-42.6742356128,1.82501616557));
#73308=CARTESIAN_POINT('Ctrl Pts',(-3.57482509928,-42.6742356128,1.90688399481));
#73309=CARTESIAN_POINT('Ctrl Pts',(-3.52621069777,-42.6372245963,1.98875182405));
#73310=CARTESIAN_POINT('Ctrl Pts',(-3.48778588555,-42.5627311721,2.05346013832));
#73311=CARTESIAN_POINT('Ctrl Pts',(-3.46869505468,-42.4684833924,2.08560955965));
#73312=CARTESIAN_POINT('Ctrl Pts',(-3.46869505468,-42.3742356128,2.08560955965));
#73313=CARTESIAN_POINT('Ctrl Pts',(-3.01239604925,-42.6742356128,1.41174509036));
#73314=CARTESIAN_POINT('Ctrl Pts',(-2.95448305204,-42.6742356128,1.48733455128));
#73315=CARTESIAN_POINT('Ctrl Pts',(-2.89657005483,-42.6372245963,1.5629240122));
#73316=CARTESIAN_POINT('Ctrl Pts',(-2.85079564102,-42.5627311721,1.62266993413));
#73317=CARTESIAN_POINT('Ctrl Pts',(-2.82805325375,-42.4684833924,1.65235381737));
#73318=CARTESIAN_POINT('Ctrl Pts',(-2.82805325375,-42.3742356128,1.65235381737));
#73319=CARTESIAN_POINT('Ctrl Pts',(-2.04894527302,-42.6742356128,0.527537333153));
#73320=CARTESIAN_POINT('Ctrl Pts',(-1.97636933137,-42.6742356128,0.589684852453));
#73321=CARTESIAN_POINT('Ctrl Pts',(-1.90379338972,-42.6372245963,0.651832371753));
#73322=CARTESIAN_POINT('Ctrl Pts',(-1.84642937642,-42.5627311721,0.700953735078));
#73323=CARTESIAN_POINT('Ctrl Pts',(-1.81792887576,-42.4684833924,0.725359031103));
#73324=CARTESIAN_POINT('Ctrl Pts',(-1.81792887576,-42.3742356128,0.725359031103));
#73325=CARTESIAN_POINT('Ctrl Pts',(-1.34746460805,-42.6742356128,-0.569990686554));
#73326=CARTESIAN_POINT('Ctrl Pts',(-1.26422030149,-42.6742356128,-0.524548982088));
#73327=CARTESIAN_POINT('Ctrl Pts',(-1.18097599493,-42.6372245963,-0.479107277622));
#73328=CARTESIAN_POINT('Ctrl Pts',(-1.11517971718,-42.5627311721,-0.443190147097));
#73329=CARTESIAN_POINT('Ctrl Pts',(-1.08248975058,-42.4684833924,-0.425345248789));
#73330=CARTESIAN_POINT('Ctrl Pts',(-1.08248975058,-42.3742356128,-0.425345248789));
#73331=CARTESIAN_POINT('Ctrl Pts',(-1.09663661983,-42.6742356128,-1.08402978875));
#73332=CARTESIAN_POINT('Ctrl Pts',(-1.00960204779,-42.6742356128,-1.04634891047));
#73333=CARTESIAN_POINT('Ctrl Pts',(-0.92256747575,-42.6372245963,-1.0086680322));
#73334=CARTESIAN_POINT('Ctrl Pts',(-0.853775353599,-42.5627311721,-0.978885143705));
#73335=CARTESIAN_POINT('Ctrl Pts',(-0.81959697263,-42.4684833924,-0.964087827993));
#73336=CARTESIAN_POINT('Ctrl Pts',(-0.81959697263,-42.3742356128,-0.964087827993));
#73337=CARTESIAN_POINT('Ctrl Pts',(-0.906464192514,-42.6742356128,-1.62228962869));
#73338=CARTESIAN_POINT('Ctrl Pts',(-0.816530141078,-42.6742356128,-1.59281044263));
#73339=CARTESIAN_POINT('Ctrl Pts',(-0.726596089643,-42.6372245963,-1.56333125657));
#73340=CARTESIAN_POINT('Ctrl Pts',(-0.655512245516,-42.5627311721,-1.54003086813));
#73341=CARTESIAN_POINT('Ctrl Pts',(-0.620195215749,-42.4684833924,-1.52845446509));
#73342=CARTESIAN_POINT('Ctrl Pts',(-0.620195215749,-42.3742356128,-1.52845446509));
#73343=CARTESIAN_POINT('Ctrl Pts',(-0.779760514736,-42.6742356128,-2.17481998786));
#73344=CARTESIAN_POINT('Ctrl Pts',(-0.68789712753,-42.6742356128,-2.15375432708));
#73345=CARTESIAN_POINT('Ctrl Pts',(-0.596033740324,-42.6372245963,-2.13268866631));
#73346=CARTESIAN_POINT('Ctrl Pts',(-0.523424939273,-42.5627311721,-2.11603837266));
#73347=CARTESIAN_POINT('Ctrl Pts',(-0.487350271475,-42.4684833924,-2.10776590702));
#73348=CARTESIAN_POINT('Ctrl Pts',(-0.487350271475,-42.3742356128,-2.10776590702));
#73349=CARTESIAN_POINT('',(-0.487350273345822,-42.3742356128,-2.10776590704375));
#73350=CARTESIAN_POINT('Origin',(-0.777692936443982,-42.3763569081971,-2.17434563581814));
#73351=CARTESIAN_POINT('Ctrl Pts',(-4.89234685393,-42.3742356128,2.64607413014));
#73352=CARTESIAN_POINT('Ctrl Pts',(-3.59661572838,-42.3742356128,2.2430437828));
#73353=CARTESIAN_POINT('Ctrl Pts',(-2.40362850687,-42.3742356128,1.49964984368));
#73354=CARTESIAN_POINT('Ctrl Pts',(-1.44114622406,-42.3742356128,0.46094601538));
#73355=CARTESIAN_POINT('Ctrl Pts',(-0.790651846747,-42.3742356128,-0.785131881257));
#73356=CARTESIAN_POINT('Ctrl Pts',(-0.48735027394,-42.3742356128,-2.10776590718));
#73357=CARTESIAN_POINT('Ctrl Pts',(-4.89234685393,-40.6742356128,2.64607413014));
#73358=CARTESIAN_POINT('Ctrl Pts',(-4.89234685393,-42.7142356128,2.64607413014));
#73359=CARTESIAN_POINT('Ctrl Pts',(-3.59661572838,-40.6742356128,2.2430437828));
#73360=CARTESIAN_POINT('Ctrl Pts',(-3.59661572838,-42.7142356128,2.2430437828));
#73361=CARTESIAN_POINT('Ctrl Pts',(-2.40362850687,-40.6742356128,1.49964984368));
#73362=CARTESIAN_POINT('Ctrl Pts',(-2.40362850687,-42.7142356128,1.49964984368));
#73363=CARTESIAN_POINT('Ctrl Pts',(-1.44114622406,-40.6742356128,0.46094601538));
#73364=CARTESIAN_POINT('Ctrl Pts',(-1.44114622406,-42.7142356128,0.46094601538));
#73365=CARTESIAN_POINT('Ctrl Pts',(-0.790651846747,-40.6742356128,-0.785131881257));
#73366=CARTESIAN_POINT('Ctrl Pts',(-0.790651846747,-42.7142356128,-0.785131881257));
#73367=CARTESIAN_POINT('Ctrl Pts',(-0.48735027394,-40.6742356128,-2.10776590718));
#73368=CARTESIAN_POINT('Ctrl Pts',(-0.48735027394,-42.7142356128,-2.10776590718));
#73369=CARTESIAN_POINT('',(-0.48735027394,-41.6742356128,-2.10776590718));
#73370=CARTESIAN_POINT('Ctrl Pts',(-0.779760438305,-42.6742356128,-2.17482033117));
#73371=CARTESIAN_POINT('Ctrl Pts',(-0.687897075884,-42.6742356128,-2.15375456259));
#73372=CARTESIAN_POINT('Ctrl Pts',(-0.596033713464,-42.6372245963,-2.13268879401));
#73373=CARTESIAN_POINT('Ctrl Pts',(-0.523424932005,-42.5627311721,-2.11603841516));
#73374=CARTESIAN_POINT('Ctrl Pts',(-0.48735027394,-42.4684833924,-2.10776590718));
#73375=CARTESIAN_POINT('Ctrl Pts',(-0.48735027394,-42.3742356128,-2.10776590718));
#73376=CARTESIAN_POINT('Ctrl Pts',(-0.728940682779,-42.6742356128,-2.39643453918));
#73377=CARTESIAN_POINT('Ctrl Pts',(-0.643021055832,-42.6742356128,-2.34944939701));
#73378=CARTESIAN_POINT('Ctrl Pts',(-0.557101428885,-42.6372245963,-2.30246425483));
#73379=CARTESIAN_POINT('Ctrl Pts',(-0.489190575517,-42.5627311721,-2.26532720315));
#73380=CARTESIAN_POINT('Ctrl Pts',(-0.455450016034,-42.4684833924,-2.2468761866));
#73381=CARTESIAN_POINT('Ctrl Pts',(-0.455450016034,-42.3742356128,-2.2468761866));
#73382=CARTESIAN_POINT('Ctrl Pts',(-0.600115266646,-42.6742356128,-2.60147317882));
#73383=CARTESIAN_POINT('Ctrl Pts',(-0.529241757754,-42.6742356128,-2.53022408265));
#73384=CARTESIAN_POINT('Ctrl Pts',(-0.458368248863,-42.6372245963,-2.45897498649));
#73385=CARTESIAN_POINT('Ctrl Pts',(-0.402349836567,-42.5627311721,-2.40265972476));
#73386=CARTESIAN_POINT('Ctrl Pts',(-0.374517881159,-42.4684833924,-2.3746802619));
#73387=CARTESIAN_POINT('Ctrl Pts',(-0.374517881159,-42.3742356128,-2.3746802619));
#73388=CARTESIAN_POINT('Ctrl Pts',(-0.397739638795,-42.6742356128,-2.74850259847));
#73389=CARTESIAN_POINT('Ctrl Pts',(-0.35125139287,-42.6742356128,-2.65967101811));
#73390=CARTESIAN_POINT('Ctrl Pts',(-0.304763146945,-42.6372245963,-2.57083943775));
#73391=CARTESIAN_POINT('Ctrl Pts',(-0.26801875295,-42.5627311721,-2.50062658719));
#73392=CARTESIAN_POINT('Ctrl Pts',(-0.249762956102,-42.4684833924,-2.46574289613));
#73393=CARTESIAN_POINT('Ctrl Pts',(-0.249762956102,-42.3742356128,-2.46574289613));
#73394=CARTESIAN_POINT('Ctrl Pts',(0.0424568072293,-42.6742356128,-2.86620382326));
#73395=CARTESIAN_POINT('Ctrl Pts',(0.0375764440826,-42.6742356128,-2.76378874984));
#73396=CARTESIAN_POINT('Ctrl Pts',(0.0326960809359,-42.6372245963,-2.66137367642));
#73397=CARTESIAN_POINT('Ctrl Pts',(0.0288385715632,-42.5627311721,-2.58042517097));
#73398=CARTESIAN_POINT('Ctrl Pts',(0.0269221288516,-42.4684833924,-2.54020651962));
#73399=CARTESIAN_POINT('Ctrl Pts',(0.0269221288516,-42.3742356128,-2.54020651962));
#73400=CARTESIAN_POINT('Ctrl Pts',(0.461136763067,-42.6742356128,-2.69888825006));
#73401=CARTESIAN_POINT('Ctrl Pts',(0.407040904949,-42.6742356128,-2.61589041711));
#73402=CARTESIAN_POINT('Ctrl Pts',(0.35294504683,-42.6372245963,-2.53289258416));
#73403=CARTESIAN_POINT('Ctrl Pts',(0.310187744589,-42.5627311721,-2.46729080736));
#73404=CARTESIAN_POINT('Ctrl Pts',(0.288944298659,-42.4684833924,-2.43469794247));
#73405=CARTESIAN_POINT('Ctrl Pts',(0.288944298659,-42.3742356128,-2.43469794247));
#73406=CARTESIAN_POINT('Ctrl Pts',(0.6271830499,-42.6742356128,-2.55661546807));
#73407=CARTESIAN_POINT('Ctrl Pts',(0.553146114073,-42.6742356128,-2.49065409452));
#73408=CARTESIAN_POINT('Ctrl Pts',(0.479109178246,-42.6372245963,-2.42469272097));
#73409=CARTESIAN_POINT('Ctrl Pts',(0.420590142213,-42.5627311721,-2.37255809298));
#73410=CARTESIAN_POINT('Ctrl Pts',(0.391516163736,-42.4684833924,-2.346653895));
#73411=CARTESIAN_POINT('Ctrl Pts',(0.391516163736,-42.3742356128,-2.346653895));
#73412=CARTESIAN_POINT('Ctrl Pts',(0.734479238607,-42.6742356128,-2.37228010264));
#73413=CARTESIAN_POINT('Ctrl Pts',(0.647901224488,-42.6742356128,-2.3281663573));
#73414=CARTESIAN_POINT('Ctrl Pts',(0.561323210368,-42.6372245963,-2.28405261197));
#73415=CARTESIAN_POINT('Ctrl Pts',(0.492892136152,-42.5627311721,-2.2491842994));
#73416=CARTESIAN_POINT('Ctrl Pts',(0.458892860404,-42.4684833924,-2.23186169008));
#73417=CARTESIAN_POINT('Ctrl Pts',(0.458892860404,-42.3742356128,-2.23186169008));
#73418=CARTESIAN_POINT('Ctrl Pts',(0.77975997749,-42.6742356128,-2.17482231881));
#73419=CARTESIAN_POINT('Ctrl Pts',(0.687896759445,-42.6742356128,-2.15375592622));
#73420=CARTESIAN_POINT('Ctrl Pts',(0.596033541399,-42.6372245963,-2.13268953362));
#73421=CARTESIAN_POINT('Ctrl Pts',(0.523424874053,-42.5627311721,-2.11603866155));
#73422=CARTESIAN_POINT('Ctrl Pts',(0.487350272685,-42.4684833924,-2.10776590852));
#73423=CARTESIAN_POINT('Ctrl Pts',(0.487350272685,-42.3742356128,-2.10776590852));
#73424=CARTESIAN_POINT('',(0.48735027362625,-42.3742356128,-2.107765907515));
#73425=CARTESIAN_POINT('Origin',(0.777692065618351,-42.3763569132498,-2.17434940414811));
#73426=CARTESIAN_POINT('Ctrl Pts',(-0.48735027394,-42.3742356128,-2.10776590718));
#73427=CARTESIAN_POINT('Ctrl Pts',(-0.481651530051025,-42.3742356128,-2.13261692428069));
#73428=CARTESIAN_POINT('Ctrl Pts',(-0.474067950247163,-42.3742356128,-2.15704737654675));
#73429=CARTESIAN_POINT('Ctrl Pts',(-0.46468020372962,-42.3742356128,-2.18075399603358));
#73430=CARTESIAN_POINT('Ctrl Pts',(-0.454943458649678,-42.3742356128,-2.20534193204347));
#73431=CARTESIAN_POINT('Ctrl Pts',(-0.443265892704172,-42.3742356128,-2.22915084671963));
#73432=CARTESIAN_POINT('Ctrl Pts',(-0.429786360652213,-42.3742356128,-2.25187433028169));
#73433=CARTESIAN_POINT('Ctrl Pts',(-0.416540327134175,-42.3742356128,-2.27420418741245));
#73434=CARTESIAN_POINT('Ctrl Pts',(-0.40155462641195,-42.3742356128,-2.29548581661124));
#73435=CARTESIAN_POINT('Ctrl Pts',(-0.385003695533678,-42.3742356128,-2.31546165616534));
#73436=CARTESIAN_POINT('Ctrl Pts',(-0.368353988180329,-42.3742356128,-2.33555671215701));
#73437=CARTESIAN_POINT('Ctrl Pts',(-0.350120568954219,-42.3742356128,-2.35433014302128));
#73438=CARTESIAN_POINT('Ctrl Pts',(-0.330519834913059,-42.3742356128,-2.37155591534188));
#73439=CARTESIAN_POINT('Ctrl Pts',(-0.310822118521399,-42.3742356128,-2.3888669189546));
#73440=CARTESIAN_POINT('Ctrl Pts',(-0.289743807545843,-42.3742356128,-2.40461471280278));
#73441=CARTESIAN_POINT('Ctrl Pts',(-0.267539519104164,-42.3742356128,-2.41860932865736));
#73442=CARTESIAN_POINT('Ctrl Pts',(-0.244990950343904,-42.3742356128,-2.43282093281208));
#73443=CARTESIAN_POINT('Ctrl Pts',(-0.221281477413771,-42.3742356128,-2.44522428927903));
#73444=CARTESIAN_POINT('Ctrl Pts',(-0.196709685894568,-42.3742356128,-2.45566477541128));
#73445=CARTESIAN_POINT('Ctrl Pts',(-0.172360603756016,-42.3742356128,-2.46601063294478));
#73446=CARTESIAN_POINT('Ctrl Pts',(-0.14716515001463,-42.3742356128,-2.47442895047424));
#73447=CARTESIAN_POINT('Ctrl Pts',(-0.121439934607891,-42.3742356128,-2.48081496692291));
#73448=CARTESIAN_POINT('Ctrl Pts',(-0.0953617748833097,-42.3742356128,-2.48728859811779));
#73449=CARTESIAN_POINT('Ctrl Pts',(-0.0687395329780045,-42.3742356128,-2.49167351118973));
#73450=CARTESIAN_POINT('Ctrl Pts',(-0.0419247854849334,-42.3742356128,-2.49391070858224));
#73451=CARTESIAN_POINT('Ctrl Pts',(-0.0151100379918623,-42.3742356128,-2.49614790597475));
#73452=CARTESIAN_POINT('Ctrl Pts',(0.0118968385201095,-42.3742356128,-2.4962372385907));
#73453=CARTESIAN_POINT('Ctrl Pts',(0.0387279584952791,-42.3742356128,-2.49417248854828));
#73454=CARTESIAN_POINT('Ctrl Pts',(0.0651866464420061,-42.3742356128,-2.4921363984741));
#73455=CARTESIAN_POINT('Ctrl Pts',(0.0914718021070565,-42.3742356128,-2.48800590743246));
#73456=CARTESIAN_POINT('Ctrl Pts',(0.117243785997238,-42.3742356128,-2.4818389652788));
#73457=CARTESIAN_POINT('Ctrl Pts',(0.143035952064683,-42.3742356128,-2.47566719376003));
#73458=CARTESIAN_POINT('Ctrl Pts',(0.168313814172657,-42.3742356128,-2.46745595774278));
#73459=CARTESIAN_POINT('Ctrl Pts',(0.192758820941668,-42.3742356128,-2.45731088970016));
#73460=CARTESIAN_POINT('Ctrl Pts',(0.217190759828193,-42.3742356128,-2.44717124503739));
#73461=CARTESIAN_POINT('Ctrl Pts',(0.2407904171663,-42.3742356128,-2.43510003092528));
#73462=CARTESIAN_POINT('Ctrl Pts',(0.263266435042778,-42.3742356128,-2.42124737424211));
#73463=CARTESIAN_POINT('Ctrl Pts',(0.28569519560683,-42.3742356128,-2.40742384368477));
#73464=CARTESIAN_POINT('Ctrl Pts',(0.30700473924559,-42.3742356128,-2.39182656556059));
#73465=CARTESIAN_POINT('Ctrl Pts',(0.326936706536049,-42.3742356128,-2.37464614284886));
#73466=CARTESIAN_POINT('Ctrl Pts',(0.346909828510513,-42.3742356128,-2.35743024672612));
#73467=CARTESIAN_POINT('Ctrl Pts',(0.365499366722612,-42.3742356128,-2.33862485253807));
#73468=CARTESIAN_POINT('Ctrl Pts',(0.382481299280299,-42.3742356128,-2.31846040320672));
#73469=CARTESIAN_POINT('Ctrl Pts',(0.399249784105912,-42.3742356128,-2.29854940300218));
#73470=CARTESIAN_POINT('Ctrl Pts',(0.414450625550339,-42.3742356128,-2.27731357042829));
#73471=CARTESIAN_POINT('Ctrl Pts',(0.427906795226446,-42.3742356128,-2.25500882472017));
#73472=CARTESIAN_POINT('Ctrl Pts',(0.441619892310991,-42.3742356128,-2.23227819998046));
#73473=CARTESIAN_POINT('Ctrl Pts',(0.453520636330002,-42.3742356128,-2.2084375657962));
#73474=CARTESIAN_POINT('Ctrl Pts',(0.463467024799772,-42.3742356128,-2.18379071638894));
#73475=CARTESIAN_POINT('Ctrl Pts',(0.473413413269542,-42.3742356128,-2.15914386698167));
#73476=CARTESIAN_POINT('Ctrl Pts',(0.481405173011034,-42.3742356128,-2.13369102719235));
#73477=CARTESIAN_POINT('Ctrl Pts',(0.487350272685,-42.3742356128,-2.10776590852));
#73478=CARTESIAN_POINT('Ctrl Pts',(-0.48735027394,-40.6742356128,-2.10776590718));
#73479=CARTESIAN_POINT('Ctrl Pts',(-0.48735027394,-42.7142356128,-2.10776590718));
#73480=CARTESIAN_POINT('Ctrl Pts',(-0.427207937888,-40.6742356128,-2.37003391761));
#73481=CARTESIAN_POINT('Ctrl Pts',(-0.427207937888,-42.7142356128,-2.37003391761));
#73482=CARTESIAN_POINT('Ctrl Pts',(-0.191539291907,-40.6742356128,-2.59726293898));
#73483=CARTESIAN_POINT('Ctrl Pts',(-0.191539291907,-42.7142356128,-2.59726293898));
#73484=CARTESIAN_POINT('Ctrl Pts',(0.191539291907,-40.6742356128,-2.59726293898));
#73485=CARTESIAN_POINT('Ctrl Pts',(0.191539291907,-42.7142356128,-2.59726293898));
#73486=CARTESIAN_POINT('Ctrl Pts',(0.427207937888,-40.6742356128,-2.37003391761));
#73487=CARTESIAN_POINT('Ctrl Pts',(0.427207937888,-42.7142356128,-2.37003391761));
#73488=CARTESIAN_POINT('Ctrl Pts',(0.48735027394,-40.6742356128,-2.10776590718));
#73489=CARTESIAN_POINT('Ctrl Pts',(0.48735027394,-42.7142356128,-2.10776590718));
#73490=CARTESIAN_POINT('',(0.48735027394,-41.6742356128,-2.10776590718));
#73491=CARTESIAN_POINT('Ctrl Pts',(0.779760438305,-42.6742356128,-2.17482033117));
#73492=CARTESIAN_POINT('Ctrl Pts',(0.687897075884,-42.6742356128,-2.15375456259));
#73493=CARTESIAN_POINT('Ctrl Pts',(0.596033713464,-42.6372245963,-2.13268879401));
#73494=CARTESIAN_POINT('Ctrl Pts',(0.523424932005,-42.5627311721,-2.11603841516));
#73495=CARTESIAN_POINT('Ctrl Pts',(0.48735027394,-42.4684833924,-2.10776590718));
#73496=CARTESIAN_POINT('Ctrl Pts',(0.48735027394,-42.3742356128,-2.10776590718));
#73497=CARTESIAN_POINT('Ctrl Pts',(0.942351637347,-42.6742356128,-1.46579449204));
#73498=CARTESIAN_POINT('Ctrl Pts',(0.852970215394,-42.6742356128,-1.43390550589));
#73499=CARTESIAN_POINT('Ctrl Pts',(0.763588793442,-42.6372245963,-1.40201651973));
#73500=CARTESIAN_POINT('Ctrl Pts',(0.692941737192,-42.5627311721,-1.37681147207));
#73501=CARTESIAN_POINT('Ctrl Pts',(0.65784173486,-42.4684833924,-1.36428869651));
#73502=CARTESIAN_POINT('Ctrl Pts',(0.65784173486,-42.3742356128,-1.36428869651));
#73503=CARTESIAN_POINT('Ctrl Pts',(1.20950872503,-42.6742356128,-0.780080242745));
#73504=CARTESIAN_POINT('Ctrl Pts',(1.12418018063,-42.6742356128,-0.737834047536));
#73505=CARTESIAN_POINT('Ctrl Pts',(1.03885163623,-42.6372245963,-0.695587852327));
#73506=CARTESIAN_POINT('Ctrl Pts',(0.971407973461,-42.5627311721,-0.662196468967));
#73507=CARTESIAN_POINT('Ctrl Pts',(0.937899532468,-42.4684833924,-0.645606426859));
#73508=CARTESIAN_POINT('Ctrl Pts',(0.937899532468,-42.3742356128,-0.645606426859));
#73509=CARTESIAN_POINT('Ctrl Pts',(1.57510282168,-42.6742356128,-0.139371230964));
#73510=CARTESIAN_POINT('Ctrl Pts',(1.49532714866,-42.6742356128,-0.0873758096127));
#73511=CARTESIAN_POINT('Ctrl Pts',(1.41555147563,-42.6372245963,-0.0353803882614));
#73512=CARTESIAN_POINT('Ctrl Pts',(1.35249677314,-42.5627311721,0.00571677273303));
#73513=CARTESIAN_POINT('Ctrl Pts',(1.32116896768,-42.4684833924,0.0261353355601));
#73514=CARTESIAN_POINT('Ctrl Pts',(1.32116896768,-42.3742356128,0.0261353355601));
#73515=CARTESIAN_POINT('Ctrl Pts',(2.38346297254,-42.6742356128,0.88854638374));
#73516=CARTESIAN_POINT('Ctrl Pts',(2.31597494511,-42.6742356128,0.956184742789));
#73517=CARTESIAN_POINT('Ctrl Pts',(2.24848691768,-42.6372245963,1.02382310184));
#73518=CARTESIAN_POINT('Ctrl Pts',(2.19514441746,-42.5627311721,1.07728445262));
#73519=CARTESIAN_POINT('Ctrl Pts',(2.16864190924,-42.4684833924,1.10384596745));
#73520=CARTESIAN_POINT('Ctrl Pts',(2.16864190924,-42.3742356128,1.10384596745));
#73521=CARTESIAN_POINT('Ctrl Pts',(3.42445237435,-42.6742356128,1.67147929445));
#73522=CARTESIAN_POINT('Ctrl Pts',(3.37281026135,-42.6742356128,1.75102585468));
#73523=CARTESIAN_POINT('Ctrl Pts',(3.32116814834,-42.6372245963,1.8305724149));
#73524=CARTESIAN_POINT('Ctrl Pts',(3.28035021661,-42.5627311721,1.89344599346));
#73525=CARTESIAN_POINT('Ctrl Pts',(3.26007042322,-42.4684833924,1.92468385976));
#73526=CARTESIAN_POINT('Ctrl Pts',(3.26007042322,-42.3742356128,1.92468385976));
#73527=CARTESIAN_POINT('Ctrl Pts',(3.91792270746,-42.6742356128,1.96068148776));
#73528=CARTESIAN_POINT('Ctrl Pts',(3.87373062544,-42.6742356128,2.0445976674));
#73529=CARTESIAN_POINT('Ctrl Pts',(3.82953854342,-42.6372245963,2.12851384703));
#73530=CARTESIAN_POINT('Ctrl Pts',(3.79460919954,-42.5627311721,2.19484119775));
#73531=CARTESIAN_POINT('Ctrl Pts',(3.77725494148,-42.4684833924,2.22779498365));
#73532=CARTESIAN_POINT('Ctrl Pts',(3.77725494148,-42.3742356128,2.22779498365));
#73533=CARTESIAN_POINT('Ctrl Pts',(4.44015743262,-42.6742356128,2.19124622755));
#73534=CARTESIAN_POINT('Ctrl Pts',(4.40392272888,-42.6742356128,2.27867735624));
#73535=CARTESIAN_POINT('Ctrl Pts',(4.36768802515,-42.6372245963,2.36610848493));
#73536=CARTESIAN_POINT('Ctrl Pts',(4.33904807794,-42.5627311721,2.43521401597));
#73537=CARTESIAN_POINT('Ctrl Pts',(4.3248187884,-42.4684833924,2.46954815377));
#73538=CARTESIAN_POINT('Ctrl Pts',(4.3248187884,-42.3742356128,2.46954815377));
#73539=CARTESIAN_POINT('Ctrl Pts',(4.98144914733,-42.6742356128,2.3596116021));
#73540=CARTESIAN_POINT('Ctrl Pts',(4.95345683619,-42.6742356128,2.44960646023));
#73541=CARTESIAN_POINT('Ctrl Pts',(4.92546452504,-42.6372245963,2.53960131836));
#73542=CARTESIAN_POINT('Ctrl Pts',(4.90333940847,-42.5627311721,2.61073323444));
#73543=CARTESIAN_POINT('Ctrl Pts',(4.89234685358,-42.4684833924,2.64607413258));
#73544=CARTESIAN_POINT('Ctrl Pts',(4.89234685358,-42.3742356128,2.64607413258));
#73545=CARTESIAN_POINT('Ctrl Pts',(0.48735027394,-42.3742356128,-2.10776590718));
#73546=CARTESIAN_POINT('Ctrl Pts',(0.790651846747,-42.3742356128,-0.785131881257001));
#73547=CARTESIAN_POINT('Ctrl Pts',(1.44114622406,-42.3742356128,0.46094601538));
#73548=CARTESIAN_POINT('Ctrl Pts',(2.40362850687,-42.3742356128,1.49964984368));
#73549=CARTESIAN_POINT('Ctrl Pts',(3.59661572838,-42.3742356128,2.2430437828));
#73550=CARTESIAN_POINT('Ctrl Pts',(4.89234685393,-42.3742356128,2.64607413014));
#73551=CARTESIAN_POINT('Ctrl Pts',(0.48735027394,-40.6742356128,-2.10776590718));
#73552=CARTESIAN_POINT('Ctrl Pts',(0.48735027394,-42.7142356128,-2.10776590718));
#73553=CARTESIAN_POINT('Ctrl Pts',(0.790651846747,-40.6742356128,-0.785131881257));
#73554=CARTESIAN_POINT('Ctrl Pts',(0.790651846747,-42.7142356128,-0.785131881257));
#73555=CARTESIAN_POINT('Ctrl Pts',(1.44114622406,-40.6742356128,0.46094601538));
#73556=CARTESIAN_POINT('Ctrl Pts',(1.44114622406,-42.7142356128,0.46094601538));
#73557=CARTESIAN_POINT('Ctrl Pts',(2.40362850687,-40.6742356128,1.49964984368));
#73558=CARTESIAN_POINT('Ctrl Pts',(2.40362850687,-42.7142356128,1.49964984368));
#73559=CARTESIAN_POINT('Ctrl Pts',(3.59661572838,-40.6742356128,2.2430437828));
#73560=CARTESIAN_POINT('Ctrl Pts',(3.59661572838,-42.7142356128,2.2430437828));
#73561=CARTESIAN_POINT('Ctrl Pts',(4.89234685393,-40.6742356128,2.64607413014));
#73562=CARTESIAN_POINT('Ctrl Pts',(4.89234685393,-42.7142356128,2.64607413014));
#73563=CARTESIAN_POINT('Ctrl Pts',(6.74948971107,-42.3742356128,2.9389736393));
#73564=CARTESIAN_POINT('Ctrl Pts',(6.74948971107,-42.4684833924,2.9389736393));
#73565=CARTESIAN_POINT('Ctrl Pts',(6.74990773128,-42.5627311721,2.90196498354));
#73566=CARTESIAN_POINT('Ctrl Pts',(6.75074909582,-42.6372245963,2.82747631079));
#73567=CARTESIAN_POINT('Ctrl Pts',(6.75181357554,-42.6742356128,2.73323454275));
#73568=CARTESIAN_POINT('Ctrl Pts',(6.75287805526,-42.6742356128,2.63899277471));
#73569=CARTESIAN_POINT('Ctrl Pts',(6.66016121042,-42.3742356128,2.93796465593));
#73570=CARTESIAN_POINT('Ctrl Pts',(6.66016121042,-42.4684833924,2.93796465593));
#73571=CARTESIAN_POINT('Ctrl Pts',(6.65383637296,-42.5627311721,2.90087983603));
#73572=CARTESIAN_POINT('Ctrl Pts',(6.64110613629,-42.6372245963,2.82623787152));
#73573=CARTESIAN_POINT('Ctrl Pts',(6.62500006538,-42.6742356128,2.73180215865));
#73574=CARTESIAN_POINT('Ctrl Pts',(6.60889399448,-42.6742356128,2.63736644579));
#73575=CARTESIAN_POINT('Ctrl Pts',(6.56930976652,-42.3742356128,2.95731325003));
#73576=CARTESIAN_POINT('Ctrl Pts',(6.56930978704,-42.4684833931,2.95731325253));
#73577=CARTESIAN_POINT('Ctrl Pts',(6.55645224693,-42.5627311733,2.92167994217));
#73578=CARTESIAN_POINT('Ctrl Pts',(6.53057339717,-42.6372245978,2.8499594543));
#73579=CARTESIAN_POINT('Ctrl Pts',(6.49783190936,-42.6742356138,2.75921995253));
#73580=CARTESIAN_POINT('Ctrl Pts',(6.46509041354,-42.6742356128,2.66848045015));
#73581=CARTESIAN_POINT('Ctrl Pts',(6.48517929362,-42.3742356128,2.99677643843));
#73582=CARTESIAN_POINT('Ctrl Pts',(6.48517930736,-42.4684833932,2.99677642435));
#73583=CARTESIAN_POINT('Ctrl Pts',(6.46607746743,-42.5627311736,2.96400514186));
#73584=CARTESIAN_POINT('Ctrl Pts',(6.42763047779,-42.6372245982,2.89804241892));
#73585=CARTESIAN_POINT('Ctrl Pts',(6.37898801081,-42.6742356141,2.81458871105));
#73586=CARTESIAN_POINT('Ctrl Pts',(6.330345539,-42.6742356128,2.73113500859));
#73587=CARTESIAN_POINT('Ctrl Pts',(6.35806155931,-42.3742356128,3.0966048171));
#73588=CARTESIAN_POINT('Ctrl Pts',(6.35806154885,-42.4684833919,3.09660482782));
#73589=CARTESIAN_POINT('Ctrl Pts',(6.32947675772,-42.5627311709,3.07128279651));
#73590=CARTESIAN_POINT('Ctrl Pts',(6.27194313738,-42.6372245949,3.02031830205));
#73591=CARTESIAN_POINT('Ctrl Pts',(6.19915260335,-42.6742356119,2.95583802709));
#73592=CARTESIAN_POINT('Ctrl Pts',(6.12636207301,-42.6742356128,2.89135774799));
#73593=CARTESIAN_POINT('Ctrl Pts',(6.27916935631,-42.3742356128,3.23622606791));
#73594=CARTESIAN_POINT('Ctrl Pts',(6.27916936428,-42.4684833929,3.23622605975));
#73595=CARTESIAN_POINT('Ctrl Pts',(6.24474924576,-42.562731173,3.22125677195));
#73596=CARTESIAN_POINT('Ctrl Pts',(6.17547057799,-42.6372245974,3.19112597217));
#73597=CARTESIAN_POINT('Ctrl Pts',(6.08782042473,-42.6742356135,3.15300567784));
#73598=CARTESIAN_POINT('Ctrl Pts',(6.00017026865,-42.6742356128,3.11488538668));
#73599=CARTESIAN_POINT('Ctrl Pts',(6.25564469688,-42.3742356128,3.30224048175));
#73600=CARTESIAN_POINT('Ctrl Pts',(6.25564469441,-42.4684833903,3.30224046041));
#73601=CARTESIAN_POINT('Ctrl Pts',(6.21952273597,-42.5627311677,3.29207824683));
#73602=CARTESIAN_POINT('Ctrl Pts',(6.14681880931,-42.6372245911,3.2716308039));
#73603=CARTESIAN_POINT('Ctrl Pts',(6.05483504826,-42.6742356094,3.24575838595));
#73604=CARTESIAN_POINT('Ctrl Pts',(5.96285128692,-42.6742356128,3.21988597629));
#73605=CARTESIAN_POINT('Ctrl Pts',(6.24384239412,-42.3742356128,3.37085211609));
#73606=CARTESIAN_POINT('Ctrl Pts',(6.24384239414,-42.4684833933,3.37085211656));
#73607=CARTESIAN_POINT('Ctrl Pts',(6.20683138795,-42.5627311738,3.36573100796));
#73608=CARTESIAN_POINT('Ctrl Pts',(6.13233794388,-42.6372245985,3.35541931075));
#73609=CARTESIAN_POINT('Ctrl Pts',(6.03809015669,-42.6742356142,3.3423749178));
#73610=CARTESIAN_POINT('Ctrl Pts',(5.94384237,-42.6742356128,3.32933052468));
#73611=CARTESIAN_POINT('Ctrl Pts',(6.24384247119,-42.3742356128,3.43894174635));
#73612=CARTESIAN_POINT('Ctrl Pts',(6.24384247119,-42.4684833925,3.43894174639));
#73613=CARTESIAN_POINT('Ctrl Pts',(6.206831455,-42.5627311721,3.43894191067));
#73614=CARTESIAN_POINT('Ctrl Pts',(6.13233803133,-42.6372245964,3.43894224126));
#73615=CARTESIAN_POINT('Ctrl Pts',(6.03809025252,-42.6742356129,3.4389426595));
#73616=CARTESIAN_POINT('Ctrl Pts',(5.94384247373,-42.6742356128,3.43894307771));
#73617=CARTESIAN_POINT('',(6.74948971103925,-42.3742356128,2.93897363980053));
#73618=CARTESIAN_POINT('Origin',(6.75285456584568,-42.3763569074475,2.64111394033772));
#73619=CARTESIAN_POINT('',(6.24384247076,-42.3742356128,3.43894174696));
#73620=CARTESIAN_POINT('Ctrl Pts',(6.74948971107,-42.3742356128,2.9389736393));
#73621=CARTESIAN_POINT('Ctrl Pts',(6.59129069763,-42.3742356128,2.93718674963));
#73622=CARTESIAN_POINT('Ctrl Pts',(6.43081292755,-42.3742356128,2.99918925876));
#73623=CARTESIAN_POINT('Ctrl Pts',(6.30765353814,-42.3742356128,3.12096539428));
#73624=CARTESIAN_POINT('Ctrl Pts',(6.24384247076,-42.3742356128,3.28073264221));
#73625=CARTESIAN_POINT('Ctrl Pts',(6.24384247076,-42.3742356128,3.43894174696));
#73626=CARTESIAN_POINT('Origin',(5.94596381538561,-42.3763569542133,3.43894399659967));
#73627=CARTESIAN_POINT('Ctrl Pts',(6.24384247076,-40.6742356128,3.43894174696));
#73628=CARTESIAN_POINT('Ctrl Pts',(6.24384247076,-42.7142356128,3.43894174696));
#73629=CARTESIAN_POINT('Ctrl Pts',(6.24384247076,-40.6742356128,3.28073264221));
#73630=CARTESIAN_POINT('Ctrl Pts',(6.24384247076,-42.7142356128,3.28073264221));
#73631=CARTESIAN_POINT('Ctrl Pts',(6.30765353814,-40.6742356128,3.12096539428));
#73632=CARTESIAN_POINT('Ctrl Pts',(6.30765353814,-42.7142356128,3.12096539428));
#73633=CARTESIAN_POINT('Ctrl Pts',(6.43081292755,-40.6742356128,2.99918925876));
#73634=CARTESIAN_POINT('Ctrl Pts',(6.43081292755,-42.7142356128,2.99918925876));
#73635=CARTESIAN_POINT('Ctrl Pts',(6.59129069763,-40.6742356128,2.93718674963));
#73636=CARTESIAN_POINT('Ctrl Pts',(6.59129069763,-42.7142356128,2.93718674963));
#73637=CARTESIAN_POINT('Ctrl Pts',(6.74948971107,-40.6742356128,2.9389736393));
#73638=CARTESIAN_POINT('Ctrl Pts',(6.74948971107,-42.7142356128,2.9389736393));
#73639=CARTESIAN_POINT('',(6.74948971107,-41.6742356128,2.9389736393));
#73640=CARTESIAN_POINT('',(6.24384247076,-41.5242356128,3.43894174696));
#73641=CARTESIAN_POINT('Ctrl Pts',(0.487165434784,-42.3742356128,-5.01265134236));
#73642=CARTESIAN_POINT('Ctrl Pts',(0.487165434783,-42.4684833925,-5.01265134236));
#73643=CARTESIAN_POINT('Ctrl Pts',(0.523241153367,-42.5627311721,-5.00438346023));
#73644=CARTESIAN_POINT('Ctrl Pts',(0.595852069376,-42.6372245964,-4.98774239199));
#73645=CARTESIAN_POINT('Ctrl Pts',(0.687718132381,-42.6742356129,-4.96668840305));
#73646=CARTESIAN_POINT('Ctrl Pts',(0.779584195372,-42.6742356128,-4.94563441411));
#73647=CARTESIAN_POINT('Ctrl Pts',(0.81460270388,-42.3742356128,-6.44137631405));
#73648=CARTESIAN_POINT('Ctrl Pts',(0.814602703711,-42.4684833979,-6.44137631333));
#73649=CARTESIAN_POINT('Ctrl Pts',(0.848817867564,-42.562731183,-6.4249900945));
#73650=CARTESIAN_POINT('Ctrl Pts',(0.917683903123,-42.6372246092,-6.39200862181));
#73651=CARTESIAN_POINT('Ctrl Pts',(1.0048120379,-42.6742356214,-6.35028117911));
#73652=CARTESIAN_POINT('Ctrl Pts',(1.09194016947,-42.6742356128,-6.30855373743));
#73653=CARTESIAN_POINT('Ctrl Pts',(1.54487166721,-42.3742356128,-7.77811177525));
#73654=CARTESIAN_POINT('Ctrl Pts',(1.5448713568,-42.4684833875,-7.77811123165));
#73655=CARTESIAN_POINT('Ctrl Pts',(1.57490766806,-42.5627311622,-7.75405190508));
#73656=CARTESIAN_POINT('Ctrl Pts',(1.6353633393,-42.6372245846,-7.70562798343));
#73657=CARTESIAN_POINT('Ctrl Pts',(1.71185094269,-42.6742356051,-7.64436300383));
#73658=CARTESIAN_POINT('Ctrl Pts',(1.7883386711,-42.6742356128,-7.58309823758));
#73659=CARTESIAN_POINT('Ctrl Pts',(2.64459800142,-42.3742356128,-8.86954551869));
#73660=CARTESIAN_POINT('Ctrl Pts',(2.64459795101,-42.468483394,-8.86954558844));
#73661=CARTESIAN_POINT('Ctrl Pts',(2.66838977506,-42.5627311752,-8.83932950434));
#73662=CARTESIAN_POINT('Ctrl Pts',(2.7162764821,-42.6372246,-8.7785122786));
#73663=CARTESIAN_POINT('Ctrl Pts',(2.77686194922,-42.6742356153,-8.70156739678));
#73664=CARTESIAN_POINT('Ctrl Pts',(2.83744743521,-42.6742356128,-8.62462248786));
#73665=CARTESIAN_POINT('Ctrl Pts',(5.32102214868,-42.3742356128,-10.3065086991));
#73666=CARTESIAN_POINT('Ctrl Pts',(5.32102219883,-42.4684833909,-10.3065086297));
#73667=CARTESIAN_POINT('Ctrl Pts',(5.32957386707,-42.562731169,-10.2680846534));
#73668=CARTESIAN_POINT('Ctrl Pts',(5.34678608834,-42.6372245927,-10.1907475223));
#73669=CARTESIAN_POINT('Ctrl Pts',(5.36856264868,-42.6742356104,-10.0929019242));
#73670=CARTESIAN_POINT('Ctrl Pts',(5.39033919025,-42.6742356128,-9.99505635309));
#73671=CARTESIAN_POINT('Ctrl Pts',(8.35327745821,-42.3742356128,-10.1381955831));
#73672=CARTESIAN_POINT('Ctrl Pts',(8.35327740833,-42.468483394,-10.1381956522));
#73673=CARTESIAN_POINT('Ctrl Pts',(8.34456301547,-42.5627311751,-10.1007555191));
#73674=CARTESIAN_POINT('Ctrl Pts',(8.32702327197,-42.6372246,-10.0253981883));
#73675=CARTESIAN_POINT('Ctrl Pts',(8.30483233612,-42.6742356153,-9.93005741943));
#73676=CARTESIAN_POINT('Ctrl Pts',(8.28264141894,-42.6742356128,-9.83471662374));
#73677=CARTESIAN_POINT('Ctrl Pts',(9.80390850636,-42.3742356128,-9.62023799647));
#73678=CARTESIAN_POINT('Ctrl Pts',(9.8039083944,-42.4684833936,-9.62023813852));
#73679=CARTESIAN_POINT('Ctrl Pts',(9.78693869153,-42.5627311743,-9.58574518127));
#73680=CARTESIAN_POINT('Ctrl Pts',(9.7527832879,-42.637224599,-9.51631977282));
#73681=CARTESIAN_POINT('Ctrl Pts',(9.70957053609,-42.6742356146,-9.42848387231));
#73682=CARTESIAN_POINT('Ctrl Pts',(9.66635782899,-42.6742356128,-9.34064791616));
#73683=CARTESIAN_POINT('Ctrl Pts',(12.2505485061,-42.3742356128,-7.83535708458));
#73684=CARTESIAN_POINT('Ctrl Pts',(12.250548618,-42.4684833913,-7.83535694254));
#73685=CARTESIAN_POINT('Ctrl Pts',(12.2196394502,-42.5627311698,-7.81100596215));
#73686=CARTESIAN_POINT('Ctrl Pts',(12.1574273028,-42.6372245937,-7.76199402851));
#73687=CARTESIAN_POINT('Ctrl Pts',(12.0787175117,-42.6742356111,-7.69998507205));
#73688=CARTESIAN_POINT('Ctrl Pts',(12.0000076759,-42.6742356128,-7.63797617123));
#73689=CARTESIAN_POINT('Ctrl Pts',(13.4125693644,-42.3742356128,-5.03814078999));
#73690=CARTESIAN_POINT('Ctrl Pts',(13.4125692525,-42.4684833936,-5.03814093202));
#73691=CARTESIAN_POINT('Ctrl Pts',(13.3750518255,-42.5627311743,-5.02973844738));
#73692=CARTESIAN_POINT('Ctrl Pts',(13.2995392669,-42.637224599,-5.01282628628));
#73693=CARTESIAN_POINT('Ctrl Pts',(13.204002165,-42.6742356146,-4.99142922913));
#73694=CARTESIAN_POINT('Ctrl Pts',(13.1084651078,-42.6742356128,-4.97003211634));
#73695=CARTESIAN_POINT('Ctrl Pts',(13.5759583006,-42.3742356128,-3.50667079674));
#73696=CARTESIAN_POINT('Ctrl Pts',(13.5759583811,-42.4684833893,-3.50667095934));
#73697=CARTESIAN_POINT('Ctrl Pts',(13.5375192988,-42.5627311657,-3.50696861096));
#73698=CARTESIAN_POINT('Ctrl Pts',(13.4601513294,-42.6372245889,-3.50756750816));
#73699=CARTESIAN_POINT('Ctrl Pts',(13.3622667292,-42.6742356079,-3.50832512382));
#73700=CARTESIAN_POINT('Ctrl Pts',(13.2643820967,-42.6742356128,-3.50908267685));
#73701=CARTESIAN_POINT('Ctrl Pts',(13.0288342859,-42.3742356128,-0.519322029858));
#73702=CARTESIAN_POINT('Ctrl Pts',(13.028834205,-42.4684833956,-0.519321866398));
#73703=CARTESIAN_POINT('Ctrl Pts',(12.9934845041,-42.5627311784,-0.536648062284));
#73704=CARTESIAN_POINT('Ctrl Pts',(12.9223350964,-42.6372246039,-0.571521327091));
#73705=CARTESIAN_POINT('Ctrl Pts',(12.8323181043,-42.6742356178,-0.6156424721));
#73706=CARTESIAN_POINT('Ctrl Pts',(12.7423011448,-42.6742356128,-0.659763680066));
#73707=CARTESIAN_POINT('Ctrl Pts',(11.004586804,-42.3742356128,1.74562563294));
#73708=CARTESIAN_POINT('Ctrl Pts',(11.0045868854,-42.4684833892,1.74562546861));
#73709=CARTESIAN_POINT('Ctrl Pts',(10.9807897791,-42.5627311657,1.71542042139));
#73710=CARTESIAN_POINT('Ctrl Pts',(10.9328922473,-42.6372245888,1.65462581836));
#73711=CARTESIAN_POINT('Ctrl Pts',(10.8722931303,-42.6742356078,1.57770964821));
#73712=CARTESIAN_POINT('Ctrl Pts',(10.8116939805,-42.6742356128,1.50079354136));
#73713=CARTESIAN_POINT('Ctrl Pts',(9.68588827029,-42.3742356128,2.55889041883));
#73714=CARTESIAN_POINT('Ctrl Pts',(9.6858884488,-42.4684834004,2.55889048283));
#73715=CARTESIAN_POINT('Ctrl Pts',(9.66954131867,-42.5627311879,2.52404881238));
#73716=CARTESIAN_POINT('Ctrl Pts',(9.63663914597,-42.637224615,2.45392163988));
#73717=CARTESIAN_POINT('Ctrl Pts',(9.5950115686,-42.6742356253,2.36519792666));
#73718=CARTESIAN_POINT('Ctrl Pts',(9.55338392126,-42.6742356128,2.27647419301));
#73719=CARTESIAN_POINT('Ctrl Pts',(8.21519030725,-42.3742356128,2.95553030618));
#73720=CARTESIAN_POINT('Ctrl Pts',(8.21519030799,-42.468483387,2.95553030619));
#73721=CARTESIAN_POINT('Ctrl Pts',(8.20727993006,-42.5627311611,2.91842756273));
#73722=CARTESIAN_POINT('Ctrl Pts',(8.19135808192,-42.6372245834,2.84374951081));
#73723=CARTESIAN_POINT('Ctrl Pts',(8.17121418034,-42.6742356043,2.7492681436));
#73724=CARTESIAN_POINT('Ctrl Pts',(8.15107027851,-42.6742356128,2.65478677305));
#73725=CARTESIAN_POINT('Ctrl Pts',(6.74948971076,-42.3742356128,2.9389736413));
#73726=CARTESIAN_POINT('Ctrl Pts',(6.74948971076,-42.4684833924,2.9389736413));
#73727=CARTESIAN_POINT('Ctrl Pts',(6.74990776683,-42.562731172,2.90196498592));
#73728=CARTESIAN_POINT('Ctrl Pts',(6.75074920355,-42.6372245963,2.82747631396));
#73729=CARTESIAN_POINT('Ctrl Pts',(6.75181377459,-42.6742356128,2.7332345469));
#73730=CARTESIAN_POINT('Ctrl Pts',(6.75287834563,-42.6742356128,2.63899277983));
#73731=CARTESIAN_POINT('',(0.487165436324921,-42.3742356128,-5.01265134230888));
#73732=CARTESIAN_POINT('Origin',(0.777516257206663,-42.3763569108251,-4.9461071823497));
#73733=CARTESIAN_POINT('Ctrl Pts',(0.4871654368,-42.3742356128,-5.0126513422));
#73734=CARTESIAN_POINT('Ctrl Pts',(0.813757598474,-42.3742356128,-6.43768308726));
#73735=CARTESIAN_POINT('Ctrl Pts',(1.54099672242,-42.3742356128,-7.77089360944));
#73736=CARTESIAN_POINT('Ctrl Pts',(2.63582398808,-42.3742356128,-8.86093046307));
#73737=CARTESIAN_POINT('Ctrl Pts',(5.30859738244,-42.3742356128,-10.303702289));
#73738=CARTESIAN_POINT('Ctrl Pts',(8.3416246802,-42.3742356128,-10.1422911046));
#73739=CARTESIAN_POINT('Ctrl Pts',(9.79740146658,-42.3742356128,-9.62504741726));
#73740=CARTESIAN_POINT('Ctrl Pts',(12.2523240225,-42.3742356128,-7.83656666427));
#73741=CARTESIAN_POINT('Ctrl Pts',(13.4155860878,-42.3742356128,-5.03083511496));
#73742=CARTESIAN_POINT('Ctrl Pts',(13.5772083053,-42.3742356128,-3.49437641304));
#73743=CARTESIAN_POINT('Ctrl Pts',(13.0232255151,-42.3742356128,-0.50800550047));
#73744=CARTESIAN_POINT('Ctrl Pts',(10.9941845663,-42.3742356128,1.75214958001));
#73745=CARTESIAN_POINT('Ctrl Pts',(9.67790042305,-42.3742356128,2.56099019349));
#73746=CARTESIAN_POINT('Ctrl Pts',(8.21137385808,-42.3742356128,2.95548591471));
#73747=CARTESIAN_POINT('Ctrl Pts',(6.74948971107,-42.3742356128,2.9389736393));
#73748=CARTESIAN_POINT('Ctrl Pts',(6.74948971107,-40.6742356128,2.9389736393));
#73749=CARTESIAN_POINT('Ctrl Pts',(6.74948971107,-42.7142356128,2.9389736393));
#73750=CARTESIAN_POINT('Ctrl Pts',(8.21137385808,-40.6742356128,2.95548591471));
#73751=CARTESIAN_POINT('Ctrl Pts',(8.21137385808,-42.7142356128,2.95548591471));
#73752=CARTESIAN_POINT('Ctrl Pts',(9.67790042305,-40.6742356128,2.56099019349));
#73753=CARTESIAN_POINT('Ctrl Pts',(9.67790042305,-42.7142356128,2.56099019349));
#73754=CARTESIAN_POINT('Ctrl Pts',(10.9941845663,-40.6742356128,1.75214958001));
#73755=CARTESIAN_POINT('Ctrl Pts',(10.9941845663,-42.7142356128,1.75214958001));
#73756=CARTESIAN_POINT('Ctrl Pts',(13.0232255151,-40.6742356128,-0.50800550047));
#73757=CARTESIAN_POINT('Ctrl Pts',(13.0232255151,-42.7142356128,-0.50800550047));
#73758=CARTESIAN_POINT('Ctrl Pts',(13.5772083053,-40.6742356128,-3.49437641304));
#73759=CARTESIAN_POINT('Ctrl Pts',(13.5772083053,-42.7142356128,-3.49437641304));
#73760=CARTESIAN_POINT('Ctrl Pts',(13.4155860878,-40.6742356128,-5.03083511496));
#73761=CARTESIAN_POINT('Ctrl Pts',(13.4155860878,-42.7142356128,-5.03083511496));
#73762=CARTESIAN_POINT('Ctrl Pts',(12.2523240225,-40.6742356128,-7.83656666427));
#73763=CARTESIAN_POINT('Ctrl Pts',(12.2523240225,-42.7142356128,-7.83656666427));
#73764=CARTESIAN_POINT('Ctrl Pts',(9.79740146658,-40.6742356128,-9.62504741726));
#73765=CARTESIAN_POINT('Ctrl Pts',(9.79740146658,-42.7142356128,-9.62504741726));
#73766=CARTESIAN_POINT('Ctrl Pts',(8.3416246802,-40.6742356128,-10.1422911046));
#73767=CARTESIAN_POINT('Ctrl Pts',(8.3416246802,-42.7142356128,-10.1422911046));
#73768=CARTESIAN_POINT('Ctrl Pts',(5.30859738244,-40.6742356128,-10.303702289));
#73769=CARTESIAN_POINT('Ctrl Pts',(5.30859738244,-42.7142356128,-10.303702289));
#73770=CARTESIAN_POINT('Ctrl Pts',(2.63582398808,-40.6742356128,-8.86093046307));
#73771=CARTESIAN_POINT('Ctrl Pts',(2.63582398808,-42.7142356128,-8.86093046307));
#73772=CARTESIAN_POINT('Ctrl Pts',(1.54099672242,-40.6742356128,-7.77089360944));
#73773=CARTESIAN_POINT('Ctrl Pts',(1.54099672242,-42.7142356128,-7.77089360944));
#73774=CARTESIAN_POINT('Ctrl Pts',(0.813757598474,-40.6742356128,-6.43768308726));
#73775=CARTESIAN_POINT('Ctrl Pts',(0.813757598474,-42.7142356128,-6.43768308726));
#73776=CARTESIAN_POINT('Ctrl Pts',(0.4871654368,-40.6742356128,-5.0126513422));
#73777=CARTESIAN_POINT('Ctrl Pts',(0.4871654368,-42.7142356128,-5.0126513422));
#73778=CARTESIAN_POINT('',(0.4871654368,-41.6742356128,-5.0126513422));
#73779=CARTESIAN_POINT('Ctrl Pts',(-6.10622663544E-16,-42.3742356128,-4.62434669465));
#73780=CARTESIAN_POINT('Ctrl Pts',(-5.82867087928E-16,-42.4684833924,-4.62434669465));
#73781=CARTESIAN_POINT('Ctrl Pts',(-1.33226762955E-15,-42.5627311721,-4.58733567815));
#73782=CARTESIAN_POINT('Ctrl Pts',(-2.69229083472E-15,-42.6372245963,-4.51284225387));
#73783=CARTESIAN_POINT('Ctrl Pts',(-4.55191440096E-15,-42.6742356128,-4.41859447426));
#73784=CARTESIAN_POINT('Ctrl Pts',(-6.27276008913E-15,-42.6742356128,-4.32434669465));
#73785=CARTESIAN_POINT('Ctrl Pts',(0.0757509451836,-42.3742356128,-4.62434669465));
#73786=CARTESIAN_POINT('Ctrl Pts',(0.0757509451836,-42.4684833924,-4.62434669465));
#73787=CARTESIAN_POINT('Ctrl Pts',(0.0814347989626,-42.5627311721,-4.58733567684));
#73788=CARTESIAN_POINT('Ctrl Pts',(0.0928749048103,-42.6372245963,-4.51284225387));
#73789=CARTESIAN_POINT('Ctrl Pts',(0.107348724535,-42.6742356128,-4.41859447426));
#73790=CARTESIAN_POINT('Ctrl Pts',(0.121822544253,-42.6742356128,-4.32434669465));
#73791=CARTESIAN_POINT('Ctrl Pts',(0.152161902464,-42.3742356128,-4.63889679318));
#73792=CARTESIAN_POINT('Ctrl Pts',(0.152161789276,-42.4684833943,-4.63889677644));
#73793=CARTESIAN_POINT('Ctrl Pts',(0.163415494185,-42.5627311758,-4.60297257201));
#73794=CARTESIAN_POINT('Ctrl Pts',(0.186066359196,-42.6372246007,-4.53066662124));
#73795=CARTESIAN_POINT('Ctrl Pts',(0.214723913443,-42.6742356158,-4.43918641142));
#73796=CARTESIAN_POINT('Ctrl Pts',(0.243381511931,-42.6742356128,-4.34770620929));
#73797=CARTESIAN_POINT('Ctrl Pts',(0.224510888247,-42.3742356128,-4.66787112912));
#73798=CARTESIAN_POINT('Ctrl Pts',(0.224510927626,-42.4684833926,-4.66787117042));
#73799=CARTESIAN_POINT('Ctrl Pts',(0.241126667402,-42.5627311724,-4.63407065981));
#73800=CARTESIAN_POINT('Ctrl Pts',(0.27456862703,-42.6372245967,-4.56603424662));
#73801=CARTESIAN_POINT('Ctrl Pts',(0.316879247465,-42.6742356131,-4.47995777227));
#73802=CARTESIAN_POINT('Ctrl Pts',(0.359189852064,-42.6742356128,-4.39388128157));
#73803=CARTESIAN_POINT('Ctrl Pts',(0.339412867472,-42.3742356128,-4.74197790598));
#73804=CARTESIAN_POINT('Ctrl Pts',(0.3394128372,-42.4684833923,-4.74197787423));
#73805=CARTESIAN_POINT('Ctrl Pts',(0.364563818788,-42.5627311718,-4.71367989972));
#73806=CARTESIAN_POINT('Ctrl Pts',(0.415186981668,-42.637224596,-4.656727276));
#73807=CARTESIAN_POINT('Ctrl Pts',(0.479234194727,-42.6742356126,-4.58467027499));
#73808=CARTESIAN_POINT('Ctrl Pts',(0.543281419947,-42.6742356128,-4.51261328653));
#73809=CARTESIAN_POINT('Ctrl Pts',(0.423242092027,-42.3742356128,-4.84894453188));
#73810=CARTESIAN_POINT('Ctrl Pts',(0.423242115298,-42.4684833925,-4.84894455629));
#73811=CARTESIAN_POINT('Ctrl Pts',(0.454600156263,-42.5627311722,-4.82857509388));
#73812=CARTESIAN_POINT('Ctrl Pts',(0.517714979555,-42.6372245966,-4.78757386924));
#73813=CARTESIAN_POINT('Ctrl Pts',(0.597566998874,-42.674235613,-4.73570101093));
#73814=CARTESIAN_POINT('Ctrl Pts',(0.677419008856,-42.6742356128,-4.68382814298));
#73815=CARTESIAN_POINT('Ctrl Pts',(0.452677771562,-42.3742356128,-4.90062212276));
#73816=CARTESIAN_POINT('Ctrl Pts',(0.452677723796,-42.4684833907,-4.90062199961));
#73817=CARTESIAN_POINT('Ctrl Pts',(0.486189267495,-42.5627311685,-4.88403912837));
#73818=CARTESIAN_POINT('Ctrl Pts',(0.553641781761,-42.6372245921,-4.85067372199));
#73819=CARTESIAN_POINT('Ctrl Pts',(0.638980484601,-42.6742356101,-4.80845568264));
#73820=CARTESIAN_POINT('Ctrl Pts',(0.724319207107,-42.6742356128,-4.76623769098));
#73821=CARTESIAN_POINT('Ctrl Pts',(0.474132994671,-42.3742356128,-4.95578655666));
#73822=CARTESIAN_POINT('Ctrl Pts',(0.474132994712,-42.468483392,-4.95578655679));
#73823=CARTESIAN_POINT('Ctrl Pts',(0.509236440803,-42.5627311712,-4.94327645524));
#73824=CARTESIAN_POINT('Ctrl Pts',(0.579888733321,-42.6372245954,-4.91808932499));
#73825=CARTESIAN_POINT('Ctrl Pts',(0.66927749198,-42.6742356122,-4.88622619544));
#73826=CARTESIAN_POINT('Ctrl Pts',(0.75866625092,-42.6742356128,-4.85436306591));
#73827=CARTESIAN_POINT('Ctrl Pts',(0.487165436864,-42.3742356128,-5.01265134225));
#73828=CARTESIAN_POINT('Ctrl Pts',(0.487165436863,-42.4684833925,-5.01265134225));
#73829=CARTESIAN_POINT('Ctrl Pts',(0.52324113624,-42.5627311721,-5.00438337628));
#73830=CARTESIAN_POINT('Ctrl Pts',(0.595852013591,-42.6372245963,-4.98774213931));
#73831=CARTESIAN_POINT('Ctrl Pts',(0.687718027696,-42.6742356128,-4.96668793687));
#73832=CARTESIAN_POINT('Ctrl Pts',(0.779584041801,-42.6742356128,-4.94563373444));
#73833=CARTESIAN_POINT('',(-6.66133814775E-16,-42.3742356128,-4.62434669465));
#73834=CARTESIAN_POINT('Origin',(-6.2003040155756E-7,-42.3763569029672,
-4.32646798455307));
#73835=CARTESIAN_POINT('Ctrl Pts',(-6.66133814775E-16,-42.3742356128,-4.62434669465));
#73836=CARTESIAN_POINT('Ctrl Pts',(0.134351406801,-42.3742356128,-4.62434669465));
#73837=CARTESIAN_POINT('Ctrl Pts',(0.269654391195,-42.3742356128,-4.67008903963));
#73838=CARTESIAN_POINT('Ctrl Pts',(0.38229629568,-42.3742356128,-4.75983578098));
#73839=CARTESIAN_POINT('Ctrl Pts',(0.457108114206,-42.3742356128,-4.88150110685));
#73840=CARTESIAN_POINT('Ctrl Pts',(0.4871654368,-42.3742356128,-5.0126513422));
#73841=CARTESIAN_POINT('Ctrl Pts',(0.4871654368,-40.6742356128,-5.0126513422));
#73842=CARTESIAN_POINT('Ctrl Pts',(0.4871654368,-42.7142356128,-5.0126513422));
#73843=CARTESIAN_POINT('Ctrl Pts',(0.457108114206,-40.6742356128,-4.88150110685));
#73844=CARTESIAN_POINT('Ctrl Pts',(0.457108114206,-42.7142356128,-4.88150110685));
#73845=CARTESIAN_POINT('Ctrl Pts',(0.38229629568,-40.6742356128,-4.75983578098));
#73846=CARTESIAN_POINT('Ctrl Pts',(0.38229629568,-42.7142356128,-4.75983578098));
#73847=CARTESIAN_POINT('Ctrl Pts',(0.269654391195,-40.6742356128,-4.67008903963));
#73848=CARTESIAN_POINT('Ctrl Pts',(0.269654391195,-42.7142356128,-4.67008903963));
#73849=CARTESIAN_POINT('Ctrl Pts',(0.134351406801,-40.6742356128,-4.62434669465));
#73850=CARTESIAN_POINT('Ctrl Pts',(0.134351406801,-42.7142356128,-4.62434669465));
#73851=CARTESIAN_POINT('Ctrl Pts',(-1.11022302463E-15,-40.6742356128,-4.62434669465));
#73852=CARTESIAN_POINT('Ctrl Pts',(-1.11022302463E-15,-42.7142356128,-4.62434669465));
#73853=CARTESIAN_POINT('',(-6.66133814775E-16,-41.6742356128,-4.62434669465));
#73854=CARTESIAN_POINT('Ctrl Pts',(-0.4871654368,-42.3742356128,-5.0126513422));
#73855=CARTESIAN_POINT('Ctrl Pts',(-0.4871654368,-42.4684833924,-5.0126513422));
#73856=CARTESIAN_POINT('Ctrl Pts',(-0.523241147327,-42.5627311721,-5.00438342513));
#73857=CARTESIAN_POINT('Ctrl Pts',(-0.595852047118,-42.6372245963,-4.98774228657));
#73858=CARTESIAN_POINT('Ctrl Pts',(-0.687718089613,-42.6742356128,-4.96668820865));
#73859=CARTESIAN_POINT('Ctrl Pts',(-0.779584132109,-42.6742356128,-4.94563413072));
#73860=CARTESIAN_POINT('Ctrl Pts',(-0.470219247563,-42.3742356128,-4.93870940343));
#73861=CARTESIAN_POINT('Ctrl Pts',(-0.470219247563,-42.4684833924,-4.93870940343));
#73862=CARTESIAN_POINT('Ctrl Pts',(-0.5050271879,-42.5627311721,-4.92490977213));
#73863=CARTESIAN_POINT('Ctrl Pts',(-0.575086395474,-42.6372245963,-4.89713474521));
#73864=CARTESIAN_POINT('Ctrl Pts',(-0.663724083576,-42.6742356128,-4.86199426829));
#73865=CARTESIAN_POINT('Ctrl Pts',(-0.752361771679,-42.6742356128,-4.82685379139));
#73866=CARTESIAN_POINT('Ctrl Pts',(-0.438960828789,-42.3742356128,-4.86744285923));
#73867=CARTESIAN_POINT('Ctrl Pts',(-0.438960870115,-42.4684833944,-4.86744296509));
#73868=CARTESIAN_POINT('Ctrl Pts',(-0.471468366068,-42.562731176,-4.84845573386));
#73869=CARTESIAN_POINT('Ctrl Pts',(-0.536897355711,-42.6372246009,-4.81023932414));
#73870=CARTESIAN_POINT('Ctrl Pts',(-0.619676938308,-42.6742356159,-4.76188852036));
#73871=CARTESIAN_POINT('Ctrl Pts',(-0.70245650358,-42.6742356128,-4.71353767549));
#73872=CARTESIAN_POINT('Ctrl Pts',(-0.394558742266,-42.3742356128,-4.80337215755));
#73873=CARTESIAN_POINT('Ctrl Pts',(-0.394558692852,-42.4684833926,-4.80337212861));
#73874=CARTESIAN_POINT('Ctrl Pts',(-0.42379715787,-42.5627311723,-4.77962978503));
#73875=CARTESIAN_POINT('Ctrl Pts',(-0.482651660681,-42.6372245967,-4.73184272758));
#73876=CARTESIAN_POINT('Ctrl Pts',(-0.557111231681,-42.6742356131,-4.67138339935));
#73877=CARTESIAN_POINT('Ctrl Pts',(-0.631570822294,-42.6742356128,-4.61092408283));
#73878=CARTESIAN_POINT('Ctrl Pts',(-0.296664664887,-42.3742356128,-4.70791349655));
#73879=CARTESIAN_POINT('Ctrl Pts',(-0.296664702856,-42.4684833923,-4.70791351879));
#73880=CARTESIAN_POINT('Ctrl Pts',(-0.318633564797,-42.5627311718,-4.67707994976));
#73881=CARTESIAN_POINT('Ctrl Pts',(-0.362847138464,-42.6372245961,-4.61502009393));
#73882=CARTESIAN_POINT('Ctrl Pts',(-0.418786998681,-42.6742356127,-4.53650302527));
#73883=CARTESIAN_POINT('Ctrl Pts',(-0.474726843846,-42.6742356128,-4.45798594764));
#73884=CARTESIAN_POINT('Ctrl Pts',(-0.173690010613,-42.3742356128,-4.6500860894));
#73885=CARTESIAN_POINT('Ctrl Pts',(-0.173689981439,-42.4684833925,-4.65008607231));
#73886=CARTESIAN_POINT('Ctrl Pts',(-0.186545459408,-42.5627311722,-4.61497252538));
#73887=CARTESIAN_POINT('Ctrl Pts',(-0.212423173742,-42.6372245965,-4.54429820168));
#73888=CARTESIAN_POINT('Ctrl Pts',(-0.245161968871,-42.674235613,-4.45488230314));
#73889=CARTESIAN_POINT('Ctrl Pts',(-0.277900775553,-42.6742356128,-4.36546641149));
#73890=CARTESIAN_POINT('Ctrl Pts',(-0.116772148725,-42.3742356128,-4.63293650019));
#73891=CARTESIAN_POINT('Ctrl Pts',(-0.11677228042,-42.4684833908,-4.63293651935));
#73892=CARTESIAN_POINT('Ctrl Pts',(-0.125457169651,-42.5627311687,-4.59656929085));
#73893=CARTESIAN_POINT('Ctrl Pts',(-0.14292537866,-42.6372245923,-4.52337168016));
#73894=CARTESIAN_POINT('Ctrl Pts',(-0.165030820729,-42.6742356102,-4.43076330315));
#73895=CARTESIAN_POINT('Ctrl Pts',(-0.187136211538,-42.6742356128,-4.33815491762));
#73896=CARTESIAN_POINT('Ctrl Pts',(-0.0582513837293,-42.3742356128,-4.62434672797));
#73897=CARTESIAN_POINT('Ctrl Pts',(-0.0582513835551,-42.4684833921,-4.62434672797));
#73898=CARTESIAN_POINT('Ctrl Pts',(-0.0626101237973,-42.5627311713,-4.58733574114));
#73899=CARTESIAN_POINT('Ctrl Pts',(-0.0713911309205,-42.6372245954,-4.51284233288));
#73900=CARTESIAN_POINT('Ctrl Pts',(-0.0824973438866,-42.6742356122,-4.4185945918));
#73901=CARTESIAN_POINT('Ctrl Pts',(-0.0936035567729,-42.6742356128,-4.32434685045));
#73902=CARTESIAN_POINT('Ctrl Pts',(7.0763099266E-11,-42.3742356128,-4.6243466946));
#73903=CARTESIAN_POINT('Ctrl Pts',(6.59831173003E-11,-42.4684833925,-4.6243466946));
#73904=CARTESIAN_POINT('Ctrl Pts',(-4.72553275957E-8,-42.5627311721,-4.58733567804));
#73905=CARTESIAN_POINT('Ctrl Pts',(-1.42494814745E-7,-42.6372245963,-4.51284225365));
#73906=CARTESIAN_POINT('Ctrl Pts',(-2.62987247912E-7,-42.6742356128,-4.4185944739));
#73907=CARTESIAN_POINT('Ctrl Pts',(-3.8347780408E-7,-42.6742356128,-4.32434669416));
#73908=CARTESIAN_POINT('',(-0.4871654368,-42.3742356128,-5.0126513422));
#73909=CARTESIAN_POINT('Origin',(-0.777515787161492,-42.3763569160989,-4.94610519328655));
#73910=CARTESIAN_POINT('Ctrl Pts',(-0.4871654368,-42.3742356128,-5.0126513422));
#73911=CARTESIAN_POINT('Ctrl Pts',(-0.457108114206,-42.3742356128,-4.88150110685));
#73912=CARTESIAN_POINT('Ctrl Pts',(-0.38229629568,-42.3742356128,-4.75983578098));
#73913=CARTESIAN_POINT('Ctrl Pts',(-0.269654391195,-42.3742356128,-4.67008903963));
#73914=CARTESIAN_POINT('Ctrl Pts',(-0.134351406801,-42.3742356128,-4.62434669465));
#73915=CARTESIAN_POINT('Ctrl Pts',(-6.66133814775E-16,-42.3742356128,-4.62434669465));
#73916=CARTESIAN_POINT('Ctrl Pts',(-6.17561557448E-16,-40.6742356128,-4.62434669465));
#73917=CARTESIAN_POINT('Ctrl Pts',(-6.17561557448E-16,-42.7142356128,-4.62434669465));
#73918=CARTESIAN_POINT('Ctrl Pts',(-0.134351406801,-40.6742356128,-4.62434669465));
#73919=CARTESIAN_POINT('Ctrl Pts',(-0.134351406801,-42.7142356128,-4.62434669465));
#73920=CARTESIAN_POINT('Ctrl Pts',(-0.269654391195,-40.6742356128,-4.67008903963));
#73921=CARTESIAN_POINT('Ctrl Pts',(-0.269654391195,-42.7142356128,-4.67008903963));
#73922=CARTESIAN_POINT('Ctrl Pts',(-0.38229629568,-40.6742356128,-4.75983578098));
#73923=CARTESIAN_POINT('Ctrl Pts',(-0.38229629568,-42.7142356128,-4.75983578098));
#73924=CARTESIAN_POINT('Ctrl Pts',(-0.457108114206,-40.6742356128,-4.88150110685));
#73925=CARTESIAN_POINT('Ctrl Pts',(-0.457108114206,-42.7142356128,-4.88150110685));
#73926=CARTESIAN_POINT('Ctrl Pts',(-0.4871654368,-40.6742356128,-5.0126513422));
#73927=CARTESIAN_POINT('Ctrl Pts',(-0.4871654368,-42.7142356128,-5.0126513422));
#73928=CARTESIAN_POINT('',(-0.4871654368,-41.6742356128,-5.0126513422));
#73929=CARTESIAN_POINT('Ctrl Pts',(-6.74948971107,-42.3742356128,2.9389736393));
#73930=CARTESIAN_POINT('Ctrl Pts',(-6.74948971107,-42.4684833924,2.9389736393));
#73931=CARTESIAN_POINT('Ctrl Pts',(-6.74990773128,-42.5627311721,2.90196498354));
#73932=CARTESIAN_POINT('Ctrl Pts',(-6.75074909582,-42.6372245963,2.82747631079));
#73933=CARTESIAN_POINT('Ctrl Pts',(-6.75181357554,-42.6742356128,2.73323454275));
#73934=CARTESIAN_POINT('Ctrl Pts',(-6.75287805526,-42.6742356128,2.63899277471));
#73935=CARTESIAN_POINT('Ctrl Pts',(-8.20750926282,-42.3742356128,2.95544226333));
#73936=CARTESIAN_POINT('Ctrl Pts',(-8.20750926282,-42.4684833924,2.95544226333));
#73937=CARTESIAN_POINT('Ctrl Pts',(-8.19962531608,-42.5627311721,2.91833983518));
#73938=CARTESIAN_POINT('Ctrl Pts',(-8.18375700837,-42.6372245963,2.84366242333));
#73939=CARTESIAN_POINT('Ctrl Pts',(-8.16368070265,-42.6742356128,2.74918186586));
#73940=CARTESIAN_POINT('Ctrl Pts',(-8.14360439693,-42.6742356128,2.6547013084));
#73941=CARTESIAN_POINT('Ctrl Pts',(-9.67024722863,-42.3742356128,2.5630230066));
#73942=CARTESIAN_POINT('Ctrl Pts',(-9.67024704898,-42.4684833943,2.56302294195));
#73943=CARTESIAN_POINT('Ctrl Pts',(-9.65401144272,-42.5627311758,2.52816442735));
#73944=CARTESIAN_POINT('Ctrl Pts',(-9.62133366522,-42.6372246008,2.45800350109));
#73945=CARTESIAN_POINT('Ctrl Pts',(-9.579990421,-42.6742356158,2.36923716228));
#73946=CARTESIAN_POINT('Ctrl Pts',(-9.53864724787,-42.6742356128,2.28047084985));
#73947=CARTESIAN_POINT('Ctrl Pts',(-10.9836939618,-42.3742356128,1.75867662573));
#73948=CARTESIAN_POINT('Ctrl Pts',(-10.9836938807,-42.4684833913,1.75867678874));
#73949=CARTESIAN_POINT('Ctrl Pts',(-10.9600136456,-42.5627311698,1.72838802594));
#73950=CARTESIAN_POINT('Ctrl Pts',(-10.912351671,-42.6372245937,1.66742452742));
#73951=CARTESIAN_POINT('Ctrl Pts',(-10.852050622,-42.6742356111,1.59029447444));
#73952=CARTESIAN_POINT('Ctrl Pts',(-10.7917496044,-42.6742356128,1.51316435682));
#73953=CARTESIAN_POINT('Ctrl Pts',(-13.0127891544,-42.3742356128,-0.491277894672));
#73954=CARTESIAN_POINT('Ctrl Pts',(-13.0127892356,-42.4684833936,-0.491278057762));
#73955=CARTESIAN_POINT('Ctrl Pts',(-12.9775329168,-42.5627311743,-0.508754582936));
#73956=CARTESIAN_POINT('Ctrl Pts',(-12.9065711376,-42.637224599,-0.543930023858));
#73957=CARTESIAN_POINT('Ctrl Pts',(-12.8167914846,-42.6742356146,-0.588433278065));
#73958=CARTESIAN_POINT('Ctrl Pts',(-12.7270118002,-42.6742356128,-0.632936467611));
#73959=CARTESIAN_POINT('Ctrl Pts',(-13.5757021091,-42.3742356128,-3.4678350886));
#73960=CARTESIAN_POINT('Ctrl Pts',(-13.5757020279,-42.4684833913,-3.46783492542));
#73961=CARTESIAN_POINT('Ctrl Pts',(-13.5372624578,-42.5627311698,-3.46836301962));
#73962=CARTESIAN_POINT('Ctrl Pts',(-13.4598938305,-42.6372245937,-3.46942613318));
#73963=CARTESIAN_POINT('Ctrl Pts',(-13.3620084433,-42.6742356111,-3.47077126553));
#73964=CARTESIAN_POINT('Ctrl Pts',(-13.2641230876,-42.6742356128,-3.47211646258));
#73965=CARTESIAN_POINT('Ctrl Pts',(-13.4210719777,-42.3742356128,-5.00117407132));
#73966=CARTESIAN_POINT('Ctrl Pts',(-13.4210720895,-42.4684833921,-5.00117392804));
#73967=CARTESIAN_POINT('Ctrl Pts',(-13.383504567,-42.5627311713,-4.99297868135));
#73968=CARTESIAN_POINT('Ctrl Pts',(-13.3078909057,-42.6372245955,-4.97648398449));
#73969=CARTESIAN_POINT('Ctrl Pts',(-13.2122257538,-42.6742356123,-4.95561526881));
#73970=CARTESIAN_POINT('Ctrl Pts',(-13.1165605577,-42.6742356128,-4.93474660917));
#73971=CARTESIAN_POINT('Ctrl Pts',(-12.2737890543,-42.3742356128,-7.80629649793));
#73972=CARTESIAN_POINT('Ctrl Pts',(-12.2737889425,-42.4684833928,-7.80629664121));
#73973=CARTESIAN_POINT('Ctrl Pts',(-12.2427485647,-42.5627311728,-7.78211510142));
#73974=CARTESIAN_POINT('Ctrl Pts',(-12.1802726,-42.6372245972,-7.73344385831));
#73975=CARTESIAN_POINT('Ctrl Pts',(-12.1012291684,-42.6742356134,-7.67186576452));
#73976=CARTESIAN_POINT('Ctrl Pts',(-12.022185781,-42.6742356128,-7.61028761468));
#73977=CARTESIAN_POINT('Ctrl Pts',(-9.83534450901,-42.3742356128,-9.60498420728));
#73978=CARTESIAN_POINT('Ctrl Pts',(-9.83534462085,-42.4684833921,-9.604984064));
#73979=CARTESIAN_POINT('Ctrl Pts',(-9.8181953458,-42.5627311713,-9.57057329056));
#73980=CARTESIAN_POINT('Ctrl Pts',(-9.7836782372,-42.6372245955,-9.50131364513));
#73981=CARTESIAN_POINT('Ctrl Pts',(-9.74000772596,-42.6742356123,-9.4136876382));
#73982=CARTESIAN_POINT('Ctrl Pts',(-9.69633717052,-42.6742356128,-9.3260616873));
#73983=CARTESIAN_POINT('Ctrl Pts',(-8.38661907184,-42.3742356128,-10.1306138711));
#73984=CARTESIAN_POINT('Ctrl Pts',(-8.38661911955,-42.4684833948,-10.1306137972));
#73985=CARTESIAN_POINT('Ctrl Pts',(-8.37771609534,-42.5627311767,-10.0932252432));
#73986=CARTESIAN_POINT('Ctrl Pts',(-8.35979658423,-42.6372246018,-10.017971977));
#73987=CARTESIAN_POINT('Ctrl Pts',(-8.33712510637,-42.6742356165,-9.92276292417));
#73988=CARTESIAN_POINT('Ctrl Pts',(-8.3144536084,-42.6742356128,-9.82755390065));
#73989=CARTESIAN_POINT('Ctrl Pts',(-5.34778827807,-42.3742356128,-10.3144544476));
#73990=CARTESIAN_POINT('Ctrl Pts',(-5.34778822992,-42.4684833901,-10.3144545222));
#73991=CARTESIAN_POINT('Ctrl Pts',(-5.35618547139,-42.5627311674,-10.2759765996));
#73992=CARTESIAN_POINT('Ctrl Pts',(-5.37308697531,-42.6372245908,-10.198530638));
#73993=CARTESIAN_POINT('Ctrl Pts',(-5.39447048864,-42.6742356092,-10.1005472936));
#73994=CARTESIAN_POINT('Ctrl Pts',(-5.41585402228,-42.6742356128,-10.0025639196));
#73995=CARTESIAN_POINT('Ctrl Pts',(-2.6588016357,-42.3742356128,-8.88354817531));
#73996=CARTESIAN_POINT('Ctrl Pts',(-2.65880168429,-42.4684833948,-8.88354810004));
#73997=CARTESIAN_POINT('Ctrl Pts',(-2.68251543773,-42.5627311768,-8.85326127917));
#73998=CARTESIAN_POINT('Ctrl Pts',(-2.73024490553,-42.6372246019,-8.79230193136));
#73999=CARTESIAN_POINT('Ctrl Pts',(-2.79063136862,-42.6742356165,-8.71517729568));
#74000=CARTESIAN_POINT('Ctrl Pts',(-2.85101781122,-42.6742356128,-8.63805268983));
#74001=CARTESIAN_POINT('Ctrl Pts',(-1.5511450484,-42.3742356128,-7.78971751005));
#74002=CARTESIAN_POINT('Ctrl Pts',(-1.55114537045,-42.4684833818,-7.78971807464));
#74003=CARTESIAN_POINT('Ctrl Pts',(-1.58113889708,-42.5627311508,-7.76555835799));
#74004=CARTESIAN_POINT('Ctrl Pts',(-1.64150761259,-42.6372245712,-7.71693072276));
#74005=CARTESIAN_POINT('Ctrl Pts',(-1.71788484767,-42.6742355961,-7.65540746012));
#74006=CARTESIAN_POINT('Ctrl Pts',(-1.79426196246,-42.6742356128,-7.59388397371));
#74007=CARTESIAN_POINT('Ctrl Pts',(-0.815993189233,-42.3742356128,-6.44741976998));
#74008=CARTESIAN_POINT('Ctrl Pts',(-0.815993188532,-42.4684833972,-6.44741976695));
#74009=CARTESIAN_POINT('Ctrl Pts',(-0.850205838116,-42.5627311816,-6.43102299012));
#74010=CARTESIAN_POINT('Ctrl Pts',(-0.919066859411,-42.6372246076,-6.39802046996));
#74011=CARTESIAN_POINT('Ctrl Pts',(-1.00618863168,-42.6742356204,-6.35626631563));
#74012=CARTESIAN_POINT('Ctrl Pts',(-1.09331040135,-42.6742356128,-6.31451216314));
#74013=CARTESIAN_POINT('Ctrl Pts',(-0.48716542938,-42.3742356128,-5.01265134292));
#74014=CARTESIAN_POINT('Ctrl Pts',(-0.487165429388,-42.4684833924,-5.01265134296));
#74015=CARTESIAN_POINT('Ctrl Pts',(-0.523241090791,-42.562731172,-5.00438321101));
#74016=CARTESIAN_POINT('Ctrl Pts',(-0.595851891697,-42.6372245963,-4.9877416399));
#74017=CARTESIAN_POINT('Ctrl Pts',(-0.687717809092,-42.6742356128,-4.9666870147));
#74018=CARTESIAN_POINT('Ctrl Pts',(-0.779583726501,-42.6742356128,-4.94563238948));
#74019=CARTESIAN_POINT('',(-6.74948971107,-42.3742356128,2.9389736393));
#74020=CARTESIAN_POINT('Origin',(-6.75285593709817,-42.3763569039433,2.641113951342));
#74021=CARTESIAN_POINT('Ctrl Pts',(-6.74948971107,-42.3742356128,2.9389736393));
#74022=CARTESIAN_POINT('Ctrl Pts',(-8.21137385808,-42.3742356128,2.95548591471));
#74023=CARTESIAN_POINT('Ctrl Pts',(-9.67790042305,-42.3742356128,2.56099019349));
#74024=CARTESIAN_POINT('Ctrl Pts',(-10.9941845663,-42.3742356128,1.75214958001));
#74025=CARTESIAN_POINT('Ctrl Pts',(-13.0232255151,-42.3742356128,-0.50800550047));
#74026=CARTESIAN_POINT('Ctrl Pts',(-13.5772083053,-42.3742356128,-3.49437641304));
#74027=CARTESIAN_POINT('Ctrl Pts',(-13.4155860878,-42.3742356128,-5.03083511496));
#74028=CARTESIAN_POINT('Ctrl Pts',(-12.2523240225,-42.3742356128,-7.83656666427));
#74029=CARTESIAN_POINT('Ctrl Pts',(-9.79740146658,-42.3742356128,-9.62504741726));
#74030=CARTESIAN_POINT('Ctrl Pts',(-8.3416246802,-42.3742356128,-10.1422911046));
#74031=CARTESIAN_POINT('Ctrl Pts',(-5.30859738244,-42.3742356128,-10.303702289));
#74032=CARTESIAN_POINT('Ctrl Pts',(-2.63582398808,-42.3742356128,-8.86093046307));
#74033=CARTESIAN_POINT('Ctrl Pts',(-1.54099672242,-42.3742356128,-7.77089360944));
#74034=CARTESIAN_POINT('Ctrl Pts',(-0.813757598474,-42.3742356128,-6.43768308726));
#74035=CARTESIAN_POINT('Ctrl Pts',(-0.4871654368,-42.3742356128,-5.0126513422));
#74036=CARTESIAN_POINT('Ctrl Pts',(-0.4871654368,-40.6742356128,-5.0126513422));
#74037=CARTESIAN_POINT('Ctrl Pts',(-0.4871654368,-42.7142356128,-5.0126513422));
#74038=CARTESIAN_POINT('Ctrl Pts',(-0.813757598474,-40.6742356128,-6.43768308726));
#74039=CARTESIAN_POINT('Ctrl Pts',(-0.813757598474,-42.7142356128,-6.43768308726));
#74040=CARTESIAN_POINT('Ctrl Pts',(-1.54099672242,-40.6742356128,-7.77089360944));
#74041=CARTESIAN_POINT('Ctrl Pts',(-1.54099672242,-42.7142356128,-7.77089360944));
#74042=CARTESIAN_POINT('Ctrl Pts',(-2.63582398808,-40.6742356128,-8.86093046307));
#74043=CARTESIAN_POINT('Ctrl Pts',(-2.63582398808,-42.7142356128,-8.86093046307));
#74044=CARTESIAN_POINT('Ctrl Pts',(-5.30859738244,-40.6742356128,-10.303702289));
#74045=CARTESIAN_POINT('Ctrl Pts',(-5.30859738244,-42.7142356128,-10.303702289));
#74046=CARTESIAN_POINT('Ctrl Pts',(-8.3416246802,-40.6742356128,-10.1422911046));
#74047=CARTESIAN_POINT('Ctrl Pts',(-8.3416246802,-42.7142356128,-10.1422911046));
#74048=CARTESIAN_POINT('Ctrl Pts',(-9.79740146658,-40.6742356128,-9.62504741726));
#74049=CARTESIAN_POINT('Ctrl Pts',(-9.79740146658,-42.7142356128,-9.62504741726));
#74050=CARTESIAN_POINT('Ctrl Pts',(-12.2523240225,-40.6742356128,-7.83656666427));
#74051=CARTESIAN_POINT('Ctrl Pts',(-12.2523240225,-42.7142356128,-7.83656666427));
#74052=CARTESIAN_POINT('Ctrl Pts',(-13.4155860878,-40.6742356128,-5.03083511496));
#74053=CARTESIAN_POINT('Ctrl Pts',(-13.4155860878,-42.7142356128,-5.03083511496));
#74054=CARTESIAN_POINT('Ctrl Pts',(-13.5772083053,-40.6742356128,-3.49437641304));
#74055=CARTESIAN_POINT('Ctrl Pts',(-13.5772083053,-42.7142356128,-3.49437641304));
#74056=CARTESIAN_POINT('Ctrl Pts',(-13.0232255151,-40.6742356128,-0.50800550047));
#74057=CARTESIAN_POINT('Ctrl Pts',(-13.0232255151,-42.7142356128,-0.50800550047));
#74058=CARTESIAN_POINT('Ctrl Pts',(-10.9941845663,-40.6742356128,1.75214958001));
#74059=CARTESIAN_POINT('Ctrl Pts',(-10.9941845663,-42.7142356128,1.75214958001));
#74060=CARTESIAN_POINT('Ctrl Pts',(-9.67790042305,-40.6742356128,2.56099019349));
#74061=CARTESIAN_POINT('Ctrl Pts',(-9.67790042305,-42.7142356128,2.56099019349));
#74062=CARTESIAN_POINT('Ctrl Pts',(-8.21137385808,-40.6742356128,2.95548591471));
#74063=CARTESIAN_POINT('Ctrl Pts',(-8.21137385808,-42.7142356128,2.95548591471));
#74064=CARTESIAN_POINT('Ctrl Pts',(-6.74948971107,-40.6742356128,2.9389736393));
#74065=CARTESIAN_POINT('Ctrl Pts',(-6.74948971107,-42.7142356128,2.9389736393));
#74066=CARTESIAN_POINT('',(-6.74948971107,-41.6742356128,2.9389736393));
#74067=CARTESIAN_POINT('Ctrl Pts',(-6.24384247076,-42.3742356128,3.43894174696));
#74068=CARTESIAN_POINT('Ctrl Pts',(-6.24384247076,-42.4684833924,3.43894174696));
#74069=CARTESIAN_POINT('Ctrl Pts',(-6.20683145426,-42.5627311721,3.43894174696));
#74070=CARTESIAN_POINT('Ctrl Pts',(-6.13233802997,-42.6372245963,3.43894174696));
#74071=CARTESIAN_POINT('Ctrl Pts',(-6.03809025037,-42.6742356128,3.43894174696));
#74072=CARTESIAN_POINT('Ctrl Pts',(-5.94384247076,-42.6742356128,3.43894174696));
#74073=CARTESIAN_POINT('Ctrl Pts',(-6.24384247076,-42.3742356128,3.34960754815));
#74074=CARTESIAN_POINT('Ctrl Pts',(-6.24384247076,-42.4684833924,3.34960754815));
#74075=CARTESIAN_POINT('Ctrl Pts',(-6.20683145206,-42.5627311721,3.34286426034));
#74076=CARTESIAN_POINT('Ctrl Pts',(-6.13233802997,-42.6372245963,3.32929179344));
#74077=CARTESIAN_POINT('Ctrl Pts',(-6.03809025037,-42.6742356128,3.31212014752));
#74078=CARTESIAN_POINT('Ctrl Pts',(-5.94384247076,-42.6742356128,3.29494850162));
#74079=CARTESIAN_POINT('Ctrl Pts',(-6.26421595059,-42.3742356128,3.2589804315));
#74080=CARTESIAN_POINT('Ctrl Pts',(-6.26421595287,-42.4684833931,3.25898045204));
#74081=CARTESIAN_POINT('Ctrl Pts',(-6.2287301346,-42.5627311733,3.24572127232));
#74082=CARTESIAN_POINT('Ctrl Pts',(-6.15730650956,-42.6372245978,3.21903402757));
#74083=CARTESIAN_POINT('Ctrl Pts',(-6.06694259369,-42.6742356138,3.18526977261));
#74084=CARTESIAN_POINT('Ctrl Pts',(-5.97657867728,-42.6742356128,3.15150550965));
#74085=CARTESIAN_POINT('Ctrl Pts',(-6.30462683184,-42.3742356128,3.17530104105));
#74086=CARTESIAN_POINT('Ctrl Pts',(-6.30462681761,-42.4684833932,3.17530105464));
#74087=CARTESIAN_POINT('Ctrl Pts',(-6.27207337078,-42.5627311736,3.1558302985));
#74088=CARTESIAN_POINT('Ctrl Pts',(-6.20654909404,-42.6372245982,3.11664074649));
#74089=CARTESIAN_POINT('Ctrl Pts',(-6.12365010064,-42.6742356141,3.06705881587));
#74090=CARTESIAN_POINT('Ctrl Pts',(-6.0407511127,-42.6742356128,3.01747688048));
#74091=CARTESIAN_POINT('Ctrl Pts',(-6.40588457178,-42.3742356128,3.0493189246));
#74092=CARTESIAN_POINT('Ctrl Pts',(-6.40588458262,-42.4684833919,3.04931891426));
#74093=CARTESIAN_POINT('Ctrl Pts',(-6.38088701684,-42.5627311709,3.02044994721));
#74094=CARTESIAN_POINT('Ctrl Pts',(-6.33057558549,-42.6372245949,2.96234437914));
#74095=CARTESIAN_POINT('Ctrl Pts',(-6.26692155466,-42.6742356119,2.88883021682));
#74096=CARTESIAN_POINT('Ctrl Pts',(-6.20326751965,-42.6742356128,2.81531605813));
#74097=CARTESIAN_POINT('Ctrl Pts',(-6.54638796335,-42.3742356128,2.97200870323));
#74098=CARTESIAN_POINT('Ctrl Pts',(-6.5463879551,-42.4684833929,2.97200871111));
#74099=CARTESIAN_POINT('Ctrl Pts',(-6.53180837948,-42.562731173,2.93742171773));
#74100=CARTESIAN_POINT('Ctrl Pts',(-6.50246196815,-42.6372245974,2.86780715714));
#74101=CARTESIAN_POINT('Ctrl Pts',(-6.46533406827,-42.6742356135,2.77973204569));
#74102=CARTESIAN_POINT('Ctrl Pts',(-6.42820617159,-42.6742356128,2.69165693147));
#74103=CARTESIAN_POINT('Ctrl Pts',(-6.61266386529,-42.3742356128,2.94923114283));
#74104=CARTESIAN_POINT('Ctrl Pts',(-6.61266384398,-42.4684833903,2.94923114012));
#74105=CARTESIAN_POINT('Ctrl Pts',(-6.60291025736,-42.5627311677,2.91299670879));
#74106=CARTESIAN_POINT('Ctrl Pts',(-6.58328527175,-42.6372245911,2.84006647627));
#74107=CARTESIAN_POINT('Ctrl Pts',(-6.55845341287,-42.6742356094,2.74779636686));
#74108=CARTESIAN_POINT('Ctrl Pts',(-6.53362156228,-42.6742356128,2.65552625724));
#74109=CARTESIAN_POINT('Ctrl Pts',(-6.68140442414,-42.3742356128,2.93820452565));
#74110=CARTESIAN_POINT('Ctrl Pts',(-6.68140442461,-42.4684833933,2.93820452567));
#74111=CARTESIAN_POINT('Ctrl Pts',(-6.67670166275,-42.5627311738,2.90113803996));
#74112=CARTESIAN_POINT('Ctrl Pts',(-6.66723198803,-42.6372245985,2.82653288217));
#74113=CARTESIAN_POINT('Ctrl Pts',(-6.65525290692,-42.6742356142,2.7321437769));
#74114=CARTESIAN_POINT('Ctrl Pts',(-6.64327382563,-42.6742356128,2.63775467212));
#74115=CARTESIAN_POINT('Ctrl Pts',(-6.74948971045,-42.3742356128,2.93897363973));
#74116=CARTESIAN_POINT('Ctrl Pts',(-6.7494897105,-42.4684833925,2.93897363973));
#74117=CARTESIAN_POINT('Ctrl Pts',(-6.74990789497,-42.5627311721,2.90196498613));
#74118=CARTESIAN_POINT('Ctrl Pts',(-6.75074959007,-42.6372245964,2.82747631774));
#74119=CARTESIAN_POINT('Ctrl Pts',(-6.75181448799,-42.6742356129,2.73323455521));
#74120=CARTESIAN_POINT('Ctrl Pts',(-6.7528793859,-42.6742356128,2.63899279271));
#74121=CARTESIAN_POINT('',(-6.24384247076,-42.3742356128,3.43894174696));
#74122=CARTESIAN_POINT('Origin',(-5.94596376190762,-42.3763569039501,3.43894174696));
#74123=CARTESIAN_POINT('Ctrl Pts',(-6.24384247076,-42.3742356128,3.43894174696));
#74124=CARTESIAN_POINT('Ctrl Pts',(-6.24384247076,-42.3742356128,3.28073264221));
#74125=CARTESIAN_POINT('Ctrl Pts',(-6.30765353814,-42.3742356128,3.12096539428));
#74126=CARTESIAN_POINT('Ctrl Pts',(-6.43081292755,-42.3742356128,2.99918925876));
#74127=CARTESIAN_POINT('Ctrl Pts',(-6.59129069763,-42.3742356128,2.93718674963));
#74128=CARTESIAN_POINT('Ctrl Pts',(-6.74948971107,-42.3742356128,2.9389736393));
#74129=CARTESIAN_POINT('Ctrl Pts',(-6.74948971107,-40.6742356128,2.9389736393));
#74130=CARTESIAN_POINT('Ctrl Pts',(-6.74948971107,-42.7142356128,2.9389736393));
#74131=CARTESIAN_POINT('Ctrl Pts',(-6.59129069763,-40.6742356128,2.93718674963));
#74132=CARTESIAN_POINT('Ctrl Pts',(-6.59129069763,-42.7142356128,2.93718674963));
#74133=CARTESIAN_POINT('Ctrl Pts',(-6.43081292755,-40.6742356128,2.99918925876));
#74134=CARTESIAN_POINT('Ctrl Pts',(-6.43081292755,-42.7142356128,2.99918925876));
#74135=CARTESIAN_POINT('Ctrl Pts',(-6.30765353814,-40.6742356128,3.12096539428));
#74136=CARTESIAN_POINT('Ctrl Pts',(-6.30765353814,-42.7142356128,3.12096539428));
#74137=CARTESIAN_POINT('Ctrl Pts',(-6.24384247076,-40.6742356128,3.28073264221));
#74138=CARTESIAN_POINT('Ctrl Pts',(-6.24384247076,-42.7142356128,3.28073264221));
#74139=CARTESIAN_POINT('Ctrl Pts',(-6.24384247076,-40.6742356128,3.43894174696));
#74140=CARTESIAN_POINT('Ctrl Pts',(-6.24384247076,-42.7142356128,3.43894174696));
#74141=CARTESIAN_POINT('',(-6.24384247076,-41.5242356128,3.43894174696));
#74142=CARTESIAN_POINT('Origin',(-5.94384247076,-42.3742356128,1.43032185727));
#74143=CARTESIAN_POINT('',(-6.2438424664575,-42.3742356128,6.9209196413125));
#74144=CARTESIAN_POINT('Origin',(-5.94596379715983,-42.3763569539716,6.92091847872721));
#74145=CARTESIAN_POINT('',(-6.24384247076,-42.3742356128,5.17993069345));
#74146=CARTESIAN_POINT('Origin',(-6.24384247076,-40.6742356128,3.43894174696));
#74147=CARTESIAN_POINT('',(-6.24384247076,-41.6742356128,6.92091963994));
#74148=CARTESIAN_POINT('Ctrl Pts',(-3.99680288865E-15,-42.3742356128,13.1643460036));
#74149=CARTESIAN_POINT('Ctrl Pts',(-3.99680288865E-15,-42.4684833924,13.1643460036));
#74150=CARTESIAN_POINT('Ctrl Pts',(-3.99680288865E-15,-42.5627311721,13.127334987));
#74151=CARTESIAN_POINT('Ctrl Pts',(-3.5527136788E-15,-42.6372245963,13.0528415628));
#74152=CARTESIAN_POINT('Ctrl Pts',(-2.44249065418E-15,-42.6742356128,12.9585937832));
#74153=CARTESIAN_POINT('Ctrl Pts',(-2.22044604925E-15,-42.6742356128,12.8643460036));
#74154=CARTESIAN_POINT('Ctrl Pts',(-0.830355780019,-42.3742356128,13.1643460036));
#74155=CARTESIAN_POINT('Ctrl Pts',(-0.830355780019,-42.4684833924,13.1643460036));
#74156=CARTESIAN_POINT('Ctrl Pts',(-0.825449681018,-42.5627311721,13.1273349871));
#74157=CARTESIAN_POINT('Ctrl Pts',(-0.815574996274,-42.6372245963,13.0528415628));
#74158=CARTESIAN_POINT('Ctrl Pts',(-0.803081717631,-42.6742356128,12.9585937832));
#74159=CARTESIAN_POINT('Ctrl Pts',(-0.790588438987,-42.6742356128,12.8643460036));
#74160=CARTESIAN_POINT('Ctrl Pts',(-1.66094634074,-42.3742356128,13.0267583307));
#74161=CARTESIAN_POINT('Ctrl Pts',(-1.66094608426,-42.4684833982,13.0267583306));
#74162=CARTESIAN_POINT('Ctrl Pts',(-1.65110706951,-42.5627311836,12.9905602371));
#74163=CARTESIAN_POINT('Ctrl Pts',(-1.63130403909,-42.6372246099,12.9177030127));
#74164=CARTESIAN_POINT('Ctrl Pts',(-1.60624974683,-42.6742356219,12.825525327));
#74165=CARTESIAN_POINT('Ctrl Pts',(-1.58119555591,-42.6742356128,12.7333476449));
#74166=CARTESIAN_POINT('Ctrl Pts',(-2.46049232399,-42.3742356128,12.7504708603));
#74167=CARTESIAN_POINT('Ctrl Pts',(-2.46049212731,-42.4684833922,12.7504710156));
#74168=CARTESIAN_POINT('Ctrl Pts',(-2.44590069233,-42.5627311716,12.7159220787));
#74169=CARTESIAN_POINT('Ctrl Pts',(-2.41653221863,-42.6372245958,12.6463839634));
#74170=CARTESIAN_POINT('Ctrl Pts',(-2.37937585833,-42.6742356125,12.5584054672));
#74171=CARTESIAN_POINT('Ctrl Pts',(-2.34221957571,-42.6742356128,12.4704269092));
#74172=CARTESIAN_POINT('Ctrl Pts',(-4.20512684159,-42.3742356128,11.7964487758));
#74173=CARTESIAN_POINT('Ctrl Pts',(-4.20512710956,-42.4684833928,11.7964485642));
#74174=CARTESIAN_POINT('Ctrl Pts',(-4.18019508788,-42.5627311727,11.7675458902));
#74175=CARTESIAN_POINT('Ctrl Pts',(-4.13001317043,-42.6372245971,11.7093727067));
#74176=CARTESIAN_POINT('Ctrl Pts',(-4.06652372142,-42.6742356133,11.6357731294));
#74177=CARTESIAN_POINT('Ctrl Pts',(-4.00303416657,-42.6742356128,11.5621736363));
#74178=CARTESIAN_POINT('Ctrl Pts',(-5.47475449391,-42.3742356128,10.2366927474));
#74179=CARTESIAN_POINT('Ctrl Pts',(-5.47475412882,-42.468483392,10.2366930358));
#74180=CARTESIAN_POINT('Ctrl Pts',(-5.44231202099,-42.5627311712,10.2170346303));
#74181=CARTESIAN_POINT('Ctrl Pts',(-5.37701505136,-42.6372245953,10.1774670535));
#74182=CARTESIAN_POINT('Ctrl Pts',(-5.29440268823,-42.6742356122,10.1274066844));
#74183=CARTESIAN_POINT('Ctrl Pts',(-5.21179046929,-42.6742356128,10.0773462007));
#74184=CARTESIAN_POINT('Ctrl Pts',(-5.98838818076,-42.3742356128,9.18394779498));
#74185=CARTESIAN_POINT('Ctrl Pts',(-5.98838818346,-42.4684833776,9.18394826002));
#74186=CARTESIAN_POINT('Ctrl Pts',(-5.9528871956,-42.5627311424,9.17049598399));
#74187=CARTESIAN_POINT('Ctrl Pts',(-5.88143305972,-42.6372245614,9.14341966516));
#74188=CARTESIAN_POINT('Ctrl Pts',(-5.79103052636,-42.6742355896,9.1091628388));
#74189=CARTESIAN_POINT('Ctrl Pts',(-5.70062798276,-42.6742356128,9.0749058287));
#74190=CARTESIAN_POINT('Ctrl Pts',(-6.24384251168,-42.3742356128,8.05203845412));
#74191=CARTESIAN_POINT('Ctrl Pts',(-6.24384251169,-42.4684833956,8.05203845264));
#74192=CARTESIAN_POINT('Ctrl Pts',(-6.2068314946,-42.5627311784,8.04537359323));
#74193=CARTESIAN_POINT('Ctrl Pts',(-6.13233806792,-42.6372246038,8.03195889811));
#74194=CARTESIAN_POINT('Ctrl Pts',(-6.03809028705,-42.6742356178,8.01498689923));
#74195=CARTESIAN_POINT('Ctrl Pts',(-5.94384250813,-42.6742356128,7.99801490093));
#74196=CARTESIAN_POINT('Ctrl Pts',(-6.24384245355,-42.3742356128,6.9209196436));
#74197=CARTESIAN_POINT('Ctrl Pts',(-6.24384245355,-42.4684833924,6.92091964364));
#74198=CARTESIAN_POINT('Ctrl Pts',(-6.20683143735,-42.562731172,6.92091949894));
#74199=CARTESIAN_POINT('Ctrl Pts',(-6.13233801368,-42.6372245963,6.92091920766));
#74200=CARTESIAN_POINT('Ctrl Pts',(-6.03809023484,-42.6742356128,6.92091883911));
#74201=CARTESIAN_POINT('Ctrl Pts',(-5.94384245598,-42.6742356128,6.92091847055));
#74202=CARTESIAN_POINT('',(3.5527148831751E-15,-42.3742356128,13.1643460036));
#74203=CARTESIAN_POINT('Origin',(-1.89812050115279E-6,-42.3763568746686,
12.8664672572934));
#74204=CARTESIAN_POINT('Ctrl Pts',(3.5527136788E-15,-42.3742356128,13.1643460036));
#74205=CARTESIAN_POINT('Ctrl Pts',(-1.96184634686,-42.3742356128,13.1643460036));
#74206=CARTESIAN_POINT('Ctrl Pts',(-3.92510661379,-42.3742356128,12.3963108842));
#74207=CARTESIAN_POINT('Ctrl Pts',(-5.47580735138,-42.3742356128,10.8456101466));
#74208=CARTESIAN_POINT('Ctrl Pts',(-6.24384247076,-42.3742356128,8.88234987966));
#74209=CARTESIAN_POINT('Ctrl Pts',(-6.24384247076,-42.3742356128,6.92091963994));
#74210=CARTESIAN_POINT('Ctrl Pts',(-6.24384247076,-40.6742356128,6.92091963994));
#74211=CARTESIAN_POINT('Ctrl Pts',(-6.24384247076,-42.7142356128,6.92091963994));
#74212=CARTESIAN_POINT('Ctrl Pts',(-6.24384247076,-40.6742356128,8.88234987966));
#74213=CARTESIAN_POINT('Ctrl Pts',(-6.24384247076,-42.7142356128,8.88234987966));
#74214=CARTESIAN_POINT('Ctrl Pts',(-5.47580735138,-40.6742356128,10.8456101466));
#74215=CARTESIAN_POINT('Ctrl Pts',(-5.47580735138,-42.7142356128,10.8456101466));
#74216=CARTESIAN_POINT('Ctrl Pts',(-3.92510661379,-40.6742356128,12.3963108842));
#74217=CARTESIAN_POINT('Ctrl Pts',(-3.92510661379,-42.7142356128,12.3963108842));
#74218=CARTESIAN_POINT('Ctrl Pts',(-1.96184634686,-40.6742356128,13.1643460036));
#74219=CARTESIAN_POINT('Ctrl Pts',(-1.96184634686,-42.7142356128,13.1643460036));
#74220=CARTESIAN_POINT('Ctrl Pts',(5.44009282066E-15,-40.6742356128,13.1643460036));
#74221=CARTESIAN_POINT('Ctrl Pts',(5.44009282066E-15,-42.7142356128,13.1643460036));
#74222=CARTESIAN_POINT('',(3.5527136788E-15,-41.6742356128,13.1643460036));
#74223=CARTESIAN_POINT('Ctrl Pts',(6.24384247076,-42.3742356128,6.92091963994));
#74224=CARTESIAN_POINT('Ctrl Pts',(6.24384247076,-42.4684833924,6.92091963994));
#74225=CARTESIAN_POINT('Ctrl Pts',(6.20683145426,-42.5627311721,6.92091963994));
#74226=CARTESIAN_POINT('Ctrl Pts',(6.13233802997,-42.6372245963,6.92091963994));
#74227=CARTESIAN_POINT('Ctrl Pts',(6.03809025037,-42.6742356128,6.92091963994));
#74228=CARTESIAN_POINT('Ctrl Pts',(5.94384247076,-42.6742356128,6.92091963994));
#74229=CARTESIAN_POINT('Ctrl Pts',(6.24384247076,-42.3742356128,7.75113701566));
#74230=CARTESIAN_POINT('Ctrl Pts',(6.24384247076,-42.4684833924,7.75113701566));
#74231=CARTESIAN_POINT('Ctrl Pts',(6.20683145426,-42.5627311721,7.74622965293));
#74232=CARTESIAN_POINT('Ctrl Pts',(6.13233802997,-42.6372245963,7.73635242463));
#74233=CARTESIAN_POINT('Ctrl Pts',(6.03809025037,-42.6742356128,7.72385592793));
#74234=CARTESIAN_POINT('Ctrl Pts',(5.94384247076,-42.6742356128,7.71135943123));
#74235=CARTESIAN_POINT('Ctrl Pts',(6.10624229678,-42.3742356128,8.58162297024));
#74236=CARTESIAN_POINT('Ctrl Pts',(6.10624229668,-42.4684833981,8.58162271341));
#74237=CARTESIAN_POINT('Ctrl Pts',(6.07004462212,-42.5627311834,8.5717822858));
#74238=CARTESIAN_POINT('Ctrl Pts',(5.99718824085,-42.6372246097,8.55197641205));
#74239=CARTESIAN_POINT('Ctrl Pts',(5.90501162182,-42.6742356217,8.52691852269));
#74240=CARTESIAN_POINT('Ctrl Pts',(5.81283500628,-42.6742356128,8.50186073478));
#74241=CARTESIAN_POINT('Ctrl Pts',(5.82995657026,-42.3742356128,9.38108114077));
#74242=CARTESIAN_POINT('Ctrl Pts',(5.82995672559,-42.4684833923,9.38108094408));
#74243=CARTESIAN_POINT('Ctrl Pts',(5.79540828589,-42.5627311717,9.36648855896));
#74244=CARTESIAN_POINT('Ctrl Pts',(5.72587117149,-42.6372245959,9.3371181729));
#74245=CARTESIAN_POINT('Ctrl Pts',(5.63789394152,-42.6742356126,9.29995939314));
#74246=CARTESIAN_POINT('Ctrl Pts',(5.54991664977,-42.6742356128,9.26280069107));
#74247=CARTESIAN_POINT('Ctrl Pts',(4.87592249919,-42.3742356128,11.1256648367));
#74248=CARTESIAN_POINT('Ctrl Pts',(4.87592228753,-42.4684833927,11.1256651047));
#74249=CARTESIAN_POINT('Ctrl Pts',(4.84702017121,-42.5627311725,11.1007324623));
#74250=CARTESIAN_POINT('Ctrl Pts',(4.78884811012,-42.6372245969,11.0505492956));
#74251=CARTESIAN_POINT('Ctrl Pts',(4.71524995296,-42.6742356132,10.9870582659));
#74252=CARTESIAN_POINT('Ctrl Pts',(4.64165187997,-42.6742356128,10.9235671304));
#74253=CARTESIAN_POINT('Ctrl Pts',(3.31613637806,-42.3742356128,12.395285601));
#74254=CARTESIAN_POINT('Ctrl Pts',(3.31613666647,-42.4684833921,12.3952852358));
#74255=CARTESIAN_POINT('Ctrl Pts',(3.29647895881,-42.5627311714,12.3628425782));
#74256=CARTESIAN_POINT('Ctrl Pts',(3.25691278652,-42.6372245955,12.2975445024));
#74257=CARTESIAN_POINT('Ctrl Pts',(3.20685419435,-42.6742356123,12.2149307397));
#74258=CARTESIAN_POINT('Ctrl Pts',(3.15679548747,-42.6742356128,12.1323171213));
#74259=CARTESIAN_POINT('Ctrl Pts',(2.26330649455,-42.3742356128,12.9089230556));
#74260=CARTESIAN_POINT('Ctrl Pts',(2.26330695882,-42.4684833774,12.9089230583));
#74261=CARTESIAN_POINT('Ctrl Pts',(2.24985627251,-42.5627311421,12.8734212448));
#74262=CARTESIAN_POINT('Ctrl Pts',(2.22278315419,-42.637224561,12.8019654469));
#74263=CARTESIAN_POINT('Ctrl Pts',(2.18853037756,-42.6742355893,12.7115608108));
#74264=CARTESIAN_POINT('Ctrl Pts',(2.15427741744,-42.6742356128,12.6211561643));
#74265=CARTESIAN_POINT('Ctrl Pts',(1.13128927566,-42.3742356128,13.1643460756));
#74266=CARTESIAN_POINT('Ctrl Pts',(1.13128927419,-42.4684833956,13.1643460756));
#74267=CARTESIAN_POINT('Ctrl Pts',(1.12462623999,-42.5627311784,13.127335058));
#74268=CARTESIAN_POINT('Ctrl Pts',(1.11121521855,-42.6372246038,13.0528416302));
#74269=CARTESIAN_POINT('Ctrl Pts',(1.09424786752,-42.6742356178,12.958593848));
#74270=CARTESIAN_POINT('Ctrl Pts',(1.07728051707,-42.6742356128,12.8643460678));
#74271=CARTESIAN_POINT('Ctrl Pts',(3.77707154442E-9,-42.3742356128,13.1643459857));
#74272=CARTESIAN_POINT('Ctrl Pts',(3.8111913625E-9,-42.4684833924,13.1643459857));
#74273=CARTESIAN_POINT('Ctrl Pts',(-1.41464807424E-7,-42.562731172,13.1273349695));
#74274=CARTESIAN_POINT('Ctrl Pts',(-4.33908818209E-7,-42.6372245963,13.0528415459));
#74275=CARTESIAN_POINT('Ctrl Pts',(-8.03924593562E-7,-42.6742356128,12.9585937671));
#74276=CARTESIAN_POINT('Ctrl Pts',(-1.17395376664E-6,-42.6742356128,12.8643459882));
#74277=CARTESIAN_POINT('',(6.24384247076,-42.3742356128,6.92091963994));
#74278=CARTESIAN_POINT('Origin',(5.94596376190762,-42.3763569039501,6.92091963994));
#74279=CARTESIAN_POINT('Ctrl Pts',(6.24384247076,-42.3742356128,6.92091963994));
#74280=CARTESIAN_POINT('Ctrl Pts',(6.24384247076,-42.3742356128,8.88234987966));
#74281=CARTESIAN_POINT('Ctrl Pts',(5.47580735138,-42.3742356128,10.8456101466));
#74282=CARTESIAN_POINT('Ctrl Pts',(3.92510661379,-42.3742356128,12.3963108842));
#74283=CARTESIAN_POINT('Ctrl Pts',(1.96184634686,-42.3742356128,13.1643460036));
#74284=CARTESIAN_POINT('Ctrl Pts',(3.5527136788E-15,-42.3742356128,13.1643460036));
#74285=CARTESIAN_POINT('Ctrl Pts',(5.55111512313E-15,-40.6742356128,13.1643460036));
#74286=CARTESIAN_POINT('Ctrl Pts',(5.55111512313E-15,-42.7142356128,13.1643460036));
#74287=CARTESIAN_POINT('Ctrl Pts',(1.96184634686,-40.6742356128,13.1643460036));
#74288=CARTESIAN_POINT('Ctrl Pts',(1.96184634686,-42.7142356128,13.1643460036));
#74289=CARTESIAN_POINT('Ctrl Pts',(3.92510661379,-40.6742356128,12.3963108842));
#74290=CARTESIAN_POINT('Ctrl Pts',(3.92510661379,-42.7142356128,12.3963108842));
#74291=CARTESIAN_POINT('Ctrl Pts',(5.47580735138,-40.6742356128,10.8456101466));
#74292=CARTESIAN_POINT('Ctrl Pts',(5.47580735138,-42.7142356128,10.8456101466));
#74293=CARTESIAN_POINT('Ctrl Pts',(6.24384247076,-40.6742356128,8.88234987966));
#74294=CARTESIAN_POINT('Ctrl Pts',(6.24384247076,-42.7142356128,8.88234987966));
#74295=CARTESIAN_POINT('Ctrl Pts',(6.24384247076,-40.6742356128,6.92091963994));
#74296=CARTESIAN_POINT('Ctrl Pts',(6.24384247076,-42.7142356128,6.92091963994));
#74297=CARTESIAN_POINT('',(6.24384247076,-41.5242356128,6.92091963994));
#74298=CARTESIAN_POINT('Origin',(5.94384247076,-42.3742356128,1.43032185727));
#74299=CARTESIAN_POINT('',(6.24384247076,-42.3742356128,5.17993069345));
#74300=CARTESIAN_POINT('Origin',(6.24384247076,-40.6742356128,6.92091963994));
#74301=CARTESIAN_POINT('',(0.,0.,0.));
#74302=CARTESIAN_POINT('Origin',(-3.35265884719E-30,-38.2742356128,3.15283103411E-22));
#74303=CARTESIAN_POINT('',(-2.02924878182,-38.2742356128,-3.59534899368));
#74304=CARTESIAN_POINT('',(-1.71727342606,-38.2742356128,-3.85789277743));
#74305=CARTESIAN_POINT('Ctrl Pts',(-2.02924878182,-38.2742356128,-3.59534899368));
#74306=CARTESIAN_POINT('Ctrl Pts',(-1.93266642605,-38.2742356128,-3.68930297977));
#74307=CARTESIAN_POINT('Ctrl Pts',(-1.82884081082,-38.2742356128,-3.77671908511));
#74308=CARTESIAN_POINT('Ctrl Pts',(-1.71727342605654,-38.2742356128,-3.85789277742524));
#74309=CARTESIAN_POINT('',(-1.71727342606,-38.2742356128,-3.68636669298));
#74310=CARTESIAN_POINT('',(-1.71727342606,-38.2742356128,0.));
#74311=CARTESIAN_POINT('Origin',(4.8544501751735E-13,-38.2742356128,2.77999550541204));
#74312=CARTESIAN_POINT('Origin',(-6.28286804938E-15,-37.6642356128,2.77999550541));
#74313=CARTESIAN_POINT('',(-2.02924878182,-39.7742356128,-3.59534899368));
#74314=CARTESIAN_POINT('',(-2.02924878182,-38.7792356128,-3.59534899368));
#74315=CARTESIAN_POINT('',(-1.71727342606,-39.7742356128,-3.68636669298));
#74316=CARTESIAN_POINT('',(-1.71727342606,-38.7792356128,-3.68636669298));
#74317=CARTESIAN_POINT('Origin',(-6.28286804938E-15,-39.7742356128,2.77999550541));
#74318=CARTESIAN_POINT('Origin',(-1.71727342606,-39.2742356128,-2.86512409447));
#74319=CARTESIAN_POINT('',(-1.71727342606,-39.7742356128,-3.85789277743));
#74320=CARTESIAN_POINT('',(-1.71727342606,-38.2792356128,-3.85789277743));
#74321=CARTESIAN_POINT('',(-1.71727342606,-39.7742356128,-5.61958386968));
#74322=CARTESIAN_POINT('Ctrl Pts',(-2.02924878182,-39.7742356128,-3.59534899368));
#74323=CARTESIAN_POINT('Ctrl Pts',(-2.02924878182,-37.9742356128,-3.59534899368));
#74324=CARTESIAN_POINT('Ctrl Pts',(-1.93266642605,-39.7742356128,-3.68930297977));
#74325=CARTESIAN_POINT('Ctrl Pts',(-1.93266642605,-37.9742356128,-3.68930297977));
#74326=CARTESIAN_POINT('Ctrl Pts',(-1.82884081082,-39.7742356128,-3.77671908511));
#74327=CARTESIAN_POINT('Ctrl Pts',(-1.82884081082,-37.9742356128,-3.77671908511));
#74328=CARTESIAN_POINT('Ctrl Pts',(-1.71727342605,-39.7742356128,-3.85789277743));
#74329=CARTESIAN_POINT('Ctrl Pts',(-1.71727342605,-37.9742356128,-3.85789277743));
#74330=CARTESIAN_POINT('Ctrl Pts',(-2.02924878182,-39.7742356128,-3.59534899368));
#74331=CARTESIAN_POINT('Ctrl Pts',(-1.93266642605,-39.7742356128,-3.68930297977));
#74332=CARTESIAN_POINT('Ctrl Pts',(-1.82884081082,-39.7742356128,-3.77671908511));
#74333=CARTESIAN_POINT('Ctrl Pts',(-1.71727342605654,-39.7742356128,-3.85789277742524));
#74334=CARTESIAN_POINT('Origin',(-3.35265884719E-30,-39.7742356128,3.15283103411E-22));
#74335=CARTESIAN_POINT('Origin',(-3.35265884719E-30,-38.2742356128,3.15283103411E-22));
#74336=CARTESIAN_POINT('',(2.02924878231356,-38.2742356128,-3.59534899352193));
#74337=CARTESIAN_POINT('',(1.71727342605667,-38.2742356128,-3.85789277798081));
#74338=CARTESIAN_POINT('Ctrl Pts',(2.02924878182,-38.2742356128,-3.59534899368));
#74339=CARTESIAN_POINT('Ctrl Pts',(1.93266642605,-38.2742356128,-3.68930297977));
#74340=CARTESIAN_POINT('Ctrl Pts',(1.82884081082,-38.2742356128,-3.77671908511));
#74341=CARTESIAN_POINT('Ctrl Pts',(1.71727342605,-38.2742356128,-3.85789277743));
#74342=CARTESIAN_POINT('',(1.71727342606,-38.2742356128,-3.68636669298));
#74343=CARTESIAN_POINT('Origin',(-3.60822483003176E-15,-38.2742356128,2.7799955054097));
#74344=CARTESIAN_POINT('',(1.71727342606,-38.2742356128,0.));
#74345=CARTESIAN_POINT('Origin',(1.71727342606,-39.2742356128,-2.86512409447));
#74346=CARTESIAN_POINT('',(1.71727342606,-39.7742356128,-3.68636669298));
#74347=CARTESIAN_POINT('',(1.71727342606,-38.2792356128,-3.68636669298));
#74348=CARTESIAN_POINT('',(1.71727342606,-39.7742356128,-3.85789277743));
#74349=CARTESIAN_POINT('',(1.71727342606,-39.7742356128,-5.61958386968));
#74350=CARTESIAN_POINT('',(1.71727342606,-38.2792356128,-3.85789277743));
#74351=CARTESIAN_POINT('Origin',(6.28286804938E-15,-37.6642356128,2.77999550541));
#74352=CARTESIAN_POINT('',(2.02924878182,-39.7742356128,-3.59534899368));
#74353=CARTESIAN_POINT('',(2.02924878182,-38.7792356128,-3.59534899368));
#74354=CARTESIAN_POINT('Origin',(6.28286804938E-15,-39.7742356128,2.77999550541));
#74355=CARTESIAN_POINT('Ctrl Pts',(2.02924878182,-39.7742356128,-3.59534899368));
#74356=CARTESIAN_POINT('Ctrl Pts',(2.02924878182,-37.9742356128,-3.59534899368));
#74357=CARTESIAN_POINT('Ctrl Pts',(1.93266642605,-39.7742356128,-3.68930297977));
#74358=CARTESIAN_POINT('Ctrl Pts',(1.93266642605,-37.9742356128,-3.68930297977));
#74359=CARTESIAN_POINT('Ctrl Pts',(1.82884081082,-39.7742356128,-3.77671908511));
#74360=CARTESIAN_POINT('Ctrl Pts',(1.82884081082,-37.9742356128,-3.77671908511));
#74361=CARTESIAN_POINT('Ctrl Pts',(1.71727342605,-39.7742356128,-3.85789277743));
#74362=CARTESIAN_POINT('Ctrl Pts',(1.71727342605,-37.9742356128,-3.85789277743));
#74363=CARTESIAN_POINT('Ctrl Pts',(2.02924878182,-39.7742356128,-3.59534899368));
#74364=CARTESIAN_POINT('Ctrl Pts',(1.93266642605,-39.7742356128,-3.68930297977));
#74365=CARTESIAN_POINT('Ctrl Pts',(1.82884081082,-39.7742356128,-3.77671908511));
#74366=CARTESIAN_POINT('Ctrl Pts',(1.71727342605654,-39.7742356128,-3.85789277742524));
#74367=CARTESIAN_POINT('Origin',(-3.35265884719E-30,-39.7742356128,3.15283103411E-22));
#74368=CARTESIAN_POINT('Origin',(0.000416107150126,-40.1142356128,6.92091963994));
#74369=CARTESIAN_POINT('',(4.44384247076,-41.6742356128,6.92091963994));
#74370=CARTESIAN_POINT('',(-0.000416107140392043,-41.6742356128,11.3643459775889));
#74371=CARTESIAN_POINT('Origin',(0.000416107150126,-41.6742356128,6.92091963994));
#74372=CARTESIAN_POINT('',(-0.000416107136785584,-39.7742356128,11.3643459650651));
#74373=CARTESIAN_POINT('',(-0.000416107150125,-40.1142356128,11.3643460036));
#74374=CARTESIAN_POINT('',(3.64378781517,-39.7742356128,9.46451560746));
#74375=CARTESIAN_POINT('Origin',(0.000416107150126,-39.7742356128,6.92091963994));
#74376=CARTESIAN_POINT('',(4.44384247076,-39.7742356128,6.92091963994));
#74377=CARTESIAN_POINT('Origin',(0.000416107150126,-39.7742356128,6.92091963994));
#74378=CARTESIAN_POINT('',(4.44384247076,-40.1142356128,6.92091963994));
#74379=CARTESIAN_POINT('Origin',(-0.000416107150126,-40.1142356128,6.92091963994));
#74380=CARTESIAN_POINT('',(0.000416107143369473,-40.6742356128,13.1643459761606));
#74381=CARTESIAN_POINT('',(-6.24384247076,-40.6742356128,6.92091963994));
#74382=CARTESIAN_POINT('Origin',(-0.000416107150126,-40.6742356128,6.92091963994));
#74383=CARTESIAN_POINT('',(0.000416107145187488,-41.6742356128,13.1643459850784));
#74384=CARTESIAN_POINT('',(0.000416107150124,-40.1142356128,13.1643460036));
#74385=CARTESIAN_POINT('',(-6.24384247076,-41.6742356128,6.92091963994));
#74386=CARTESIAN_POINT('Origin',(-0.000416107150126,-41.6742356128,6.92091963994));
#74387=CARTESIAN_POINT('',(-6.24384247076,-40.1142356128,6.92091963994));
#74388=CARTESIAN_POINT('Origin',(6.86146892388,-41.6742356128,4.85630581709));
#74389=CARTESIAN_POINT('',(7.34384247076,-41.6742356128,5.03150262953));
#74390=CARTESIAN_POINT('',(7.34384247076,-39.7742356128,5.03150262895));
#74391=CARTESIAN_POINT('',(7.34384247076,-40.7242356128,5.03150262895));
#74392=CARTESIAN_POINT('',(13.5647513306,-39.7742356128,7.2909204726));
#74393=CARTESIAN_POINT('',(10.4542969007,-39.7742356128,6.16121155078));
#74394=CARTESIAN_POINT('',(14.2293511975,-39.7742356128,7.53230140778));
#74395=CARTESIAN_POINT('',(13.8970512641,-39.7742356128,7.41161094019));
#74396=CARTESIAN_POINT('',(14.2293511975,-41.6742356128,7.53230140778));
#74397=CARTESIAN_POINT('',(14.2293511975,-40.7242356128,7.53230140778));
#74398=CARTESIAN_POINT('',(10.7865968341,-41.6742356128,6.28190201837));
#74399=CARTESIAN_POINT('Origin',(-3.35265884719E-30,-41.6742356128,3.15283103411E-22));
#74400=CARTESIAN_POINT('',(-16.2234398325,-41.6742356128,-2.4));
#74401=CARTESIAN_POINT('',(-17.2336839201,-41.6742356128,-2.4));
#74402=CARTESIAN_POINT('',(-16.7285618762,-41.6742356128,-2.4));
#74403=CARTESIAN_POINT('',(-17.0705772097,-41.6742356128,-3.4));
#74404=CARTESIAN_POINT('Ctrl Pts',(-17.0705772097,-41.6742356128,-3.4));
#74405=CARTESIAN_POINT('Ctrl Pts',(-17.1142405474,-41.6742356128,-3.15603772018));
#74406=CARTESIAN_POINT('Ctrl Pts',(-17.1569007064,-41.6742356128,-2.91066121221));
#74407=CARTESIAN_POINT('Ctrl Pts',(-17.1980377987,-41.6742356128,-2.65606214167));
#74408=CARTESIAN_POINT('Ctrl Pts',(-17.2336839201,-41.6742356128,-2.4));
#74409=CARTESIAN_POINT('',(-17.0645832062,-41.6742356128,-3.4));
#74410=CARTESIAN_POINT('',(-17.067580208,-41.6742356128,-3.4));
#74411=CARTESIAN_POINT('',(17.0645832062,-41.6742356128,-3.4));
#74412=CARTESIAN_POINT('Origin',(-3.5527136788E-15,-41.6742356128,-8.88178104417E-16));
#74413=CARTESIAN_POINT('',(17.0705772097,-41.6742356128,-3.4));
#74414=CARTESIAN_POINT('',(17.067580208,-41.6742356128,-3.4));
#74415=CARTESIAN_POINT('',(17.2336839201,-41.6742356128,-2.4));
#74416=CARTESIAN_POINT('Ctrl Pts',(17.0705772097,-41.6742356128,-3.4));
#74417=CARTESIAN_POINT('Ctrl Pts',(17.1142405474,-41.6742356128,-3.15603772018));
#74418=CARTESIAN_POINT('Ctrl Pts',(17.1569007064,-41.6742356128,-2.91066121221));
#74419=CARTESIAN_POINT('Ctrl Pts',(17.1980377987,-41.6742356128,-2.65606214167));
#74420=CARTESIAN_POINT('Ctrl Pts',(17.2336839201,-41.6742356128,-2.39999999999));
#74421=CARTESIAN_POINT('',(16.2234398325,-41.6742356128,-2.4));
#74422=CARTESIAN_POINT('',(16.7285618762,-41.6742356128,-2.4));
#74423=CARTESIAN_POINT('',(16.2234398325,-41.6742356128,2.4));
#74424=CARTESIAN_POINT('Origin',(-3.35265884719E-30,-41.6742356128,3.15283103411E-22));
#74425=CARTESIAN_POINT('',(17.2336839201,-41.6742356128,2.4));
#74426=CARTESIAN_POINT('',(16.7285618762,-41.6742356128,2.4));
#74427=CARTESIAN_POINT('',(17.0705772096,-41.6742356128,3.4));
#74428=CARTESIAN_POINT('Ctrl Pts',(17.2336839201,-41.6742356128,2.39999999999));
#74429=CARTESIAN_POINT('Ctrl Pts',(17.1980377987,-41.6742356128,2.65606214167));
#74430=CARTESIAN_POINT('Ctrl Pts',(17.1569007064,-41.6742356128,2.91066121221));
#74431=CARTESIAN_POINT('Ctrl Pts',(17.1142405474,-41.6742356128,3.15603772019));
#74432=CARTESIAN_POINT('Ctrl Pts',(17.0705772097,-41.6742356128,3.40000000002));
#74433=CARTESIAN_POINT('',(17.0645832062,-41.6742356128,3.4));
#74434=CARTESIAN_POINT('',(17.0675802079,-41.6742356128,3.4));
#74435=CARTESIAN_POINT('',(-17.0645832062,-41.6742356128,3.4));
#74436=CARTESIAN_POINT('Origin',(-3.5527136788E-15,-41.6742356128,-8.88178104417E-16));
#74437=CARTESIAN_POINT('',(-17.0705772096,-41.6742356128,3.4));
#74438=CARTESIAN_POINT('',(-17.0675802079,-41.6742356128,3.4));
#74439=CARTESIAN_POINT('',(-17.2336839201,-41.6742356128,2.4));
#74440=CARTESIAN_POINT('Ctrl Pts',(-17.2336839201,-41.6742356128,2.39999999999));
#74441=CARTESIAN_POINT('Ctrl Pts',(-17.1980377987,-41.6742356128,2.65606214167));
#74442=CARTESIAN_POINT('Ctrl Pts',(-17.1569007064,-41.6742356128,2.91066121221));
#74443=CARTESIAN_POINT('Ctrl Pts',(-17.1142405474,-41.6742356128,3.15603772019));
#74444=CARTESIAN_POINT('Ctrl Pts',(-17.0705772097,-41.6742356128,3.40000000002));
#74445=CARTESIAN_POINT('',(-16.2234398325,-41.6742356128,2.4));
#74446=CARTESIAN_POINT('',(-16.7285618762,-41.6742356128,2.4));
#74447=CARTESIAN_POINT('Origin',(-3.35265884719E-30,-41.6742356128,3.15283103411E-22));
#74448=CARTESIAN_POINT('',(-14.4212065313,-41.6742356128,-3.4));
#74449=CARTESIAN_POINT('',(-15.7368993134,-41.6742356128,-3.4));
#74450=CARTESIAN_POINT('',(-15.0790529224,-41.6742356128,-3.4));
#74451=CARTESIAN_POINT('',(-0.174946252184,-41.6742356128,-7.24363497156));
#74452=CARTESIAN_POINT('Origin',(-6.82290383517,-41.6742356128,-3.56061176027));
#74453=CARTESIAN_POINT('',(0.174946252184,-41.6742356128,-7.24363497156));
#74454=CARTESIAN_POINT('Origin',(1.44328993201E-15,-41.6742356128,-7.34055663501));
#74455=CARTESIAN_POINT('',(14.4212065313,-41.6742356128,-3.4));
#74456=CARTESIAN_POINT('Origin',(6.82290383517,-41.6742356128,-3.56061176027));
#74457=CARTESIAN_POINT('',(15.7368993134,-41.6742356128,-3.4));
#74458=CARTESIAN_POINT('',(15.0790529224,-41.6742356128,-3.4));
#74459=CARTESIAN_POINT('Origin',(-3.5527136788E-15,-41.6742356128,-8.88178104417E-16));
#74460=CARTESIAN_POINT('',(-7.52535686472,-41.6742356128,4.00685543432));
#74461=CARTESIAN_POINT('',(-7.34384247076,-41.6742356128,4.20599930786));
#74462=CARTESIAN_POINT('Origin',(-7.54384247076,-41.6742356128,4.20599930786));
#74463=CARTESIAN_POINT('',(-14.2514385284,-41.6742356128,-1.95534782199));
#74464=CARTESIAN_POINT('Origin',(-6.82290383517,-41.6742356128,-3.56061176027));
#74465=CARTESIAN_POINT('',(-14.251438528,-41.6742356128,3.4));
#74466=CARTESIAN_POINT('',(-14.2514385284,-41.6742356128,0.722326088933));
#74467=CARTESIAN_POINT('',(-15.7368993134,-41.6742356128,3.4));
#74468=CARTESIAN_POINT('',(-14.9941689207,-41.6742356128,3.4));
#74469=CARTESIAN_POINT('',(-14.2293511975,-41.6742356128,7.53230140778));
#74470=CARTESIAN_POINT('Origin',(-3.5527136788E-15,-41.6742356128,-8.88178104417E-16));
#74471=CARTESIAN_POINT('',(-7.34384247076,-41.6742356128,5.03150262953));
#74472=CARTESIAN_POINT('',(-10.7865968341,-41.6742356128,6.28190201837));
#74473=CARTESIAN_POINT('',(-7.34384247076,-41.6742356128,4.61875096898));
#74474=CARTESIAN_POINT('',(15.7368993134,-41.6742356128,3.4));
#74475=CARTESIAN_POINT('',(14.251438528,-41.6742356128,3.4));
#74476=CARTESIAN_POINT('',(14.9941689207,-41.6742356128,3.4));
#74477=CARTESIAN_POINT('',(14.2514385284,-41.6742356128,-1.95534782199));
#74478=CARTESIAN_POINT('',(14.2514385284,-41.6742356128,0.722326088933));
#74479=CARTESIAN_POINT('',(7.52535686472,-41.6742356128,4.00685543432));
#74480=CARTESIAN_POINT('Origin',(6.82290383517,-41.6742356128,-3.56061176027));
#74481=CARTESIAN_POINT('',(7.34384247076,-41.6742356128,4.20599930843));
#74482=CARTESIAN_POINT('Origin',(7.54384247076,-41.6742356128,4.20599930786));
#74483=CARTESIAN_POINT('',(7.34384247076,-41.6742356128,4.61875096898));
#74484=CARTESIAN_POINT('Origin',(-3.5527136788E-15,-41.6742356128,-8.88178104417E-16));
#74485=CARTESIAN_POINT('',(-5.26789531411,-41.6742356128,12.0375174903));
#74486=CARTESIAN_POINT('',(-6.88660115785,-41.6742356128,9.47167760676));
#74487=CARTESIAN_POINT('Origin',(-7.48272894647,-41.6742356128,11.6412701168));
#74488=CARTESIAN_POINT('',(-7.34384247076,-41.6742356128,6.92091963994));
#74489=CARTESIAN_POINT('Origin',(-0.000416107150126,-41.6742356128,6.92091963994));
#74490=CARTESIAN_POINT('',(-7.34384247076,-41.6742356128,6.09541632061));
#74491=CARTESIAN_POINT('',(-7.34384247076,-41.6742356128,6.50816798058));
#74492=CARTESIAN_POINT('',(-13.7266446428,-41.6742356128,8.41363339168));
#74493=CARTESIAN_POINT('',(-10.5352435568,-41.6742356128,7.25452485585));
#74494=CARTESIAN_POINT('',(-0.5,-41.6742356128,16.0922341519));
#74495=CARTESIAN_POINT('Origin',(-3.5527136788E-15,-41.6742356128,-8.88178104417E-16));
#74496=CARTESIAN_POINT('',(-0.5,-41.6742356128,14.2473325884));
#74497=CARTESIAN_POINT('',(-0.5,-41.6742356128,15.1697833702));
#74498=CARTESIAN_POINT('Origin',(-0.000416107150126,-41.6742356128,6.92091963994));
#74499=CARTESIAN_POINT('',(6.24384247076,-41.6742356128,6.92091963994));
#74500=CARTESIAN_POINT('',(6.24384247076,-41.6742356128,3.43894174696));
#74501=CARTESIAN_POINT('',(6.24384247076,-41.6742356128,5.17993069345));
#74502=CARTESIAN_POINT('',(6.74948971107,-41.6742356128,2.9389736393));
#74503=CARTESIAN_POINT('Origin',(6.74384247076,-41.6742356128,3.43894174696));
#74504=CARTESIAN_POINT('',(0.4871654368,-41.6742356128,-5.0126513422));
#74505=CARTESIAN_POINT('Origin',(6.82290383517,-41.6742356128,-3.56061176027));
#74506=CARTESIAN_POINT('',(0.000199055245640775,-41.6742356128,-4.62434677356992));
#74507=CARTESIAN_POINT('Origin',(-0.000199055382223,-41.6742356128,-5.12434669465));
#74508=CARTESIAN_POINT('',(-0.4871654368,-41.6742356128,-5.0126513422));
#74509=CARTESIAN_POINT('Origin',(0.000199055382222,-41.6742356128,-5.12434669465));
#74510=CARTESIAN_POINT('',(-6.74948971107,-41.6742356128,2.9389736393));
#74511=CARTESIAN_POINT('Origin',(-6.82290383517,-41.6742356128,-3.56061176027));
#74512=CARTESIAN_POINT('',(-6.24384247076,-41.6742356128,3.43894174696));
#74513=CARTESIAN_POINT('Origin',(-6.74384247076,-41.6742356128,3.43894174696));
#74514=CARTESIAN_POINT('',(-6.24384247076,-41.6742356128,5.17993069345));
#74515=CARTESIAN_POINT('Origin',(0.000416107150126,-41.6742356128,6.92091963994));
#74516=CARTESIAN_POINT('',(6.88660115785,-41.6742356128,9.47167760676));
#74517=CARTESIAN_POINT('',(5.26789531411,-41.6742356128,12.0375174903));
#74518=CARTESIAN_POINT('Origin',(7.48272894647,-41.6742356128,11.6412701168));
#74519=CARTESIAN_POINT('',(0.5,-41.6742356128,14.2473325884));
#74520=CARTESIAN_POINT('Origin',(0.000416107150126,-41.6742356128,6.92091963994));
#74521=CARTESIAN_POINT('',(0.5,-41.6742356128,16.0922341519));
#74522=CARTESIAN_POINT('',(0.5,-41.6742356128,15.1697833702));
#74523=CARTESIAN_POINT('',(13.7266446428,-41.6742356128,8.41363339168));
#74524=CARTESIAN_POINT('Origin',(-3.5527136788E-15,-41.6742356128,-8.88178104417E-16));
#74525=CARTESIAN_POINT('',(7.34384247076,-41.6742356128,6.09541632061));
#74526=CARTESIAN_POINT('',(10.5352435568,-41.6742356128,7.25452485585));
#74527=CARTESIAN_POINT('',(7.34384247076,-41.6742356128,6.92091963994));
#74528=CARTESIAN_POINT('',(7.34384247076,-41.6742356128,6.50816798058));
#74529=CARTESIAN_POINT('Origin',(0.000416107150126,-41.6742356128,6.92091963994));
#74530=CARTESIAN_POINT('Origin',(-3.5527136788E-15,-37.9242356128,-8.88178104417E-16));
#74531=CARTESIAN_POINT('',(15.7368993134,-39.7742356128,3.4));
#74532=CARTESIAN_POINT('Origin',(-3.5527136788E-15,-39.7742356128,-8.88178104417E-16));
#74533=CARTESIAN_POINT('',(15.7368993134,-40.7242356128,3.4));
#74534=CARTESIAN_POINT('Origin',(-3.35265884719E-30,-39.7742356128,3.15283103411E-22));
#74535=CARTESIAN_POINT('',(15.0199866844,-39.7742356128,3.4));
#74536=CARTESIAN_POINT('Origin',(3.59850171506006,-39.7742356128,1.3458683859422));
#74537=CARTESIAN_POINT('',(-3.5527136788E-15,-39.7742356128,3.4));
#74538=CARTESIAN_POINT('Origin',(-3.35265884719E-30,-39.7742356128,3.15283103411E-22));
#74539=CARTESIAN_POINT('',(7.34384247076,-39.7742356128,4.25491502787));
#74540=CARTESIAN_POINT('',(7.34384247076,-39.7742356128,0.717649133781));
#74541=CARTESIAN_POINT('',(7.4311653291,-39.7742356128,4.27488229452));
#74542=CARTESIAN_POINT('Origin',(7.20379737320062,-39.7742356128,5.068302267313));
#74543=CARTESIAN_POINT('',(9.78216646656,-39.7742356128,3.43958571397));
#74544=CARTESIAN_POINT('Ctrl Pts',(9.78216646656,-39.7742356128,3.43958571397));
#74545=CARTESIAN_POINT('Ctrl Pts',(9.44950651023,-39.7742356128,3.84219609922));
#74546=CARTESIAN_POINT('Ctrl Pts',(9.03618230028,-39.7742356128,4.19379483572));
#74547=CARTESIAN_POINT('Ctrl Pts',(8.49317585373,-39.7742356128,4.40265075658));
#74548=CARTESIAN_POINT('Ctrl Pts',(7.94364631071,-39.7742356128,4.41424876979));
#74549=CARTESIAN_POINT('Ctrl Pts',(7.4311653291,-39.7742356128,4.27488229452));
#74550=CARTESIAN_POINT('',(14.2514385284,-39.7742356128,-1.95534782207));
#74551=CARTESIAN_POINT('Origin',(6.82290383517001,-39.7742356128,-3.56061176026998));
#74552=CARTESIAN_POINT('',(14.2514385284,-39.7742356128,3.4));
#74553=CARTESIAN_POINT('',(14.2514385284,-39.7742356128,0.717649133781));
#74554=CARTESIAN_POINT('',(0.,-39.7742356128,3.4));
#74555=CARTESIAN_POINT('Origin',(7.34384247076,-41.6742356128,6.92091963994));
#74556=CARTESIAN_POINT('',(7.34384247076,-39.7742356128,4.20599930786));
#74557=CARTESIAN_POINT('',(7.34384247076,-40.7242356128,4.20599930786));
#74558=CARTESIAN_POINT('',(7.34384247076,-39.7742356128,5.5634594739));
#74559=CARTESIAN_POINT('Origin',(-3.35265884719E-30,-38.2742356128,3.15283103411E-22));
#74560=CARTESIAN_POINT('',(-9.86073561073,-37.2742356128,13.1044226585));
#74561=CARTESIAN_POINT('',(-9.86073561073,-33.7742356128,13.1044226585));
#74562=CARTESIAN_POINT('',(-9.86073561073,-38.2742356128,13.1044226585));
#74563=CARTESIAN_POINT('',(-13.4701563816,-33.7742356128,9.35493917959));
#74564=CARTESIAN_POINT('Origin',(-3.35265884719E-30,-33.7742356128,3.15283103411E-22));
#74565=CARTESIAN_POINT('',(-13.4701563816,-37.2742356128,9.35493917959));
#74566=CARTESIAN_POINT('',(-13.4701563816,-38.2742356128,9.35493917959));
#74567=CARTESIAN_POINT('',(-16.2234398325,-37.2742356128,2.4));
#74568=CARTESIAN_POINT('Origin',(-3.35265884719E-30,-37.2742356128,3.15283103411E-22));
#74569=CARTESIAN_POINT('',(-16.2234398325,-34.4742356128,2.4));
#74570=CARTESIAN_POINT('',(-16.2234398325,-38.2742356128,2.4));
#74571=CARTESIAN_POINT('',(-16.2234398325,-34.4742356128,-2.4));
#74572=CARTESIAN_POINT('Origin',(-3.35265884719E-30,-34.4742356128,3.15283103411E-22));
#74573=CARTESIAN_POINT('',(-16.2234398325,-37.2742356128,-2.4));
#74574=CARTESIAN_POINT('',(-16.2234398325,-38.2742356128,-2.4));
#74575=CARTESIAN_POINT('',(-13.1697266566,-37.2742356128,-9.77334639667));
#74576=CARTESIAN_POINT('Origin',(-3.35265884719E-30,-37.2742356128,3.15283103411E-22));
#74577=CARTESIAN_POINT('',(-13.1697266566,-33.7742356128,-9.77334639667));
#74578=CARTESIAN_POINT('',(-13.1697266566,-38.2742356128,-9.77334639667));
#74579=CARTESIAN_POINT('',(-10.2666800782,-33.7742356128,-12.7888732956));
#74580=CARTESIAN_POINT('Origin',(-3.35265884719E-30,-33.7742356128,3.15283103411E-22));
#74581=CARTESIAN_POINT('',(-10.2666800782,-37.2742356128,-12.7888732956));
#74582=CARTESIAN_POINT('',(-10.2666800782,-38.2742356128,-12.7888732956));
#74583=CARTESIAN_POINT('',(-4.7,-37.2742356128,-15.7120972502));
#74584=CARTESIAN_POINT('Origin',(-3.35265884719E-30,-37.2742356128,3.15283103411E-22));
#74585=CARTESIAN_POINT('',(-4.7,-39.2742356128,-15.7120972502));
#74586=CARTESIAN_POINT('',(-4.7,-38.2742356128,-15.7120972502));
#74587=CARTESIAN_POINT('',(-16.2234398325,-39.2742356128,-2.4));
#74588=CARTESIAN_POINT('Origin',(-3.35265884719E-30,-39.2742356128,3.15283103411E-22));
#74589=CARTESIAN_POINT('',(-16.2234398325,-38.2742356128,-2.4));
#74590=CARTESIAN_POINT('',(-16.2234398325,-39.2742356128,2.4));
#74591=CARTESIAN_POINT('',(-16.2234398325,-38.2742356128,2.4));
#74592=CARTESIAN_POINT('',(-3.7,-39.2742356128,15.9771712139));
#74593=CARTESIAN_POINT('Origin',(-3.35265884719E-30,-39.2742356128,3.15283103411E-22));
#74594=CARTESIAN_POINT('',(-3.7,-37.2742356128,15.9771712139));
#74595=CARTESIAN_POINT('',(-3.7,-38.2742356128,15.9771712139));
#74596=CARTESIAN_POINT('Origin',(-3.35265884719E-30,-37.2742356128,3.15283103411E-22));
#74597=CARTESIAN_POINT('Origin',(-16.2234398325,-41.6742356128,2.4));
#74598=CARTESIAN_POINT('',(-17.2336839201,-39.2742356128,2.4));
#74599=CARTESIAN_POINT('',(-17.2336839201,-40.4742356128,2.4));
#74600=CARTESIAN_POINT('',(-16.2433767578,-39.2742356128,2.4));
#74601=CARTESIAN_POINT('Ctrl Pts',(-17.2336839201,-41.6742356128,2.39999999999));
#74602=CARTESIAN_POINT('Ctrl Pts',(-17.2336839201,-38.7942356128,2.39999999999));
#74603=CARTESIAN_POINT('Ctrl Pts',(-17.1980377987,-41.6742356128,2.65606214167));
#74604=CARTESIAN_POINT('Ctrl Pts',(-17.1980377987,-38.7942356128,2.65606214167));
#74605=CARTESIAN_POINT('Ctrl Pts',(-17.1569007064,-41.6742356128,2.91066121221));
#74606=CARTESIAN_POINT('Ctrl Pts',(-17.1569007064,-38.7942356128,2.91066121221));
#74607=CARTESIAN_POINT('Ctrl Pts',(-17.1142405474,-41.6742356128,3.15603772019));
#74608=CARTESIAN_POINT('Ctrl Pts',(-17.1142405474,-38.7942356128,3.15603772019));
#74609=CARTESIAN_POINT('Ctrl Pts',(-17.0705772097,-41.6742356128,3.40000000002));
#74610=CARTESIAN_POINT('Ctrl Pts',(-17.0705772097,-38.7942356128,3.40000000002));
#74611=CARTESIAN_POINT('',(-17.0705772096,-39.2742356128,3.4));
#74612=CARTESIAN_POINT('',(-17.0705772097,-40.4742356128,3.4));
#74613=CARTESIAN_POINT('Ctrl Pts',(-17.2336839201,-39.2742356128,2.39999999999));
#74614=CARTESIAN_POINT('Ctrl Pts',(-17.1980377987,-39.2742356128,2.65606214167));
#74615=CARTESIAN_POINT('Ctrl Pts',(-17.1569007064,-39.2742356128,2.91066121221));
#74616=CARTESIAN_POINT('Ctrl Pts',(-17.1142405474,-39.2742356128,3.15603772019));
#74617=CARTESIAN_POINT('Ctrl Pts',(-17.0705772097,-39.2742356128,3.40000000002));
#74618=CARTESIAN_POINT('Origin',(-16.2234398325,-41.6742356128,3.4));
#74619=CARTESIAN_POINT('',(-17.0645832062,-39.2742356128,3.4));
#74620=CARTESIAN_POINT('',(-15.6610078691,-39.2742356128,3.4));
#74621=CARTESIAN_POINT('',(-17.0645832062,-40.4742356128,3.4));
#74622=CARTESIAN_POINT('Origin',(-3.5527136788E-15,-37.9242356128,-8.88178104417E-16));
#74623=CARTESIAN_POINT('',(17.0645832062,-39.2742356128,3.4));
#74624=CARTESIAN_POINT('',(17.0645832062,-37.9242356128,3.4));
#74625=CARTESIAN_POINT('',(3.7,-39.2742356128,17.0020586989));
#74626=CARTESIAN_POINT('Origin',(-3.5527136788E-15,-39.2742356128,-8.88178104417E-16));
#74627=CARTESIAN_POINT('',(3.7,-35.1742356128,17.0020586989));
#74628=CARTESIAN_POINT('',(3.7,-36.7242356128,17.0020586989));
#74629=CARTESIAN_POINT('',(3.,-34.4742356128,17.1394282285));
#74630=CARTESIAN_POINT('Ctrl Pts',(3.,-34.4742356128,17.1394282285028));
#74631=CARTESIAN_POINT('Ctrl Pts',(3.08822072668697,-34.4742356128001,17.1239865126806));
#74632=CARTESIAN_POINT('Ctrl Pts',(3.18225911112969,-34.4919134675103,17.1067526995575));
#74633=CARTESIAN_POINT('Ctrl Pts',(3.35531488240593,-34.5638806129857,17.0736528901812));
#74634=CARTESIAN_POINT('Ctrl Pts',(3.43433873884385,-34.6181717006057,17.0578246368735));
#74635=CARTESIAN_POINT('Ctrl Pts',(3.55804988739417,-34.7427937550804,17.0324452764604));
#74636=CARTESIAN_POINT('Ctrl Pts',(3.61145665151433,-34.8210247498864,17.021125060463));
#74637=CARTESIAN_POINT('Ctrl Pts',(3.68243822155749,-34.9928100970052,17.0059097439477));
#74638=CARTESIAN_POINT('Ctrl Pts',(3.7,-35.0863737311305,17.0020586988753));
#74639=CARTESIAN_POINT('Ctrl Pts',(3.7,-35.1742356128,17.0020586988753));
#74640=CARTESIAN_POINT('',(-3.,-34.4742356128,17.1394282285));
#74641=CARTESIAN_POINT('Origin',(-3.35265884719E-30,-34.4742356128,3.15283103411E-22));
#74642=CARTESIAN_POINT('',(-3.7,-35.1742356128,17.0020586989));
#74643=CARTESIAN_POINT('Ctrl Pts',(-3.7,-35.1742356128,17.0020586988753));
#74644=CARTESIAN_POINT('Ctrl Pts',(-3.7,-35.0863737311305,17.0020586988753));
#74645=CARTESIAN_POINT('Ctrl Pts',(-3.68243822155749,-34.9928100970052,
17.0059097439477));
#74646=CARTESIAN_POINT('Ctrl Pts',(-3.61145665151433,-34.8210247498864,
17.021125060463));
#74647=CARTESIAN_POINT('Ctrl Pts',(-3.55804988739417,-34.7427937550804,
17.0324452764604));
#74648=CARTESIAN_POINT('Ctrl Pts',(-3.43433873884385,-34.6181717006057,
17.0578246368735));
#74649=CARTESIAN_POINT('Ctrl Pts',(-3.35531488240592,-34.5638806129857,
17.0736528901812));
#74650=CARTESIAN_POINT('Ctrl Pts',(-3.18225911112969,-34.4919134675103,
17.1067526995575));
#74651=CARTESIAN_POINT('Ctrl Pts',(-3.08822072668697,-34.4742356128,17.1239865126806));
#74652=CARTESIAN_POINT('Ctrl Pts',(-3.,-34.4742356128,17.1394282285028));
#74653=CARTESIAN_POINT('',(-3.7,-39.2742356128,17.0020586989));
#74654=CARTESIAN_POINT('',(-3.7,-37.2242356128,17.0020586989));
#74655=CARTESIAN_POINT('Origin',(-3.5527136788E-15,-39.2742356128,-8.88178104417E-16));
#74656=CARTESIAN_POINT('Origin',(-16.2234398325,-41.6742356128,3.4));
#74657=CARTESIAN_POINT('',(17.0705772096,-39.2742356128,3.4));
#74658=CARTESIAN_POINT('',(17.0705772097,-40.4742356128,3.4));
#74659=CARTESIAN_POINT('',(-15.6610078691,-39.2742356128,3.4));
#74660=CARTESIAN_POINT('Ctrl Pts',(17.2336839201,-41.6742356128,2.39999999999));
#74661=CARTESIAN_POINT('Ctrl Pts',(17.2336839201,-38.7942356128,2.39999999999));
#74662=CARTESIAN_POINT('Ctrl Pts',(17.1980377987,-41.6742356128,2.65606214167));
#74663=CARTESIAN_POINT('Ctrl Pts',(17.1980377987,-38.7942356128,2.65606214167));
#74664=CARTESIAN_POINT('Ctrl Pts',(17.1569007064,-41.6742356128,2.91066121221));
#74665=CARTESIAN_POINT('Ctrl Pts',(17.1569007064,-38.7942356128,2.91066121221));
#74666=CARTESIAN_POINT('Ctrl Pts',(17.1142405474,-41.6742356128,3.15603772019));
#74667=CARTESIAN_POINT('Ctrl Pts',(17.1142405474,-38.7942356128,3.15603772019));
#74668=CARTESIAN_POINT('Ctrl Pts',(17.0705772097,-41.6742356128,3.40000000002));
#74669=CARTESIAN_POINT('Ctrl Pts',(17.0705772097,-38.7942356128,3.40000000002));
#74670=CARTESIAN_POINT('',(17.2336839201,-39.2742356128,2.4));
#74671=CARTESIAN_POINT('',(17.2336839201,-40.4742356128,2.4));
#74672=CARTESIAN_POINT('Ctrl Pts',(17.2336839201,-39.2742356128,2.39999999999));
#74673=CARTESIAN_POINT('Ctrl Pts',(17.1980377987,-39.2742356128,2.65606214167));
#74674=CARTESIAN_POINT('Ctrl Pts',(17.1569007064,-39.2742356128,2.91066121221));
#74675=CARTESIAN_POINT('Ctrl Pts',(17.1142405474,-39.2742356128,3.15603772019));
#74676=CARTESIAN_POINT('Ctrl Pts',(17.0705772097,-39.2742356128,3.40000000002));
#74677=CARTESIAN_POINT('Origin',(-16.2234398325,-41.6742356128,2.4));
#74678=CARTESIAN_POINT('',(16.2234398325,-39.2742356128,2.4));
#74679=CARTESIAN_POINT('',(16.2234398325,-40.4742356128,2.4));
#74680=CARTESIAN_POINT('',(-16.2433767578,-39.2742356128,2.4));
#74681=CARTESIAN_POINT('Origin',(-3.35265884719E-30,-38.2742356128,3.15283103411E-22));
#74682=CARTESIAN_POINT('',(10.2666800782,-37.2742356128,-12.7888732956));
#74683=CARTESIAN_POINT('',(10.2666800782,-33.7742356128,-12.7888732956));
#74684=CARTESIAN_POINT('',(10.2666800782,-38.2742356128,-12.7888732956));
#74685=CARTESIAN_POINT('',(13.1697266566,-33.7742356128,-9.77334639667));
#74686=CARTESIAN_POINT('Origin',(-3.35265884719E-30,-33.7742356128,3.15283103411E-22));
#74687=CARTESIAN_POINT('',(13.1697266566,-37.2742356128,-9.77334639667));
#74688=CARTESIAN_POINT('',(13.1697266566,-38.2742356128,-9.77334639667));
#74689=CARTESIAN_POINT('',(16.2234398325,-37.2742356128,-2.4));
#74690=CARTESIAN_POINT('Origin',(-3.35265884719E-30,-37.2742356128,3.15283103411E-22));
#74691=CARTESIAN_POINT('',(16.2234398325,-34.4742356128,-2.4));
#74692=CARTESIAN_POINT('',(16.2234398325,-38.2742356128,-2.4));
#74693=CARTESIAN_POINT('',(16.2234398325,-34.4742356128,2.4));
#74694=CARTESIAN_POINT('Origin',(-3.35265884719E-30,-34.4742356128,3.15283103411E-22));
#74695=CARTESIAN_POINT('',(16.2234398325,-37.2742356128,2.4));
#74696=CARTESIAN_POINT('',(16.2234398325,-38.2742356128,2.4));
#74697=CARTESIAN_POINT('',(13.1697266566,-37.2742356128,9.77334639667));
#74698=CARTESIAN_POINT('Origin',(-3.35265884719E-30,-37.2742356128,3.15283103411E-22));
#74699=CARTESIAN_POINT('',(13.1697266566,-33.7742356128,9.77334639667));
#74700=CARTESIAN_POINT('',(13.1697266566,-38.2742356128,9.77334639667));
#74701=CARTESIAN_POINT('',(10.2666800782,-33.7742356128,12.7888732956));
#74702=CARTESIAN_POINT('Origin',(-3.35265884719E-30,-33.7742356128,3.15283103411E-22));
#74703=CARTESIAN_POINT('',(10.2666800782,-37.2742356128,12.7888732956));
#74704=CARTESIAN_POINT('',(10.2666800782,-38.2742356128,12.7888732956));
#74705=CARTESIAN_POINT('',(3.7,-37.2742356128,15.977171214));
#74706=CARTESIAN_POINT('Origin',(-3.35265884719E-30,-37.2742356128,3.15283103411E-22));
#74707=CARTESIAN_POINT('',(3.7,-39.2742356128,15.9771712139));
#74708=CARTESIAN_POINT('',(3.7,-38.2742356128,15.9771712139));
#74709=CARTESIAN_POINT('Origin',(-3.35265884719E-30,-39.2742356128,3.15283103411E-22));
#74710=CARTESIAN_POINT('',(16.2234398325,-39.2742356128,-2.4));
#74711=CARTESIAN_POINT('',(16.2234398325,-38.2742356128,-2.4));
#74712=CARTESIAN_POINT('',(4.7,-39.2742356128,-15.7120972502));
#74713=CARTESIAN_POINT('Origin',(-3.35265884719E-30,-39.2742356128,3.15283103411E-22));
#74714=CARTESIAN_POINT('',(4.7,-37.2742356128,-15.7120972502));
#74715=CARTESIAN_POINT('',(4.7,-38.2742356128,-15.7120972502));
#74716=CARTESIAN_POINT('Origin',(-3.35265884719E-30,-37.2742356128,3.15283103411E-22));
#74717=CARTESIAN_POINT('Origin',(-14.2514385284,-41.6742356128,-2.4));
#74718=CARTESIAN_POINT('',(17.2336839201,-39.2742356128,-2.4));
#74719=CARTESIAN_POINT('',(17.2336839201,-40.4742356128,-2.4));
#74720=CARTESIAN_POINT('',(-16.2433767578,-39.2742356128,-2.4));
#74721=CARTESIAN_POINT('Ctrl Pts',(17.0705772097,-41.6742356128,-3.4));
#74722=CARTESIAN_POINT('Ctrl Pts',(17.0705772097,-38.7942356128,-3.4));
#74723=CARTESIAN_POINT('Ctrl Pts',(17.1142405474,-41.6742356128,-3.15603772018));
#74724=CARTESIAN_POINT('Ctrl Pts',(17.1142405474,-38.7942356128,-3.15603772018));
#74725=CARTESIAN_POINT('Ctrl Pts',(17.1569007064,-41.6742356128,-2.91066121221));
#74726=CARTESIAN_POINT('Ctrl Pts',(17.1569007064,-38.7942356128,-2.91066121221));
#74727=CARTESIAN_POINT('Ctrl Pts',(17.1980377987,-41.6742356128,-2.65606214167));
#74728=CARTESIAN_POINT('Ctrl Pts',(17.1980377987,-38.7942356128,-2.65606214167));
#74729=CARTESIAN_POINT('Ctrl Pts',(17.2336839201,-41.6742356128,-2.39999999999));
#74730=CARTESIAN_POINT('Ctrl Pts',(17.2336839201,-38.7942356128,-2.39999999999));
#74731=CARTESIAN_POINT('',(17.0705772097,-39.2742356128,-3.4));
#74732=CARTESIAN_POINT('',(17.0705772097,-40.4742356128,-3.4));
#74733=CARTESIAN_POINT('Ctrl Pts',(17.0705772097,-39.2742356128,-3.4));
#74734=CARTESIAN_POINT('Ctrl Pts',(17.1142405474,-39.2742356128,-3.15603772018));
#74735=CARTESIAN_POINT('Ctrl Pts',(17.1569007064,-39.2742356128,-2.91066121221));
#74736=CARTESIAN_POINT('Ctrl Pts',(17.1980377987,-39.2742356128,-2.65606214167));
#74737=CARTESIAN_POINT('Ctrl Pts',(17.2336839201,-39.2742356128,-2.39999999999));
#74738=CARTESIAN_POINT('Origin',(-14.2514385284,-41.6742356128,-3.4));
#74739=CARTESIAN_POINT('',(17.0645832063,-39.2742356128,-3.4));
#74740=CARTESIAN_POINT('',(-15.6610078691,-39.2742356128,-3.4));
#74741=CARTESIAN_POINT('',(17.0645832062,-40.4742356128,-3.4));
#74742=CARTESIAN_POINT('Origin',(-3.5527136788E-15,-37.9242356128,-8.88178104417E-16));
#74743=CARTESIAN_POINT('',(-17.0645832063,-39.2742356128,-3.4));
#74744=CARTESIAN_POINT('',(-17.0645832062,-37.9242356128,-3.4));
#74745=CARTESIAN_POINT('',(-4.7,-39.2742356128,-16.7532086479));
#74746=CARTESIAN_POINT('Origin',(-3.5527136788E-15,-39.2742356128,-8.88178104417E-16));
#74747=CARTESIAN_POINT('',(-4.7,-35.1742356128,-16.7532086479));
#74748=CARTESIAN_POINT('',(-4.7,-37.9242356128,-16.7532086479));
#74749=CARTESIAN_POINT('',(-4.,-34.4742356128,-16.9339894886));
#74750=CARTESIAN_POINT('Ctrl Pts',(-4.,-34.4742356128,-16.9339894885996));
#74751=CARTESIAN_POINT('Ctrl Pts',(-4.08836998503334,-34.4742356128,-16.9131154978385));
#74752=CARTESIAN_POINT('Ctrl Pts',(-4.18258473523978,-34.4919628383768,
-16.8900560280459));
#74753=CARTESIAN_POINT('Ctrl Pts',(-4.35608524188229,-34.5642875640868,
-16.8461428541903));
#74754=CARTESIAN_POINT('Ctrl Pts',(-4.43537858782587,-34.6188898563745,
-16.8253270374741));
#74755=CARTESIAN_POINT('Ctrl Pts',(-4.55872416788887,-34.74379828014,-16.7923189265584));
#74756=CARTESIAN_POINT('Ctrl Pts',(-4.61180004333827,-34.8216954565953,
-16.7777425183049));
#74757=CARTESIAN_POINT('Ctrl Pts',(-4.68244878672198,-34.9929968204804,
-16.7581626981184));
#74758=CARTESIAN_POINT('Ctrl Pts',(-4.7,-35.0864155763189,-16.7532086478979));
#74759=CARTESIAN_POINT('Ctrl Pts',(-4.7,-35.1742356128,-16.7532086478979));
#74760=CARTESIAN_POINT('',(4.,-34.4742356128,-16.9339894886));
#74761=CARTESIAN_POINT('Origin',(-3.5527136788E-15,-34.4742356128,-8.88178104417E-16));
#74762=CARTESIAN_POINT('',(4.7,-35.1742356128,-16.7532086479));
#74763=CARTESIAN_POINT('Ctrl Pts',(4.7,-35.1742356128,-16.7532086478979));
#74764=CARTESIAN_POINT('Ctrl Pts',(4.7,-35.0864155763189,-16.7532086478979));
#74765=CARTESIAN_POINT('Ctrl Pts',(4.68244878672198,-34.9929968204804,-16.7581626981184));
#74766=CARTESIAN_POINT('Ctrl Pts',(4.61180004333826,-34.8216954565953,-16.7777425183049));
#74767=CARTESIAN_POINT('Ctrl Pts',(4.55872416788887,-34.74379828014,-16.7923189265584));
#74768=CARTESIAN_POINT('Ctrl Pts',(4.43537858782587,-34.6188898563745,-16.8253270374741));
#74769=CARTESIAN_POINT('Ctrl Pts',(4.35608524188229,-34.5642875640868,-16.8461428541903));
#74770=CARTESIAN_POINT('Ctrl Pts',(4.18258473523978,-34.4919628383767,-16.8900560280459));
#74771=CARTESIAN_POINT('Ctrl Pts',(4.08836998503334,-34.4742356128,-16.9131154978385));
#74772=CARTESIAN_POINT('Ctrl Pts',(4.,-34.4742356128,-16.9339894885995));
#74773=CARTESIAN_POINT('',(4.7,-39.2742356128,-16.7532086479));
#74774=CARTESIAN_POINT('',(4.7,-37.9242356128,-16.7532086479));
#74775=CARTESIAN_POINT('Origin',(-3.5527136788E-15,-39.2742356128,-8.88178104417E-16));
#74776=CARTESIAN_POINT('Origin',(-14.2514385284,-41.6742356128,-3.4));
#74777=CARTESIAN_POINT('',(-17.0705772097,-39.2742356128,-3.4));
#74778=CARTESIAN_POINT('',(-17.0705772097,-40.4742356128,-3.4));
#74779=CARTESIAN_POINT('',(-15.6610078691,-39.2742356128,-3.4));
#74780=CARTESIAN_POINT('Ctrl Pts',(-17.0705772097,-41.6742356128,-3.4));
#74781=CARTESIAN_POINT('Ctrl Pts',(-17.0705772097,-38.7942356128,-3.4));
#74782=CARTESIAN_POINT('Ctrl Pts',(-17.1142405474,-41.6742356128,-3.15603772018));
#74783=CARTESIAN_POINT('Ctrl Pts',(-17.1142405474,-38.7942356128,-3.15603772018));
#74784=CARTESIAN_POINT('Ctrl Pts',(-17.1569007064,-41.6742356128,-2.91066121221));
#74785=CARTESIAN_POINT('Ctrl Pts',(-17.1569007064,-38.7942356128,-2.91066121221));
#74786=CARTESIAN_POINT('Ctrl Pts',(-17.1980377987,-41.6742356128,-2.65606214167));
#74787=CARTESIAN_POINT('Ctrl Pts',(-17.1980377987,-38.7942356128,-2.65606214167));
#74788=CARTESIAN_POINT('Ctrl Pts',(-17.2336839201,-41.6742356128,-2.39999999999));
#74789=CARTESIAN_POINT('Ctrl Pts',(-17.2336839201,-38.7942356128,-2.39999999999));
#74790=CARTESIAN_POINT('',(-17.2336839201,-39.2742356128,-2.4));
#74791=CARTESIAN_POINT('Ctrl Pts',(-17.0705772097,-39.2742356128,-3.4));
#74792=CARTESIAN_POINT('Ctrl Pts',(-17.1142405474,-39.2742356128,-3.15603772018));
#74793=CARTESIAN_POINT('Ctrl Pts',(-17.1569007064,-39.2742356128,-2.91066121221));
#74794=CARTESIAN_POINT('Ctrl Pts',(-17.1980377987,-39.2742356128,-2.65606214167));
#74795=CARTESIAN_POINT('Ctrl Pts',(-17.2336839201,-39.2742356128,-2.39999999999));
#74796=CARTESIAN_POINT('',(-17.2336839201,-40.4742356128,-2.4));
#74797=CARTESIAN_POINT('Origin',(-14.2514385284,-41.6742356128,-2.4));
#74798=CARTESIAN_POINT('',(-16.2433767578,-39.2742356128,-2.4));
#74799=CARTESIAN_POINT('Origin',(-3.5527136788E-15,-37.9242356128,-8.88178104417E-16));
#74800=CARTESIAN_POINT('',(-15.7368993134,-39.7742356128,-3.4));
#74801=CARTESIAN_POINT('',(-15.7368993134,-40.7242356128,-3.4));
#74802=CARTESIAN_POINT('',(15.7368993134,-39.7742356128,-3.4));
#74803=CARTESIAN_POINT('',(15.7368993134,-40.7242356128,-3.4));
#74804=CARTESIAN_POINT('',(3.7,-39.7742356128,-15.6690778286));
#74805=CARTESIAN_POINT('Origin',(-3.5527136788E-15,-39.7742356128,-8.88178104417E-16));
#74806=CARTESIAN_POINT('',(-3.7,-39.7742356128,-15.6690778286));
#74807=CARTESIAN_POINT('Origin',(-3.5527136788E-15,-39.7742356128,-8.88178104417E-16));
#74808=CARTESIAN_POINT('Origin',(-3.5527136788E-15,-39.7742356128,-8.88178104417E-16));
#74809=CARTESIAN_POINT('Origin',(-14.2514385284,-41.6742356128,-3.4));
#74810=CARTESIAN_POINT('',(14.4212065313,-39.7742356128,-3.4));
#74811=CARTESIAN_POINT('',(14.4212065313,-40.4742356128,-3.4));
#74812=CARTESIAN_POINT('',(15.0199866844,-39.7742356128,-3.4));
#74813=CARTESIAN_POINT('',(-15.6610078691,-39.7742356128,-3.4));
#74814=CARTESIAN_POINT('',(-15.6610078691,-39.7742356128,-3.4));
#74815=CARTESIAN_POINT('Origin',(6.82290383517,-40.1142356128,-3.56061176027));
#74816=CARTESIAN_POINT('',(0.174946252184,-39.7742356128,-7.24363497156));
#74817=CARTESIAN_POINT('',(0.174946252184,-40.7242356128,-7.24363497156));
#74818=CARTESIAN_POINT('',(0.517273426056,-39.7742356128,-7.80313755792));
#74819=CARTESIAN_POINT('Origin',(6.82290383517,-39.7742356128,-3.56061176027));
#74820=CARTESIAN_POINT('',(1.78291107349,-39.7742356128,-9.24906260055));
#74821=CARTESIAN_POINT('Origin',(6.82290383517,-39.7742356128,-3.56061176027));
#74822=CARTESIAN_POINT('',(2.42784894914,-39.7742356128,-9.76089341103));
#74823=CARTESIAN_POINT('Origin',(6.82290383517,-39.7742356128,-3.56061176027));
#74824=CARTESIAN_POINT('Origin',(6.82290383517,-39.7742356128,-3.56061176027));
#74825=CARTESIAN_POINT('Origin',(1.44328993201E-15,-40.7242356128,-7.34055663501));
#74826=CARTESIAN_POINT('',(-0.174946252184,-39.7742356128,-7.24363497156));
#74827=CARTESIAN_POINT('',(-0.174946252184,-40.7242356128,-7.24363497156));
#74828=CARTESIAN_POINT('Origin',(1.44328993201E-15,-39.7742356128,-7.34055663501));
#74829=CARTESIAN_POINT('Origin',(-6.82290383517,-40.1142356128,-3.56061176027));
#74830=CARTESIAN_POINT('',(-2.42784894914,-39.7742356128,-9.76089341103));
#74831=CARTESIAN_POINT('',(-14.4212065313,-39.7742356128,-3.4));
#74832=CARTESIAN_POINT('Origin',(-6.82290383517,-39.7742356128,-3.56061176027));
#74833=CARTESIAN_POINT('',(-1.78291107349,-39.7742356128,-9.24906260055));
#74834=CARTESIAN_POINT('Origin',(-6.82290383517,-39.7742356128,-3.56061176027));
#74835=CARTESIAN_POINT('',(-0.517273426056,-39.7742356128,-7.80313755792));
#74836=CARTESIAN_POINT('Origin',(-6.82290383517,-39.7742356128,-3.56061176027));
#74837=CARTESIAN_POINT('Origin',(-6.82290383517,-39.7742356128,-3.56061176027));
#74838=CARTESIAN_POINT('',(-14.4212065313,-40.7242356128,-3.4));
#74839=CARTESIAN_POINT('Origin',(-14.2514385284,-41.6742356128,-3.4));
#74840=CARTESIAN_POINT('',(-15.0199866844,-39.7742356128,-3.4));
#74841=CARTESIAN_POINT('',(-15.6610078691,-39.7742356128,-3.4));
#74842=CARTESIAN_POINT('',(-15.6610078691,-39.7742356128,-3.4));
#74843=CARTESIAN_POINT('Origin',(-7.34384247076,-41.6742356128,6.92091963994));
#74844=CARTESIAN_POINT('',(-7.34384247076,-39.7742356128,5.03150262895));
#74845=CARTESIAN_POINT('',(-7.34384247076,-40.7242356128,5.03150262895));
#74846=CARTESIAN_POINT('',(-7.34384247076,-39.7742356128,4.25491502787));
#74847=CARTESIAN_POINT('',(-7.34384247076,-39.7742356128,5.5634594739));
#74848=CARTESIAN_POINT('',(-7.34384247076,-39.7742356128,4.20599930786));
#74849=CARTESIAN_POINT('',(-7.34384247076,-39.7742356128,5.5634594739));
#74850=CARTESIAN_POINT('',(-7.34384247076,-40.7242356128,4.20599930786));
#74851=CARTESIAN_POINT('Origin',(-6.71477748978,-41.6742356128,4.80302787151));
#74852=CARTESIAN_POINT('',(-14.2293511975,-39.7742356128,7.53230140778));
#74853=CARTESIAN_POINT('',(-14.2293511975,-40.7242356128,7.53230140778));
#74854=CARTESIAN_POINT('',(-13.5647513306,-39.7742356128,7.2909204726));
#74855=CARTESIAN_POINT('',(-13.8970512641,-39.7742356128,7.41161094019));
#74856=CARTESIAN_POINT('',(-10.4542969007,-39.7742356128,6.16121155078));
#74857=CARTESIAN_POINT('Origin',(-3.5527136788E-15,-37.9242356128,-8.88178104417E-16));
#74858=CARTESIAN_POINT('',(-15.7368993134,-39.7742356128,3.4));
#74859=CARTESIAN_POINT('',(-15.7368993134,-40.7242356128,3.4));
#74860=CARTESIAN_POINT('Origin',(-3.5527136788E-15,-39.7742356128,-8.88178104417E-16));
#74861=CARTESIAN_POINT('Origin',(-16.2234398325,-41.6742356128,3.4));
#74862=CARTESIAN_POINT('',(-14.2514385284,-39.7742356128,3.4));
#74863=CARTESIAN_POINT('',(-14.2514385284,-40.4742356128,3.4));
#74864=CARTESIAN_POINT('',(-15.0199866844,-39.7742356128,3.4));
#74865=CARTESIAN_POINT('',(-15.6610078691,-39.7742356128,3.4));
#74866=CARTESIAN_POINT('',(-15.6610078691,-39.7742356128,3.4));
#74867=CARTESIAN_POINT('Origin',(-14.2514385284,-41.6742356128,2.4));
#74868=CARTESIAN_POINT('',(-14.2514385284,-39.7742356128,-1.95534782207));
#74869=CARTESIAN_POINT('',(-14.2514385284,-40.7242356128,-1.95534782207));
#74870=CARTESIAN_POINT('',(-14.2514385284,-39.7742356128,0.722326088964));
#74871=CARTESIAN_POINT('Origin',(-6.82290383517,-40.1142356128,-3.56061176027));
#74872=CARTESIAN_POINT('',(-7.52535686472,-39.7742356128,4.00685543432));
#74873=CARTESIAN_POINT('',(-7.52535686472,-40.7242356128,4.00685543432));
#74874=CARTESIAN_POINT('',(-9.78216646656,-39.7742356128,3.43958571397));
#74875=CARTESIAN_POINT('Origin',(-6.82290383517,-39.7742356128,-3.56061176027));
#74876=CARTESIAN_POINT('Origin',(-6.82290383517,-39.7742356128,-3.56061176027));
#74877=CARTESIAN_POINT('Origin',(-7.54384247076,-40.7242356128,4.20599930786));
#74878=CARTESIAN_POINT('Origin',(-7.54384247076,-39.7742356128,4.20599930786));
#74879=CARTESIAN_POINT('Origin',(7.54384247076,-40.7242356128,4.20599930786));
#74880=CARTESIAN_POINT('',(7.52535686472,-39.7742356128,4.00685543432));
#74881=CARTESIAN_POINT('',(7.52535686472,-40.7242356128,4.00685543432));
#74882=CARTESIAN_POINT('Origin',(7.54384247076,-39.7742356128,4.20599930786));
#74883=CARTESIAN_POINT('Origin',(6.82290383517,-40.1142356128,-3.56061176027));
#74884=CARTESIAN_POINT('Origin',(6.82290383517,-39.7742356128,-3.56061176027));
#74885=CARTESIAN_POINT('',(14.2514385284,-40.7242356128,-1.95534782207));
#74886=CARTESIAN_POINT('Origin',(14.2514385284,-41.6742356128,2.4));
#74887=CARTESIAN_POINT('',(14.2514385284,-40.7242356128,3.4));
#74888=CARTESIAN_POINT('Origin',(-16.2234398325,-41.6742356128,3.4));
#74889=CARTESIAN_POINT('Origin',(-0.000416107150126,-40.1142356128,6.92091963994));
#74890=CARTESIAN_POINT('',(-0.5,-39.7742356128,14.2473325884));
#74891=CARTESIAN_POINT('',(-0.5,-40.7242356128,14.2473325884));
#74892=CARTESIAN_POINT('',(-5.26789531411,-39.7742356128,12.0375174903));
#74893=CARTESIAN_POINT('Origin',(-0.000416107150126,-39.7742356128,6.92091963994));
#74894=CARTESIAN_POINT('',(-5.26789531411,-40.7242356128,12.0375174903));
#74895=CARTESIAN_POINT('Origin',(-0.5,-41.6742356128,13.1643460036));
#74896=CARTESIAN_POINT('',(-0.5,-39.7742356128,16.0922341519));
#74897=CARTESIAN_POINT('',(-0.5,-40.7242356128,16.0922341519));
#74898=CARTESIAN_POINT('',(-0.5,-39.7742356128,15.1697833702));
#74899=CARTESIAN_POINT('Origin',(-3.5527136788E-15,-37.9242356128,-8.88178104417E-16));
#74900=CARTESIAN_POINT('',(-13.7266446428,-39.7742356128,8.41363339168));
#74901=CARTESIAN_POINT('',(-13.7266446428,-40.7242356128,8.41363339168));
#74902=CARTESIAN_POINT('',(-2.7,-39.7742356128,15.8719879032));
#74903=CARTESIAN_POINT('Origin',(-3.5527136788E-15,-39.7742356128,-8.88178104417E-16));
#74904=CARTESIAN_POINT('Origin',(-3.5527136788E-15,-39.7742356128,-8.88178104417E-16));
#74905=CARTESIAN_POINT('Origin',(-6.37339887025,-41.6742356128,5.74295373993));
#74906=CARTESIAN_POINT('',(-7.34384247076,-39.7742356128,6.09541632002));
#74907=CARTESIAN_POINT('',(-7.34384247076,-40.7242356128,6.09541632002));
#74908=CARTESIAN_POINT('',(-13.0544719111,-39.7742356128,8.16950201179));
#74909=CARTESIAN_POINT('',(-10.1991571909,-39.7742356128,7.13245916591));
#74910=CARTESIAN_POINT('',(-13.390558277,-39.7742356128,8.29156770174));
#74911=CARTESIAN_POINT('Origin',(-7.34384247076,-41.6742356128,6.92091963994));
#74912=CARTESIAN_POINT('',(-7.34384247076,-39.7742356128,6.92091963994));
#74913=CARTESIAN_POINT('',(-7.34384247076,-40.7242356128,6.92091963994));
#74914=CARTESIAN_POINT('',(-7.34384247076,-39.7742356128,5.5634594739));
#74915=CARTESIAN_POINT('Origin',(-0.000416107150126,-40.1142356128,6.92091963994));
#74916=CARTESIAN_POINT('',(-6.88660115785,-39.7742356128,9.47167760676));
#74917=CARTESIAN_POINT('Origin',(-0.000416107150126,-39.7742356128,6.92091963994));
#74918=CARTESIAN_POINT('',(-6.88660115785,-40.7242356128,9.47167760676));
#74919=CARTESIAN_POINT('Origin',(-7.48272894647,-41.3342356129,11.6412701168));
#74920=CARTESIAN_POINT('',(-9.73272894647,-43.9742356128,11.6412701168));
#74921=CARTESIAN_POINT('Origin',(-7.48272894647,-43.9742356128,11.6412701168));
#74922=CARTESIAN_POINT('',(-9.73272894647,-39.7742356128,11.6412701168));
#74923=CARTESIAN_POINT('',(-9.73272894647,-41.3342356129,11.6412701168));
#74924=CARTESIAN_POINT('Origin',(-7.48272894647,-39.7742356128,11.6412701168));
#74925=CARTESIAN_POINT('',(-6.84013384355,-39.7742356128,13.7975566316));
#74926=CARTESIAN_POINT('Origin',(-7.48272894647,-39.7742356128,11.6412701168));
#74927=CARTESIAN_POINT('',(-9.71115043835,-39.7742356128,11.952136092));
#74928=CARTESIAN_POINT('Origin',(-7.48272894647,-39.7742356128,11.6412701168));
#74929=CARTESIAN_POINT('Origin',(-7.48272894647,-39.7742356128,11.6412701168));
#74930=CARTESIAN_POINT('Origin',(0.000416107150126,-40.1142356128,6.92091963994));
#74931=CARTESIAN_POINT('',(6.24384247076,-40.6742356128,6.92091963994));
#74932=CARTESIAN_POINT('',(6.24384247076,-40.1142356128,6.92091963994));
#74933=CARTESIAN_POINT('Origin',(0.000416107150126,-40.6742356128,6.92091963994));
#74934=CARTESIAN_POINT('Origin',(-6.24384247076,-41.6742356128,6.92091963994));
#74935=CARTESIAN_POINT('',(-6.24384247076,-40.6742356128,3.43894174696));
#74936=CARTESIAN_POINT('',(-6.24384247076,-41.1742356128,3.43894174696));
#74937=CARTESIAN_POINT('',(-6.24384247076,-40.6742356128,5.17993069345));
#74938=CARTESIAN_POINT('Origin',(-6.74384247076,-41.1742356128,3.43894174696));
#74939=CARTESIAN_POINT('',(-6.74948971107,-40.6742356128,2.9389736393));
#74940=CARTESIAN_POINT('Origin',(-6.74384247076,-40.6742356128,3.43894174696));
#74941=CARTESIAN_POINT('',(-6.74948971107,-41.1742356128,2.9389736393));
#74942=CARTESIAN_POINT('Origin',(-6.82290383517,-40.1142356128,-3.56061176027));
#74943=CARTESIAN_POINT('',(-0.4871654368,-40.6742356128,-5.0126513422));
#74944=CARTESIAN_POINT('Origin',(-6.82290383517,-40.6742356128,-3.56061176027));
#74945=CARTESIAN_POINT('',(-0.4871654368,-40.1142356128,-5.0126513422));
#74946=CARTESIAN_POINT('Origin',(0.000199055382222,-41.1742356128,-5.12434669465));
#74947=CARTESIAN_POINT('',(0.000199055298121561,-40.6742356128,-4.62434674748069));
#74948=CARTESIAN_POINT('Origin',(0.000199055382222,-40.6742356128,-5.12434669465));
#74949=CARTESIAN_POINT('',(0.000199055382222,-41.1742356128,-4.62434669465));
#74950=CARTESIAN_POINT('Origin',(-0.000199055382223,-41.1742356128,-5.12434669465));
#74951=CARTESIAN_POINT('',(0.4871654368,-40.6742356128,-5.0126513422));
#74952=CARTESIAN_POINT('Origin',(-0.000199055382223,-40.6742356128,-5.12434669465));
#74953=CARTESIAN_POINT('',(0.4871654368,-41.1742356128,-5.0126513422));
#74954=CARTESIAN_POINT('Origin',(6.82290383517,-40.1142356128,-3.56061176027));
#74955=CARTESIAN_POINT('',(6.74948971107,-40.6742356128,2.9389736393));
#74956=CARTESIAN_POINT('',(6.74948971107,-40.1142356128,2.9389736393));
#74957=CARTESIAN_POINT('Origin',(6.82290383517,-40.6742356128,-3.56061176027));
#74958=CARTESIAN_POINT('Origin',(6.74384247076,-41.1742356128,3.43894174696));
#74959=CARTESIAN_POINT('',(6.24384247076,-40.6742356128,3.43894174696));
#74960=CARTESIAN_POINT('Origin',(6.74384247076,-40.6742356128,3.43894174696));
#74961=CARTESIAN_POINT('',(6.24384247076,-41.1742356128,3.43894174696));
#74962=CARTESIAN_POINT('Origin',(6.24384247076,-41.6742356128,6.92091963994));
#74963=CARTESIAN_POINT('',(6.24384247076,-40.6742356128,5.17993069345));
#74964=CARTESIAN_POINT('Origin',(0.000416107150126,-40.1142356128,6.92091963994));
#74965=CARTESIAN_POINT('',(7.34384247076,-39.7742356128,6.92091963994));
#74966=CARTESIAN_POINT('',(7.34384247076,-40.7242356128,6.92091963994));
#74967=CARTESIAN_POINT('',(6.88660115785,-39.7742356128,9.47167760676));
#74968=CARTESIAN_POINT('Origin',(0.000416107150126,-39.7742356128,6.92091963994));
#74969=CARTESIAN_POINT('',(6.88660115785,-40.7242356128,9.47167760676));
#74970=CARTESIAN_POINT('Origin',(7.34384247076,-41.6742356128,6.92091963994));
#74971=CARTESIAN_POINT('',(7.34384247076,-39.7742356128,6.09541632002));
#74972=CARTESIAN_POINT('',(7.34384247076,-39.7742356128,5.5634594739));
#74973=CARTESIAN_POINT('',(7.34384247076,-40.7242356128,6.09541632002));
#74974=CARTESIAN_POINT('Origin',(6.52009030435,-41.6742356128,5.79623168551));
#74975=CARTESIAN_POINT('',(13.7266446428,-39.7742356128,8.41363339168));
#74976=CARTESIAN_POINT('',(13.7266446428,-40.7242356128,8.41363339168));
#74977=CARTESIAN_POINT('',(13.0544719111,-39.7742356128,8.16950201179));
#74978=CARTESIAN_POINT('',(13.390558277,-39.7742356128,8.29156770174));
#74979=CARTESIAN_POINT('',(10.1991571909,-39.7742356128,7.13245916591));
#74980=CARTESIAN_POINT('Origin',(-3.5527136788E-15,-37.9242356128,-8.88178104417E-16));
#74981=CARTESIAN_POINT('',(0.5,-39.7742356128,16.0922341519));
#74982=CARTESIAN_POINT('',(0.5,-40.7242356128,16.0922341519));
#74983=CARTESIAN_POINT('',(2.7,-39.7742356128,15.8719879032));
#74984=CARTESIAN_POINT('Origin',(-3.5527136788E-15,-39.7742356128,-8.88178104417E-16));
#74985=CARTESIAN_POINT('Origin',(-3.5527136788E-15,-39.7742356128,-8.88178104417E-16));
#74986=CARTESIAN_POINT('Origin',(0.5,-41.6742356128,13.1643460036));
#74987=CARTESIAN_POINT('',(0.5,-39.7742356128,14.2473325884));
#74988=CARTESIAN_POINT('',(0.5,-40.7242356128,14.2473325884));
#74989=CARTESIAN_POINT('',(0.5,-39.7742356128,15.1697833702));
#74990=CARTESIAN_POINT('Origin',(0.000416107150126,-40.1142356128,6.92091963994));
#74991=CARTESIAN_POINT('',(5.26789531411,-39.7742356128,12.0375174903));
#74992=CARTESIAN_POINT('Origin',(0.000416107150126,-39.7742356128,6.92091963994));
#74993=CARTESIAN_POINT('',(5.26789531411,-40.7242356128,12.0375174903));
#74994=CARTESIAN_POINT('Origin',(7.48272894647,-41.3342356129,11.6412701168));
#74995=CARTESIAN_POINT('',(9.71115043835,-39.7742356128,11.952136092));
#74996=CARTESIAN_POINT('',(9.73272894647,-39.7742356128,11.6412701168));
#74997=CARTESIAN_POINT('Origin',(7.48272894647,-39.7742356128,11.6412701168));
#74998=CARTESIAN_POINT('',(6.84013384355,-39.7742356128,13.7975566316));
#74999=CARTESIAN_POINT('Origin',(7.48272894647,-39.7742356128,11.6412701168));
#75000=CARTESIAN_POINT('Origin',(7.48272894647,-39.7742356128,11.6412701168));
#75001=CARTESIAN_POINT('Origin',(7.48272894647,-39.7742356128,11.6412701168));
#75002=CARTESIAN_POINT('',(9.73272894647,-43.9742356128,11.6412701168));
#75003=CARTESIAN_POINT('',(9.73272894647,-41.3342356129,11.6412701168));
#75004=CARTESIAN_POINT('',(5.23272894647,-43.9742356128,11.6412701168));
#75005=CARTESIAN_POINT('Origin',(7.48272894647,-43.9742356128,11.6412701168));
#75006=CARTESIAN_POINT('Origin',(7.48272894647,-43.9742356128,11.6412701168));
#75007=CARTESIAN_POINT('Origin',(-3.35265884719E-30,-39.7742356128,3.15283103411E-22));
#75008=CARTESIAN_POINT('Origin',(-3.35265884719E-30,-39.2742356128,3.15283103411E-22));
#75009=CARTESIAN_POINT('',(-3.7,-39.2742356128,0.));
#75010=CARTESIAN_POINT('Origin',(-3.7,-34.1742356128,16.9339894886));
#75011=CARTESIAN_POINT('',(-3.7,-35.1742356128,15.977171214));
#75012=CARTESIAN_POINT('',(-3.7,-35.1742356128,16.4899553024));
#75013=CARTESIAN_POINT('',(-3.7,-37.2242356128,15.977171214));
#75014=CARTESIAN_POINT('Origin',(-14.2514385284,-38.7742356128,2.4));
#75015=CARTESIAN_POINT('',(-14.2514385284,-33.4742356128,2.4));
#75016=CARTESIAN_POINT('',(-14.2514385284,-38.7742356128,2.4));
#75017=CARTESIAN_POINT('',(-14.2514385284,-36.1242356128,2.4));
#75018=CARTESIAN_POINT('',(-16.5266451526,-33.4742356128,2.4));
#75019=CARTESIAN_POINT('',(-15.3890418405,-33.4742356128,2.4));
#75020=CARTESIAN_POINT('',(-16.5266451526,-34.4742356128,2.4));
#75021=CARTESIAN_POINT('',(-16.5266451526,-33.9742356128,2.4));
#75022=CARTESIAN_POINT('',(-16.3750424925,-34.4742356128,2.4));
#75023=CARTESIAN_POINT('',(-15.2118374958,-37.2742356128,2.4));
#75024=CARTESIAN_POINT('',(-15.7176386641,-37.2742356128,2.4));
#75025=CARTESIAN_POINT('',(-15.2118374958,-38.7742356128,2.4));
#75026=CARTESIAN_POINT('',(-15.2118374958,-38.0242356128,2.4));
#75027=CARTESIAN_POINT('',(-14.7316380121,-38.7742356128,2.4));
#75028=CARTESIAN_POINT('Origin',(-3.35265884719E-30,-34.4742356128,3.15283103411E-22));
#75029=CARTESIAN_POINT('',(-16.5266451526,-34.4742356128,-2.4));
#75030=CARTESIAN_POINT('Origin',(6.66133814775094E-15,-34.4742356128,3.71924713249427E-14));
#75031=CARTESIAN_POINT('',(-15.8187195902,-34.4742356128,-2.4));
#75032=CARTESIAN_POINT('Origin',(-14.2514385284,-38.7742356128,-2.4));
#75033=CARTESIAN_POINT('',(-14.2514385284,-38.7742356128,-2.4));
#75034=CARTESIAN_POINT('',(-15.2118374958,-38.7742356128,-2.4));
#75035=CARTESIAN_POINT('',(-14.7316380121,-38.7742356128,-2.4));
#75036=CARTESIAN_POINT('',(-15.2118374958,-37.2742356128,-2.4));
#75037=CARTESIAN_POINT('',(-15.2118374958,-38.0242356128,-2.4));
#75038=CARTESIAN_POINT('',(-15.7176386641,-37.2742356128,-2.4));
#75039=CARTESIAN_POINT('',(-16.5266451526,-33.4742356128,-2.4));
#75040=CARTESIAN_POINT('',(-16.5266451526,-33.9742356128,-2.4));
#75041=CARTESIAN_POINT('',(-14.2514385284,-33.4742356128,-2.4));
#75042=CARTESIAN_POINT('',(-15.3890418405,-33.4742356128,-2.4));
#75043=CARTESIAN_POINT('',(-14.2514385284,-36.1242356128,-2.4));
#75044=CARTESIAN_POINT('Origin',(-4.7,-34.1742356128,-14.1421356237));
#75045=CARTESIAN_POINT('',(-4.7,-35.1742356128,-15.7120972502));
#75046=CARTESIAN_POINT('',(-4.7,-35.1742356128,-16.2330883256));
#75047=CARTESIAN_POINT('',(-4.7,-39.2742356128,-16.2330883256));
#75048=CARTESIAN_POINT('',(-4.7,-37.2242356128,-15.7120972502));
#75049=CARTESIAN_POINT('Origin',(-3.35265884719E-30,-39.2742356128,3.15283103411E-22));
#75050=CARTESIAN_POINT('Origin',(-3.35265884719E-30,-39.2742356128,3.15283103411E-22));
#75051=CARTESIAN_POINT('',(3.7,-39.2742356128,0.));
#75052=CARTESIAN_POINT('Origin',(3.7,-34.1742356128,16.9339894886));
#75053=CARTESIAN_POINT('',(3.7,-35.1742356128,15.977171214));
#75054=CARTESIAN_POINT('',(3.7,-37.2242356128,15.977171214));
#75055=CARTESIAN_POINT('',(3.7,-35.1742356128,16.4899553024));
#75056=CARTESIAN_POINT('Origin',(-3.35265884719E-30,-39.2742356128,3.15283103411E-22));
#75057=CARTESIAN_POINT('',(4.7,-39.2742356128,0.));
#75058=CARTESIAN_POINT('Origin',(4.7,-34.1742356128,-14.1421356237));
#75059=CARTESIAN_POINT('',(4.7,-35.1742356128,-15.7120972502));
#75060=CARTESIAN_POINT('',(4.7,-37.2242356128,-15.7120972502));
#75061=CARTESIAN_POINT('',(4.7,-35.1742356128,-16.2330883256));
#75062=CARTESIAN_POINT('Origin',(-14.2514385284,-38.7742356128,-2.4));
#75063=CARTESIAN_POINT('',(15.2118374958,-37.2742356128,-2.4));
#75064=CARTESIAN_POINT('',(15.7176386641,-37.2742356128,-2.4));
#75065=CARTESIAN_POINT('',(15.2118374958,-38.7742356128,-2.4));
#75066=CARTESIAN_POINT('',(15.2118374958,-38.0242356128,-2.4));
#75067=CARTESIAN_POINT('',(14.2514385284,-38.7742356128,-2.4));
#75068=CARTESIAN_POINT('',(14.7316380121,-38.7742356128,-2.4));
#75069=CARTESIAN_POINT('',(14.2514385284,-33.4742356128,-2.4));
#75070=CARTESIAN_POINT('',(14.2514385284,-36.1242356128,-2.4));
#75071=CARTESIAN_POINT('',(16.5266451526,-33.4742356128,-2.4));
#75072=CARTESIAN_POINT('',(15.3890418405,-33.4742356128,-2.4));
#75073=CARTESIAN_POINT('',(16.5266451526,-34.4742356128,-2.4));
#75074=CARTESIAN_POINT('',(16.5266451526,-33.9742356128,-2.4));
#75075=CARTESIAN_POINT('',(16.3750424925,-34.4742356128,-2.4));
#75076=CARTESIAN_POINT('Origin',(-3.35265884719E-30,-34.4742356128,3.15283103411E-22));
#75077=CARTESIAN_POINT('',(16.5266451526,-34.4742356128,2.4));
#75078=CARTESIAN_POINT('Origin',(-6.66133814775094E-15,-34.4742356128004,
3.71924713249427E-14));
#75079=CARTESIAN_POINT('',(-15.8187195902,-34.4742356128,2.4));
#75080=CARTESIAN_POINT('Origin',(-14.2514385284,-38.7742356128,2.4));
#75081=CARTESIAN_POINT('',(16.5266451526,-33.4742356128,2.4));
#75082=CARTESIAN_POINT('',(16.5266451526,-33.9742356128,2.4));
#75083=CARTESIAN_POINT('',(14.2514385284,-33.4742356128,2.4));
#75084=CARTESIAN_POINT('',(15.3890418405,-33.4742356128,2.4));
#75085=CARTESIAN_POINT('',(14.2514385284,-38.7742356128,2.4));
#75086=CARTESIAN_POINT('',(14.2514385284,-36.1242356128,2.4));
#75087=CARTESIAN_POINT('',(15.2118374958,-38.7742356128,2.4));
#75088=CARTESIAN_POINT('',(14.7316380121,-38.7742356128,2.4));
#75089=CARTESIAN_POINT('',(15.2118374958,-37.2742356128,2.4));
#75090=CARTESIAN_POINT('',(15.2118374958,-38.0242356128,2.4));
#75091=CARTESIAN_POINT('',(15.7176386641,-37.2742356128,2.4));
#75092=CARTESIAN_POINT('Origin',(-3.35265884719E-30,-34.4742356128,3.15283103411E-22));
#75093=CARTESIAN_POINT('',(4.,-34.4742356128,-15.9047162817));
#75094=CARTESIAN_POINT('',(4.,-34.4742356128,0.));
#75095=CARTESIAN_POINT('',(-4.,-34.4742356128,-15.9047162817));
#75096=CARTESIAN_POINT('',(-4.,-34.4742356128,0.));
#75097=CARTESIAN_POINT('Origin',(1.09356967925578E-13,-34.4742356128,9.10382880192628E-14));
#75098=CARTESIAN_POINT('Origin',(4.,-35.1742356128,-16.5096094651));
#75099=CARTESIAN_POINT('Ctrl Pts',(4.,-34.4742356128,-15.9047162816568));
#75100=CARTESIAN_POINT('Ctrl Pts',(4.0884342264605,-34.4742356127987,-15.8824752746765));
#75101=CARTESIAN_POINT('Ctrl Pts',(4.18270996429947,-34.4919847748025,-15.8579009499871));
#75102=CARTESIAN_POINT('Ctrl Pts',(4.35634416466974,-34.5644258306867,-15.8110831603776));
#75103=CARTESIAN_POINT('Ctrl Pts',(4.43571134875728,-34.6191227440986,-15.7888798171352));
#75104=CARTESIAN_POINT('Ctrl Pts',(4.55893320645631,-34.7441108613033,-15.7537322365075));
#75105=CARTESIAN_POINT('Ctrl Pts',(4.61190458227807,-34.821900720567,-15.738223817141));
#75106=CARTESIAN_POINT('Ctrl Pts',(4.68245030316865,-34.9930487805266,-15.7173792968254));
#75107=CARTESIAN_POINT('Ctrl Pts',(4.7,-35.0864237188467,-15.7120972502082));
#75108=CARTESIAN_POINT('Ctrl Pts',(4.7,-35.1742356128,-15.7120972502082));
#75109=CARTESIAN_POINT('Origin',(-4.,-35.1742356128,-16.5096094651));
#75110=CARTESIAN_POINT('Ctrl Pts',(-4.,-34.4742356128,-15.9047162816568));
#75111=CARTESIAN_POINT('Ctrl Pts',(-4.0884342264605,-34.4742356127987,-15.8824752746765));
#75112=CARTESIAN_POINT('Ctrl Pts',(-4.18270996429947,-34.4919847748025,
-15.8579009499871));
#75113=CARTESIAN_POINT('Ctrl Pts',(-4.35634416466974,-34.5644258306867,
-15.8110831603776));
#75114=CARTESIAN_POINT('Ctrl Pts',(-4.43571134875728,-34.6191227440986,
-15.7888798171352));
#75115=CARTESIAN_POINT('Ctrl Pts',(-4.55893320645631,-34.7441108613033,
-15.7537322365075));
#75116=CARTESIAN_POINT('Ctrl Pts',(-4.61190458227807,-34.821900720567,-15.738223817141));
#75117=CARTESIAN_POINT('Ctrl Pts',(-4.68245030316865,-34.9930487805266,
-15.7173792968254));
#75118=CARTESIAN_POINT('Ctrl Pts',(-4.7,-35.0864237188467,-15.7120972502082));
#75119=CARTESIAN_POINT('Ctrl Pts',(-4.7,-35.1742356128,-15.7120972502082));
#75120=CARTESIAN_POINT('Origin',(-3.35265884719E-30,-39.7742356128,3.15283103411E-22));
#75121=CARTESIAN_POINT('',(-3.7,-39.7742356128,-14.9489130039));
#75122=CARTESIAN_POINT('',(-3.7,-39.7742356128,0.0995229481798));
#75123=CARTESIAN_POINT('Ctrl Pts',(-3.7,-39.7742356128,-14.9489130039));
#75124=CARTESIAN_POINT('Ctrl Pts',(-7.0053528771,-39.7742356128,-14.13080632));
#75125=CARTESIAN_POINT('Ctrl Pts',(-10.0851737187,-39.7742356128,-12.3997944898));
#75126=CARTESIAN_POINT('Ctrl Pts',(-12.5992021916,-39.7742356128,-9.8349243241));
#75127=CARTESIAN_POINT('Ctrl Pts',(-14.2682129749,-39.7742356128,-6.72106797252));
#75128=CARTESIAN_POINT('Ctrl Pts',(-15.0199866844,-39.7742356128,-3.4));
#75129=CARTESIAN_POINT('Origin',(-3.35265884719E-30,-39.7742356128,3.15283103411E-22));
#75130=CARTESIAN_POINT('',(1.34531962036,-39.7742356128,-9.93626746742));
#75131=CARTESIAN_POINT('Ctrl Pts',(1.34531962036,-39.7742356128,-9.93626746742));
#75132=CARTESIAN_POINT('Ctrl Pts',(1.61677669863,-39.7742356128,-9.89864634179));
#75133=CARTESIAN_POINT('Ctrl Pts',(1.86584893824,-39.7742356128,-9.86245065748));
#75134=CARTESIAN_POINT('Ctrl Pts',(2.0496779846,-39.7742356128,-9.83314926899));
#75135=CARTESIAN_POINT('Ctrl Pts',(2.23813956402,-39.7742356128,-9.79905599631));
#75136=CARTESIAN_POINT('Ctrl Pts',(2.42784894914,-39.7742356128,-9.76089341103));
#75137=CARTESIAN_POINT('',(-1.34531962036,-39.7742356128,-9.93626746742));
#75138=CARTESIAN_POINT('Origin',(-1.99840144432528E-14,-39.7742356128,-2.6737364819903));
#75139=CARTESIAN_POINT('Ctrl Pts',(-1.34531962036,-39.7742356128,-9.93626746742));
#75140=CARTESIAN_POINT('Ctrl Pts',(-1.61677669863,-39.7742356128,-9.89864634179));
#75141=CARTESIAN_POINT('Ctrl Pts',(-1.86584893824,-39.7742356128,-9.86245065748));
#75142=CARTESIAN_POINT('Ctrl Pts',(-2.0496779846,-39.7742356128,-9.83314926899));
#75143=CARTESIAN_POINT('Ctrl Pts',(-2.23813956402,-39.7742356128,-9.79905599631));
#75144=CARTESIAN_POINT('Ctrl Pts',(-2.42784894914,-39.7742356128,-9.76089341103));
#75145=CARTESIAN_POINT('',(3.7,-39.7742356128,-14.9489130039));
#75146=CARTESIAN_POINT('',(3.7,-39.7742356128,0.717649133781));
#75147=CARTESIAN_POINT('Ctrl Pts',(15.0199866844,-39.7742356128,-3.4));
#75148=CARTESIAN_POINT('Ctrl Pts',(14.2682129749,-39.7742356128,-6.72106797252));
#75149=CARTESIAN_POINT('Ctrl Pts',(12.5992021916,-39.7742356128,-9.8349243241));
#75150=CARTESIAN_POINT('Ctrl Pts',(10.0851737187,-39.7742356128,-12.3997944898));
#75151=CARTESIAN_POINT('Ctrl Pts',(7.0053528771,-39.7742356128,-14.13080632));
#75152=CARTESIAN_POINT('Ctrl Pts',(3.7,-39.7742356128,-14.9489130039));
#75153=CARTESIAN_POINT('Origin',(-3.35265884719E-30,-39.7742356128,3.15283103411E-22));
#75154=CARTESIAN_POINT('Origin',(-3.35265884719E-30,-39.7742356128,3.15283103411E-22));
#75155=CARTESIAN_POINT('',(0.517273426056,-39.7742356128,-7.9495168227));
#75156=CARTESIAN_POINT('Ctrl Pts',(1.78291107349,-39.7742356128,-9.24906260055));
#75157=CARTESIAN_POINT('Ctrl Pts',(1.28116922679,-39.7742356128,-9.2357956341));
#75158=CARTESIAN_POINT('Ctrl Pts',(0.780312185558,-39.7742356128,-8.95942136571));
#75159=CARTESIAN_POINT('Ctrl Pts',(0.517273426057,-39.7742356128,-8.45143404011));
#75160=CARTESIAN_POINT('Ctrl Pts',(0.517273426056,-39.7742356128,-7.9495168227));
#75161=CARTESIAN_POINT('',(0.517273426056,-39.7742356128,0.717649133781));
#75162=CARTESIAN_POINT('',(-0.517273426056,-39.7742356128,-7.9495168227));
#75163=CARTESIAN_POINT('',(-0.517273426056,-39.7742356128,0.717649133781));
#75164=CARTESIAN_POINT('Ctrl Pts',(-0.517273426056,-39.7742356128,-7.9495168227));
#75165=CARTESIAN_POINT('Ctrl Pts',(-0.517273426057,-39.7742356128,-8.45143404011));
#75166=CARTESIAN_POINT('Ctrl Pts',(-0.780312185558,-39.7742356128,-8.95942136571));
#75167=CARTESIAN_POINT('Ctrl Pts',(-1.28116922679,-39.7742356128,-9.2357956341));
#75168=CARTESIAN_POINT('Ctrl Pts',(-1.78291107349,-39.7742356128,-9.24906260055));
#75169=CARTESIAN_POINT('Origin',(-3.35265884719E-30,-39.7742356128,3.15283103411E-22));
#75170=CARTESIAN_POINT('Origin',(-3.35265884719E-30,-39.7742356128,3.15283103411E-22));
#75171=CARTESIAN_POINT('Origin',(-3.35265884719E-30,-39.7742356128,3.15283103411E-22));
#75172=CARTESIAN_POINT('',(-7.4311653291,-39.7742356128,4.27488229452));
#75173=CARTESIAN_POINT('Ctrl Pts',(-9.78216646656,-39.7742356128,3.43958571397));
#75174=CARTESIAN_POINT('Ctrl Pts',(-9.44950651023,-39.7742356128,3.84219609922));
#75175=CARTESIAN_POINT('Ctrl Pts',(-9.03618230028,-39.7742356128,4.19379483572));
#75176=CARTESIAN_POINT('Ctrl Pts',(-8.49317585372,-39.7742356128,4.40265075658));
#75177=CARTESIAN_POINT('Ctrl Pts',(-7.94364631071,-39.7742356128,4.41424876979));
#75178=CARTESIAN_POINT('Ctrl Pts',(-7.4311653291,-39.7742356128,4.27488229452));
#75179=CARTESIAN_POINT('Origin',(-7.20379737374474,-39.7742356128,5.06830226500522));
#75180=CARTESIAN_POINT('Origin',(-3.35265884719E-30,-39.7742356128,3.15283103411E-22));
#75181=CARTESIAN_POINT('Origin',(-3.59850171520844,-39.7742356128,1.3458683859997));
#75182=CARTESIAN_POINT('Origin',(-3.35265884719E-30,-39.7742356128,3.15283103411E-22));
#75183=CARTESIAN_POINT('Origin',(-3.35265884719E-30,-39.7742356128,3.15283103411E-22));
#75184=CARTESIAN_POINT('',(-2.7,-39.7742356128,15.1614643092));
#75185=CARTESIAN_POINT('',(-2.7,-39.7742356128,0.717649133781));
#75186=CARTESIAN_POINT('Origin',(-1.20186252263148,-39.7742356128,3.64824670717903));
#75187=CARTESIAN_POINT('Origin',(-3.35265884719E-30,-39.7742356128,3.15283103411E-22));
#75188=CARTESIAN_POINT('Origin',(-2.87571670214971,-39.7742356128,2.54173286620876));
#75189=CARTESIAN_POINT('Origin',(-3.35265884719E-30,-39.7742356128,3.15283103411E-22));
#75190=CARTESIAN_POINT('Origin',(-7.48272894647,-43.9742356128,11.6412701168));
#75191=CARTESIAN_POINT('',(-9.23272894647,-44.4742356128,11.6412701168));
#75192=CARTESIAN_POINT('Origin',(-9.23272894647,-43.9742356128,11.6412701168));
#75193=CARTESIAN_POINT('Origin',(-7.48272894647,-44.4742356128,11.6412701168));
#75194=CARTESIAN_POINT('Origin',(-3.35265884719E-30,-40.6742356128,3.15283103411E-22));
#75195=CARTESIAN_POINT('',(4.89234685393,-40.6742356128,2.64607413014));
#75196=CARTESIAN_POINT('',(5.24384247076,-40.6742356128,3.12351150632));
#75197=CARTESIAN_POINT('Origin',(4.74384247076,-40.6742356128,3.12351150632));
#75198=CARTESIAN_POINT('',(0.48735027394,-40.6742356128,-2.10776590718));
#75199=CARTESIAN_POINT('Origin',(6.82290383517,-40.6742356128,-3.56061176027));
#75200=CARTESIAN_POINT('',(-0.48735027394,-40.6742356128,-2.10776590718));
#75201=CARTESIAN_POINT('Origin',(-4.99600361081E-16,-40.6742356128,-1.99600853387));
#75202=CARTESIAN_POINT('',(-4.89234685393,-40.6742356128,2.64607413014));
#75203=CARTESIAN_POINT('Origin',(-6.82290383517,-40.6742356128,-3.56061176027));
#75204=CARTESIAN_POINT('',(-5.24384247076,-40.6742356128,3.12351150632));
#75205=CARTESIAN_POINT('Origin',(-4.74384247076,-40.6742356128,3.12351150632));
#75206=CARTESIAN_POINT('',(-5.24384247076,-40.6742356128,6.92091963994));
#75207=CARTESIAN_POINT('',(-5.24384247076,-40.6742356128,5.02221557313));
#75208=CARTESIAN_POINT('',(-0.000416107143134986,-40.6742356128,12.1643459815524));
#75209=CARTESIAN_POINT('Origin',(-0.000416107150126,-40.6742356128,6.92091963994));
#75210=CARTESIAN_POINT('',(5.24384247076,-40.6742356128,6.92091963994));
#75211=CARTESIAN_POINT('Origin',(0.000416107150126,-40.6742356128,6.92091963994));
#75212=CARTESIAN_POINT('',(5.24384247076,-40.6742356128,5.02221557313));
#75213=CARTESIAN_POINT('',(12.3229038352,-40.6742356128,-3.56061176027));
#75214=CARTESIAN_POINT('Origin',(6.82290383517,-40.6742356128,-3.56061176027));
#75215=CARTESIAN_POINT('',(-12.3229038352,-40.6742356128,-3.56061176027));
#75216=CARTESIAN_POINT('Origin',(-6.82290383517,-40.6742356128,-3.56061176027));
#75217=CARTESIAN_POINT('Origin',(-3.35265884719E-30,-39.7742356128,3.15283103411E-22));
#75218=CARTESIAN_POINT('Origin',(2.87571670201055,-39.7742356128,2.54173286608641));
#75219=CARTESIAN_POINT('Origin',(-3.35265884719E-30,-39.7742356128,3.15283103411E-22));
#75220=CARTESIAN_POINT('',(2.7,-39.7742356128,15.1614643092));
#75221=CARTESIAN_POINT('',(2.7,-39.7742356128,0.0995229481798));
#75222=CARTESIAN_POINT('Origin',(1.20186252262849,-39.7742356128,3.64824670717053));
#75223=CARTESIAN_POINT('Origin',(-3.35265884719E-30,-39.7742356128,3.15283103411E-22));
#75224=CARTESIAN_POINT('Origin',(7.48272894647,-43.9742356128,11.6412701168));
#75225=CARTESIAN_POINT('',(5.73272894647,-44.4742356128,11.6412701168));
#75226=CARTESIAN_POINT('Origin',(5.73272894647,-43.9742356128,11.6412701168));
#75227=CARTESIAN_POINT('Origin',(7.48272894647,-44.4742356128,11.6412701168));
#75228=CARTESIAN_POINT('Origin',(-3.,-35.1742356128,16.6523581407));
#75229=CARTESIAN_POINT('',(-3.,-34.4742356128,16.1232751015));
#75230=CARTESIAN_POINT('',(-3.,-34.4742356128,16.5582997212));
#75231=CARTESIAN_POINT('Ctrl Pts',(-3.,-34.4742356128,16.1232751015419));
#75232=CARTESIAN_POINT('Ctrl Pts',(-3.08826358006266,-34.474235612801,16.1068522136037));
#75233=CARTESIAN_POINT('Ctrl Pts',(-3.182339037103,-34.491928240058,16.0885214326175));
#75234=CARTESIAN_POINT('Ctrl Pts',(-3.35547017666015,-34.5639636844578,
16.0533056885098));
#75235=CARTESIAN_POINT('Ctrl Pts',(-3.43453320463452,-34.618308389591,16.03646071159));
#75236=CARTESIAN_POINT('Ctrl Pts',(-3.55816883888233,-34.7429717428544,
16.0094769404987));
#75237=CARTESIAN_POINT('Ctrl Pts',(-3.61151559883288,-34.8211404463089,
15.9974459840977));
#75238=CARTESIAN_POINT('Ctrl Pts',(-3.68243855940585,-34.9928379015306,
15.9812693237053));
#75239=CARTESIAN_POINT('Ctrl Pts',(-3.7,-35.0863772305776,15.977171213954));
#75240=CARTESIAN_POINT('Ctrl Pts',(-3.7,-35.1742356128,15.977171213954));
#75241=CARTESIAN_POINT('Origin',(-3.5527136788E-15,-37.9242356128,-8.88178104417E-16));
#75242=CARTESIAN_POINT('',(3.,-34.4742356128,16.1232751015));
#75243=CARTESIAN_POINT('Origin',(-3.5527136788E-15,-34.4742356128,-8.88178104417E-16));
#75244=CARTESIAN_POINT('Ctrl Pts',(3.7,-35.1742356128,15.977171213954));
#75245=CARTESIAN_POINT('Ctrl Pts',(3.7,-35.0863772305776,15.977171213954));
#75246=CARTESIAN_POINT('Ctrl Pts',(3.68243855940585,-34.9928379015306,15.9812693237053));
#75247=CARTESIAN_POINT('Ctrl Pts',(3.61151559883287,-34.8211404463089,15.9974459840977));
#75248=CARTESIAN_POINT('Ctrl Pts',(3.55816883888233,-34.7429717428544,16.0094769404987));
#75249=CARTESIAN_POINT('Ctrl Pts',(3.43453320463452,-34.618308389591,16.03646071159));
#75250=CARTESIAN_POINT('Ctrl Pts',(3.35547017666015,-34.5639636844578,16.0533056885098));
#75251=CARTESIAN_POINT('Ctrl Pts',(3.182339037103,-34.491928240058,16.0885214326175));
#75252=CARTESIAN_POINT('Ctrl Pts',(3.08826358006266,-34.4742356128,16.1068522136038));
#75253=CARTESIAN_POINT('Ctrl Pts',(3.,-34.4742356128,16.1232751015419));
#75254=CARTESIAN_POINT('Origin',(-3.5527136788E-15,-37.2742356128,-8.88178104417E-16));
#75255=CARTESIAN_POINT('Origin',(-3.35265884719E-30,-38.2742356128,3.15283103411E-22));
#75256=CARTESIAN_POINT('',(-12.8848511691,-38.7742356128,8.43448933535));
#75257=CARTESIAN_POINT('',(-12.8848511691,-37.2742356128,8.43448933535));
#75258=CARTESIAN_POINT('',(-12.8848511691,-38.2742356128,8.43448933535));
#75259=CARTESIAN_POINT('Origin',(-3.35265884719E-30,-38.7742356128,3.15283103411E-22));
#75260=CARTESIAN_POINT('Origin',(-3.35265884719E-30,-37.2742356128,3.15283103411E-22));
#75261=CARTESIAN_POINT('Origin',(-3.35265884719E-30,-36.1242356128,3.15283103411E-22));
#75262=CARTESIAN_POINT('',(-9.94046468191,-38.7742356128,11.7621070351));
#75263=CARTESIAN_POINT('',(-12.1387953782,-38.7742356128,9.47679517369));
#75264=CARTESIAN_POINT('Origin',(-3.35265884719E-30,-38.7742356128,3.15283103411E-22));
#75265=CARTESIAN_POINT('',(-12.1387953782,-33.7742356128,9.47679517369));
#75266=CARTESIAN_POINT('',(-12.1387953782,-36.1242356128,9.47679517369));
#75267=CARTESIAN_POINT('',(-9.94046468191,-33.7742356128,11.7621070351));
#75268=CARTESIAN_POINT('Origin',(-3.35265884719E-30,-33.7742356128,3.15283103411E-22));
#75269=CARTESIAN_POINT('',(-9.94046468191,-36.1242356128,11.7621070351));
#75270=CARTESIAN_POINT('Origin',(-3.35265884719E-30,-38.2742356128,3.15283103411E-22));
#75271=CARTESIAN_POINT('',(-8.92662908173,-38.7742356128,12.5489160184));
#75272=CARTESIAN_POINT('',(-8.92662908173,-37.2742356128,12.5489160184));
#75273=CARTESIAN_POINT('',(-8.92662908173,-38.2742356128,12.5489160184));
#75274=CARTESIAN_POINT('',(-0.5,-37.2742356128,15.3918809766));
#75275=CARTESIAN_POINT('Origin',(-3.35265884719E-30,-37.2742356128,3.15283103411E-22));
#75276=CARTESIAN_POINT('',(-0.5,-38.7742356128,15.3918809766));
#75277=CARTESIAN_POINT('',(-0.5,-38.2742356128,15.3918809766));
#75278=CARTESIAN_POINT('Origin',(-3.35265884719E-30,-38.7742356128,3.15283103411E-22));
#75279=CARTESIAN_POINT('Origin',(-3.35265884719E-30,-38.2742356128,3.15283103411E-22));
#75280=CARTESIAN_POINT('',(9.33467257157,-38.7742356128,12.2484238978));
#75281=CARTESIAN_POINT('',(9.33467257157,-37.2742356128,12.2484238978));
#75282=CARTESIAN_POINT('',(9.33467257157,-38.2742356128,12.2484238978));
#75283=CARTESIAN_POINT('',(0.5,-38.7742356128,15.3918809766));
#75284=CARTESIAN_POINT('Origin',(-3.35265884719E-30,-38.7742356128,3.15283103411E-22));
#75285=CARTESIAN_POINT('',(0.5,-37.2742356128,15.3918809766));
#75286=CARTESIAN_POINT('',(0.5,-38.2742356128,15.3918809766));
#75287=CARTESIAN_POINT('Origin',(-3.35265884719E-30,-37.2742356128,3.15283103411E-22));
#75288=CARTESIAN_POINT('Origin',(-3.35265884719E-30,-36.1242356128,3.15283103411E-22));
#75289=CARTESIAN_POINT('',(11.816958431,-38.7742356128,9.87519586841));
#75290=CARTESIAN_POINT('',(10.3256459325,-38.7742356128,11.4254556179));
#75291=CARTESIAN_POINT('Origin',(-3.35265884719E-30,-38.7742356128,3.15283103411E-22));
#75292=CARTESIAN_POINT('',(10.3256459325,-33.7742356128,11.4254556179));
#75293=CARTESIAN_POINT('',(10.3256459325,-36.1242356128,11.4254556179));
#75294=CARTESIAN_POINT('',(11.816958431,-33.7742356128,9.87519586841));
#75295=CARTESIAN_POINT('Origin',(-3.35265884719E-30,-33.7742356128,3.15283103411E-22));
#75296=CARTESIAN_POINT('',(11.816958431,-36.1242356128,9.87519586841));
#75297=CARTESIAN_POINT('Origin',(-3.35265884719E-30,-38.2742356128,3.15283103411E-22));
#75298=CARTESIAN_POINT('',(12.5997104365,-38.7742356128,8.85478949011));
#75299=CARTESIAN_POINT('',(12.5997104365,-37.2742356128,8.85478949011));
#75300=CARTESIAN_POINT('',(12.5997104365,-38.2742356128,8.85478949011));
#75301=CARTESIAN_POINT('Origin',(-3.35265884719E-30,-37.2742356128,3.15283103411E-22));
#75302=CARTESIAN_POINT('Origin',(-3.35265884719E-30,-38.7742356128,3.15283103411E-22));
#75303=CARTESIAN_POINT('Origin',(-14.2514385284,-41.6742356128,2.4));
#75304=CARTESIAN_POINT('',(-14.2514385284,-33.4742356128,0.));
#75305=CARTESIAN_POINT('',(-14.2514385284,-38.7742356128,0.));
#75306=CARTESIAN_POINT('Origin',(-3.35265884719E-30,-33.4742356128,3.15283103411E-22));
#75307=CARTESIAN_POINT('Origin',(-3.35265884719E-30,-33.4742356128,3.15283103411E-22));
#75308=CARTESIAN_POINT('Origin',(-3.35265884719E-30,-38.1842356129,3.15283103411E-22));
#75309=CARTESIAN_POINT('Origin',(-3.35265884719E-30,-38.7742356128,3.15283103411E-22));
#75310=CARTESIAN_POINT('',(-9.33467257157,-38.7742356128,-12.2484238978));
#75311=CARTESIAN_POINT('',(-6.35435667676,-38.7742356128,-9.34315312398));
#75312=CARTESIAN_POINT('',(-9.33467257157,-38.7742356128,-12.2484238978));
#75313=CARTESIAN_POINT('',(-1.48259713265,-38.7742356128,-10.9268000942));
#75314=CARTESIAN_POINT('Ctrl Pts',(-1.48259713264981,-38.7742356128,-10.9268000941986));
#75315=CARTESIAN_POINT('Ctrl Pts',(-1.71328083841,-38.7742356128,-10.8948297336));
#75316=CARTESIAN_POINT('Ctrl Pts',(-1.91354623838,-38.7742356128,-10.8659465412));
#75317=CARTESIAN_POINT('Ctrl Pts',(-2.0855726443,-38.7742356128,-10.8395401686));
#75318=CARTESIAN_POINT('Ctrl Pts',(-3.07854611663017,-38.7742356128,-10.6733698534772));
#75319=CARTESIAN_POINT('Ctrl Pts',(-4.05813867421687,-38.7742356128,-10.4126758711406));
#75320=CARTESIAN_POINT('Ctrl Pts',(-4.86043811085114,-38.7742356128,-10.1190200263027));
#75321=CARTESIAN_POINT('Ctrl Pts',(-5.62475805695127,-38.7742356128,-9.76080244433856));
#75322=CARTESIAN_POINT('Ctrl Pts',(-6.35435667676406,-38.7742356128,-9.34315312398709));
#75323=CARTESIAN_POINT('',(-0.5,-38.7742356128,-11.0174674429));
#75324=CARTESIAN_POINT('Origin',(2.38004060904018E-14,-38.7742356128,-0.229047725439793));
#75325=CARTESIAN_POINT('',(-0.5,-38.7742356128,-15.3918809766));
#75326=CARTESIAN_POINT('',(-0.5,-38.7742356128,0.));
#75327=CARTESIAN_POINT('Origin',(2.22044604925031E-15,-38.7742356128,-2.88657986402541E-14));
#75328=CARTESIAN_POINT('Origin',(-3.35265884719E-30,-38.7742356128,3.15283103411E-22));
#75329=CARTESIAN_POINT('',(-11.816958431,-38.7742356128,-9.87519586841));
#75330=CARTESIAN_POINT('',(-10.3256459325,-38.7742356128,-11.4254556179));
#75331=CARTESIAN_POINT('Origin',(4.59632332194815E-13,-38.7742356128,3.530509218308E-13));
#75332=CARTESIAN_POINT('',(-11.7961681305,-38.7742356128,-9.46800252678));
#75333=CARTESIAN_POINT('Origin',(-11.586757942,-38.7742356128,-9.68282192292));
#75334=CARTESIAN_POINT('',(-9.33306511227,-38.7742356128,-7.06692107621));
#75335=CARTESIAN_POINT('',(-11.7961681305,-38.7742356128,-9.46800252678));
#75336=CARTESIAN_POINT('',(-7.22695685732,-38.7742356128,-8.79725906681));
#75337=CARTESIAN_POINT('Ctrl Pts',(-7.22695685732232,-38.7742356128,-8.79725906681339));
#75338=CARTESIAN_POINT('Ctrl Pts',(-7.28150888554724,-38.7742356128,-8.76017689804407));
#75339=CARTESIAN_POINT('Ctrl Pts',(-7.3358430836494,-38.7742356128,-8.72268025917252));
#75340=CARTESIAN_POINT('Ctrl Pts',(-7.3899712392707,-38.7742356128,-8.68477139569698));
#75341=CARTESIAN_POINT('Ctrl Pts',(-7.46720182448399,-38.7742356128,-8.63068265616057));
#75342=CARTESIAN_POINT('Ctrl Pts',(-7.54401747222364,-38.7742356128,-8.57575348443564));
#75343=CARTESIAN_POINT('Ctrl Pts',(-7.6205551490896,-38.7742356128,-8.51991134544531));
#75344=CARTESIAN_POINT('Ctrl Pts',(-7.69952766934175,-38.7742356128,-8.46229273676896));
#75345=CARTESIAN_POINT('Ctrl Pts',(-7.77820421333981,-38.7742356128,-8.40370214573728));
#75346=CARTESIAN_POINT('Ctrl Pts',(-7.85668116624427,-38.7742356128,-8.34407402226636));
#75347=CARTESIAN_POINT('Ctrl Pts',(-7.9369257319336,-38.7742356128,-8.28310283653978));
#75348=CARTESIAN_POINT('Ctrl Pts',(-8.01696145430612,-38.7742356128,-8.2210468784774));
#75349=CARTESIAN_POINT('Ctrl Pts',(-8.09683736040204,-38.7742356128,-8.15785041906033));
#75350=CARTESIAN_POINT('Ctrl Pts',(-8.17873759713216,-38.7742356128,-8.09305234364884));
#75351=CARTESIAN_POINT('Ctrl Pts',(-8.26046963077621,-38.7742356128,-8.02705525395073));
#75352=CARTESIAN_POINT('Ctrl Pts',(-8.34203275379583,-38.7742356128,-7.95981359656426));
#75353=CARTESIAN_POINT('Ctrl Pts',(-8.42751622477607,-38.7742356128,-7.88933995535172));
#75354=CARTESIAN_POINT('Ctrl Pts',(-8.51281409409125,-38.7742356128,-7.81749921791734));
#75355=CARTESIAN_POINT('Ctrl Pts',(-8.59786908945091,-38.7742356128,-7.74425465003792));
#75356=CARTESIAN_POINT('Ctrl Pts',(-8.68560880784547,-38.7742356128,-7.66869815000525));
#75357=CARTESIAN_POINT('Ctrl Pts',(-8.77308976965873,-38.7742356128,-7.59164784533776));
#75358=CARTESIAN_POINT('Ctrl Pts',(-8.86019351231532,-38.7742356128,-7.51307941783206));
#75359=CARTESIAN_POINT('Ctrl Pts',(-8.95286440609457,-38.7742356128,-7.42948936558264));
#75360=CARTESIAN_POINT('Ctrl Pts',(-9.04510813530844,-38.7742356128,-7.34418092104821));
#75361=CARTESIAN_POINT('Ctrl Pts',(-9.13672354646749,-38.7742356128,-7.257142461433));
#75362=CARTESIAN_POINT('Ctrl Pts',(-9.20252620421849,-38.7742356128,-7.1946271935673));
#75363=CARTESIAN_POINT('Ctrl Pts',(-9.26800342965979,-38.7742356128,-7.1312198308518));
#75364=CARTESIAN_POINT('Ctrl Pts',(-9.33306511226659,-38.7742356128,-7.06692107620598));
#75365=CARTESIAN_POINT('',(-9.91508679725,-38.7742356128,-11.4177012033));
#75366=CARTESIAN_POINT('',(-9.91508679725,-38.7742356128,-11.4177012033));
#75367=CARTESIAN_POINT('Origin',(-10.1244969857,-38.7742356128,-11.2028818071));
#75368=CARTESIAN_POINT('Origin',(-3.35265884719E-30,-38.7742356128,3.15283103411E-22));
#75369=CARTESIAN_POINT('',(-12.5997104365,-38.7742356128,-8.85478949011));
#75370=CARTESIAN_POINT('',(-10.0162216343,-38.7742356128,-6.33635360057));
#75371=CARTESIAN_POINT('',(-12.5997104365,-38.7742356128,-8.85478949011));
#75372=CARTESIAN_POINT('Origin',(2.44249065417534E-14,-38.7742356128,-4.38538094726937E-14));
#75373=CARTESIAN_POINT('',(-11.9679209449,-38.7742356128,7.54064765005));
#75374=CARTESIAN_POINT('',(-11.9679209449,-38.7742356128,7.54064765005));
#75375=CARTESIAN_POINT('',(-11.5436913602,-38.7742356128,7.54605685771));
#75376=CARTESIAN_POINT('Origin',(-11.7585107564,-38.7742356128,7.7554670462));
#75377=CARTESIAN_POINT('',(-11.2644777756,-38.7742356128,7.83248271924));
#75378=CARTESIAN_POINT('',(-11.5436913602,-38.7742356128,7.54605685771));
#75379=CARTESIAN_POINT('',(-11.2698869833,-38.7742356128,8.25671230387));
#75380=CARTESIAN_POINT('Origin',(-11.4792971717,-38.7742356128,8.04189290772));
#75381=CARTESIAN_POINT('',(-12.1117355269,-38.7742356128,9.07736288456));
#75382=CARTESIAN_POINT('',(-11.2698869833,-38.7742356128,8.25671230387));
#75383=CARTESIAN_POINT('Origin',(-11.9023253384,-38.7742356128,9.2921822807));
#75384=CARTESIAN_POINT('',(-9.53740907755,-38.7742356128,11.7477944761));
#75385=CARTESIAN_POINT('Origin',(-9.74681926603,-38.7742356128,11.5329750799));
#75386=CARTESIAN_POINT('',(-8.68076107776,-38.7742356128,10.9127170933));
#75387=CARTESIAN_POINT('',(-8.68076107776,-38.7742356128,10.9127170933));
#75388=CARTESIAN_POINT('',(-8.25653149313,-38.7742356128,10.918126301));
#75389=CARTESIAN_POINT('Origin',(-8.47135088927,-38.7742356128,11.1275364894));
#75390=CARTESIAN_POINT('',(-7.97731790849,-38.7742356128,11.2045521625));
#75391=CARTESIAN_POINT('',(-8.25653149313,-38.7742356128,10.918126301));
#75392=CARTESIAN_POINT('',(-7.98272711615,-38.7742356128,11.6287817471));
#75393=CARTESIAN_POINT('Origin',(-8.19213730463,-38.7742356128,11.413962351));
#75394=CARTESIAN_POINT('',(-7.98272711615,-38.7742356128,11.6287817471));
#75395=CARTESIAN_POINT('',(-0.5,-38.7742356128,12.4465469186));
#75396=CARTESIAN_POINT('',(-0.5,-38.7742356128,0.));
#75397=CARTESIAN_POINT('',(-7.04251644773,-38.7742356128,5.33751720019));
#75398=CARTESIAN_POINT('Origin',(0.000416107150123801,-38.7742356128,5.42091963994));
#75399=CARTESIAN_POINT('',(-7.16875088157,-38.7742356128,5.23983755655));
#75400=CARTESIAN_POINT('Origin',(-7.14250943682,-38.7742356128,5.33633308276));
#75401=CARTESIAN_POINT('',(-11.0086556946,-38.7742356128,3.43000353527));
#75402=CARTESIAN_POINT('Ctrl Pts',(-11.0086556946,-38.7742356128,3.43000353527));
#75403=CARTESIAN_POINT('Ctrl Pts',(-10.8267791086,-38.7742356128,3.7279970062));
#75404=CARTESIAN_POINT('Ctrl Pts',(-10.6180941124,-38.7742356128,4.02812460647));
#75405=CARTESIAN_POINT('Ctrl Pts',(-10.3610804417,-38.7742356128,4.34854162483));
#75406=CARTESIAN_POINT('Ctrl Pts',(-9.81894561437,-38.7742356128,4.82846996464));
#75407=CARTESIAN_POINT('Ctrl Pts',(-9.1449448519,-38.7742356128,5.15260465424));
#75408=CARTESIAN_POINT('Ctrl Pts',(-8.86735473037,-38.7742356128,5.24791616482));
#75409=CARTESIAN_POINT('Ctrl Pts',(-8.35592834321,-38.7742356128,5.35778460397));
#75410=CARTESIAN_POINT('Ctrl Pts',(-7.83459380784,-38.7742356128,5.3594412401));
#75411=CARTESIAN_POINT('Ctrl Pts',(-7.6075384225,-38.7742356128,5.33903210576));
#75412=CARTESIAN_POINT('Ctrl Pts',(-7.38481168145,-38.7742356128,5.2985941411));
#75413=CARTESIAN_POINT('Ctrl Pts',(-7.16875088157,-38.7742356128,5.23983755655));
#75414=CARTESIAN_POINT('',(-11.8354184104,-38.7742356128,0.924526608307));
#75415=CARTESIAN_POINT('Ctrl Pts',(-11.0086556946,-38.7742356128,3.43000353527));
#75416=CARTESIAN_POINT('Ctrl Pts',(-11.0817932058,-38.7742356128,3.31017227332));
#75417=CARTESIAN_POINT('Ctrl Pts',(-11.1567853729,-38.7742356128,3.18040212706));
#75418=CARTESIAN_POINT('Ctrl Pts',(-11.2288017566,-38.7742356128,3.0447194315));
#75419=CARTESIAN_POINT('Ctrl Pts',(-11.4529799792,-38.7742356128,2.57934328034));
#75420=CARTESIAN_POINT('Ctrl Pts',(-11.6140362762,-38.7742356128,2.09446235244));
#75421=CARTESIAN_POINT('Ctrl Pts',(-11.6871718767,-38.7742356128,1.76491172368));
#75422=CARTESIAN_POINT('Ctrl Pts',(-11.7534189237,-38.7742356128,1.41966067629));
#75423=CARTESIAN_POINT('Ctrl Pts',(-11.809039671,-38.7742356128,1.08859783468));
#75424=CARTESIAN_POINT('Ctrl Pts',(-11.8179542567,-38.7742356128,1.03442695212));
#75425=CARTESIAN_POINT('Ctrl Pts',(-11.8267316409,-38.7742356128,0.979949794408));
#75426=CARTESIAN_POINT('Ctrl Pts',(-11.8354184104,-38.7742356128,0.924526608307));
#75427=CARTESIAN_POINT('Ctrl Pts',(-10.0162216343,-38.7742356128,-6.33635360057));
#75428=CARTESIAN_POINT('Ctrl Pts',(-10.3224768783,-38.7742356128,-5.97981782527));
#75429=CARTESIAN_POINT('Ctrl Pts',(-10.6115458029,-38.7742356128,-5.60497678219));
#75430=CARTESIAN_POINT('Ctrl Pts',(-10.876460919,-38.7742356128,-5.21255294902));
#75431=CARTESIAN_POINT('Ctrl Pts',(-11.5273586686,-38.7742356128,-4.07233951466));
#75432=CARTESIAN_POINT('Ctrl Pts',(-11.912489836,-38.7742356128,-2.80791655207));
#75433=CARTESIAN_POINT('Ctrl Pts',(-12.0219871572,-38.7742356128,-1.97477394764));
#75434=CARTESIAN_POINT('Ctrl Pts',(-12.0360485934,-38.7742356128,-0.887789304964));
#75435=CARTESIAN_POINT('Ctrl Pts',(-11.941568867,-38.7742356128,0.143912935026));
#75436=CARTESIAN_POINT('Ctrl Pts',(-11.9112061973,-38.7742356128,0.407077462691));
#75437=CARTESIAN_POINT('Ctrl Pts',(-11.8758398702,-38.7742356128,0.666630263604));
#75438=CARTESIAN_POINT('Ctrl Pts',(-11.8354184104,-38.7742356128,0.924526608307));
#75439=CARTESIAN_POINT('Origin',(-3.35265884719E-30,-38.2742356128,3.15283103411E-22));
#75440=CARTESIAN_POINT('',(-12.5997104365,-37.2742356128,-8.85478949011));
#75441=CARTESIAN_POINT('',(-12.5997104365,-38.2742356128,-8.85478949011));
#75442=CARTESIAN_POINT('Origin',(-3.35265884719E-30,-37.2742356128,3.15283103411E-22));
#75443=CARTESIAN_POINT('Origin',(-3.35265884719E-30,-36.1242356128,3.15283103411E-22));
#75444=CARTESIAN_POINT('',(-10.3256459325,-33.7742356128,-11.4254556179));
#75445=CARTESIAN_POINT('',(-10.3256459325,-36.1242356128,-11.4254556179));
#75446=CARTESIAN_POINT('',(-11.816958431,-33.7742356128,-9.87519586841));
#75447=CARTESIAN_POINT('Origin',(-3.35265884719E-30,-33.7742356128,3.15283103411E-22));
#75448=CARTESIAN_POINT('',(-11.816958431,-36.1242356128,-9.87519586841));
#75449=CARTESIAN_POINT('Origin',(-3.35265884719E-30,-38.2742356128,3.15283103411E-22));
#75450=CARTESIAN_POINT('',(-9.33467257157,-37.2742356128,-12.2484238978));
#75451=CARTESIAN_POINT('',(-9.33467257157,-38.2742356128,-12.2484238978));
#75452=CARTESIAN_POINT('',(-0.5,-37.2742356128,-15.3918809766));
#75453=CARTESIAN_POINT('',(-0.5,-38.2742356128,-15.3918809766));
#75454=CARTESIAN_POINT('Origin',(-3.35265884719E-30,-37.2742356128,3.15283103411E-22));
#75455=CARTESIAN_POINT('Origin',(-3.35265884719E-30,-38.2742356128,3.15283103411E-22));
#75456=CARTESIAN_POINT('',(9.33467257157,-38.7742356128,-12.2484238978));
#75457=CARTESIAN_POINT('',(9.33467257157,-37.2742356128,-12.2484238978));
#75458=CARTESIAN_POINT('',(9.33467257157,-38.2742356128,-12.2484238978));
#75459=CARTESIAN_POINT('',(0.5,-37.2742356128,-15.3918809766));
#75460=CARTESIAN_POINT('Origin',(-3.35265884719E-30,-37.2742356128,3.15283103411E-22));
#75461=CARTESIAN_POINT('',(0.5,-38.7742356128,-15.3918809766));
#75462=CARTESIAN_POINT('',(0.5,-38.2742356128,-15.3918809766));
#75463=CARTESIAN_POINT('Origin',(-3.35265884719E-30,-38.7742356128,3.15283103411E-22));
#75464=CARTESIAN_POINT('Origin',(-3.35265884719E-30,-36.1242356128,3.15283103411E-22));
#75465=CARTESIAN_POINT('',(10.3256459325,-38.7742356128,-11.4254556179));
#75466=CARTESIAN_POINT('',(11.816958431,-38.7742356128,-9.87519586841));
#75467=CARTESIAN_POINT('Origin',(-3.35265884719E-30,-38.7742356128,3.15283103411E-22));
#75468=CARTESIAN_POINT('',(11.816958431,-33.7742356128,-9.87519586841));
#75469=CARTESIAN_POINT('',(11.816958431,-36.1242356128,-9.87519586841));
#75470=CARTESIAN_POINT('',(10.3256459325,-33.7742356128,-11.4254556179));
#75471=CARTESIAN_POINT('Origin',(-3.35265884719E-30,-33.7742356128,3.15283103411E-22));
#75472=CARTESIAN_POINT('',(10.3256459325,-36.1242356128,-11.4254556179));
#75473=CARTESIAN_POINT('Origin',(-3.35265884719E-30,-38.2742356128,3.15283103411E-22));
#75474=CARTESIAN_POINT('',(12.5997104365,-38.7742356128,-8.85478949011));
#75475=CARTESIAN_POINT('',(12.5997104365,-37.2742356128,-8.85478949011));
#75476=CARTESIAN_POINT('',(12.5997104365,-38.2742356128,-8.85478949011));
#75477=CARTESIAN_POINT('Origin',(-3.35265884719E-30,-38.7742356128,3.15283103411E-22));
#75478=CARTESIAN_POINT('Origin',(-3.35265884719E-30,-37.2742356128,3.15283103411E-22));
#75479=CARTESIAN_POINT('Origin',(-3.5527136788E-15,-37.9242356128,-8.88178104417E-16));
#75480=CARTESIAN_POINT('Origin',(-3.5527136788E-15,-37.2742356128,-8.88178104417E-16));
#75481=CARTESIAN_POINT('Origin',(-3.35265884719E-30,-34.4742356128,3.15283103411E-22));
#75482=CARTESIAN_POINT('',(3.,-34.4742356128,0.));
#75483=CARTESIAN_POINT('Origin',(3.,-35.1742356128,16.6523581407));
#75484=CARTESIAN_POINT('Origin',(-3.35265884719E-30,-38.1842356129,3.15283103411E-22));
#75485=CARTESIAN_POINT('Origin',(-3.35265884719E-30,-33.4742356128,3.15283103411E-22));
#75486=CARTESIAN_POINT('Origin',(-3.35265884719E-30,-33.4742356128,3.15283103411E-22));
#75487=CARTESIAN_POINT('',(14.2514385284,-33.4742356128,0.));
#75488=CARTESIAN_POINT('Origin',(14.2514385284,-41.6742356128,2.4));
#75489=CARTESIAN_POINT('',(14.2514385284,-38.7742356128,0.));
#75490=CARTESIAN_POINT('Origin',(-3.35265884719E-30,-38.7742356128,3.15283103411E-22));
#75491=CARTESIAN_POINT('',(0.5,-38.7742356128,-11.0174674429));
#75492=CARTESIAN_POINT('',(0.5,-38.7742356128,0.));
#75493=CARTESIAN_POINT('',(1.48259713265,-38.7742356128,-10.9268000942));
#75494=CARTESIAN_POINT('Origin',(-8.24340595784179E-14,-38.7742356128,-0.229047725441214));
#75495=CARTESIAN_POINT('',(6.35435667676,-38.7742356128,-9.34315312398));
#75496=CARTESIAN_POINT('Ctrl Pts',(1.48259713264981,-38.7742356128,-10.9268000941986));
#75497=CARTESIAN_POINT('Ctrl Pts',(1.71328083841,-38.7742356128,-10.8948297336));
#75498=CARTESIAN_POINT('Ctrl Pts',(1.91354623838,-38.7742356128,-10.8659465412));
#75499=CARTESIAN_POINT('Ctrl Pts',(2.0855726443,-38.7742356128,-10.8395401686));
#75500=CARTESIAN_POINT('Ctrl Pts',(3.07854611663014,-38.7742356128,-10.6733698534529));
#75501=CARTESIAN_POINT('Ctrl Pts',(4.05813867422129,-38.7742356128,-10.4126758711658));
#75502=CARTESIAN_POINT('Ctrl Pts',(4.86043811084938,-38.7742356128,-10.1190200262464));
#75503=CARTESIAN_POINT('Ctrl Pts',(5.62475805694812,-38.7742356128,-9.76080244433078));
#75504=CARTESIAN_POINT('Ctrl Pts',(6.35435667676222,-38.7742356128,-9.34315312398388));
#75505=CARTESIAN_POINT('',(9.33467257157,-38.7742356128,-12.2484238978));
#75506=CARTESIAN_POINT('Origin',(-3.35265884719E-30,-38.7742356128,3.15283103411E-22));
#75507=CARTESIAN_POINT('',(11.7961681305,-38.7742356128,-9.46800252678));
#75508=CARTESIAN_POINT('',(9.33306511227,-38.7742356128,-7.06692107621));
#75509=CARTESIAN_POINT('',(11.7961681305,-38.7742356128,-9.46800252678));
#75510=CARTESIAN_POINT('Origin',(11.586757942,-38.7742356128,-9.68282192292));
#75511=CARTESIAN_POINT('',(9.91508679725,-38.7742356128,-11.4177012033));
#75512=CARTESIAN_POINT('Origin',(10.1244969857,-38.7742356128,-11.2028818071));
#75513=CARTESIAN_POINT('',(7.22695685732,-38.7742356128,-8.79725906681));
#75514=CARTESIAN_POINT('',(9.91508679725,-38.7742356128,-11.4177012033));
#75515=CARTESIAN_POINT('Ctrl Pts',(7.22695685732231,-38.7742356128,-8.7972590668134));
#75516=CARTESIAN_POINT('Ctrl Pts',(7.28150888554723,-38.7742356128,-8.76017689804407));
#75517=CARTESIAN_POINT('Ctrl Pts',(7.3358430836494,-38.7742356128,-8.72268025917252));
#75518=CARTESIAN_POINT('Ctrl Pts',(7.3899712392707,-38.7742356128,-8.68477139569698));
#75519=CARTESIAN_POINT('Ctrl Pts',(7.467201824484,-38.7742356128,-8.63068265616057));
#75520=CARTESIAN_POINT('Ctrl Pts',(7.54401747222365,-38.7742356128,-8.57575348443563));
#75521=CARTESIAN_POINT('Ctrl Pts',(7.62055514908962,-38.7742356128,-8.5199113454453));
#75522=CARTESIAN_POINT('Ctrl Pts',(7.69952766934177,-38.7742356128,-8.46229273676895));
#75523=CARTESIAN_POINT('Ctrl Pts',(7.77820421333981,-38.7742356128,-8.40370214573728));
#75524=CARTESIAN_POINT('Ctrl Pts',(7.85668116624427,-38.7742356128,-8.34407402226636));
#75525=CARTESIAN_POINT('Ctrl Pts',(7.93692573193363,-38.7742356128,-8.28310283653976));
#75526=CARTESIAN_POINT('Ctrl Pts',(8.01696145430617,-38.7742356128,-8.22104687847736));
#75527=CARTESIAN_POINT('Ctrl Pts',(8.09683736040211,-38.7742356128,-8.15785041906028));
#75528=CARTESIAN_POINT('Ctrl Pts',(8.1787375971322,-38.7742356128,-8.09305234364882));
#75529=CARTESIAN_POINT('Ctrl Pts',(8.2604696307762,-38.7742356128,-8.02705525395073));
#75530=CARTESIAN_POINT('Ctrl Pts',(8.34203275379579,-38.7742356128,-7.9598135965643));
#75531=CARTESIAN_POINT('Ctrl Pts',(8.42751622477602,-38.7742356128,-7.88933995535176));
#75532=CARTESIAN_POINT('Ctrl Pts',(8.5128140940912,-38.7742356128,-7.81749921791738));
#75533=CARTESIAN_POINT('Ctrl Pts',(8.59786908945085,-38.7742356128,-7.74425465003797));
#75534=CARTESIAN_POINT('Ctrl Pts',(8.68560880784544,-38.7742356128,-7.66869815000527));
#75535=CARTESIAN_POINT('Ctrl Pts',(8.77308976965874,-38.7742356128,-7.59164784533776));
#75536=CARTESIAN_POINT('Ctrl Pts',(8.86019351231535,-38.7742356128,-7.51307941783203));
#75537=CARTESIAN_POINT('Ctrl Pts',(8.9528644060946,-38.7742356128,-7.42948936558261));
#75538=CARTESIAN_POINT('Ctrl Pts',(9.04510813530846,-38.7742356128,-7.34418092104819));
#75539=CARTESIAN_POINT('Ctrl Pts',(9.1367235464675,-38.7742356128,-7.25714246143299));
#75540=CARTESIAN_POINT('Ctrl Pts',(9.2025262042184,-38.7742356128,-7.19462719356739));
#75541=CARTESIAN_POINT('Ctrl Pts',(9.2680034296596,-38.7742356128,-7.13121983085198));
#75542=CARTESIAN_POINT('Ctrl Pts',(9.3330651122663,-38.7742356128,-7.06692107620626));
#75543=CARTESIAN_POINT('Origin',(-3.35265884719E-30,-38.7742356128,3.15283103411E-22));
#75544=CARTESIAN_POINT('',(11.7961681305,-38.7742356128,9.46800252678));
#75545=CARTESIAN_POINT('Origin',(11.586757942,-38.7742356128,9.68282192292));
#75546=CARTESIAN_POINT('',(10.9208700025,-38.7742356128,8.61474463077));
#75547=CARTESIAN_POINT('',(10.9208700025,-38.7742356128,8.61474463077));
#75548=CARTESIAN_POINT('',(10.9154607948,-38.7742356128,8.19051504615));
#75549=CARTESIAN_POINT('Origin',(11.1302801909,-38.7742356128,8.39992523463));
#75550=CARTESIAN_POINT('',(11.1946743794,-38.7742356128,7.90408918462));
#75551=CARTESIAN_POINT('',(11.1946743794,-38.7742356128,7.90408918462));
#75552=CARTESIAN_POINT('',(11.6189039641,-38.7742356128,7.89867997696));
#75553=CARTESIAN_POINT('Origin',(11.4094937756,-38.7742356128,8.1134993731));
#75554=CARTESIAN_POINT('',(11.6189039641,-38.7742356128,7.89867997696));
#75555=CARTESIAN_POINT('',(10.0162216343,-38.7742356128,-6.33635360057));
#75556=CARTESIAN_POINT('',(12.5997104365,-38.7742356128,-8.85478949011));
#75557=CARTESIAN_POINT('',(11.8354184104,-38.7742356128,0.924526608307));
#75558=CARTESIAN_POINT('Ctrl Pts',(10.0162216343,-38.7742356128,-6.33635360057));
#75559=CARTESIAN_POINT('Ctrl Pts',(10.3224768783,-38.7742356128,-5.97981782527));
#75560=CARTESIAN_POINT('Ctrl Pts',(10.6115458029,-38.7742356128,-5.60497678219));
#75561=CARTESIAN_POINT('Ctrl Pts',(10.876460919,-38.7742356128,-5.21255294902));
#75562=CARTESIAN_POINT('Ctrl Pts',(11.5273586686,-38.7742356128,-4.07233951466));
#75563=CARTESIAN_POINT('Ctrl Pts',(11.912489836,-38.7742356128,-2.80791655207));
#75564=CARTESIAN_POINT('Ctrl Pts',(12.0219871572,-38.7742356128,-1.97477394764));
#75565=CARTESIAN_POINT('Ctrl Pts',(12.0360485934,-38.7742356128,-0.887789304964));
#75566=CARTESIAN_POINT('Ctrl Pts',(11.941568867,-38.7742356128,0.143912935026));
#75567=CARTESIAN_POINT('Ctrl Pts',(11.9112061973,-38.7742356128,0.407077462691));
#75568=CARTESIAN_POINT('Ctrl Pts',(11.8758398702,-38.7742356128,0.666630263604));
#75569=CARTESIAN_POINT('Ctrl Pts',(11.8354184104,-38.7742356128,0.924526608307));
#75570=CARTESIAN_POINT('',(11.0086556946,-38.7742356128,3.43000353527));
#75571=CARTESIAN_POINT('Ctrl Pts',(11.0086556946,-38.7742356128,3.43000353527));
#75572=CARTESIAN_POINT('Ctrl Pts',(11.0817932058,-38.7742356128,3.31017227332));
#75573=CARTESIAN_POINT('Ctrl Pts',(11.1567853729,-38.7742356128,3.18040212706));
#75574=CARTESIAN_POINT('Ctrl Pts',(11.2288017566,-38.7742356128,3.0447194315));
#75575=CARTESIAN_POINT('Ctrl Pts',(11.4529799792,-38.7742356128,2.57934328034));
#75576=CARTESIAN_POINT('Ctrl Pts',(11.6140362762,-38.7742356128,2.09446235244));
#75577=CARTESIAN_POINT('Ctrl Pts',(11.6871718767,-38.7742356128,1.76491172368));
#75578=CARTESIAN_POINT('Ctrl Pts',(11.7534189237,-38.7742356128,1.41966067629));
#75579=CARTESIAN_POINT('Ctrl Pts',(11.809039671,-38.7742356128,1.08859783468));
#75580=CARTESIAN_POINT('Ctrl Pts',(11.8179542567,-38.7742356128,1.03442695212));
#75581=CARTESIAN_POINT('Ctrl Pts',(11.8267316409,-38.7742356128,0.979949794408));
#75582=CARTESIAN_POINT('Ctrl Pts',(11.8354184104,-38.7742356128,0.924526608307));
#75583=CARTESIAN_POINT('',(7.16875088157,-38.7742356128,5.23983755655));
#75584=CARTESIAN_POINT('Ctrl Pts',(11.0086556946,-38.7742356128,3.43000353527));
#75585=CARTESIAN_POINT('Ctrl Pts',(10.8267791086,-38.7742356128,3.7279970062));
#75586=CARTESIAN_POINT('Ctrl Pts',(10.6180941124,-38.7742356128,4.02812460647));
#75587=CARTESIAN_POINT('Ctrl Pts',(10.3610804417,-38.7742356128,4.34854162483));
#75588=CARTESIAN_POINT('Ctrl Pts',(9.81894561437,-38.7742356128,4.82846996464));
#75589=CARTESIAN_POINT('Ctrl Pts',(9.1449448519,-38.7742356128,5.15260465424));
#75590=CARTESIAN_POINT('Ctrl Pts',(8.86735473037,-38.7742356128,5.24791616482));
#75591=CARTESIAN_POINT('Ctrl Pts',(8.35592834321,-38.7742356128,5.35778460397));
#75592=CARTESIAN_POINT('Ctrl Pts',(7.83459380784,-38.7742356128,5.3594412401));
#75593=CARTESIAN_POINT('Ctrl Pts',(7.6075384225,-38.7742356128,5.33903210576));
#75594=CARTESIAN_POINT('Ctrl Pts',(7.38481168145,-38.7742356128,5.2985941411));
#75595=CARTESIAN_POINT('Ctrl Pts',(7.16875088157,-38.7742356128,5.23983755655));
#75596=CARTESIAN_POINT('',(7.04251644773,-38.7742356128,5.33751720019));
#75597=CARTESIAN_POINT('Origin',(7.14250943682,-38.7742356128,5.33633308276));
#75598=CARTESIAN_POINT('',(0.5,-38.7742356128,12.4465469186));
#75599=CARTESIAN_POINT('Origin',(-0.00041610715012616,-38.7742356128,5.42091963994));
#75600=CARTESIAN_POINT('',(0.5,-38.7742356128,0.));
#75601=CARTESIAN_POINT('',(8.33174409695,-38.7742356128,11.2707494202));
#75602=CARTESIAN_POINT('',(8.33174409695,-38.7742356128,11.2707494202));
#75603=CARTESIAN_POINT('',(8.32633488929,-38.7742356128,10.8465198356));
#75604=CARTESIAN_POINT('Origin',(8.54115428543,-38.7742356128,11.0559300241));
#75605=CARTESIAN_POINT('',(8.60554847393,-38.7742356128,10.560093974));
#75606=CARTESIAN_POINT('',(8.60554847393,-38.7742356128,10.560093974));
#75607=CARTESIAN_POINT('',(9.02977805856,-38.7742356128,10.5546847664));
#75608=CARTESIAN_POINT('Origin',(8.82036787008,-38.7742356128,10.7695041625));
#75609=CARTESIAN_POINT('',(9.91508679725,-38.7742356128,11.4177012033));
#75610=CARTESIAN_POINT('',(9.02977805856,-38.7742356128,10.5546847664));
#75611=CARTESIAN_POINT('Origin',(10.1244969857,-38.7742356128,11.2028818071));
#75612=CARTESIAN_POINT('Origin',(-3.35265884719E-30,-44.4742356128,3.15283103411E-22));
#75613=CARTESIAN_POINT('',(-8.73272894647,-44.4742356128,11.6412701168));
#75614=CARTESIAN_POINT('Origin',(-7.48272894647,-44.4742356128,11.6412701168));
#75615=CARTESIAN_POINT('Origin',(4.74384247076,-41.1742356128,3.12351150632));
#75616=CARTESIAN_POINT('',(5.24384247076,-41.6742356128,3.12351150632));
#75617=CARTESIAN_POINT('',(5.24384247076,-41.1742356128,3.12351150632));
#75618=CARTESIAN_POINT('',(4.89234685393,-41.6742356128,2.64607413014));
#75619=CARTESIAN_POINT('Origin',(4.74384247076,-41.6742356128,3.12351150632));
#75620=CARTESIAN_POINT('',(4.89234685393,-41.1742356128,2.64607413014));
#75621=CARTESIAN_POINT('Origin',(6.82290383517,-40.1142356128,-3.56061176027));
#75622=CARTESIAN_POINT('',(0.48735027394,-41.6742356128,-2.10776590718));
#75623=CARTESIAN_POINT('Origin',(6.82290383517,-41.6742356128,-3.56061176027));
#75624=CARTESIAN_POINT('',(0.48735027394,-40.1142356128,-2.10776590718));
#75625=CARTESIAN_POINT('Origin',(-4.99600361081E-16,-41.1742356128,-1.99600853387));
#75626=CARTESIAN_POINT('',(-0.48735027394,-41.6742356128,-2.10776590718));
#75627=CARTESIAN_POINT('Origin',(-4.99600361081E-16,-41.6742356128,-1.99600853387));
#75628=CARTESIAN_POINT('',(-0.48735027394,-41.1742356128,-2.10776590718));
#75629=CARTESIAN_POINT('Origin',(-6.82290383517,-40.1142356128,-3.56061176027));
#75630=CARTESIAN_POINT('',(-4.89234685393,-41.6742356128,2.64607413014));
#75631=CARTESIAN_POINT('',(-4.89234685393,-40.1142356128,2.64607413014));
#75632=CARTESIAN_POINT('Origin',(-6.82290383517,-41.6742356128,-3.56061176027));
#75633=CARTESIAN_POINT('Origin',(-4.74384247076,-41.1742356128,3.12351150632));
#75634=CARTESIAN_POINT('',(-5.24384247076,-41.6742356128,3.12351150632));
#75635=CARTESIAN_POINT('Origin',(-4.74384247076,-41.6742356128,3.12351150632));
#75636=CARTESIAN_POINT('',(-5.24384247076,-41.1742356128,3.12351150632));
#75637=CARTESIAN_POINT('Origin',(-5.24384247076,-41.6742356128,6.92091963994));
#75638=CARTESIAN_POINT('',(-5.24384247076,-41.6742356128,6.92091963994));
#75639=CARTESIAN_POINT('',(-5.24384247076,-41.6742356128,5.02221557313));
#75640=CARTESIAN_POINT('',(-5.24384247076,-41.1742356128,6.92091963994));
#75641=CARTESIAN_POINT('Origin',(-0.000416107150126,-40.1142356128,6.92091963994));
#75642=CARTESIAN_POINT('',(-0.000416107143134986,-41.6742356128,12.1643459815524));
#75643=CARTESIAN_POINT('Origin',(-0.000416107150126,-41.6742356128,6.92091963994));
#75644=CARTESIAN_POINT('',(-0.000416107150124,-40.1142356128,12.1643460036));
#75645=CARTESIAN_POINT('Origin',(0.000416107150126,-40.1142356128,6.92091963994));
#75646=CARTESIAN_POINT('',(5.24384247076,-41.6742356128,6.92091963994));
#75647=CARTESIAN_POINT('Origin',(0.000416107150126,-41.6742356128,6.92091963994));
#75648=CARTESIAN_POINT('',(5.24384247076,-40.1142356128,6.92091963994));
#75649=CARTESIAN_POINT('Origin',(5.24384247076,-41.6742356128,6.92091963994));
#75650=CARTESIAN_POINT('',(5.24384247076,-41.6742356128,5.02221557313));
#75651=CARTESIAN_POINT('Origin',(6.82290383517,-40.1142356128,-3.56061176027));
#75652=CARTESIAN_POINT('',(12.3229038352,-41.6742356128,-3.56061176027));
#75653=CARTESIAN_POINT('',(12.32290383517,-40.1142356128,-3.56061176027));
#75654=CARTESIAN_POINT('Origin',(6.82290383517,-41.6742356128,-3.56061176027));
#75655=CARTESIAN_POINT('Origin',(-6.82290383517,-40.1142356128,-3.56061176027));
#75656=CARTESIAN_POINT('',(-12.3229038352,-41.6742356128,-3.56061176027));
#75657=CARTESIAN_POINT('Origin',(-6.82290383517,-41.6742356128,-3.56061176027));
#75658=CARTESIAN_POINT('',(-12.32290383517,-40.1142356128,-3.56061176027));
#75659=CARTESIAN_POINT('Origin',(-3.35265884719E-30,-44.4742356128,3.15283103411E-22));
#75660=CARTESIAN_POINT('',(8.73272894647,-44.4742356128,11.6412701168));
#75661=CARTESIAN_POINT('Origin',(7.48272894647,-44.4742356128,11.6412701168));
#75662=CARTESIAN_POINT('Origin',(0.000416107150126,-37.6642356128,5.42091963994));
#75663=CARTESIAN_POINT('',(-0.5,-37.2742356128,12.4465469186));
#75664=CARTESIAN_POINT('',(-7.04251644773,-37.2742356128,5.33751720019));
#75665=CARTESIAN_POINT('Origin',(0.000416107150126,-37.2742356128,5.42091963994));
#75666=CARTESIAN_POINT('',(-7.04251644773,-37.6642356128,5.33751720019));
#75667=CARTESIAN_POINT('',(-0.5,-37.6642356128,12.4465469186));
#75668=CARTESIAN_POINT('Origin',(-7.14250943682,-38.2742356128,5.33633308276));
#75669=CARTESIAN_POINT('',(-7.16875088104636,-37.2742356128,5.23983755640952));
#75670=CARTESIAN_POINT('Origin',(-7.14250943682,-37.2742356128,5.33633308276));
#75671=CARTESIAN_POINT('',(-7.16875088157,-38.2742356128,5.23983755655));
#75672=CARTESIAN_POINT('Ctrl Pts',(-11.0086556946,-38.7742356128,3.43000353527));
#75673=CARTESIAN_POINT('Ctrl Pts',(-11.0086556946,-36.9742356128,3.43000353527));
#75674=CARTESIAN_POINT('Ctrl Pts',(-10.8267791086,-38.7742356128,3.7279970062));
#75675=CARTESIAN_POINT('Ctrl Pts',(-10.8267791086,-36.9742356128,3.7279970062));
#75676=CARTESIAN_POINT('Ctrl Pts',(-10.6180941124,-38.7742356128,4.02812460647));
#75677=CARTESIAN_POINT('Ctrl Pts',(-10.6180941124,-36.9742356128,4.02812460647));
#75678=CARTESIAN_POINT('Ctrl Pts',(-10.3610804417,-38.7742356128,4.34854162483));
#75679=CARTESIAN_POINT('Ctrl Pts',(-10.3610804417,-36.9742356128,4.34854162483));
#75680=CARTESIAN_POINT('Ctrl Pts',(-9.81894561437,-38.7742356128,4.82846996464));
#75681=CARTESIAN_POINT('Ctrl Pts',(-9.81894561437,-36.9742356128,4.82846996464));
#75682=CARTESIAN_POINT('Ctrl Pts',(-9.1449448519,-38.7742356128,5.15260465424));
#75683=CARTESIAN_POINT('Ctrl Pts',(-9.1449448519,-36.9742356128,5.15260465424));
#75684=CARTESIAN_POINT('Ctrl Pts',(-8.86735473037,-38.7742356128,5.24791616482));
#75685=CARTESIAN_POINT('Ctrl Pts',(-8.86735473037,-36.9742356128,5.24791616482));
#75686=CARTESIAN_POINT('Ctrl Pts',(-8.35592834321,-38.7742356128,5.35778460397));
#75687=CARTESIAN_POINT('Ctrl Pts',(-8.35592834321,-36.9742356128,5.35778460397));
#75688=CARTESIAN_POINT('Ctrl Pts',(-7.83459380784,-38.7742356128,5.3594412401));
#75689=CARTESIAN_POINT('Ctrl Pts',(-7.83459380784,-36.9742356128,5.3594412401));
#75690=CARTESIAN_POINT('Ctrl Pts',(-7.6075384225,-38.7742356128,5.33903210576));
#75691=CARTESIAN_POINT('Ctrl Pts',(-7.6075384225,-36.9742356128,5.33903210576));
#75692=CARTESIAN_POINT('Ctrl Pts',(-7.38481168145,-38.7742356128,5.2985941411));
#75693=CARTESIAN_POINT('Ctrl Pts',(-7.38481168145,-36.9742356128,5.2985941411));
#75694=CARTESIAN_POINT('Ctrl Pts',(-7.16875088157,-38.7742356128,5.23983755655));
#75695=CARTESIAN_POINT('Ctrl Pts',(-7.16875088157,-36.9742356128,5.23983755655));
#75696=CARTESIAN_POINT('',(-11.0086556946,-37.2742356128,3.43000353527));
#75697=CARTESIAN_POINT('',(-11.0086556946,-37.6642356128,3.43000353527));
#75698=CARTESIAN_POINT('Ctrl Pts',(-11.0086556946,-37.2742356128,3.43000353527));
#75699=CARTESIAN_POINT('Ctrl Pts',(-10.8267791086,-37.2742356128,3.7279970062));
#75700=CARTESIAN_POINT('Ctrl Pts',(-10.6180941124,-37.2742356128,4.02812460647));
#75701=CARTESIAN_POINT('Ctrl Pts',(-10.3610804417,-37.2742356128,4.34854162483));
#75702=CARTESIAN_POINT('Ctrl Pts',(-9.81894561437,-37.2742356128,4.82846996464));
#75703=CARTESIAN_POINT('Ctrl Pts',(-9.1449448519,-37.2742356128,5.15260465424));
#75704=CARTESIAN_POINT('Ctrl Pts',(-8.86735473037,-37.2742356128,5.24791616482));
#75705=CARTESIAN_POINT('Ctrl Pts',(-8.35592834321,-37.2742356128,5.35778460397));
#75706=CARTESIAN_POINT('Ctrl Pts',(-7.83459380784,-37.2742356128,5.3594412401));
#75707=CARTESIAN_POINT('Ctrl Pts',(-7.6075384225,-37.2742356128,5.33903210576));
#75708=CARTESIAN_POINT('Ctrl Pts',(-7.38481168145,-37.2742356128,5.2985941411));
#75709=CARTESIAN_POINT('Ctrl Pts',(-7.16875088157,-37.2742356128,5.23983755655));
#75710=CARTESIAN_POINT('Ctrl Pts',(-11.0086556946,-38.7742356128,3.43000353527));
#75711=CARTESIAN_POINT('Ctrl Pts',(-11.0086556946,-36.9742356128,3.43000353527));
#75712=CARTESIAN_POINT('Ctrl Pts',(-11.0817932058,-38.7742356128,3.31017227332));
#75713=CARTESIAN_POINT('Ctrl Pts',(-11.0817932058,-36.9742356128,3.31017227332));
#75714=CARTESIAN_POINT('Ctrl Pts',(-11.1567853729,-38.7742356128,3.18040212706));
#75715=CARTESIAN_POINT('Ctrl Pts',(-11.1567853729,-36.9742356128,3.18040212706));
#75716=CARTESIAN_POINT('Ctrl Pts',(-11.2288017566,-38.7742356128,3.0447194315));
#75717=CARTESIAN_POINT('Ctrl Pts',(-11.2288017566,-36.9742356128,3.0447194315));
#75718=CARTESIAN_POINT('Ctrl Pts',(-11.4529799792,-38.7742356128,2.57934328034));
#75719=CARTESIAN_POINT('Ctrl Pts',(-11.4529799792,-36.9742356128,2.57934328034));
#75720=CARTESIAN_POINT('Ctrl Pts',(-11.6140362762,-38.7742356128,2.09446235244));
#75721=CARTESIAN_POINT('Ctrl Pts',(-11.6140362762,-36.9742356128,2.09446235244));
#75722=CARTESIAN_POINT('Ctrl Pts',(-11.6871718767,-38.7742356128,1.76491172368));
#75723=CARTESIAN_POINT('Ctrl Pts',(-11.6871718767,-36.9742356128,1.76491172368));
#75724=CARTESIAN_POINT('Ctrl Pts',(-11.7534189237,-38.7742356128,1.41966067629));
#75725=CARTESIAN_POINT('Ctrl Pts',(-11.7534189237,-36.9742356128,1.41966067629));
#75726=CARTESIAN_POINT('Ctrl Pts',(-11.809039671,-38.7742356128,1.08859783468));
#75727=CARTESIAN_POINT('Ctrl Pts',(-11.809039671,-36.9742356128,1.08859783468));
#75728=CARTESIAN_POINT('Ctrl Pts',(-11.8179542567,-38.7742356128,1.03442695212));
#75729=CARTESIAN_POINT('Ctrl Pts',(-11.8179542567,-36.9742356128,1.03442695212));
#75730=CARTESIAN_POINT('Ctrl Pts',(-11.8267316409,-38.7742356128,0.979949794408));
#75731=CARTESIAN_POINT('Ctrl Pts',(-11.8267316409,-36.9742356128,0.979949794408));
#75732=CARTESIAN_POINT('Ctrl Pts',(-11.8354184104,-38.7742356128,0.924526608307));
#75733=CARTESIAN_POINT('Ctrl Pts',(-11.8354184104,-36.9742356128,0.924526608307));
#75734=CARTESIAN_POINT('',(-11.8354184104,-37.2742356128,0.924526608307));
#75735=CARTESIAN_POINT('Ctrl Pts',(-11.0086556946,-37.2742356128,3.43000353527));
#75736=CARTESIAN_POINT('Ctrl Pts',(-11.0817932058,-37.2742356128,3.31017227332));
#75737=CARTESIAN_POINT('Ctrl Pts',(-11.1567853729,-37.2742356128,3.18040212706));
#75738=CARTESIAN_POINT('Ctrl Pts',(-11.2288017566,-37.2742356128,3.0447194315));
#75739=CARTESIAN_POINT('Ctrl Pts',(-11.4529799792,-37.2742356128,2.57934328034));
#75740=CARTESIAN_POINT('Ctrl Pts',(-11.6140362762,-37.2742356128,2.09446235244));
#75741=CARTESIAN_POINT('Ctrl Pts',(-11.6871718767,-37.2742356128,1.76491172368));
#75742=CARTESIAN_POINT('Ctrl Pts',(-11.7534189237,-37.2742356128,1.41966067629));
#75743=CARTESIAN_POINT('Ctrl Pts',(-11.809039671,-37.2742356128,1.08859783468));
#75744=CARTESIAN_POINT('Ctrl Pts',(-11.8179542567,-37.2742356128,1.03442695212));
#75745=CARTESIAN_POINT('Ctrl Pts',(-11.8267316409,-37.2742356128,0.979949794408));
#75746=CARTESIAN_POINT('Ctrl Pts',(-11.8354184104,-37.2742356128,0.924526608307));
#75747=CARTESIAN_POINT('',(-11.8354184104,-37.6642356128,0.924526608307));
#75748=CARTESIAN_POINT('Ctrl Pts',(-10.0162216343,-38.7742356128,-6.33635360057));
#75749=CARTESIAN_POINT('Ctrl Pts',(-10.0162216343,-36.9742356128,-6.33635360057));
#75750=CARTESIAN_POINT('Ctrl Pts',(-10.3224768783,-38.7742356128,-5.97981782527));
#75751=CARTESIAN_POINT('Ctrl Pts',(-10.3224768783,-36.9742356128,-5.97981782527));
#75752=CARTESIAN_POINT('Ctrl Pts',(-10.6115458029,-38.7742356128,-5.60497678219));
#75753=CARTESIAN_POINT('Ctrl Pts',(-10.6115458029,-36.9742356128,-5.60497678219));
#75754=CARTESIAN_POINT('Ctrl Pts',(-10.876460919,-38.7742356128,-5.21255294902));
#75755=CARTESIAN_POINT('Ctrl Pts',(-10.876460919,-36.9742356128,-5.21255294902));
#75756=CARTESIAN_POINT('Ctrl Pts',(-11.5273586686,-38.7742356128,-4.07233951466));
#75757=CARTESIAN_POINT('Ctrl Pts',(-11.5273586686,-36.9742356128,-4.07233951466));
#75758=CARTESIAN_POINT('Ctrl Pts',(-11.912489836,-38.7742356128,-2.80791655207));
#75759=CARTESIAN_POINT('Ctrl Pts',(-11.912489836,-36.9742356128,-2.80791655207));
#75760=CARTESIAN_POINT('Ctrl Pts',(-12.0219871572,-38.7742356128,-1.97477394764));
#75761=CARTESIAN_POINT('Ctrl Pts',(-12.0219871572,-36.9742356128,-1.97477394764));
#75762=CARTESIAN_POINT('Ctrl Pts',(-12.0360485934,-38.7742356128,-0.887789304964));
#75763=CARTESIAN_POINT('Ctrl Pts',(-12.0360485934,-36.9742356128,-0.887789304964));
#75764=CARTESIAN_POINT('Ctrl Pts',(-11.941568867,-38.7742356128,0.143912935026));
#75765=CARTESIAN_POINT('Ctrl Pts',(-11.941568867,-36.9742356128,0.143912935026));
#75766=CARTESIAN_POINT('Ctrl Pts',(-11.9112061973,-38.7742356128,0.407077462691));
#75767=CARTESIAN_POINT('Ctrl Pts',(-11.9112061973,-36.9742356128,0.407077462691));
#75768=CARTESIAN_POINT('Ctrl Pts',(-11.8758398702,-38.7742356128,0.666630263604));
#75769=CARTESIAN_POINT('Ctrl Pts',(-11.8758398702,-36.9742356128,0.666630263604));
#75770=CARTESIAN_POINT('Ctrl Pts',(-11.8354184104,-38.7742356128,0.924526608307));
#75771=CARTESIAN_POINT('Ctrl Pts',(-11.8354184104,-36.9742356128,0.924526608307));
#75772=CARTESIAN_POINT('',(-10.0162216343,-37.2742356128,-6.33635360057));
#75773=CARTESIAN_POINT('Ctrl Pts',(-10.0162216343,-37.2742356128,-6.33635360057));
#75774=CARTESIAN_POINT('Ctrl Pts',(-10.3224768783,-37.2742356128,-5.97981782527));
#75775=CARTESIAN_POINT('Ctrl Pts',(-10.6115458029,-37.2742356128,-5.60497678219));
#75776=CARTESIAN_POINT('Ctrl Pts',(-10.876460919,-37.2742356128,-5.21255294902));
#75777=CARTESIAN_POINT('Ctrl Pts',(-11.5273586686,-37.2742356128,-4.07233951466));
#75778=CARTESIAN_POINT('Ctrl Pts',(-11.912489836,-37.2742356128,-2.80791655207));
#75779=CARTESIAN_POINT('Ctrl Pts',(-12.0219871572,-37.2742356128,-1.97477394764));
#75780=CARTESIAN_POINT('Ctrl Pts',(-12.0360485934,-37.2742356128,-0.887789304964));
#75781=CARTESIAN_POINT('Ctrl Pts',(-11.941568867,-37.2742356128,0.143912935026));
#75782=CARTESIAN_POINT('Ctrl Pts',(-11.9112061973,-37.2742356128,0.407077462691));
#75783=CARTESIAN_POINT('Ctrl Pts',(-11.8758398702,-37.2742356128,0.666630263604));
#75784=CARTESIAN_POINT('Ctrl Pts',(-11.8354184104,-37.2742356128,0.924526608307));
#75785=CARTESIAN_POINT('',(-10.0162216343,-37.6642356128,-6.33635360057));
#75786=CARTESIAN_POINT('Ctrl Pts',(-7.22695646354,-38.7742356128,-8.79725933449));
#75787=CARTESIAN_POINT('Ctrl Pts',(-7.22695646354,-36.9742356128,-8.79725933449));
#75788=CARTESIAN_POINT('Ctrl Pts',(-7.25968775986,-38.7742356128,-8.77500998089));
#75789=CARTESIAN_POINT('Ctrl Pts',(-7.25968775986,-36.9742356128,-8.77500998089));
#75790=CARTESIAN_POINT('Ctrl Pts',(-7.29235374605,-38.7742356128,-8.75263626704));
#75791=CARTESIAN_POINT('Ctrl Pts',(-7.29235374605,-36.9742356128,-8.75263626704));
#75792=CARTESIAN_POINT('Ctrl Pts',(-7.3249555226,-38.7742356128,-8.73013845435));
#75793=CARTESIAN_POINT('Ctrl Pts',(-7.3249555226,-36.9742356128,-8.73013845435));
#75794=CARTESIAN_POINT('Ctrl Pts',(-7.75723078658,-38.7742356128,-8.42961072436));
#75795=CARTESIAN_POINT('Ctrl Pts',(-7.75723078658,-36.9742356128,-8.42961072436));
#75796=CARTESIAN_POINT('Ctrl Pts',(-8.17860364499,-38.7742356128,-8.10725352709));
#75797=CARTESIAN_POINT('Ctrl Pts',(-8.17860364499,-36.9742356128,-8.10725352709));
#75798=CARTESIAN_POINT('Ctrl Pts',(-8.5693207085,-38.7742356128,-7.78543946907));
#75799=CARTESIAN_POINT('Ctrl Pts',(-8.5693207085,-36.9742356128,-7.78543946907));
#75800=CARTESIAN_POINT('Ctrl Pts',(-8.95699215017,-38.7742356128,-7.43858429643));
#75801=CARTESIAN_POINT('Ctrl Pts',(-8.95699215017,-36.9742356128,-7.43858429643));
#75802=CARTESIAN_POINT('Ctrl Pts',(-9.33306737369,-38.7742356128,-7.0669188413));
#75803=CARTESIAN_POINT('Ctrl Pts',(-9.33306737369,-36.9742356128,-7.0669188413));
#75804=CARTESIAN_POINT('',(-9.33306511227,-37.2742356128,-7.06692107621));
#75805=CARTESIAN_POINT('',(-9.33306511227,-37.6642356128,-7.06692107621));
#75806=CARTESIAN_POINT('',(-7.22695685732,-37.2742356128,-8.79725906681));
#75807=CARTESIAN_POINT('Ctrl Pts',(-7.22695685732231,-37.2742356128,-8.7972590668134));
#75808=CARTESIAN_POINT('Ctrl Pts',(-7.28150888554724,-37.2742356128,-8.76017689804407));
#75809=CARTESIAN_POINT('Ctrl Pts',(-7.3358430836494,-37.2742356128,-8.72268025917252));
#75810=CARTESIAN_POINT('Ctrl Pts',(-7.3899712392707,-37.2742356128,-8.68477139569698));
#75811=CARTESIAN_POINT('Ctrl Pts',(-7.46720182448402,-37.2742356128,-8.63068265616056));
#75812=CARTESIAN_POINT('Ctrl Pts',(-7.54401747222369,-37.2742356128,-8.5757534844356));
#75813=CARTESIAN_POINT('Ctrl Pts',(-7.62055514908967,-37.2742356128,-8.51991134544526));
#75814=CARTESIAN_POINT('Ctrl Pts',(-7.69952766934181,-37.2742356128,-8.46229273676892));
#75815=CARTESIAN_POINT('Ctrl Pts',(-7.77820421333984,-37.2742356128,-8.40370214573726));
#75816=CARTESIAN_POINT('Ctrl Pts',(-7.85668116624429,-37.2742356128,-8.34407402226635));
#75817=CARTESIAN_POINT('Ctrl Pts',(-7.93692573193362,-37.2742356128,-8.28310283653977));
#75818=CARTESIAN_POINT('Ctrl Pts',(-8.01696145430614,-37.2742356128,-8.22104687847739));
#75819=CARTESIAN_POINT('Ctrl Pts',(-8.09683736040206,-37.2742356128,-8.15785041906032));
#75820=CARTESIAN_POINT('Ctrl Pts',(-8.17873759713219,-37.2742356128,-8.09305234364882));
#75821=CARTESIAN_POINT('Ctrl Pts',(-8.26046963077625,-37.2742356128,-8.0270552539507));
#75822=CARTESIAN_POINT('Ctrl Pts',(-8.34203275379588,-37.2742356128,-7.95981359656422));
#75823=CARTESIAN_POINT('Ctrl Pts',(-8.42751622477611,-37.2742356128,-7.88933995535169));
#75824=CARTESIAN_POINT('Ctrl Pts',(-8.51281409409128,-37.2742356128,-7.81749921791731));
#75825=CARTESIAN_POINT('Ctrl Pts',(-8.59786908945093,-37.2742356128,-7.7442546500379));
#75826=CARTESIAN_POINT('Ctrl Pts',(-8.68560880784551,-37.2742356128,-7.66869815000521));
#75827=CARTESIAN_POINT('Ctrl Pts',(-8.77308976965879,-37.2742356128,-7.59164784533771));
#75828=CARTESIAN_POINT('Ctrl Pts',(-8.86019351231539,-37.2742356128,-7.513079417832));
#75829=CARTESIAN_POINT('Ctrl Pts',(-8.95286440609459,-37.2742356128,-7.42948936558262));
#75830=CARTESIAN_POINT('Ctrl Pts',(-9.04510813530841,-37.2742356128,-7.34418092104824));
#75831=CARTESIAN_POINT('Ctrl Pts',(-9.13672354646741,-37.2742356128,-7.25714246143308));
#75832=CARTESIAN_POINT('Ctrl Pts',(-9.20252620421834,-37.2742356128,-7.19462719356745));
#75833=CARTESIAN_POINT('Ctrl Pts',(-9.26800342965957,-37.2742356128,-7.13121983085201));
#75834=CARTESIAN_POINT('Ctrl Pts',(-9.3330651122663,-37.2742356128,-7.06692107620626));
#75835=CARTESIAN_POINT('',(-7.22695685732,-37.6642356128,-8.79725906681));
#75836=CARTESIAN_POINT('Ctrl Pts',(-1.48259713264,-38.7742356128,-10.9268000942));
#75837=CARTESIAN_POINT('Ctrl Pts',(-1.48259713264,-36.9742356128,-10.9268000942));
#75838=CARTESIAN_POINT('Ctrl Pts',(-1.71328083841,-38.7742356128,-10.8948297336));
#75839=CARTESIAN_POINT('Ctrl Pts',(-1.71328083841,-36.9742356128,-10.8948297336));
#75840=CARTESIAN_POINT('Ctrl Pts',(-1.91354623838,-38.7742356128,-10.8659465412));
#75841=CARTESIAN_POINT('Ctrl Pts',(-1.91354623838,-36.9742356128,-10.8659465412));
#75842=CARTESIAN_POINT('Ctrl Pts',(-2.0855726443,-38.7742356128,-10.8395401686));
#75843=CARTESIAN_POINT('Ctrl Pts',(-2.0855726443,-36.9742356128,-10.8395401686));
#75844=CARTESIAN_POINT('Ctrl Pts',(-3.07854615175,-38.7742356128,-10.6733698476));
#75845=CARTESIAN_POINT('Ctrl Pts',(-3.07854615175,-36.9742356128,-10.6733698476));
#75846=CARTESIAN_POINT('Ctrl Pts',(-4.05813874351,-38.7742356128,-10.4126758527));
#75847=CARTESIAN_POINT('Ctrl Pts',(-4.05813874351,-36.9742356128,-10.4126758527));
#75848=CARTESIAN_POINT('Ctrl Pts',(-4.8604382114,-38.7742356128,-10.1190199895));
#75849=CARTESIAN_POINT('Ctrl Pts',(-4.8604382114,-36.9742356128,-10.1190199895));
#75850=CARTESIAN_POINT('Ctrl Pts',(-5.62475818467,-38.7742356128,-9.76080238448));
#75851=CARTESIAN_POINT('Ctrl Pts',(-5.62475818467,-36.9742356128,-9.76080238448));
#75852=CARTESIAN_POINT('Ctrl Pts',(-6.35435682916,-38.7742356128,-9.34315303675));
#75853=CARTESIAN_POINT('Ctrl Pts',(-6.35435682916,-36.9742356128,-9.34315303675));
#75854=CARTESIAN_POINT('',(-1.48259713217599,-37.2742356128,-10.9268000942492));
#75855=CARTESIAN_POINT('',(-6.35435667676,-37.2742356128,-9.34315312398));
#75856=CARTESIAN_POINT('Ctrl Pts',(-1.48259713264,-37.2742356128,-10.9268000942));
#75857=CARTESIAN_POINT('Ctrl Pts',(-1.71328083841,-37.2742356128,-10.8948297336));
#75858=CARTESIAN_POINT('Ctrl Pts',(-1.91354623838,-37.2742356128,-10.8659465412));
#75859=CARTESIAN_POINT('Ctrl Pts',(-2.0855726443,-37.2742356128,-10.8395401686));
#75860=CARTESIAN_POINT('Ctrl Pts',(-3.07854611663017,-37.2742356128,-10.6733698534772));
#75861=CARTESIAN_POINT('Ctrl Pts',(-4.05813867421687,-37.2742356128,-10.4126758711406));
#75862=CARTESIAN_POINT('Ctrl Pts',(-4.86043811085114,-37.2742356128,-10.1190200263027));
#75863=CARTESIAN_POINT('Ctrl Pts',(-5.62475805695127,-37.2742356128,-9.76080244433856));
#75864=CARTESIAN_POINT('Ctrl Pts',(-6.35435667676406,-37.2742356128,-9.34315312398709));
#75865=CARTESIAN_POINT('',(-1.48259713265,-37.6642356128,-10.9268000942));
#75866=CARTESIAN_POINT('',(-6.35435667676,-37.6642356128,-9.34315312398));
#75867=CARTESIAN_POINT('Origin',(-7.77156117238E-15,-38.2742356128,-0.229047725441));
#75868=CARTESIAN_POINT('',(-0.5,-37.2742356128,-11.0174674429));
#75869=CARTESIAN_POINT('Origin',(-7.77156117238E-15,-37.2742356128,-0.229047725441));
#75870=CARTESIAN_POINT('',(-0.5,-38.2742356128,-11.0174674429));
#75871=CARTESIAN_POINT('Origin',(-7.77156117238E-15,-38.2742356128,-0.229047725441));
#75872=CARTESIAN_POINT('',(0.5,-37.2742356128,-11.0174674429));
#75873=CARTESIAN_POINT('',(1.48259713217599,-37.2742356128,-10.9268000942492));
#75874=CARTESIAN_POINT('Origin',(-7.77156117238E-15,-37.2742356128,-0.229047725441));
#75875=CARTESIAN_POINT('',(1.48259713265,-38.2742356128,-10.9268000942));
#75876=CARTESIAN_POINT('',(0.5,-38.2742356128,-11.0174674429));
#75877=CARTESIAN_POINT('Ctrl Pts',(1.48259713264,-38.7742356128,-10.9268000942));
#75878=CARTESIAN_POINT('Ctrl Pts',(1.48259713264,-36.9742356128,-10.9268000942));
#75879=CARTESIAN_POINT('Ctrl Pts',(1.71328083841,-38.7742356128,-10.8948297336));
#75880=CARTESIAN_POINT('Ctrl Pts',(1.71328083841,-36.9742356128,-10.8948297336));
#75881=CARTESIAN_POINT('Ctrl Pts',(1.91354623838,-38.7742356128,-10.8659465412));
#75882=CARTESIAN_POINT('Ctrl Pts',(1.91354623838,-36.9742356128,-10.8659465412));
#75883=CARTESIAN_POINT('Ctrl Pts',(2.0855726443,-38.7742356128,-10.8395401686));
#75884=CARTESIAN_POINT('Ctrl Pts',(2.0855726443,-36.9742356128,-10.8395401686));
#75885=CARTESIAN_POINT('Ctrl Pts',(3.07854619941,-38.7742356128,-10.6733698396));
#75886=CARTESIAN_POINT('Ctrl Pts',(3.07854619941,-36.9742356128,-10.6733698396));
#75887=CARTESIAN_POINT('Ctrl Pts',(4.05813883755,-38.7742356128,-10.4126758277));
#75888=CARTESIAN_POINT('Ctrl Pts',(4.05813883755,-36.9742356128,-10.4126758277));
#75889=CARTESIAN_POINT('Ctrl Pts',(4.86043834785,-38.7742356128,-10.1190199395));
#75890=CARTESIAN_POINT('Ctrl Pts',(4.86043834785,-36.9742356128,-10.1190199395));
#75891=CARTESIAN_POINT('Ctrl Pts',(5.62475835799,-38.7742356128,-9.76080230324));
#75892=CARTESIAN_POINT('Ctrl Pts',(5.62475835799,-36.9742356128,-9.76080230324));
#75893=CARTESIAN_POINT('Ctrl Pts',(6.35435703597,-38.7742356128,-9.34315291836));
#75894=CARTESIAN_POINT('Ctrl Pts',(6.35435703597,-36.9742356128,-9.34315291836));
#75895=CARTESIAN_POINT('',(6.35435667676,-37.2742356128,-9.34315312398));
#75896=CARTESIAN_POINT('',(6.35435667676,-37.6642356128,-9.34315312398));
#75897=CARTESIAN_POINT('Ctrl Pts',(1.48259713264,-37.2742356128,-10.9268000942));
#75898=CARTESIAN_POINT('Ctrl Pts',(1.71328083841,-37.2742356128,-10.8948297336));
#75899=CARTESIAN_POINT('Ctrl Pts',(1.91354623838,-37.2742356128,-10.8659465412));
#75900=CARTESIAN_POINT('Ctrl Pts',(2.0855726443,-37.2742356128,-10.8395401686));
#75901=CARTESIAN_POINT('Ctrl Pts',(3.07854611663014,-37.2742356128,-10.6733698534529));
#75902=CARTESIAN_POINT('Ctrl Pts',(4.05813867422129,-37.2742356128,-10.4126758711658));
#75903=CARTESIAN_POINT('Ctrl Pts',(4.86043811084938,-37.2742356128,-10.1190200262464));
#75904=CARTESIAN_POINT('Ctrl Pts',(5.62475805694812,-37.2742356128,-9.76080244433078));
#75905=CARTESIAN_POINT('Ctrl Pts',(6.35435667676222,-37.2742356128,-9.34315312398388));
#75906=CARTESIAN_POINT('Ctrl Pts',(7.22695646354,-38.7742356128,-8.79725933449));
#75907=CARTESIAN_POINT('Ctrl Pts',(7.22695646354,-36.9742356128,-8.79725933449));
#75908=CARTESIAN_POINT('Ctrl Pts',(7.25968775986,-38.7742356128,-8.77500998089));
#75909=CARTESIAN_POINT('Ctrl Pts',(7.25968775986,-36.9742356128,-8.77500998089));
#75910=CARTESIAN_POINT('Ctrl Pts',(7.29235374605,-38.7742356128,-8.75263626704));
#75911=CARTESIAN_POINT('Ctrl Pts',(7.29235374605,-36.9742356128,-8.75263626704));
#75912=CARTESIAN_POINT('Ctrl Pts',(7.3249555226,-38.7742356128,-8.73013845435));
#75913=CARTESIAN_POINT('Ctrl Pts',(7.3249555226,-36.9742356128,-8.73013845435));
#75914=CARTESIAN_POINT('Ctrl Pts',(7.75723078658,-38.7742356128,-8.42961072436));
#75915=CARTESIAN_POINT('Ctrl Pts',(7.75723078658,-36.9742356128,-8.42961072436));
#75916=CARTESIAN_POINT('Ctrl Pts',(8.17860364499,-38.7742356128,-8.10725352709));
#75917=CARTESIAN_POINT('Ctrl Pts',(8.17860364499,-36.9742356128,-8.10725352709));
#75918=CARTESIAN_POINT('Ctrl Pts',(8.5693207085,-38.7742356128,-7.78543946907));
#75919=CARTESIAN_POINT('Ctrl Pts',(8.5693207085,-36.9742356128,-7.78543946907));
#75920=CARTESIAN_POINT('Ctrl Pts',(8.95699215017,-38.7742356128,-7.43858429643));
#75921=CARTESIAN_POINT('Ctrl Pts',(8.95699215017,-36.9742356128,-7.43858429643));
#75922=CARTESIAN_POINT('Ctrl Pts',(9.33306737369,-38.7742356128,-7.0669188413));
#75923=CARTESIAN_POINT('Ctrl Pts',(9.33306737369,-36.9742356128,-7.0669188413));
#75924=CARTESIAN_POINT('',(9.33306511227,-37.2742356128,-7.06692107621));
#75925=CARTESIAN_POINT('',(9.33306511227,-37.6642356128,-7.06692107621));
#75926=CARTESIAN_POINT('',(7.22695685732,-37.2742356128,-8.79725906681));
#75927=CARTESIAN_POINT('',(7.22695685732,-37.6642356128,-8.79725906681));
#75928=CARTESIAN_POINT('Ctrl Pts',(7.22695685732231,-37.2742356128,-8.7972590668134));
#75929=CARTESIAN_POINT('Ctrl Pts',(7.28150888554723,-37.2742356128,-8.76017689804407));
#75930=CARTESIAN_POINT('Ctrl Pts',(7.3358430836494,-37.2742356128,-8.72268025917252));
#75931=CARTESIAN_POINT('Ctrl Pts',(7.3899712392707,-37.2742356128,-8.68477139569698));
#75932=CARTESIAN_POINT('Ctrl Pts',(7.46720182448396,-37.2742356128,-8.6306826561606));
#75933=CARTESIAN_POINT('Ctrl Pts',(7.54401747222357,-37.2742356128,-8.57575348443569));
#75934=CARTESIAN_POINT('Ctrl Pts',(7.62055514908949,-37.2742356128,-8.51991134544539));
#75935=CARTESIAN_POINT('Ctrl Pts',(7.69952766934165,-37.2742356128,-8.46229273676904));
#75936=CARTESIAN_POINT('Ctrl Pts',(7.77820421333969,-37.2742356128,-8.40370214573737));
#75937=CARTESIAN_POINT('Ctrl Pts',(7.85668116624415,-37.2742356128,-8.34407402226645));
#75938=CARTESIAN_POINT('Ctrl Pts',(7.93692573193349,-37.2742356128,-8.28310283653987));
#75939=CARTESIAN_POINT('Ctrl Pts',(8.01696145430602,-37.2742356128,-8.22104687847748));
#75940=CARTESIAN_POINT('Ctrl Pts',(8.09683736040194,-37.2742356128,-8.15785041906041));
#75941=CARTESIAN_POINT('Ctrl Pts',(8.17873759713205,-37.2742356128,-8.09305234364894));
#75942=CARTESIAN_POINT('Ctrl Pts',(8.26046963077608,-37.2742356128,-8.02705525395084));
#75943=CARTESIAN_POINT('Ctrl Pts',(8.34203275379568,-37.2742356128,-7.95981359656439));
#75944=CARTESIAN_POINT('Ctrl Pts',(8.42751622477591,-37.2742356128,-7.88933995535186));
#75945=CARTESIAN_POINT('Ctrl Pts',(8.51281409409109,-37.2742356128,-7.81749921791748));
#75946=CARTESIAN_POINT('Ctrl Pts',(8.59786908945074,-37.2742356128,-7.74425465003807));
#75947=CARTESIAN_POINT('Ctrl Pts',(8.68560880784532,-37.2742356128,-7.66869815000537));
#75948=CARTESIAN_POINT('Ctrl Pts',(8.77308976965861,-37.2742356128,-7.59164784533787));
#75949=CARTESIAN_POINT('Ctrl Pts',(8.86019351231522,-37.2742356128,-7.51307941783215));
#75950=CARTESIAN_POINT('Ctrl Pts',(8.95286440609447,-37.2742356128,-7.42948936558273));
#75951=CARTESIAN_POINT('Ctrl Pts',(9.04510813530834,-37.2742356128,-7.3441809210483));
#75952=CARTESIAN_POINT('Ctrl Pts',(9.13672354646738,-37.2742356128,-7.25714246143311));
#75953=CARTESIAN_POINT('Ctrl Pts',(9.20252620421832,-37.2742356128,-7.19462719356746));
#75954=CARTESIAN_POINT('Ctrl Pts',(9.26800342965956,-37.2742356128,-7.13121983085202));
#75955=CARTESIAN_POINT('Ctrl Pts',(9.3330651122663,-37.2742356128,-7.06692107620626));
#75956=CARTESIAN_POINT('Ctrl Pts',(10.0162216343,-38.7742356128,-6.33635360057));
#75957=CARTESIAN_POINT('Ctrl Pts',(10.0162216343,-36.9742356128,-6.33635360057));
#75958=CARTESIAN_POINT('Ctrl Pts',(10.3224768783,-38.7742356128,-5.97981782527));
#75959=CARTESIAN_POINT('Ctrl Pts',(10.3224768783,-36.9742356128,-5.97981782527));
#75960=CARTESIAN_POINT('Ctrl Pts',(10.6115458029,-38.7742356128,-5.60497678219));
#75961=CARTESIAN_POINT('Ctrl Pts',(10.6115458029,-36.9742356128,-5.60497678219));
#75962=CARTESIAN_POINT('Ctrl Pts',(10.876460919,-38.7742356128,-5.21255294902));
#75963=CARTESIAN_POINT('Ctrl Pts',(10.876460919,-36.9742356128,-5.21255294902));
#75964=CARTESIAN_POINT('Ctrl Pts',(11.5273586686,-38.7742356128,-4.07233951466));
#75965=CARTESIAN_POINT('Ctrl Pts',(11.5273586686,-36.9742356128,-4.07233951466));
#75966=CARTESIAN_POINT('Ctrl Pts',(11.912489836,-38.7742356128,-2.80791655207));
#75967=CARTESIAN_POINT('Ctrl Pts',(11.912489836,-36.9742356128,-2.80791655207));
#75968=CARTESIAN_POINT('Ctrl Pts',(12.0219871572,-38.7742356128,-1.97477394764));
#75969=CARTESIAN_POINT('Ctrl Pts',(12.0219871572,-36.9742356128,-1.97477394764));
#75970=CARTESIAN_POINT('Ctrl Pts',(12.0360485934,-38.7742356128,-0.887789304964));
#75971=CARTESIAN_POINT('Ctrl Pts',(12.0360485934,-36.9742356128,-0.887789304964));
#75972=CARTESIAN_POINT('Ctrl Pts',(11.941568867,-38.7742356128,0.143912935026));
#75973=CARTESIAN_POINT('Ctrl Pts',(11.941568867,-36.9742356128,0.143912935026));
#75974=CARTESIAN_POINT('Ctrl Pts',(11.9112061973,-38.7742356128,0.407077462691));
#75975=CARTESIAN_POINT('Ctrl Pts',(11.9112061973,-36.9742356128,0.407077462691));
#75976=CARTESIAN_POINT('Ctrl Pts',(11.8758398702,-38.7742356128,0.666630263604));
#75977=CARTESIAN_POINT('Ctrl Pts',(11.8758398702,-36.9742356128,0.666630263604));
#75978=CARTESIAN_POINT('Ctrl Pts',(11.8354184104,-38.7742356128,0.924526608307));
#75979=CARTESIAN_POINT('Ctrl Pts',(11.8354184104,-36.9742356128,0.924526608307));
#75980=CARTESIAN_POINT('',(10.0162216343,-37.2742356128,-6.33635360057));
#75981=CARTESIAN_POINT('',(10.0162216343,-37.6642356128,-6.33635360057));
#75982=CARTESIAN_POINT('',(11.8354184104,-37.2742356128,0.924526608307));
#75983=CARTESIAN_POINT('Ctrl Pts',(10.0162216343,-37.2742356128,-6.33635360057));
#75984=CARTESIAN_POINT('Ctrl Pts',(10.3224768783,-37.2742356128,-5.97981782527));
#75985=CARTESIAN_POINT('Ctrl Pts',(10.6115458029,-37.2742356128,-5.60497678219));
#75986=CARTESIAN_POINT('Ctrl Pts',(10.876460919,-37.2742356128,-5.21255294902));
#75987=CARTESIAN_POINT('Ctrl Pts',(11.5273586686,-37.2742356128,-4.07233951466));
#75988=CARTESIAN_POINT('Ctrl Pts',(11.912489836,-37.2742356128,-2.80791655207));
#75989=CARTESIAN_POINT('Ctrl Pts',(12.0219871572,-37.2742356128,-1.97477394764));
#75990=CARTESIAN_POINT('Ctrl Pts',(12.0360485934,-37.2742356128,-0.887789304964));
#75991=CARTESIAN_POINT('Ctrl Pts',(11.941568867,-37.2742356128,0.143912935026));
#75992=CARTESIAN_POINT('Ctrl Pts',(11.9112061973,-37.2742356128,0.407077462691));
#75993=CARTESIAN_POINT('Ctrl Pts',(11.8758398702,-37.2742356128,0.666630263604));
#75994=CARTESIAN_POINT('Ctrl Pts',(11.8354184104,-37.2742356128,0.924526608307));
#75995=CARTESIAN_POINT('',(11.8354184104,-37.6642356128,0.924526608307));
#75996=CARTESIAN_POINT('Ctrl Pts',(11.0086556946,-38.7742356128,3.43000353527));
#75997=CARTESIAN_POINT('Ctrl Pts',(11.0086556946,-36.9742356128,3.43000353527));
#75998=CARTESIAN_POINT('Ctrl Pts',(11.0817932058,-38.7742356128,3.31017227332));
#75999=CARTESIAN_POINT('Ctrl Pts',(11.0817932058,-36.9742356128,3.31017227332));
#76000=CARTESIAN_POINT('Ctrl Pts',(11.1567853729,-38.7742356128,3.18040212706));
#76001=CARTESIAN_POINT('Ctrl Pts',(11.1567853729,-36.9742356128,3.18040212706));
#76002=CARTESIAN_POINT('Ctrl Pts',(11.2288017566,-38.7742356128,3.0447194315));
#76003=CARTESIAN_POINT('Ctrl Pts',(11.2288017566,-36.9742356128,3.0447194315));
#76004=CARTESIAN_POINT('Ctrl Pts',(11.4529799792,-38.7742356128,2.57934328034));
#76005=CARTESIAN_POINT('Ctrl Pts',(11.4529799792,-36.9742356128,2.57934328034));
#76006=CARTESIAN_POINT('Ctrl Pts',(11.6140362762,-38.7742356128,2.09446235244));
#76007=CARTESIAN_POINT('Ctrl Pts',(11.6140362762,-36.9742356128,2.09446235244));
#76008=CARTESIAN_POINT('Ctrl Pts',(11.6871718767,-38.7742356128,1.76491172368));
#76009=CARTESIAN_POINT('Ctrl Pts',(11.6871718767,-36.9742356128,1.76491172368));
#76010=CARTESIAN_POINT('Ctrl Pts',(11.7534189237,-38.7742356128,1.41966067629));
#76011=CARTESIAN_POINT('Ctrl Pts',(11.7534189237,-36.9742356128,1.41966067629));
#76012=CARTESIAN_POINT('Ctrl Pts',(11.809039671,-38.7742356128,1.08859783468));
#76013=CARTESIAN_POINT('Ctrl Pts',(11.809039671,-36.9742356128,1.08859783468));
#76014=CARTESIAN_POINT('Ctrl Pts',(11.8179542567,-38.7742356128,1.03442695212));
#76015=CARTESIAN_POINT('Ctrl Pts',(11.8179542567,-36.9742356128,1.03442695212));
#76016=CARTESIAN_POINT('Ctrl Pts',(11.8267316409,-38.7742356128,0.979949794408));
#76017=CARTESIAN_POINT('Ctrl Pts',(11.8267316409,-36.9742356128,0.979949794408));
#76018=CARTESIAN_POINT('Ctrl Pts',(11.8354184104,-38.7742356128,0.924526608307));
#76019=CARTESIAN_POINT('Ctrl Pts',(11.8354184104,-36.9742356128,0.924526608307));
#76020=CARTESIAN_POINT('',(11.0086556946,-37.2742356128,3.43000353527));
#76021=CARTESIAN_POINT('',(11.0086556946,-37.6642356128,3.43000353527));
#76022=CARTESIAN_POINT('Ctrl Pts',(11.0086556946,-37.2742356128,3.43000353527));
#76023=CARTESIAN_POINT('Ctrl Pts',(11.0817932058,-37.2742356128,3.31017227332));
#76024=CARTESIAN_POINT('Ctrl Pts',(11.1567853729,-37.2742356128,3.18040212706));
#76025=CARTESIAN_POINT('Ctrl Pts',(11.2288017566,-37.2742356128,3.0447194315));
#76026=CARTESIAN_POINT('Ctrl Pts',(11.4529799792,-37.2742356128,2.57934328034));
#76027=CARTESIAN_POINT('Ctrl Pts',(11.6140362762,-37.2742356128,2.09446235244));
#76028=CARTESIAN_POINT('Ctrl Pts',(11.6871718767,-37.2742356128,1.76491172368));
#76029=CARTESIAN_POINT('Ctrl Pts',(11.7534189237,-37.2742356128,1.41966067629));
#76030=CARTESIAN_POINT('Ctrl Pts',(11.809039671,-37.2742356128,1.08859783468));
#76031=CARTESIAN_POINT('Ctrl Pts',(11.8179542567,-37.2742356128,1.03442695212));
#76032=CARTESIAN_POINT('Ctrl Pts',(11.8267316409,-37.2742356128,0.979949794408));
#76033=CARTESIAN_POINT('Ctrl Pts',(11.8354184104,-37.2742356128,0.924526608307));
#76034=CARTESIAN_POINT('Ctrl Pts',(11.0086556946,-38.7742356128,3.43000353527));
#76035=CARTESIAN_POINT('Ctrl Pts',(11.0086556946,-36.9742356128,3.43000353527));
#76036=CARTESIAN_POINT('Ctrl Pts',(10.8267791086,-38.7742356128,3.7279970062));
#76037=CARTESIAN_POINT('Ctrl Pts',(10.8267791086,-36.9742356128,3.7279970062));
#76038=CARTESIAN_POINT('Ctrl Pts',(10.6180941124,-38.7742356128,4.02812460647));
#76039=CARTESIAN_POINT('Ctrl Pts',(10.6180941124,-36.9742356128,4.02812460647));
#76040=CARTESIAN_POINT('Ctrl Pts',(10.3610804417,-38.7742356128,4.34854162483));
#76041=CARTESIAN_POINT('Ctrl Pts',(10.3610804417,-36.9742356128,4.34854162483));
#76042=CARTESIAN_POINT('Ctrl Pts',(9.81894561437,-38.7742356128,4.82846996464));
#76043=CARTESIAN_POINT('Ctrl Pts',(9.81894561437,-36.9742356128,4.82846996464));
#76044=CARTESIAN_POINT('Ctrl Pts',(9.1449448519,-38.7742356128,5.15260465424));
#76045=CARTESIAN_POINT('Ctrl Pts',(9.1449448519,-36.9742356128,5.15260465424));
#76046=CARTESIAN_POINT('Ctrl Pts',(8.86735473037,-38.7742356128,5.24791616482));
#76047=CARTESIAN_POINT('Ctrl Pts',(8.86735473037,-36.9742356128,5.24791616482));
#76048=CARTESIAN_POINT('Ctrl Pts',(8.35592834321,-38.7742356128,5.35778460397));
#76049=CARTESIAN_POINT('Ctrl Pts',(8.35592834321,-36.9742356128,5.35778460397));
#76050=CARTESIAN_POINT('Ctrl Pts',(7.83459380784,-38.7742356128,5.3594412401));
#76051=CARTESIAN_POINT('Ctrl Pts',(7.83459380784,-36.9742356128,5.3594412401));
#76052=CARTESIAN_POINT('Ctrl Pts',(7.6075384225,-38.7742356128,5.33903210576));
#76053=CARTESIAN_POINT('Ctrl Pts',(7.6075384225,-36.9742356128,5.33903210576));
#76054=CARTESIAN_POINT('Ctrl Pts',(7.38481168145,-38.7742356128,5.2985941411));
#76055=CARTESIAN_POINT('Ctrl Pts',(7.38481168145,-36.9742356128,5.2985941411));
#76056=CARTESIAN_POINT('Ctrl Pts',(7.16875088157,-38.7742356128,5.23983755655));
#76057=CARTESIAN_POINT('Ctrl Pts',(7.16875088157,-36.9742356128,5.23983755655));
#76058=CARTESIAN_POINT('',(7.16875088104636,-37.2742356128,5.23983755640952));
#76059=CARTESIAN_POINT('Ctrl Pts',(11.0086556946,-37.2742356128,3.43000353527));
#76060=CARTESIAN_POINT('Ctrl Pts',(10.8267791086,-37.2742356128,3.7279970062));
#76061=CARTESIAN_POINT('Ctrl Pts',(10.6180941124,-37.2742356128,4.02812460647));
#76062=CARTESIAN_POINT('Ctrl Pts',(10.3610804417,-37.2742356128,4.34854162483));
#76063=CARTESIAN_POINT('Ctrl Pts',(9.81894561437,-37.2742356128,4.82846996464));
#76064=CARTESIAN_POINT('Ctrl Pts',(9.1449448519,-37.2742356128,5.15260465424));
#76065=CARTESIAN_POINT('Ctrl Pts',(8.86735473037,-37.2742356128,5.24791616482));
#76066=CARTESIAN_POINT('Ctrl Pts',(8.35592834321,-37.2742356128,5.35778460397));
#76067=CARTESIAN_POINT('Ctrl Pts',(7.83459380784,-37.2742356128,5.3594412401));
#76068=CARTESIAN_POINT('Ctrl Pts',(7.6075384225,-37.2742356128,5.33903210576));
#76069=CARTESIAN_POINT('Ctrl Pts',(7.38481168145,-37.2742356128,5.2985941411));
#76070=CARTESIAN_POINT('Ctrl Pts',(7.16875088157,-37.2742356128,5.23983755655));
#76071=CARTESIAN_POINT('',(7.16875088157,-37.6642356128,5.23983755655));
#76072=CARTESIAN_POINT('Origin',(7.14250943682,-38.2742356128,5.33633308276));
#76073=CARTESIAN_POINT('',(7.04251644773,-37.2742356128,5.33751720019));
#76074=CARTESIAN_POINT('Origin',(7.14250943682,-37.2742356128,5.33633308276));
#76075=CARTESIAN_POINT('',(7.04251644773,-38.2742356128,5.33751720019));
#76076=CARTESIAN_POINT('Origin',(-0.000416107150126,-37.6642356128,5.42091963994));
#76077=CARTESIAN_POINT('',(0.5,-37.2742356128,12.4465469186));
#76078=CARTESIAN_POINT('Origin',(-0.000416107150126,-37.2742356128,5.42091963994));
#76079=CARTESIAN_POINT('',(0.5,-37.6642356128,12.4465469186));
#76080=CARTESIAN_POINT('Origin',(-7.48272894647,-41.3342356129,11.6412701168));
#76081=CARTESIAN_POINT('',(-8.73272894647,-40.7742356128,11.6412701168));
#76082=CARTESIAN_POINT('Origin',(-7.48272894647,-40.7742356128,11.6412701168));
#76083=CARTESIAN_POINT('',(-8.73272894647,-41.3342356129,11.6412701168));
#76084=CARTESIAN_POINT('Origin',(-3.35265884719E-30,-41.6742356128,3.15283103411E-22));
#76085=CARTESIAN_POINT('',(-4.44384247076,-41.6742356128,6.92091963994));
#76086=CARTESIAN_POINT('Origin',(-0.000416107150126,-41.6742356128,6.92091963994));
#76087=CARTESIAN_POINT('',(4.44384247076,-41.6742356128,3.34084221874));
#76088=CARTESIAN_POINT('',(4.44384247076,-41.6742356128,5.13088092934));
#76089=CARTESIAN_POINT('',(2.13594446644908E-16,-41.6742356128,-0.964849202557427));
#76090=CARTESIAN_POINT('Origin',(6.82290383517,-41.6742356128,-3.56061176027));
#76091=CARTESIAN_POINT('',(-4.44384247076,-41.6742356128,3.34084221874));
#76092=CARTESIAN_POINT('Origin',(-6.82290383517,-41.6742356128,-3.56061176027));
#76093=CARTESIAN_POINT('',(-4.44384247076,-41.6742356128,5.13088092934));
#76094=CARTESIAN_POINT('Origin',(-3.35265884719E-30,-41.6742356128,3.15283103411E-22));
#76095=CARTESIAN_POINT('',(11.5229038352,-41.6742356128,-3.56061176027));
#76096=CARTESIAN_POINT('Origin',(6.82290383517,-41.6742356128,-3.56061176027));
#76097=CARTESIAN_POINT('Origin',(-3.35265884719E-30,-41.6742356128,3.15283103411E-22));
#76098=CARTESIAN_POINT('',(-11.5229038352,-41.6742356128,-3.56061176027));
#76099=CARTESIAN_POINT('Origin',(-6.82290383517,-41.6742356128,-3.56061176027));
#76100=CARTESIAN_POINT('Origin',(7.48272894647,-41.3342356129,11.6412701168));
#76101=CARTESIAN_POINT('',(8.73272894647,-40.7742356128,11.6412701168));
#76102=CARTESIAN_POINT('',(8.73272894647,-41.3342356129,11.6412701168));
#76103=CARTESIAN_POINT('Origin',(7.48272894647,-40.7742356128,11.6412701168));
#76104=CARTESIAN_POINT('Origin',(-3.35265884719E-30,-40.7742356128,3.15283103411E-22));
#76105=CARTESIAN_POINT('Origin',(-0.000416107150126,-40.1142356128,6.92091963994));
#76106=CARTESIAN_POINT('',(-4.44384247076,-39.7742356128,6.92091963994));
#76107=CARTESIAN_POINT('',(-4.44384247076,-40.1142356128,6.92091963994));
#76108=CARTESIAN_POINT('',(-3.64378781517,-39.7742356128,9.46451560746));
#76109=CARTESIAN_POINT('Origin',(-0.000416107150126,-39.7742356128,6.92091963994));
#76110=CARTESIAN_POINT('Origin',(-0.000416107150126,-39.7742356128,6.92091963994));
#76111=CARTESIAN_POINT('Origin',(4.44384247076,-41.6742356128,6.92091963994));
#76112=CARTESIAN_POINT('',(4.44384253205641,-39.7742356128,5.42595709132001));
#76113=CARTESIAN_POINT('',(4.44384247076,-39.7742356128,6.17343837159));
#76114=CARTESIAN_POINT('',(4.44384264824955,-39.7742356128,5.30375137006997));
#76115=CARTESIAN_POINT('Ctrl Pts',(4.44384282525,-39.7742356128,5.30375137007));
#76116=CARTESIAN_POINT('Ctrl Pts',(4.44414005184279,-39.7742356128,5.32817576412788));
#76117=CARTESIAN_POINT('Ctrl Pts',(4.44428140248426,-39.7742356128,5.35261020505899));
#76118=CARTESIAN_POINT('Ctrl Pts',(4.44427352568687,-39.7742356128,5.37705311235898));
#76119=CARTESIAN_POINT('Ctrl Pts',(4.44412423208254,-39.7742356128,5.40150273088309));
#76120=CARTESIAN_POINT('Ctrl Pts',(4.44384259285,-39.7742356128,5.42595709132));
#76121=CARTESIAN_POINT('',(4.44384247076,-39.7742356128,3.34084221874));
#76122=CARTESIAN_POINT('',(4.44384247076,-39.7742356128,4.32229681001));
#76123=CARTESIAN_POINT('',(4.44384247076,-40.7242356128,3.34084221874));
#76124=CARTESIAN_POINT('Origin',(6.82290383517,-40.1142356128,-3.56061176027));
#76125=CARTESIAN_POINT('',(3.94523376325645,-39.7742356128,3.14826407381823));
#76126=CARTESIAN_POINT('Origin',(6.82290383517,-39.7742356128,-3.56061176027));
#76127=CARTESIAN_POINT('',(2.13594446644908E-16,-39.7742356128,-0.964849202557427));
#76128=CARTESIAN_POINT('Origin',(6.82290383517,-39.7742356128,-3.56061176027));
#76129=CARTESIAN_POINT('',(0.,-40.1142356128,-0.964849202557427));
#76130=CARTESIAN_POINT('Origin',(-6.82290383517,-40.1142356128,-3.56061176027));
#76131=CARTESIAN_POINT('',(-3.94523376325647,-39.7742356128,3.14826407381824));
#76132=CARTESIAN_POINT('Origin',(-6.82290383517,-39.7742356128,-3.56061176027));
#76133=CARTESIAN_POINT('',(-4.44384247076,-39.7742356128,3.34084221874));
#76134=CARTESIAN_POINT('Origin',(-6.82290383517,-39.7742356128,-3.56061176027));
#76135=CARTESIAN_POINT('',(-4.44384247076,-40.1142356128,3.34084221874));
#76136=CARTESIAN_POINT('Origin',(-4.44384247076,-41.6742356128,6.92091963994));
#76137=CARTESIAN_POINT('',(-4.44384264824955,-39.7742356128,5.30375137006997));
#76138=CARTESIAN_POINT('',(-4.44384247076,-39.7742356128,4.32229681001));
#76139=CARTESIAN_POINT('',(-4.44384253205641,-39.7742356128,5.42595709132));
#76140=CARTESIAN_POINT('',(-4.44384282525,-39.7742356128,5.30375137007));
#76141=CARTESIAN_POINT('',(-4.44384247076,-39.7742356128,6.17343837159));
#76142=CARTESIAN_POINT('Origin',(6.82290383517,-40.1142356128,-3.56061176027));
#76143=CARTESIAN_POINT('',(11.52290383517,-39.7742356128,-3.56061176027));
#76144=CARTESIAN_POINT('',(11.52290383517,-40.1142356128,-3.56061176027));
#76145=CARTESIAN_POINT('',(4.25781969055054,-39.7742356128,-7.49892908595644));
#76146=CARTESIAN_POINT('Origin',(6.82290383517,-39.7742356128,-3.56061176027));
#76147=CARTESIAN_POINT('',(2.26246783444344,-39.7742356128,-4.69745981422045));
#76148=CARTESIAN_POINT('Origin',(6.82290383517,-39.7742356128,-3.56061176027));
#76149=CARTESIAN_POINT('',(2.12330457313532,-39.7742356128,-3.4993320503742));
#76150=CARTESIAN_POINT('Origin',(6.82290383517,-39.7742356128,-3.56061176027));
#76151=CARTESIAN_POINT('',(6.02437852526,-39.7742356128,1.07105719697));
#76152=CARTESIAN_POINT('Origin',(6.82290383517,-39.7742356128,-3.56061176027));
#76153=CARTESIAN_POINT('',(7.04639034599947,-39.7742356128,1.1340718008604));
#76154=CARTESIAN_POINT('Origin',(6.82290383517,-39.7742356128,-3.56061176027));
#76155=CARTESIAN_POINT('',(9.24345637220266,-39.7742356128,0.468150497498442));
#76156=CARTESIAN_POINT('Origin',(6.82290383517,-39.7742356128,-3.56061176027));
#76157=CARTESIAN_POINT('Origin',(6.82290383517,-39.7742356128,-3.56061176027));
#76158=CARTESIAN_POINT('Origin',(-6.82290383517,-40.1142356128,-3.56061176027));
#76159=CARTESIAN_POINT('',(-4.25781969055053,-39.7742356128,-7.49892908595644));
#76160=CARTESIAN_POINT('',(-11.52290383517,-39.7742356128,-3.56061176027));
#76161=CARTESIAN_POINT('Origin',(-6.82290383517,-39.7742356128,-3.56061176027));
#76162=CARTESIAN_POINT('',(-11.52290383517,-40.1142356128,-3.56061176027));
#76163=CARTESIAN_POINT('',(-9.24345637220266,-39.7742356128,0.468150497498443));
#76164=CARTESIAN_POINT('Origin',(-6.82290383517,-39.7742356128,-3.56061176027));
#76165=CARTESIAN_POINT('',(-7.04639034599947,-39.7742356128,1.1340718008604));
#76166=CARTESIAN_POINT('Origin',(-6.82290383517,-39.7742356128,-3.56061176027));
#76167=CARTESIAN_POINT('',(-6.02437852526,-39.7742356128,1.07105719696));
#76168=CARTESIAN_POINT('Origin',(-6.82290383517,-39.7742356128,-3.56061176027));
#76169=CARTESIAN_POINT('',(-2.12330457313532,-39.7742356128,-3.4993320503742));
#76170=CARTESIAN_POINT('Origin',(-6.82290383517,-39.7742356128,-3.56061176027));
#76171=CARTESIAN_POINT('',(-2.26246783444344,-39.7742356128,-4.69745981422044));
#76172=CARTESIAN_POINT('Origin',(-6.82290383517,-39.7742356128,-3.56061176027));
#76173=CARTESIAN_POINT('Origin',(-6.82290383517,-39.7742356128,-3.56061176027));
#76174=CARTESIAN_POINT('Origin',(-3.35265884719E-30,-40.7742356128,3.15283103411E-22));
#76175=CARTESIAN_POINT('Origin',(0.000416107150126,-37.6642356128,5.42091963994));
#76176=CARTESIAN_POINT('',(2.84060969191E-17,-37.2742356128,11.6643459897));
#76177=CARTESIAN_POINT('',(-6.16208308783,-37.2742356128,4.4189333977));
#76178=CARTESIAN_POINT('Origin',(0.000416107150126,-37.2742356128,5.42091963994));
#76179=CARTESIAN_POINT('',(-1.41472120477E-15,-38.2742356128,11.6643459897));
#76180=CARTESIAN_POINT('',(-1.41472120477E-15,-37.6642356128,11.6643459897));
#76181=CARTESIAN_POINT('',(-6.16208308783,-38.2742356128,4.4189333977));
#76182=CARTESIAN_POINT('Origin',(0.000416107150126,-38.2742356128,5.42091963994));
#76183=CARTESIAN_POINT('',(-6.16208308783,-37.6642356128,4.4189333977));
#76184=CARTESIAN_POINT('Origin',(-6.45819449379,-38.2742356128,4.370787419));
#76185=CARTESIAN_POINT('',(-6.62478636305302,-37.2742356128,4.12129363273029));
#76186=CARTESIAN_POINT('',(-6.62478636278,-38.2742356128,4.12129363314));
#76187=CARTESIAN_POINT('',(-6.62478636278,-38.2742356128,4.12129363314));
#76188=CARTESIAN_POINT('Origin',(-6.45819449379,-37.2742356128,4.370787419));
#76189=CARTESIAN_POINT('Origin',(-6.45819449379,-38.2742356128,4.370787419));
#76190=CARTESIAN_POINT('Ctrl Pts',(-10.3257952821,-38.2742356128,3.01322822759));
#76191=CARTESIAN_POINT('Ctrl Pts',(-10.3257952821,-37.0742356128,3.01322822759));
#76192=CARTESIAN_POINT('Ctrl Pts',(-10.1889067725,-38.2742356128,3.23751153419));
#76193=CARTESIAN_POINT('Ctrl Pts',(-10.1889067725,-37.0742356128,3.23751153419));
#76194=CARTESIAN_POINT('Ctrl Pts',(-10.0345376971,-38.2742356128,3.46376526851));
#76195=CARTESIAN_POINT('Ctrl Pts',(-10.0345376971,-37.0742356128,3.46376526851));
#76196=CARTESIAN_POINT('Ctrl Pts',(-9.84518696085,-38.2742356128,3.7116414664));
#76197=CARTESIAN_POINT('Ctrl Pts',(-9.84518696085,-37.0742356128,3.7116414664));
#76198=CARTESIAN_POINT('Ctrl Pts',(-9.43247784233,-38.2742356128,4.11040580001));
#76199=CARTESIAN_POINT('Ctrl Pts',(-9.43247784233,-37.0742356128,4.11040580001));
#76200=CARTESIAN_POINT('Ctrl Pts',(-8.89477751089,-38.2742356128,4.39069936375));
#76201=CARTESIAN_POINT('Ctrl Pts',(-8.89477751089,-37.0742356128,4.39069936375));
#76202=CARTESIAN_POINT('Ctrl Pts',(-8.65375386005,-38.2742356128,4.47753838835));
#76203=CARTESIAN_POINT('Ctrl Pts',(-8.65375386005,-37.0742356128,4.47753838835));
#76204=CARTESIAN_POINT('Ctrl Pts',(-8.18724170147,-38.2742356128,4.57349385703));
#76205=CARTESIAN_POINT('Ctrl Pts',(-8.18724170147,-37.0742356128,4.57349385703));
#76206=CARTESIAN_POINT('Ctrl Pts',(-7.71488023342,-38.2742356128,4.54915455659));
#76207=CARTESIAN_POINT('Ctrl Pts',(-7.71488023342,-37.0742356128,4.54915455659));
#76208=CARTESIAN_POINT('Ctrl Pts',(-7.50094363126,-38.2742356128,4.51252661069));
#76209=CARTESIAN_POINT('Ctrl Pts',(-7.50094363126,-37.0742356128,4.51252661069));
#76210=CARTESIAN_POINT('Ctrl Pts',(-7.18780951373,-38.2742356128,4.42164672508));
#76211=CARTESIAN_POINT('Ctrl Pts',(-7.18780951373,-37.0742356128,4.42164672508));
#76212=CARTESIAN_POINT('Ctrl Pts',(-6.90087465334,-38.2742356128,4.28688202824));
#76213=CARTESIAN_POINT('Ctrl Pts',(-6.90087465334,-37.0742356128,4.28688202824));
#76214=CARTESIAN_POINT('Ctrl Pts',(-6.80533495241,-38.2742356128,4.23572805208));
#76215=CARTESIAN_POINT('Ctrl Pts',(-6.80533495241,-37.0742356128,4.23572805208));
#76216=CARTESIAN_POINT('Ctrl Pts',(-6.71329436634,-38.2742356128,4.1803921541));
#76217=CARTESIAN_POINT('Ctrl Pts',(-6.71329436634,-37.0742356128,4.1803921541));
#76218=CARTESIAN_POINT('Ctrl Pts',(-6.62478636278,-38.2742356128,4.12129363314));
#76219=CARTESIAN_POINT('Ctrl Pts',(-6.62478636278,-37.0742356128,4.12129363314));
#76220=CARTESIAN_POINT('',(-10.3257952821,-38.2742356128,3.01322822759));
#76221=CARTESIAN_POINT('Ctrl Pts',(-10.3257952821,-38.2742356128,3.01322822759));
#76222=CARTESIAN_POINT('Ctrl Pts',(-10.1889067725,-38.2742356128,3.23751153419));
#76223=CARTESIAN_POINT('Ctrl Pts',(-10.0345376971,-38.2742356128,3.46376526851));
#76224=CARTESIAN_POINT('Ctrl Pts',(-9.84518696085,-38.2742356128,3.7116414664));
#76225=CARTESIAN_POINT('Ctrl Pts',(-9.43247784233,-38.2742356128,4.11040580001));
#76226=CARTESIAN_POINT('Ctrl Pts',(-8.89477751089,-38.2742356128,4.39069936375));
#76227=CARTESIAN_POINT('Ctrl Pts',(-8.65375386005,-38.2742356128,4.47753838835));
#76228=CARTESIAN_POINT('Ctrl Pts',(-8.18724170147,-38.2742356128,4.57349385703));
#76229=CARTESIAN_POINT('Ctrl Pts',(-7.71488023342,-38.2742356128,4.54915455659));
#76230=CARTESIAN_POINT('Ctrl Pts',(-7.50094363126,-38.2742356128,4.51252661069));
#76231=CARTESIAN_POINT('Ctrl Pts',(-7.18780951373,-38.2742356128,4.42164672508));
#76232=CARTESIAN_POINT('Ctrl Pts',(-6.90087465334,-38.2742356128,4.28688202824));
#76233=CARTESIAN_POINT('Ctrl Pts',(-6.80533495241,-38.2742356128,4.23572805208));
#76234=CARTESIAN_POINT('Ctrl Pts',(-6.71329436634,-38.2742356128,4.1803921541));
#76235=CARTESIAN_POINT('Ctrl Pts',(-6.62478636278,-38.2742356128,4.12129363314));
#76236=CARTESIAN_POINT('',(-10.3257952821,-37.2742356128,3.01322822759));
#76237=CARTESIAN_POINT('',(-10.3257952821,-37.6642356128,3.01322822759));
#76238=CARTESIAN_POINT('Ctrl Pts',(-10.3257952821,-37.2742356128,3.01322822759));
#76239=CARTESIAN_POINT('Ctrl Pts',(-10.1889067725,-37.2742356128,3.23751153419));
#76240=CARTESIAN_POINT('Ctrl Pts',(-10.0345376971,-37.2742356128,3.46376526851));
#76241=CARTESIAN_POINT('Ctrl Pts',(-9.84518696085,-37.2742356128,3.7116414664));
#76242=CARTESIAN_POINT('Ctrl Pts',(-9.43247784233,-37.2742356128,4.11040580001));
#76243=CARTESIAN_POINT('Ctrl Pts',(-8.89477751089,-37.2742356128,4.39069936375));
#76244=CARTESIAN_POINT('Ctrl Pts',(-8.65375386005,-37.2742356128,4.47753838835));
#76245=CARTESIAN_POINT('Ctrl Pts',(-8.18724170147,-37.2742356128,4.57349385703));
#76246=CARTESIAN_POINT('Ctrl Pts',(-7.71488023342,-37.2742356128,4.54915455659));
#76247=CARTESIAN_POINT('Ctrl Pts',(-7.50094363126,-37.2742356128,4.51252661069));
#76248=CARTESIAN_POINT('Ctrl Pts',(-7.18780951373,-37.2742356128,4.42164672508));
#76249=CARTESIAN_POINT('Ctrl Pts',(-6.90087465334,-37.2742356128,4.28688202824));
#76250=CARTESIAN_POINT('Ctrl Pts',(-6.80533495241,-37.2742356128,4.23572805208));
#76251=CARTESIAN_POINT('Ctrl Pts',(-6.71329436634,-37.2742356128,4.1803921541));
#76252=CARTESIAN_POINT('Ctrl Pts',(-6.62478636278,-37.2742356128,4.12129363314));
#76253=CARTESIAN_POINT('Ctrl Pts',(-10.3257952821,-38.2742356128,3.01322822759));
#76254=CARTESIAN_POINT('Ctrl Pts',(-10.3257952821,-37.0742356128,3.01322822759));
#76255=CARTESIAN_POINT('Ctrl Pts',(-10.3936895385,-38.2742356128,2.90198771249));
#76256=CARTESIAN_POINT('Ctrl Pts',(-10.3936895385,-37.0742356128,2.90198771249));
#76257=CARTESIAN_POINT('Ctrl Pts',(-10.4633847104,-38.2742356128,2.78112368582));
#76258=CARTESIAN_POINT('Ctrl Pts',(-10.4633847104,-37.0742356128,2.78112368582));
#76259=CARTESIAN_POINT('Ctrl Pts',(-10.529369928,-38.2742356128,2.6551197645));
#76260=CARTESIAN_POINT('Ctrl Pts',(-10.529369928,-37.0742356128,2.6551197645));
#76261=CARTESIAN_POINT('Ctrl Pts',(-10.7481461165,-38.2742356128,2.18905363863));
#76262=CARTESIAN_POINT('Ctrl Pts',(-10.7481461165,-37.0742356128,2.18905363863));
#76263=CARTESIAN_POINT('Ctrl Pts',(-10.8940097918,-38.2742356128,1.69832265276));
#76264=CARTESIAN_POINT('Ctrl Pts',(-10.8940097918,-37.0742356128,1.69832265276));
#76265=CARTESIAN_POINT('Ctrl Pts',(-10.9488467638,-38.2742356128,1.36851337106));
#76266=CARTESIAN_POINT('Ctrl Pts',(-10.9488467638,-37.0742356128,1.36851337106));
#76267=CARTESIAN_POINT('Ctrl Pts',(-10.9986655796,-38.2742356128,1.09670268406));
#76268=CARTESIAN_POINT('Ctrl Pts',(-10.9986655796,-37.0742356128,1.09670268406));
#76269=CARTESIAN_POINT('Ctrl Pts',(-11.0450673741,-38.2742356128,0.800650704934));
#76270=CARTESIAN_POINT('Ctrl Pts',(-11.0450673741,-37.0742356128,0.800650704934));
#76271=CARTESIAN_POINT('',(-11.0450673741,-38.2742356128,0.800650704934));
#76272=CARTESIAN_POINT('',(-11.0450673741,-37.2742356128,0.800650704934));
#76273=CARTESIAN_POINT('',(-11.0450673741,-37.6642356128,0.800650704934));
#76274=CARTESIAN_POINT('Ctrl Pts',(-10.3257952821,-37.2742356128,3.01322822759));
#76275=CARTESIAN_POINT('Ctrl Pts',(-10.3936895385,-37.2742356128,2.90198771249));
#76276=CARTESIAN_POINT('Ctrl Pts',(-10.4633847104,-37.2742356128,2.78112368582));
#76277=CARTESIAN_POINT('Ctrl Pts',(-10.529369928,-37.2742356128,2.6551197645));
#76278=CARTESIAN_POINT('Ctrl Pts',(-10.7481461165,-37.2742356128,2.18905363863));
#76279=CARTESIAN_POINT('Ctrl Pts',(-10.8940097918,-37.2742356128,1.69832265276));
#76280=CARTESIAN_POINT('Ctrl Pts',(-10.9488467638,-37.2742356128,1.36851337106));
#76281=CARTESIAN_POINT('Ctrl Pts',(-10.9986655796,-37.2742356128,1.09670268406));
#76282=CARTESIAN_POINT('Ctrl Pts',(-11.0450673741,-37.2742356128,0.800650704934));
#76283=CARTESIAN_POINT('Ctrl Pts',(-10.3257952821,-38.2742356128,3.01322822759));
#76284=CARTESIAN_POINT('Ctrl Pts',(-10.3936895385,-38.2742356128,2.90198771249));
#76285=CARTESIAN_POINT('Ctrl Pts',(-10.4633847104,-38.2742356128,2.78112368582));
#76286=CARTESIAN_POINT('Ctrl Pts',(-10.529369928,-38.2742356128,2.6551197645));
#76287=CARTESIAN_POINT('Ctrl Pts',(-10.7481461165,-38.2742356128,2.18905363863));
#76288=CARTESIAN_POINT('Ctrl Pts',(-10.8940097918,-38.2742356128,1.69832265276));
#76289=CARTESIAN_POINT('Ctrl Pts',(-10.9488467638,-38.2742356128,1.36851337106));
#76290=CARTESIAN_POINT('Ctrl Pts',(-10.9986655796,-38.2742356128,1.09670268406));
#76291=CARTESIAN_POINT('Ctrl Pts',(-11.0450673741,-38.2742356128,0.800650704934));
#76292=CARTESIAN_POINT('Ctrl Pts',(-1.38699292007,-38.2742356128,-10.1328356959));
#76293=CARTESIAN_POINT('Ctrl Pts',(-1.38699292007,-37.0742356128,-10.1328356959));
#76294=CARTESIAN_POINT('Ctrl Pts',(-1.5965448998,-38.2742356128,-10.1034873192));
#76295=CARTESIAN_POINT('Ctrl Pts',(-1.5965448998,-37.0742356128,-10.1034873192));
#76296=CARTESIAN_POINT('Ctrl Pts',(-1.7801692912,-38.2742356128,-10.0769073631));
#76297=CARTESIAN_POINT('Ctrl Pts',(-1.7801692912,-37.0742356128,-10.0769073631));
#76298=CARTESIAN_POINT('Ctrl Pts',(-1.93876160799,-38.2742356128,-10.0526765385));
#76299=CARTESIAN_POINT('Ctrl Pts',(-1.93876160799,-37.0742356128,-10.0526765385));
#76300=CARTESIAN_POINT('Ctrl Pts',(-2.99097855121,-38.2742356128,-9.87862177772));
#76301=CARTESIAN_POINT('Ctrl Pts',(-2.99097855121,-37.0742356128,-9.87862177772));
#76302=CARTESIAN_POINT('Ctrl Pts',(-4.02327852642,-38.2742356128,-9.59280526012));
#76303=CARTESIAN_POINT('Ctrl Pts',(-4.02327852642,-37.0742356128,-9.59280526012));
#76304=CARTESIAN_POINT('Ctrl Pts',(-4.87817843107,-38.2742356128,-9.25578182833));
#76305=CARTESIAN_POINT('Ctrl Pts',(-4.87817843107,-37.0742356128,-9.25578182833));
#76306=CARTESIAN_POINT('Ctrl Pts',(-6.60543506376,-38.2742356128,-8.36113191267));
#76307=CARTESIAN_POINT('Ctrl Pts',(-6.60543506376,-37.0742356128,-8.36113191267));
#76308=CARTESIAN_POINT('Ctrl Pts',(-8.13232532707,-38.2742356128,-7.15483556723));
#76309=CARTESIAN_POINT('Ctrl Pts',(-8.13232532707,-37.0742356128,-7.15483556723));
#76310=CARTESIAN_POINT('Ctrl Pts',(-8.9654395686,-38.2742356128,-6.4061359759));
#76311=CARTESIAN_POINT('Ctrl Pts',(-8.9654395686,-37.0742356128,-6.4061359759));
#76312=CARTESIAN_POINT('Ctrl Pts',(-10.2944051979,-38.2742356128,-4.9247261457));
#76313=CARTESIAN_POINT('Ctrl Pts',(-10.2944051979,-37.0742356128,-4.9247261457));
#76314=CARTESIAN_POINT('Ctrl Pts',(-11.0595201702,-38.2742356128,-3.0374430354));
#76315=CARTESIAN_POINT('Ctrl Pts',(-11.0595201702,-37.0742356128,-3.0374430354));
#76316=CARTESIAN_POINT('Ctrl Pts',(-11.2122743937,-38.2742356128,-2.16854923298));
#76317=CARTESIAN_POINT('Ctrl Pts',(-11.2122743937,-37.0742356128,-2.16854923298));
#76318=CARTESIAN_POINT('Ctrl Pts',(-11.2441303156,-38.2742356128,-1.03705260495));
#76319=CARTESIAN_POINT('Ctrl Pts',(-11.2441303156,-37.0742356128,-1.03705260495));
#76320=CARTESIAN_POINT('Ctrl Pts',(-11.1482748814,-38.2742356128,0.0384368560119));
#76321=CARTESIAN_POINT('Ctrl Pts',(-11.1482748814,-37.0742356128,0.0384368560119));
#76322=CARTESIAN_POINT('Ctrl Pts',(-11.1189319926,-38.2742356128,0.295374077233));
#76323=CARTESIAN_POINT('Ctrl Pts',(-11.1189319926,-37.0742356128,0.295374077233));
#76324=CARTESIAN_POINT('Ctrl Pts',(-11.0845422068,-38.2742356128,0.548794015622));
#76325=CARTESIAN_POINT('Ctrl Pts',(-11.0845422068,-37.0742356128,0.548794015622));
#76326=CARTESIAN_POINT('Ctrl Pts',(-11.0450673741,-38.2742356128,0.800650704934));
#76327=CARTESIAN_POINT('Ctrl Pts',(-11.0450673741,-37.0742356128,0.800650704934));
#76328=CARTESIAN_POINT('',(-1.3869929218376,-37.2742356128,-10.132835695642));
#76329=CARTESIAN_POINT('Ctrl Pts',(-1.38699292183902,-37.2742356128,-10.1328356956522));
#76330=CARTESIAN_POINT('Ctrl Pts',(-1.59654490104011,-37.2742356128,-10.1034873190205));
#76331=CARTESIAN_POINT('Ctrl Pts',(-1.7801692920033,-37.2742356128,-10.0769073629773));
#76332=CARTESIAN_POINT('Ctrl Pts',(-1.93876160846405,-37.2742356128,-10.0526765384216));
#76333=CARTESIAN_POINT('Ctrl Pts',(-2.99097855144254,-37.2742356128,-9.87862177765562));
#76334=CARTESIAN_POINT('Ctrl Pts',(-4.02327852642,-37.2742356128,-9.59280526012));
#76335=CARTESIAN_POINT('Ctrl Pts',(-4.87817843107,-37.2742356128,-9.25578182833));
#76336=CARTESIAN_POINT('Ctrl Pts',(-6.60543506376,-37.2742356128,-8.36113191267));
#76337=CARTESIAN_POINT('Ctrl Pts',(-8.13232532707,-37.2742356128,-7.15483556723));
#76338=CARTESIAN_POINT('Ctrl Pts',(-8.9654395686,-37.2742356128,-6.4061359759));
#76339=CARTESIAN_POINT('Ctrl Pts',(-10.2944051979,-37.2742356128,-4.9247261457));
#76340=CARTESIAN_POINT('Ctrl Pts',(-11.0595201702,-37.2742356128,-3.0374430354));
#76341=CARTESIAN_POINT('Ctrl Pts',(-11.2122743937,-37.2742356128,-2.16854923298));
#76342=CARTESIAN_POINT('Ctrl Pts',(-11.2441303156,-37.2742356128,-1.03705260495));
#76343=CARTESIAN_POINT('Ctrl Pts',(-11.1482748814,-37.2742356128,0.0384368560119));
#76344=CARTESIAN_POINT('Ctrl Pts',(-11.1189319926,-37.2742356128,0.295374077233));
#76345=CARTESIAN_POINT('Ctrl Pts',(-11.0845422068,-37.2742356128,0.548794015622));
#76346=CARTESIAN_POINT('Ctrl Pts',(-11.0450673741,-37.2742356128,0.800650704934));
#76347=CARTESIAN_POINT('',(-1.38699292008,-38.2742356128,-10.1328356959));
#76348=CARTESIAN_POINT('Ctrl Pts',(-1.38699292007981,-38.2742356128,-10.1328356958986));
#76349=CARTESIAN_POINT('Ctrl Pts',(-1.5965448998,-38.2742356128,-10.1034873192));
#76350=CARTESIAN_POINT('Ctrl Pts',(-1.7801692912,-38.2742356128,-10.0769073631));
#76351=CARTESIAN_POINT('Ctrl Pts',(-1.93876160799,-38.2742356128,-10.0526765385));
#76352=CARTESIAN_POINT('Ctrl Pts',(-2.99097855121,-38.2742356128,-9.87862177772));
#76353=CARTESIAN_POINT('Ctrl Pts',(-4.02327852642,-38.2742356128,-9.59280526012));
#76354=CARTESIAN_POINT('Ctrl Pts',(-4.87817843107,-38.2742356128,-9.25578182833));
#76355=CARTESIAN_POINT('Ctrl Pts',(-6.60543506376,-38.2742356128,-8.36113191267));
#76356=CARTESIAN_POINT('Ctrl Pts',(-8.13232532707,-38.2742356128,-7.15483556723));
#76357=CARTESIAN_POINT('Ctrl Pts',(-8.9654395686,-38.2742356128,-6.4061359759));
#76358=CARTESIAN_POINT('Ctrl Pts',(-10.2944051979,-38.2742356128,-4.9247261457));
#76359=CARTESIAN_POINT('Ctrl Pts',(-11.0595201702,-38.2742356128,-3.0374430354));
#76360=CARTESIAN_POINT('Ctrl Pts',(-11.2122743937,-38.2742356128,-2.16854923298));
#76361=CARTESIAN_POINT('Ctrl Pts',(-11.2441303156,-38.2742356128,-1.03705260495));
#76362=CARTESIAN_POINT('Ctrl Pts',(-11.1482748814,-38.2742356128,0.0384368560119));
#76363=CARTESIAN_POINT('Ctrl Pts',(-11.1189319926,-38.2742356128,0.295374077233));
#76364=CARTESIAN_POINT('Ctrl Pts',(-11.0845422068,-38.2742356128,0.548794015622));
#76365=CARTESIAN_POINT('Ctrl Pts',(-11.0450673741,-38.2742356128,0.800650704934));
#76366=CARTESIAN_POINT('',(-1.38699292008,-37.6642356128,-10.1328356959));
#76367=CARTESIAN_POINT('Origin',(1.35447209004E-14,-38.2742356128,-0.229490269211));
#76368=CARTESIAN_POINT('',(1.3869929218376,-37.2742356128,-10.132835695642));
#76369=CARTESIAN_POINT('Origin',(1.35447209004E-14,-37.2742356128,-0.229490269211));
#76370=CARTESIAN_POINT('',(1.38699292008,-38.2742356128,-10.1328356959));
#76371=CARTESIAN_POINT('Origin',(1.35447209004E-14,-38.2742356128,-0.229490269211));
#76372=CARTESIAN_POINT('',(1.38699292008,-38.2742356128,-10.1328356959));
#76373=CARTESIAN_POINT('Ctrl Pts',(1.38699292007,-38.2742356128,-10.1328356959));
#76374=CARTESIAN_POINT('Ctrl Pts',(1.38699292007,-37.0742356128,-10.1328356959));
#76375=CARTESIAN_POINT('Ctrl Pts',(1.5965448998,-38.2742356128,-10.1034873192));
#76376=CARTESIAN_POINT('Ctrl Pts',(1.5965448998,-37.0742356128,-10.1034873192));
#76377=CARTESIAN_POINT('Ctrl Pts',(1.7801692912,-38.2742356128,-10.0769073631));
#76378=CARTESIAN_POINT('Ctrl Pts',(1.7801692912,-37.0742356128,-10.0769073631));
#76379=CARTESIAN_POINT('Ctrl Pts',(1.93876160799,-38.2742356128,-10.0526765385));
#76380=CARTESIAN_POINT('Ctrl Pts',(1.93876160799,-37.0742356128,-10.0526765385));
#76381=CARTESIAN_POINT('Ctrl Pts',(2.99097855121,-38.2742356128,-9.87862177772));
#76382=CARTESIAN_POINT('Ctrl Pts',(2.99097855121,-37.0742356128,-9.87862177772));
#76383=CARTESIAN_POINT('Ctrl Pts',(4.02327852642,-38.2742356128,-9.59280526012));
#76384=CARTESIAN_POINT('Ctrl Pts',(4.02327852642,-37.0742356128,-9.59280526012));
#76385=CARTESIAN_POINT('Ctrl Pts',(4.87817843107,-38.2742356128,-9.25578182833));
#76386=CARTESIAN_POINT('Ctrl Pts',(4.87817843107,-37.0742356128,-9.25578182833));
#76387=CARTESIAN_POINT('Ctrl Pts',(6.60543506376,-38.2742356128,-8.36113191267));
#76388=CARTESIAN_POINT('Ctrl Pts',(6.60543506376,-37.0742356128,-8.36113191267));
#76389=CARTESIAN_POINT('Ctrl Pts',(8.13232532707,-38.2742356128,-7.15483556723));
#76390=CARTESIAN_POINT('Ctrl Pts',(8.13232532707,-37.0742356128,-7.15483556723));
#76391=CARTESIAN_POINT('Ctrl Pts',(8.9654395686,-38.2742356128,-6.4061359759));
#76392=CARTESIAN_POINT('Ctrl Pts',(8.9654395686,-37.0742356128,-6.4061359759));
#76393=CARTESIAN_POINT('Ctrl Pts',(10.2944051979,-38.2742356128,-4.9247261457));
#76394=CARTESIAN_POINT('Ctrl Pts',(10.2944051979,-37.0742356128,-4.9247261457));
#76395=CARTESIAN_POINT('Ctrl Pts',(11.0595201702,-38.2742356128,-3.0374430354));
#76396=CARTESIAN_POINT('Ctrl Pts',(11.0595201702,-37.0742356128,-3.0374430354));
#76397=CARTESIAN_POINT('Ctrl Pts',(11.2122743937,-38.2742356128,-2.16854923298));
#76398=CARTESIAN_POINT('Ctrl Pts',(11.2122743937,-37.0742356128,-2.16854923298));
#76399=CARTESIAN_POINT('Ctrl Pts',(11.2441303156,-38.2742356128,-1.03705260495));
#76400=CARTESIAN_POINT('Ctrl Pts',(11.2441303156,-37.0742356128,-1.03705260495));
#76401=CARTESIAN_POINT('Ctrl Pts',(11.1482748814,-38.2742356128,0.0384368560119));
#76402=CARTESIAN_POINT('Ctrl Pts',(11.1482748814,-37.0742356128,0.0384368560119));
#76403=CARTESIAN_POINT('Ctrl Pts',(11.1189319926,-38.2742356128,0.295374077233));
#76404=CARTESIAN_POINT('Ctrl Pts',(11.1189319926,-37.0742356128,0.295374077233));
#76405=CARTESIAN_POINT('Ctrl Pts',(11.0845422068,-38.2742356128,0.548794015622));
#76406=CARTESIAN_POINT('Ctrl Pts',(11.0845422068,-37.0742356128,0.548794015622));
#76407=CARTESIAN_POINT('Ctrl Pts',(11.0450673741,-38.2742356128,0.800650704934));
#76408=CARTESIAN_POINT('Ctrl Pts',(11.0450673741,-37.0742356128,0.800650704934));
#76409=CARTESIAN_POINT('',(11.0450673741,-38.2742356128,0.800650704934));
#76410=CARTESIAN_POINT('',(11.0450673741,-37.2742356128,0.800650704934));
#76411=CARTESIAN_POINT('',(11.0450673741,-37.6642356128,0.800650704934));
#76412=CARTESIAN_POINT('Ctrl Pts',(1.38699292183902,-37.2742356128,-10.1328356956522));
#76413=CARTESIAN_POINT('Ctrl Pts',(1.59654490104011,-37.2742356128,-10.1034873190205));
#76414=CARTESIAN_POINT('Ctrl Pts',(1.78016929200329,-37.2742356128,-10.0769073629773));
#76415=CARTESIAN_POINT('Ctrl Pts',(1.93876160846405,-37.2742356128,-10.0526765384216));
#76416=CARTESIAN_POINT('Ctrl Pts',(2.99097855144254,-37.2742356128,-9.87862177765562));
#76417=CARTESIAN_POINT('Ctrl Pts',(4.02327852642,-37.2742356128,-9.59280526012));
#76418=CARTESIAN_POINT('Ctrl Pts',(4.87817843107,-37.2742356128,-9.25578182833));
#76419=CARTESIAN_POINT('Ctrl Pts',(6.60543506376,-37.2742356128,-8.36113191267));
#76420=CARTESIAN_POINT('Ctrl Pts',(8.13232532707,-37.2742356128,-7.15483556723));
#76421=CARTESIAN_POINT('Ctrl Pts',(8.9654395686,-37.2742356128,-6.4061359759));
#76422=CARTESIAN_POINT('Ctrl Pts',(10.2944051979,-37.2742356128,-4.9247261457));
#76423=CARTESIAN_POINT('Ctrl Pts',(11.0595201702,-37.2742356128,-3.0374430354));
#76424=CARTESIAN_POINT('Ctrl Pts',(11.2122743937,-37.2742356128,-2.16854923298));
#76425=CARTESIAN_POINT('Ctrl Pts',(11.2441303156,-37.2742356128,-1.03705260495));
#76426=CARTESIAN_POINT('Ctrl Pts',(11.1482748814,-37.2742356128,0.0384368560119));
#76427=CARTESIAN_POINT('Ctrl Pts',(11.1189319926,-37.2742356128,0.295374077233));
#76428=CARTESIAN_POINT('Ctrl Pts',(11.0845422068,-37.2742356128,0.548794015622));
#76429=CARTESIAN_POINT('Ctrl Pts',(11.0450673741,-37.2742356128,0.800650704934));
#76430=CARTESIAN_POINT('Ctrl Pts',(1.38699292008,-38.2742356128,-10.1328356959));
#76431=CARTESIAN_POINT('Ctrl Pts',(1.5965448998,-38.2742356128,-10.1034873192));
#76432=CARTESIAN_POINT('Ctrl Pts',(1.7801692912,-38.2742356128,-10.0769073631));
#76433=CARTESIAN_POINT('Ctrl Pts',(1.93876160799,-38.2742356128,-10.0526765385));
#76434=CARTESIAN_POINT('Ctrl Pts',(2.99097855121,-38.2742356128,-9.87862177772));
#76435=CARTESIAN_POINT('Ctrl Pts',(4.02327852642,-38.2742356128,-9.59280526012));
#76436=CARTESIAN_POINT('Ctrl Pts',(4.87817843107,-38.2742356128,-9.25578182833));
#76437=CARTESIAN_POINT('Ctrl Pts',(6.60543506376,-38.2742356128,-8.36113191267));
#76438=CARTESIAN_POINT('Ctrl Pts',(8.13232532707,-38.2742356128,-7.15483556723));
#76439=CARTESIAN_POINT('Ctrl Pts',(8.9654395686,-38.2742356128,-6.4061359759));
#76440=CARTESIAN_POINT('Ctrl Pts',(10.2944051979,-38.2742356128,-4.9247261457));
#76441=CARTESIAN_POINT('Ctrl Pts',(11.0595201702,-38.2742356128,-3.0374430354));
#76442=CARTESIAN_POINT('Ctrl Pts',(11.2122743937,-38.2742356128,-2.16854923298));
#76443=CARTESIAN_POINT('Ctrl Pts',(11.2441303156,-38.2742356128,-1.03705260495));
#76444=CARTESIAN_POINT('Ctrl Pts',(11.1482748814,-38.2742356128,0.0384368560119));
#76445=CARTESIAN_POINT('Ctrl Pts',(11.1189319926,-38.2742356128,0.295374077233));
#76446=CARTESIAN_POINT('Ctrl Pts',(11.0845422068,-38.2742356128,0.548794015622));
#76447=CARTESIAN_POINT('Ctrl Pts',(11.0450673741,-38.2742356128,0.800650704934));
#76448=CARTESIAN_POINT('Ctrl Pts',(10.3257952821,-38.2742356128,3.01322822759));
#76449=CARTESIAN_POINT('Ctrl Pts',(10.3257952821,-37.0742356128,3.01322822759));
#76450=CARTESIAN_POINT('Ctrl Pts',(10.3936895385,-38.2742356128,2.90198771249));
#76451=CARTESIAN_POINT('Ctrl Pts',(10.3936895385,-37.0742356128,2.90198771249));
#76452=CARTESIAN_POINT('Ctrl Pts',(10.4633847104,-38.2742356128,2.78112368582));
#76453=CARTESIAN_POINT('Ctrl Pts',(10.4633847104,-37.0742356128,2.78112368582));
#76454=CARTESIAN_POINT('Ctrl Pts',(10.529369928,-38.2742356128,2.6551197645));
#76455=CARTESIAN_POINT('Ctrl Pts',(10.529369928,-37.0742356128,2.6551197645));
#76456=CARTESIAN_POINT('Ctrl Pts',(10.7481461165,-38.2742356128,2.18905363863));
#76457=CARTESIAN_POINT('Ctrl Pts',(10.7481461165,-37.0742356128,2.18905363863));
#76458=CARTESIAN_POINT('Ctrl Pts',(10.8940097918,-38.2742356128,1.69832265276));
#76459=CARTESIAN_POINT('Ctrl Pts',(10.8940097918,-37.0742356128,1.69832265276));
#76460=CARTESIAN_POINT('Ctrl Pts',(10.9488467638,-38.2742356128,1.36851337106));
#76461=CARTESIAN_POINT('Ctrl Pts',(10.9488467638,-37.0742356128,1.36851337106));
#76462=CARTESIAN_POINT('Ctrl Pts',(10.9986655796,-38.2742356128,1.09670268406));
#76463=CARTESIAN_POINT('Ctrl Pts',(10.9986655796,-37.0742356128,1.09670268406));
#76464=CARTESIAN_POINT('Ctrl Pts',(11.0450673741,-38.2742356128,0.800650704934));
#76465=CARTESIAN_POINT('Ctrl Pts',(11.0450673741,-37.0742356128,0.800650704934));
#76466=CARTESIAN_POINT('',(10.3257952821,-37.2742356128,3.01322822759));
#76467=CARTESIAN_POINT('Ctrl Pts',(10.3257952821,-37.2742356128,3.01322822759));
#76468=CARTESIAN_POINT('Ctrl Pts',(10.3936895385,-37.2742356128,2.90198771249));
#76469=CARTESIAN_POINT('Ctrl Pts',(10.4633847104,-37.2742356128,2.78112368582));
#76470=CARTESIAN_POINT('Ctrl Pts',(10.529369928,-37.2742356128,2.6551197645));
#76471=CARTESIAN_POINT('Ctrl Pts',(10.7481461165,-37.2742356128,2.18905363863));
#76472=CARTESIAN_POINT('Ctrl Pts',(10.8940097918,-37.2742356128,1.69832265276));
#76473=CARTESIAN_POINT('Ctrl Pts',(10.9488467638,-37.2742356128,1.36851337106));
#76474=CARTESIAN_POINT('Ctrl Pts',(10.9986655796,-37.2742356128,1.09670268406));
#76475=CARTESIAN_POINT('Ctrl Pts',(11.0450673741,-37.2742356128,0.800650704934));
#76476=CARTESIAN_POINT('',(10.3257952821,-38.2742356128,3.01322822759));
#76477=CARTESIAN_POINT('Ctrl Pts',(10.3257952821,-38.2742356128,3.01322822759));
#76478=CARTESIAN_POINT('Ctrl Pts',(10.3936895385,-38.2742356128,2.90198771249));
#76479=CARTESIAN_POINT('Ctrl Pts',(10.4633847104,-38.2742356128,2.78112368582));
#76480=CARTESIAN_POINT('Ctrl Pts',(10.529369928,-38.2742356128,2.6551197645));
#76481=CARTESIAN_POINT('Ctrl Pts',(10.7481461165,-38.2742356128,2.18905363863));
#76482=CARTESIAN_POINT('Ctrl Pts',(10.8940097918,-38.2742356128,1.69832265276));
#76483=CARTESIAN_POINT('Ctrl Pts',(10.9488467638,-38.2742356128,1.36851337106));
#76484=CARTESIAN_POINT('Ctrl Pts',(10.9986655796,-38.2742356128,1.09670268406));
#76485=CARTESIAN_POINT('Ctrl Pts',(11.0450673741,-38.2742356128,0.800650704934));
#76486=CARTESIAN_POINT('',(10.3257952821,-37.6642356128,3.01322822759));
#76487=CARTESIAN_POINT('Ctrl Pts',(10.3257952821,-38.2742356128,3.01322822759));
#76488=CARTESIAN_POINT('Ctrl Pts',(10.3257952821,-37.0742356128,3.01322822759));
#76489=CARTESIAN_POINT('Ctrl Pts',(10.1889067725,-38.2742356128,3.23751153419));
#76490=CARTESIAN_POINT('Ctrl Pts',(10.1889067725,-37.0742356128,3.23751153419));
#76491=CARTESIAN_POINT('Ctrl Pts',(10.0345376971,-38.2742356128,3.46376526851));
#76492=CARTESIAN_POINT('Ctrl Pts',(10.0345376971,-37.0742356128,3.46376526851));
#76493=CARTESIAN_POINT('Ctrl Pts',(9.84518696085,-38.2742356128,3.7116414664));
#76494=CARTESIAN_POINT('Ctrl Pts',(9.84518696085,-37.0742356128,3.7116414664));
#76495=CARTESIAN_POINT('Ctrl Pts',(9.43247784233,-38.2742356128,4.11040580001));
#76496=CARTESIAN_POINT('Ctrl Pts',(9.43247784233,-37.0742356128,4.11040580001));
#76497=CARTESIAN_POINT('Ctrl Pts',(8.89477751089,-38.2742356128,4.39069936375));
#76498=CARTESIAN_POINT('Ctrl Pts',(8.89477751089,-37.0742356128,4.39069936375));
#76499=CARTESIAN_POINT('Ctrl Pts',(8.65375386005,-38.2742356128,4.47753838835));
#76500=CARTESIAN_POINT('Ctrl Pts',(8.65375386005,-37.0742356128,4.47753838835));
#76501=CARTESIAN_POINT('Ctrl Pts',(8.18724170147,-38.2742356128,4.57349385703));
#76502=CARTESIAN_POINT('Ctrl Pts',(8.18724170147,-37.0742356128,4.57349385703));
#76503=CARTESIAN_POINT('Ctrl Pts',(7.71488023342,-38.2742356128,4.54915455659));
#76504=CARTESIAN_POINT('Ctrl Pts',(7.71488023342,-37.0742356128,4.54915455659));
#76505=CARTESIAN_POINT('Ctrl Pts',(7.50094363126,-38.2742356128,4.51252661069));
#76506=CARTESIAN_POINT('Ctrl Pts',(7.50094363126,-37.0742356128,4.51252661069));
#76507=CARTESIAN_POINT('Ctrl Pts',(7.18780951373,-38.2742356128,4.42164672508));
#76508=CARTESIAN_POINT('Ctrl Pts',(7.18780951373,-37.0742356128,4.42164672508));
#76509=CARTESIAN_POINT('Ctrl Pts',(6.90087465334,-38.2742356128,4.28688202824));
#76510=CARTESIAN_POINT('Ctrl Pts',(6.90087465334,-37.0742356128,4.28688202824));
#76511=CARTESIAN_POINT('Ctrl Pts',(6.80533495241,-38.2742356128,4.23572805208));
#76512=CARTESIAN_POINT('Ctrl Pts',(6.80533495241,-37.0742356128,4.23572805208));
#76513=CARTESIAN_POINT('Ctrl Pts',(6.71329436634,-38.2742356128,4.1803921541));
#76514=CARTESIAN_POINT('Ctrl Pts',(6.71329436634,-37.0742356128,4.1803921541));
#76515=CARTESIAN_POINT('Ctrl Pts',(6.62478636278,-38.2742356128,4.12129363314));
#76516=CARTESIAN_POINT('Ctrl Pts',(6.62478636278,-37.0742356128,4.12129363314));
#76517=CARTESIAN_POINT('',(6.62478636278,-38.2742356128,4.12129363314));
#76518=CARTESIAN_POINT('',(6.62478636305302,-37.2742356128,4.12129363273029));
#76519=CARTESIAN_POINT('',(6.62478636278,-37.6642356128,4.12129363314));
#76520=CARTESIAN_POINT('Ctrl Pts',(10.3257952821,-37.2742356128,3.01322822759));
#76521=CARTESIAN_POINT('Ctrl Pts',(10.1889067725,-37.2742356128,3.23751153419));
#76522=CARTESIAN_POINT('Ctrl Pts',(10.0345376971,-37.2742356128,3.46376526851));
#76523=CARTESIAN_POINT('Ctrl Pts',(9.84518696085,-37.2742356128,3.7116414664));
#76524=CARTESIAN_POINT('Ctrl Pts',(9.43247784233,-37.2742356128,4.11040580001));
#76525=CARTESIAN_POINT('Ctrl Pts',(8.89477751089,-37.2742356128,4.39069936375));
#76526=CARTESIAN_POINT('Ctrl Pts',(8.65375386005,-37.2742356128,4.47753838835));
#76527=CARTESIAN_POINT('Ctrl Pts',(8.18724170147,-37.2742356128,4.57349385703));
#76528=CARTESIAN_POINT('Ctrl Pts',(7.71488023342,-37.2742356128,4.54915455659));
#76529=CARTESIAN_POINT('Ctrl Pts',(7.50094363126,-37.2742356128,4.51252661069));
#76530=CARTESIAN_POINT('Ctrl Pts',(7.18780951373,-37.2742356128,4.42164672508));
#76531=CARTESIAN_POINT('Ctrl Pts',(6.90087465334,-37.2742356128,4.28688202824));
#76532=CARTESIAN_POINT('Ctrl Pts',(6.80533495241,-37.2742356128,4.23572805208));
#76533=CARTESIAN_POINT('Ctrl Pts',(6.71329436634,-37.2742356128,4.1803921541));
#76534=CARTESIAN_POINT('Ctrl Pts',(6.62478636278,-37.2742356128,4.12129363314));
#76535=CARTESIAN_POINT('Ctrl Pts',(10.3257952821,-38.2742356128,3.01322822759));
#76536=CARTESIAN_POINT('Ctrl Pts',(10.1889067725,-38.2742356128,3.23751153419));
#76537=CARTESIAN_POINT('Ctrl Pts',(10.0345376971,-38.2742356128,3.46376526851));
#76538=CARTESIAN_POINT('Ctrl Pts',(9.84518696085,-38.2742356128,3.7116414664));
#76539=CARTESIAN_POINT('Ctrl Pts',(9.43247784233,-38.2742356128,4.11040580001));
#76540=CARTESIAN_POINT('Ctrl Pts',(8.89477751089,-38.2742356128,4.39069936375));
#76541=CARTESIAN_POINT('Ctrl Pts',(8.65375386005,-38.2742356128,4.47753838835));
#76542=CARTESIAN_POINT('Ctrl Pts',(8.18724170147,-38.2742356128,4.57349385703));
#76543=CARTESIAN_POINT('Ctrl Pts',(7.71488023342,-38.2742356128,4.54915455659));
#76544=CARTESIAN_POINT('Ctrl Pts',(7.50094363126,-38.2742356128,4.51252661069));
#76545=CARTESIAN_POINT('Ctrl Pts',(7.18780951373,-38.2742356128,4.42164672508));
#76546=CARTESIAN_POINT('Ctrl Pts',(6.90087465334,-38.2742356128,4.28688202824));
#76547=CARTESIAN_POINT('Ctrl Pts',(6.80533495241,-38.2742356128,4.23572805208));
#76548=CARTESIAN_POINT('Ctrl Pts',(6.71329436634,-38.2742356128,4.1803921541));
#76549=CARTESIAN_POINT('Ctrl Pts',(6.62478636278,-38.2742356128,4.12129363314));
#76550=CARTESIAN_POINT('Origin',(6.45819449379,-38.2742356128,4.370787419));
#76551=CARTESIAN_POINT('',(6.16208308783,-38.2742356128,4.4189333977));
#76552=CARTESIAN_POINT('',(6.16208308783,-37.2742356128,4.4189333977));
#76553=CARTESIAN_POINT('',(6.16208308783,-38.2742356128,4.4189333977));
#76554=CARTESIAN_POINT('Origin',(6.45819449379,-37.2742356128,4.370787419));
#76555=CARTESIAN_POINT('Origin',(6.45819449379,-38.2742356128,4.370787419));
#76556=CARTESIAN_POINT('Origin',(-0.000416107150126,-37.6642356128,5.42091963994));
#76557=CARTESIAN_POINT('Origin',(-0.000416107150126,-37.2742356128,5.42091963994));
#76558=CARTESIAN_POINT('Origin',(-0.000416107150126,-38.2742356128,5.42091963994));
#76559=CARTESIAN_POINT('Origin',(-3.35265884719E-30,-39.7742356128,3.15283103411E-22));
#76560=CARTESIAN_POINT('',(-9.36455599938E-5,-39.7742356128,10.8643459797));
#76561=CARTESIAN_POINT('Origin',(0.0108494330597224,-39.7742356128,5.39376217080941));
#76562=CARTESIAN_POINT('Origin',(-0.0118852773128557,-39.7742356128,5.39166608075836));
#76563=CARTESIAN_POINT('Origin',(-3.35265884719E-30,-39.7742356128,3.15283103411E-22));
#76564=CARTESIAN_POINT('',(-4.44050669832,-39.7742356128,5.57005878528));
#76565=CARTESIAN_POINT('Ctrl Pts',(-4.44050669832,-39.7742356128,5.57005878528));
#76566=CARTESIAN_POINT('Ctrl Pts',(-4.44147453346363,-39.7742356128,5.54123951619091));
#76567=CARTESIAN_POINT('Ctrl Pts',(-4.44231065914721,-39.7742356128,5.51241582391387));
#76568=CARTESIAN_POINT('Ctrl Pts',(-4.44299515202408,-39.7742356128,5.48359182392916));
#76569=CARTESIAN_POINT('Ctrl Pts',(-4.44351074301195,-39.7742356128,5.45477116963976));
#76570=CARTESIAN_POINT('Ctrl Pts',(-4.4438425928504,-39.7742356128,5.42595709132));
#76571=CARTESIAN_POINT('',(3.98812927127E-15,-39.7742356128,9.86434598407));
#76572=CARTESIAN_POINT('Origin',(0.000416107150120569,-39.7742356128,5.42091963994));
#76573=CARTESIAN_POINT('',(4.44050669832,-39.7742356128,5.57005878528));
#76574=CARTESIAN_POINT('Origin',(-0.000416107150128624,-39.7742356128,5.42091963994));
#76575=CARTESIAN_POINT('Ctrl Pts',(4.44050669832,-39.7742356128,5.57005878528));
#76576=CARTESIAN_POINT('Ctrl Pts',(4.44147453346363,-39.7742356128,5.54123951619091));
#76577=CARTESIAN_POINT('Ctrl Pts',(4.44231065914721,-39.7742356128,5.51241582391387));
#76578=CARTESIAN_POINT('Ctrl Pts',(4.44299515202408,-39.7742356128,5.48359182392916));
#76579=CARTESIAN_POINT('Ctrl Pts',(4.44351074301195,-39.7742356128,5.45477116963976));
#76580=CARTESIAN_POINT('Ctrl Pts',(4.4438425928504,-39.7742356128,5.42595709132));
#76581=CARTESIAN_POINT('Origin',(-3.35265884719E-30,-39.7742356128,3.15283103411E-22));
#76582=CARTESIAN_POINT('Ctrl Pts',(4.44384282525284,-39.7742356128,5.30375137006997));
#76583=CARTESIAN_POINT('Ctrl Pts',(4.43847639264561,-39.7742356128,4.86276818888142));
#76584=CARTESIAN_POINT('Ctrl Pts',(4.3822968816921,-39.7742356128,4.42505108085605));
#76585=CARTESIAN_POINT('Ctrl Pts',(4.23617161309801,-39.7742356128,3.99973909354992));
#76586=CARTESIAN_POINT('Ctrl Pts',(4.084425172493,-39.7742356128,3.57446610480042));
#76587=CARTESIAN_POINT('Ctrl Pts',(3.94523376325647,-39.7742356128,3.14826407381826));
#76588=CARTESIAN_POINT('Ctrl Pts',(4.44050669832,-39.7742356128,5.57005878528));
#76589=CARTESIAN_POINT('Ctrl Pts',(4.44050669832,-36.7742356128,5.57005878528));
#76590=CARTESIAN_POINT('Ctrl Pts',(4.46448048797,-39.7742356128,4.85619021008));
#76591=CARTESIAN_POINT('Ctrl Pts',(4.46448048797,-36.7742356128,4.85619021008));
#76592=CARTESIAN_POINT('Ctrl Pts',(4.40764009695,-39.7742356128,4.1396076589));
#76593=CARTESIAN_POINT('Ctrl Pts',(4.40764009695,-36.7742356128,4.1396076589));
#76594=CARTESIAN_POINT('Ctrl Pts',(3.96717692929,-39.7742356128,3.48286100495));
#76595=CARTESIAN_POINT('Ctrl Pts',(3.96717692929,-36.7742356128,3.48286100495));
#76596=CARTESIAN_POINT('Ctrl Pts',(3.83955824331,-39.7742356128,2.77453753392));
#76597=CARTESIAN_POINT('Ctrl Pts',(3.83955824331,-36.7742356128,2.77453753392));
#76598=CARTESIAN_POINT('Ctrl Pts',(3.62746705121,-39.7742356128,2.09248151608));
#76599=CARTESIAN_POINT('Ctrl Pts',(3.62746705121,-36.7742356128,2.09248151608));
#76600=CARTESIAN_POINT('',(4.44050669832,-37.2742356128,5.57005878528));
#76601=CARTESIAN_POINT('',(3.62746705121,-37.2742356128,2.09248151608));
#76602=CARTESIAN_POINT('Ctrl Pts',(4.44050669832,-37.2742356128,5.57005878528));
#76603=CARTESIAN_POINT('Ctrl Pts',(4.46448048797,-37.2742356128,4.85619021008));
#76604=CARTESIAN_POINT('Ctrl Pts',(4.40764009695,-37.2742356128,4.1396076589));
#76605=CARTESIAN_POINT('Ctrl Pts',(3.96717692929,-37.2742356128,3.48286100495));
#76606=CARTESIAN_POINT('Ctrl Pts',(3.83955824331,-37.2742356128,2.77453753392));
#76607=CARTESIAN_POINT('Ctrl Pts',(3.62746705121,-37.2742356128,2.09248151608));
#76608=CARTESIAN_POINT('',(3.62746705121,-39.7742356128,2.09248151608));
#76609=CARTESIAN_POINT('',(3.62746705121,-39.6642356128,2.09248151608));
#76610=CARTESIAN_POINT('Ctrl Pts',(3.94523376325647,-39.7742356128,3.14826407381826));
#76611=CARTESIAN_POINT('Ctrl Pts',(3.87620988630884,-39.7742356128,2.93691398617489));
#76612=CARTESIAN_POINT('Ctrl Pts',(3.81027340038231,-39.7742356128,2.72533543899502));
#76613=CARTESIAN_POINT('Ctrl Pts',(3.74964078603135,-39.7742356128,2.5134103854269));
#76614=CARTESIAN_POINT('Ctrl Pts',(3.69252846020896,-39.7742356128,2.30171003282089));
#76615=CARTESIAN_POINT('Ctrl Pts',(3.62746705121,-39.7742356128,2.09248151608));
#76616=CARTESIAN_POINT('',(4.44050669832,-39.6642356128,5.57005878528));
#76617=CARTESIAN_POINT('Origin',(-3.35265884719E-30,-39.7742356128,3.15283103411E-22));
#76618=CARTESIAN_POINT('',(0.772076508426,-39.7742356128,-1.09035382089));
#76619=CARTESIAN_POINT('Ctrl Pts',(0.772076508426,-39.7742356128,-1.09035382089));
#76620=CARTESIAN_POINT('Ctrl Pts',(0.886178610516,-39.7742356128,-1.05996501737));
#76621=CARTESIAN_POINT('Ctrl Pts',(0.999471783383,-39.7742356128,-1.02648938573));
#76622=CARTESIAN_POINT('Ctrl Pts',(1.28376436686776,-39.7742356128,-0.933262719920861));
#76623=CARTESIAN_POINT('Ctrl Pts',(1.55846384573443,-39.7742356128,-0.816903495533422));
#76624=CARTESIAN_POINT('Ctrl Pts',(1.99336348977486,-39.7742356128,-0.570669430159104));
#76625=CARTESIAN_POINT('Ctrl Pts',(2.3976244972855,-39.7742356128,-0.230794401633491));
#76626=CARTESIAN_POINT('Ctrl Pts',(2.71790928753969,-39.7742356128,0.199910378054401));
#76627=CARTESIAN_POINT('Ctrl Pts',(3.04613205154736,-39.7742356128,0.706586155851523));
#76628=CARTESIAN_POINT('Ctrl Pts',(3.3135563642201,-39.7742356128,1.24160867153818));
#76629=CARTESIAN_POINT('Ctrl Pts',(3.46527948246,-39.7742356128,1.60915269898));
#76630=CARTESIAN_POINT('Ctrl Pts',(3.55147728822,-39.7742356128,1.84810892036));
#76631=CARTESIAN_POINT('Ctrl Pts',(3.62746705121,-39.7742356128,2.09248151608));
#76632=CARTESIAN_POINT('',(-0.772076508426,-39.7742356128,-1.09035382089));
#76633=CARTESIAN_POINT('Origin',(-3.57491813929E-14,-39.7742356128,1.80859389597));
#76634=CARTESIAN_POINT('',(-3.62746705121,-39.7742356128,2.09248151608));
#76635=CARTESIAN_POINT('Ctrl Pts',(-0.772076508424,-39.7742356128,-1.09035382089));
#76636=CARTESIAN_POINT('Ctrl Pts',(-0.886178610516,-39.7742356128,-1.05996501737));
#76637=CARTESIAN_POINT('Ctrl Pts',(-0.999471783383,-39.7742356128,-1.02648938573));
#76638=CARTESIAN_POINT('Ctrl Pts',(-1.11165616418,-39.7742356128,-0.989701314619));
#76639=CARTESIAN_POINT('Ctrl Pts',(-1.3921632233,-39.7742356128,-0.887346335547));
#76640=CARTESIAN_POINT('Ctrl Pts',(-1.65990259641,-39.7742356128,-0.759470300753));
#76641=CARTESIAN_POINT('Ctrl Pts',(-1.81552533939,-39.7742356128,-0.67135889116));
#76642=CARTESIAN_POINT('Ctrl Pts',(-2.13001246648,-39.7742356128,-0.455784308931));
#76643=CARTESIAN_POINT('Ctrl Pts',(-2.40225756964,-39.7742356128,-0.187376365848));
#76644=CARTESIAN_POINT('Ctrl Pts',(-2.53491876149,-39.7742356128,-0.0306790811922));
#76645=CARTESIAN_POINT('Ctrl Pts',(-2.74588721076,-39.7742356128,0.250416153254));
#76646=CARTESIAN_POINT('Ctrl Pts',(-2.93290680803,-39.7742356128,0.545770364295));
#76647=CARTESIAN_POINT('Ctrl Pts',(-3.00715366555,-39.7742356128,0.670355528577));
#76648=CARTESIAN_POINT('Ctrl Pts',(-3.20108514097,-39.7742356128,1.0165930916));
#76649=CARTESIAN_POINT('Ctrl Pts',(-3.36887363395,-39.7742356128,1.37561285195));
#76650=CARTESIAN_POINT('Ctrl Pts',(-3.46527948246,-39.7742356128,1.60915269898));
#76651=CARTESIAN_POINT('Ctrl Pts',(-3.55147728822,-39.7742356128,1.84810892036));
#76652=CARTESIAN_POINT('Ctrl Pts',(-3.62746705121,-39.7742356128,2.09248151608));
#76653=CARTESIAN_POINT('Ctrl Pts',(-3.94523376325647,-39.7742356128,3.14826407381827));
#76654=CARTESIAN_POINT('Ctrl Pts',(-3.87620988630884,-39.7742356128,2.9369139861749));
#76655=CARTESIAN_POINT('Ctrl Pts',(-3.81027340038232,-39.7742356128,2.72533543899502));
#76656=CARTESIAN_POINT('Ctrl Pts',(-3.74964078603135,-39.7742356128,2.5134103854269));
#76657=CARTESIAN_POINT('Ctrl Pts',(-3.69252846020896,-39.7742356128,2.30171003282089));
#76658=CARTESIAN_POINT('Ctrl Pts',(-3.62746705121,-39.7742356128,2.09248151608));
#76659=CARTESIAN_POINT('Origin',(-3.35265884719E-30,-39.7742356128,3.15283103411E-22));
#76660=CARTESIAN_POINT('Ctrl Pts',(-4.44384282525284,-39.7742356128,5.30375137006997));
#76661=CARTESIAN_POINT('Ctrl Pts',(-4.43847639264561,-39.7742356128,4.86276818888142));
#76662=CARTESIAN_POINT('Ctrl Pts',(-4.3822968816921,-39.7742356128,4.42505108085606));
#76663=CARTESIAN_POINT('Ctrl Pts',(-4.23617161309801,-39.7742356128,3.99973909354993));
#76664=CARTESIAN_POINT('Ctrl Pts',(-4.084425172493,-39.7742356128,3.57446610480043));
#76665=CARTESIAN_POINT('Ctrl Pts',(-3.94523376325647,-39.7742356128,3.14826407381827));
#76666=CARTESIAN_POINT('Ctrl Pts',(-4.44050669832,-39.7742356128,5.57005878528));
#76667=CARTESIAN_POINT('Ctrl Pts',(-4.44050669832,-36.7742356128,5.57005878528));
#76668=CARTESIAN_POINT('Ctrl Pts',(-4.46448048797,-39.7742356128,4.85619021008));
#76669=CARTESIAN_POINT('Ctrl Pts',(-4.46448048797,-36.7742356128,4.85619021008));
#76670=CARTESIAN_POINT('Ctrl Pts',(-4.40764009695,-39.7742356128,4.1396076589));
#76671=CARTESIAN_POINT('Ctrl Pts',(-4.40764009695,-36.7742356128,4.1396076589));
#76672=CARTESIAN_POINT('Ctrl Pts',(-3.96717692929,-39.7742356128,3.48286100495));
#76673=CARTESIAN_POINT('Ctrl Pts',(-3.96717692929,-36.7742356128,3.48286100495));
#76674=CARTESIAN_POINT('Ctrl Pts',(-3.83955824331,-39.7742356128,2.77453753392));
#76675=CARTESIAN_POINT('Ctrl Pts',(-3.83955824331,-36.7742356128,2.77453753392));
#76676=CARTESIAN_POINT('Ctrl Pts',(-3.62746705121,-39.7742356128,2.09248151608));
#76677=CARTESIAN_POINT('Ctrl Pts',(-3.62746705121,-36.7742356128,2.09248151608));
#76678=CARTESIAN_POINT('',(-4.44050669832,-37.2742356128,5.57005878528));
#76679=CARTESIAN_POINT('',(-4.44050669832,-39.6642356128,5.57005878528));
#76680=CARTESIAN_POINT('',(-3.62746705121,-37.2742356128,2.09248151608));
#76681=CARTESIAN_POINT('',(-3.62746705121,-39.6642356128,2.09248151608));
#76682=CARTESIAN_POINT('Ctrl Pts',(-4.44050669832,-37.2742356128,5.57005878528));
#76683=CARTESIAN_POINT('Ctrl Pts',(-4.46448048797,-37.2742356128,4.85619021008));
#76684=CARTESIAN_POINT('Ctrl Pts',(-4.40764009695,-37.2742356128,4.1396076589));
#76685=CARTESIAN_POINT('Ctrl Pts',(-3.96717692929,-37.2742356128,3.48286100495));
#76686=CARTESIAN_POINT('Ctrl Pts',(-3.83955824331,-37.2742356128,2.77453753392));
#76687=CARTESIAN_POINT('Ctrl Pts',(-3.62746705121,-37.2742356128,2.09248151608));
#76688=CARTESIAN_POINT('Origin',(-3.35265884719E-30,-39.7742356128,3.15283103411E-22));
#76689=CARTESIAN_POINT('',(3.51985615629,-39.7742356128,-3.20601908088));
#76690=CARTESIAN_POINT('Origin',(-1143.38887689168,-39.774235612772,1093.0893729638));
#76691=CARTESIAN_POINT('',(3.67755401867,-39.7742356128,-3.05915055738));
#76692=CARTESIAN_POINT('Origin',(3.78952269078,-39.7742356128,-3.33747234321));
#76693=CARTESIAN_POINT('Ctrl Pts',(7.04639034878034,-39.7742356128,1.13407180047521));
#76694=CARTESIAN_POINT('Ctrl Pts',(6.98577032985781,-39.7742356128,0.696425342316252));
#76695=CARTESIAN_POINT('Ctrl Pts',(6.89012094467166,-39.7742356128,0.272653387012416));
#76696=CARTESIAN_POINT('Ctrl Pts',(6.75651149488734,-39.7742356128,-0.133493132432014));
#76697=CARTESIAN_POINT('Ctrl Pts',(6.39374256643522,-39.7742356128,-0.93640428199725));
#76698=CARTESIAN_POINT('Ctrl Pts',(5.86106085412,-39.7742356128,-1.62790491519));
#76699=CARTESIAN_POINT('Ctrl Pts',(5.53842443335,-39.7742356128,-1.95360958375));
#76700=CARTESIAN_POINT('Ctrl Pts',(4.98933040959,-39.7742356128,-2.39194593497));
#76701=CARTESIAN_POINT('Ctrl Pts',(4.36273333629,-39.7742356128,-2.74903878258));
#76702=CARTESIAN_POINT('Ctrl Pts',(4.14078300625,-39.7742356128,-2.86156599489));
#76703=CARTESIAN_POINT('Ctrl Pts',(3.91246466012,-39.7742356128,-2.96464616022));
#76704=CARTESIAN_POINT('Ctrl Pts',(3.67755401867,-39.7742356128,-3.05915055738));
#76705=CARTESIAN_POINT('',(3.30432511166,-39.7742356128,-2.13141127128));
#76706=CARTESIAN_POINT('Ctrl Pts',(6.02437852526,-39.7742356128,1.07105719697));
#76707=CARTESIAN_POINT('Ctrl Pts',(5.86422039559,-39.7742356128,0.163050845024));
#76708=CARTESIAN_POINT('Ctrl Pts',(5.51798981241,-39.7742356128,-0.6356582873));
#76709=CARTESIAN_POINT('Ctrl Pts',(4.97390737876,-39.7742356128,-1.26910580103));
#76710=CARTESIAN_POINT('Ctrl Pts',(4.20012016579,-39.7742356128,-1.77103350786));
#76711=CARTESIAN_POINT('Ctrl Pts',(3.30432511166,-39.7742356128,-2.13141127128));
#76712=CARTESIAN_POINT('',(2.62096770799,-39.7742356128,-2.76784153979));
#76713=CARTESIAN_POINT('Origin',(3.57176864033797,-39.7742356128,-3.1036622151543));
#76714=CARTESIAN_POINT('Ctrl Pts',(2.62096770799,-39.7742356128,-2.76784153979));
#76715=CARTESIAN_POINT('Ctrl Pts',(2.48674506753,-39.7742356128,-3.04318924635));
#76716=CARTESIAN_POINT('Ctrl Pts',(2.32123277945,-39.7742356128,-3.28726285739));
#76717=CARTESIAN_POINT('Ctrl Pts',(2.12330703536,-39.7742356128,-3.49933208248));
#76718=CARTESIAN_POINT('Origin',(-3.35265884719E-30,-39.7742356128,3.15283103411E-22));
#76719=CARTESIAN_POINT('Origin',(-3.35265884719E-30,-39.7742356128,3.15283103411E-22));
#76720=CARTESIAN_POINT('',(7.07911993306,-39.7742356128,1.41233341424));
#76721=CARTESIAN_POINT('Ctrl Pts',(7.07911993306,-39.7742356128,1.41233341424));
#76722=CARTESIAN_POINT('Ctrl Pts',(7.07459783011676,-39.7742356128,1.36585334327933));
#76723=CARTESIAN_POINT('Ctrl Pts',(7.06961906998812,-39.7742356128,1.31941671396487));
#76724=CARTESIAN_POINT('Ctrl Pts',(7.05871909787096,-39.7742356128,1.22665564708758));
#76725=CARTESIAN_POINT('Ctrl Pts',(7.05279772717288,-39.7742356128,1.18032989304728));
#76726=CARTESIAN_POINT('Ctrl Pts',(7.04639034822407,-39.7742356128,1.1340717964593));
#76727=CARTESIAN_POINT('',(7.21384189758,-39.7742356128,2.18958432614));
#76728=CARTESIAN_POINT('Ctrl Pts',(7.21384189758,-39.7742356128,2.18958432614));
#76729=CARTESIAN_POINT('Ctrl Pts',(7.13908599018,-39.7742356128,2.05065155888));
#76730=CARTESIAN_POINT('Ctrl Pts',(7.08905059141,-39.7742356128,1.8984189694));
#76731=CARTESIAN_POINT('Ctrl Pts',(7.1053290044,-39.7742356128,1.72681022597));
#76732=CARTESIAN_POINT('Ctrl Pts',(7.09439724612,-39.7742356128,1.56936004643));
#76733=CARTESIAN_POINT('Ctrl Pts',(7.07911993306,-39.7742356128,1.41233341424));
#76734=CARTESIAN_POINT('',(8.75956299023,-39.7742356128,2.0634404101));
#76735=CARTESIAN_POINT('Ctrl Pts',(8.75956299023,-39.7742356128,2.0634404101));
#76736=CARTESIAN_POINT('Ctrl Pts',(8.67258032609,-39.7742356128,2.20595609378));
#76737=CARTESIAN_POINT('Ctrl Pts',(8.57679326147,-39.7742356128,2.34786591099));
#76738=CARTESIAN_POINT('Ctrl Pts',(8.46448329596,-39.7742356128,2.49604426586));
#76739=CARTESIAN_POINT('Ctrl Pts',(8.27825186329,-39.7742356128,2.67220081215));
#76740=CARTESIAN_POINT('Ctrl Pts',(8.05379939761,-39.7742356128,2.74035894609));
#76741=CARTESIAN_POINT('Ctrl Pts',(7.9779370982,-39.7742356128,2.74765496713));
#76742=CARTESIAN_POINT('Ctrl Pts',(7.82203636779,-39.7742356128,2.73225108729));
#76743=CARTESIAN_POINT('Ctrl Pts',(7.67278421879,-39.7742356128,2.66639360485));
#76744=CARTESIAN_POINT('Ctrl Pts',(7.59903734004,-39.7742356128,2.62164000818));
#76745=CARTESIAN_POINT('Ctrl Pts',(7.46503014366,-39.7742356128,2.52047218586));
#76746=CARTESIAN_POINT('Ctrl Pts',(7.35007323494,-39.7742356128,2.39634839519));
#76747=CARTESIAN_POINT('Ctrl Pts',(7.29780025627,-39.7742356128,2.32993852802));
#76748=CARTESIAN_POINT('Ctrl Pts',(7.25230657394,-39.7742356128,2.26107036804));
#76749=CARTESIAN_POINT('Ctrl Pts',(7.21384189758,-39.7742356128,2.18958432614));
#76750=CARTESIAN_POINT('',(9.23698117862,-39.7742356128,0.509886547137));
#76751=CARTESIAN_POINT('Ctrl Pts',(8.75956299023,-39.7742356128,2.0634404101));
#76752=CARTESIAN_POINT('Ctrl Pts',(8.92890465395,-39.7742356128,1.78598462948));
#76753=CARTESIAN_POINT('Ctrl Pts',(9.07290910839,-39.7742356128,1.49306491902));
#76754=CARTESIAN_POINT('Ctrl Pts',(9.12674985892,-39.7742356128,1.15064933619));
#76755=CARTESIAN_POINT('Ctrl Pts',(9.18664865847,-39.7742356128,0.831017278591));
#76756=CARTESIAN_POINT('Ctrl Pts',(9.23698117862,-39.7742356128,0.509886547137));
#76757=CARTESIAN_POINT('Origin',(8.43479356605655,-39.7742356128,0.840596259915162));
#76758=CARTESIAN_POINT('Origin',(-3.35265884719E-30,-39.7742356128,3.15283103411E-22));
#76759=CARTESIAN_POINT('Ctrl Pts',(4.25781969174464,-39.7742356128,-7.49892908854306));
#76760=CARTESIAN_POINT('Ctrl Pts',(4.65322788995043,-39.7742356128,-7.3163913616492));
#76761=CARTESIAN_POINT('Ctrl Pts',(5.03801677004475,-39.7742356128,-7.11164628336145));
#76762=CARTESIAN_POINT('Ctrl Pts',(5.41306173043686,-39.7742356128,-6.88530054623907));
#76763=CARTESIAN_POINT('Ctrl Pts',(6.471884508719,-39.7742356128,-6.17278862552067));
#76764=CARTESIAN_POINT('Ctrl Pts',(7.447100543,-39.7742356128,-5.31497212719));
#76765=CARTESIAN_POINT('Ctrl Pts',(8.1250786803,-39.7742356128,-4.64371494659));
#76766=CARTESIAN_POINT('Ctrl Pts',(8.99226462924,-39.7742356128,-3.46343233105));
#76767=CARTESIAN_POINT('Ctrl Pts',(9.35827765375,-39.7742356128,-2.07942227767));
#76768=CARTESIAN_POINT('Ctrl Pts',(9.40334820731,-39.7742356128,-1.48595469944));
#76769=CARTESIAN_POINT('Ctrl Pts',(9.38742862291538,-39.7742356128,-0.735709765136425));
#76770=CARTESIAN_POINT('Ctrl Pts',(9.30750311921127,-39.7742356128,0.00658879758684674));
#76771=CARTESIAN_POINT('Ctrl Pts',(9.28837293696608,-39.7742356128,0.161032819096423));
#76772=CARTESIAN_POINT('Ctrl Pts',(9.26699040489341,-39.7742356128,0.314888765115395));
#76773=CARTESIAN_POINT('Ctrl Pts',(9.24345636582343,-39.7742356128,0.468150490677146));
#76774=CARTESIAN_POINT('Origin',(-3.35265884719E-30,-39.7742356128,3.15283103411E-22));
#76775=CARTESIAN_POINT('',(1.87043161062015,-39.7742356128,-8.24476960831419));
#76776=CARTESIAN_POINT('Ctrl Pts',(1.87043161102975,-39.7742356128,-8.24476960823859));
#76777=CARTESIAN_POINT('Ctrl Pts',(2.37456097010993,-39.7742356128,-8.15400466703051));
#76778=CARTESIAN_POINT('Ctrl Pts',(2.86812085476427,-39.7742356128,-8.03407528099285));
#76779=CARTESIAN_POINT('Ctrl Pts',(3.34590835694244,-39.7742356128,-7.88493442690442));
#76780=CARTESIAN_POINT('Ctrl Pts',(3.80871374571701,-39.7742356128,-7.70625604558236));
#76781=CARTESIAN_POINT('Ctrl Pts',(4.25781969174463,-39.7742356128,-7.49892908854306));
#76782=CARTESIAN_POINT('',(1.51727342606,-39.7742356128,-7.9495168227));
#76783=CARTESIAN_POINT('Origin',(1.81727342606,-39.7742356128,-7.9495168227));
#76784=CARTESIAN_POINT('',(1.51727342606,-39.7742356128,-5.3088808072));
#76785=CARTESIAN_POINT('',(1.51727342606,-39.7742356128,-6.62919881495));
#76786=CARTESIAN_POINT('',(1.68475792039,-39.7742356128,-5.03973467448));
#76787=CARTESIAN_POINT('Origin',(1.81727342606,-39.7742356128,-5.3088808072));
#76788=CARTESIAN_POINT('Origin',(-4.74165425577699,-39.7742356127985,1.63373408714116));
#76789=CARTESIAN_POINT('Origin',(-3.35265884719E-30,-39.7742356128,3.15283103411E-22));
#76790=CARTESIAN_POINT('Ctrl Pts',(-4.25781969174463,-39.7742356128,-7.49892908854306));
#76791=CARTESIAN_POINT('Ctrl Pts',(-4.65322788995043,-39.7742356128,-7.3163913616492));
#76792=CARTESIAN_POINT('Ctrl Pts',(-5.03801677004475,-39.7742356128,-7.11164628336145));
#76793=CARTESIAN_POINT('Ctrl Pts',(-5.41306173043686,-39.7742356128,-6.88530054623907));
#76794=CARTESIAN_POINT('Ctrl Pts',(-6.471884508719,-39.7742356128,-6.17278862552066));
#76795=CARTESIAN_POINT('Ctrl Pts',(-7.447100543,-39.7742356128,-5.31497212719));
#76796=CARTESIAN_POINT('Ctrl Pts',(-8.1250786803,-39.7742356128,-4.64371494659));
#76797=CARTESIAN_POINT('Ctrl Pts',(-8.99226462924,-39.7742356128,-3.46343233105));
#76798=CARTESIAN_POINT('Ctrl Pts',(-9.35827765375,-39.7742356128,-2.07942227767));
#76799=CARTESIAN_POINT('Ctrl Pts',(-9.40334820731,-39.7742356128,-1.48595469944));
#76800=CARTESIAN_POINT('Ctrl Pts',(-9.38742862291538,-39.7742356128,-0.735709765136425));
#76801=CARTESIAN_POINT('Ctrl Pts',(-9.30750311921127,-39.7742356128,0.00658879758684674));
#76802=CARTESIAN_POINT('Ctrl Pts',(-9.28837293696608,-39.7742356128,0.161032819096423));
#76803=CARTESIAN_POINT('Ctrl Pts',(-9.26699040489341,-39.7742356128,0.314888765115395));
#76804=CARTESIAN_POINT('Ctrl Pts',(-9.24345636582343,-39.7742356128,0.468150490677146));
#76805=CARTESIAN_POINT('Origin',(-3.35265884719E-30,-39.7742356128,3.15283103411E-22));
#76806=CARTESIAN_POINT('',(-1.68475792039,-39.7742356128,-5.03973467448));
#76807=CARTESIAN_POINT('Origin',(4.74165425391462,-39.7742356127985,1.63373408533383));
#76808=CARTESIAN_POINT('',(-1.51727342606,-39.7742356128,-5.3088808072));
#76809=CARTESIAN_POINT('Origin',(-1.81727342606,-39.7742356128,-5.3088808072));
#76810=CARTESIAN_POINT('',(-1.51727342606,-39.7742356128,-7.9495168227));
#76811=CARTESIAN_POINT('',(-1.51727342606,-39.7742356128,-6.62919881495));
#76812=CARTESIAN_POINT('',(-1.87043161062015,-39.7742356128,-8.24476960831419));
#76813=CARTESIAN_POINT('Origin',(-1.81727342606,-39.7742356128,-7.9495168227));
#76814=CARTESIAN_POINT('Ctrl Pts',(-1.87043161102975,-39.7742356128,-8.24476960823859));
#76815=CARTESIAN_POINT('Ctrl Pts',(-2.37456097010993,-39.7742356128,-8.15400466703051));
#76816=CARTESIAN_POINT('Ctrl Pts',(-2.86812085476427,-39.7742356128,-8.03407528099285));
#76817=CARTESIAN_POINT('Ctrl Pts',(-3.34590835694244,-39.7742356128,-7.88493442690443));
#76818=CARTESIAN_POINT('Ctrl Pts',(-3.80871374571701,-39.7742356128,-7.70625604558236));
#76819=CARTESIAN_POINT('Ctrl Pts',(-4.25781969174463,-39.7742356128,-7.49892908854306));
#76820=CARTESIAN_POINT('Origin',(-3.35265884719E-30,-39.7742356128,3.15283103411E-22));
#76821=CARTESIAN_POINT('',(-3.67755401867,-39.7742356128,-3.05915055738));
#76822=CARTESIAN_POINT('Ctrl Pts',(-7.04639034878034,-39.7742356128,1.13407180047521));
#76823=CARTESIAN_POINT('Ctrl Pts',(-6.98577032985781,-39.7742356128,0.696425342316252));
#76824=CARTESIAN_POINT('Ctrl Pts',(-6.89012094467166,-39.7742356128,0.272653387012416));
#76825=CARTESIAN_POINT('Ctrl Pts',(-6.75651149488734,-39.7742356128,-0.133493132432014));
#76826=CARTESIAN_POINT('Ctrl Pts',(-6.39374256643522,-39.7742356128,-0.93640428199725));
#76827=CARTESIAN_POINT('Ctrl Pts',(-5.86106085412,-39.7742356128,-1.62790491519));
#76828=CARTESIAN_POINT('Ctrl Pts',(-5.53842443335,-39.7742356128,-1.95360958375));
#76829=CARTESIAN_POINT('Ctrl Pts',(-4.98933040959,-39.7742356128,-2.39194593497));
#76830=CARTESIAN_POINT('Ctrl Pts',(-4.36273333629,-39.7742356128,-2.74903878258));
#76831=CARTESIAN_POINT('Ctrl Pts',(-4.14078300625,-39.7742356128,-2.86156599489));
#76832=CARTESIAN_POINT('Ctrl Pts',(-3.91246466012,-39.7742356128,-2.96464616022));
#76833=CARTESIAN_POINT('Ctrl Pts',(-3.67755401867,-39.7742356128,-3.05915055738));
#76834=CARTESIAN_POINT('',(-3.51985615629,-39.7742356128,-3.20601908088));
#76835=CARTESIAN_POINT('Origin',(-3.78952269078,-39.7742356128,-3.33747234321));
#76836=CARTESIAN_POINT('Origin',(1143.38887689168,-39.774235612772,1093.0893729638));
#76837=CARTESIAN_POINT('',(-2.62096770799,-39.7742356128,-2.76784153979));
#76838=CARTESIAN_POINT('Ctrl Pts',(-2.62096770799,-39.7742356128,-2.76784153979));
#76839=CARTESIAN_POINT('Ctrl Pts',(-2.48674506753,-39.7742356128,-3.04318924635));
#76840=CARTESIAN_POINT('Ctrl Pts',(-2.32123277945,-39.7742356128,-3.28726285739));
#76841=CARTESIAN_POINT('Ctrl Pts',(-2.12330703536,-39.7742356128,-3.49933208248));
#76842=CARTESIAN_POINT('',(-3.30432511166,-39.7742356128,-2.13141127128));
#76843=CARTESIAN_POINT('Origin',(-3.57176864012569,-39.7742356128,-3.10366221508032));
#76844=CARTESIAN_POINT('Ctrl Pts',(-6.02437852526,-39.7742356128,1.07105719696));
#76845=CARTESIAN_POINT('Ctrl Pts',(-5.86422039559,-39.7742356128,0.163050845024));
#76846=CARTESIAN_POINT('Ctrl Pts',(-5.51798981241,-39.7742356128,-0.635658287301));
#76847=CARTESIAN_POINT('Ctrl Pts',(-4.97390737876,-39.7742356128,-1.26910580103));
#76848=CARTESIAN_POINT('Ctrl Pts',(-4.20012016579,-39.7742356128,-1.77103350786));
#76849=CARTESIAN_POINT('Ctrl Pts',(-3.30432511166,-39.7742356128,-2.13141127128));
#76850=CARTESIAN_POINT('Origin',(-3.35265884719E-30,-39.7742356128,3.15283103411E-22));
#76851=CARTESIAN_POINT('Origin',(-3.35265884719E-30,-39.7742356128,3.15283103411E-22));
#76852=CARTESIAN_POINT('',(-9.23698117862,-39.7742356128,0.509886547152));
#76853=CARTESIAN_POINT('Origin',(-8.43479129614805,-39.7742356128,0.840597206515149));
#76854=CARTESIAN_POINT('',(-8.75956299023,-39.7742356128,2.0634404101));
#76855=CARTESIAN_POINT('Ctrl Pts',(-8.75956299023,-39.7742356128,2.0634404101));
#76856=CARTESIAN_POINT('Ctrl Pts',(-8.92890465395,-39.7742356128,1.78598462948));
#76857=CARTESIAN_POINT('Ctrl Pts',(-9.07290910839,-39.7742356128,1.49306491902));
#76858=CARTESIAN_POINT('Ctrl Pts',(-9.12674985892,-39.7742356128,1.15064933619));
#76859=CARTESIAN_POINT('Ctrl Pts',(-9.18664865847,-39.7742356128,0.831017278591));
#76860=CARTESIAN_POINT('Ctrl Pts',(-9.23698117861771,-39.7742356128,0.509886547151641));
#76861=CARTESIAN_POINT('',(-7.21384189758,-39.7742356128,2.18958432614));
#76862=CARTESIAN_POINT('Ctrl Pts',(-8.75956299024,-39.7742356128,2.0634404101));
#76863=CARTESIAN_POINT('Ctrl Pts',(-8.67258032609,-39.7742356128,2.20595609378));
#76864=CARTESIAN_POINT('Ctrl Pts',(-8.57679326147,-39.7742356128,2.34786591099));
#76865=CARTESIAN_POINT('Ctrl Pts',(-8.46448329596,-39.7742356128,2.49604426586));
#76866=CARTESIAN_POINT('Ctrl Pts',(-8.27825186329,-39.7742356128,2.67220081215));
#76867=CARTESIAN_POINT('Ctrl Pts',(-8.05379939761,-39.7742356128,2.74035894609));
#76868=CARTESIAN_POINT('Ctrl Pts',(-7.9779370982,-39.7742356128,2.74765496713));
#76869=CARTESIAN_POINT('Ctrl Pts',(-7.82203636779,-39.7742356128,2.73225108729));
#76870=CARTESIAN_POINT('Ctrl Pts',(-7.67278421879,-39.7742356128,2.66639360485));
#76871=CARTESIAN_POINT('Ctrl Pts',(-7.59903734004,-39.7742356128,2.62164000818));
#76872=CARTESIAN_POINT('Ctrl Pts',(-7.46503014366,-39.7742356128,2.52047218586));
#76873=CARTESIAN_POINT('Ctrl Pts',(-7.35007323494,-39.7742356128,2.39634839519));
#76874=CARTESIAN_POINT('Ctrl Pts',(-7.29780025627,-39.7742356128,2.32993852802));
#76875=CARTESIAN_POINT('Ctrl Pts',(-7.25230657394,-39.7742356128,2.26107036804));
#76876=CARTESIAN_POINT('Ctrl Pts',(-7.21384189758,-39.7742356128,2.18958432614));
#76877=CARTESIAN_POINT('',(-7.07911993306,-39.7742356128,1.41233341424));
#76878=CARTESIAN_POINT('Ctrl Pts',(-7.21384189758,-39.7742356128,2.18958432614));
#76879=CARTESIAN_POINT('Ctrl Pts',(-7.13908599018,-39.7742356128,2.05065155888));
#76880=CARTESIAN_POINT('Ctrl Pts',(-7.08905059141,-39.7742356128,1.8984189694));
#76881=CARTESIAN_POINT('Ctrl Pts',(-7.1053290044,-39.7742356128,1.72681022597));
#76882=CARTESIAN_POINT('Ctrl Pts',(-7.09439724612,-39.7742356128,1.56936004643));
#76883=CARTESIAN_POINT('Ctrl Pts',(-7.07911993306,-39.7742356128,1.41233341424));
#76884=CARTESIAN_POINT('Ctrl Pts',(-7.07911993306,-39.7742356128,1.41233341424));
#76885=CARTESIAN_POINT('Ctrl Pts',(-7.07459783011678,-39.7742356128,1.36585334327954));
#76886=CARTESIAN_POINT('Ctrl Pts',(-7.06961906998814,-39.7742356128,1.31941671396497));
#76887=CARTESIAN_POINT('Ctrl Pts',(-7.05871909787096,-39.7742356128,1.22665564708761));
#76888=CARTESIAN_POINT('Ctrl Pts',(-7.05279772717288,-39.7742356128,1.18032989304729));
#76889=CARTESIAN_POINT('Ctrl Pts',(-7.04639034822408,-39.7742356128,1.1340717964593));
#76890=CARTESIAN_POINT('Origin',(-3.35265884719E-30,-38.2742356128,3.15283103411E-22));
#76891=CARTESIAN_POINT('',(9.47221976654,-38.2742356128,2.49225909299));
#76892=CARTESIAN_POINT('',(6.53914701908,-38.2742356128,2.5806950957));
#76893=CARTESIAN_POINT('Ctrl Pts',(9.47221976654,-38.2742356128,2.49225909299));
#76894=CARTESIAN_POINT('Ctrl Pts',(9.39947240551,-38.2742356128,2.61145111814));
#76895=CARTESIAN_POINT('Ctrl Pts',(9.32101749845,-38.2742356128,2.73104611971));
#76896=CARTESIAN_POINT('Ctrl Pts',(9.23447554945,-38.2742356128,2.85280836926));
#76897=CARTESIAN_POINT('Ctrl Pts',(9.02906684789,-38.2742356128,3.10681559939));
#76898=CARTESIAN_POINT('Ctrl Pts',(8.75253761634,-38.2742356128,3.33309151087));
#76899=CARTESIAN_POINT('Ctrl Pts',(8.5879953064,-38.2742356128,3.43383230551));
#76900=CARTESIAN_POINT('Ctrl Pts',(8.23034267354,-38.2742356128,3.56436456904));
#76901=CARTESIAN_POINT('Ctrl Pts',(7.84867458413,-38.2742356128,3.56156543232));
#76902=CARTESIAN_POINT('Ctrl Pts',(7.67119781066,-38.2742356128,3.52757441198));
#76903=CARTESIAN_POINT('Ctrl Pts',(7.27066371621,-38.2742356128,3.38466568023));
#76904=CARTESIAN_POINT('Ctrl Pts',(6.95203985001,-38.2742356128,3.13761299508));
#76905=CARTESIAN_POINT('Ctrl Pts',(6.78734156337,-38.2742356128,2.96846990237));
#76906=CARTESIAN_POINT('Ctrl Pts',(6.6484900876,-38.2742356128,2.78390759916));
#76907=CARTESIAN_POINT('Ctrl Pts',(6.53914701908,-38.2742356128,2.5806950957));
#76908=CARTESIAN_POINT('',(2.42434411094,-38.2742356128,-2.36824808793));
#76909=CARTESIAN_POINT('Ctrl Pts',(6.53914701908,-38.2742356128,2.5806950957));
#76910=CARTESIAN_POINT('Ctrl Pts',(5.92921620253,-38.2742356128,1.44714753899));
#76911=CARTESIAN_POINT('Ctrl Pts',(6.2734552887,-38.2742356128,-0.199812643821));
#76912=CARTESIAN_POINT('Ctrl Pts',(4.66846608736,-38.2742356128,-1.09094389297));
#76913=CARTESIAN_POINT('Ctrl Pts',(3.58890539941,-38.2742356128,-1.81984798791));
#76914=CARTESIAN_POINT('Ctrl Pts',(2.42434411094,-38.2742356128,-2.36824808793));
#76915=CARTESIAN_POINT('',(1.11895565834,-38.2742356128,-2.79941259037));
#76916=CARTESIAN_POINT('Origin',(5.88418203051333E-14,-38.2742356128,2.77999550540993));
#76917=CARTESIAN_POINT('',(0.717273426056,-38.2742356128,-3.28965091665));
#76918=CARTESIAN_POINT('Origin',(1.21727342606,-38.2742356128,-3.28965091665));
#76919=CARTESIAN_POINT('',(0.717273426056,-38.2742356128,-7.9495168227));
#76920=CARTESIAN_POINT('',(0.717273426056,-38.2742356128,0.717427860236));
#76921=CARTESIAN_POINT('',(2.02820898725,-38.2742356128,-9.02284995699));
#76922=CARTESIAN_POINT('Origin',(1.81725567298,-38.2742356128,-7.94326730652));
#76923=CARTESIAN_POINT('',(2.06575948168,-38.2742356128,-9.01576047707));
#76924=CARTESIAN_POINT('Origin',(2.60353656354866,-38.2742356128,-11.9671681877212));
#76925=CARTESIAN_POINT('',(10.0571285787,-38.2742356128,0.645805825719));
#76926=CARTESIAN_POINT('Ctrl Pts',(2.06575948168004,-38.2742356128,-9.0157604770702));
#76927=CARTESIAN_POINT('Ctrl Pts',(2.96721946584242,-38.2742356128,-8.8515051248253));
#76928=CARTESIAN_POINT('Ctrl Pts',(3.84599035268564,-38.2742356128,-8.59864711375854));
#76929=CARTESIAN_POINT('Ctrl Pts',(4.67357601907077,-38.2742356128,-8.25401330976187));
#76930=CARTESIAN_POINT('Ctrl Pts',(6.17345275440962,-38.2742356128,-7.42645694768941));
#76931=CARTESIAN_POINT('Ctrl Pts',(7.5161640814,-38.2742356128,-6.34532321195));
#76932=CARTESIAN_POINT('Ctrl Pts',(8.15806093588,-38.2742356128,-5.76170299258));
#76933=CARTESIAN_POINT('Ctrl Pts',(9.14108523272,-38.2742356128,-4.69984607968));
#76934=CARTESIAN_POINT('Ctrl Pts',(9.81302959348,-38.2742356128,-3.42961050122));
#76935=CARTESIAN_POINT('Ctrl Pts',(10.0098671635,-38.2742356128,-2.88411398337));
#76936=CARTESIAN_POINT('Ctrl Pts',(10.222733632,-38.2742356128,-1.82926592992));
#76937=CARTESIAN_POINT('Ctrl Pts',(10.2199521215,-38.2742356128,-0.771812654558));
#76938=CARTESIAN_POINT('Ctrl Pts',(10.184046519,-38.2742356128,-0.287190507733));
#76939=CARTESIAN_POINT('Ctrl Pts',(10.1298079404,-38.2742356128,0.182098137249));
#76940=CARTESIAN_POINT('Ctrl Pts',(10.0571285787022,-38.2742356128,0.645805825719337));
#76941=CARTESIAN_POINT('Ctrl Pts',(9.47221976654,-38.2742356128,2.49225909299));
#76942=CARTESIAN_POINT('Ctrl Pts',(9.54575444005,-38.2742356128,2.3717771053));
#76943=CARTESIAN_POINT('Ctrl Pts',(9.61961951766,-38.2742356128,2.24151541202));
#76944=CARTESIAN_POINT('Ctrl Pts',(9.68609489427,-38.2742356128,2.10542437124));
#76945=CARTESIAN_POINT('Ctrl Pts',(9.84457330898,-38.2742356128,1.72211870919));
#76946=CARTESIAN_POINT('Ctrl Pts',(9.94207621049,-38.2742356128,1.33157301839));
#76947=CARTESIAN_POINT('Ctrl Pts',(9.98299011243,-38.2742356128,1.0898271634));
#76948=CARTESIAN_POINT('Ctrl Pts',(10.0216701384,-38.2742356128,0.872037193625));
#76949=CARTESIAN_POINT('Ctrl Pts',(10.0571285787,-38.2742356128,0.645805825719));
#76950=CARTESIAN_POINT('',(-5.2400559546,-38.2742356128,5.59690998219));
#76951=CARTESIAN_POINT('',(-4.39152711004478,-38.2742356128,1.85538989759538));
#76952=CARTESIAN_POINT('Ctrl Pts',(-5.2400559546,-38.2742356128,5.59690998219));
#76953=CARTESIAN_POINT('Ctrl Pts',(-5.25990082634,-38.2742356128,5.0059883748));
#76954=CARTESIAN_POINT('Ctrl Pts',(-5.23061607717,-38.2742356128,4.36229648927));
#76955=CARTESIAN_POINT('Ctrl Pts',(-5.00490058958,-38.2742356128,3.77298874453));
#76956=CARTESIAN_POINT('Ctrl Pts',(-4.75506448705,-38.2742356128,3.08655684628));
#76957=CARTESIAN_POINT('Ctrl Pts',(-4.54755634075,-38.2742356128,2.39287258614));
#76958=CARTESIAN_POINT('Ctrl Pts',(-4.4987250478,-38.2742356128,2.21955031284));
#76959=CARTESIAN_POINT('Ctrl Pts',(-4.44893332626,-38.2742356128,2.04003858973));
#76960=CARTESIAN_POINT('Ctrl Pts',(-4.39152710765,-38.2742356128,1.85538989834));
#76961=CARTESIAN_POINT('',(-0.605290084208,-38.2742356128,-1.95105924441));
#76962=CARTESIAN_POINT('Ctrl Pts',(-0.605290084206,-38.2742356128,-1.95105924441));
#76963=CARTESIAN_POINT('Ctrl Pts',(-0.774096521679,-38.2742356128,-1.91628513625));
#76964=CARTESIAN_POINT('Ctrl Pts',(-0.942624183674,-38.2742356128,-1.87619510128));
#76965=CARTESIAN_POINT('Ctrl Pts',(-1.11061388614,-38.2742356128,-1.83037525603));
#76966=CARTESIAN_POINT('Ctrl Pts',(-1.74274860628,-38.2742356128,-1.63293852912));
#76967=CARTESIAN_POINT('Ctrl Pts',(-2.34679547467,-38.2742356128,-1.33257881069));
#76968=CARTESIAN_POINT('Ctrl Pts',(-2.73083933763,-38.2742356128,-1.04090474176));
#76969=CARTESIAN_POINT('Ctrl Pts',(-3.39638296129,-38.2742356128,-0.293897533174));
#76970=CARTESIAN_POINT('Ctrl Pts',(-3.86916001537,-38.2742356128,0.542814468562));
#76971=CARTESIAN_POINT('Ctrl Pts',(-4.06911877342,-38.2742356128,0.942104314053));
#76972=CARTESIAN_POINT('Ctrl Pts',(-4.24744781279,-38.2742356128,1.39201586348));
#76973=CARTESIAN_POINT('Ctrl Pts',(-4.39143626207,-38.2742356128,1.85509771049));
#76974=CARTESIAN_POINT('Ctrl Pts',(-4.39145443226365,-38.2742356128,1.85515614772492));
#76975=CARTESIAN_POINT('Ctrl Pts',(-4.3914726024573,-38.2742356128,1.85521458495984));
#76976=CARTESIAN_POINT('Ctrl Pts',(-4.39149077265095,-38.2742356128,1.85527302219476));
#76977=CARTESIAN_POINT('Ctrl Pts',(-4.3915089428446,-38.2742356128,1.85533145942968));
#76978=CARTESIAN_POINT('Ctrl Pts',(-4.39152711303826,-38.2742356128,1.8553898966646));
#76979=CARTESIAN_POINT('',(0.605290084208,-38.2742356128,-1.95105924441));
#76980=CARTESIAN_POINT('Origin',(1.39679934285653E-13,-38.2742356128,0.987243652491003));
#76981=CARTESIAN_POINT('',(4.39138551652333,-38.2742356128,1.85493449099992));
#76982=CARTESIAN_POINT('Ctrl Pts',(0.605290084206,-38.2742356128,-1.95105924441));
#76983=CARTESIAN_POINT('Ctrl Pts',(0.774096521679,-38.2742356128,-1.91628513625));
#76984=CARTESIAN_POINT('Ctrl Pts',(0.942624183674,-38.2742356128,-1.87619510128));
#76985=CARTESIAN_POINT('Ctrl Pts',(1.11061388614,-38.2742356128,-1.83037525603));
#76986=CARTESIAN_POINT('Ctrl Pts',(1.74274860628,-38.2742356128,-1.63293852912));
#76987=CARTESIAN_POINT('Ctrl Pts',(2.34679547467,-38.2742356128,-1.33257881069));
#76988=CARTESIAN_POINT('Ctrl Pts',(2.73083933763,-38.2742356128,-1.04090474176));
#76989=CARTESIAN_POINT('Ctrl Pts',(3.39635927668,-38.2742356128,-0.29392411682));
#76990=CARTESIAN_POINT('Ctrl Pts',(3.86912636582,-38.2742356128,0.542754916759));
#76991=CARTESIAN_POINT('Ctrl Pts',(4.06899942193,-38.2742356128,0.941795900815));
#76992=CARTESIAN_POINT('Ctrl Pts',(4.2473975181,-38.2742356128,1.39188897252));
#76993=CARTESIAN_POINT('Ctrl Pts',(4.39138551009,-38.2742356128,1.854934493));
#76994=CARTESIAN_POINT('',(5.2400559546,-38.2742356128,5.59690998219));
#76995=CARTESIAN_POINT('Ctrl Pts',(5.2400559546,-38.2742356128,5.59690998219));
#76996=CARTESIAN_POINT('Ctrl Pts',(5.25990082634,-38.2742356128,5.0059883748));
#76997=CARTESIAN_POINT('Ctrl Pts',(5.23061607717,-38.2742356128,4.36229648927));
#76998=CARTESIAN_POINT('Ctrl Pts',(5.00490058958,-38.2742356128,3.77298874453));
#76999=CARTESIAN_POINT('Ctrl Pts',(4.75506448705,-38.2742356128,3.08655684628));
#77000=CARTESIAN_POINT('Ctrl Pts',(4.54755634075,-38.2742356128,2.39287258614));
#77001=CARTESIAN_POINT('Ctrl Pts',(4.4987250478,-38.2742356128,2.21955031284));
#77002=CARTESIAN_POINT('Ctrl Pts',(4.44893332626,-38.2742356128,2.04003858973));
#77003=CARTESIAN_POINT('Ctrl Pts',(4.39152710765,-38.2742356128,1.85538989834));
#77004=CARTESIAN_POINT('Ctrl Pts',(4.3914987908103,-38.2742356128,1.8552988164412));
#77005=CARTESIAN_POINT('Ctrl Pts',(4.39147047397061,-38.2742356128001,1.85520773454239));
#77006=CARTESIAN_POINT('Ctrl Pts',(4.39144215713091,-38.2742356128001,1.85511665264359));
#77007=CARTESIAN_POINT('Ctrl Pts',(4.39141384029122,-38.2742356128001,1.85502557074478));
#77008=CARTESIAN_POINT('Ctrl Pts',(4.39138552345152,-38.2742356128001,1.85493448884598));
#77009=CARTESIAN_POINT('',(-7.34769233304E-15,-38.2742356128,10.664345987));
#77010=CARTESIAN_POINT('Origin',(-0.000416107150120478,-38.2742356128,5.42091963994));
#77011=CARTESIAN_POINT('Origin',(0.00041610715012382,-38.2742356128,5.42091963994));
#77012=CARTESIAN_POINT('',(-2.06575948168,-38.2742356128,-9.01576047707));
#77013=CARTESIAN_POINT('',(-2.02820898725,-38.2742356128,-9.02284995699));
#77014=CARTESIAN_POINT('Origin',(-2.60353654477611,-38.2742356128,-11.967168053913));
#77015=CARTESIAN_POINT('',(-0.717273426055,-38.2742356128,-7.9495168227));
#77016=CARTESIAN_POINT('Origin',(-1.81725567298,-38.2742356128,-7.94326730652));
#77017=CARTESIAN_POINT('',(-0.717273426056,-38.2742356128,-3.28965091665));
#77018=CARTESIAN_POINT('',(-0.717273426056,-38.2742356128,0.717427860236));
#77019=CARTESIAN_POINT('',(-1.11895565834,-38.2742356128,-2.79941259037));
#77020=CARTESIAN_POINT('Origin',(-1.21727342606,-38.2742356128,-3.28965091665));
#77021=CARTESIAN_POINT('',(-2.42434411094,-38.2742356128,-2.36824808793));
#77022=CARTESIAN_POINT('Origin',(-5.88418203051333E-14,-38.2742356128,2.77999550540993));
#77023=CARTESIAN_POINT('',(-6.53914701908,-38.2742356128,2.5806950957));
#77024=CARTESIAN_POINT('Ctrl Pts',(-6.53914701908,-38.2742356128,2.5806950957));
#77025=CARTESIAN_POINT('Ctrl Pts',(-5.92921620253,-38.2742356128,1.44714753899));
#77026=CARTESIAN_POINT('Ctrl Pts',(-6.2734552887,-38.2742356128,-0.199812643821));
#77027=CARTESIAN_POINT('Ctrl Pts',(-4.66846608736,-38.2742356128,-1.09094389297));
#77028=CARTESIAN_POINT('Ctrl Pts',(-3.58890539941,-38.2742356128,-1.81984798791));
#77029=CARTESIAN_POINT('Ctrl Pts',(-2.42434411094,-38.2742356128,-2.36824808793));
#77030=CARTESIAN_POINT('',(-9.47221976654,-38.2742356128,2.49225909299));
#77031=CARTESIAN_POINT('Ctrl Pts',(-9.47221976654,-38.2742356128,2.49225909299));
#77032=CARTESIAN_POINT('Ctrl Pts',(-9.39947240551,-38.2742356128,2.61145111814));
#77033=CARTESIAN_POINT('Ctrl Pts',(-9.32101749845,-38.2742356128,2.73104611971));
#77034=CARTESIAN_POINT('Ctrl Pts',(-9.23447554945,-38.2742356128,2.85280836926));
#77035=CARTESIAN_POINT('Ctrl Pts',(-9.02906684789,-38.2742356128,3.10681559939));
#77036=CARTESIAN_POINT('Ctrl Pts',(-8.75253761634,-38.2742356128,3.33309151087));
#77037=CARTESIAN_POINT('Ctrl Pts',(-8.5879953064,-38.2742356128,3.43383230551));
#77038=CARTESIAN_POINT('Ctrl Pts',(-8.23034267354,-38.2742356128,3.56436456904));
#77039=CARTESIAN_POINT('Ctrl Pts',(-7.84867458413,-38.2742356128,3.56156543232));
#77040=CARTESIAN_POINT('Ctrl Pts',(-7.67119781066,-38.2742356128,3.52757441198));
#77041=CARTESIAN_POINT('Ctrl Pts',(-7.27066371621,-38.2742356128,3.38466568023));
#77042=CARTESIAN_POINT('Ctrl Pts',(-6.95203985001,-38.2742356128,3.13761299508));
#77043=CARTESIAN_POINT('Ctrl Pts',(-6.78734156337,-38.2742356128,2.96846990237));
#77044=CARTESIAN_POINT('Ctrl Pts',(-6.6484900876,-38.2742356128,2.78390759916));
#77045=CARTESIAN_POINT('Ctrl Pts',(-6.53914701908,-38.2742356128,2.5806950957));
#77046=CARTESIAN_POINT('',(-10.0571285787,-38.2742356128,0.645805825719));
#77047=CARTESIAN_POINT('Ctrl Pts',(-9.47221976654,-38.2742356128,2.49225909299));
#77048=CARTESIAN_POINT('Ctrl Pts',(-9.54575444005,-38.2742356128,2.3717771053));
#77049=CARTESIAN_POINT('Ctrl Pts',(-9.61961951766,-38.2742356128,2.24151541202));
#77050=CARTESIAN_POINT('Ctrl Pts',(-9.68609489427,-38.2742356128,2.10542437124));
#77051=CARTESIAN_POINT('Ctrl Pts',(-9.84457330898,-38.2742356128,1.72211870919));
#77052=CARTESIAN_POINT('Ctrl Pts',(-9.94207621049,-38.2742356128,1.33157301839));
#77053=CARTESIAN_POINT('Ctrl Pts',(-9.98299011243,-38.2742356128,1.0898271634));
#77054=CARTESIAN_POINT('Ctrl Pts',(-10.0216701384,-38.2742356128,0.872037193625));
#77055=CARTESIAN_POINT('Ctrl Pts',(-10.0571285787,-38.2742356128,0.645805825719));
#77056=CARTESIAN_POINT('Ctrl Pts',(-2.06575948168004,-38.2742356128,-9.0157604770702));
#77057=CARTESIAN_POINT('Ctrl Pts',(-2.96721946584242,-38.2742356128,-8.8515051248253));
#77058=CARTESIAN_POINT('Ctrl Pts',(-3.84599035268564,-38.2742356128,-8.59864711375854));
#77059=CARTESIAN_POINT('Ctrl Pts',(-4.67357601907077,-38.2742356128,-8.25401330976187));
#77060=CARTESIAN_POINT('Ctrl Pts',(-6.17345275440962,-38.2742356128,-7.42645694768941));
#77061=CARTESIAN_POINT('Ctrl Pts',(-7.5161640814,-38.2742356128,-6.34532321195));
#77062=CARTESIAN_POINT('Ctrl Pts',(-8.15806093588,-38.2742356128,-5.76170299258));
#77063=CARTESIAN_POINT('Ctrl Pts',(-9.14108523272,-38.2742356128,-4.69984607968));
#77064=CARTESIAN_POINT('Ctrl Pts',(-9.81302959348,-38.2742356128,-3.42961050122));
#77065=CARTESIAN_POINT('Ctrl Pts',(-10.0098671635,-38.2742356128,-2.88411398337));
#77066=CARTESIAN_POINT('Ctrl Pts',(-10.222733632,-38.2742356128,-1.82926592992));
#77067=CARTESIAN_POINT('Ctrl Pts',(-10.2199521215,-38.2742356128,-0.771812654558));
#77068=CARTESIAN_POINT('Ctrl Pts',(-10.184046519,-38.2742356128,-0.287190507733));
#77069=CARTESIAN_POINT('Ctrl Pts',(-10.1298079404,-38.2742356128,0.182098137249));
#77070=CARTESIAN_POINT('Ctrl Pts',(-10.0571285787022,-38.2742356128,0.645805825719337));
#77071=CARTESIAN_POINT('Origin',(-0.000416107150126,-37.6642356128,5.42091963994));
#77072=CARTESIAN_POINT('',(3.98812927127E-15,-37.2742356128,9.86434598407));
#77073=CARTESIAN_POINT('Origin',(-0.000416107150126,-37.2742356128,5.42091963994));
#77074=CARTESIAN_POINT('',(-1.02820313028E-15,-39.6642356128,9.86434598407));
#77075=CARTESIAN_POINT('Origin',(0.000416107150126,-37.6642356128,5.42091963994));
#77076=CARTESIAN_POINT('Origin',(0.000416107150126,-37.2742356128,5.42091963994));
#77077=CARTESIAN_POINT('Ctrl Pts',(0.772076508424,-39.7742356128,-1.09035382089));
#77078=CARTESIAN_POINT('Ctrl Pts',(0.772076508424,-36.7742356128,-1.09035382089));
#77079=CARTESIAN_POINT('Ctrl Pts',(0.886178610516,-39.7742356128,-1.05996501737));
#77080=CARTESIAN_POINT('Ctrl Pts',(0.886178610516,-36.7742356128,-1.05996501737));
#77081=CARTESIAN_POINT('Ctrl Pts',(0.999471783383,-39.7742356128,-1.02648938573));
#77082=CARTESIAN_POINT('Ctrl Pts',(0.999471783383,-36.7742356128,-1.02648938573));
#77083=CARTESIAN_POINT('Ctrl Pts',(1.11165616418,-39.7742356128,-0.989701314619));
#77084=CARTESIAN_POINT('Ctrl Pts',(1.11165616418,-36.7742356128,-0.989701314619));
#77085=CARTESIAN_POINT('Ctrl Pts',(1.3921632233,-39.7742356128,-0.887346335547));
#77086=CARTESIAN_POINT('Ctrl Pts',(1.3921632233,-36.7742356128,-0.887346335547));
#77087=CARTESIAN_POINT('Ctrl Pts',(1.65990259641,-39.7742356128,-0.759470300753));
#77088=CARTESIAN_POINT('Ctrl Pts',(1.65990259641,-36.7742356128,-0.759470300753));
#77089=CARTESIAN_POINT('Ctrl Pts',(1.81552533939,-39.7742356128,-0.67135889116));
#77090=CARTESIAN_POINT('Ctrl Pts',(1.81552533939,-36.7742356128,-0.67135889116));
#77091=CARTESIAN_POINT('Ctrl Pts',(2.13001246648,-39.7742356128,-0.455784308931));
#77092=CARTESIAN_POINT('Ctrl Pts',(2.13001246648,-36.7742356128,-0.455784308931));
#77093=CARTESIAN_POINT('Ctrl Pts',(2.40225756964,-39.7742356128,-0.187376365848));
#77094=CARTESIAN_POINT('Ctrl Pts',(2.40225756964,-36.7742356128,-0.187376365848));
#77095=CARTESIAN_POINT('Ctrl Pts',(2.53491876149,-39.7742356128,-0.0306790811922));
#77096=CARTESIAN_POINT('Ctrl Pts',(2.53491876149,-36.7742356128,-0.0306790811922));
#77097=CARTESIAN_POINT('Ctrl Pts',(2.74588721076,-39.7742356128,0.250416153254));
#77098=CARTESIAN_POINT('Ctrl Pts',(2.74588721076,-36.7742356128,0.250416153254));
#77099=CARTESIAN_POINT('Ctrl Pts',(2.93290680803,-39.7742356128,0.545770364295));
#77100=CARTESIAN_POINT('Ctrl Pts',(2.93290680803,-36.7742356128,0.545770364295));
#77101=CARTESIAN_POINT('Ctrl Pts',(3.00715366555,-39.7742356128,0.670355528577));
#77102=CARTESIAN_POINT('Ctrl Pts',(3.00715366555,-36.7742356128,0.670355528577));
#77103=CARTESIAN_POINT('Ctrl Pts',(3.20108514097,-39.7742356128,1.0165930916));
#77104=CARTESIAN_POINT('Ctrl Pts',(3.20108514097,-36.7742356128,1.0165930916));
#77105=CARTESIAN_POINT('Ctrl Pts',(3.36887363395,-39.7742356128,1.37561285195));
#77106=CARTESIAN_POINT('Ctrl Pts',(3.36887363395,-36.7742356128,1.37561285195));
#77107=CARTESIAN_POINT('Ctrl Pts',(3.46527948246,-39.7742356128,1.60915269898));
#77108=CARTESIAN_POINT('Ctrl Pts',(3.46527948246,-36.7742356128,1.60915269898));
#77109=CARTESIAN_POINT('Ctrl Pts',(3.55147728822,-39.7742356128,1.84810892036));
#77110=CARTESIAN_POINT('Ctrl Pts',(3.55147728822,-36.7742356128,1.84810892036));
#77111=CARTESIAN_POINT('Ctrl Pts',(3.62746705121,-39.7742356128,2.09248151608));
#77112=CARTESIAN_POINT('Ctrl Pts',(3.62746705121,-36.7742356128,2.09248151608));
#77113=CARTESIAN_POINT('',(0.772076508359764,-37.2742356128,-1.09035382049956));
#77114=CARTESIAN_POINT('Ctrl Pts',(0.772076508424,-37.2742356128,-1.09035382089));
#77115=CARTESIAN_POINT('Ctrl Pts',(0.886178610516,-37.2742356128,-1.05996501737));
#77116=CARTESIAN_POINT('Ctrl Pts',(0.999471783383,-37.2742356128,-1.02648938573));
#77117=CARTESIAN_POINT('Ctrl Pts',(1.11165616418,-37.2742356128,-0.989701314619));
#77118=CARTESIAN_POINT('Ctrl Pts',(1.3921632233,-37.2742356128,-0.887346335547));
#77119=CARTESIAN_POINT('Ctrl Pts',(1.65990259641,-37.2742356128,-0.759470300753));
#77120=CARTESIAN_POINT('Ctrl Pts',(1.81552533939,-37.2742356128,-0.67135889116));
#77121=CARTESIAN_POINT('Ctrl Pts',(2.13001246648,-37.2742356128,-0.455784308931));
#77122=CARTESIAN_POINT('Ctrl Pts',(2.40225756964,-37.2742356128,-0.187376365848));
#77123=CARTESIAN_POINT('Ctrl Pts',(2.53491876149,-37.2742356128,-0.0306790811922));
#77124=CARTESIAN_POINT('Ctrl Pts',(2.74588721076,-37.2742356128,0.250416153254));
#77125=CARTESIAN_POINT('Ctrl Pts',(2.93290680803,-37.2742356128,0.545770364295));
#77126=CARTESIAN_POINT('Ctrl Pts',(3.00715366555,-37.2742356128,0.670355528577));
#77127=CARTESIAN_POINT('Ctrl Pts',(3.20108514097,-37.2742356128,1.0165930916));
#77128=CARTESIAN_POINT('Ctrl Pts',(3.36887363395,-37.2742356128,1.37561285195));
#77129=CARTESIAN_POINT('Ctrl Pts',(3.46527948246,-37.2742356128,1.60915269898));
#77130=CARTESIAN_POINT('Ctrl Pts',(3.55147728822,-37.2742356128,1.84810892036));
#77131=CARTESIAN_POINT('Ctrl Pts',(3.62746705121,-37.2742356128,2.09248151608));
#77132=CARTESIAN_POINT('',(0.772076508426,-39.6642356128,-1.09035382089));
#77133=CARTESIAN_POINT('Origin',(-3.35265884719E-30,-37.2742356128,3.15283103411E-22));
#77134=CARTESIAN_POINT('',(-0.605290084059043,-37.2742356128,-1.95105924377086));
#77135=CARTESIAN_POINT('',(-4.39152711004478,-37.2742356128,1.85538989759537));
#77136=CARTESIAN_POINT('Ctrl Pts',(-0.605290084206,-37.2742356128,-1.95105924441));
#77137=CARTESIAN_POINT('Ctrl Pts',(-0.774096521679,-37.2742356128,-1.91628513625));
#77138=CARTESIAN_POINT('Ctrl Pts',(-0.942624183674,-37.2742356128,-1.87619510128));
#77139=CARTESIAN_POINT('Ctrl Pts',(-1.11061388614,-37.2742356128,-1.83037525603));
#77140=CARTESIAN_POINT('Ctrl Pts',(-1.74274860628,-37.2742356128,-1.63293852912));
#77141=CARTESIAN_POINT('Ctrl Pts',(-2.34679547467,-37.2742356128,-1.33257881069));
#77142=CARTESIAN_POINT('Ctrl Pts',(-2.73083933763,-37.2742356128,-1.04090474176));
#77143=CARTESIAN_POINT('Ctrl Pts',(-3.39638296129,-37.2742356128,-0.293897533174));
#77144=CARTESIAN_POINT('Ctrl Pts',(-3.86916001537,-37.2742356128,0.542814468562));
#77145=CARTESIAN_POINT('Ctrl Pts',(-4.06911877342,-37.2742356128,0.942104314053));
#77146=CARTESIAN_POINT('Ctrl Pts',(-4.24744781279,-37.2742356128,1.39201586348));
#77147=CARTESIAN_POINT('Ctrl Pts',(-4.39143626207,-37.2742356128,1.85509771049));
#77148=CARTESIAN_POINT('Ctrl Pts',(-4.39145443226365,-37.2742356128,1.85515614772492));
#77149=CARTESIAN_POINT('Ctrl Pts',(-4.3914726024573,-37.2742356128,1.85521458495984));
#77150=CARTESIAN_POINT('Ctrl Pts',(-4.39149077265095,-37.2742356128,1.85527302219476));
#77151=CARTESIAN_POINT('Ctrl Pts',(-4.3915089428446,-37.2742356128,1.85533145942968));
#77152=CARTESIAN_POINT('Ctrl Pts',(-4.39152711303826,-37.2742356128,1.8553898966646));
#77153=CARTESIAN_POINT('',(-5.2400559546,-37.2742356128,5.59690998219));
#77154=CARTESIAN_POINT('Ctrl Pts',(-5.2400559546,-37.2742356128,5.59690998219));
#77155=CARTESIAN_POINT('Ctrl Pts',(-5.25990082634,-37.2742356128,5.0059883748));
#77156=CARTESIAN_POINT('Ctrl Pts',(-5.23061607717,-37.2742356128,4.36229648927));
#77157=CARTESIAN_POINT('Ctrl Pts',(-5.00490058958,-37.2742356128,3.77298874453));
#77158=CARTESIAN_POINT('Ctrl Pts',(-4.75506448705,-37.2742356128,3.08655684628));
#77159=CARTESIAN_POINT('Ctrl Pts',(-4.54755634075,-37.2742356128,2.39287258614));
#77160=CARTESIAN_POINT('Ctrl Pts',(-4.4987250478,-37.2742356128,2.21955031284));
#77161=CARTESIAN_POINT('Ctrl Pts',(-4.44893332626,-37.2742356128,2.04003858973));
#77162=CARTESIAN_POINT('Ctrl Pts',(-4.39152710765,-37.2742356128,1.85538989834));
#77163=CARTESIAN_POINT('',(4.37703259054E-15,-37.2742356128,10.664345987));
#77164=CARTESIAN_POINT('Origin',(0.000416107150126,-37.2742356128,5.42091963994));
#77165=CARTESIAN_POINT('',(5.2400559546,-37.2742356128,5.59690998219));
#77166=CARTESIAN_POINT('Origin',(-0.000416107150126,-37.2742356128,5.42091963994));
#77167=CARTESIAN_POINT('',(4.39138551612134,-37.2742356128,1.85493449668939));
#77168=CARTESIAN_POINT('Ctrl Pts',(5.2400559546,-37.2742356128,5.59690998219));
#77169=CARTESIAN_POINT('Ctrl Pts',(5.25990082634,-37.2742356128,5.0059883748));
#77170=CARTESIAN_POINT('Ctrl Pts',(5.23061607717,-37.2742356128,4.36229648927));
#77171=CARTESIAN_POINT('Ctrl Pts',(5.00490058958,-37.2742356128,3.77298874453));
#77172=CARTESIAN_POINT('Ctrl Pts',(4.75506448705,-37.2742356128,3.08655684628));
#77173=CARTESIAN_POINT('Ctrl Pts',(4.54755634075,-37.2742356128,2.39287258614));
#77174=CARTESIAN_POINT('Ctrl Pts',(4.4987250478,-37.2742356128,2.21955031284));
#77175=CARTESIAN_POINT('Ctrl Pts',(4.44893332626,-37.2742356128,2.04003858973));
#77176=CARTESIAN_POINT('Ctrl Pts',(4.39152710765,-37.2742356128,1.85538989834));
#77177=CARTESIAN_POINT('Ctrl Pts',(4.39149879112577,-37.2742356128,1.8552988174559));
#77178=CARTESIAN_POINT('Ctrl Pts',(4.39147047460154,-37.2742356128,1.85520773657181));
#77179=CARTESIAN_POINT('Ctrl Pts',(4.39144215807731,-37.2742356128,1.85511665568771));
#77180=CARTESIAN_POINT('Ctrl Pts',(4.39141384155308,-37.2742356128,1.85502557480361));
#77181=CARTESIAN_POINT('Ctrl Pts',(4.39138552502885,-37.2742356128,1.85493449391952));
#77182=CARTESIAN_POINT('',(0.605290084059048,-37.2742356128,-1.95105924377088));
#77183=CARTESIAN_POINT('Ctrl Pts',(0.605290084206,-37.2742356128,-1.95105924441));
#77184=CARTESIAN_POINT('Ctrl Pts',(0.774096521679,-37.2742356128,-1.91628513625));
#77185=CARTESIAN_POINT('Ctrl Pts',(0.942624183674,-37.2742356128,-1.87619510128));
#77186=CARTESIAN_POINT('Ctrl Pts',(1.11061388614,-37.2742356128,-1.83037525603));
#77187=CARTESIAN_POINT('Ctrl Pts',(1.74274860628,-37.2742356128,-1.63293852912));
#77188=CARTESIAN_POINT('Ctrl Pts',(2.34679547467,-37.2742356128,-1.33257881069));
#77189=CARTESIAN_POINT('Ctrl Pts',(2.73083933763,-37.2742356128,-1.04090474176));
#77190=CARTESIAN_POINT('Ctrl Pts',(3.39635927668,-37.2742356128,-0.29392411682));
#77191=CARTESIAN_POINT('Ctrl Pts',(3.86912636582,-37.2742356128,0.542754916759));
#77192=CARTESIAN_POINT('Ctrl Pts',(4.06899942193,-37.2742356128,0.941795900815));
#77193=CARTESIAN_POINT('Ctrl Pts',(4.2473975181,-37.2742356128,1.39188897252));
#77194=CARTESIAN_POINT('Ctrl Pts',(4.39138551009,-37.2742356128,1.854934493));
#77195=CARTESIAN_POINT('Origin',(1.44440015504E-13,-37.2742356128,0.987243652491));
#77196=CARTESIAN_POINT('',(-0.772076508359766,-37.2742356128,-1.09035382049957));
#77197=CARTESIAN_POINT('Origin',(-3.57491813929E-14,-37.2742356128,1.80859389597));
#77198=CARTESIAN_POINT('Ctrl Pts',(-0.772076508424,-37.2742356128,-1.09035382089));
#77199=CARTESIAN_POINT('Ctrl Pts',(-0.886178610516,-37.2742356128,-1.05996501737));
#77200=CARTESIAN_POINT('Ctrl Pts',(-0.999471783383,-37.2742356128,-1.02648938573));
#77201=CARTESIAN_POINT('Ctrl Pts',(-1.11165616418,-37.2742356128,-0.989701314619));
#77202=CARTESIAN_POINT('Ctrl Pts',(-1.3921632233,-37.2742356128,-0.887346335547));
#77203=CARTESIAN_POINT('Ctrl Pts',(-1.65990259641,-37.2742356128,-0.759470300753));
#77204=CARTESIAN_POINT('Ctrl Pts',(-1.81552533939,-37.2742356128,-0.67135889116));
#77205=CARTESIAN_POINT('Ctrl Pts',(-2.13001246648,-37.2742356128,-0.455784308931));
#77206=CARTESIAN_POINT('Ctrl Pts',(-2.40225756964,-37.2742356128,-0.187376365848));
#77207=CARTESIAN_POINT('Ctrl Pts',(-2.53491876149,-37.2742356128,-0.0306790811922));
#77208=CARTESIAN_POINT('Ctrl Pts',(-2.74588721076,-37.2742356128,0.250416153254));
#77209=CARTESIAN_POINT('Ctrl Pts',(-2.93290680803,-37.2742356128,0.545770364295));
#77210=CARTESIAN_POINT('Ctrl Pts',(-3.00715366555,-37.2742356128,0.670355528577));
#77211=CARTESIAN_POINT('Ctrl Pts',(-3.20108514097,-37.2742356128,1.0165930916));
#77212=CARTESIAN_POINT('Ctrl Pts',(-3.36887363395,-37.2742356128,1.37561285195));
#77213=CARTESIAN_POINT('Ctrl Pts',(-3.46527948246,-37.2742356128,1.60915269898));
#77214=CARTESIAN_POINT('Ctrl Pts',(-3.55147728822,-37.2742356128,1.84810892036));
#77215=CARTESIAN_POINT('Ctrl Pts',(-3.62746705121,-37.2742356128,2.09248151608));
#77216=CARTESIAN_POINT('Origin',(-3.57491813929E-14,-38.2742356128,1.80859389597));
#77217=CARTESIAN_POINT('',(-0.772076508426,-38.2742356128,-1.09035382089));
#77218=CARTESIAN_POINT('Ctrl Pts',(-0.772076508424,-39.7742356128,-1.09035382089));
#77219=CARTESIAN_POINT('Ctrl Pts',(-0.772076508424,-36.7742356128,-1.09035382089));
#77220=CARTESIAN_POINT('Ctrl Pts',(-0.886178610516,-39.7742356128,-1.05996501737));
#77221=CARTESIAN_POINT('Ctrl Pts',(-0.886178610516,-36.7742356128,-1.05996501737));
#77222=CARTESIAN_POINT('Ctrl Pts',(-0.999471783383,-39.7742356128,-1.02648938573));
#77223=CARTESIAN_POINT('Ctrl Pts',(-0.999471783383,-36.7742356128,-1.02648938573));
#77224=CARTESIAN_POINT('Ctrl Pts',(-1.11165616418,-39.7742356128,-0.989701314619));
#77225=CARTESIAN_POINT('Ctrl Pts',(-1.11165616418,-36.7742356128,-0.989701314619));
#77226=CARTESIAN_POINT('Ctrl Pts',(-1.3921632233,-39.7742356128,-0.887346335547));
#77227=CARTESIAN_POINT('Ctrl Pts',(-1.3921632233,-36.7742356128,-0.887346335547));
#77228=CARTESIAN_POINT('Ctrl Pts',(-1.65990259641,-39.7742356128,-0.759470300753));
#77229=CARTESIAN_POINT('Ctrl Pts',(-1.65990259641,-36.7742356128,-0.759470300753));
#77230=CARTESIAN_POINT('Ctrl Pts',(-1.81552533939,-39.7742356128,-0.67135889116));
#77231=CARTESIAN_POINT('Ctrl Pts',(-1.81552533939,-36.7742356128,-0.67135889116));
#77232=CARTESIAN_POINT('Ctrl Pts',(-2.13001246648,-39.7742356128,-0.455784308931));
#77233=CARTESIAN_POINT('Ctrl Pts',(-2.13001246648,-36.7742356128,-0.455784308931));
#77234=CARTESIAN_POINT('Ctrl Pts',(-2.40225756964,-39.7742356128,-0.187376365848));
#77235=CARTESIAN_POINT('Ctrl Pts',(-2.40225756964,-36.7742356128,-0.187376365848));
#77236=CARTESIAN_POINT('Ctrl Pts',(-2.53491876149,-39.7742356128,-0.0306790811922));
#77237=CARTESIAN_POINT('Ctrl Pts',(-2.53491876149,-36.7742356128,-0.0306790811922));
#77238=CARTESIAN_POINT('Ctrl Pts',(-2.74588721076,-39.7742356128,0.250416153254));
#77239=CARTESIAN_POINT('Ctrl Pts',(-2.74588721076,-36.7742356128,0.250416153254));
#77240=CARTESIAN_POINT('Ctrl Pts',(-2.93290680803,-39.7742356128,0.545770364295));
#77241=CARTESIAN_POINT('Ctrl Pts',(-2.93290680803,-36.7742356128,0.545770364295));
#77242=CARTESIAN_POINT('Ctrl Pts',(-3.00715366555,-39.7742356128,0.670355528577));
#77243=CARTESIAN_POINT('Ctrl Pts',(-3.00715366555,-36.7742356128,0.670355528577));
#77244=CARTESIAN_POINT('Ctrl Pts',(-3.20108514097,-39.7742356128,1.0165930916));
#77245=CARTESIAN_POINT('Ctrl Pts',(-3.20108514097,-36.7742356128,1.0165930916));
#77246=CARTESIAN_POINT('Ctrl Pts',(-3.36887363395,-39.7742356128,1.37561285195));
#77247=CARTESIAN_POINT('Ctrl Pts',(-3.36887363395,-36.7742356128,1.37561285195));
#77248=CARTESIAN_POINT('Ctrl Pts',(-3.46527948246,-39.7742356128,1.60915269898));
#77249=CARTESIAN_POINT('Ctrl Pts',(-3.46527948246,-36.7742356128,1.60915269898));
#77250=CARTESIAN_POINT('Ctrl Pts',(-3.55147728822,-39.7742356128,1.84810892036));
#77251=CARTESIAN_POINT('Ctrl Pts',(-3.55147728822,-36.7742356128,1.84810892036));
#77252=CARTESIAN_POINT('Ctrl Pts',(-3.62746705121,-39.7742356128,2.09248151608));
#77253=CARTESIAN_POINT('Ctrl Pts',(-3.62746705121,-36.7742356128,2.09248151608));
#77254=CARTESIAN_POINT('Ctrl Pts',(7.07911993306,-39.7742356128,1.41233341424));
#77255=CARTESIAN_POINT('Ctrl Pts',(7.07911993306,-36.7742356128,1.41233341424));
#77256=CARTESIAN_POINT('Ctrl Pts',(7.03043912742,-39.7742356128,0.911971673481));
#77257=CARTESIAN_POINT('Ctrl Pts',(7.03043912742,-36.7742356128,0.911971673481));
#77258=CARTESIAN_POINT('Ctrl Pts',(6.93879090488,-39.7742356128,0.427451671407));
#77259=CARTESIAN_POINT('Ctrl Pts',(6.93879090488,-36.7742356128,0.427451671407));
#77260=CARTESIAN_POINT('Ctrl Pts',(6.79968866463,-39.7742356128,-0.0361534703089));
#77261=CARTESIAN_POINT('Ctrl Pts',(6.79968866463,-36.7742356128,-0.0361534703089));
#77262=CARTESIAN_POINT('Ctrl Pts',(6.4258973146,-39.7742356128,-0.894662603614));
#77263=CARTESIAN_POINT('Ctrl Pts',(6.4258973146,-36.7742356128,-0.894662603614));
#77264=CARTESIAN_POINT('Ctrl Pts',(5.86106085412,-39.7742356128,-1.62790491519));
#77265=CARTESIAN_POINT('Ctrl Pts',(5.86106085412,-36.7742356128,-1.62790491519));
#77266=CARTESIAN_POINT('Ctrl Pts',(5.53842443335,-39.7742356128,-1.95360958375));
#77267=CARTESIAN_POINT('Ctrl Pts',(5.53842443335,-36.7742356128,-1.95360958375));
#77268=CARTESIAN_POINT('Ctrl Pts',(4.98933040959,-39.7742356128,-2.39194593497));
#77269=CARTESIAN_POINT('Ctrl Pts',(4.98933040959,-36.7742356128,-2.39194593497));
#77270=CARTESIAN_POINT('Ctrl Pts',(4.36273333629,-39.7742356128,-2.74903878258));
#77271=CARTESIAN_POINT('Ctrl Pts',(4.36273333629,-36.7742356128,-2.74903878258));
#77272=CARTESIAN_POINT('Ctrl Pts',(4.14078300625,-39.7742356128,-2.86156599489));
#77273=CARTESIAN_POINT('Ctrl Pts',(4.14078300625,-36.7742356128,-2.86156599489));
#77274=CARTESIAN_POINT('Ctrl Pts',(3.91246466012,-39.7742356128,-2.96464616022));
#77275=CARTESIAN_POINT('Ctrl Pts',(3.91246466012,-36.7742356128,-2.96464616022));
#77276=CARTESIAN_POINT('Ctrl Pts',(3.67755401867,-39.7742356128,-3.05915055738));
#77277=CARTESIAN_POINT('Ctrl Pts',(3.67755401867,-36.7742356128,-3.05915055738));
#77278=CARTESIAN_POINT('',(3.67755401867,-37.2742356128,-3.05915055738));
#77279=CARTESIAN_POINT('',(3.67755401867,-39.6642356128,-3.05915055738));
#77280=CARTESIAN_POINT('',(7.07911993306,-37.2742356128,1.41233341424));
#77281=CARTESIAN_POINT('Ctrl Pts',(7.07911993306,-37.2742356128,1.41233341424));
#77282=CARTESIAN_POINT('Ctrl Pts',(7.03043912742,-37.2742356128,0.911971673481));
#77283=CARTESIAN_POINT('Ctrl Pts',(6.93879090488,-37.2742356128,0.427451671407));
#77284=CARTESIAN_POINT('Ctrl Pts',(6.79968866463,-37.2742356128,-0.0361534703089));
#77285=CARTESIAN_POINT('Ctrl Pts',(6.4258973146,-37.2742356128,-0.894662603614));
#77286=CARTESIAN_POINT('Ctrl Pts',(5.86106085412,-37.2742356128,-1.62790491519));
#77287=CARTESIAN_POINT('Ctrl Pts',(5.53842443335,-37.2742356128,-1.95360958375));
#77288=CARTESIAN_POINT('Ctrl Pts',(4.98933040959,-37.2742356128,-2.39194593497));
#77289=CARTESIAN_POINT('Ctrl Pts',(4.36273333629,-37.2742356128,-2.74903878258));
#77290=CARTESIAN_POINT('Ctrl Pts',(4.14078300625,-37.2742356128,-2.86156599489));
#77291=CARTESIAN_POINT('Ctrl Pts',(3.91246466012,-37.2742356128,-2.96464616022));
#77292=CARTESIAN_POINT('Ctrl Pts',(3.67755401867,-37.2742356128,-3.05915055738));
#77293=CARTESIAN_POINT('',(7.07911993306,-39.6642356128,1.41233341424));
#77294=CARTESIAN_POINT('Origin',(3.78952269078,-37.6642356128,-3.33747234321));
#77295=CARTESIAN_POINT('',(3.51985615629,-37.2742356128,-3.20601908088));
#77296=CARTESIAN_POINT('Origin',(3.78952269078,-37.2742356128,-3.33747234321));
#77297=CARTESIAN_POINT('',(3.51985615629,-39.6642356128,-3.20601908088));
#77298=CARTESIAN_POINT('Ctrl Pts',(3.51985615629,-39.7742356128,-3.20601908088));
#77299=CARTESIAN_POINT('Ctrl Pts',(3.51985615629,-36.7742356128,-3.20601908088));
#77300=CARTESIAN_POINT('Ctrl Pts',(3.35540949155,-39.7742356128,-3.54336911238));
#77301=CARTESIAN_POINT('Ctrl Pts',(3.35540949155,-36.7742356128,-3.54336911238));
#77302=CARTESIAN_POINT('Ctrl Pts',(3.15758359021,-39.7742356128,-3.85751660428));
#77303=CARTESIAN_POINT('Ctrl Pts',(3.15758359021,-36.7742356128,-3.85751660428));
#77304=CARTESIAN_POINT('Ctrl Pts',(2.92553217282,-39.7742356128,-4.14369667075));
#77305=CARTESIAN_POINT('Ctrl Pts',(2.92553217282,-36.7742356128,-4.14369667075));
#77306=CARTESIAN_POINT('Ctrl Pts',(2.54664760633,-39.7742356128,-4.50813716291));
#77307=CARTESIAN_POINT('Ctrl Pts',(2.54664760633,-36.7742356128,-4.50813716291));
#77308=CARTESIAN_POINT('Ctrl Pts',(2.10878664609,-39.7742356128,-4.80650592873));
#77309=CARTESIAN_POINT('Ctrl Pts',(2.10878664609,-36.7742356128,-4.80650592873));
#77310=CARTESIAN_POINT('Ctrl Pts',(1.97163547839,-39.7742356128,-4.89045414442));
#77311=CARTESIAN_POINT('Ctrl Pts',(1.97163547839,-36.7742356128,-4.89045414442));
#77312=CARTESIAN_POINT('Ctrl Pts',(1.8303523356,-39.7742356128,-4.96805050291));
#77313=CARTESIAN_POINT('Ctrl Pts',(1.8303523356,-36.7742356128,-4.96805050291));
#77314=CARTESIAN_POINT('Ctrl Pts',(1.68475792039,-39.7742356128,-5.03973467448));
#77315=CARTESIAN_POINT('Ctrl Pts',(1.68475792039,-36.7742356128,-5.03973467448));
#77316=CARTESIAN_POINT('',(1.68475792039,-37.2742356128,-5.03973467448));
#77317=CARTESIAN_POINT('',(1.68475792039,-39.6642356128,-5.03973467448));
#77318=CARTESIAN_POINT('Ctrl Pts',(3.51985615629,-37.2742356128,-3.20601908088));
#77319=CARTESIAN_POINT('Ctrl Pts',(3.35540949155,-37.2742356128,-3.54336911238));
#77320=CARTESIAN_POINT('Ctrl Pts',(3.15758359021,-37.2742356128,-3.85751660428));
#77321=CARTESIAN_POINT('Ctrl Pts',(2.92553217282,-37.2742356128,-4.14369667075));
#77322=CARTESIAN_POINT('Ctrl Pts',(2.54664760633,-37.2742356128,-4.50813716291));
#77323=CARTESIAN_POINT('Ctrl Pts',(2.10878664609,-37.2742356128,-4.80650592873));
#77324=CARTESIAN_POINT('Ctrl Pts',(1.97163547839,-37.2742356128,-4.89045414442));
#77325=CARTESIAN_POINT('Ctrl Pts',(1.8303523356,-37.2742356128,-4.96805050291));
#77326=CARTESIAN_POINT('Ctrl Pts',(1.68475792039,-37.2742356128,-5.03973467448));
#77327=CARTESIAN_POINT('Ctrl Pts',(7.21384189758,-39.7742356128,2.18958432614));
#77328=CARTESIAN_POINT('Ctrl Pts',(7.21384189758,-36.7742356128,2.18958432614));
#77329=CARTESIAN_POINT('Ctrl Pts',(7.13908599018,-39.7742356128,2.05065155888));
#77330=CARTESIAN_POINT('Ctrl Pts',(7.13908599018,-36.7742356128,2.05065155888));
#77331=CARTESIAN_POINT('Ctrl Pts',(7.08905059141,-39.7742356128,1.8984189694));
#77332=CARTESIAN_POINT('Ctrl Pts',(7.08905059141,-36.7742356128,1.8984189694));
#77333=CARTESIAN_POINT('Ctrl Pts',(7.1053290044,-39.7742356128,1.72681022597));
#77334=CARTESIAN_POINT('Ctrl Pts',(7.1053290044,-36.7742356128,1.72681022597));
#77335=CARTESIAN_POINT('Ctrl Pts',(7.09439724612,-39.7742356128,1.56936004643));
#77336=CARTESIAN_POINT('Ctrl Pts',(7.09439724612,-36.7742356128,1.56936004643));
#77337=CARTESIAN_POINT('Ctrl Pts',(7.07911993306,-39.7742356128,1.41233341424));
#77338=CARTESIAN_POINT('Ctrl Pts',(7.07911993306,-36.7742356128,1.41233341424));
#77339=CARTESIAN_POINT('',(7.21384189758,-37.2742356128,2.18958432614));
#77340=CARTESIAN_POINT('',(7.21384189758,-39.6642356128,2.18958432614));
#77341=CARTESIAN_POINT('Ctrl Pts',(7.21384189758,-37.2742356128,2.18958432614));
#77342=CARTESIAN_POINT('Ctrl Pts',(7.13908599018,-37.2742356128,2.05065155888));
#77343=CARTESIAN_POINT('Ctrl Pts',(7.08905059141,-37.2742356128,1.8984189694));
#77344=CARTESIAN_POINT('Ctrl Pts',(7.1053290044,-37.2742356128,1.72681022597));
#77345=CARTESIAN_POINT('Ctrl Pts',(7.09439724612,-37.2742356128,1.56936004643));
#77346=CARTESIAN_POINT('Ctrl Pts',(7.07911993306,-37.2742356128,1.41233341424));
#77347=CARTESIAN_POINT('Ctrl Pts',(8.75956299024,-39.7742356128,2.0634404101));
#77348=CARTESIAN_POINT('Ctrl Pts',(8.75956299024,-36.7742356128,2.0634404101));
#77349=CARTESIAN_POINT('Ctrl Pts',(8.67258032609,-39.7742356128,2.20595609378));
#77350=CARTESIAN_POINT('Ctrl Pts',(8.67258032609,-36.7742356128,2.20595609378));
#77351=CARTESIAN_POINT('Ctrl Pts',(8.57679326147,-39.7742356128,2.34786591099));
#77352=CARTESIAN_POINT('Ctrl Pts',(8.57679326147,-36.7742356128,2.34786591099));
#77353=CARTESIAN_POINT('Ctrl Pts',(8.46448329596,-39.7742356128,2.49604426586));
#77354=CARTESIAN_POINT('Ctrl Pts',(8.46448329596,-36.7742356128,2.49604426586));
#77355=CARTESIAN_POINT('Ctrl Pts',(8.27825186329,-39.7742356128,2.67220081215));
#77356=CARTESIAN_POINT('Ctrl Pts',(8.27825186329,-36.7742356128,2.67220081215));
#77357=CARTESIAN_POINT('Ctrl Pts',(8.05379939761,-39.7742356128,2.74035894609));
#77358=CARTESIAN_POINT('Ctrl Pts',(8.05379939761,-36.7742356128,2.74035894609));
#77359=CARTESIAN_POINT('Ctrl Pts',(7.9779370982,-39.7742356128,2.74765496713));
#77360=CARTESIAN_POINT('Ctrl Pts',(7.9779370982,-36.7742356128,2.74765496713));
#77361=CARTESIAN_POINT('Ctrl Pts',(7.82203636779,-39.7742356128,2.73225108729));
#77362=CARTESIAN_POINT('Ctrl Pts',(7.82203636779,-36.7742356128,2.73225108729));
#77363=CARTESIAN_POINT('Ctrl Pts',(7.67278421879,-39.7742356128,2.66639360485));
#77364=CARTESIAN_POINT('Ctrl Pts',(7.67278421879,-36.7742356128,2.66639360485));
#77365=CARTESIAN_POINT('Ctrl Pts',(7.59903734004,-39.7742356128,2.62164000818));
#77366=CARTESIAN_POINT('Ctrl Pts',(7.59903734004,-36.7742356128,2.62164000818));
#77367=CARTESIAN_POINT('Ctrl Pts',(7.46503014366,-39.7742356128,2.52047218586));
#77368=CARTESIAN_POINT('Ctrl Pts',(7.46503014366,-36.7742356128,2.52047218586));
#77369=CARTESIAN_POINT('Ctrl Pts',(7.35007323494,-39.7742356128,2.39634839519));
#77370=CARTESIAN_POINT('Ctrl Pts',(7.35007323494,-36.7742356128,2.39634839519));
#77371=CARTESIAN_POINT('Ctrl Pts',(7.29780025627,-39.7742356128,2.32993852802));
#77372=CARTESIAN_POINT('Ctrl Pts',(7.29780025627,-36.7742356128,2.32993852802));
#77373=CARTESIAN_POINT('Ctrl Pts',(7.25230657394,-39.7742356128,2.26107036804));
#77374=CARTESIAN_POINT('Ctrl Pts',(7.25230657394,-36.7742356128,2.26107036804));
#77375=CARTESIAN_POINT('Ctrl Pts',(7.21384189758,-39.7742356128,2.18958432614));
#77376=CARTESIAN_POINT('Ctrl Pts',(7.21384189758,-36.7742356128,2.18958432614));
#77377=CARTESIAN_POINT('',(8.75956299023,-37.2742356128,2.0634404101));
#77378=CARTESIAN_POINT('',(8.75956299024,-39.6642356128,2.0634404101));
#77379=CARTESIAN_POINT('Ctrl Pts',(8.75956299024,-37.2742356128,2.0634404101));
#77380=CARTESIAN_POINT('Ctrl Pts',(8.67258032609,-37.2742356128,2.20595609378));
#77381=CARTESIAN_POINT('Ctrl Pts',(8.57679326147,-37.2742356128,2.34786591099));
#77382=CARTESIAN_POINT('Ctrl Pts',(8.46448329596,-37.2742356128,2.49604426586));
#77383=CARTESIAN_POINT('Ctrl Pts',(8.27825186329,-37.2742356128,2.67220081215));
#77384=CARTESIAN_POINT('Ctrl Pts',(8.05379939761,-37.2742356128,2.74035894609));
#77385=CARTESIAN_POINT('Ctrl Pts',(7.9779370982,-37.2742356128,2.74765496713));
#77386=CARTESIAN_POINT('Ctrl Pts',(7.82203636779,-37.2742356128,2.73225108729));
#77387=CARTESIAN_POINT('Ctrl Pts',(7.67278421879,-37.2742356128,2.66639360485));
#77388=CARTESIAN_POINT('Ctrl Pts',(7.59903734004,-37.2742356128,2.62164000818));
#77389=CARTESIAN_POINT('Ctrl Pts',(7.46503014366,-37.2742356128,2.52047218586));
#77390=CARTESIAN_POINT('Ctrl Pts',(7.35007323494,-37.2742356128,2.39634839519));
#77391=CARTESIAN_POINT('Ctrl Pts',(7.29780025627,-37.2742356128,2.32993852802));
#77392=CARTESIAN_POINT('Ctrl Pts',(7.25230657394,-37.2742356128,2.26107036804));
#77393=CARTESIAN_POINT('Ctrl Pts',(7.21384189758,-37.2742356128,2.18958432614));
#77394=CARTESIAN_POINT('Ctrl Pts',(8.75956299023,-39.7742356128,2.0634404101));
#77395=CARTESIAN_POINT('Ctrl Pts',(8.75956299023,-36.7742356128,2.0634404101));
#77396=CARTESIAN_POINT('Ctrl Pts',(8.92890465395,-39.7742356128,1.78598462948));
#77397=CARTESIAN_POINT('Ctrl Pts',(8.92890465395,-36.7742356128,1.78598462948));
#77398=CARTESIAN_POINT('Ctrl Pts',(9.07290910839,-39.7742356128,1.49306491902));
#77399=CARTESIAN_POINT('Ctrl Pts',(9.07290910839,-36.7742356128,1.49306491902));
#77400=CARTESIAN_POINT('Ctrl Pts',(9.12674985892,-39.7742356128,1.15064933619));
#77401=CARTESIAN_POINT('Ctrl Pts',(9.12674985892,-36.7742356128,1.15064933619));
#77402=CARTESIAN_POINT('Ctrl Pts',(9.18664865847,-39.7742356128,0.831017278591));
#77403=CARTESIAN_POINT('Ctrl Pts',(9.18664865847,-36.7742356128,0.831017278591));
#77404=CARTESIAN_POINT('Ctrl Pts',(9.23698117862,-39.7742356128,0.509886547137));
#77405=CARTESIAN_POINT('Ctrl Pts',(9.23698117862,-36.7742356128,0.509886547137));
#77406=CARTESIAN_POINT('',(9.23698117862,-37.2742356128,0.509886547137));
#77407=CARTESIAN_POINT('Ctrl Pts',(8.75956299023,-37.2742356128,2.0634404101));
#77408=CARTESIAN_POINT('Ctrl Pts',(8.92890465395,-37.2742356128,1.78598462948));
#77409=CARTESIAN_POINT('Ctrl Pts',(9.07290910839,-37.2742356128,1.49306491902));
#77410=CARTESIAN_POINT('Ctrl Pts',(9.12674985892,-37.2742356128,1.15064933619));
#77411=CARTESIAN_POINT('Ctrl Pts',(9.18664865847,-37.2742356128,0.831017278591));
#77412=CARTESIAN_POINT('Ctrl Pts',(9.23698117862,-37.2742356128,0.509886547137));
#77413=CARTESIAN_POINT('',(9.23698117862,-39.6642356128,0.509886547137));
#77414=CARTESIAN_POINT('Ctrl Pts',(1.8704316098,-39.7742356128,-8.24476960846));
#77415=CARTESIAN_POINT('Ctrl Pts',(1.8704316098,-36.7742356128,-8.24476960846));
#77416=CARTESIAN_POINT('Ctrl Pts',(2.8184136576,-39.7742356128,-8.07409211621));
#77417=CARTESIAN_POINT('Ctrl Pts',(2.8184136576,-36.7742356128,-8.07409211621));
#77418=CARTESIAN_POINT('Ctrl Pts',(3.72902170056,-39.7742356128,-7.80028819978));
#77419=CARTESIAN_POINT('Ctrl Pts',(3.72902170056,-36.7742356128,-7.80028819978));
#77420=CARTESIAN_POINT('Ctrl Pts',(4.56766016636,-39.7742356128,-7.42304518879));
#77421=CARTESIAN_POINT('Ctrl Pts',(4.56766016636,-36.7742356128,-7.42304518879));
#77422=CARTESIAN_POINT('Ctrl Pts',(6.0885112091,-39.7742356128,-6.51001025629));
#77423=CARTESIAN_POINT('Ctrl Pts',(6.0885112091,-36.7742356128,-6.51001025629));
#77424=CARTESIAN_POINT('Ctrl Pts',(7.447100543,-39.7742356128,-5.31497212719));
#77425=CARTESIAN_POINT('Ctrl Pts',(7.447100543,-36.7742356128,-5.31497212719));
#77426=CARTESIAN_POINT('Ctrl Pts',(8.1250786803,-39.7742356128,-4.64371494659));
#77427=CARTESIAN_POINT('Ctrl Pts',(8.1250786803,-36.7742356128,-4.64371494659));
#77428=CARTESIAN_POINT('Ctrl Pts',(8.99226462924,-39.7742356128,-3.46343233105));
#77429=CARTESIAN_POINT('Ctrl Pts',(8.99226462924,-36.7742356128,-3.46343233105));
#77430=CARTESIAN_POINT('Ctrl Pts',(9.35827765375,-39.7742356128,-2.07942227767));
#77431=CARTESIAN_POINT('Ctrl Pts',(9.35827765375,-36.7742356128,-2.07942227767));
#77432=CARTESIAN_POINT('Ctrl Pts',(9.40334820731,-39.7742356128,-1.48595469944));
#77433=CARTESIAN_POINT('Ctrl Pts',(9.40334820731,-36.7742356128,-1.48595469944));
#77434=CARTESIAN_POINT('Ctrl Pts',(9.38724768323,-39.7742356128,-0.727182590117));
#77435=CARTESIAN_POINT('Ctrl Pts',(9.38724768323,-36.7742356128,-0.727182590117));
#77436=CARTESIAN_POINT('Ctrl Pts',(9.30567800741,-39.7742356128,0.0234614864805));
#77437=CARTESIAN_POINT('Ctrl Pts',(9.30567800741,-36.7742356128,0.0234614864805));
#77438=CARTESIAN_POINT('Ctrl Pts',(9.28522407236,-39.7742356128,0.186274742007));
#77439=CARTESIAN_POINT('Ctrl Pts',(9.28522407236,-36.7742356128,0.186274742007));
#77440=CARTESIAN_POINT('Ctrl Pts',(9.26229015361,-39.7742356128,0.348410633982));
#77441=CARTESIAN_POINT('Ctrl Pts',(9.26229015361,-36.7742356128,0.348410633982));
#77442=CARTESIAN_POINT('Ctrl Pts',(9.23698117862,-39.7742356128,0.509886547152));
#77443=CARTESIAN_POINT('Ctrl Pts',(9.23698117862,-36.7742356128,0.509886547152));
#77444=CARTESIAN_POINT('',(1.87043161062015,-37.2742356128,-8.24476960831419));
#77445=CARTESIAN_POINT('Ctrl Pts',(1.87043161102975,-37.2742356128,-8.24476960823859));
#77446=CARTESIAN_POINT('Ctrl Pts',(2.81841365854501,-37.2742356128,-8.07409211592585));
#77447=CARTESIAN_POINT('Ctrl Pts',(3.72902170121274,-37.2742356128,-7.80028819948638));
#77448=CARTESIAN_POINT('Ctrl Pts',(4.56766016677875,-37.2742356128,-7.42304518853861));
#77449=CARTESIAN_POINT('Ctrl Pts',(6.08851120928704,-37.2742356128,-6.51001025612548));
#77450=CARTESIAN_POINT('Ctrl Pts',(7.447100543,-37.2742356128,-5.31497212719));
#77451=CARTESIAN_POINT('Ctrl Pts',(8.1250786803,-37.2742356128,-4.64371494659));
#77452=CARTESIAN_POINT('Ctrl Pts',(8.99226462924,-37.2742356128,-3.46343233105));
#77453=CARTESIAN_POINT('Ctrl Pts',(9.35827765375,-37.2742356128,-2.07942227767));
#77454=CARTESIAN_POINT('Ctrl Pts',(9.40334820731,-37.2742356128,-1.48595469944));
#77455=CARTESIAN_POINT('Ctrl Pts',(9.38724768323,-37.2742356128,-0.727182590117));
#77456=CARTESIAN_POINT('Ctrl Pts',(9.30567800741,-37.2742356128,0.0234614864805));
#77457=CARTESIAN_POINT('Ctrl Pts',(9.28522407236,-37.2742356128,0.186274742007));
#77458=CARTESIAN_POINT('Ctrl Pts',(9.26229015361,-37.2742356128,0.348410633982));
#77459=CARTESIAN_POINT('Ctrl Pts',(9.23698117862229,-37.2742356128,0.509886547137359));
#77460=CARTESIAN_POINT('',(1.8704316098,-39.6642356128,-8.24476960846));
#77461=CARTESIAN_POINT('Origin',(1.81727342606,-37.6642356128,-7.9495168227));
#77462=CARTESIAN_POINT('',(1.51727342606,-37.2742356128,-7.9495168227));
#77463=CARTESIAN_POINT('Origin',(1.81727342606,-37.2742356128,-7.9495168227));
#77464=CARTESIAN_POINT('',(1.51727342606,-39.6642356128,-7.9495168227));
#77465=CARTESIAN_POINT('Origin',(1.51727342606,-39.2742356128,-5.3088808072));
#77466=CARTESIAN_POINT('',(1.51727342606,-37.2742356128,-5.3088808072));
#77467=CARTESIAN_POINT('',(1.51727342606,-37.2742356128,-6.62919881495));
#77468=CARTESIAN_POINT('',(1.51727342606,-38.5242356128,-5.3088808072));
#77469=CARTESIAN_POINT('Origin',(1.81727342606,-37.6642356128,-5.3088808072));
#77470=CARTESIAN_POINT('Origin',(1.81727342606,-37.2742356128,-5.3088808072));
#77471=CARTESIAN_POINT('Ctrl Pts',(-1.8704316098,-39.7742356128,-8.24476960846));
#77472=CARTESIAN_POINT('Ctrl Pts',(-1.8704316098,-36.7742356128,-8.24476960846));
#77473=CARTESIAN_POINT('Ctrl Pts',(-2.8184136576,-39.7742356128,-8.07409211621));
#77474=CARTESIAN_POINT('Ctrl Pts',(-2.8184136576,-36.7742356128,-8.07409211621));
#77475=CARTESIAN_POINT('Ctrl Pts',(-3.72902170056,-39.7742356128,-7.80028819978));
#77476=CARTESIAN_POINT('Ctrl Pts',(-3.72902170056,-36.7742356128,-7.80028819978));
#77477=CARTESIAN_POINT('Ctrl Pts',(-4.56766016636,-39.7742356128,-7.42304518879));
#77478=CARTESIAN_POINT('Ctrl Pts',(-4.56766016636,-36.7742356128,-7.42304518879));
#77479=CARTESIAN_POINT('Ctrl Pts',(-6.0885112091,-39.7742356128,-6.51001025629));
#77480=CARTESIAN_POINT('Ctrl Pts',(-6.0885112091,-36.7742356128,-6.51001025629));
#77481=CARTESIAN_POINT('Ctrl Pts',(-7.447100543,-39.7742356128,-5.31497212719));
#77482=CARTESIAN_POINT('Ctrl Pts',(-7.447100543,-36.7742356128,-5.31497212719));
#77483=CARTESIAN_POINT('Ctrl Pts',(-8.1250786803,-39.7742356128,-4.64371494659));
#77484=CARTESIAN_POINT('Ctrl Pts',(-8.1250786803,-36.7742356128,-4.64371494659));
#77485=CARTESIAN_POINT('Ctrl Pts',(-8.99226462924,-39.7742356128,-3.46343233105));
#77486=CARTESIAN_POINT('Ctrl Pts',(-8.99226462924,-36.7742356128,-3.46343233105));
#77487=CARTESIAN_POINT('Ctrl Pts',(-9.35827765375,-39.7742356128,-2.07942227767));
#77488=CARTESIAN_POINT('Ctrl Pts',(-9.35827765375,-36.7742356128,-2.07942227767));
#77489=CARTESIAN_POINT('Ctrl Pts',(-9.40334820731,-39.7742356128,-1.48595469944));
#77490=CARTESIAN_POINT('Ctrl Pts',(-9.40334820731,-36.7742356128,-1.48595469944));
#77491=CARTESIAN_POINT('Ctrl Pts',(-9.38724768323,-39.7742356128,-0.727182590117));
#77492=CARTESIAN_POINT('Ctrl Pts',(-9.38724768323,-36.7742356128,-0.727182590117));
#77493=CARTESIAN_POINT('Ctrl Pts',(-9.30567800741,-39.7742356128,0.0234614864805));
#77494=CARTESIAN_POINT('Ctrl Pts',(-9.30567800741,-36.7742356128,0.0234614864805));
#77495=CARTESIAN_POINT('Ctrl Pts',(-9.28522407236,-39.7742356128,0.186274742007));
#77496=CARTESIAN_POINT('Ctrl Pts',(-9.28522407236,-36.7742356128,0.186274742007));
#77497=CARTESIAN_POINT('Ctrl Pts',(-9.26229015361,-39.7742356128,0.348410633982));
#77498=CARTESIAN_POINT('Ctrl Pts',(-9.26229015361,-36.7742356128,0.348410633982));
#77499=CARTESIAN_POINT('Ctrl Pts',(-9.23698117862,-39.7742356128,0.509886547152));
#77500=CARTESIAN_POINT('Ctrl Pts',(-9.23698117862,-36.7742356128,0.509886547152));
#77501=CARTESIAN_POINT('',(-1.87043161062015,-37.2742356128,-8.24476960831419));
#77502=CARTESIAN_POINT('',(-9.23698117862,-37.2742356128,0.509886547152));
#77503=CARTESIAN_POINT('Ctrl Pts',(-1.87043161102975,-37.2742356128,-8.24476960823859));
#77504=CARTESIAN_POINT('Ctrl Pts',(-2.81841365854501,-37.2742356128,-8.07409211592585));
#77505=CARTESIAN_POINT('Ctrl Pts',(-3.72902170121274,-37.2742356128,-7.80028819948638));
#77506=CARTESIAN_POINT('Ctrl Pts',(-4.56766016677875,-37.2742356128,-7.42304518853861));
#77507=CARTESIAN_POINT('Ctrl Pts',(-6.08851120928704,-37.2742356128,-6.51001025612548));
#77508=CARTESIAN_POINT('Ctrl Pts',(-7.447100543,-37.2742356128,-5.31497212719));
#77509=CARTESIAN_POINT('Ctrl Pts',(-8.1250786803,-37.2742356128,-4.64371494659));
#77510=CARTESIAN_POINT('Ctrl Pts',(-8.99226462924,-37.2742356128,-3.46343233105));
#77511=CARTESIAN_POINT('Ctrl Pts',(-9.35827765375,-37.2742356128,-2.07942227767));
#77512=CARTESIAN_POINT('Ctrl Pts',(-9.40334820731,-37.2742356128,-1.48595469944));
#77513=CARTESIAN_POINT('Ctrl Pts',(-9.38724768323,-37.2742356128,-0.727182590117));
#77514=CARTESIAN_POINT('Ctrl Pts',(-9.30567800741,-37.2742356128,0.0234614864805));
#77515=CARTESIAN_POINT('Ctrl Pts',(-9.28522407236,-37.2742356128,0.186274742007));
#77516=CARTESIAN_POINT('Ctrl Pts',(-9.26229015361,-37.2742356128,0.348410633982));
#77517=CARTESIAN_POINT('Ctrl Pts',(-9.23698117862,-37.2742356128,0.509886547152));
#77518=CARTESIAN_POINT('',(-9.23698117862,-39.6642356128,0.509886547152));
#77519=CARTESIAN_POINT('',(-1.8704316098,-39.6642356128,-8.24476960846));
#77520=CARTESIAN_POINT('Ctrl Pts',(-3.51985615629,-39.7742356128,-3.20601908088));
#77521=CARTESIAN_POINT('Ctrl Pts',(-3.51985615629,-36.7742356128,-3.20601908088));
#77522=CARTESIAN_POINT('Ctrl Pts',(-3.35540949155,-39.7742356128,-3.54336911238));
#77523=CARTESIAN_POINT('Ctrl Pts',(-3.35540949155,-36.7742356128,-3.54336911238));
#77524=CARTESIAN_POINT('Ctrl Pts',(-3.15758359021,-39.7742356128,-3.85751660428));
#77525=CARTESIAN_POINT('Ctrl Pts',(-3.15758359021,-36.7742356128,-3.85751660428));
#77526=CARTESIAN_POINT('Ctrl Pts',(-2.92553217282,-39.7742356128,-4.14369667075));
#77527=CARTESIAN_POINT('Ctrl Pts',(-2.92553217282,-36.7742356128,-4.14369667075));
#77528=CARTESIAN_POINT('Ctrl Pts',(-2.54664760633,-39.7742356128,-4.50813716291));
#77529=CARTESIAN_POINT('Ctrl Pts',(-2.54664760633,-36.7742356128,-4.50813716291));
#77530=CARTESIAN_POINT('Ctrl Pts',(-2.10878664609,-39.7742356128,-4.80650592873));
#77531=CARTESIAN_POINT('Ctrl Pts',(-2.10878664609,-36.7742356128,-4.80650592873));
#77532=CARTESIAN_POINT('Ctrl Pts',(-1.97163547839,-39.7742356128,-4.89045414442));
#77533=CARTESIAN_POINT('Ctrl Pts',(-1.97163547839,-36.7742356128,-4.89045414442));
#77534=CARTESIAN_POINT('Ctrl Pts',(-1.8303523356,-39.7742356128,-4.96805050291));
#77535=CARTESIAN_POINT('Ctrl Pts',(-1.8303523356,-36.7742356128,-4.96805050291));
#77536=CARTESIAN_POINT('Ctrl Pts',(-1.68475792039,-39.7742356128,-5.03973467448));
#77537=CARTESIAN_POINT('Ctrl Pts',(-1.68475792039,-36.7742356128,-5.03973467448));
#77538=CARTESIAN_POINT('',(-3.51985615629,-37.2742356128,-3.20601908088));
#77539=CARTESIAN_POINT('',(-1.68475792039,-37.2742356128,-5.03973467448));
#77540=CARTESIAN_POINT('Ctrl Pts',(-3.51985615629,-37.2742356128,-3.20601908088));
#77541=CARTESIAN_POINT('Ctrl Pts',(-3.35540949155,-37.2742356128,-3.54336911238));
#77542=CARTESIAN_POINT('Ctrl Pts',(-3.15758359021,-37.2742356128,-3.85751660428));
#77543=CARTESIAN_POINT('Ctrl Pts',(-2.92553217282,-37.2742356128,-4.14369667075));
#77544=CARTESIAN_POINT('Ctrl Pts',(-2.54664760633,-37.2742356128,-4.50813716291));
#77545=CARTESIAN_POINT('Ctrl Pts',(-2.10878664609,-37.2742356128,-4.80650592873));
#77546=CARTESIAN_POINT('Ctrl Pts',(-1.97163547839,-37.2742356128,-4.89045414442));
#77547=CARTESIAN_POINT('Ctrl Pts',(-1.8303523356,-37.2742356128,-4.96805050291));
#77548=CARTESIAN_POINT('Ctrl Pts',(-1.68475792039,-37.2742356128,-5.03973467448));
#77549=CARTESIAN_POINT('',(-1.68475792039,-39.6642356128,-5.03973467448));
#77550=CARTESIAN_POINT('',(-3.51985615629,-39.6642356128,-3.20601908088));
#77551=CARTESIAN_POINT('Origin',(-1.81727342606,-37.6642356128,-5.3088808072));
#77552=CARTESIAN_POINT('',(-1.51727342606,-37.2742356128,-5.3088808072));
#77553=CARTESIAN_POINT('Origin',(-1.81727342606,-37.2742356128,-5.3088808072));
#77554=CARTESIAN_POINT('',(-1.51727342606,-39.6642356128,-5.3088808072));
#77555=CARTESIAN_POINT('Origin',(-1.51727342606,-39.2742356128,-5.3088808072));
#77556=CARTESIAN_POINT('',(-1.51727342606,-37.2742356128,-7.9495168227));
#77557=CARTESIAN_POINT('',(-1.51727342606,-37.2742356128,-6.62919881495));
#77558=CARTESIAN_POINT('',(-1.51727342606,-38.5242356128,-7.9495168227));
#77559=CARTESIAN_POINT('Origin',(-1.81727342606,-37.6642356128,-7.9495168227));
#77560=CARTESIAN_POINT('Origin',(-1.81727342606,-37.2742356128,-7.9495168227));
#77561=CARTESIAN_POINT('Origin',(-3.78952269078,-37.6642356128,-3.33747234321));
#77562=CARTESIAN_POINT('',(-3.67755401867,-37.2742356128,-3.05915055738));
#77563=CARTESIAN_POINT('Origin',(-3.78952269078,-37.2742356128,-3.33747234321));
#77564=CARTESIAN_POINT('',(-3.67755401867,-39.6642356128,-3.05915055738));
#77565=CARTESIAN_POINT('Ctrl Pts',(-7.07911993306,-39.7742356128,1.41233341424));
#77566=CARTESIAN_POINT('Ctrl Pts',(-7.07911993306,-36.7742356128,1.41233341424));
#77567=CARTESIAN_POINT('Ctrl Pts',(-7.03043912742,-39.7742356128,0.911971673481));
#77568=CARTESIAN_POINT('Ctrl Pts',(-7.03043912742,-36.7742356128,0.911971673481));
#77569=CARTESIAN_POINT('Ctrl Pts',(-6.93879090488,-39.7742356128,0.427451671407));
#77570=CARTESIAN_POINT('Ctrl Pts',(-6.93879090488,-36.7742356128,0.427451671407));
#77571=CARTESIAN_POINT('Ctrl Pts',(-6.79968866463,-39.7742356128,-0.0361534703089));
#77572=CARTESIAN_POINT('Ctrl Pts',(-6.79968866463,-36.7742356128,-0.0361534703089));
#77573=CARTESIAN_POINT('Ctrl Pts',(-6.4258973146,-39.7742356128,-0.894662603614));
#77574=CARTESIAN_POINT('Ctrl Pts',(-6.4258973146,-36.7742356128,-0.894662603614));
#77575=CARTESIAN_POINT('Ctrl Pts',(-5.86106085412,-39.7742356128,-1.62790491519));
#77576=CARTESIAN_POINT('Ctrl Pts',(-5.86106085412,-36.7742356128,-1.62790491519));
#77577=CARTESIAN_POINT('Ctrl Pts',(-5.53842443335,-39.7742356128,-1.95360958375));
#77578=CARTESIAN_POINT('Ctrl Pts',(-5.53842443335,-36.7742356128,-1.95360958375));
#77579=CARTESIAN_POINT('Ctrl Pts',(-4.98933040959,-39.7742356128,-2.39194593497));
#77580=CARTESIAN_POINT('Ctrl Pts',(-4.98933040959,-36.7742356128,-2.39194593497));
#77581=CARTESIAN_POINT('Ctrl Pts',(-4.36273333629,-39.7742356128,-2.74903878258));
#77582=CARTESIAN_POINT('Ctrl Pts',(-4.36273333629,-36.7742356128,-2.74903878258));
#77583=CARTESIAN_POINT('Ctrl Pts',(-4.14078300625,-39.7742356128,-2.86156599489));
#77584=CARTESIAN_POINT('Ctrl Pts',(-4.14078300625,-36.7742356128,-2.86156599489));
#77585=CARTESIAN_POINT('Ctrl Pts',(-3.91246466012,-39.7742356128,-2.96464616022));
#77586=CARTESIAN_POINT('Ctrl Pts',(-3.91246466012,-36.7742356128,-2.96464616022));
#77587=CARTESIAN_POINT('Ctrl Pts',(-3.67755401867,-39.7742356128,-3.05915055738));
#77588=CARTESIAN_POINT('Ctrl Pts',(-3.67755401867,-36.7742356128,-3.05915055738));
#77589=CARTESIAN_POINT('',(-7.07911993306,-37.2742356128,1.41233341424));
#77590=CARTESIAN_POINT('Ctrl Pts',(-7.07911993306,-37.2742356128,1.41233341424));
#77591=CARTESIAN_POINT('Ctrl Pts',(-7.03043912742,-37.2742356128,0.911971673481));
#77592=CARTESIAN_POINT('Ctrl Pts',(-6.93879090488,-37.2742356128,0.427451671407));
#77593=CARTESIAN_POINT('Ctrl Pts',(-6.79968866463,-37.2742356128,-0.0361534703089));
#77594=CARTESIAN_POINT('Ctrl Pts',(-6.4258973146,-37.2742356128,-0.894662603614));
#77595=CARTESIAN_POINT('Ctrl Pts',(-5.86106085412,-37.2742356128,-1.62790491519));
#77596=CARTESIAN_POINT('Ctrl Pts',(-5.53842443335,-37.2742356128,-1.95360958375));
#77597=CARTESIAN_POINT('Ctrl Pts',(-4.98933040959,-37.2742356128,-2.39194593497));
#77598=CARTESIAN_POINT('Ctrl Pts',(-4.36273333629,-37.2742356128,-2.74903878258));
#77599=CARTESIAN_POINT('Ctrl Pts',(-4.14078300625,-37.2742356128,-2.86156599489));
#77600=CARTESIAN_POINT('Ctrl Pts',(-3.91246466012,-37.2742356128,-2.96464616022));
#77601=CARTESIAN_POINT('Ctrl Pts',(-3.67755401867,-37.2742356128,-3.05915055738));
#77602=CARTESIAN_POINT('',(-7.07911993306,-39.6642356128,1.41233341424));
#77603=CARTESIAN_POINT('Ctrl Pts',(-8.75956299023,-39.7742356128,2.0634404101));
#77604=CARTESIAN_POINT('Ctrl Pts',(-8.75956299023,-36.7742356128,2.0634404101));
#77605=CARTESIAN_POINT('Ctrl Pts',(-8.92890465395,-39.7742356128,1.78598462948));
#77606=CARTESIAN_POINT('Ctrl Pts',(-8.92890465395,-36.7742356128,1.78598462948));
#77607=CARTESIAN_POINT('Ctrl Pts',(-9.07290910839,-39.7742356128,1.49306491902));
#77608=CARTESIAN_POINT('Ctrl Pts',(-9.07290910839,-36.7742356128,1.49306491902));
#77609=CARTESIAN_POINT('Ctrl Pts',(-9.12674985892,-39.7742356128,1.15064933619));
#77610=CARTESIAN_POINT('Ctrl Pts',(-9.12674985892,-36.7742356128,1.15064933619));
#77611=CARTESIAN_POINT('Ctrl Pts',(-9.18664865847,-39.7742356128,0.831017278591));
#77612=CARTESIAN_POINT('Ctrl Pts',(-9.18664865847,-36.7742356128,0.831017278591));
#77613=CARTESIAN_POINT('Ctrl Pts',(-9.23698117862,-39.7742356128,0.509886547137));
#77614=CARTESIAN_POINT('Ctrl Pts',(-9.23698117862,-36.7742356128,0.509886547137));
#77615=CARTESIAN_POINT('',(-8.75956299023,-37.2742356128,2.0634404101));
#77616=CARTESIAN_POINT('Ctrl Pts',(-8.75956299023,-37.2742356128,2.0634404101));
#77617=CARTESIAN_POINT('Ctrl Pts',(-8.92890465395,-37.2742356128,1.78598462948));
#77618=CARTESIAN_POINT('Ctrl Pts',(-9.07290910839,-37.2742356128,1.49306491902));
#77619=CARTESIAN_POINT('Ctrl Pts',(-9.12674985892,-37.2742356128,1.15064933619));
#77620=CARTESIAN_POINT('Ctrl Pts',(-9.18664865847,-37.2742356128,0.831017278591));
#77621=CARTESIAN_POINT('Ctrl Pts',(-9.23698117861771,-37.2742356128,0.509886547151641));
#77622=CARTESIAN_POINT('',(-8.75956299023,-39.6642356128,2.0634404101));
#77623=CARTESIAN_POINT('Ctrl Pts',(-8.75956299024,-39.7742356128,2.0634404101));
#77624=CARTESIAN_POINT('Ctrl Pts',(-8.75956299024,-36.7742356128,2.0634404101));
#77625=CARTESIAN_POINT('Ctrl Pts',(-8.67258032609,-39.7742356128,2.20595609378));
#77626=CARTESIAN_POINT('Ctrl Pts',(-8.67258032609,-36.7742356128,2.20595609378));
#77627=CARTESIAN_POINT('Ctrl Pts',(-8.57679326147,-39.7742356128,2.34786591099));
#77628=CARTESIAN_POINT('Ctrl Pts',(-8.57679326147,-36.7742356128,2.34786591099));
#77629=CARTESIAN_POINT('Ctrl Pts',(-8.46448329596,-39.7742356128,2.49604426586));
#77630=CARTESIAN_POINT('Ctrl Pts',(-8.46448329596,-36.7742356128,2.49604426586));
#77631=CARTESIAN_POINT('Ctrl Pts',(-8.27825186329,-39.7742356128,2.67220081215));
#77632=CARTESIAN_POINT('Ctrl Pts',(-8.27825186329,-36.7742356128,2.67220081215));
#77633=CARTESIAN_POINT('Ctrl Pts',(-8.05379939761,-39.7742356128,2.74035894609));
#77634=CARTESIAN_POINT('Ctrl Pts',(-8.05379939761,-36.7742356128,2.74035894609));
#77635=CARTESIAN_POINT('Ctrl Pts',(-7.9779370982,-39.7742356128,2.74765496713));
#77636=CARTESIAN_POINT('Ctrl Pts',(-7.9779370982,-36.7742356128,2.74765496713));
#77637=CARTESIAN_POINT('Ctrl Pts',(-7.82203636779,-39.7742356128,2.73225108729));
#77638=CARTESIAN_POINT('Ctrl Pts',(-7.82203636779,-36.7742356128,2.73225108729));
#77639=CARTESIAN_POINT('Ctrl Pts',(-7.67278421879,-39.7742356128,2.66639360485));
#77640=CARTESIAN_POINT('Ctrl Pts',(-7.67278421879,-36.7742356128,2.66639360485));
#77641=CARTESIAN_POINT('Ctrl Pts',(-7.59903734004,-39.7742356128,2.62164000818));
#77642=CARTESIAN_POINT('Ctrl Pts',(-7.59903734004,-36.7742356128,2.62164000818));
#77643=CARTESIAN_POINT('Ctrl Pts',(-7.46503014366,-39.7742356128,2.52047218586));
#77644=CARTESIAN_POINT('Ctrl Pts',(-7.46503014366,-36.7742356128,2.52047218586));
#77645=CARTESIAN_POINT('Ctrl Pts',(-7.35007323494,-39.7742356128,2.39634839519));
#77646=CARTESIAN_POINT('Ctrl Pts',(-7.35007323494,-36.7742356128,2.39634839519));
#77647=CARTESIAN_POINT('Ctrl Pts',(-7.29780025627,-39.7742356128,2.32993852802));
#77648=CARTESIAN_POINT('Ctrl Pts',(-7.29780025627,-36.7742356128,2.32993852802));
#77649=CARTESIAN_POINT('Ctrl Pts',(-7.25230657394,-39.7742356128,2.26107036804));
#77650=CARTESIAN_POINT('Ctrl Pts',(-7.25230657394,-36.7742356128,2.26107036804));
#77651=CARTESIAN_POINT('Ctrl Pts',(-7.21384189758,-39.7742356128,2.18958432614));
#77652=CARTESIAN_POINT('Ctrl Pts',(-7.21384189758,-36.7742356128,2.18958432614));
#77653=CARTESIAN_POINT('',(-7.21384189758,-37.2742356128,2.18958432614));
#77654=CARTESIAN_POINT('Ctrl Pts',(-8.75956299023,-37.2742356128,2.0634404101));
#77655=CARTESIAN_POINT('Ctrl Pts',(-8.67258032609,-37.2742356128,2.20595609378));
#77656=CARTESIAN_POINT('Ctrl Pts',(-8.57679326147,-37.2742356128,2.34786591099));
#77657=CARTESIAN_POINT('Ctrl Pts',(-8.46448329596,-37.2742356128,2.49604426586));
#77658=CARTESIAN_POINT('Ctrl Pts',(-8.27825186329,-37.2742356128,2.67220081215));
#77659=CARTESIAN_POINT('Ctrl Pts',(-8.05379939761,-37.2742356128,2.74035894609));
#77660=CARTESIAN_POINT('Ctrl Pts',(-7.9779370982,-37.2742356128,2.74765496713));
#77661=CARTESIAN_POINT('Ctrl Pts',(-7.82203636779,-37.2742356128,2.73225108729));
#77662=CARTESIAN_POINT('Ctrl Pts',(-7.67278421879,-37.2742356128,2.66639360485));
#77663=CARTESIAN_POINT('Ctrl Pts',(-7.59903734004,-37.2742356128,2.62164000818));
#77664=CARTESIAN_POINT('Ctrl Pts',(-7.46503014366,-37.2742356128,2.52047218586));
#77665=CARTESIAN_POINT('Ctrl Pts',(-7.35007323494,-37.2742356128,2.39634839519));
#77666=CARTESIAN_POINT('Ctrl Pts',(-7.29780025627,-37.2742356128,2.32993852802));
#77667=CARTESIAN_POINT('Ctrl Pts',(-7.25230657394,-37.2742356128,2.26107036804));
#77668=CARTESIAN_POINT('Ctrl Pts',(-7.21384189758,-37.2742356128,2.18958432614));
#77669=CARTESIAN_POINT('',(-7.21384189758,-39.6642356128,2.18958432614));
#77670=CARTESIAN_POINT('Ctrl Pts',(-7.21384189758,-39.7742356128,2.18958432614));
#77671=CARTESIAN_POINT('Ctrl Pts',(-7.21384189758,-36.7742356128,2.18958432614));
#77672=CARTESIAN_POINT('Ctrl Pts',(-7.13908599018,-39.7742356128,2.05065155888));
#77673=CARTESIAN_POINT('Ctrl Pts',(-7.13908599018,-36.7742356128,2.05065155888));
#77674=CARTESIAN_POINT('Ctrl Pts',(-7.08905059141,-39.7742356128,1.8984189694));
#77675=CARTESIAN_POINT('Ctrl Pts',(-7.08905059141,-36.7742356128,1.8984189694));
#77676=CARTESIAN_POINT('Ctrl Pts',(-7.1053290044,-39.7742356128,1.72681022597));
#77677=CARTESIAN_POINT('Ctrl Pts',(-7.1053290044,-36.7742356128,1.72681022597));
#77678=CARTESIAN_POINT('Ctrl Pts',(-7.09439724612,-39.7742356128,1.56936004643));
#77679=CARTESIAN_POINT('Ctrl Pts',(-7.09439724612,-36.7742356128,1.56936004643));
#77680=CARTESIAN_POINT('Ctrl Pts',(-7.07911993306,-39.7742356128,1.41233341424));
#77681=CARTESIAN_POINT('Ctrl Pts',(-7.07911993306,-36.7742356128,1.41233341424));
#77682=CARTESIAN_POINT('Ctrl Pts',(-7.21384189758,-37.2742356128,2.18958432614));
#77683=CARTESIAN_POINT('Ctrl Pts',(-7.13908599018,-37.2742356128,2.05065155888));
#77684=CARTESIAN_POINT('Ctrl Pts',(-7.08905059141,-37.2742356128,1.8984189694));
#77685=CARTESIAN_POINT('Ctrl Pts',(-7.1053290044,-37.2742356128,1.72681022597));
#77686=CARTESIAN_POINT('Ctrl Pts',(-7.09439724612,-37.2742356128,1.56936004643));
#77687=CARTESIAN_POINT('Ctrl Pts',(-7.07911993306,-37.2742356128,1.41233341424));
#77688=CARTESIAN_POINT('Ctrl Pts',(9.47221976654,-38.2742356128,2.49225909299));
#77689=CARTESIAN_POINT('Ctrl Pts',(9.47221976654,-37.0742356128,2.49225909299));
#77690=CARTESIAN_POINT('Ctrl Pts',(9.39947240551,-38.2742356128,2.61145111814));
#77691=CARTESIAN_POINT('Ctrl Pts',(9.39947240551,-37.0742356128,2.61145111814));
#77692=CARTESIAN_POINT('Ctrl Pts',(9.32101749845,-38.2742356128,2.73104611971));
#77693=CARTESIAN_POINT('Ctrl Pts',(9.32101749845,-37.0742356128,2.73104611971));
#77694=CARTESIAN_POINT('Ctrl Pts',(9.23447554945,-38.2742356128,2.85280836926));
#77695=CARTESIAN_POINT('Ctrl Pts',(9.23447554945,-37.0742356128,2.85280836926));
#77696=CARTESIAN_POINT('Ctrl Pts',(9.02906684789,-38.2742356128,3.10681559939));
#77697=CARTESIAN_POINT('Ctrl Pts',(9.02906684789,-37.0742356128,3.10681559939));
#77698=CARTESIAN_POINT('Ctrl Pts',(8.75253761634,-38.2742356128,3.33309151087));
#77699=CARTESIAN_POINT('Ctrl Pts',(8.75253761634,-37.0742356128,3.33309151087));
#77700=CARTESIAN_POINT('Ctrl Pts',(8.5879953064,-38.2742356128,3.43383230551));
#77701=CARTESIAN_POINT('Ctrl Pts',(8.5879953064,-37.0742356128,3.43383230551));
#77702=CARTESIAN_POINT('Ctrl Pts',(8.23034267354,-38.2742356128,3.56436456904));
#77703=CARTESIAN_POINT('Ctrl Pts',(8.23034267354,-37.0742356128,3.56436456904));
#77704=CARTESIAN_POINT('Ctrl Pts',(7.84867458413,-38.2742356128,3.56156543232));
#77705=CARTESIAN_POINT('Ctrl Pts',(7.84867458413,-37.0742356128,3.56156543232));
#77706=CARTESIAN_POINT('Ctrl Pts',(7.67119781066,-38.2742356128,3.52757441198));
#77707=CARTESIAN_POINT('Ctrl Pts',(7.67119781066,-37.0742356128,3.52757441198));
#77708=CARTESIAN_POINT('Ctrl Pts',(7.27066371621,-38.2742356128,3.38466568023));
#77709=CARTESIAN_POINT('Ctrl Pts',(7.27066371621,-37.0742356128,3.38466568023));
#77710=CARTESIAN_POINT('Ctrl Pts',(6.95203985001,-38.2742356128,3.13761299508));
#77711=CARTESIAN_POINT('Ctrl Pts',(6.95203985001,-37.0742356128,3.13761299508));
#77712=CARTESIAN_POINT('Ctrl Pts',(6.78734156337,-38.2742356128,2.96846990237));
#77713=CARTESIAN_POINT('Ctrl Pts',(6.78734156337,-37.0742356128,2.96846990237));
#77714=CARTESIAN_POINT('Ctrl Pts',(6.6484900876,-38.2742356128,2.78390759916));
#77715=CARTESIAN_POINT('Ctrl Pts',(6.6484900876,-37.0742356128,2.78390759916));
#77716=CARTESIAN_POINT('Ctrl Pts',(6.53914701908,-38.2742356128,2.5806950957));
#77717=CARTESIAN_POINT('Ctrl Pts',(6.53914701908,-37.0742356128,2.5806950957));
#77718=CARTESIAN_POINT('',(9.47221976654,-37.2742356128,2.49225909299));
#77719=CARTESIAN_POINT('',(9.47221976654,-37.6642356128,2.49225909299));
#77720=CARTESIAN_POINT('',(6.53914701908,-37.2742356128,2.5806950957));
#77721=CARTESIAN_POINT('Ctrl Pts',(9.47221976654,-37.2742356128,2.49225909299));
#77722=CARTESIAN_POINT('Ctrl Pts',(9.39947240551,-37.2742356128,2.61145111814));
#77723=CARTESIAN_POINT('Ctrl Pts',(9.32101749845,-37.2742356128,2.73104611971));
#77724=CARTESIAN_POINT('Ctrl Pts',(9.23447554945,-37.2742356128,2.85280836926));
#77725=CARTESIAN_POINT('Ctrl Pts',(9.02906684789,-37.2742356128,3.10681559939));
#77726=CARTESIAN_POINT('Ctrl Pts',(8.75253761634,-37.2742356128,3.33309151087));
#77727=CARTESIAN_POINT('Ctrl Pts',(8.5879953064,-37.2742356128,3.43383230551));
#77728=CARTESIAN_POINT('Ctrl Pts',(8.23034267354,-37.2742356128,3.56436456904));
#77729=CARTESIAN_POINT('Ctrl Pts',(7.84867458413,-37.2742356128,3.56156543232));
#77730=CARTESIAN_POINT('Ctrl Pts',(7.67119781066,-37.2742356128,3.52757441198));
#77731=CARTESIAN_POINT('Ctrl Pts',(7.27066371621,-37.2742356128,3.38466568023));
#77732=CARTESIAN_POINT('Ctrl Pts',(6.95203985001,-37.2742356128,3.13761299508));
#77733=CARTESIAN_POINT('Ctrl Pts',(6.78734156337,-37.2742356128,2.96846990237));
#77734=CARTESIAN_POINT('Ctrl Pts',(6.6484900876,-37.2742356128,2.78390759916));
#77735=CARTESIAN_POINT('Ctrl Pts',(6.53914701908,-37.2742356128,2.5806950957));
#77736=CARTESIAN_POINT('',(6.53914701908,-37.6642356128,2.5806950957));
#77737=CARTESIAN_POINT('Ctrl Pts',(6.53914701908,-38.2742356128,2.5806950957));
#77738=CARTESIAN_POINT('Ctrl Pts',(6.53914701908,-37.0742356128,2.5806950957));
#77739=CARTESIAN_POINT('Ctrl Pts',(5.92921620253,-38.2742356128,1.44714753899));
#77740=CARTESIAN_POINT('Ctrl Pts',(5.92921620253,-37.0742356128,1.44714753899));
#77741=CARTESIAN_POINT('Ctrl Pts',(6.2734552887,-38.2742356128,-0.199812643821));
#77742=CARTESIAN_POINT('Ctrl Pts',(6.2734552887,-37.0742356128,-0.199812643821));
#77743=CARTESIAN_POINT('Ctrl Pts',(4.66846608736,-38.2742356128,-1.09094389297));
#77744=CARTESIAN_POINT('Ctrl Pts',(4.66846608736,-37.0742356128,-1.09094389297));
#77745=CARTESIAN_POINT('Ctrl Pts',(3.58890539941,-38.2742356128,-1.81984798791));
#77746=CARTESIAN_POINT('Ctrl Pts',(3.58890539941,-37.0742356128,-1.81984798791));
#77747=CARTESIAN_POINT('Ctrl Pts',(2.42434411094,-38.2742356128,-2.36824808793));
#77748=CARTESIAN_POINT('Ctrl Pts',(2.42434411094,-37.0742356128,-2.36824808793));
#77749=CARTESIAN_POINT('',(2.42434411094,-37.2742356128,-2.36824808793));
#77750=CARTESIAN_POINT('Ctrl Pts',(6.53914701908,-37.2742356128,2.5806950957));
#77751=CARTESIAN_POINT('Ctrl Pts',(5.92921620253,-37.2742356128,1.44714753899));
#77752=CARTESIAN_POINT('Ctrl Pts',(6.2734552887,-37.2742356128,-0.199812643821));
#77753=CARTESIAN_POINT('Ctrl Pts',(4.66846608736,-37.2742356128,-1.09094389297));
#77754=CARTESIAN_POINT('Ctrl Pts',(3.58890539941,-37.2742356128,-1.81984798791));
#77755=CARTESIAN_POINT('Ctrl Pts',(2.42434411094,-37.2742356128,-2.36824808793));
#77756=CARTESIAN_POINT('',(2.42434411094,-37.6642356128,-2.36824808793));
#77757=CARTESIAN_POINT('Origin',(6.28286804938E-15,-37.6642356128,2.77999550541));
#77758=CARTESIAN_POINT('',(1.11895565834,-37.2742356128,-2.79941259037));
#77759=CARTESIAN_POINT('Origin',(6.28286804938E-15,-37.2742356128,2.77999550541));
#77760=CARTESIAN_POINT('',(1.11895565834,-37.6642356128,-2.79941259037));
#77761=CARTESIAN_POINT('Origin',(1.21727342606,-38.2742356128,-3.28965091665));
#77762=CARTESIAN_POINT('',(0.717273426056,-37.2742356128,-3.28965091665));
#77763=CARTESIAN_POINT('',(0.717273426056,-38.2742356128,-3.28965091665));
#77764=CARTESIAN_POINT('Origin',(1.21727342606,-37.2742356128,-3.28965091665));
#77765=CARTESIAN_POINT('Origin',(0.717273426056,-39.2742356128,-2.86512409447));
#77766=CARTESIAN_POINT('',(0.717273426055,-37.2742356128,-7.9495168227));
#77767=CARTESIAN_POINT('',(0.717273426056,-37.2742356128,-5.61958386968));
#77768=CARTESIAN_POINT('',(0.717273426056,-37.7742356128,-7.9495168227));
#77769=CARTESIAN_POINT('Origin',(1.81725567298,-37.6642356128,-7.94326730652));
#77770=CARTESIAN_POINT('',(2.02820898725,-37.2742356128,-9.02284995699));
#77771=CARTESIAN_POINT('',(2.02820898725,-37.6642356128,-9.02284995699));
#77772=CARTESIAN_POINT('Origin',(1.81725567298,-37.2742356128,-7.94326730652));
#77773=CARTESIAN_POINT('Origin',(2.60353620801,-38.2742356128,-11.9671662765));
#77774=CARTESIAN_POINT('',(2.06575948168,-37.2742356128,-9.01576047707));
#77775=CARTESIAN_POINT('Origin',(2.60353620801,-37.2742356128,-11.9671662765));
#77776=CARTESIAN_POINT('',(2.06575948168,-38.2742356128,-9.01576047707));
#77777=CARTESIAN_POINT('Ctrl Pts',(2.06575946829,-38.2742356128,-9.01576047951));
#77778=CARTESIAN_POINT('Ctrl Pts',(2.06575946829,-37.0742356128,-9.01576047951));
#77779=CARTESIAN_POINT('Ctrl Pts',(2.9672194554,-38.2742356128,-8.85150512783));
#77780=CARTESIAN_POINT('Ctrl Pts',(2.9672194554,-37.0742356128,-8.85150512783));
#77781=CARTESIAN_POINT('Ctrl Pts',(3.84599034531,-38.2742356128,-8.59864711683));
#77782=CARTESIAN_POINT('Ctrl Pts',(3.84599034531,-37.0742356128,-8.59864711683));
#77783=CARTESIAN_POINT('Ctrl Pts',(4.67357601438,-38.2742356128,-8.25401331235));
#77784=CARTESIAN_POINT('Ctrl Pts',(4.67357601438,-37.0742356128,-8.25401331235));
#77785=CARTESIAN_POINT('Ctrl Pts',(6.17345275231,-38.2742356128,-7.42645694938));
#77786=CARTESIAN_POINT('Ctrl Pts',(6.17345275231,-37.0742356128,-7.42645694938));
#77787=CARTESIAN_POINT('Ctrl Pts',(7.5161640814,-38.2742356128,-6.34532321195));
#77788=CARTESIAN_POINT('Ctrl Pts',(7.5161640814,-37.0742356128,-6.34532321195));
#77789=CARTESIAN_POINT('Ctrl Pts',(8.15806093588,-38.2742356128,-5.76170299258));
#77790=CARTESIAN_POINT('Ctrl Pts',(8.15806093588,-37.0742356128,-5.76170299258));
#77791=CARTESIAN_POINT('Ctrl Pts',(9.14108523272,-38.2742356128,-4.69984607968));
#77792=CARTESIAN_POINT('Ctrl Pts',(9.14108523272,-37.0742356128,-4.69984607968));
#77793=CARTESIAN_POINT('Ctrl Pts',(9.81302959348,-38.2742356128,-3.42961050122));
#77794=CARTESIAN_POINT('Ctrl Pts',(9.81302959348,-37.0742356128,-3.42961050122));
#77795=CARTESIAN_POINT('Ctrl Pts',(10.0098671635,-38.2742356128,-2.88411398337));
#77796=CARTESIAN_POINT('Ctrl Pts',(10.0098671635,-37.0742356128,-2.88411398337));
#77797=CARTESIAN_POINT('Ctrl Pts',(10.222733632,-38.2742356128,-1.82926592992));
#77798=CARTESIAN_POINT('Ctrl Pts',(10.222733632,-37.0742356128,-1.82926592992));
#77799=CARTESIAN_POINT('Ctrl Pts',(10.2199521215,-38.2742356128,-0.771812654558));
#77800=CARTESIAN_POINT('Ctrl Pts',(10.2199521215,-37.0742356128,-0.771812654558));
#77801=CARTESIAN_POINT('Ctrl Pts',(10.184046519,-38.2742356128,-0.287190507733));
#77802=CARTESIAN_POINT('Ctrl Pts',(10.184046519,-37.0742356128,-0.287190507733));
#77803=CARTESIAN_POINT('Ctrl Pts',(10.1298079404,-38.2742356128,0.182098137249));
#77804=CARTESIAN_POINT('Ctrl Pts',(10.1298079404,-37.0742356128,0.182098137249));
#77805=CARTESIAN_POINT('Ctrl Pts',(10.0571285787,-38.2742356128,0.645805825733));
#77806=CARTESIAN_POINT('Ctrl Pts',(10.0571285787,-37.0742356128,0.645805825733));
#77807=CARTESIAN_POINT('',(10.0571285787,-37.2742356128,0.645805825719));
#77808=CARTESIAN_POINT('Ctrl Pts',(2.06575948168004,-37.2742356128,-9.0157604770702));
#77809=CARTESIAN_POINT('Ctrl Pts',(2.96721946584242,-37.2742356128,-8.8515051248253));
#77810=CARTESIAN_POINT('Ctrl Pts',(3.84599035268564,-37.2742356128,-8.59864711375854));
#77811=CARTESIAN_POINT('Ctrl Pts',(4.67357601907077,-37.2742356128,-8.25401330976187));
#77812=CARTESIAN_POINT('Ctrl Pts',(6.17345275440962,-37.2742356128,-7.42645694768941));
#77813=CARTESIAN_POINT('Ctrl Pts',(7.5161640814,-37.2742356128,-6.34532321195));
#77814=CARTESIAN_POINT('Ctrl Pts',(8.15806093588,-37.2742356128,-5.76170299258));
#77815=CARTESIAN_POINT('Ctrl Pts',(9.14108523272,-37.2742356128,-4.69984607968));
#77816=CARTESIAN_POINT('Ctrl Pts',(9.81302959348,-37.2742356128,-3.42961050122));
#77817=CARTESIAN_POINT('Ctrl Pts',(10.0098671635,-37.2742356128,-2.88411398337));
#77818=CARTESIAN_POINT('Ctrl Pts',(10.222733632,-37.2742356128,-1.82926592992));
#77819=CARTESIAN_POINT('Ctrl Pts',(10.2199521215,-37.2742356128,-0.771812654558));
#77820=CARTESIAN_POINT('Ctrl Pts',(10.184046519,-37.2742356128,-0.287190507733));
#77821=CARTESIAN_POINT('Ctrl Pts',(10.1298079404,-37.2742356128,0.182098137249));
#77822=CARTESIAN_POINT('Ctrl Pts',(10.0571285787022,-37.2742356128,0.645805825719337));
#77823=CARTESIAN_POINT('',(10.0571285787,-37.6642356128,0.645805825719));
#77824=CARTESIAN_POINT('Ctrl Pts',(9.47221976654,-38.2742356128,2.49225909299));
#77825=CARTESIAN_POINT('Ctrl Pts',(9.47221976654,-37.0742356128,2.49225909299));
#77826=CARTESIAN_POINT('Ctrl Pts',(9.54575444005,-38.2742356128,2.3717771053));
#77827=CARTESIAN_POINT('Ctrl Pts',(9.54575444005,-37.0742356128,2.3717771053));
#77828=CARTESIAN_POINT('Ctrl Pts',(9.61961951766,-38.2742356128,2.24151541202));
#77829=CARTESIAN_POINT('Ctrl Pts',(9.61961951766,-37.0742356128,2.24151541202));
#77830=CARTESIAN_POINT('Ctrl Pts',(9.68609489427,-38.2742356128,2.10542437124));
#77831=CARTESIAN_POINT('Ctrl Pts',(9.68609489427,-37.0742356128,2.10542437124));
#77832=CARTESIAN_POINT('Ctrl Pts',(9.84457330898,-38.2742356128,1.72211870919));
#77833=CARTESIAN_POINT('Ctrl Pts',(9.84457330898,-37.0742356128,1.72211870919));
#77834=CARTESIAN_POINT('Ctrl Pts',(9.94207621049,-38.2742356128,1.33157301839));
#77835=CARTESIAN_POINT('Ctrl Pts',(9.94207621049,-37.0742356128,1.33157301839));
#77836=CARTESIAN_POINT('Ctrl Pts',(9.98299011243,-38.2742356128,1.0898271634));
#77837=CARTESIAN_POINT('Ctrl Pts',(9.98299011243,-37.0742356128,1.0898271634));
#77838=CARTESIAN_POINT('Ctrl Pts',(10.0216701384,-38.2742356128,0.872037193625));
#77839=CARTESIAN_POINT('Ctrl Pts',(10.0216701384,-37.0742356128,0.872037193625));
#77840=CARTESIAN_POINT('Ctrl Pts',(10.0571285787,-38.2742356128,0.645805825719));
#77841=CARTESIAN_POINT('Ctrl Pts',(10.0571285787,-37.0742356128,0.645805825719));
#77842=CARTESIAN_POINT('Ctrl Pts',(9.47221976654,-37.2742356128,2.49225909299));
#77843=CARTESIAN_POINT('Ctrl Pts',(9.54575444005,-37.2742356128,2.3717771053));
#77844=CARTESIAN_POINT('Ctrl Pts',(9.61961951766,-37.2742356128,2.24151541202));
#77845=CARTESIAN_POINT('Ctrl Pts',(9.68609489427,-37.2742356128,2.10542437124));
#77846=CARTESIAN_POINT('Ctrl Pts',(9.84457330898,-37.2742356128,1.72211870919));
#77847=CARTESIAN_POINT('Ctrl Pts',(9.94207621049,-37.2742356128,1.33157301839));
#77848=CARTESIAN_POINT('Ctrl Pts',(9.98299011243,-37.2742356128,1.0898271634));
#77849=CARTESIAN_POINT('Ctrl Pts',(10.0216701384,-37.2742356128,0.872037193625));
#77850=CARTESIAN_POINT('Ctrl Pts',(10.0571285787,-37.2742356128,0.645805825719));
#77851=CARTESIAN_POINT('Ctrl Pts',(-5.2400559546,-38.2742356128,5.59690998219));
#77852=CARTESIAN_POINT('Ctrl Pts',(-5.2400559546,-37.0742356128,5.59690998219));
#77853=CARTESIAN_POINT('Ctrl Pts',(-5.25990082634,-38.2742356128,5.0059883748));
#77854=CARTESIAN_POINT('Ctrl Pts',(-5.25990082634,-37.0742356128,5.0059883748));
#77855=CARTESIAN_POINT('Ctrl Pts',(-5.23061607717,-38.2742356128,4.36229648927));
#77856=CARTESIAN_POINT('Ctrl Pts',(-5.23061607717,-37.0742356128,4.36229648927));
#77857=CARTESIAN_POINT('Ctrl Pts',(-5.00490058958,-38.2742356128,3.77298874453));
#77858=CARTESIAN_POINT('Ctrl Pts',(-5.00490058958,-37.0742356128,3.77298874453));
#77859=CARTESIAN_POINT('Ctrl Pts',(-4.75506448705,-38.2742356128,3.08655684628));
#77860=CARTESIAN_POINT('Ctrl Pts',(-4.75506448705,-37.0742356128,3.08655684628));
#77861=CARTESIAN_POINT('Ctrl Pts',(-4.54755634075,-38.2742356128,2.39287258614));
#77862=CARTESIAN_POINT('Ctrl Pts',(-4.54755634075,-37.0742356128,2.39287258614));
#77863=CARTESIAN_POINT('Ctrl Pts',(-4.4987250478,-38.2742356128,2.21955031284));
#77864=CARTESIAN_POINT('Ctrl Pts',(-4.4987250478,-37.0742356128,2.21955031284));
#77865=CARTESIAN_POINT('Ctrl Pts',(-4.44893332626,-38.2742356128,2.04003858973));
#77866=CARTESIAN_POINT('Ctrl Pts',(-4.44893332626,-37.0742356128,2.04003858973));
#77867=CARTESIAN_POINT('Ctrl Pts',(-4.39152710765,-38.2742356128,1.85538989834));
#77868=CARTESIAN_POINT('Ctrl Pts',(-4.39152710765,-37.0742356128,1.85538989834));
#77869=CARTESIAN_POINT('',(-4.39152710765,-37.6642356128,1.85538989834));
#77870=CARTESIAN_POINT('',(-5.2400559546,-37.6642356128,5.59690998219));
#77871=CARTESIAN_POINT('Ctrl Pts',(-0.605290084206,-38.2742356128,-1.95105924441));
#77872=CARTESIAN_POINT('Ctrl Pts',(-0.605290084206,-37.0742356128,-1.95105924441));
#77873=CARTESIAN_POINT('Ctrl Pts',(-0.774096521679,-38.2742356128,-1.91628513625));
#77874=CARTESIAN_POINT('Ctrl Pts',(-0.774096521679,-37.0742356128,-1.91628513625));
#77875=CARTESIAN_POINT('Ctrl Pts',(-0.942624183674,-38.2742356128,-1.87619510128));
#77876=CARTESIAN_POINT('Ctrl Pts',(-0.942624183674,-37.0742356128,-1.87619510128));
#77877=CARTESIAN_POINT('Ctrl Pts',(-1.11061388614,-38.2742356128,-1.83037525603));
#77878=CARTESIAN_POINT('Ctrl Pts',(-1.11061388614,-37.0742356128,-1.83037525603));
#77879=CARTESIAN_POINT('Ctrl Pts',(-1.74274860628,-38.2742356128,-1.63293852912));
#77880=CARTESIAN_POINT('Ctrl Pts',(-1.74274860628,-37.0742356128,-1.63293852912));
#77881=CARTESIAN_POINT('Ctrl Pts',(-2.34679547467,-38.2742356128,-1.33257881069));
#77882=CARTESIAN_POINT('Ctrl Pts',(-2.34679547467,-37.0742356128,-1.33257881069));
#77883=CARTESIAN_POINT('Ctrl Pts',(-2.73083933763,-38.2742356128,-1.04090474176));
#77884=CARTESIAN_POINT('Ctrl Pts',(-2.73083933763,-37.0742356128,-1.04090474176));
#77885=CARTESIAN_POINT('Ctrl Pts',(-3.39638296129,-38.2742356128,-0.293897533174));
#77886=CARTESIAN_POINT('Ctrl Pts',(-3.39638296129,-37.0742356128,-0.293897533174));
#77887=CARTESIAN_POINT('Ctrl Pts',(-3.86916001537,-38.2742356128,0.542814468562));
#77888=CARTESIAN_POINT('Ctrl Pts',(-3.86916001537,-37.0742356128,0.542814468562));
#77889=CARTESIAN_POINT('Ctrl Pts',(-4.06911877342,-38.2742356128,0.942104314053));
#77890=CARTESIAN_POINT('Ctrl Pts',(-4.06911877342,-37.0742356128,0.942104314053));
#77891=CARTESIAN_POINT('Ctrl Pts',(-4.24744781279,-38.2742356128,1.39201586348));
#77892=CARTESIAN_POINT('Ctrl Pts',(-4.24744781279,-37.0742356128,1.39201586348));
#77893=CARTESIAN_POINT('Ctrl Pts',(-4.39143626207,-38.2742356128,1.85509771049));
#77894=CARTESIAN_POINT('Ctrl Pts',(-4.39143626207,-37.0742356128,1.85509771049));
#77895=CARTESIAN_POINT('Ctrl Pts',(-4.39145443226365,-38.2742356128,1.85515614772492));
#77896=CARTESIAN_POINT('Ctrl Pts',(-4.39145443226365,-37.0742356128,1.85515614772492));
#77897=CARTESIAN_POINT('Ctrl Pts',(-4.3914726024573,-38.2742356128,1.85521458495984));
#77898=CARTESIAN_POINT('Ctrl Pts',(-4.3914726024573,-37.0742356128,1.85521458495984));
#77899=CARTESIAN_POINT('Ctrl Pts',(-4.39149077265095,-38.2742356128,1.85527302219476));
#77900=CARTESIAN_POINT('Ctrl Pts',(-4.39149077265095,-37.0742356128,1.85527302219476));
#77901=CARTESIAN_POINT('Ctrl Pts',(-4.3915089428446,-38.2742356128,1.85533145942968));
#77902=CARTESIAN_POINT('Ctrl Pts',(-4.3915089428446,-37.0742356128,1.85533145942968));
#77903=CARTESIAN_POINT('Ctrl Pts',(-4.39152711303826,-38.2742356128,1.8553898966646));
#77904=CARTESIAN_POINT('Ctrl Pts',(-4.39152711303826,-37.0742356128,1.8553898966646));
#77905=CARTESIAN_POINT('',(-0.605290084208,-37.6642356128,-1.95105924441));
#77906=CARTESIAN_POINT('Origin',(1.44440015504E-13,-38.2742356128,0.987243652491));
#77907=CARTESIAN_POINT('',(0.605290084208,-38.2742356128,-1.95105924441));
#77908=CARTESIAN_POINT('Ctrl Pts',(0.605290084206,-38.2742356128,-1.95105924441));
#77909=CARTESIAN_POINT('Ctrl Pts',(0.605290084206,-37.0742356128,-1.95105924441));
#77910=CARTESIAN_POINT('Ctrl Pts',(0.774096521679,-38.2742356128,-1.91628513625));
#77911=CARTESIAN_POINT('Ctrl Pts',(0.774096521679,-37.0742356128,-1.91628513625));
#77912=CARTESIAN_POINT('Ctrl Pts',(0.942624183674,-38.2742356128,-1.87619510128));
#77913=CARTESIAN_POINT('Ctrl Pts',(0.942624183674,-37.0742356128,-1.87619510128));
#77914=CARTESIAN_POINT('Ctrl Pts',(1.11061388614,-38.2742356128,-1.83037525603));
#77915=CARTESIAN_POINT('Ctrl Pts',(1.11061388614,-37.0742356128,-1.83037525603));
#77916=CARTESIAN_POINT('Ctrl Pts',(1.74274860628,-38.2742356128,-1.63293852912));
#77917=CARTESIAN_POINT('Ctrl Pts',(1.74274860628,-37.0742356128,-1.63293852912));
#77918=CARTESIAN_POINT('Ctrl Pts',(2.34679547467,-38.2742356128,-1.33257881069));
#77919=CARTESIAN_POINT('Ctrl Pts',(2.34679547467,-37.0742356128,-1.33257881069));
#77920=CARTESIAN_POINT('Ctrl Pts',(2.73083933763,-38.2742356128,-1.04090474176));
#77921=CARTESIAN_POINT('Ctrl Pts',(2.73083933763,-37.0742356128,-1.04090474176));
#77922=CARTESIAN_POINT('Ctrl Pts',(3.39635927668,-38.2742356128,-0.29392411682));
#77923=CARTESIAN_POINT('Ctrl Pts',(3.39635927668,-37.0742356128,-0.29392411682));
#77924=CARTESIAN_POINT('Ctrl Pts',(3.86912636582,-38.2742356128,0.542754916759));
#77925=CARTESIAN_POINT('Ctrl Pts',(3.86912636582,-37.0742356128,0.542754916759));
#77926=CARTESIAN_POINT('Ctrl Pts',(4.06899942193,-38.2742356128,0.941795900815));
#77927=CARTESIAN_POINT('Ctrl Pts',(4.06899942193,-37.0742356128,0.941795900815));
#77928=CARTESIAN_POINT('Ctrl Pts',(4.2473975181,-38.2742356128,1.39188897252));
#77929=CARTESIAN_POINT('Ctrl Pts',(4.2473975181,-37.0742356128,1.39188897252));
#77930=CARTESIAN_POINT('Ctrl Pts',(4.39138551009,-38.2742356128,1.854934493));
#77931=CARTESIAN_POINT('Ctrl Pts',(4.39138551009,-37.0742356128,1.854934493));
#77932=CARTESIAN_POINT('',(4.39138551009,-37.6642356128,1.854934493));
#77933=CARTESIAN_POINT('Ctrl Pts',(5.2400559546,-38.2742356128,5.59690998219));
#77934=CARTESIAN_POINT('Ctrl Pts',(5.2400559546,-37.0742356128,5.59690998219));
#77935=CARTESIAN_POINT('Ctrl Pts',(5.25990082634,-38.2742356128,5.0059883748));
#77936=CARTESIAN_POINT('Ctrl Pts',(5.25990082634,-37.0742356128,5.0059883748));
#77937=CARTESIAN_POINT('Ctrl Pts',(5.23061607717,-38.2742356128,4.36229648927));
#77938=CARTESIAN_POINT('Ctrl Pts',(5.23061607717,-37.0742356128,4.36229648927));
#77939=CARTESIAN_POINT('Ctrl Pts',(5.00490058958,-38.2742356128,3.77298874453));
#77940=CARTESIAN_POINT('Ctrl Pts',(5.00490058958,-37.0742356128,3.77298874453));
#77941=CARTESIAN_POINT('Ctrl Pts',(4.75506448705,-38.2742356128,3.08655684628));
#77942=CARTESIAN_POINT('Ctrl Pts',(4.75506448705,-37.0742356128,3.08655684628));
#77943=CARTESIAN_POINT('Ctrl Pts',(4.54755634075,-38.2742356128,2.39287258614));
#77944=CARTESIAN_POINT('Ctrl Pts',(4.54755634075,-37.0742356128,2.39287258614));
#77945=CARTESIAN_POINT('Ctrl Pts',(4.4987250478,-38.2742356128,2.21955031284));
#77946=CARTESIAN_POINT('Ctrl Pts',(4.4987250478,-37.0742356128,2.21955031284));
#77947=CARTESIAN_POINT('Ctrl Pts',(4.44893332626,-38.2742356128,2.04003858973));
#77948=CARTESIAN_POINT('Ctrl Pts',(4.44893332626,-37.0742356128,2.04003858973));
#77949=CARTESIAN_POINT('Ctrl Pts',(4.39152710765,-38.2742356128,1.85538989834));
#77950=CARTESIAN_POINT('Ctrl Pts',(4.39152710765,-37.0742356128,1.85538989834));
#77951=CARTESIAN_POINT('Ctrl Pts',(4.3914987908103,-38.2742356128,1.8552988164412));
#77952=CARTESIAN_POINT('Ctrl Pts',(4.3914987908103,-37.0742356128,1.8552988164412));
#77953=CARTESIAN_POINT('Ctrl Pts',(4.39147047397061,-38.2742356128001,1.85520773454239));
#77954=CARTESIAN_POINT('Ctrl Pts',(4.39147047397061,-37.0742356128,1.85520773454239));
#77955=CARTESIAN_POINT('Ctrl Pts',(4.39144215713091,-38.2742356128001,1.85511665264359));
#77956=CARTESIAN_POINT('Ctrl Pts',(4.39144215713091,-37.0742356128,1.85511665264359));
#77957=CARTESIAN_POINT('Ctrl Pts',(4.39141384029122,-38.2742356128001,1.85502557074478));
#77958=CARTESIAN_POINT('Ctrl Pts',(4.39141384029122,-37.0742356128,1.85502557074478));
#77959=CARTESIAN_POINT('Ctrl Pts',(4.39138552345152,-38.2742356128001,1.85493448884598));
#77960=CARTESIAN_POINT('Ctrl Pts',(4.39138552345152,-37.0742356128,1.85493448884598));
#77961=CARTESIAN_POINT('',(5.2400559546,-37.6642356128,5.59690998219));
#77962=CARTESIAN_POINT('Origin',(-0.000416107150126,-37.6642356128,5.42091963994));
#77963=CARTESIAN_POINT('',(-7.34769233304E-15,-37.6642356128,10.664345987));
#77964=CARTESIAN_POINT('Origin',(0.000416107150126,-37.6642356128,5.42091963994));
#77965=CARTESIAN_POINT('Origin',(-2.60353620801,-38.2742356128,-11.9671662765));
#77966=CARTESIAN_POINT('',(-2.02820898725,-37.2742356128,-9.02284995699));
#77967=CARTESIAN_POINT('',(-2.06575948168,-37.2742356128,-9.01576047707));
#77968=CARTESIAN_POINT('Origin',(-2.60353620801,-37.2742356128,-11.9671662765));
#77969=CARTESIAN_POINT('',(-2.02820898726,-38.2742356128,-9.02284995699));
#77970=CARTESIAN_POINT('',(-2.06575948168,-38.2742356128,-9.01576047707));
#77971=CARTESIAN_POINT('Origin',(-1.81725567298,-37.6642356128,-7.94326730652));
#77972=CARTESIAN_POINT('',(-0.717273426055,-37.2742356128,-7.9495168227));
#77973=CARTESIAN_POINT('Origin',(-1.81725567298,-37.2742356128,-7.94326730652));
#77974=CARTESIAN_POINT('',(-0.717273426055,-37.6642356128,-7.9495168227));
#77975=CARTESIAN_POINT('Origin',(-0.717273426056,-39.2742356128,-2.86512409447));
#77976=CARTESIAN_POINT('',(-0.717273426056,-37.2742356128,-3.28965091665));
#77977=CARTESIAN_POINT('',(-0.717273426056,-37.2742356128,-5.61958386968));
#77978=CARTESIAN_POINT('',(-0.717273426056,-37.7742356128,-3.28965091665));
#77979=CARTESIAN_POINT('Origin',(-1.21727342606,-38.2742356128,-3.28965091665));
#77980=CARTESIAN_POINT('',(-1.11895565834,-37.2742356128,-2.79941259037));
#77981=CARTESIAN_POINT('Origin',(-1.21727342606,-37.2742356128,-3.28965091665));
#77982=CARTESIAN_POINT('',(-1.11895565834,-38.2742356128,-2.79941259037));
#77983=CARTESIAN_POINT('Origin',(-6.28286804938E-15,-37.6642356128,2.77999550541));
#77984=CARTESIAN_POINT('',(-2.42434411094,-37.2742356128,-2.36824808793));
#77985=CARTESIAN_POINT('Origin',(-6.28286804938E-15,-37.2742356128,2.77999550541));
#77986=CARTESIAN_POINT('',(-2.42434411094,-37.6642356128,-2.36824808793));
#77987=CARTESIAN_POINT('Ctrl Pts',(-6.53914701908,-38.2742356128,2.5806950957));
#77988=CARTESIAN_POINT('Ctrl Pts',(-6.53914701908,-37.0742356128,2.5806950957));
#77989=CARTESIAN_POINT('Ctrl Pts',(-5.92921620253,-38.2742356128,1.44714753899));
#77990=CARTESIAN_POINT('Ctrl Pts',(-5.92921620253,-37.0742356128,1.44714753899));
#77991=CARTESIAN_POINT('Ctrl Pts',(-6.2734552887,-38.2742356128,-0.199812643821));
#77992=CARTESIAN_POINT('Ctrl Pts',(-6.2734552887,-37.0742356128,-0.199812643821));
#77993=CARTESIAN_POINT('Ctrl Pts',(-4.66846608736,-38.2742356128,-1.09094389297));
#77994=CARTESIAN_POINT('Ctrl Pts',(-4.66846608736,-37.0742356128,-1.09094389297));
#77995=CARTESIAN_POINT('Ctrl Pts',(-3.58890539941,-38.2742356128,-1.81984798791));
#77996=CARTESIAN_POINT('Ctrl Pts',(-3.58890539941,-37.0742356128,-1.81984798791));
#77997=CARTESIAN_POINT('Ctrl Pts',(-2.42434411094,-38.2742356128,-2.36824808793));
#77998=CARTESIAN_POINT('Ctrl Pts',(-2.42434411094,-37.0742356128,-2.36824808793));
#77999=CARTESIAN_POINT('',(-6.53914701908,-37.2742356128,2.5806950957));
#78000=CARTESIAN_POINT('Ctrl Pts',(-6.53914701908,-37.2742356128,2.5806950957));
#78001=CARTESIAN_POINT('Ctrl Pts',(-5.92921620253,-37.2742356128,1.44714753899));
#78002=CARTESIAN_POINT('Ctrl Pts',(-6.2734552887,-37.2742356128,-0.199812643821));
#78003=CARTESIAN_POINT('Ctrl Pts',(-4.66846608736,-37.2742356128,-1.09094389297));
#78004=CARTESIAN_POINT('Ctrl Pts',(-3.58890539941,-37.2742356128,-1.81984798791));
#78005=CARTESIAN_POINT('Ctrl Pts',(-2.42434411094,-37.2742356128,-2.36824808793));
#78006=CARTESIAN_POINT('',(-6.53914701908,-37.6642356128,2.5806950957));
#78007=CARTESIAN_POINT('Ctrl Pts',(-9.47221976654,-38.2742356128,2.49225909299));
#78008=CARTESIAN_POINT('Ctrl Pts',(-9.47221976654,-37.0742356128,2.49225909299));
#78009=CARTESIAN_POINT('Ctrl Pts',(-9.39947240551,-38.2742356128,2.61145111814));
#78010=CARTESIAN_POINT('Ctrl Pts',(-9.39947240551,-37.0742356128,2.61145111814));
#78011=CARTESIAN_POINT('Ctrl Pts',(-9.32101749845,-38.2742356128,2.73104611971));
#78012=CARTESIAN_POINT('Ctrl Pts',(-9.32101749845,-37.0742356128,2.73104611971));
#78013=CARTESIAN_POINT('Ctrl Pts',(-9.23447554945,-38.2742356128,2.85280836926));
#78014=CARTESIAN_POINT('Ctrl Pts',(-9.23447554945,-37.0742356128,2.85280836926));
#78015=CARTESIAN_POINT('Ctrl Pts',(-9.02906684789,-38.2742356128,3.10681559939));
#78016=CARTESIAN_POINT('Ctrl Pts',(-9.02906684789,-37.0742356128,3.10681559939));
#78017=CARTESIAN_POINT('Ctrl Pts',(-8.75253761634,-38.2742356128,3.33309151087));
#78018=CARTESIAN_POINT('Ctrl Pts',(-8.75253761634,-37.0742356128,3.33309151087));
#78019=CARTESIAN_POINT('Ctrl Pts',(-8.5879953064,-38.2742356128,3.43383230551));
#78020=CARTESIAN_POINT('Ctrl Pts',(-8.5879953064,-37.0742356128,3.43383230551));
#78021=CARTESIAN_POINT('Ctrl Pts',(-8.23034267354,-38.2742356128,3.56436456904));
#78022=CARTESIAN_POINT('Ctrl Pts',(-8.23034267354,-37.0742356128,3.56436456904));
#78023=CARTESIAN_POINT('Ctrl Pts',(-7.84867458413,-38.2742356128,3.56156543232));
#78024=CARTESIAN_POINT('Ctrl Pts',(-7.84867458413,-37.0742356128,3.56156543232));
#78025=CARTESIAN_POINT('Ctrl Pts',(-7.67119781066,-38.2742356128,3.52757441198));
#78026=CARTESIAN_POINT('Ctrl Pts',(-7.67119781066,-37.0742356128,3.52757441198));
#78027=CARTESIAN_POINT('Ctrl Pts',(-7.27066371621,-38.2742356128,3.38466568023));
#78028=CARTESIAN_POINT('Ctrl Pts',(-7.27066371621,-37.0742356128,3.38466568023));
#78029=CARTESIAN_POINT('Ctrl Pts',(-6.95203985001,-38.2742356128,3.13761299508));
#78030=CARTESIAN_POINT('Ctrl Pts',(-6.95203985001,-37.0742356128,3.13761299508));
#78031=CARTESIAN_POINT('Ctrl Pts',(-6.78734156337,-38.2742356128,2.96846990237));
#78032=CARTESIAN_POINT('Ctrl Pts',(-6.78734156337,-37.0742356128,2.96846990237));
#78033=CARTESIAN_POINT('Ctrl Pts',(-6.6484900876,-38.2742356128,2.78390759916));
#78034=CARTESIAN_POINT('Ctrl Pts',(-6.6484900876,-37.0742356128,2.78390759916));
#78035=CARTESIAN_POINT('Ctrl Pts',(-6.53914701908,-38.2742356128,2.5806950957));
#78036=CARTESIAN_POINT('Ctrl Pts',(-6.53914701908,-37.0742356128,2.5806950957));
#78037=CARTESIAN_POINT('',(-9.47221976654,-37.2742356128,2.49225909299));
#78038=CARTESIAN_POINT('Ctrl Pts',(-9.47221976654,-37.2742356128,2.49225909299));
#78039=CARTESIAN_POINT('Ctrl Pts',(-9.39947240551,-37.2742356128,2.61145111814));
#78040=CARTESIAN_POINT('Ctrl Pts',(-9.32101749845,-37.2742356128,2.73104611971));
#78041=CARTESIAN_POINT('Ctrl Pts',(-9.23447554945,-37.2742356128,2.85280836926));
#78042=CARTESIAN_POINT('Ctrl Pts',(-9.02906684789,-37.2742356128,3.10681559939));
#78043=CARTESIAN_POINT('Ctrl Pts',(-8.75253761634,-37.2742356128,3.33309151087));
#78044=CARTESIAN_POINT('Ctrl Pts',(-8.5879953064,-37.2742356128,3.43383230551));
#78045=CARTESIAN_POINT('Ctrl Pts',(-8.23034267354,-37.2742356128,3.56436456904));
#78046=CARTESIAN_POINT('Ctrl Pts',(-7.84867458413,-37.2742356128,3.56156543232));
#78047=CARTESIAN_POINT('Ctrl Pts',(-7.67119781066,-37.2742356128,3.52757441198));
#78048=CARTESIAN_POINT('Ctrl Pts',(-7.27066371621,-37.2742356128,3.38466568023));
#78049=CARTESIAN_POINT('Ctrl Pts',(-6.95203985001,-37.2742356128,3.13761299508));
#78050=CARTESIAN_POINT('Ctrl Pts',(-6.78734156337,-37.2742356128,2.96846990237));
#78051=CARTESIAN_POINT('Ctrl Pts',(-6.6484900876,-37.2742356128,2.78390759916));
#78052=CARTESIAN_POINT('Ctrl Pts',(-6.53914701908,-37.2742356128,2.5806950957));
#78053=CARTESIAN_POINT('',(-9.47221976654,-37.6642356128,2.49225909299));
#78054=CARTESIAN_POINT('Ctrl Pts',(-9.47221976654,-38.2742356128,2.49225909299));
#78055=CARTESIAN_POINT('Ctrl Pts',(-9.47221976654,-37.0742356128,2.49225909299));
#78056=CARTESIAN_POINT('Ctrl Pts',(-9.54575444005,-38.2742356128,2.3717771053));
#78057=CARTESIAN_POINT('Ctrl Pts',(-9.54575444005,-37.0742356128,2.3717771053));
#78058=CARTESIAN_POINT('Ctrl Pts',(-9.61961951766,-38.2742356128,2.24151541202));
#78059=CARTESIAN_POINT('Ctrl Pts',(-9.61961951766,-37.0742356128,2.24151541202));
#78060=CARTESIAN_POINT('Ctrl Pts',(-9.68609489427,-38.2742356128,2.10542437124));
#78061=CARTESIAN_POINT('Ctrl Pts',(-9.68609489427,-37.0742356128,2.10542437124));
#78062=CARTESIAN_POINT('Ctrl Pts',(-9.84457330898,-38.2742356128,1.72211870919));
#78063=CARTESIAN_POINT('Ctrl Pts',(-9.84457330898,-37.0742356128,1.72211870919));
#78064=CARTESIAN_POINT('Ctrl Pts',(-9.94207621049,-38.2742356128,1.33157301839));
#78065=CARTESIAN_POINT('Ctrl Pts',(-9.94207621049,-37.0742356128,1.33157301839));
#78066=CARTESIAN_POINT('Ctrl Pts',(-9.98299011243,-38.2742356128,1.0898271634));
#78067=CARTESIAN_POINT('Ctrl Pts',(-9.98299011243,-37.0742356128,1.0898271634));
#78068=CARTESIAN_POINT('Ctrl Pts',(-10.0216701384,-38.2742356128,0.872037193625));
#78069=CARTESIAN_POINT('Ctrl Pts',(-10.0216701384,-37.0742356128,0.872037193625));
#78070=CARTESIAN_POINT('Ctrl Pts',(-10.0571285787,-38.2742356128,0.645805825719));
#78071=CARTESIAN_POINT('Ctrl Pts',(-10.0571285787,-37.0742356128,0.645805825719));
#78072=CARTESIAN_POINT('',(-10.0571285787,-37.2742356128,0.645805825719));
#78073=CARTESIAN_POINT('Ctrl Pts',(-9.47221976654,-37.2742356128,2.49225909299));
#78074=CARTESIAN_POINT('Ctrl Pts',(-9.54575444005,-37.2742356128,2.3717771053));
#78075=CARTESIAN_POINT('Ctrl Pts',(-9.61961951766,-37.2742356128,2.24151541202));
#78076=CARTESIAN_POINT('Ctrl Pts',(-9.68609489427,-37.2742356128,2.10542437124));
#78077=CARTESIAN_POINT('Ctrl Pts',(-9.84457330898,-37.2742356128,1.72211870919));
#78078=CARTESIAN_POINT('Ctrl Pts',(-9.94207621049,-37.2742356128,1.33157301839));
#78079=CARTESIAN_POINT('Ctrl Pts',(-9.98299011243,-37.2742356128,1.0898271634));
#78080=CARTESIAN_POINT('Ctrl Pts',(-10.0216701384,-37.2742356128,0.872037193625));
#78081=CARTESIAN_POINT('Ctrl Pts',(-10.0571285787,-37.2742356128,0.645805825719));
#78082=CARTESIAN_POINT('',(-10.0571285787,-37.6642356128,0.645805825719));
#78083=CARTESIAN_POINT('Ctrl Pts',(-2.06575946829,-38.2742356128,-9.01576047951));
#78084=CARTESIAN_POINT('Ctrl Pts',(-2.06575946829,-37.0742356128,-9.01576047951));
#78085=CARTESIAN_POINT('Ctrl Pts',(-2.9672194554,-38.2742356128,-8.85150512783));
#78086=CARTESIAN_POINT('Ctrl Pts',(-2.9672194554,-37.0742356128,-8.85150512783));
#78087=CARTESIAN_POINT('Ctrl Pts',(-3.84599034531,-38.2742356128,-8.59864711683));
#78088=CARTESIAN_POINT('Ctrl Pts',(-3.84599034531,-37.0742356128,-8.59864711683));
#78089=CARTESIAN_POINT('Ctrl Pts',(-4.67357601438,-38.2742356128,-8.25401331235));
#78090=CARTESIAN_POINT('Ctrl Pts',(-4.67357601438,-37.0742356128,-8.25401331235));
#78091=CARTESIAN_POINT('Ctrl Pts',(-6.17345275231,-38.2742356128,-7.42645694938));
#78092=CARTESIAN_POINT('Ctrl Pts',(-6.17345275231,-37.0742356128,-7.42645694938));
#78093=CARTESIAN_POINT('Ctrl Pts',(-7.5161640814,-38.2742356128,-6.34532321195));
#78094=CARTESIAN_POINT('Ctrl Pts',(-7.5161640814,-37.0742356128,-6.34532321195));
#78095=CARTESIAN_POINT('Ctrl Pts',(-8.15806093588,-38.2742356128,-5.76170299258));
#78096=CARTESIAN_POINT('Ctrl Pts',(-8.15806093588,-37.0742356128,-5.76170299258));
#78097=CARTESIAN_POINT('Ctrl Pts',(-9.14108523272,-38.2742356128,-4.69984607968));
#78098=CARTESIAN_POINT('Ctrl Pts',(-9.14108523272,-37.0742356128,-4.69984607968));
#78099=CARTESIAN_POINT('Ctrl Pts',(-9.81302959348,-38.2742356128,-3.42961050122));
#78100=CARTESIAN_POINT('Ctrl Pts',(-9.81302959348,-37.0742356128,-3.42961050122));
#78101=CARTESIAN_POINT('Ctrl Pts',(-10.0098671635,-38.2742356128,-2.88411398337));
#78102=CARTESIAN_POINT('Ctrl Pts',(-10.0098671635,-37.0742356128,-2.88411398337));
#78103=CARTESIAN_POINT('Ctrl Pts',(-10.222733632,-38.2742356128,-1.82926592992));
#78104=CARTESIAN_POINT('Ctrl Pts',(-10.222733632,-37.0742356128,-1.82926592992));
#78105=CARTESIAN_POINT('Ctrl Pts',(-10.2199521215,-38.2742356128,-0.771812654558));
#78106=CARTESIAN_POINT('Ctrl Pts',(-10.2199521215,-37.0742356128,-0.771812654558));
#78107=CARTESIAN_POINT('Ctrl Pts',(-10.184046519,-38.2742356128,-0.287190507733));
#78108=CARTESIAN_POINT('Ctrl Pts',(-10.184046519,-37.0742356128,-0.287190507733));
#78109=CARTESIAN_POINT('Ctrl Pts',(-10.1298079404,-38.2742356128,0.182098137249));
#78110=CARTESIAN_POINT('Ctrl Pts',(-10.1298079404,-37.0742356128,0.182098137249));
#78111=CARTESIAN_POINT('Ctrl Pts',(-10.0571285787,-38.2742356128,0.645805825733));
#78112=CARTESIAN_POINT('Ctrl Pts',(-10.0571285787,-37.0742356128,0.645805825733));
#78113=CARTESIAN_POINT('Ctrl Pts',(-2.06575948168004,-37.2742356128,-9.0157604770702));
#78114=CARTESIAN_POINT('Ctrl Pts',(-2.96721946584242,-37.2742356128,-8.8515051248253));
#78115=CARTESIAN_POINT('Ctrl Pts',(-3.84599035268564,-37.2742356128,-8.59864711375854));
#78116=CARTESIAN_POINT('Ctrl Pts',(-4.67357601907077,-37.2742356128,-8.25401330976187));
#78117=CARTESIAN_POINT('Ctrl Pts',(-6.17345275440962,-37.2742356128,-7.42645694768941));
#78118=CARTESIAN_POINT('Ctrl Pts',(-7.5161640814,-37.2742356128,-6.34532321195));
#78119=CARTESIAN_POINT('Ctrl Pts',(-8.15806093588,-37.2742356128,-5.76170299258));
#78120=CARTESIAN_POINT('Ctrl Pts',(-9.14108523272,-37.2742356128,-4.69984607968));
#78121=CARTESIAN_POINT('Ctrl Pts',(-9.81302959348,-37.2742356128,-3.42961050122));
#78122=CARTESIAN_POINT('Ctrl Pts',(-10.0098671635,-37.2742356128,-2.88411398337));
#78123=CARTESIAN_POINT('Ctrl Pts',(-10.222733632,-37.2742356128,-1.82926592992));
#78124=CARTESIAN_POINT('Ctrl Pts',(-10.2199521215,-37.2742356128,-0.771812654558));
#78125=CARTESIAN_POINT('Ctrl Pts',(-10.184046519,-37.2742356128,-0.287190507733));
#78126=CARTESIAN_POINT('Ctrl Pts',(-10.1298079404,-37.2742356128,0.182098137249));
#78127=CARTESIAN_POINT('Ctrl Pts',(-10.0571285787022,-37.2742356128,0.645805825719337));
#78128=CARTESIAN_POINT('Origin',(-3.35265884719E-30,-37.2742356128,3.15283103411E-22));
#78129=CARTESIAN_POINT('Origin',(-3.35265884719E-30,-37.2742356128,3.15283103411E-22));
#78130=CARTESIAN_POINT('Origin',(0.5,-41.6742356128,13.1643460036));
#78131=CARTESIAN_POINT('',(0.5,-37.2742356128,13.9192139476));
#78132=CARTESIAN_POINT('Origin',(-0.5,-41.6742356128,13.1643460036));
#78133=CARTESIAN_POINT('',(-0.5,-37.2742356128,13.9192139476));
#78134=CARTESIAN_POINT('Origin',(0.5,-41.6742356128,13.1643460036));
#78135=CARTESIAN_POINT('',(0.5,-37.2742356128,-13.2046742098));
#78136=CARTESIAN_POINT('Origin',(-0.5,-41.6742356128,13.1643460036));
#78137=CARTESIAN_POINT('',(-0.5,-37.2742356128,-13.2046742098));
#78138=CARTESIAN_POINT('Origin',(-10.9208700025,-38.7742356128,-8.61474463077));
#78139=CARTESIAN_POINT('',(-11.7961681305,-33.7742356128,-9.46800252678));
#78140=CARTESIAN_POINT('',(-11.7961681305,-36.2742356128,-9.46800252678));
#78141=CARTESIAN_POINT('',(-10.9208700025,-33.7742356128,-8.61474463077));
#78142=CARTESIAN_POINT('',(-11.3585190665,-33.7742356128,-9.04137357878));
#78143=CARTESIAN_POINT('',(-10.9208700025,-37.2742356128,-8.61474463077));
#78144=CARTESIAN_POINT('',(-10.9208700025,-35.5242356128,-8.61474463077));
#78145=CARTESIAN_POINT('',(-10.1269675574,-37.2742356128,-7.84083285349));
#78146=CARTESIAN_POINT('Origin',(-11.6189039641,-38.7742356128,-7.89867997696));
#78147=CARTESIAN_POINT('',(-11.6189039641,-37.2742356128,-7.89867997696));
#78148=CARTESIAN_POINT('',(-10.8175627992,-37.2742356128,-7.11751678877));
#78149=CARTESIAN_POINT('',(-11.6189039641,-33.7742356128,-7.89867997696));
#78150=CARTESIAN_POINT('',(-11.6189039641,-35.5242356128,-7.89867997696));
#78151=CARTESIAN_POINT('',(-13.1382272111,-33.7742356128,-9.37974627375));
#78152=CARTESIAN_POINT('',(-12.3785655876,-33.7742356128,-8.63921312536));
#78153=CARTESIAN_POINT('',(-13.1382272111,-37.2742356128,-9.37974627375));
#78154=CARTESIAN_POINT('',(-13.1382272111,-35.5242356128,-9.37974627375));
#78155=CARTESIAN_POINT('',(-12.8689688238,-37.2742356128,-9.11726788193));
#78156=CARTESIAN_POINT('Origin',(-8.33174409695,-38.7742356128,-11.2707494202));
#78157=CARTESIAN_POINT('',(-9.86946476635,-37.2742356128,-12.7697498875));
#78158=CARTESIAN_POINT('',(-9.60206866896,-37.2742356128,-12.5090868927));
#78159=CARTESIAN_POINT('',(-9.86946476635,-33.7742356128,-12.7697498875));
#78160=CARTESIAN_POINT('',(-9.86946476635,-35.5242356128,-12.7697498875));
#78161=CARTESIAN_POINT('',(-8.33174409695,-33.7742356128,-11.2707494202));
#78162=CARTESIAN_POINT('',(-9.10060443165,-33.7742356128,-12.0202496539));
#78163=CARTESIAN_POINT('',(-8.33174409695,-37.2742356128,-11.2707494202));
#78164=CARTESIAN_POINT('',(-8.33174409695,-35.5242356128,-11.2707494202));
#78165=CARTESIAN_POINT('',(-7.34305038686,-37.2742356128,-10.3069512721));
#78166=CARTESIAN_POINT('Origin',(-9.02977805856,-38.7742356128,-10.5546847664));
#78167=CARTESIAN_POINT('',(-9.02977805856,-37.2742356128,-10.5546847664));
#78168=CARTESIAN_POINT('',(-8.12836745794,-37.2742356128,-9.6759719166));
#78169=CARTESIAN_POINT('',(-9.02977805856,-33.7742356128,-10.5546847664));
#78170=CARTESIAN_POINT('',(-9.02977805856,-35.5242356128,-10.5546847664));
#78171=CARTESIAN_POINT('',(-9.91508679725,-33.7742356128,-11.4177012033));
#78172=CARTESIAN_POINT('',(-9.47243242791,-33.7742356128,-10.9861929848));
#78173=CARTESIAN_POINT('',(-9.91508679725,-36.2742356128,-11.4177012033));
#78174=CARTESIAN_POINT('Origin',(9.02977805856,-38.7742356128,-10.5546847664));
#78175=CARTESIAN_POINT('',(9.91508679725,-33.7742356128,-11.4177012033));
#78176=CARTESIAN_POINT('',(9.91508679725,-36.2742356128,-11.4177012033));
#78177=CARTESIAN_POINT('',(9.02977805856,-33.7742356128,-10.5546847664));
#78178=CARTESIAN_POINT('',(9.47243242791,-33.7742356128,-10.9861929848));
#78179=CARTESIAN_POINT('',(9.02977805856,-37.2742356128,-10.5546847664));
#78180=CARTESIAN_POINT('',(9.02977805856,-35.5242356128,-10.5546847664));
#78181=CARTESIAN_POINT('',(8.12836745794,-37.2742356128,-9.6759719166));
#78182=CARTESIAN_POINT('Origin',(8.33174409695,-38.7742356128,-11.2707494202));
#78183=CARTESIAN_POINT('',(8.33174409695,-37.2742356128,-11.2707494202));
#78184=CARTESIAN_POINT('',(7.34305038686,-37.2742356128,-10.3069512721));
#78185=CARTESIAN_POINT('',(8.33174409695,-33.7742356128,-11.2707494202));
#78186=CARTESIAN_POINT('',(8.33174409695,-35.5242356128,-11.2707494202));
#78187=CARTESIAN_POINT('',(9.86946476635,-33.7742356128,-12.7697498875));
#78188=CARTESIAN_POINT('',(9.10060443165,-33.7742356128,-12.0202496539));
#78189=CARTESIAN_POINT('',(9.86946476635,-37.2742356128,-12.7697498875));
#78190=CARTESIAN_POINT('',(9.86946476635,-35.5242356128,-12.7697498875));
#78191=CARTESIAN_POINT('',(9.60206866896,-37.2742356128,-12.5090868927));
#78192=CARTESIAN_POINT('Origin',(11.6189039641,-38.7742356128,-7.89867997696));
#78193=CARTESIAN_POINT('',(13.1382272111,-37.2742356128,-9.37974627375));
#78194=CARTESIAN_POINT('',(12.8689688238,-37.2742356128,-9.11726788193));
#78195=CARTESIAN_POINT('',(13.1382272111,-33.7742356128,-9.37974627375));
#78196=CARTESIAN_POINT('',(13.1382272111,-35.5242356128,-9.37974627375));
#78197=CARTESIAN_POINT('',(11.6189039641,-33.7742356128,-7.89867997696));
#78198=CARTESIAN_POINT('',(12.3785655876,-33.7742356128,-8.63921312536));
#78199=CARTESIAN_POINT('',(11.6189039641,-37.2742356128,-7.89867997696));
#78200=CARTESIAN_POINT('',(11.6189039641,-35.5242356128,-7.89867997696));
#78201=CARTESIAN_POINT('',(10.8175627992,-37.2742356128,-7.11751678877));
#78202=CARTESIAN_POINT('Origin',(10.9208700025,-38.7742356128,-8.61474463077));
#78203=CARTESIAN_POINT('',(10.9208700025,-37.2742356128,-8.61474463077));
#78204=CARTESIAN_POINT('',(10.1269675574,-37.2742356128,-7.84083285349));
#78205=CARTESIAN_POINT('',(10.9208700025,-33.7742356128,-8.61474463077));
#78206=CARTESIAN_POINT('',(10.9208700025,-35.5242356128,-8.61474463077));
#78207=CARTESIAN_POINT('',(11.7961681305,-33.7742356128,-9.46800252678));
#78208=CARTESIAN_POINT('',(11.3585190665,-33.7742356128,-9.04137357878));
#78209=CARTESIAN_POINT('',(11.7961681305,-36.2742356128,-9.46800252678));
#78210=CARTESIAN_POINT('Origin',(-3.35265884719E-30,-37.2742356128,3.15283103411E-22));
#78211=CARTESIAN_POINT('Origin',(12.9288170226,-37.2742356128,-9.5945656699));
#78212=CARTESIAN_POINT('Origin',(-3.35265884719E-30,-37.2742356128,3.15283103411E-22));
#78213=CARTESIAN_POINT('',(13.1382272111,-37.2742356128,9.37974627375));
#78214=CARTESIAN_POINT('',(12.8689688238,-37.2742356128,9.11726788193));
#78215=CARTESIAN_POINT('Origin',(12.9288170226,-37.2742356128,9.5945656699));
#78216=CARTESIAN_POINT('Origin',(-3.35265884719E-30,-37.2742356128,3.15283103411E-22));
#78217=CARTESIAN_POINT('',(8.60554847393,-37.2742356128,-10.560093974));
#78218=CARTESIAN_POINT('Origin',(8.82036787008,-37.2742356128,-10.7695041625));
#78219=CARTESIAN_POINT('',(8.32633488929,-37.2742356128,-10.8465198356));
#78220=CARTESIAN_POINT('',(8.46594168161,-37.2742356128,-10.7033069048));
#78221=CARTESIAN_POINT('Origin',(8.54115428543,-37.2742356128,-11.0559300241));
#78222=CARTESIAN_POINT('Origin',(10.0788749548,-37.2742356128,-12.5549304914));
#78223=CARTESIAN_POINT('Origin',(-10.0788749548,-37.2742356128,-12.5549304914));
#78224=CARTESIAN_POINT('',(-8.32633488929,-37.2742356128,-10.8465198356));
#78225=CARTESIAN_POINT('Origin',(-8.54115428543,-37.2742356128,-11.0559300241));
#78226=CARTESIAN_POINT('',(-8.60554847393,-37.2742356128,-10.560093974));
#78227=CARTESIAN_POINT('',(-8.46594168161,-37.2742356128,-10.7033069048));
#78228=CARTESIAN_POINT('Origin',(-8.82036787008,-37.2742356128,-10.7695041625));
#78229=CARTESIAN_POINT('',(-10.9154607948,-37.2742356128,-8.19051504615));
#78230=CARTESIAN_POINT('Origin',(-11.1302801909,-37.2742356128,-8.39992523463));
#78231=CARTESIAN_POINT('',(-11.1946743794,-37.2742356128,-7.90408918462));
#78232=CARTESIAN_POINT('',(-11.0550675871,-37.2742356128,-8.04730211538));
#78233=CARTESIAN_POINT('Origin',(-11.4094937756,-37.2742356128,-8.1134993731));
#78234=CARTESIAN_POINT('',(-9.4709461123,-37.2742356128,13.0795270061));
#78235=CARTESIAN_POINT('',(-9.19878759701,-37.2742356128,12.8142215122));
#78236=CARTESIAN_POINT('Origin',(-9.68035630078,-37.2742356128,12.8647076099));
#78237=CARTESIAN_POINT('',(9.86946476635,-37.2742356128,12.7697498875));
#78238=CARTESIAN_POINT('Origin',(10.0788749548,-37.2742356128,12.5549304914));
#78239=CARTESIAN_POINT('',(9.60206866896,-37.2742356128,12.5090868927));
#78240=CARTESIAN_POINT('',(11.1946743794,-37.2742356128,-7.90408918462));
#78241=CARTESIAN_POINT('Origin',(11.4094937756,-37.2742356128,-8.1134993731));
#78242=CARTESIAN_POINT('',(10.9154607948,-37.2742356128,-8.19051504615));
#78243=CARTESIAN_POINT('',(11.0550675871,-37.2742356128,-8.04730211538));
#78244=CARTESIAN_POINT('Origin',(11.1302801909,-37.2742356128,-8.39992523463));
#78245=CARTESIAN_POINT('Origin',(-3.35265884719E-30,-37.2742356128,3.15283103411E-22));
#78246=CARTESIAN_POINT('Origin',(-12.9288170226,-37.2742356128,-9.5945656699));
#78247=CARTESIAN_POINT('Origin',(-3.35265884719E-30,-37.2742356128,3.15283103411E-22));
#78248=CARTESIAN_POINT('',(-13.4331612704,-37.2742356128,8.96899284723));
#78249=CARTESIAN_POINT('Origin',(-13.2237510819,-37.2742356128,9.18381224337));
#78250=CARTESIAN_POINT('',(-13.1590062198,-37.2742356128,8.70174109129));
#78251=CARTESIAN_POINT('Origin',(12.1468815993,-33.7742356128,-8.83231958171));
#78252=CARTESIAN_POINT('',(11.4094937756,-33.4742356128,-8.1134993731));
#78253=CARTESIAN_POINT('Origin',(11.4094937756,-33.7742356128,-8.1134993731));
#78254=CARTESIAN_POINT('',(12.9288170226,-33.4742356128,-9.5945656699));
#78255=CARTESIAN_POINT('Origin',(12.9288170226,-33.7742356128,-9.5945656699));
#78256=CARTESIAN_POINT('',(12.1468815993,-33.4742356128,-8.83231958171));
#78257=CARTESIAN_POINT('Origin',(12.9288170226,-36.1242356128,-9.5945656699));
#78258=CARTESIAN_POINT('Origin',(12.9288170226,-33.7742356128,-9.5945656699));
#78259=CARTESIAN_POINT('Origin',(12.9288170226,-33.7742356128,-9.5945656699));
#78260=CARTESIAN_POINT('Origin',(12.9288170226,-33.7742356128,-9.5945656699));
#78261=CARTESIAN_POINT('Origin',(11.4094937756,-36.1242356128,-8.1134993731));
#78262=CARTESIAN_POINT('',(11.1946743794,-33.7742356128,-7.90408918462));
#78263=CARTESIAN_POINT('Origin',(11.4094937756,-33.7742356128,-8.1134993731));
#78264=CARTESIAN_POINT('',(11.1946743794,-36.1242356128,-7.90408918462));
#78265=CARTESIAN_POINT('Origin',(11.4094937756,-33.7742356128,-8.1134993731));
#78266=CARTESIAN_POINT('Origin',(11.4094937756,-33.7742356128,-8.1134993731));
#78267=CARTESIAN_POINT('Origin',(-1.7763568394E-15,-33.7742356128,3.55271399408E-15));
#78268=CARTESIAN_POINT('',(10.0788749548,-33.4742356128,-12.5549304914));
#78269=CARTESIAN_POINT('Origin',(10.0788749548,-33.7742356128,-12.5549304914));
#78270=CARTESIAN_POINT('Origin',(-1.7763568394E-15,-33.4742356128,3.55271399408E-15));
#78271=CARTESIAN_POINT('Origin',(10.0788749548,-36.1242356128,-12.5549304914));
#78272=CARTESIAN_POINT('Origin',(10.0788749548,-33.7742356128,-12.5549304914));
#78273=CARTESIAN_POINT('Origin',(10.0788749548,-33.7742356128,-12.5549304914));
#78274=CARTESIAN_POINT('Origin',(10.0788749548,-33.7742356128,-12.5549304914));
#78275=CARTESIAN_POINT('Origin',(-3.35265884719E-30,-33.4742356128,3.15283103411E-22));
#78276=CARTESIAN_POINT('',(8.54115428543,-33.4742356128,-11.0559300241));
#78277=CARTESIAN_POINT('',(9.31001462013,-33.4742356128,-11.8054302577));
#78278=CARTESIAN_POINT('',(8.82036787008,-33.4742356128,-10.7695041625));
#78279=CARTESIAN_POINT('',(8.68076107776,-33.4742356128,-10.9127170933));
#78280=CARTESIAN_POINT('',(9.70567660877,-33.4742356128,-11.6325205994));
#78281=CARTESIAN_POINT('',(9.26302223942,-33.4742356128,-11.201012381));
#78282=CARTESIAN_POINT('',(10.5267948792,-33.4742356128,-11.6480294286));
#78283=CARTESIAN_POINT('Origin',(10.1244969857,-33.4742356128,-11.2028818071));
#78284=CARTESIAN_POINT('',(12.0471589199,-33.4742356128,-10.0675698139));
#78285=CARTESIAN_POINT('Origin',(-3.35265884719E-30,-33.4742356128,7.1009945507E-16));
#78286=CARTESIAN_POINT('',(12.005578319,-33.4742356128,-9.25318313064));
#78287=CARTESIAN_POINT('Origin',(11.586757942,-33.4742356128,-9.68282192292));
#78288=CARTESIAN_POINT('',(11.1302801909,-33.4742356128,-8.39992523463));
#78289=CARTESIAN_POINT('',(11.567929255,-33.4742356128,-8.82655418263));
#78290=CARTESIAN_POINT('',(11.2698869833,-33.4742356128,-8.25671230387));
#78291=CARTESIAN_POINT('Origin',(9.96422937677,-33.7742356128,-9.59609593478));
#78292=CARTESIAN_POINT('',(10.9154607948,-33.7742356128,-8.19051504615));
#78293=CARTESIAN_POINT('Origin',(11.1302801909,-33.7742356128,-8.39992523463));
#78294=CARTESIAN_POINT('',(9.74940998063,-33.7742356128,-9.38668574629));
#78295=CARTESIAN_POINT('Origin',(11.1302801909,-33.7742356128,-8.39992523463));
#78296=CARTESIAN_POINT('Origin',(11.1302801909,-33.7742356128,-8.39992523463));
#78297=CARTESIAN_POINT('Origin',(11.1302801909,-33.7742356128,-8.39992523463));
#78298=CARTESIAN_POINT('Origin',(9.33228841993,-33.7742356128,-11.8271431975));
#78299=CARTESIAN_POINT('Origin',(8.54115428543,-33.7742356128,-11.0559300241));
#78300=CARTESIAN_POINT('Origin',(8.54115428543,-33.7742356128,-11.0559300241));
#78301=CARTESIAN_POINT('',(8.32633488929,-33.7742356128,-10.8465198356));
#78302=CARTESIAN_POINT('Origin',(8.54115428543,-33.7742356128,-11.0559300241));
#78303=CARTESIAN_POINT('Origin',(8.54115428543,-33.7742356128,-11.0559300241));
#78304=CARTESIAN_POINT('Origin',(9.96422937677,-33.7742356128,-9.59609593478));
#78305=CARTESIAN_POINT('',(8.60554847393,-33.7742356128,-10.560093974));
#78306=CARTESIAN_POINT('',(9.74940998063,-33.7742356128,-9.38668574629));
#78307=CARTESIAN_POINT('Origin',(8.82036787008,-33.7742356128,-10.7695041625));
#78308=CARTESIAN_POINT('Origin',(8.82036787008,-33.7742356128,-10.7695041625));
#78309=CARTESIAN_POINT('Origin',(8.82036787008,-33.7742356128,-10.7695041625));
#78310=CARTESIAN_POINT('Origin',(8.82036787008,-33.7742356128,-10.7695041625));
#78311=CARTESIAN_POINT('Origin',(9.61880743047,-33.7742356128,-11.5478388094));
#78312=CARTESIAN_POINT('Origin',(9.70567660877,-33.7742356128,-11.6325205994));
#78313=CARTESIAN_POINT('Origin',(10.1244969857,-33.7742356128,-11.2028818071));
#78314=CARTESIAN_POINT('Origin',(10.1244969857,-33.7742356128,-11.2028818071));
#78315=CARTESIAN_POINT('Origin',(10.5267948792,-33.7742356128,-11.6480294286));
#78316=CARTESIAN_POINT('Origin',(1.7763568394E-14,-33.7742356128,-1.42108543999E-14));
#78317=CARTESIAN_POINT('Origin',(12.0471589199,-33.7742356128,-10.0675698139));
#78318=CARTESIAN_POINT('Origin',(11.586757942,-33.7742356128,-9.68282192292));
#78319=CARTESIAN_POINT('Origin',(11.586757942,-33.7742356128,-9.68282192292));
#78320=CARTESIAN_POINT('Origin',(12.005578319,-33.7742356128,-9.25318313064));
#78321=CARTESIAN_POINT('Origin',(11.8603625888,-33.7742356128,-9.11162396985));
#78322=CARTESIAN_POINT('Origin',(11.5436913602,-37.2742356128,-7.54605685771));
#78323=CARTESIAN_POINT('',(10.9154607948,-36.1242356128,-8.19051504615));
#78324=CARTESIAN_POINT('Origin',(11.1302801909,-36.1242356128,-8.39992523463));
#78325=CARTESIAN_POINT('Origin',(8.54115428543,-36.1242356128,-11.0559300241));
#78326=CARTESIAN_POINT('',(8.32633488929,-36.1242356128,-10.8465198356));
#78327=CARTESIAN_POINT('Origin',(11.5436913602,-37.2742356128,-7.54605685771));
#78328=CARTESIAN_POINT('',(8.60554847393,-36.1242356128,-10.560093974));
#78329=CARTESIAN_POINT('Origin',(8.82036787008,-36.1242356128,-10.7695041625));
#78330=CARTESIAN_POINT('Origin',(10.1244969857,-36.1242356128,-11.2028818071));
#78331=CARTESIAN_POINT('Origin',(11.586757942,-36.1242356128,-9.68282192292));
#78332=CARTESIAN_POINT('Origin',(7.97371177005,-37.2742356128,10.9217324394));
#78333=CARTESIAN_POINT('',(9.86946476635,-33.7742356128,12.7697498875));
#78334=CARTESIAN_POINT('',(9.86946476635,-36.1242356128,12.7697498875));
#78335=CARTESIAN_POINT('',(8.33174409695,-33.7742356128,11.2707494202));
#78336=CARTESIAN_POINT('',(9.08759374531,-33.7742356128,12.00756658));
#78337=CARTESIAN_POINT('',(8.33174409695,-36.1242356128,11.2707494202));
#78338=CARTESIAN_POINT('Origin',(9.33228841993,-33.7742356128,11.8271431975));
#78339=CARTESIAN_POINT('',(8.54115428543,-33.4742356128,11.0559300241));
#78340=CARTESIAN_POINT('Origin',(8.54115428543,-33.7742356128,11.0559300241));
#78341=CARTESIAN_POINT('',(10.0788749548,-33.4742356128,12.5549304914));
#78342=CARTESIAN_POINT('Origin',(10.0788749548,-33.7742356128,12.5549304914));
#78343=CARTESIAN_POINT('',(9.33228841993,-33.4742356128,11.8271431975));
#78344=CARTESIAN_POINT('Origin',(10.0788749548,-36.1242356128,12.5549304914));
#78345=CARTESIAN_POINT('Origin',(10.0788749548,-33.7742356128,12.5549304914));
#78346=CARTESIAN_POINT('Origin',(10.0788749548,-33.7742356128,12.5549304914));
#78347=CARTESIAN_POINT('Origin',(10.0788749548,-33.7742356128,12.5549304914));
#78348=CARTESIAN_POINT('Origin',(8.54115428543,-36.1242356128,11.0559300241));
#78349=CARTESIAN_POINT('',(8.32633488929,-33.7742356128,10.8465198356));
#78350=CARTESIAN_POINT('',(8.32633488929,-36.1242356128,10.8465198356));
#78351=CARTESIAN_POINT('Origin',(8.54115428543,-33.7742356128,11.0559300241));
#78352=CARTESIAN_POINT('Origin',(8.54115428543,-33.7742356128,11.0559300241));
#78353=CARTESIAN_POINT('Origin',(8.54115428543,-33.7742356128,11.0559300241));
#78354=CARTESIAN_POINT('Origin',(-3.35265884719E-30,-33.7742356128,3.15283103411E-22));
#78355=CARTESIAN_POINT('',(12.9288170226,-33.4742356128,9.5945656699));
#78356=CARTESIAN_POINT('Origin',(12.9288170226,-33.7742356128,9.5945656699));
#78357=CARTESIAN_POINT('Origin',(-3.35265884719E-30,-33.4742356128,3.15283103411E-22));
#78358=CARTESIAN_POINT('Origin',(12.9288170226,-36.1242356128,9.5945656699));
#78359=CARTESIAN_POINT('',(13.1382272111,-33.7742356128,9.37974627375));
#78360=CARTESIAN_POINT('',(13.1382272111,-36.1242356128,9.37974627375));
#78361=CARTESIAN_POINT('Origin',(12.9288170226,-33.7742356128,9.5945656699));
#78362=CARTESIAN_POINT('Origin',(12.9288170226,-33.7742356128,9.5945656699));
#78363=CARTESIAN_POINT('Origin',(12.9288170226,-33.7742356128,9.5945656699));
#78364=CARTESIAN_POINT('Origin',(-3.35265884719E-30,-33.4742356128,3.15283103411E-22));
#78365=CARTESIAN_POINT('',(11.4094937756,-33.4742356128,8.1134993731));
#78366=CARTESIAN_POINT('',(12.1691553991,-33.4742356128,8.8540325215));
#78367=CARTESIAN_POINT('',(11.1302801909,-33.4742356128,8.39992523463));
#78368=CARTESIAN_POINT('',(11.2698869833,-33.4742356128,8.25671230387));
#78369=CARTESIAN_POINT('',(12.005578319,-33.4742356128,9.25318313064));
#78370=CARTESIAN_POINT('',(11.567929255,-33.4742356128,8.82655418263));
#78371=CARTESIAN_POINT('',(12.0471589199,-33.4742356128,10.0675698139));
#78372=CARTESIAN_POINT('Origin',(11.586757942,-33.4742356128,9.68282192292));
#78373=CARTESIAN_POINT('',(10.5267948792,-33.4742356128,11.6480294286));
#78374=CARTESIAN_POINT('Origin',(-3.35265884719E-30,-33.4742356128,7.1009945507E-16));
#78375=CARTESIAN_POINT('',(9.70567660877,-33.4742356128,11.6325205994));
#78376=CARTESIAN_POINT('Origin',(10.1244969857,-33.4742356128,11.2028818071));
#78377=CARTESIAN_POINT('',(8.82036787008,-33.4742356128,10.7695041625));
#78378=CARTESIAN_POINT('',(9.26302223942,-33.4742356128,11.201012381));
#78379=CARTESIAN_POINT('',(8.68076107776,-33.4742356128,10.9127170933));
#78380=CARTESIAN_POINT('Origin',(9.96422937677,-33.7742356128,9.59609593478));
#78381=CARTESIAN_POINT('',(8.60554847393,-33.7742356128,10.560093974));
#78382=CARTESIAN_POINT('Origin',(8.82036787008,-33.7742356128,10.7695041625));
#78383=CARTESIAN_POINT('',(9.74940998063,-33.7742356128,9.38668574629));
#78384=CARTESIAN_POINT('Origin',(8.82036787008,-33.7742356128,10.7695041625));
#78385=CARTESIAN_POINT('',(9.02977805856,-33.7742356128,10.5546847664));
#78386=CARTESIAN_POINT('Origin',(8.82036787008,-33.7742356128,10.7695041625));
#78387=CARTESIAN_POINT('Origin',(8.82036787008,-33.7742356128,10.7695041625));
#78388=CARTESIAN_POINT('Origin',(12.1468815993,-33.7742356128,8.83231958171));
#78389=CARTESIAN_POINT('',(11.6189039641,-33.7742356128,7.89867997696));
#78390=CARTESIAN_POINT('',(12.3562917878,-33.7742356128,8.61750018557));
#78391=CARTESIAN_POINT('Origin',(11.4094937756,-33.7742356128,8.1134993731));
#78392=CARTESIAN_POINT('Origin',(11.4094937756,-33.7742356128,8.1134993731));
#78393=CARTESIAN_POINT('',(11.1946743794,-33.7742356128,7.90408918462));
#78394=CARTESIAN_POINT('Origin',(11.4094937756,-33.7742356128,8.1134993731));
#78395=CARTESIAN_POINT('Origin',(11.4094937756,-33.7742356128,8.1134993731));
#78396=CARTESIAN_POINT('Origin',(9.96422937677,-33.7742356128,9.59609593478));
#78397=CARTESIAN_POINT('',(10.9154607948,-33.7742356128,8.19051504615));
#78398=CARTESIAN_POINT('',(9.74940998063,-33.7742356128,9.38668574629));
#78399=CARTESIAN_POINT('Origin',(11.1302801909,-33.7742356128,8.39992523463));
#78400=CARTESIAN_POINT('Origin',(11.1302801909,-33.7742356128,8.39992523463));
#78401=CARTESIAN_POINT('',(10.9208700025,-33.7742356128,8.61474463077));
#78402=CARTESIAN_POINT('Origin',(11.1302801909,-33.7742356128,8.39992523463));
#78403=CARTESIAN_POINT('Origin',(11.1302801909,-33.7742356128,8.39992523463));
#78404=CARTESIAN_POINT('Origin',(11.8603625888,-33.7742356128,9.11162396985));
#78405=CARTESIAN_POINT('',(11.7961681305,-33.7742356128,9.46800252678));
#78406=CARTESIAN_POINT('',(11.6509524003,-33.7742356128,9.32644336599));
#78407=CARTESIAN_POINT('Origin',(12.005578319,-33.7742356128,9.25318313064));
#78408=CARTESIAN_POINT('Origin',(11.586757942,-33.7742356128,9.68282192292));
#78409=CARTESIAN_POINT('Origin',(11.586757942,-33.7742356128,9.68282192292));
#78410=CARTESIAN_POINT('Origin',(12.0471589199,-33.7742356128,10.0675698139));
#78411=CARTESIAN_POINT('Origin',(1.24344978758E-14,-33.7742356128,1.59872118699E-14));
#78412=CARTESIAN_POINT('Origin',(10.5267948792,-33.7742356128,11.6480294286));
#78413=CARTESIAN_POINT('Origin',(10.1244969857,-33.7742356128,11.2028818071));
#78414=CARTESIAN_POINT('',(9.91508679725,-33.7742356128,11.4177012033));
#78415=CARTESIAN_POINT('Origin',(10.1244969857,-33.7742356128,11.2028818071));
#78416=CARTESIAN_POINT('Origin',(9.70567660877,-33.7742356128,11.6325205994));
#78417=CARTESIAN_POINT('Origin',(9.61880743047,-33.7742356128,11.5478388094));
#78418=CARTESIAN_POINT('',(9.82821761895,-33.7742356128,11.3330194132));
#78419=CARTESIAN_POINT('Origin',(11.5436913602,-37.2742356128,7.54605685771));
#78420=CARTESIAN_POINT('',(8.60554847393,-36.1242356128,10.560093974));
#78421=CARTESIAN_POINT('Origin',(8.82036787008,-36.1242356128,10.7695041625));
#78422=CARTESIAN_POINT('',(9.02977805856,-36.1242356128,10.5546847664));
#78423=CARTESIAN_POINT('Origin',(11.2608716372,-37.2742356128,7.54966299616));
#78424=CARTESIAN_POINT('',(11.6189039641,-36.1242356128,7.89867997696));
#78425=CARTESIAN_POINT('Origin',(11.4094937756,-36.1242356128,8.1134993731));
#78426=CARTESIAN_POINT('',(11.1946743794,-36.1242356128,7.90408918462));
#78427=CARTESIAN_POINT('Origin',(11.5436913602,-37.2742356128,7.54605685771));
#78428=CARTESIAN_POINT('',(10.9154607948,-36.1242356128,8.19051504615));
#78429=CARTESIAN_POINT('Origin',(11.1302801909,-36.1242356128,8.39992523463));
#78430=CARTESIAN_POINT('',(10.9208700025,-36.1242356128,8.61474463077));
#78431=CARTESIAN_POINT('Origin',(10.5628376756,-37.2742356128,8.26572764997));
#78432=CARTESIAN_POINT('',(11.7961681305,-36.1242356128,9.46800252678));
#78433=CARTESIAN_POINT('Origin',(11.586757942,-36.1242356128,9.68282192292));
#78434=CARTESIAN_POINT('Origin',(10.1244969857,-36.1242356128,11.2028818071));
#78435=CARTESIAN_POINT('',(9.91508679725,-36.1242356128,11.4177012033));
#78436=CARTESIAN_POINT('Origin',(8.67174573165,-37.2742356128,10.2056677856));
#78437=CARTESIAN_POINT('Origin',(-12.1468815993,-33.7742356128,-8.83231958171));
#78438=CARTESIAN_POINT('',(-11.4094937756,-33.4742356128,-8.1134993731));
#78439=CARTESIAN_POINT('Origin',(-11.4094937756,-33.7742356128,-8.1134993731));
#78440=CARTESIAN_POINT('',(-12.9288170226,-33.4742356128,-9.5945656699));
#78441=CARTESIAN_POINT('',(-12.1468815993,-33.4742356128,-8.83231958171));
#78442=CARTESIAN_POINT('Origin',(-12.9288170226,-33.7742356128,-9.5945656699));
#78443=CARTESIAN_POINT('Origin',(-12.9288170226,-36.1242356128,-9.5945656699));
#78444=CARTESIAN_POINT('Origin',(-12.9288170226,-33.7742356128,-9.5945656699));
#78445=CARTESIAN_POINT('Origin',(-12.9288170226,-33.7742356128,-9.5945656699));
#78446=CARTESIAN_POINT('Origin',(-12.9288170226,-33.7742356128,-9.5945656699));
#78447=CARTESIAN_POINT('Origin',(-11.4094937756,-36.1242356128,-8.1134993731));
#78448=CARTESIAN_POINT('',(-11.1946743794,-33.7742356128,-7.90408918462));
#78449=CARTESIAN_POINT('',(-11.1946743794,-36.1242356128,-7.90408918462));
#78450=CARTESIAN_POINT('Origin',(-11.4094937756,-33.7742356128,-8.1134993731));
#78451=CARTESIAN_POINT('Origin',(-11.4094937756,-33.7742356128,-8.1134993731));
#78452=CARTESIAN_POINT('Origin',(-11.4094937756,-33.7742356128,-8.1134993731));
#78453=CARTESIAN_POINT('Origin',(-3.35265884719E-30,-33.7742356128,3.55271399408E-15));
#78454=CARTESIAN_POINT('',(-10.0788749548,-33.4742356128,-12.5549304914));
#78455=CARTESIAN_POINT('Origin',(-3.35265884719E-30,-33.4742356128,3.55271399408E-15));
#78456=CARTESIAN_POINT('Origin',(-10.0788749548,-33.7742356128,-12.5549304914));
#78457=CARTESIAN_POINT('Origin',(-10.0788749548,-36.1242356128,-12.5549304914));
#78458=CARTESIAN_POINT('Origin',(-10.0788749548,-33.7742356128,-12.5549304914));
#78459=CARTESIAN_POINT('Origin',(-10.0788749548,-33.7742356128,-12.5549304914));
#78460=CARTESIAN_POINT('Origin',(-10.0788749548,-33.7742356128,-12.5549304914));
#78461=CARTESIAN_POINT('Origin',(-3.35265884719E-30,-33.4742356128,3.15283103411E-22));
#78462=CARTESIAN_POINT('',(-11.1302801909,-33.4742356128,-8.39992523463));
#78463=CARTESIAN_POINT('',(-11.2698869833,-33.4742356128,-8.25671230387));
#78464=CARTESIAN_POINT('',(-12.005578319,-33.4742356128,-9.25318313064));
#78465=CARTESIAN_POINT('',(-11.567929255,-33.4742356128,-8.82655418263));
#78466=CARTESIAN_POINT('',(-12.0471589199,-33.4742356128,-10.0675698139));
#78467=CARTESIAN_POINT('Origin',(-11.586757942,-33.4742356128,-9.68282192292));
#78468=CARTESIAN_POINT('',(-10.5267948792,-33.4742356128,-11.6480294286));
#78469=CARTESIAN_POINT('Origin',(7.10099139787E-16,-33.4742356128,-1.0651483944E-15));
#78470=CARTESIAN_POINT('',(-9.70567660877,-33.4742356128,-11.6325205994));
#78471=CARTESIAN_POINT('Origin',(-10.1244969857,-33.4742356128,-11.2028818071));
#78472=CARTESIAN_POINT('',(-8.82036787008,-33.4742356128,-10.7695041625));
#78473=CARTESIAN_POINT('',(-9.26302223942,-33.4742356128,-11.201012381));
#78474=CARTESIAN_POINT('',(-8.54115428543,-33.4742356128,-11.0559300241));
#78475=CARTESIAN_POINT('',(-8.68076107776,-33.4742356128,-10.9127170933));
#78476=CARTESIAN_POINT('',(-9.31001462013,-33.4742356128,-11.8054302577));
#78477=CARTESIAN_POINT('Origin',(-9.96422937677,-33.7742356128,-9.59609593478));
#78478=CARTESIAN_POINT('',(-10.9154607948,-33.7742356128,-8.19051504615));
#78479=CARTESIAN_POINT('Origin',(-11.1302801909,-33.7742356128,-8.39992523463));
#78480=CARTESIAN_POINT('',(-9.74940998063,-33.7742356128,-9.38668574629));
#78481=CARTESIAN_POINT('Origin',(-11.1302801909,-33.7742356128,-8.39992523463));
#78482=CARTESIAN_POINT('Origin',(-11.1302801909,-33.7742356128,-8.39992523463));
#78483=CARTESIAN_POINT('Origin',(-11.1302801909,-33.7742356128,-8.39992523463));
#78484=CARTESIAN_POINT('Origin',(-9.33228841993,-33.7742356128,-11.8271431975));
#78485=CARTESIAN_POINT('Origin',(-8.54115428543,-33.7742356128,-11.0559300241));
#78486=CARTESIAN_POINT('Origin',(-8.54115428543,-33.7742356128,-11.0559300241));
#78487=CARTESIAN_POINT('',(-8.32633488929,-33.7742356128,-10.8465198356));
#78488=CARTESIAN_POINT('Origin',(-8.54115428543,-33.7742356128,-11.0559300241));
#78489=CARTESIAN_POINT('Origin',(-8.54115428543,-33.7742356128,-11.0559300241));
#78490=CARTESIAN_POINT('Origin',(-9.96422937677,-33.7742356128,-9.59609593478));
#78491=CARTESIAN_POINT('',(-8.60554847393,-33.7742356128,-10.560093974));
#78492=CARTESIAN_POINT('Origin',(-8.82036787008,-33.7742356128,-10.7695041625));
#78493=CARTESIAN_POINT('',(-9.74940998063,-33.7742356128,-9.38668574629));
#78494=CARTESIAN_POINT('Origin',(-8.82036787008,-33.7742356128,-10.7695041625));
#78495=CARTESIAN_POINT('Origin',(-8.82036787008,-33.7742356128,-10.7695041625));
#78496=CARTESIAN_POINT('Origin',(-8.82036787008,-33.7742356128,-10.7695041625));
#78497=CARTESIAN_POINT('Origin',(-9.61880743047,-33.7742356128,-11.5478388094));
#78498=CARTESIAN_POINT('Origin',(-9.70567660877,-33.7742356128,-11.6325205994));
#78499=CARTESIAN_POINT('Origin',(-10.1244969857,-33.7742356128,-11.2028818071));
#78500=CARTESIAN_POINT('Origin',(-10.5267948792,-33.7742356128,-11.6480294286));
#78501=CARTESIAN_POINT('Origin',(-10.1244969857,-33.7742356128,-11.2028818071));
#78502=CARTESIAN_POINT('Origin',(-1.7763568394E-15,-33.7742356128,-3.55271336352E-15));
#78503=CARTESIAN_POINT('Origin',(-12.0471589199,-33.7742356128,-10.0675698139));
#78504=CARTESIAN_POINT('Origin',(-11.586757942,-33.7742356128,-9.68282192292));
#78505=CARTESIAN_POINT('Origin',(-12.005578319,-33.7742356128,-9.25318313064));
#78506=CARTESIAN_POINT('Origin',(-11.586757942,-33.7742356128,-9.68282192292));
#78507=CARTESIAN_POINT('Origin',(-11.8603625888,-33.7742356128,-9.11162396985));
#78508=CARTESIAN_POINT('Origin',(-11.5436913602,-37.2742356128,-7.54605685771));
#78509=CARTESIAN_POINT('',(-10.9154607948,-36.1242356128,-8.19051504615));
#78510=CARTESIAN_POINT('Origin',(-11.1302801909,-36.1242356128,-8.39992523463));
#78511=CARTESIAN_POINT('Origin',(-8.54115428543,-36.1242356128,-11.0559300241));
#78512=CARTESIAN_POINT('',(-8.32633488929,-36.1242356128,-10.8465198356));
#78513=CARTESIAN_POINT('Origin',(-11.5436913602,-37.2742356128,-7.54605685771));
#78514=CARTESIAN_POINT('',(-8.60554847393,-36.1242356128,-10.560093974));
#78515=CARTESIAN_POINT('Origin',(-8.82036787008,-36.1242356128,-10.7695041625));
#78516=CARTESIAN_POINT('Origin',(-10.1244969857,-36.1242356128,-11.2028818071));
#78517=CARTESIAN_POINT('Origin',(-11.586757942,-36.1242356128,-9.68282192292));
#78518=CARTESIAN_POINT('Origin',(-7.62469478924,-37.2742356128,11.2797647663));
#78519=CARTESIAN_POINT('',(-7.98272711615,-33.7742356128,11.6287817471));
#78520=CARTESIAN_POINT('',(-7.98272711615,-36.1242356128,11.6287817471));
#78521=CARTESIAN_POINT('',(-9.4709461123,-33.7742356128,13.0795270061));
#78522=CARTESIAN_POINT('',(-8.71080409351,-33.7742356128,12.3385255589));
#78523=CARTESIAN_POINT('',(-9.4709461123,-36.1242356128,13.0795270061));
#78524=CARTESIAN_POINT('Origin',(-8.96263144028,-33.7742356128,12.165055246));
#78525=CARTESIAN_POINT('',(-8.19213730463,-33.4742356128,11.413962351));
#78526=CARTESIAN_POINT('Origin',(-8.19213730463,-33.7742356128,11.413962351));
#78527=CARTESIAN_POINT('',(-9.68035630078,-33.4742356128,12.8647076099));
#78528=CARTESIAN_POINT('',(-8.96263144028,-33.4742356128,12.165055246));
#78529=CARTESIAN_POINT('Origin',(-9.68035630078,-33.7742356128,12.8647076099));
#78530=CARTESIAN_POINT('Origin',(-8.19213730463,-36.1242356128,11.413962351));
#78531=CARTESIAN_POINT('',(-7.97731790849,-33.7742356128,11.2045521625));
#78532=CARTESIAN_POINT('',(-7.97731790849,-36.1242356128,11.2045521625));
#78533=CARTESIAN_POINT('Origin',(-8.19213730463,-33.7742356128,11.413962351));
#78534=CARTESIAN_POINT('Origin',(-8.19213730463,-33.7742356128,11.413962351));
#78535=CARTESIAN_POINT('Origin',(-8.19213730463,-33.7742356128,11.413962351));
#78536=CARTESIAN_POINT('Origin',(-9.68035630078,-36.1242356128,12.8647076099));
#78537=CARTESIAN_POINT('Origin',(-9.68035630078,-33.7742356128,12.8647076099));
#78538=CARTESIAN_POINT('Origin',(-9.68035630078,-33.7742356128,12.8647076099));
#78539=CARTESIAN_POINT('Origin',(-9.68035630078,-33.7742356128,12.8647076099));
#78540=CARTESIAN_POINT('Origin',(-3.35265884719E-30,-33.4742356128,3.15283103411E-22));
#78541=CARTESIAN_POINT('',(-8.47135088927,-33.4742356128,11.1275364894));
#78542=CARTESIAN_POINT('',(-8.33174409695,-33.4742356128,11.2707494202));
#78543=CARTESIAN_POINT('',(-9.32799888907,-33.4742356128,11.9626138722));
#78544=CARTESIAN_POINT('',(-8.89967488917,-33.4742356128,11.5450751808));
#78545=CARTESIAN_POINT('',(-10.1341100978,-33.4742356128,11.9912389904));
#78546=CARTESIAN_POINT('Origin',(-9.74681926603,-33.4742356128,11.5329750799));
#78547=CARTESIAN_POINT('',(-12.3752654181,-33.4742356128,9.66140806669));
#78548=CARTESIAN_POINT('Origin',(7.10099139787E-16,-33.4742356128,-1.0651483944E-15));
#78549=CARTESIAN_POINT('',(-12.3211457154,-33.4742356128,8.86254348841));
#78550=CARTESIAN_POINT('Origin',(-11.9023253384,-33.4742356128,9.2921822807));
#78551=CARTESIAN_POINT('',(-11.4792971717,-33.4742356128,8.04189290772));
#78552=CARTESIAN_POINT('',(-11.9002214436,-33.4742356128,8.45221819807));
#78553=CARTESIAN_POINT('',(-11.7585107564,-33.4742356128,7.7554670462));
#78554=CARTESIAN_POINT('',(-11.6189039641,-33.4742356128,7.89867997696));
#78555=CARTESIAN_POINT('',(-13.2237510819,-33.4742356128,9.18381224337));
#78556=CARTESIAN_POINT('',(-12.4911309192,-33.4742356128,8.46963964479));
#78557=CARTESIAN_POINT('Origin',(1.01287953956E-15,-33.4742356128,-6.7525271109E-16));
#78558=CARTESIAN_POINT('Origin',(-9.96493365594,-33.7742356128,9.5953734636));
#78559=CARTESIAN_POINT('',(-8.25653149313,-33.7742356128,10.918126301));
#78560=CARTESIAN_POINT('Origin',(-8.47135088927,-33.7742356128,11.1275364894));
#78561=CARTESIAN_POINT('',(-9.7501142598,-33.7742356128,9.38596327512));
#78562=CARTESIAN_POINT('Origin',(-8.47135088927,-33.7742356128,11.1275364894));
#78563=CARTESIAN_POINT('',(-8.68076107776,-33.7742356128,10.9127170933));
#78564=CARTESIAN_POINT('Origin',(-8.47135088927,-33.7742356128,11.1275364894));
#78565=CARTESIAN_POINT('Origin',(-8.47135088927,-33.7742356128,11.1275364894));
#78566=CARTESIAN_POINT('Origin',(3.5527136788E-15,-33.7742356128,-1.77635652412E-15));
#78567=CARTESIAN_POINT('Origin',(-13.2237510819,-33.7742356128,9.18381224337));
#78568=CARTESIAN_POINT('Origin',(-13.2237510819,-33.7742356128,9.18381224337));
#78569=CARTESIAN_POINT('',(-13.4331612704,-33.7742356128,8.96899284723));
#78570=CARTESIAN_POINT('Origin',(-13.2237510819,-33.7742356128,9.18381224337));
#78571=CARTESIAN_POINT('Origin',(-13.2237510819,-33.7742356128,9.18381224337));
#78572=CARTESIAN_POINT('Origin',(-9.96493365594,-33.7742356128,9.5953734636));
#78573=CARTESIAN_POINT('',(-11.5436913602,-33.7742356128,7.54605685771));
#78574=CARTESIAN_POINT('Origin',(-11.7585107564,-33.7742356128,7.7554670462));
#78575=CARTESIAN_POINT('',(-11.2644777756,-33.7742356128,7.83248271924));
#78576=CARTESIAN_POINT('Origin',(-11.4792971717,-33.7742356128,8.04189290772));
#78577=CARTESIAN_POINT('',(-9.7501142598,-33.7742356128,9.38596327512));
#78578=CARTESIAN_POINT('Origin',(-11.7585107564,-33.7742356128,7.7554670462));
#78579=CARTESIAN_POINT('',(-11.9679209449,-33.7742356128,7.54064765005));
#78580=CARTESIAN_POINT('Origin',(-11.7585107564,-33.7742356128,7.7554670462));
#78581=CARTESIAN_POINT('Origin',(-11.7585107564,-33.7742356128,7.7554670462));
#78582=CARTESIAN_POINT('Origin',(-11.4792971717,-33.7742356128,8.04189290772));
#78583=CARTESIAN_POINT('',(-11.2698869833,-33.7742356128,8.25671230387));
#78584=CARTESIAN_POINT('Origin',(-11.4792971717,-33.7742356128,8.04189290772));
#78585=CARTESIAN_POINT('Origin',(-11.4792971717,-33.7742356128,8.04189290772));
#78586=CARTESIAN_POINT('Origin',(-12.4647462816,-33.7742356128,8.44391937918));
#78587=CARTESIAN_POINT('',(-12.6741564701,-33.7742356128,8.22909998303));
#78588=CARTESIAN_POINT('Origin',(-12.1782272711,-33.7742356128,8.72322376731));
#78589=CARTESIAN_POINT('',(-12.1117355269,-33.7742356128,9.07736288456));
#78590=CARTESIAN_POINT('Origin',(-12.3211457154,-33.7742356128,8.86254348841));
#78591=CARTESIAN_POINT('',(-11.9688170826,-33.7742356128,8.93804316346));
#78592=CARTESIAN_POINT('Origin',(-11.9023253384,-33.7742356128,9.2921822807));
#78593=CARTESIAN_POINT('Origin',(-12.3752654181,-33.7742356128,9.66140806669));
#78594=CARTESIAN_POINT('Origin',(-11.9023253384,-33.7742356128,9.2921822807));
#78595=CARTESIAN_POINT('Origin',(1.7763568394E-15,-33.7742356128,-1.77635652412E-15));
#78596=CARTESIAN_POINT('Origin',(-10.1341100978,-33.7742356128,11.9912389904));
#78597=CARTESIAN_POINT('Origin',(-9.74681926603,-33.7742356128,11.5329750799));
#78598=CARTESIAN_POINT('',(-9.53740907755,-33.7742356128,11.7477944761));
#78599=CARTESIAN_POINT('Origin',(-9.32799888907,-33.7742356128,11.9626138722));
#78600=CARTESIAN_POINT('Origin',(-9.74681926603,-33.7742356128,11.5329750799));
#78601=CARTESIAN_POINT('Origin',(-9.24915045081,-33.7742356128,11.8857508579));
#78602=CARTESIAN_POINT('',(-9.45856063929,-33.7742356128,11.6709314618));
#78603=CARTESIAN_POINT('Origin',(-11.5436913602,-37.2742356128,7.54605685771));
#78604=CARTESIAN_POINT('',(-8.25653149313,-36.1242356128,10.918126301));
#78605=CARTESIAN_POINT('Origin',(-8.47135088927,-36.1242356128,11.1275364894));
#78606=CARTESIAN_POINT('',(-8.68076107776,-36.1242356128,10.9127170933));
#78607=CARTESIAN_POINT('Origin',(-13.2237510819,-36.1242356128,9.18381224337));
#78608=CARTESIAN_POINT('',(-13.4331612704,-36.1242356128,8.96899284723));
#78609=CARTESIAN_POINT('Origin',(-11.5436913602,-37.2742356128,7.54605685771));
#78610=CARTESIAN_POINT('',(-11.2644777756,-36.1242356128,7.83248271924));
#78611=CARTESIAN_POINT('',(-11.5436913602,-36.1242356128,7.54605685771));
#78612=CARTESIAN_POINT('Origin',(-11.7585107564,-36.1242356128,7.7554670462));
#78613=CARTESIAN_POINT('',(-11.9679209449,-36.1242356128,7.54064765005));
#78614=CARTESIAN_POINT('Origin',(-11.4792971717,-36.1242356128,8.04189290772));
#78615=CARTESIAN_POINT('',(-11.2698869833,-36.1242356128,8.25671230387));
#78616=CARTESIAN_POINT('Origin',(-11.609888618,-37.2742356128,7.19163066925));
#78617=CARTESIAN_POINT('Origin',(-10.9118546564,-37.2742356128,7.90769532306));
#78618=CARTESIAN_POINT('',(-12.1117355269,-36.1242356128,9.07736288456));
#78619=CARTESIAN_POINT('Origin',(-11.9023253384,-36.1242356128,9.2921822807));
#78620=CARTESIAN_POINT('Origin',(-9.74681926603,-36.1242356128,11.5329750799));
#78621=CARTESIAN_POINT('',(-9.53740907755,-36.1242356128,11.7477944761));
#78622=CARTESIAN_POINT('Origin',(-8.32272875085,-37.2742356128,10.5637001125));
#78623=CARTESIAN_POINT('',(0.,0.,0.));
#78624=CARTESIAN_POINT('Origin',(7.54951656745E-15,-20.7780221998,-1.3270392201));
#78625=CARTESIAN_POINT('',(-3.61308907991371,-19.2125922380406,-0.960540656330234));
#78626=CARTESIAN_POINT('',(-3.88711717726,-19.0254782583927,-1.22484599905396));
#78627=CARTESIAN_POINT('Ctrl Pts',(-3.61308907991371,-19.2125922380406,
-0.960540656330234));
#78628=CARTESIAN_POINT('Ctrl Pts',(-3.61334186378693,-19.1910253579796,
-1.05216616964079));
#78629=CARTESIAN_POINT('Ctrl Pts',(-3.64741581668055,-19.1548229963094,
-1.14028371652892));
#78630=CARTESIAN_POINT('Ctrl Pts',(-3.71492697253399,-19.108516931192,-1.20628614736713));
#78631=CARTESIAN_POINT('Ctrl Pts',(-3.801022074897,-19.0627803730605,-1.23357916236737));
#78632=CARTESIAN_POINT('Ctrl Pts',(-3.88711717726,-19.0254782583,-1.22484599945));
#78633=CARTESIAN_POINT('',(-3.64161503967,-19.2306411737,-0.82776370433));
#78634=CARTESIAN_POINT('Origin',(-3.93441475488739,-19.0698572267847,-0.942962194752341));
#78635=CARTESIAN_POINT('',(-2.63891667039959,-17.8998816182875,-0.516206449181057));
#78636=CARTESIAN_POINT('Origin',(7.51064056026E-15,-20.8084305484,-1.19715554699));
#78637=CARTESIAN_POINT('',(-2.61824688650184,-17.8922584277925,-0.651424276437992));
#78638=CARTESIAN_POINT('Origin',(-2.76894427741165,-17.7302609546611,-0.594856157802496));
#78639=CARTESIAN_POINT('',(-2.81682310404,-17.6050062358,-0.892285274267));
#78640=CARTESIAN_POINT('Ctrl Pts',(-2.61824688650184,-17.8922584277925,
-0.651424276437992));
#78641=CARTESIAN_POINT('Ctrl Pts',(-2.61820300293512,-17.8744033188817,
-0.72790778770481));
#78642=CARTESIAN_POINT('Ctrl Pts',(-2.63960889197191,-17.8330169329895,
-0.798385310068769));
#78643=CARTESIAN_POINT('Ctrl Pts',(-2.71314604228615,-17.7266466553736,
-0.8875574924106));
#78644=CARTESIAN_POINT('Ctrl Pts',(-2.76482447353174,-17.6623177748382,
-0.905703044325404));
#78645=CARTESIAN_POINT('Ctrl Pts',(-2.81682310404,-17.6050062358,-0.892285274267));
#78646=CARTESIAN_POINT('Origin',(4.85143369921559E-9,-20.7096354418264,
-1.61914066024343));
#78647=CARTESIAN_POINT('Origin',(-6.2172489379E-15,-20.3611579168,2.27304371988));
#78648=CARTESIAN_POINT('',(-3.29086024220978,-18.2454109371054,1.04173423462419));
#78649=CARTESIAN_POINT('',(-3.53153637160979,-17.9397782141428,1.21096986282933));
#78650=CARTESIAN_POINT('Origin',(-3.52914694744576,-18.0912695033716,0.95419825055126));
#78651=CARTESIAN_POINT('',(-3.30849193722298,-18.2908119190758,0.937647175475319));
#78652=CARTESIAN_POINT('Origin',(-3.53120754646385,-18.090985806266,0.951651527640288));
#78653=CARTESIAN_POINT('',(-3.61003714743049,-18.6956696732126,1.17326396065629));
#78654=CARTESIAN_POINT('Origin',(-6.2172489379E-15,-20.4178945359,2.17555373363));
#78655=CARTESIAN_POINT('',(-3.59076491541284,-18.6481271742909,1.27610468451569));
#78656=CARTESIAN_POINT('Origin',(-3.85341043799,-18.5228280068,1.20318385007));
#78657=CARTESIAN_POINT('',(-3.85341043799,-18.3719297863,1.46247080897));
#78658=CARTESIAN_POINT('Origin',(-3.85341043799,-18.5228280068,1.20318385007));
#78659=CARTESIAN_POINT('Origin',(0.00142139409255115,-20.2110499150628,
2.53279056392384));
#78660=CARTESIAN_POINT('Origin',(4.55191440096E-15,-20.9224910251,0.373199680532));
#78661=CARTESIAN_POINT('',(3.37113078829735,-18.8600780815313,2.36677038101639));
#78662=CARTESIAN_POINT('',(3.36990985449358,-18.8395487394787,2.34355634748983));
#78663=CARTESIAN_POINT('Origin',(3.59839803273,-18.6983201284,2.47715137666));
#78664=CARTESIAN_POINT('',(3.59839803273,-18.4921598488,2.25921115747));
#78665=CARTESIAN_POINT('Origin',(3.59839803273,-18.6983201284,2.47715137666));
#78666=CARTESIAN_POINT('',(-3.59839802628,-18.4921598544775,2.25921116347192));
#78667=CARTESIAN_POINT('Origin',(-2.62234678416E-13,-20.7163307455,0.155259461344));
#78668=CARTESIAN_POINT('',(-3.36990985449358,-18.8395487394775,2.34355634748858));
#78669=CARTESIAN_POINT('Origin',(-3.59839803273,-18.6983201284,2.47715137666));
#78670=CARTESIAN_POINT('',(-3.37113078873609,-18.8600780898805,2.36677040528946));
#78671=CARTESIAN_POINT('Origin',(-3.59839803273,-18.6983201284,2.47715137666));
#78672=CARTESIAN_POINT('Origin',(4.54374776135E-15,-20.9437750269,0.39569984413));
#78673=CARTESIAN_POINT('Origin',(6.2172489379E-15,-20.3611579168,2.27304371988));
#78674=CARTESIAN_POINT('',(3.30849193622019,-18.2908119357476,0.937647359212487));
#78675=CARTESIAN_POINT('',(3.29086019657007,-18.2454109948681,1.04173426863756));
#78676=CARTESIAN_POINT('Origin',(3.53166730415163,-18.0906254246164,0.951572436110974));
#78677=CARTESIAN_POINT('',(3.53153633351,-17.9397782658,1.2109699402));
#78678=CARTESIAN_POINT('Ctrl Pts',(3.29086019657019,-18.2454109945417,1.04173426919817));
#78679=CARTESIAN_POINT('Ctrl Pts',(3.29082949183587,-18.2059257452771,1.10962705068825));
#78680=CARTESIAN_POINT('Ctrl Pts',(3.31677120622792,-18.149985595813,1.16738387145166));
#78681=CARTESIAN_POINT('Ctrl Pts',(3.40589056391193,-18.036820722088,1.23003743451762));
#78682=CARTESIAN_POINT('Ctrl Pts',(3.46851942482175,-17.9802928485517,1.23454836645887));
#78683=CARTESIAN_POINT('Ctrl Pts',(3.53153633351,-17.9397782658,1.2109699402));
#78684=CARTESIAN_POINT('',(3.85341040044001,-18.3719297862954,1.46247080897792));
#78685=CARTESIAN_POINT('Origin',(-0.00140566648756613,-20.211041526665,
2.53278568209601));
#78686=CARTESIAN_POINT('',(3.59076516652098,-18.6481269365579,1.27610454642206));
#78687=CARTESIAN_POINT('Origin',(3.8534092721712,-18.5228276087667,1.20318547093161));
#78688=CARTESIAN_POINT('',(3.61003708783018,-18.6956695658327,1.17326382994037));
#78689=CARTESIAN_POINT('Origin',(3.85338015716578,-18.5228452831943,1.20318513359903));
#78690=CARTESIAN_POINT('Origin',(6.20159509999E-15,-20.4178945359,2.17555373363));
#78691=CARTESIAN_POINT('Origin',(-1.68753899743E-14,-20.7780221998,-1.3270392201));
#78692=CARTESIAN_POINT('',(3.64161487464907,-19.2306407860628,-0.827763585289629));
#78693=CARTESIAN_POINT('',(3.61308908062573,-19.2125922405508,-0.960540656987445));
#78694=CARTESIAN_POINT('Origin',(3.82106060895697,-19.1266175913241,-0.921769890875969));
#78695=CARTESIAN_POINT('',(3.88711718104,-19.0254782583,-1.22484599945));
#78696=CARTESIAN_POINT('Ctrl Pts',(3.61308908062573,-19.2125922405508,-0.960540656987445));
#78697=CARTESIAN_POINT('Ctrl Pts',(3.6130284012607,-19.1947148817522,-1.03701895910761));
#78698=CARTESIAN_POINT('Ctrl Pts',(3.64256777805805,-19.1641230915394,-1.11002371080264));
#78699=CARTESIAN_POINT('Ctrl Pts',(3.74404646871257,-19.0948362447271,-1.2078778611402));
#78700=CARTESIAN_POINT('Ctrl Pts',(3.81536089299333,-19.0565678454691,-1.23212468954696));
#78701=CARTESIAN_POINT('Ctrl Pts',(3.88711718104,-19.0254782583,-1.22484599945));
#78702=CARTESIAN_POINT('',(2.81682317483321,-17.6050062274254,-0.892285262814533));
#78703=CARTESIAN_POINT('Origin',(-8.31938484768813E-8,-20.7096353378519,
-1.61914063590086));
#78704=CARTESIAN_POINT('',(2.61824690546747,-17.8922583873498,-0.651424266668572));
#78705=CARTESIAN_POINT('Ctrl Pts',(2.61824690546748,-17.8922583873498,-0.651424266668573));
#78706=CARTESIAN_POINT('Ctrl Pts',(2.61843004860693,-17.8705990179235,-0.743028110698349));
#78707=CARTESIAN_POINT('Ctrl Pts',(2.64312195677522,-17.8219449998149,-0.828230451813944));
#78708=CARTESIAN_POINT('Ctrl Pts',(2.69204431205891,-17.7509683072632,-0.888456978613999));
#78709=CARTESIAN_POINT('Ctrl Pts',(2.75443362214528,-17.673769970339,-0.90838416964567));
#78710=CARTESIAN_POINT('Ctrl Pts',(2.81682319433,-17.6050062358,-0.892285274267));
#78711=CARTESIAN_POINT('',(2.63891853137576,-17.8998831837931,-0.516206775081432));
#78712=CARTESIAN_POINT('Origin',(2.85113685828544,-17.6320686833311,-0.606360018255462));
#78713=CARTESIAN_POINT('Origin',(-1.69216709352E-14,-20.8084305484,-1.19715554699));
#78714=CARTESIAN_POINT('Origin',(-3.53495011041E-13,-21.0197764855,0.650835506465));
#78715=CARTESIAN_POINT('',(-4.0532699789542,-21.571070890106,-0.0674504972475476));
#78716=CARTESIAN_POINT('',(4.05326999191,-21.5710708896,-0.0674504957552));
#78717=CARTESIAN_POINT('Origin',(-3.53328477587E-13,-21.3048372788,0.744325314097));
#78718=CARTESIAN_POINT('',(4.34627739081414,-21.2879280691877,-0.225306331462357));
#78719=CARTESIAN_POINT('Ctrl Pts',(4.34627740764,-21.2879283386,-0.225306246837));
#78720=CARTESIAN_POINT('Ctrl Pts',(4.35210058992,-21.3811601618,-0.196020670745));
#78721=CARTESIAN_POINT('Ctrl Pts',(4.31892160248,-21.4741377387,-0.1581676115));
#78722=CARTESIAN_POINT('Ctrl Pts',(4.24485535575,-21.5457105806,-0.118264986841));
#78723=CARTESIAN_POINT('Ctrl Pts',(4.14906267383,-21.5773629037,-0.0866355443942));
#78724=CARTESIAN_POINT('Ctrl Pts',(4.05326999191,-21.5710708896,-0.0674504957552));
#78725=CARTESIAN_POINT('',(0.881570449864,-19.6457838359,4.78177176907));
#78726=CARTESIAN_POINT('Origin',(-3.53505134421E-13,-21.0024479625,0.645152366871));
#78727=CARTESIAN_POINT('',(-4.44088090492117,-20.9747479205191,0.729452226642898));
#78728=CARTESIAN_POINT('Ctrl Pts',(-4.44088090408204,-20.9747479074319,
0.729452222330876));
#78729=CARTESIAN_POINT('Ctrl Pts',(-4.44033851341439,-20.9662886381893,
0.755232231741162));
#78730=CARTESIAN_POINT('Ctrl Pts',(-4.43956056840391,-20.9580332073157,
0.780396132983051));
#78731=CARTESIAN_POINT('Ctrl Pts',(-4.43858185727784,-20.9499840167878,
0.804940747821991));
#78732=CARTESIAN_POINT('Ctrl Pts',(-4.43636923292827,-20.9317867832202,
0.860430065350874));
#78733=CARTESIAN_POINT('Ctrl Pts',(-4.43313310769655,-20.9146392251699,
0.91275188851088));
#78734=CARTESIAN_POINT('Ctrl Pts',(-4.42924276556979,-20.8985397211973,
0.961885171997912));
#78735=CARTESIAN_POINT('Ctrl Pts',(-4.42729759450641,-20.890489969211,0.986451813741426));
#78736=CARTESIAN_POINT('Ctrl Pts',(-4.42518817421974,-20.8827019166165,
1.01022167687519));
#78737=CARTESIAN_POINT('Ctrl Pts',(-4.42295644747595,-20.8751737494359,
1.03319399384914));
#78738=CARTESIAN_POINT('Ctrl Pts',(-4.42184058410406,-20.8714096658456,
1.04468015233612));
#78739=CARTESIAN_POINT('Ctrl Pts',(-4.42069410285316,-20.8677105572313,
1.05596692134127));
#78740=CARTESIAN_POINT('Ctrl Pts',(-4.41952197679202,-20.864076097256,1.06705432209663));
#78741=CARTESIAN_POINT('Ctrl Pts',(-4.41893591376145,-20.8622588672683,
1.07259802247431));
#78742=CARTESIAN_POINT('Ctrl Pts',(-4.41834343689534,-20.8604577996644,
1.07809188062318));
#78743=CARTESIAN_POINT('Ctrl Pts',(-4.41774515166877,-20.8586728527503,
1.08353590073895));
#78744=CARTESIAN_POINT('Ctrl Pts',(-4.41744600905548,-20.8577803792933,
1.08625791079684));
#78745=CARTESIAN_POINT('Ctrl Pts',(-4.41714541418869,-20.8568919360236,
1.08896746133314));
#78746=CARTESIAN_POINT('Ctrl Pts',(-4.41684344169986,-20.8560075174297,
1.0916645532355));
#78747=CARTESIAN_POINT('Ctrl Pts',(-4.41654146921104,-20.8551230988358,
1.09436164513785));
#78748=CARTESIAN_POINT('Ctrl Pts',(-4.41639664022107,-20.854698710831,1.09565585986192));
#78749=CARTESIAN_POINT('Ctrl Pts',(-4.41593346532297,-20.8533663301158,
1.09971845399856));
#78750=CARTESIAN_POINT('Ctrl Pts',(-4.40600422226456,-20.8248036165033,
1.18680971217248));
#78751=CARTESIAN_POINT('Ctrl Pts',(-4.39347291508139,-20.7970283698894,
1.27137761754194));
#78752=CARTESIAN_POINT('Ctrl Pts',(-4.37878794010872,-20.7701000627841,
1.35332388292646));
#78753=CARTESIAN_POINT('Ctrl Pts',(-4.36368716048736,-20.7424092814289,
1.43759045448469));
#78754=CARTESIAN_POINT('Ctrl Pts',(-4.34630941899308,-20.7156140029929,
1.5190850588711));
#78755=CARTESIAN_POINT('Ctrl Pts',(-4.32712048226691,-20.6897627700988,
1.59774998432596));
#78756=CARTESIAN_POINT('Ctrl Pts',(-4.30925992593525,-20.6657011241651,
1.67096922270594));
#78757=CARTESIAN_POINT('Ctrl Pts',(-4.28983019135619,-20.6424570841339,
1.74173778434547));
#78758=CARTESIAN_POINT('Ctrl Pts',(-4.26918657483247,-20.6200588534231,
1.81004248360131));
#78759=CARTESIAN_POINT('Ctrl Pts',(-4.24613721574523,-20.5950504028942,
1.88630719907324));
#78760=CARTESIAN_POINT('Ctrl Pts',(-4.22157405504016,-20.5710831539992,
1.95949758770353));
#78761=CARTESIAN_POINT('Ctrl Pts',(-4.19595352642011,-20.5481355019429,
2.02962580328218));
#78762=CARTESIAN_POINT('Ctrl Pts',(-4.1857871916205,-20.5390297759397,2.0574529776955));
#78763=CARTESIAN_POINT('Ctrl Pts',(-4.17545396884154,-20.5300844554319,
2.08479840962057));
#78764=CARTESIAN_POINT('Ctrl Pts',(-4.16498076975541,-20.5212976997503,
2.11166435494956));
#78765=CARTESIAN_POINT('Ctrl Pts',(-4.14654723630162,-20.505832419899,2.15895022223016));
#78766=CARTESIAN_POINT('Ctrl Pts',(-4.12768045405037,-20.4908572953069,
2.20475019302771));
#78767=CARTESIAN_POINT('Ctrl Pts',(-4.10851920046663,-20.4763542193862,
2.24908112387));
#78768=CARTESIAN_POINT('Ctrl Pts',(-4.09893857367477,-20.4691026814258,
2.27124658929114));
#78769=CARTESIAN_POINT('Ctrl Pts',(-4.08928424644404,-20.4619691715805,
2.29304476363202));
#78770=CARTESIAN_POINT('Ctrl Pts',(-4.07957257855448,-20.4549507827894,
2.3144784185172));
#78771=CARTESIAN_POINT('Ctrl Pts',(-4.0747167446097,-20.4514415883938,2.3251952459598));
#78772=CARTESIAN_POINT('Ctrl Pts',(-4.06984656963281,-20.4479611753603,
2.33582094142983));
#78773=CARTESIAN_POINT('Ctrl Pts',(-4.06496405358873,-20.4445091710698,
2.34635585710495));
#78774=CARTESIAN_POINT('Ctrl Pts',(-4.06252279556669,-20.4427831689246,
2.3516233149425));
#78775=CARTESIAN_POINT('Ctrl Pts',(-4.06007845192657,-20.4410642690357,
2.35686807769117));
#78776=CARTESIAN_POINT('Ctrl Pts',(-4.05763126898474,-20.4393524229206,
2.36209019124524));
#78777=CARTESIAN_POINT('Ctrl Pts',(-4.05640767751383,-20.438496499863,2.36470124802228));
#78778=CARTESIAN_POINT('Ctrl Pts',(-4.0551833761952,-20.4376423402533,2.36730664249168));
#78779=CARTESIAN_POINT('Ctrl Pts',(-4.05395839558517,-20.436789937912,2.36990638050782));
#78780=CARTESIAN_POINT('Ctrl Pts',(-4.05273341497514,-20.4359375355706,
2.37250611852396));
#78781=CARTESIAN_POINT('Ctrl Pts',(-4.05197605007509,-20.4354110607625,
2.37411174650506));
#78782=CARTESIAN_POINT('Ctrl Pts',(-4.0502814463181,-20.4342379964883,2.37768863106475));
#78783=CARTESIAN_POINT('Ctrl Pts',(-4.01118861434413,-20.4071765643552,
2.4602038187628));
#78784=CARTESIAN_POINT('Ctrl Pts',(-3.97020611342597,-20.3810987770343,
2.5396031757798));
#78785=CARTESIAN_POINT('Ctrl Pts',(-3.92779118828007,-20.3560255577381,
2.61590725626987));
#78786=CARTESIAN_POINT('Ctrl Pts',(-3.8842719929869,-20.3302995586135,2.69419790912594));
#78787=CARTESIAN_POINT('Ctrl Pts',(-3.83924511714191,-20.3056310140628,
2.76923032883936));
#78788=CARTESIAN_POINT('Ctrl Pts',(-3.79317122967888,-20.2820286625872,
2.84106897626654));
#78789=CARTESIAN_POINT('Ctrl Pts',(-3.7595712346176,-20.2648163339412,2.89345826511696));
#78790=CARTESIAN_POINT('Ctrl Pts',(-3.72541371197391,-20.2481707330716,
2.94414994133828));
#78791=CARTESIAN_POINT('Ctrl Pts',(-3.6908654173721,-20.2320912954077,2.99318105905564));
#78792=CARTESIAN_POINT('Ctrl Pts',(-3.64181519957344,-20.2092623850784,
3.06279338089863));
#78793=CARTESIAN_POINT('Ctrl Pts',(-3.59197772397555,-20.1875641826927,
3.129055007804));
#78794=CARTESIAN_POINT('Ctrl Pts',(-3.54178606204226,-20.1669387782563,
3.19209064841556));
#78795=CARTESIAN_POINT('Ctrl Pts',(-3.52643993993718,-20.1606325520276,
3.21136382249541));
#78796=CARTESIAN_POINT('Ctrl Pts',(-3.51106040139271,-20.1544265486155,
3.23033562160662));
#78797=CARTESIAN_POINT('Ctrl Pts',(-3.49565901852874,-20.1483189501994,
3.24901010602001));
#78798=CARTESIAN_POINT('Ctrl Pts',(-3.46277212706782,-20.1352772689446,
3.28888611893496));
#78799=CARTESIAN_POINT('Ctrl Pts',(-3.42978594374505,-20.1226833054986,
3.32740609871667));
#78800=CARTESIAN_POINT('Ctrl Pts',(-3.39680598782897,-20.1105123700283,
3.36461160092258));
#78801=CARTESIAN_POINT('Ctrl Pts',(-3.38031600987093,-20.1044269022932,
3.38321435202554));
#78802=CARTESIAN_POINT('Ctrl Pts',(-3.36382754753937,-20.0984472056528,
3.40148845134646));
#78803=CARTESIAN_POINT('Ctrl Pts',(-3.34735285274272,-20.0925696281575,
3.41943945376333));
#78804=CARTESIAN_POINT('Ctrl Pts',(-3.33911550534439,-20.0896308394098,
3.42841495497177));
#78805=CARTESIAN_POINT('Ctrl Pts',(-3.33088159671428,-20.0867175814878,
3.43730967957859));
#78806=CARTESIAN_POINT('Ctrl Pts',(-3.32265262387178,-20.0838293880027,
3.44612432080446));
#78807=CARTESIAN_POINT('Ctrl Pts',(-3.31853813745052,-20.0823852912602,
3.4505316414174));
#78808=CARTESIAN_POINT('Ctrl Pts',(-3.31442488479339,-20.0809474606917,
3.45491894103536));
#78809=CARTESIAN_POINT('Ctrl Pts',(-3.31031304956928,-20.079515836159,3.45928630729641));
#78810=CARTESIAN_POINT('Ctrl Pts',(-3.30651415218028,-20.0781931677147,
3.46332128812166));
#78811=CARTESIAN_POINT('Ctrl Pts',(-3.30349448908605,-20.0771448996417,
3.46651871720658));
#78812=CARTESIAN_POINT('Ctrl Pts',(-3.2990978311697,-20.0756250992641,3.47115298296621));
#78813=CARTESIAN_POINT('Ctrl Pts',(-3.29873565223483,-20.0754999042427,
3.47153473507626));
#78814=CARTESIAN_POINT('Ctrl Pts',(-3.29836410744608,-20.0753715156315,
3.47192621856882));
#78815=CARTESIAN_POINT('Ctrl Pts',(-3.29798197842631,-20.0752395201448,
3.47232869357418));
#78816=CARTESIAN_POINT('Ctrl Pts',(-3.23758565072548,-20.0543773446535,
3.53594074881669));
#78817=CARTESIAN_POINT('Ctrl Pts',(-3.17676275542274,-20.0346312495266,
3.59610390764184));
#78818=CARTESIAN_POINT('Ctrl Pts',(-3.11592842027533,-20.0159631944352,
3.65300094151748));
#78819=CARTESIAN_POINT('Ctrl Pts',(-3.09584462036267,-20.0098001373014,
3.6717848838621));
#78820=CARTESIAN_POINT('Ctrl Pts',(-3.07575920417414,-20.0037545110479,
3.69021304856488));
#78821=CARTESIAN_POINT('Ctrl Pts',(-3.05568602350684,-19.9978247650746,
3.70829256654954));
#78822=CARTESIAN_POINT('Ctrl Pts',(-3.01524834858015,-19.9858792172294,
3.74471398292656));
#78823=CARTESIAN_POINT('Ctrl Pts',(-2.97486058219296,-19.9744025284116,
3.7797200084947));
#78824=CARTESIAN_POINT('Ctrl Pts',(-2.93462718600761,-19.9633722941119,
3.81336992203629));
#78825=CARTESIAN_POINT('Ctrl Pts',(-2.91451048791493,-19.957857176962,3.83019487880708));
#78826=CARTESIAN_POINT('Ctrl Pts',(-2.89443234925921,-19.9524536882399,
3.8466807723206));
#78827=CARTESIAN_POINT('Ctrl Pts',(-2.87440469997387,-19.9471582525925,
3.86283526515468));
#78828=CARTESIAN_POINT('Ctrl Pts',(-2.8643908753312,-19.9445105347688,3.87091251157173));
#78829=CARTESIAN_POINT('Ctrl Pts',(-2.85438967038263,-19.941889831371,3.87890690506955));
#78830=CARTESIAN_POINT('Ctrl Pts',(-2.84440253537844,-19.9392956772258,
3.88681939970655));
#78831=CARTESIAN_POINT('Ctrl Pts',(-2.83669748021923,-19.9372942923669,
3.89292387387251));
#78832=CARTESIAN_POINT('Ctrl Pts',(-2.82962993939577,-19.9354704767983,
3.89848634882859));
#78833=CARTESIAN_POINT('Ctrl Pts',(-2.82174497977312,-19.9334493944361,
3.90464952892944));
#78834=CARTESIAN_POINT('Ctrl Pts',(-2.81940961590337,-19.9328507911518,
3.90647493689843));
#78835=CARTESIAN_POINT('Ctrl Pts',(-2.8170023346954,-19.9322349629246,3.90835279692559));
#78836=CARTESIAN_POINT('Ctrl Pts',(-2.81448476520693,-19.9315923875919,
3.91031213762162));
#78837=CARTESIAN_POINT('Ctrl Pts',(-2.74611514202516,-19.9141419721958,
3.96352194401839));
#78838=CARTESIAN_POINT('Ctrl Pts',(-2.6779675900044,-19.8977925243118,4.01331402163749));
#78839=CARTESIAN_POINT('Ctrl Pts',(-2.61040908145182,-19.8824919207325,
4.05993977067158));
#78840=CARTESIAN_POINT('Ctrl Pts',(-2.59087155071088,-19.8780670744889,
4.07342366817893));
#78841=CARTESIAN_POINT('Ctrl Pts',(-2.57138296302871,-19.8737299153642,
4.08664285027023));
#78842=CARTESIAN_POINT('Ctrl Pts',(-2.55195142198082,-19.8694791150827,
4.0996036035047));
#78843=CARTESIAN_POINT('Ctrl Pts',(-2.5086396471951,-19.8600043284975,4.12849236861916));
#78844=CARTESIAN_POINT('Ctrl Pts',(-2.46561133153172,-19.8509567140269,
4.15609677884506));
#78845=CARTESIAN_POINT('Ctrl Pts',(-2.42294637854088,-19.8423099220236,
4.18248542023493));
#78846=CARTESIAN_POINT('Ctrl Pts',(-2.40161390204546,-19.837986526022,4.19567974092987));
#78847=CARTESIAN_POINT('Ctrl Pts',(-2.38037223624416,-19.833763353459,4.2085700759519));
#78848=CARTESIAN_POINT('Ctrl Pts',(-2.35923010187459,-19.829636189821,4.22116502061894));
#78849=CARTESIAN_POINT('Ctrl Pts',(-2.34530431694811,-19.8269177323476,
4.22946098958442));
#78850=CARTESIAN_POINT('Ctrl Pts',(-2.33192749888427,-19.8243381868342,
4.23733234032053));
#78851=CARTESIAN_POINT('Ctrl Pts',(-2.3181038302266,-19.8217035718007,4.24536913204935));
#78852=CARTESIAN_POINT('Ctrl Pts',(-2.31094039749043,-19.8203383128347,
4.24953380196365));
#78853=CARTESIAN_POINT('Ctrl Pts',(-2.30365653629527,-19.8189584821368,
4.25374223887199));
#78854=CARTESIAN_POINT('Ctrl Pts',(-2.29611081239421,-19.8175385538874,
4.25807207736949));
#78855=CARTESIAN_POINT('Ctrl Pts',(-2.22478241720023,-19.8041162229556,
4.29900127588314));
#78856=CARTESIAN_POINT('Ctrl Pts',(-2.15398926896422,-19.791648078878,4.33701687720016));
#78857=CARTESIAN_POINT('Ctrl Pts',(-2.08420171936975,-19.780091596446,4.37225205974607));
#78858=CARTESIAN_POINT('Ctrl Pts',(-2.01208080452018,-19.7681487199547,
4.40866533997827));
#78859=CARTESIAN_POINT('Ctrl Pts',(-1.94103439245925,-19.7571793779235,
4.44210949940517));
#78860=CARTESIAN_POINT('Ctrl Pts',(-1.87156021712279,-19.7471205066914,
4.47278070489698));
#78861=CARTESIAN_POINT('Ctrl Pts',(-1.84157455921399,-19.7427790104411,
4.48601866376549));
#78862=CARTESIAN_POINT('Ctrl Pts',(-1.81188147450031,-19.7386069332423,
4.49874063615051));
#78863=CARTESIAN_POINT('Ctrl Pts',(-1.78251945458098,-19.7345984158543,
4.5109647993908));
#78864=CARTESIAN_POINT('Ctrl Pts',(-1.70718535143936,-19.7243137670739,
4.54232832195819));
#78865=CARTESIAN_POINT('Ctrl Pts',(-1.63291517057692,-19.7149314387773,
4.57087456090056));
#78866=CARTESIAN_POINT('Ctrl Pts',(-1.55983928822529,-19.7063873463962,
4.59691663623052));
#78867=CARTESIAN_POINT('Ctrl Pts',(-1.55375173433672,-19.7056755845793,
4.59908605973716));
#78868=CARTESIAN_POINT('Ctrl Pts',(-1.54767244104875,-19.7049696434347,
4.60123809422092));
#78869=CARTESIAN_POINT('Ctrl Pts',(-1.54160146907483,-19.7042694879189,
4.6033729145871));
#78870=CARTESIAN_POINT('Ctrl Pts',(-1.50212756776972,-19.6997170258344,
4.61725367186955));
#78871=CARTESIAN_POINT('Ctrl Pts',(-1.46300461299036,-19.6954074668301,
4.63040669962543));
#78872=CARTESIAN_POINT('Ctrl Pts',(-1.42423897861779,-19.6913228213346,
4.642878158682));
#78873=CARTESIAN_POINT('Ctrl Pts',(-1.40485616143151,-19.6892804985869,
4.64911388821028));
#78874=CARTESIAN_POINT('Ctrl Pts',(-1.38556265643057,-19.6872944243512,
4.65517917530087));
#78875=CARTESIAN_POINT('Ctrl Pts',(-1.36635812914976,-19.6853618384192,
4.66107956383069));
#78876=CARTESIAN_POINT('Ctrl Pts',(-1.35378375648046,-19.6840964568053,
4.66494290725918));
#78877=CARTESIAN_POINT('Ctrl Pts',(-1.34051452660817,-19.6827816842502,
4.66895619379731));
#78878=CARTESIAN_POINT('Ctrl Pts',(-1.32798939829712,-19.6815595627749,
4.6726853210244));
#78879=CARTESIAN_POINT('Ctrl Pts',(-1.32138520901345,-19.6809151684542,
4.67465159725399));
#78880=CARTESIAN_POINT('Ctrl Pts',(-1.31498818680823,-19.6802962481877,
4.67653973989695));
#78881=CARTESIAN_POINT('Ctrl Pts',(-1.30901098191806,-19.6797219011273,
4.6782913668485));
#78882=CARTESIAN_POINT('Ctrl Pts',(-1.23975806031836,-19.6730674175229,
4.69858601730414));
#78883=CARTESIAN_POINT('Ctrl Pts',(-1.1715125981574,-19.6671035761371,4.71683336740599));
#78884=CARTESIAN_POINT('Ctrl Pts',(-1.104147192934,-19.6617360511869,4.73326901928545));
#78885=CARTESIAN_POINT('Ctrl Pts',(-1.03678178771059,-19.6563685262367,
4.7497046711649));
#78886=CARTESIAN_POINT('Ctrl Pts',(-0.970295895358319,-19.6515973499143,
4.76432852674912));
#78887=CARTESIAN_POINT('Ctrl Pts',(-0.904531595433205,-19.6473433846981,
4.77732987546702));
#78888=CARTESIAN_POINT('Ctrl Pts',(-0.844034296727092,-19.6434301155738,
4.78928995833667));
#78889=CARTESIAN_POINT('Ctrl Pts',(-0.784130214998427,-19.6399493355338,
4.79987958392767));
#78890=CARTESIAN_POINT('Ctrl Pts',(-0.724577840661874,-19.6368606964938,
4.80922780530557));
#78891=CARTESIAN_POINT('Ctrl Pts',(-0.71939310622028,-19.6365917941472,
4.81004167789899));
#78892=CARTESIAN_POINT('Ctrl Pts',(-0.714211027536302,-19.6363258737797,
4.81084611154134));
#78893=CARTESIAN_POINT('Ctrl Pts',(-0.709031439732714,-19.6360629142671,
4.8116411746211));
#78894=CARTESIAN_POINT('Ctrl Pts',(-0.676695016060087,-19.6344212449816,
4.81660479287963));
#78895=CARTESIAN_POINT('Ctrl Pts',(-0.644454374652469,-19.6328953299266,
4.82120400448747));
#78896=CARTESIAN_POINT('Ctrl Pts',(-0.612260437535052,-19.6314855189305,
4.82545593040161));
#78897=CARTESIAN_POINT('Ctrl Pts',(-0.596163468976344,-19.6307806134325,
4.82758189335868));
#78898=CARTESIAN_POINT('Ctrl Pts',(-0.580078166296216,-19.630104762066,
4.82962096413189));
#78899=CARTESIAN_POINT('Ctrl Pts',(-0.563997665342666,-19.6294586694314,
4.83157512690825));
#78900=CARTESIAN_POINT('Ctrl Pts',(-0.552534605636963,-19.6289980992994,
4.83296816090916));
#78901=CARTESIAN_POINT('Ctrl Pts',(-0.540277388802875,-19.6285222854744,
4.83441058736567));
#78902=CARTESIAN_POINT('Ctrl Pts',(-0.528926901809803,-19.6280969826263,
4.83570367497362));
#78903=CARTESIAN_POINT('Ctrl Pts',(-0.524354806036902,-19.6279256661572,
4.83622454428874));
#78904=CARTESIAN_POINT('Ctrl Pts',(-0.519929910169658,-19.6277623502447,
4.83672177752299));
#78905=CARTESIAN_POINT('Ctrl Pts',(-0.515763655468914,-19.6276106046347,
4.83718460528559));
#78906=CARTESIAN_POINT('Ctrl Pts',(-0.462270835908533,-19.6256622598706,
4.8431271037093));
#78907=CARTESIAN_POINT('Ctrl Pts',(-0.409259551027216,-19.6240572226069,
4.84809105159708));
#78908=CARTESIAN_POINT('Ctrl Pts',(-0.356405021564706,-19.6227344098681,
4.85213514155229));
#78909=CARTESIAN_POINT('Ctrl Pts',(-0.351915189055131,-19.6226220409245,
4.85247867476954));
#78910=CARTESIAN_POINT('Ctrl Pts',(-0.347426483201641,-19.6225117180823,
4.85281554111355));
#78911=CARTESIAN_POINT('Ctrl Pts',(-0.342938702630177,-19.6224034092166,
4.85314576034748));
#78912=CARTESIAN_POINT('Ctrl Pts',(-0.310871126117556,-19.6216294848273,
4.85550535221737));
#78913=CARTESIAN_POINT('Ctrl Pts',(-0.278439324545288,-19.6209494103661,
4.85755146880844));
#78914=CARTESIAN_POINT('Ctrl Pts',(-0.246251603405228,-19.6203854740379,
4.85924693559752));
#78915=CARTESIAN_POINT('Ctrl Pts',(-0.220906421391697,-19.6199414205798,
4.86058197619205));
#78916=CARTESIAN_POINT('Ctrl Pts',(-0.195712706518268,-19.6195690415602,
4.86170062386772));
#78917=CARTESIAN_POINT('Ctrl Pts',(-0.170968442363936,-19.6192721290622,
4.86260634567848));
#78918=CARTESIAN_POINT('Ctrl Pts',(-0.120043389665838,-19.6186610668574,
4.8644703708382));
#78919=CARTESIAN_POINT('Ctrl Pts',(-0.0695096448294374,-19.6183493595768,
4.86549911419981));
#78920=CARTESIAN_POINT('Ctrl Pts',(-0.019010528798765,-19.6182855485251,
4.86570589228436));
#78921=CARTESIAN_POINT('Ctrl Pts',(-0.0138106051836958,-19.6182789778637,
4.86572718434508));
#78922=CARTESIAN_POINT('Ctrl Pts',(-0.00861104704102354,-19.6182750498029,
4.86573971794318));
#78923=CARTESIAN_POINT('Ctrl Pts',(-0.00341146415241323,-19.6182737179049,
4.86574347790516));
#78924=CARTESIAN_POINT('Ctrl Pts',(0.0244362308228306,-19.6182665845848,
4.86576361534244));
#78925=CARTESIAN_POINT('Ctrl Pts',(0.0522848670786102,-19.6183355811537,
4.86553316457071));
#78926=CARTESIAN_POINT('Ctrl Pts',(0.0801947426845153,-19.6184852044545,
4.86505132588967));
#78927=CARTESIAN_POINT('Ctrl Pts',(0.0966689801100628,-19.6185735219309,
4.86476691312681));
#78928=CARTESIAN_POINT('Ctrl Pts',(0.112524662857614,-19.6186850569718,
4.86440975997926));
#78929=CARTESIAN_POINT('Ctrl Pts',(0.128907271508895,-19.6188300157461,
4.86395649894601));
#78930=CARTESIAN_POINT('Ctrl Pts',(0.140279305318237,-19.6189306392865,
4.8636418665267));
#78931=CARTESIAN_POINT('Ctrl Pts',(0.151905232556995,-19.6190476668708,
4.86328001337933));
#78932=CARTESIAN_POINT('Ctrl Pts',(0.164167684591193,-19.6191891080271,
4.86284911049531));
#78933=CARTESIAN_POINT('Ctrl Pts',(0.219243055735599,-19.6198243744615,
4.86091376051812));
#78934=CARTESIAN_POINT('Ctrl Pts',(0.273839067448982,-19.6207726130671,
4.85802404995734));
#78935=CARTESIAN_POINT('Ctrl Pts',(0.328278900113335,-19.6220303246855,
4.85419059485297));
#78936=CARTESIAN_POINT('Ctrl Pts',(0.382727880026239,-19.6232882476307,
4.8503564956326));
#78937=CARTESIAN_POINT('Ctrl Pts',(0.437020950294054,-19.6248557620228,
4.84557829070741));
#78938=CARTESIAN_POINT('Ctrl Pts',(0.491478298025858,-19.6267454877189,
4.83981744742401));
#78939=CARTESIAN_POINT('Ctrl Pts',(0.545598398233708,-19.6286235105807,
4.83409228032049));
#78940=CARTESIAN_POINT('Ctrl Pts',(0.59988106922271,-19.630819769465,4.82739659815985));
#78941=CARTESIAN_POINT('Ctrl Pts',(0.654632697086247,-19.6333624172747,
4.81964450729371));
#78942=CARTESIAN_POINT('Ctrl Pts',(0.708445951353243,-19.6358614873194,
4.81202527745237));
#78943=CARTESIAN_POINT('Ctrl Pts',(0.762712537127494,-19.6386951824065,
4.80338551612137));
#78944=CARTESIAN_POINT('Ctrl Pts',(0.817711082827369,-19.6419053928723,
4.79359744533806));
#78945=CARTESIAN_POINT('Ctrl Pts',(0.838884132943331,-19.64314124277,4.78982928546044));
#78946=CARTESIAN_POINT('Ctrl Pts',(0.860165508044187,-19.644433055478,4.7858904484103));
#78947=CARTESIAN_POINT('Ctrl Pts',(0.881570449864978,-19.6457838358982,
4.7817717690745));
#78948=CARTESIAN_POINT('',(-4.34627742980843,-21.2879273673038,-0.2253061846382));
#78949=CARTESIAN_POINT('Ctrl Pts',(-4.34627742739142,-21.2879273614,-0.225306186038311));
#78950=CARTESIAN_POINT('Ctrl Pts',(-4.34876256073138,-21.2842530500451,
-0.214102742103554));
#78951=CARTESIAN_POINT('Ctrl Pts',(-4.3519425262521,-21.2794971786555,-0.199560523662125));
#78952=CARTESIAN_POINT('Ctrl Pts',(-4.35570626500914,-21.2736452569576,
-0.181658306238884));
#78953=CARTESIAN_POINT('Ctrl Pts',(-4.35946565330856,-21.2678000994214,
-0.163776781760393));
#78954=CARTESIAN_POINT('Ctrl Pts',(-4.36380750279823,-21.2608613548734,
-0.142542810694277));
#78955=CARTESIAN_POINT('Ctrl Pts',(-4.36856958664169,-21.2528125480096,
-0.117929036995139));
#78956=CARTESIAN_POINT('Ctrl Pts',(-4.37331768326236,-21.2447873821523,
-0.0933875590277396));
#78957=CARTESIAN_POINT('Ctrl Pts',(-4.37848357402662,-21.2356585710447,
-0.0654858160552947));
#78958=CARTESIAN_POINT('Ctrl Pts',(-4.38385473197136,-21.2254089829913,
-0.034194250688982));
#78959=CARTESIAN_POINT('Ctrl Pts',(-4.38540961945695,-21.2224418469732,
-0.0251357080259122));
#78960=CARTESIAN_POINT('Ctrl Pts',(-4.38698137592943,-21.2193807860287,
-0.0157930867037397));
#78961=CARTESIAN_POINT('Ctrl Pts',(-4.3885640285451,-21.216225391,-0.00616568935559134));
#78962=CARTESIAN_POINT('Ctrl Pts',(-4.39398839891311,-21.20541061641,0.0268311719766124));
#78963=CARTESIAN_POINT('Ctrl Pts',(-4.3995446940136,-21.1934868320056,0.0631739988383164));
#78964=CARTESIAN_POINT('Ctrl Pts',(-4.40495994007788,-21.1804469665788,
0.102890079547786));
#78965=CARTESIAN_POINT('Ctrl Pts',(-4.40854074396456,-21.1718244219616,
0.129152135690801));
#78966=CARTESIAN_POINT('Ctrl Pts',(-4.41205882742973,-21.162713903488,0.156889047950214));
#78967=CARTESIAN_POINT('Ctrl Pts',(-4.41542294788823,-21.1531141059222,
0.18610645229467));
#78968=CARTESIAN_POINT('Ctrl Pts',(-4.41964878608593,-21.1410553251072,
0.222807879856458));
#78969=CARTESIAN_POINT('Ctrl Pts',(-4.42363246084328,-21.1282252001997,
0.261845944632033));
#78970=CARTESIAN_POINT('Ctrl Pts',(-4.42717158187633,-21.114630400055,0.303226839575934));
#78971=CARTESIAN_POINT('Ctrl Pts',(-4.42894114239285,-21.1078329999827,
0.323917287047885));
#78972=CARTESIAN_POINT('Ctrl Pts',(-4.4305991886873,-21.1008445658588,0.345193332465333));
#78973=CARTESIAN_POINT('Ctrl Pts',(-4.43211818822347,-21.0936668708972,
0.367054961915476));
#78974=CARTESIAN_POINT('Ctrl Pts',(-4.43287768799156,-21.0900780234164,
0.377985776640548));
#78975=CARTESIAN_POINT('Ctrl Pts',(-4.43360240346858,-21.0864418615886,
0.389062989167634));
#78976=CARTESIAN_POINT('Ctrl Pts',(-4.43428875480373,-21.0827586876202,
0.400286525438272));
#78977=CARTESIAN_POINT('Ctrl Pts',(-4.43463193047131,-21.080917100636,0.40589829357359));
#78978=CARTESIAN_POINT('Ctrl Pts',(-4.43496551371776,-21.0790637606659,
0.411546642765532));
#78979=CARTESIAN_POINT('Ctrl Pts',(-4.43528904862596,-21.0771987086789,
0.41723156134437));
#78980=CARTESIAN_POINT('Ctrl Pts',(-4.43558652017649,-21.0754839017375,
0.422458513680551));
#78981=CARTESIAN_POINT('Ctrl Pts',(-4.43594350612929,-21.0733400774869,
0.428994312633909));
#78982=CARTESIAN_POINT('Ctrl Pts',(-4.43617196726052,-21.0719233268787,
0.433314000298841));
#78983=CARTESIAN_POINT('Ctrl Pts',(-4.43619198418035,-21.0717991964273,
0.433692475364639));
#78984=CARTESIAN_POINT('Ctrl Pts',(-4.43621104747127,-21.0716806479611,
0.434053936609418));
#78985=CARTESIAN_POINT('Ctrl Pts',(-4.43622904681129,-21.0715684593114,
0.434396012400812));
#78986=CARTESIAN_POINT('Ctrl Pts',(-4.43973687615582,-21.0497044000089,
0.501061984502047));
#78987=CARTESIAN_POINT('Ctrl Pts',(-4.44142459043637,-21.028785541782,0.564800751777492));
#78988=CARTESIAN_POINT('Ctrl Pts',(-4.44172071894098,-21.0088522514293,
0.625534487408663));
#78989=CARTESIAN_POINT('Ctrl Pts',(-4.44189468413807,-20.9971421366286,
0.661213444767486));
#78990=CARTESIAN_POINT('Ctrl Pts',(-4.44158774005072,-20.9857719093663,
0.695856072893091));
#78991=CARTESIAN_POINT('Ctrl Pts',(-4.44088090408204,-20.9747479074319,
0.729452222330876));
#78992=CARTESIAN_POINT('Origin',(-4.05326997582804,-21.2860101201162,-0.160940375904291));
#78993=CARTESIAN_POINT('Origin',(0.,-22.8742356128,-0.678262730068));
#78994=CARTESIAN_POINT('',(3.62140732971,-22.8742356128,-0.813060915858));
#78995=CARTESIAN_POINT('',(-3.62140732971,-22.8742356128,-0.813060915858));
#78996=CARTESIAN_POINT('',(-2.26135909998E-9,-22.8742356128,-0.813060915858));
#78997=CARTESIAN_POINT('Origin',(4.36973020788E-13,-22.8742356128,0.729452270839));
#78998=CARTESIAN_POINT('Origin',(-2.26135909998E-9,-22.5742356128,-0.813060915858));
#78999=CARTESIAN_POINT('',(3.62140732971,-22.6596242971,-0.525469586725));
#79000=CARTESIAN_POINT('Ctrl Pts',(3.62140732971,-22.6596242971005,-0.525469586723355));
#79001=CARTESIAN_POINT('Ctrl Pts',(3.62140732971008,-22.6699477832947,-0.528534730954812));
#79002=CARTESIAN_POINT('Ctrl Pts',(3.62141714315506,-22.6806901701076,-0.532327683633485));
#79003=CARTESIAN_POINT('Ctrl Pts',(3.62142184225419,-22.6917209824537,-0.537022534618477));
#79004=CARTESIAN_POINT('Ctrl Pts',(3.62142321631071,-22.6949464857043,-0.538395348935147));
#79005=CARTESIAN_POINT('Ctrl Pts',(3.62142415307669,-22.6981963160703,-0.539845282632328));
#79006=CARTESIAN_POINT('Ctrl Pts',(3.62142427933164,-22.7014663477083,-0.541376650405068));
#79007=CARTESIAN_POINT('Ctrl Pts',(3.62142455834708,-22.7086929104212,-0.544760876146999));
#79008=CARTESIAN_POINT('Ctrl Pts',(3.62142164111691,-22.7160184972014,-0.548542904520612));
#79009=CARTESIAN_POINT('Ctrl Pts',(3.62141741127485,-22.7233891494459,-0.552766423972345));
#79010=CARTESIAN_POINT('Ctrl Pts',(3.62141529635382,-22.7270744755682,-0.554878183698211));
#79011=CARTESIAN_POINT('Ctrl Pts',(3.62141285327981,-22.7307710466164,-0.557100352677717));
#79012=CARTESIAN_POINT('Ctrl Pts',(3.62141087609901,-22.7344708103863,-0.559437806787722));
#79013=CARTESIAN_POINT('Ctrl Pts',(3.62140988750862,-22.7363206922713,-0.560606533842724));
#79014=CARTESIAN_POINT('Ctrl Pts',(3.62140901539152,-22.7381713722864,-0.561804082618375));
#79015=CARTESIAN_POINT('Ctrl Pts',(3.62140838179892,-22.7400217976135,-0.563031035793675));
#79016=CARTESIAN_POINT('Ctrl Pts',(3.62140800542491,-22.7411210086764,-0.563759884715135));
#79017=CARTESIAN_POINT('Ctrl Pts',(3.62140770758826,-22.7426310270696,-0.564776697577344));
#79018=CARTESIAN_POINT('Ctrl Pts',(3.62140752622844,-22.7438174542328,-0.565589707317948));
#79019=CARTESIAN_POINT('Ctrl Pts',(3.62140740228493,-22.7446282730451,-0.566145328103387));
#79020=CARTESIAN_POINT('Ctrl Pts',(3.62140733274219,-22.7452889497865,-0.566604278368968));
#79021=CARTESIAN_POINT('Ctrl Pts',(3.62140732971009,-22.7455712334679,-0.566800677308756));
#79022=CARTESIAN_POINT('Ctrl Pts',(3.62140730352346,-22.7480091664161,-0.568496869748418));
#79023=CARTESIAN_POINT('Ctrl Pts',(3.6214211167595,-22.7511789206969,-0.570750760982344));
#79024=CARTESIAN_POINT('Ctrl Pts',(3.6214374946079,-22.755018246027,-0.57364988953821));
#79025=CARTESIAN_POINT('Ctrl Pts',(3.62145363121916,-22.7588010201036,-0.57650631544711));
#79026=CARTESIAN_POINT('Ctrl Pts',(3.62147225744839,-22.763234296542,-0.579989678194066));
#79027=CARTESIAN_POINT('Ctrl Pts',(3.62148258939903,-22.7682192058606,-0.584215191354991));
#79028=CARTESIAN_POINT('Ctrl Pts',(3.62148569805628,-22.7697190557,-0.585486555552531));
#79029=CARTESIAN_POINT('Ctrl Pts',(3.62148805585235,-22.7712685402352,-0.586825289535902));
#79030=CARTESIAN_POINT('Ctrl Pts',(3.62148936905792,-22.7728641378073,-0.588234963055801));
#79031=CARTESIAN_POINT('Ctrl Pts',(3.62149361630903,-22.7780247186582,-0.592794216779927));
#79032=CARTESIAN_POINT('Ctrl Pts',(3.62148677078224,-22.7836714580148,-0.59809482393021));
#79033=CARTESIAN_POINT('Ctrl Pts',(3.62147178598681,-22.7896502718194,-0.604263107728835));
#79034=CARTESIAN_POINT('Ctrl Pts',(3.621468940372,-22.7907856494244,-0.605434465713029));
#79035=CARTESIAN_POINT('Ctrl Pts',(3.62146580123835,-22.7919328531322,-0.606637136087257));
#79036=CARTESIAN_POINT('Ctrl Pts',(3.62146238881206,-22.7930906114698,-0.607872003981022));
#79037=CARTESIAN_POINT('Ctrl Pts',(3.62145169780773,-22.7967178251754,-0.611740799051204));
#79038=CARTESIAN_POINT('Ctrl Pts',(3.6214387449041,-22.8004490769422,-0.615925609208144));
#79039=CARTESIAN_POINT('Ctrl Pts',(3.62142766212208,-22.8042397922835,-0.620452303848787));
#79040=CARTESIAN_POINT('Ctrl Pts',(3.62142246582197,-22.8060171162892,-0.622574700897024));
#79041=CARTESIAN_POINT('Ctrl Pts',(3.62141766979187,-22.8080079092195,-0.625018234205574));
#79042=CARTESIAN_POINT('Ctrl Pts',(3.62141404227473,-22.8099186181219,-0.627444319071953));
#79043=CARTESIAN_POINT('Ctrl Pts',(3.62141025972111,-22.8119109888293,-0.629974092401307));
#79044=CARTESIAN_POINT('Ctrl Pts',(3.62140774769706,-22.8138161559041,-0.63248461828544));
#79045=CARTESIAN_POINT('Ctrl Pts',(3.62140737721721,-22.815348938655,-0.634554994121101));
#79046=CARTESIAN_POINT('Ctrl Pts',(3.62140734521127,-22.8154813565557,-0.634733854968577));
#79047=CARTESIAN_POINT('Ctrl Pts',(3.62140732918835,-22.8156110208474,-0.63490941283829));
#79048=CARTESIAN_POINT('Ctrl Pts',(3.62140732971007,-22.8157377607153,-0.63508138739397));
#79049=CARTESIAN_POINT('Ctrl Pts',(3.62140736343285,-22.8239299728543,-0.646197479479502));
#79050=CARTESIAN_POINT('Ctrl Pts',(3.62140738564739,-22.8310489680643,-0.657463854897076));
#79051=CARTESIAN_POINT('Ctrl Pts',(3.62140739929918,-22.8372039362312,-0.668673725041791));
#79052=CARTESIAN_POINT('Ctrl Pts',(3.62140741342894,-22.8435743977133,-0.680276067091498));
#79053=CARTESIAN_POINT('Ctrl Pts',(3.62140741838586,-22.8489130072506,-0.691817776465343));
#79054=CARTESIAN_POINT('Ctrl Pts',(3.62140741743574,-22.8533648006108,-0.703120493300786));
#79055=CARTESIAN_POINT('Ctrl Pts',(3.62140741643095,-22.858072765324,-0.71507360696048));
#79056=CARTESIAN_POINT('Ctrl Pts',(3.62140740881975,-22.861789805585,-0.726759362272155));
#79057=CARTESIAN_POINT('Ctrl Pts',(3.62140739846477,-22.8646999547098,-0.738024484180477));
#79058=CARTESIAN_POINT('Ctrl Pts',(3.62140738776206,-22.8677078290071,-0.749667898036567));
#79059=CARTESIAN_POINT('Ctrl Pts',(3.62140737412821,-22.869854607863,-0.760862342676822));
#79060=CARTESIAN_POINT('Ctrl Pts',(3.6214073618282,-22.8713422147409,-0.771495701036556));
#79061=CARTESIAN_POINT('Ctrl Pts',(3.6214073488987,-22.8729059559173,-0.782673264517133));
#79062=CARTESIAN_POINT('Ctrl Pts',(3.62140733744306,-22.8737421881999,-0.793231321316465));
#79063=CARTESIAN_POINT('Ctrl Pts',(3.62140733241521,-22.8740700378175,-0.803095095549144));
#79064=CARTESIAN_POINT('Ctrl Pts',(3.62140733067966,-22.8741832072463,-0.806499942272538));
#79065=CARTESIAN_POINT('Ctrl Pts',(3.62140732971,-22.8742356128,-0.809822492012007));
#79066=CARTESIAN_POINT('Ctrl Pts',(3.62140732971,-22.8742356128,-0.813060915858));
#79067=CARTESIAN_POINT('',(-3.62140732971,-22.6596242971,-0.525469586725));
#79068=CARTESIAN_POINT('',(9.81437153769E-14,-22.6596242971,-0.525469586725));
#79069=CARTESIAN_POINT('Ctrl Pts',(-3.62140732971,-22.8742356128,-0.813060915858));
#79070=CARTESIAN_POINT('Ctrl Pts',(-3.62140732970999,-22.8742356128,-0.803744725297564));
#79071=CARTESIAN_POINT('Ctrl Pts',(-3.62136469902042,-22.873804016399,-0.793745508480425));
#79072=CARTESIAN_POINT('Ctrl Pts',(-3.62131260175645,-22.8727364911915,
-0.783107191556518));
#79073=CARTESIAN_POINT('Ctrl Pts',(-3.62126327948377,-22.8717258283395,
-0.773035530816041));
#79074=CARTESIAN_POINT('Ctrl Pts',(-3.62120547226317,-22.870144557252,-0.762390552719321));
#79075=CARTESIAN_POINT('Ctrl Pts',(-3.62116732196172,-22.8677991370249,
-0.751251068384887));
#79076=CARTESIAN_POINT('Ctrl Pts',(-3.62114578449456,-22.8664750475895,
-0.744962355875019));
#79077=CARTESIAN_POINT('Ctrl Pts',(-3.62113051184974,-22.8649070869389,
-0.738516841232333));
#79078=CARTESIAN_POINT('Ctrl Pts',(-3.62112656743464,-22.8630586371168,
-0.731935946677658));
#79079=CARTESIAN_POINT('Ctrl Pts',(-3.62111996128396,-22.8599628326116,
-0.720914190627644));
#79080=CARTESIAN_POINT('Ctrl Pts',(-3.62114127299378,-22.8560800676364,
-0.709511995309836));
#79081=CARTESIAN_POINT('Ctrl Pts',(-3.62118066024351,-22.8512437853523,
-0.697880742480753));
#79082=CARTESIAN_POINT('Ctrl Pts',(-3.62119586107707,-22.8493773051454,
-0.693391859923282));
#79083=CARTESIAN_POINT('Ctrl Pts',(-3.62121375415682,-22.8473688902165,
-0.688869387884984));
#79084=CARTESIAN_POINT('Ctrl Pts',(-3.62123377372212,-22.8452094665408,
-0.684324089002303));
#79085=CARTESIAN_POINT('Ctrl Pts',(-3.62126972009617,-22.8413320870857,
-0.676162722289865));
#79086=CARTESIAN_POINT('Ctrl Pts',(-3.62131121006315,-22.83696757079,-0.667927477355911));
#79087=CARTESIAN_POINT('Ctrl Pts',(-3.62134559074755,-22.8320694821121,
-0.659693071002674));
#79088=CARTESIAN_POINT('Ctrl Pts',(-3.62136278108975,-22.8296204377731,
-0.655575867826055));
#79089=CARTESIAN_POINT('Ctrl Pts',(-3.62137808417274,-22.8270381252706,
-0.65145909978056));
#79090=CARTESIAN_POINT('Ctrl Pts',(-3.62138921781553,-22.8243176686862,
-0.647353446733183));
#79091=CARTESIAN_POINT('Ctrl Pts',(-3.62139478463693,-22.8229574403939,
-0.645300620209494));
#79092=CARTESIAN_POINT('Ctrl Pts',(-3.62139930863626,-22.821765563472,-0.643549012983476));
#79093=CARTESIAN_POINT('Ctrl Pts',(-3.62140244291738,-22.8204425274908,
-0.641648678376371));
#79094=CARTESIAN_POINT('Ctrl Pts',(-3.62140533511476,-22.8192216793752,
-0.639895120682618));
#79095=CARTESIAN_POINT('Ctrl Pts',(-3.62140704397987,-22.8178893909459,
-0.638014546259289));
#79096=CARTESIAN_POINT('Ctrl Pts',(-3.62140729694812,-22.8161762062179,
-0.635677857882931));
#79097=CARTESIAN_POINT('Ctrl Pts',(-3.62140731812216,-22.816032808617,-0.635482271556591));
#79098=CARTESIAN_POINT('Ctrl Pts',(-3.62140732909606,-22.8158867177009,
-0.635283508571965));
#79099=CARTESIAN_POINT('Ctrl Pts',(-3.62140732970999,-22.8157377607153,
-0.635081387393934));
#79100=CARTESIAN_POINT('Ctrl Pts',(-3.62140735533527,-22.8095203002477,
-0.626644854999134));
#79101=CARTESIAN_POINT('Ctrl Pts',(-3.62142235572899,-22.803325198848,-0.619159888756903));
#79102=CARTESIAN_POINT('Ctrl Pts',(-3.62143959581722,-22.7973595082029,
-0.612522322813618));
#79103=CARTESIAN_POINT('Ctrl Pts',(-3.62145759034423,-22.7911327546029,
-0.605594292164457));
#79104=CARTESIAN_POINT('Ctrl Pts',(-3.62147802487608,-22.7851558742559,
-0.599588282153463));
#79105=CARTESIAN_POINT('Ctrl Pts',(-3.62148641822033,-22.7796081474466,
-0.594378218753685));
#79106=CARTESIAN_POINT('Ctrl Pts',(-3.62148993808707,-22.7772816303239,
-0.592193305522268));
#79107=CARTESIAN_POINT('Ctrl Pts',(-3.62149134031594,-22.7750299356726,
-0.590148386434912));
#79108=CARTESIAN_POINT('Ctrl Pts',(-3.62148955689063,-22.7728636189422,
-0.588234504651515));
#79109=CARTESIAN_POINT('Ctrl Pts',(-3.62148519496225,-22.7675652089869,
-0.58355350387633));
#79110=CARTESIAN_POINT('Ctrl Pts',(-3.62147007641132,-22.7627786705937,
-0.579652790409958));
#79111=CARTESIAN_POINT('Ctrl Pts',(-3.62145348161823,-22.7586166593081,
-0.576410055541454));
#79112=CARTESIAN_POINT('Ctrl Pts',(-3.62145084388833,-22.7579551107418,
-0.575894625270851));
#79113=CARTESIAN_POINT('Ctrl Pts',(-3.62144816886139,-22.7573092469938,
-0.57539587012562));
#79114=CARTESIAN_POINT('Ctrl Pts',(-3.62144549380582,-22.7566794179112,
-0.574913360807467));
#79115=CARTESIAN_POINT('Ctrl Pts',(-3.62143574146768,-22.7543832763796,
-0.573154296776697));
#79116=CARTESIAN_POINT('Ctrl Pts',(-3.62142616868904,-22.7523005262405,
-0.571610833801016));
#79117=CARTESIAN_POINT('Ctrl Pts',(-3.62141906430083,-22.7504451611699,
-0.570264303313079));
#79118=CARTESIAN_POINT('Ctrl Pts',(-3.62141551210673,-22.7495174786345,
-0.56959103806911));
#79119=CARTESIAN_POINT('Ctrl Pts',(-3.62141257701023,-22.7486465927841,
-0.568967075004624));
#79120=CARTESIAN_POINT('Ctrl Pts',(-3.62141053318238,-22.7478338505885,
-0.568390419400569));
#79121=CARTESIAN_POINT('Ctrl Pts',(-3.62140951126845,-22.7474274794907,
-0.568102091598542));
#79122=CARTESIAN_POINT('Ctrl Pts',(-3.62140871536219,-22.7473224594101,
-0.568028214121263));
#79123=CARTESIAN_POINT('Ctrl Pts',(-3.62140817245349,-22.7470892859499,
-0.567863836596028));
#79124=CARTESIAN_POINT('Ctrl Pts',(-3.6214076295448,-22.7468561124896,-0.567699459070793));
#79125=CARTESIAN_POINT('Ctrl Pts',(-3.62140733963366,-22.746495411902,-0.567443674678283));
#79126=CARTESIAN_POINT('Ctrl Pts',(-3.62140732970999,-22.7455712334679,
-0.56680067730871));
#79127=CARTESIAN_POINT('Ctrl Pts',(-3.6214072131747,-22.7347184538603,-0.559249853265867));
#79128=CARTESIAN_POINT('Ctrl Pts',(-3.62140718217023,-22.7238266504752,
-0.552735625785393));
#79129=CARTESIAN_POINT('Ctrl Pts',(-3.62140718961521,-22.713088824196,-0.54712899659101));
#79130=CARTESIAN_POINT('Ctrl Pts',(-3.62140719744237,-22.7017997952552,
-0.541234563435771));
#79131=CARTESIAN_POINT('Ctrl Pts',(-3.62140724776773,-22.6906810403832,
-0.536342399783166));
#79132=CARTESIAN_POINT('Ctrl Pts',(-3.62140728588091,-22.6799007092827,
-0.53228540519991));
#79133=CARTESIAN_POINT('Ctrl Pts',(-3.62140731030249,-22.6729930566932,
-0.529685827424681));
#79134=CARTESIAN_POINT('Ctrl Pts',(-3.62140732971,-22.6662231970864,-0.527428864804953));
#79135=CARTESIAN_POINT('Ctrl Pts',(-3.62140732971,-22.6596242971005,-0.525469586723355));
#79136=CARTESIAN_POINT('Origin',(0.,-21.6200560145,-0.216811574779));
#79137=CARTESIAN_POINT('',(-3.92508992147,-21.7707429986,-0.261552017256));
#79138=CARTESIAN_POINT('',(3.92508992519015,-21.7707429981472,-0.261552017112367));
#79139=CARTESIAN_POINT('',(-0.0354705937405,-21.7707429986,-0.261552017256));
#79140=CARTESIAN_POINT('Origin',(3.03257419176E-14,-21.0305048468,-0.0417680548823));
#79141=CARTESIAN_POINT('Origin',(-8.33777491493E-15,-21.0305048468,-0.0417680548823));
#79142=CARTESIAN_POINT('Origin',(-0.0354705937405,-21.8561316829,0.0260393118769));
#79143=CARTESIAN_POINT('Ctrl Pts',(4.05326999191,-21.5710708896125,-0.0674504957510902));
#79144=CARTESIAN_POINT('Ctrl Pts',(4.04568105172187,-21.5766811085323,-0.0845566755192819));
#79145=CARTESIAN_POINT('Ctrl Pts',(4.03782073411841,-21.5838132252431,-0.101090041800997));
#79146=CARTESIAN_POINT('Ctrl Pts',(4.02981682449863,-21.5923201463575,-0.116801414763259));
#79147=CARTESIAN_POINT('Ctrl Pts',(4.0217466234343,-21.6008975250503,-0.132642915333036));
#79148=CARTESIAN_POINT('Ctrl Pts',(4.01353044193539,-21.6108721210905,-0.147648314175529));
#79149=CARTESIAN_POINT('Ctrl Pts',(4.00529926687375,-21.6220544382609,-0.161598220461817));
#79150=CARTESIAN_POINT('Ctrl Pts',(4.00311074712359,-21.6250276130259,-0.165307246839182));
#79151=CARTESIAN_POINT('Ctrl Pts',(4.00092116743143,-21.6280859765477,-0.168941872280921));
#79152=CARTESIAN_POINT('Ctrl Pts',(3.99873298982911,-21.6312255779638,-0.172498452698097));
#79153=CARTESIAN_POINT('Ctrl Pts',(3.98987872328167,-21.64392969657,-0.18688983984035));
#79154=CARTESIAN_POINT('Ctrl Pts',(3.98105148723871,-21.6579637936179,-0.19999754833016));
#79155=CARTESIAN_POINT('Ctrl Pts',(3.97239798326953,-21.6730612515873,-0.211626876671228));
#79156=CARTESIAN_POINT('Ctrl Pts',(3.96363330690678,-21.688352668044,-0.223405608106326));
#79157=CARTESIAN_POINT('Ctrl Pts',(3.95504685519709,-21.7047345766709,-0.233667645129993));
#79158=CARTESIAN_POINT('Ctrl Pts',(3.94679105672644,-21.7219091373593,-0.242259604014651));
#79159=CARTESIAN_POINT('Ctrl Pts',(3.94578814651856,-21.7239954942746,-0.243303350819001));
#79160=CARTESIAN_POINT('Ctrl Pts',(3.94479011584885,-21.7260935274999,-0.244322511279171));
#79161=CARTESIAN_POINT('Ctrl Pts',(3.94379723797682,-21.7282026864134,-0.245316859709329));
#79162=CARTESIAN_POINT('Ctrl Pts',(3.9373235011442,-21.7419547702585,-0.251800184837398));
#79163=CARTESIAN_POINT('Ctrl Pts',(3.93106588671667,-21.7561829643929,-0.257229000399012));
#79164=CARTESIAN_POINT('Ctrl Pts',(3.92508992725,-21.7707429985995,-0.261552017257738));
#79165=CARTESIAN_POINT('',(-9.7699626167E-15,-21.5710708896,-0.0674504957552));
#79166=CARTESIAN_POINT('Ctrl Pts',(-3.92508992147,-21.7707429985995,-0.261552017257738));
#79167=CARTESIAN_POINT('Ctrl Pts',(-3.93309231670333,-21.7512455755997,
-0.255763041274999));
#79168=CARTESIAN_POINT('Ctrl Pts',(-3.94160650345342,-21.7323352144214,
-0.24798610008293));
#79169=CARTESIAN_POINT('Ctrl Pts',(-3.95046295408005,-21.7143708969331,
-0.238354106274979));
#79170=CARTESIAN_POINT('Ctrl Pts',(-3.95931940470668,-21.6964065794448,
-0.228722112467028));
#79171=CARTESIAN_POINT('Ctrl Pts',(-3.96851811920986,-21.6793884890492,
-0.217234920628154));
#79172=CARTESIAN_POINT('Ctrl Pts',(-3.97788956994937,-21.6636589267433,
-0.204078566910147));
#79173=CARTESIAN_POINT('Ctrl Pts',(-3.98619702881204,-21.6497152273721,
-0.192415925731835));
#79174=CARTESIAN_POINT('Ctrl Pts',(-3.99463812765578,-21.6367863343899,
-0.179442566946254));
#79175=CARTESIAN_POINT('Ctrl Pts',(-4.00307451569265,-21.6251068301091,
-0.165343857166143));
#79176=CARTESIAN_POINT('Ctrl Pts',(-4.01143033516254,-21.6135388665634,
-0.151379791837931));
#79177=CARTESIAN_POINT('Ctrl Pts',(-4.0197815333735,-21.6031970209888,-0.136312056895106));
#79178=CARTESIAN_POINT('Ctrl Pts',(-4.02799368560558,-21.5942795872117,
-0.12036246401268));
#79179=CARTESIAN_POINT('Ctrl Pts',(-4.02999966943303,-21.5921013241408,
-0.11646645423688));
#79180=CARTESIAN_POINT('Ctrl Pts',(-4.03199735667665,-21.590007894118,-0.11251801042259));
#79181=CARTESIAN_POINT('Ctrl Pts',(-4.03398478808377,-21.5880018653709,
-0.108520715440977));
#79182=CARTESIAN_POINT('Ctrl Pts',(-4.04055050501333,-21.5813747099083,
-0.0953151742387814));
#79183=CARTESIAN_POINT('Ctrl Pts',(-4.04700277586667,-21.5757039879415,
-0.0815773264565373));
#79184=CARTESIAN_POINT('Ctrl Pts',(-4.0532699684,-21.5710708896125,-0.0674504957510902));
#79185=CARTESIAN_POINT('Origin',(0.,-19.3367276644,6.74530982971));
#79186=CARTESIAN_POINT('Origin',(3.62140732971,-22.5742356128,-0.813060915858));
#79187=CARTESIAN_POINT('',(3.88319581089567,-22.6692776296171,-0.924567893965636));
#79188=CARTESIAN_POINT('Origin',(3.62140732971,-22.5742356128,-0.813060915858));
#79189=CARTESIAN_POINT('Origin',(3.62140732971,-22.5742356128,-0.813060915858));
#79190=CARTESIAN_POINT('Origin',(-8.43769498715E-15,-20.9451161625,-0.329359384015));
#79191=CARTESIAN_POINT('',(4.20883143442254,-21.7161399162306,-0.641571696058489));
#79192=CARTESIAN_POINT('Origin',(3.92508988180106,-21.6853545076789,-0.549143403786509));
#79193=CARTESIAN_POINT('Origin',(-5.90154768276285E-6,-20.922394848479,
-0.405877494386963));
#79194=CARTESIAN_POINT('Ctrl Pts',(4.05326999191,-21.5710708896,-0.0674504957552));
#79195=CARTESIAN_POINT('Ctrl Pts',(4.14906267383,-21.5773629037,-0.0866355443942));
#79196=CARTESIAN_POINT('Ctrl Pts',(4.24485535575,-21.5457105806,-0.118264986841));
#79197=CARTESIAN_POINT('Ctrl Pts',(4.31892160248,-21.4741377387,-0.1581676115));
#79198=CARTESIAN_POINT('Ctrl Pts',(4.35210058992,-21.3811601618,-0.196020670745));
#79199=CARTESIAN_POINT('Ctrl Pts',(4.34627746121,-21.2879273766,-0.225306031645));
#79200=CARTESIAN_POINT('Ctrl Pts',(4.02839229827,-21.5894620357,-0.123527140032));
#79201=CARTESIAN_POINT('Ctrl Pts',(4.12621567612,-21.6002038923,-0.14353500743));
#79202=CARTESIAN_POINT('Ctrl Pts',(4.22403905397,-21.5735624324,-0.184070478262));
#79203=CARTESIAN_POINT('Ctrl Pts',(4.29855068001,-21.5064409415,-0.240682386349));
#79204=CARTESIAN_POINT('Ctrl Pts',(4.32942721023,-21.4172157026,-0.298161067627));
#79205=CARTESIAN_POINT('Ctrl Pts',(4.31960138008,-21.3273686296,-0.345566786841));
#79206=CARTESIAN_POINT('Ctrl Pts',(4.00108772463,-21.6214549247,-0.174510108847));
#79207=CARTESIAN_POINT('Ctrl Pts',(4.10130096444,-21.6370719606,-0.193345500879));
#79208=CARTESIAN_POINT('Ctrl Pts',(4.20151420426,-21.6177474532,-0.241118366914));
#79209=CARTESIAN_POINT('Ctrl Pts',(4.27654207061,-21.5590494503,-0.313527678841));
#79210=CARTESIAN_POINT('Ctrl Pts',(4.30472756187,-21.4781622142,-0.390048280054));
#79211=CARTESIAN_POINT('Ctrl Pts',(4.29032296542,-21.3959792109,-0.454901796918));
#79212=CARTESIAN_POINT('Ctrl Pts',(3.97344013776,-21.6649708651,-0.215919998082));
#79213=CARTESIAN_POINT('Ctrl Pts',(4.07632718344,-21.6845855954,-0.231221519449));
#79214=CARTESIAN_POINT('Ctrl Pts',(4.17921422913,-21.6739877397,-0.283641075841));
#79215=CARTESIAN_POINT('Ctrl Pts',(4.2548069522,-21.6274322849,-0.369678608099));
#79216=CARTESIAN_POINT('Ctrl Pts',(4.28000984415,-21.5595261872,-0.463318063595));
#79217=CARTESIAN_POINT('Ctrl Pts',(4.26067677377,-21.4893040651,-0.543710875712));
#79218=CARTESIAN_POINT('Ctrl Pts',(3.94760066504,-21.7158967526,-0.245267576656));
#79219=CARTESIAN_POINT('Ctrl Pts',(4.05328834439,-21.7371001908,-0.255802966429));
#79220=CARTESIAN_POINT('Ctrl Pts',(4.15897602375,-21.7351383126,-0.310326311117));
#79221=CARTESIAN_POINT('Ctrl Pts',(4.23514222118,-21.7035971961,-0.40670982973));
#79222=CARTESIAN_POINT('Ctrl Pts',(4.25725324903,-21.6528882528,-0.513991630809));
#79223=CARTESIAN_POINT('Ctrl Pts',(4.2329693852,-21.5985179932,-0.606648702621));
#79224=CARTESIAN_POINT('Ctrl Pts',(3.92508992725,-21.7707430499,-0.261552067196));
#79225=CARTESIAN_POINT('Ctrl Pts',(4.03342463854,-21.7911739994,-0.267618198038));
#79226=CARTESIAN_POINT('Ctrl Pts',(4.14175934982,-21.7971474076,-0.32237766681));
#79227=CARTESIAN_POINT('Ctrl Pts',(4.21845509047,-21.7823880347,-0.42509762008));
#79228=CARTESIAN_POINT('Ctrl Pts',(4.23766397715,-21.7518700624,-0.541159533462));
#79229=CARTESIAN_POINT('Ctrl Pts',(4.20883136913,-21.7161396821,-0.641571966647));
#79230=CARTESIAN_POINT('Ctrl Pts',(4.34627740764205,-21.2879283386,-0.225306246837449));
#79231=CARTESIAN_POINT('Ctrl Pts',(4.33972068909289,-21.2976225055542,-0.254865144793904));
#79232=CARTESIAN_POINT('Ctrl Pts',(4.33297529253917,-21.3094345052532,-0.283628668746071));
#79233=CARTESIAN_POINT('Ctrl Pts',(4.3261130717861,-21.3232019719801,-0.311308815013811));
#79234=CARTESIAN_POINT('Ctrl Pts',(4.31906170088675,-21.3373489249461,-0.339751936403424));
#79235=CARTESIAN_POINT('Ctrl Pts',(4.31188705509232,-21.3535602107086,-0.36705104974735));
#79236=CARTESIAN_POINT('Ctrl Pts',(4.30466668690189,-21.3716230344419,-0.392936317507967));
#79237=CARTESIAN_POINT('Ctrl Pts',(4.29724098019976,-21.3901995429687,-0.419557730880084));
#79238=CARTESIAN_POINT('Ctrl Pts',(4.28976700965491,-21.4107338684777,-0.44468365175604));
#79239=CARTESIAN_POINT('Ctrl Pts',(4.28232735834422,-21.4329636594452,-0.468066387452847));
#79240=CARTESIAN_POINT('Ctrl Pts',(4.27459360193598,-21.4560722409054,-0.492373491977681));
#79241=CARTESIAN_POINT('Ctrl Pts',(4.26689705997568,-21.4810123362882,-0.514796688212307));
#79242=CARTESIAN_POINT('Ctrl Pts',(4.25932685806936,-21.5074654407041,-0.535108738097012));
#79243=CARTESIAN_POINT('Ctrl Pts',(4.2516335219164,-21.5343488220299,-0.555751176654447));
#79244=CARTESIAN_POINT('Ctrl Pts',(4.24407080218707,-21.5627939658263,-0.574213257646628));
#79245=CARTESIAN_POINT('Ctrl Pts',(4.23672655941918,-21.592454313204,-0.590309019639578));
#79246=CARTESIAN_POINT('Ctrl Pts',(4.22932882511418,-21.6223306906916,-0.60652201455594));
#79247=CARTESIAN_POINT('Ctrl Pts',(4.22215289497375,-21.6534390908336,-0.620334206824725));
#79248=CARTESIAN_POINT('Ctrl Pts',(4.21528083331161,-21.6854267960447,-0.631607268719839));
#79249=CARTESIAN_POINT('Ctrl Pts',(4.21309968663009,-21.6955794810031,-0.635185263614525));
#79250=CARTESIAN_POINT('Ctrl Pts',(4.21094908501466,-21.7058208153124,-0.638507851389803));
#79251=CARTESIAN_POINT('Ctrl Pts',(4.20883145763016,-21.7161397917727,-0.641571658435669));
#79252=CARTESIAN_POINT('Origin',(0.,-21.2594877202,0.729452270839));
#79253=CARTESIAN_POINT('',(-0.770172012660285,-22.6692778677973,-3.42046662122282));
#79254=CARTESIAN_POINT('',(-3.88319582787855,-22.6692776500678,-0.924567836647076));
#79255=CARTESIAN_POINT('Ctrl Pts',(-0.770171998117105,-22.6692781063945,
-3.42046654285371));
#79256=CARTESIAN_POINT('Ctrl Pts',(-0.827421116550194,-22.6692778637131,
-3.40984191914858));
#79257=CARTESIAN_POINT('Ctrl Pts',(-0.885473202714977,-22.6693131840285,
-3.39783479732127));
#79258=CARTESIAN_POINT('Ctrl Pts',(-0.944508027397569,-22.6693497782976,
-3.38426788045991));
#79259=CARTESIAN_POINT('Ctrl Pts',(-1.00214482600105,-22.669385505964,-3.37102224690357));
#79260=CARTESIAN_POINT('Ctrl Pts',(-1.06071870631787,-22.6694224477752,
-3.35628980600909));
#79261=CARTESIAN_POINT('Ctrl Pts',(-1.12037526257652,-22.6694287047423,
-3.33986282387073));
#79262=CARTESIAN_POINT('Ctrl Pts',(-1.1807553272836,-22.6694350375933,-3.32323661701836));
#79263=CARTESIAN_POINT('Ctrl Pts',(-1.24222354321397,-22.66941191933,-3.30487819993372));
#79264=CARTESIAN_POINT('Ctrl Pts',(-1.30479393660715,-22.6693729785012,
-3.28455273682354));
#79265=CARTESIAN_POINT('Ctrl Pts',(-1.33607913330373,-22.6693535080868,
-3.27439000526844));
#79266=CARTESIAN_POINT('Ctrl Pts',(-1.36763842454216,-22.66933084145,-3.2637351011711));
#79267=CARTESIAN_POINT('Ctrl Pts',(-1.39946526850315,-22.6693119348859,
-3.2525563464012));
#79268=CARTESIAN_POINT('Ctrl Pts',(-1.4167002163369,-22.6693016965587,-3.2465028006729));
#79269=CARTESIAN_POINT('Ctrl Pts',(-1.43345280452839,-22.6692925607939,
-3.24049710780066));
#79270=CARTESIAN_POINT('Ctrl Pts',(-1.45063396294028,-22.6692862684275,
-3.23421133216339));
#79271=CARTESIAN_POINT('Ctrl Pts',(-1.46518031847964,-22.669280941022,-3.22888950664568));
#79272=CARTESIAN_POINT('Ctrl Pts',(-1.48003370917092,-22.6692776518028,
-3.22336628878764));
#79273=CARTESIAN_POINT('Ctrl Pts',(-1.49573670679619,-22.669277457247,-3.21741542407968));
#79274=CARTESIAN_POINT('Ctrl Pts',(-1.55860736494078,-22.6692766782972,
-3.19358973234571));
#79275=CARTESIAN_POINT('Ctrl Pts',(-1.62324025161164,-22.6693594306987,
-3.16735192589975));
#79276=CARTESIAN_POINT('Ctrl Pts',(-1.68950078842028,-22.6694495359061,
-3.1383758418892));
#79277=CARTESIAN_POINT('Ctrl Pts',(-1.75397033305575,-22.6695372056108,
-3.11018296825049));
#79278=CARTESIAN_POINT('Ctrl Pts',(-1.8199809895668,-22.6696318336522,-3.07939755499398));
#79279=CARTESIAN_POINT('Ctrl Pts',(-1.88736401840794,-22.6696633157624,
-3.04569799944922));
#79280=CARTESIAN_POINT('Ctrl Pts',(-1.90163924554861,-22.6696699853094,
-3.03855868235092));
#79281=CARTESIAN_POINT('Ctrl Pts',(-1.91597589413568,-22.6696738209404,
-3.03128850615114));
#79282=CARTESIAN_POINT('Ctrl Pts',(-1.93037207366804,-22.6696741560997,
-3.02388430536752));
#79283=CARTESIAN_POINT('Ctrl Pts',(-1.99655808933587,-22.6696756969843,
-2.98984370814027));
#79284=CARTESIAN_POINT('Ctrl Pts',(-2.0639921443857,-22.6696207195799,-2.9529710534281));
#79285=CARTESIAN_POINT('Ctrl Pts',(-2.13240457787468,-22.6695411390171,
-2.91295064540045));
#79286=CARTESIAN_POINT('Ctrl Pts',(-2.14264786298145,-22.6695292235457,
-2.90695845321243));
#79287=CARTESIAN_POINT('Ctrl Pts',(-2.15291298661854,-22.6695167564933,
-2.90089569368716));
#79288=CARTESIAN_POINT('Ctrl Pts',(-2.16319894137902,-22.6695038449986,
-2.89476131015632));
#79289=CARTESIAN_POINT('Ctrl Pts',(-2.20269062567246,-22.66945427287,-2.87120908351563));
#79290=CARTESIAN_POINT('Ctrl Pts',(-2.24248921550098,-22.6693997396279,
-2.84660073830231));
#79291=CARTESIAN_POINT('Ctrl Pts',(-2.28253057469024,-22.6693557511123,
-2.82087535025402));
#79292=CARTESIAN_POINT('Ctrl Pts',(-2.30255125428487,-22.6693337568545,
-2.80801265622987));
#79293=CARTESIAN_POINT('Ctrl Pts',(-2.32263260683188,-22.6693143869059,
-2.79487067172989));
#79294=CARTESIAN_POINT('Ctrl Pts',(-2.34276574314777,-22.6693002735175,
-2.78144180749629));
#79295=CARTESIAN_POINT('Ctrl Pts',(-2.35283231130571,-22.6692932168234,
-2.77472737537949));
#79296=CARTESIAN_POINT('Ctrl Pts',(-2.36291182443243,-22.6692874736491,
-2.76794122175153));
#79297=CARTESIAN_POINT('Ctrl Pts',(-2.37300314129246,-22.6692833898957,
-2.76108239602025));
#79298=CARTESIAN_POINT('Ctrl Pts',(-2.38038679038729,-22.669280401881,-2.75606390704554));
#79299=CARTESIAN_POINT('Ctrl Pts',(-2.38857249092499,-22.6692782681744,
-2.75045999729516));
#79300=CARTESIAN_POINT('Ctrl Pts',(-2.39581236961099,-22.6692772028579,
-2.7454688367743));
#79301=CARTESIAN_POINT('Ctrl Pts',(-2.39846731513863,-22.6692768121942,
-2.74363852167134));
#79302=CARTESIAN_POINT('Ctrl Pts',(-2.40099538064462,-22.6692765652046,
-2.7418910615617));
#79303=CARTESIAN_POINT('Ctrl Pts',(-2.40331134426068,-22.6692764724457,
-2.74028694940537));
#79304=CARTESIAN_POINT('Ctrl Pts',(-2.46397465313337,-22.6692740427598,
-2.69826955736538));
#79305=CARTESIAN_POINT('Ctrl Pts',(-2.52566450010339,-22.6693011190506,
-2.65317766664651));
#79306=CARTESIAN_POINT('Ctrl Pts',(-2.58806079523629,-22.6693303276831,
-2.60473205212716));
#79307=CARTESIAN_POINT('Ctrl Pts',(-2.64885457236354,-22.6693587861532,
-2.55753066163419));
#79308=CARTESIAN_POINT('Ctrl Pts',(-2.71031901472123,-22.6693892685942,
-2.50714516049489));
#79309=CARTESIAN_POINT('Ctrl Pts',(-2.77210904370985,-22.6693964638087,
-2.45332459335306));
#79310=CARTESIAN_POINT('Ctrl Pts',(-2.79127659167261,-22.669398695797,-2.43662920869376));
#79311=CARTESIAN_POINT('Ctrl Pts',(-2.81047510471493,-22.6693986869654,
-2.41960335863671));
#79312=CARTESIAN_POINT('Ctrl Pts',(-2.82969328071026,-22.6693956817224,
-2.40223980577816));
#79313=CARTESIAN_POINT('Ctrl Pts',(-2.88915359094509,-22.6693863836141,
-2.34851762943846));
#79314=CARTESIAN_POINT('Ctrl Pts',(-2.94880203112499,-22.6693568467461,
-2.2915606455428));
#79315=CARTESIAN_POINT('Ctrl Pts',(-3.00826142484105,-22.6693210102179,
-2.23116139277267));
#79316=CARTESIAN_POINT('Ctrl Pts',(-3.02117978164482,-22.6693132242478,
-2.21803883888839));
#79317=CARTESIAN_POINT('Ctrl Pts',(-3.03408903777896,-22.6693051409203,
-2.20475387938249));
#79318=CARTESIAN_POINT('Ctrl Pts',(-3.04698502834267,-22.6692969032137,
-2.19130453156101));
#79319=CARTESIAN_POINT('Ctrl Pts',(-3.08311124787292,-22.6692738264912,
-2.15362816311631));
#79320=CARTESIAN_POINT('Ctrl Pts',(-3.11913371676518,-22.6692501395918,
-2.11466130127486));
#79321=CARTESIAN_POINT('Ctrl Pts',(-3.15495571344203,-22.6692321258323,
-2.07436211765109));
#79322=CARTESIAN_POINT('Ctrl Pts',(-3.17286671178045,-22.6692231189525,
-2.05421252583921));
#79323=CARTESIAN_POINT('Ctrl Pts',(-3.19072756673692,-22.669215519106,-2.03372983133757));
#79324=CARTESIAN_POINT('Ctrl Pts',(-3.20852543408119,-22.6692103105793,
-2.01290924567968));
#79325=CARTESIAN_POINT('Ctrl Pts',(-3.21742436775332,-22.669207706316,-2.00249895285073));
#79326=CARTESIAN_POINT('Ctrl Pts',(-3.22630755326258,-22.6692056993086,
-1.99200418606258));
#79327=CARTESIAN_POINT('Ctrl Pts',(-3.23517335911292,-22.6692044130975,
-1.98142435854934));
#79328=CARTESIAN_POINT('Ctrl Pts',(-3.23960626203808,-22.6692037699919,
-1.97613444479272));
#79329=CARTESIAN_POINT('Ctrl Pts',(-3.24403481995821,-22.6692033070462,
-1.97082326577994));
#79330=CARTESIAN_POINT('Ctrl Pts',(-3.2484588262394,-22.6692030402757,-1.9654907498876));
#79331=CARTESIAN_POINT('Ctrl Pts',(-3.25249029555434,-22.6692027971755,
-1.9606313819697));
#79332=CARTESIAN_POINT('Ctrl Pts',(-3.25722491356279,-22.6692027395928,
-1.95489491403983));
#79333=CARTESIAN_POINT('Ctrl Pts',(-3.26072982709033,-22.6692028178804,
-1.95063061071083));
#79334=CARTESIAN_POINT('Ctrl Pts',(-3.26107109426008,-22.6692028255031,
-1.95021540311252));
#79335=CARTESIAN_POINT('Ctrl Pts',(-3.26140073474145,-22.669202834414,-1.94981417846874));
#79336=CARTESIAN_POINT('Ctrl Pts',(-3.2617169825235,-22.6692028445671,-1.94942912033732));
#79337=CARTESIAN_POINT('Ctrl Pts',(-3.31475501068454,-22.6692045473556,
-1.88485088397679));
#79338=CARTESIAN_POINT('Ctrl Pts',(-3.36728482418238,-22.6692094999319,
-1.8169814029747));
#79339=CARTESIAN_POINT('Ctrl Pts',(-3.41889782933495,-22.6692160992244,
-1.74568479034844));
#79340=CARTESIAN_POINT('Ctrl Pts',(-3.46899241050097,-22.6692225043696,
-1.67648568176115));
#79341=CARTESIAN_POINT('Ctrl Pts',(-3.51822313576445,-22.6692304607544,
-1.60405778105421));
#79342=CARTESIAN_POINT('Ctrl Pts',(-3.56617794568295,-22.6692385027401,
-1.52830714221755));
#79343=CARTESIAN_POINT('Ctrl Pts',(-3.61332783129169,-22.6692464097407,
-1.45382798231662));
#79344=CARTESIAN_POINT('Ctrl Pts',(-3.65924411183341,-22.6692543994925,
-1.37613630659395));
#79345=CARTESIAN_POINT('Ctrl Pts',(-3.70349988977995,-22.6692610790745,
-1.29517797657114));
#79346=CARTESIAN_POINT('Ctrl Pts',(-3.74668697832313,-22.6692675973577,
-1.21617462990695));
#79347=CARTESIAN_POINT('Ctrl Pts',(-3.78829254637394,-22.6692728679912,
-1.13406018429735));
#79348=CARTESIAN_POINT('Ctrl Pts',(-3.82788909455231,-22.6692755966254,
-1.04882307993202));
#79349=CARTESIAN_POINT('Ctrl Pts',(-3.84679962356306,-22.6692768997671,
-1.00811552311086));
#79350=CARTESIAN_POINT('Ctrl Pts',(-3.86525149387254,-22.6692776231228,
-0.966696345601946));
#79351=CARTESIAN_POINT('Ctrl Pts',(-3.88319583536254,-22.669277625697,-0.924567839834829));
#79352=CARTESIAN_POINT('',(-4.20883136514917,-21.7161398144877,-0.641571946513287));
#79353=CARTESIAN_POINT('Origin',(3.73454221824776E-6,-20.9223934778998,
-0.405886279792362));
#79354=CARTESIAN_POINT('Ctrl Pts',(-4.20883136830913,-21.7161398184096,
-0.64157193548822));
#79355=CARTESIAN_POINT('Ctrl Pts',(-4.21550983438282,-21.6835963441684,
-0.63190945713986));
#79356=CARTESIAN_POINT('Ctrl Pts',(-4.22251793270132,-21.6518194483258,
-0.619667932074284));
#79357=CARTESIAN_POINT('Ctrl Pts',(-4.22977564768318,-21.6211630765059,
-0.604970177269395));
#79358=CARTESIAN_POINT('Ctrl Pts',(-4.23697770143729,-21.5907418160534,
-0.59038514321472));
#79359=CARTESIAN_POINT('Ctrl Pts',(-4.24442542990854,-21.5614248621562,
-0.573381306580857));
#79360=CARTESIAN_POINT('Ctrl Pts',(-4.25203271689245,-21.5335621959175,
-0.554128793480935));
#79361=CARTESIAN_POINT('Ctrl Pts',(-4.2597570299117,-21.5052709067846,-0.534580111026121));
#79362=CARTESIAN_POINT('Ctrl Pts',(-4.26764574195468,-21.4784799550627,
-0.512712720685886));
#79363=CARTESIAN_POINT('Ctrl Pts',(-4.27560222375549,-21.4535458981271,
-0.488760025977522));
#79364=CARTESIAN_POINT('Ctrl Pts',(-4.28299622290362,-21.4303745517511,
-0.466500664528232));
#79365=CARTESIAN_POINT('Ctrl Pts',(-4.29044860517308,-21.4088073429688,
-0.442440851489234));
#79366=CARTESIAN_POINT('Ctrl Pts',(-4.2978781876711,-21.3891119189423,-0.416813074488966));
#79367=CARTESIAN_POINT('Ctrl Pts',(-4.30513300329695,-21.3698797925041,
-0.391788142457173));
#79368=CARTESIAN_POINT('Ctrl Pts',(-4.31236599107304,-21.3524329342998,
-0.365268199171376));
#79369=CARTESIAN_POINT('Ctrl Pts',(-4.31949956336828,-21.3369948228324,
-0.337511485985271));
#79370=CARTESIAN_POINT('Ctrl Pts',(-4.32640210728653,-21.3220566911352,
-0.310653703675961));
#79371=CARTESIAN_POINT('Ctrl Pts',(-4.33321149785558,-21.3089996578518,
-0.282638077731985));
#79372=CARTESIAN_POINT('Ctrl Pts',(-4.33985671302662,-21.2979956656104,
-0.253736824411127));
#79373=CARTESIAN_POINT('Ctrl Pts',(-4.34201508527133,-21.2944215584035,
-0.244349669684097));
#79374=CARTESIAN_POINT('Ctrl Pts',(-4.34415613630056,-21.2910637697605,
-0.23486938707577));
#79375=CARTESIAN_POINT('Ctrl Pts',(-4.34627743422821,-21.2879273724791,
-0.225306183921295));
#79376=CARTESIAN_POINT('',(-3.90524240041216,-19.1260440734113,0.729452270839));
#79377=CARTESIAN_POINT('Origin',(0.,-21.2594877202,0.729452270839));
#79378=CARTESIAN_POINT('Origin',(4.36980373112E-13,-22.6692776292,0.729452270839));
#79379=CARTESIAN_POINT('',(3.02151310590175,-19.2807402146197,-1.87007015835883));
#79380=CARTESIAN_POINT('',(-3.0215131091296,-19.2807402513822,-1.87007018262017));
#79381=CARTESIAN_POINT('Origin',(-7.89278894574E-12,-21.9012363954,-0.65794048406));
#79382=CARTESIAN_POINT('',(3.69310715296,-19.4536303653,-0.974172913954));
#79383=CARTESIAN_POINT('Ctrl Pts',(3.69310715296,-19.4536303653,-0.974172913954));
#79384=CARTESIAN_POINT('Ctrl Pts',(3.69310715296,-19.5414102009,-1.06722029503));
#79385=CARTESIAN_POINT('Ctrl Pts',(3.66216118733,-19.6043893474,-1.18881869517));
#79386=CARTESIAN_POINT('Ctrl Pts',(3.60362130644,-19.6185190275,-1.30670041311));
#79387=CARTESIAN_POINT('Ctrl Pts',(3.4596034448,-19.6046311185,-1.53737756014));
#79388=CARTESIAN_POINT('Ctrl Pts',(3.29105041121,-19.5054576982,-1.70454430458));
#79389=CARTESIAN_POINT('Ctrl Pts',(3.20000833496,-19.4397458552,-1.77583596615));
#79390=CARTESIAN_POINT('Ctrl Pts',(3.10925931489,-19.3640825186,-1.83151964554));
#79391=CARTESIAN_POINT('Ctrl Pts',(3.02151310998,-19.2807402046,-1.87007014598));
#79392=CARTESIAN_POINT('',(3.69310716477216,-19.422499072587,-0.940557363267574));
#79393=CARTESIAN_POINT('Origin',(3.69310715296,-21.2594877202,0.729452270839));
#79394=CARTESIAN_POINT('Ctrl Pts',(3.64161488688817,-19.230640786913,-0.827763557767012));
#79395=CARTESIAN_POINT('Ctrl Pts',(3.65108695555808,-19.2513668038831,-0.832615986554939));
#79396=CARTESIAN_POINT('Ctrl Pts',(3.65983669873976,-19.2723722033248,-0.839085878865248));
#79397=CARTESIAN_POINT('Ctrl Pts',(3.66773155157564,-19.2935662778242,-0.847342030102235));
#79398=CARTESIAN_POINT('Ctrl Pts',(3.67975962178233,-19.3308348577536,-0.865342889941905));
#79399=CARTESIAN_POINT('Ctrl Pts',(3.68778346002,-19.3668639601,-0.889584895726));
#79400=CARTESIAN_POINT('Ctrl Pts',(3.69041389404,-19.382098195,-0.901291061203));
#79401=CARTESIAN_POINT('Ctrl Pts',(3.6923955115,-19.3993093787,-0.916416350024));
#79402=CARTESIAN_POINT('Ctrl Pts',(3.69301434458,-19.4154261934,-0.932955637331));
#79403=CARTESIAN_POINT('Ctrl Pts',(3.6930761889,-19.4178108664,-0.935459919036));
#79404=CARTESIAN_POINT('Ctrl Pts',(3.69310716781,-19.4201688307,-0.937994127672));
#79405=CARTESIAN_POINT('Ctrl Pts',(3.6931071763,-19.4224990853,-0.940557351746));
#79406=CARTESIAN_POINT('',(2.15473693583979,-17.5697153947013,-0.513604012327406));
#79407=CARTESIAN_POINT('Ctrl Pts',(2.15473698243741,-17.5697154200519,-0.5136040068197));
#79408=CARTESIAN_POINT('Ctrl Pts',(2.19493586295698,-17.591587578194,-0.508845790077125));
#79409=CARTESIAN_POINT('Ctrl Pts',(2.2348493286428,-17.6144272106717,-0.504900376847478));
#79410=CARTESIAN_POINT('Ctrl Pts',(2.2743994614938,-17.6382785139004,-0.501993185534341));
#79411=CARTESIAN_POINT('Ctrl Pts',(2.30940842753783,-17.6593911980977,-0.499419799438559));
#79412=CARTESIAN_POINT('Ctrl Pts',(2.34413402145529,-17.6812972807239,-0.497659044491585));
#79413=CARTESIAN_POINT('Ctrl Pts',(2.37850602772258,-17.7040298852337,-0.496901452718552));
#79414=CARTESIAN_POINT('Ctrl Pts',(2.38296457167826,-17.7069786312465,-0.496803182160986));
#79415=CARTESIAN_POINT('Ctrl Pts',(2.38741712730049,-17.7099412802568,-0.496721852194651));
#79416=CARTESIAN_POINT('Ctrl Pts',(2.391863502787,-17.7129178995795,-0.496657937294923));
#79417=CARTESIAN_POINT('Ctrl Pts',(2.42231996126403,-17.7333069294936,-0.496220137676885));
#79418=CARTESIAN_POINT('Ctrl Pts',(2.45248265130698,-17.7543477183242,-0.496596256764844));
#79419=CARTESIAN_POINT('Ctrl Pts',(2.48227924085577,-17.7760614635646,-0.49795944147974));
#79420=CARTESIAN_POINT('Ctrl Pts',(2.50998408353963,-17.7962508847392,-0.499226929425411));
#79421=CARTESIAN_POINT('Ctrl Pts',(2.53737267544625,-17.8170222467782,-0.501347616208947));
#79422=CARTESIAN_POINT('Ctrl Pts',(2.56435886864359,-17.8383863148398,-0.504496619865039));
#79423=CARTESIAN_POINT('Ctrl Pts',(2.57208046746885,-17.8444992467988,-0.50539764887472));
#79424=CARTESIAN_POINT('Ctrl Pts',(2.57976892295044,-17.8506606552126,-0.506383113442942));
#79425=CARTESIAN_POINT('Ctrl Pts',(2.58742171090786,-17.8568706632281,-0.507457736027369));
#79426=CARTESIAN_POINT('Ctrl Pts',(2.60478336360009,-17.8709591239276,-0.509895700360085));
#79427=CARTESIAN_POINT('Ctrl Pts',(2.62196092287367,-17.8852970680121,-0.51279187018127));
#79428=CARTESIAN_POINT('Ctrl Pts',(2.63891856064913,-17.8998831585272,-0.516206737313588));
#79429=CARTESIAN_POINT('',(2.1547368415,-17.3799083486,1.05880473119));
#79430=CARTESIAN_POINT('Origin',(2.15473684211,-21.2594877202,0.729452270839));
#79431=CARTESIAN_POINT('',(2.19100518433701,-17.3987921046005,1.04094167631916));
#79432=CARTESIAN_POINT('Origin',(3.61628644811E-15,-19.5917976147,-1.03352917222));
#79433=CARTESIAN_POINT('Ctrl Pts',(3.3084919335,-18.2908119326,0.937647357484));
#79434=CARTESIAN_POINT('Ctrl Pts',(3.28842087131374,-18.267491590574,0.92407553187254));
#79435=CARTESIAN_POINT('Ctrl Pts',(3.26766831975679,-18.2440984957641,0.912142274172242));
#79436=CARTESIAN_POINT('Ctrl Pts',(3.24638447088638,-18.2207666805675,0.901668540341281));
#79437=CARTESIAN_POINT('Ctrl Pts',(3.22582983381185,-18.1982342431039,0.891553649983741));
#79438=CARTESIAN_POINT('Ctrl Pts',(3.20477919355986,-18.1757584417377,0.882800213314553));
#79439=CARTESIAN_POINT('Ctrl Pts',(3.18333873530386,-18.1534303030335,0.875266901786711));
#79440=CARTESIAN_POINT('Ctrl Pts',(3.15921334934978,-18.1283060749298,0.86679021505029));
#79441=CARTESIAN_POINT('Ctrl Pts',(3.13459444825019,-18.1033687343773,0.859858392732952));
#79442=CARTESIAN_POINT('Ctrl Pts',(3.10959055101215,-18.078705314789,0.8542965648595));
#79443=CARTESIAN_POINT('Ctrl Pts',(3.08938102407995,-18.0587709806464,0.849801189233425));
#79444=CARTESIAN_POINT('Ctrl Pts',(3.06891911829239,-18.0390147346841,0.846201455913727));
#79445=CARTESIAN_POINT('Ctrl Pts',(3.04824722283645,-18.0194683464823,0.843418598582527));
#79446=CARTESIAN_POINT('Ctrl Pts',(3.01899893748294,-17.9918125206788,0.839481184836674));
#79447=CARTESIAN_POINT('Ctrl Pts',(2.9893358395126,-17.9645820394152,0.837178062763207));
#79448=CARTESIAN_POINT('Ctrl Pts',(2.95935194210494,-17.9378418981739,0.836320919939276));
#79449=CARTESIAN_POINT('Ctrl Pts',(2.94584902770437,-17.9257997732517,0.835934915210697));
#79450=CARTESIAN_POINT('Ctrl Pts',(2.93228061517327,-17.9138566853508,0.835842668757733));
#79451=CARTESIAN_POINT('Ctrl Pts',(2.91865355127057,-17.9020170167149,0.836029309984174));
#79452=CARTESIAN_POINT('Ctrl Pts',(2.88360609593356,-17.871566564535,0.836509332687114));
#79453=CARTESIAN_POINT('Ctrl Pts',(2.84817892182265,-17.841806783168,0.838830763975885));
#79454=CARTESIAN_POINT('Ctrl Pts',(2.81246376430789,-17.8127931084377,0.842778052462115));
#79455=CARTESIAN_POINT('Ctrl Pts',(2.80346044077422,-17.8054791409607,0.843773112201319));
#79456=CARTESIAN_POINT('Ctrl Pts',(2.79443876466176,-17.7982125836861,0.844871750865417));
#79457=CARTESIAN_POINT('Ctrl Pts',(2.78540017354257,-17.7909943955887,0.846071009554622));
#79458=CARTESIAN_POINT('Ctrl Pts',(2.74590734069087,-17.75945555372,0.851310999098805));
#79459=CARTESIAN_POINT('Ctrl Pts',(2.70609545059395,-17.7288430232367,0.858467094085384));
#79460=CARTESIAN_POINT('Ctrl Pts',(2.66605514085442,-17.699203858655,0.867328013205092));
#79461=CARTESIAN_POINT('Ctrl Pts',(2.62526986382453,-17.6690132445897,0.876353793559632));
#79462=CARTESIAN_POINT('Ctrl Pts',(2.58424717397413,-17.6398322788716,0.887148373721119));
#79463=CARTESIAN_POINT('Ctrl Pts',(2.54306973129522,-17.6117030744451,0.899540127854758));
#79464=CARTESIAN_POINT('Ctrl Pts',(2.53280236413254,-17.6046892131887,0.902629943083738));
#79465=CARTESIAN_POINT('Ctrl Pts',(2.52252533030265,-17.5977407178926,0.905819307788507));
#79466=CARTESIAN_POINT('Ctrl Pts',(2.51223983513437,-17.590858201157,0.909106054093216));
#79467=CARTESIAN_POINT('Ctrl Pts',(2.47043606656942,-17.5628853002849,0.922464514683179));
#79468=CARTESIAN_POINT('Ctrl Pts',(2.42849188551327,-17.5360017282731,0.937427721947892));
#79469=CARTESIAN_POINT('Ctrl Pts',(2.38648356239168,-17.5102466215557,0.953884379719845));
#79470=CARTESIAN_POINT('Ctrl Pts',(2.36426604216151,-17.4966251636635,0.96258803889498));
#79471=CARTESIAN_POINT('Ctrl Pts',(2.34203054572053,-17.4833193629859,0.971710330389014));
#79472=CARTESIAN_POINT('Ctrl Pts',(2.31978854938119,-17.4703353212206,0.981240656882616));
#79473=CARTESIAN_POINT('Ctrl Pts',(2.27685569545361,-17.4452727342119,0.999636672644391));
#79474=CARTESIAN_POINT('Ctrl Pts',(2.23389755795098,-17.4214081160994,1.01954811987916));
#79475=CARTESIAN_POINT('Ctrl Pts',(2.19100518797971,-17.3987921063194,1.04094168467634));
#79476=CARTESIAN_POINT('',(3.69310715317639,-18.8681377509785,1.396464174652));
#79477=CARTESIAN_POINT('Ctrl Pts',(3.69310715296,-18.8681377502,1.39646417295));
#79478=CARTESIAN_POINT('Ctrl Pts',(3.69310715214544,-18.8646906714413,1.38410581980008));
#79479=CARTESIAN_POINT('Ctrl Pts',(3.69259177657766,-18.8606009274501,1.37192583995273));
#79480=CARTESIAN_POINT('Ctrl Pts',(3.69158230972186,-18.8559385497586,1.36006768999457));
#79481=CARTESIAN_POINT('Ctrl Pts',(3.69051045782158,-18.8509880371591,1.34747670645363));
#79482=CARTESIAN_POINT('Ctrl Pts',(3.68888179706811,-18.8453922761963,1.33524861672336));
#79483=CARTESIAN_POINT('Ctrl Pts',(3.68674368558374,-18.8392502571381,1.3234995562242));
#79484=CARTESIAN_POINT('Ctrl Pts',(3.68471107890988,-18.8334113151466,1.31233025146306));
#79485=CARTESIAN_POINT('Ctrl Pts',(3.6822185871438,-18.8270791977462,1.30159301515885));
#79486=CARTESIAN_POINT('Ctrl Pts',(3.67931974328277,-18.8203454871076,1.2913464747379));
#79487=CARTESIAN_POINT('Ctrl Pts',(3.67582593698265,-18.8122297410447,1.27899692119402));
#79488=CARTESIAN_POINT('Ctrl Pts',(3.67174917848949,-18.8035434413388,1.26736803909472));
#79489=CARTESIAN_POINT('Ctrl Pts',(3.66718993232582,-18.7944372259978,1.25649703253233));
#79490=CARTESIAN_POINT('Ctrl Pts',(3.66234651516983,-18.7847634338783,1.24494845239495));
#79491=CARTESIAN_POINT('Ctrl Pts',(3.65695962342466,-18.7746169626732,1.23425432847766));
#79492=CARTESIAN_POINT('Ctrl Pts',(3.65114867253215,-18.7641618421269,1.22440440488792));
#79493=CARTESIAN_POINT('Ctrl Pts',(3.64917857203113,-18.7606172177432,1.22106496186765));
#79494=CARTESIAN_POINT('Ctrl Pts',(3.64715964689312,-18.757036896294,1.2178221718728));
#79495=CARTESIAN_POINT('Ctrl Pts',(3.64509617810887,-18.7534264676304,1.21467461506629));
#79496=CARTESIAN_POINT('Ctrl Pts',(3.63944836659227,-18.7435445538637,1.20605960343313));
#79497=CARTESIAN_POINT('Ctrl Pts',(3.633460487968,-18.7334271310955,1.19815442516915));
#79498=CARTESIAN_POINT('Ctrl Pts',(3.62720830935474,-18.7231697043666,1.19091932962045));
#79499=CARTESIAN_POINT('Ctrl Pts',(3.62167996051964,-18.714099804638,1.18452185851114));
#79500=CARTESIAN_POINT('Ctrl Pts',(3.6159451061393,-18.7049204146876,1.17864749381264));
#79501=CARTESIAN_POINT('Ctrl Pts',(3.6100371140147,-18.6956695920241,1.17326377729281));
#79502=CARTESIAN_POINT('',(3.69310715887669,-18.9880798391386,1.73153298807645));
#79503=CARTESIAN_POINT('Origin',(3.69310715296,-21.2594877202,0.729452270839));
#79504=CARTESIAN_POINT('Ctrl Pts',(3.37113078856,-18.8600780815,2.3667703805));
#79505=CARTESIAN_POINT('Ctrl Pts',(3.38869201095644,-18.8750724420214,2.35258647558843));
#79506=CARTESIAN_POINT('Ctrl Pts',(3.40608515391958,-18.8895522416563,2.33732078134583));
#79507=CARTESIAN_POINT('Ctrl Pts',(3.42323107209452,-18.9033876245546,2.3209245028101));
#79508=CARTESIAN_POINT('Ctrl Pts',(3.43956662988178,-18.9165691115148,2.30530315475608));
#79509=CARTESIAN_POINT('Ctrl Pts',(3.45567875628968,-18.9291660813847,2.28865339509923));
#79510=CARTESIAN_POINT('Ctrl Pts',(3.47148097362641,-18.941031716602,2.27091454974452));
#79511=CARTESIAN_POINT('Ctrl Pts',(3.48145442077251,-18.9485206204168,2.25971881481643));
#79512=CARTESIAN_POINT('Ctrl Pts',(3.49130400916866,-18.9557174945842,2.24808899655903));
#79513=CARTESIAN_POINT('Ctrl Pts',(3.50100148868141,-18.9625766922123,2.23601134904976));
#79514=CARTESIAN_POINT('Ctrl Pts',(3.51433259176288,-18.9720060156272,2.21940823442436));
#79515=CARTESIAN_POINT('Ctrl Pts',(3.52737641560849,-18.9807981294339,2.20195966579905));
#79516=CARTESIAN_POINT('Ctrl Pts',(3.54003953644244,-18.9888089790747,2.18363951709586));
#79517=CARTESIAN_POINT('Ctrl Pts',(3.55176141000878,-18.9962243838457,2.16668110142319));
#79518=CARTESIAN_POINT('Ctrl Pts',(3.56315714645582,-19.0029702658348,2.14897543228294));
#79519=CARTESIAN_POINT('Ctrl Pts',(3.57412705154925,-19.0089055820898,2.13052377010484));
#79520=CARTESIAN_POINT('Ctrl Pts',(3.58434149779586,-19.0144321539542,2.1133428091144));
#79521=CARTESIAN_POINT('Ctrl Pts',(3.5941867472996,-19.0192558666883,2.09551485099505));
#79522=CARTESIAN_POINT('Ctrl Pts',(3.60355875961401,-19.0232399131184,2.07706497899717));
#79523=CARTESIAN_POINT('Ctrl Pts',(3.61170017077009,-19.0267008304716,2.0610376853197));
#79524=CARTESIAN_POINT('Ctrl Pts',(3.61948537973937,-19.0295289947164,2.04453960996809));
#79525=CARTESIAN_POINT('Ctrl Pts',(3.62683611450434,-19.0316290862057,2.02760646710804));
#79526=CARTESIAN_POINT('Ctrl Pts',(3.63154312600466,-19.0329738707896,2.01676340165577));
#79527=CARTESIAN_POINT('Ctrl Pts',(3.63607140171859,-19.0340197317384,2.00574295712455));
#79528=CARTESIAN_POINT('Ctrl Pts',(3.64039632492325,-19.0347403250418,1.99456470966233));
#79529=CARTESIAN_POINT('Ctrl Pts',(3.64746980999939,-19.0359188675816,1.97628249680911));
#79530=CARTESIAN_POINT('Ctrl Pts',(3.65400205458385,-19.0362261503123,1.95756779122123));
#79531=CARTESIAN_POINT('Ctrl Pts',(3.65987960155281,-19.0355527052212,1.93853802054784));
#79532=CARTESIAN_POINT('Ctrl Pts',(3.66321196102245,-19.0351708858774,1.9277488193992));
#79533=CARTESIAN_POINT('Ctrl Pts',(3.66633371725679,-19.0344740007227,1.91685925102004));
#79534=CARTESIAN_POINT('Ctrl Pts',(3.66922427296373,-19.0334452293648,1.90589752741063));
#79535=CARTESIAN_POINT('Ctrl Pts',(3.67389612842881,-19.0317824795068,1.88818066133241));
#79536=CARTESIAN_POINT('Ctrl Pts',(3.6779632719388,-19.0292505095148,1.87027265608766));
#79537=CARTESIAN_POINT('Ctrl Pts',(3.68134407166181,-19.0258010723225,1.85232717239278));
#79538=CARTESIAN_POINT('Ctrl Pts',(3.68472487138482,-19.0223516351301,1.83438168869789));
#79539=CARTESIAN_POINT('Ctrl Pts',(3.68741859100349,-19.0179838058214,1.81639899816153));
#79540=CARTESIAN_POINT('Ctrl Pts',(3.68936491766357,-19.0126923096433,1.79856209470954));
#79541=CARTESIAN_POINT('Ctrl Pts',(3.691175201474,-19.0077706744108,1.7819719414688));
#79542=CARTESIAN_POINT('Ctrl Pts',(3.692339054035,-19.002052117354,1.76551215189331));
#79543=CARTESIAN_POINT('Ctrl Pts',(3.6928332680798,-18.9955694742247,1.74933281835986));
#79544=CARTESIAN_POINT('Ctrl Pts',(3.69301576350472,-18.9931756678873,1.74335837392833));
#79545=CARTESIAN_POINT('Ctrl Pts',(3.69310717012609,-18.9906780722399,1.73742235791273));
#79546=CARTESIAN_POINT('Ctrl Pts',(3.69310716565,-18.9880798435563,1.73153298612752));
#79547=CARTESIAN_POINT('',(-3.69310712510398,-18.9880798224936,1.73153306834489));
#79548=CARTESIAN_POINT('Ctrl Pts',(-3.6931070974719,-18.9880797849051,1.73153308492801));
#79549=CARTESIAN_POINT('Ctrl Pts',(-3.69310712468246,-18.9952618512105,
1.74781251238661));
#79550=CARTESIAN_POINT('Ctrl Pts',(-3.69240312457171,-19.0016683605087,
1.76445127512417));
#79551=CARTESIAN_POINT('Ctrl Pts',(-3.69101646164415,-19.0072517991255,
1.78127248331884));
#79552=CARTESIAN_POINT('Ctrl Pts',(-3.68965395140338,-19.0127379862463,
1.79780070223347));
#79553=CARTESIAN_POINT('Ctrl Pts',(-3.68763275825615,-19.017430215499,1.81450532064328));
#79554=CARTESIAN_POINT('Ctrl Pts',(-3.68499110971516,-19.0213207375549,
1.83124459990243));
#79555=CARTESIAN_POINT('Ctrl Pts',(-3.68216847190293,-19.0254778139009,
1.8491307501049));
#79556=CARTESIAN_POINT('Ctrl Pts',(-3.67863801749283,-19.0287156564556,
1.86704641253439));
#79557=CARTESIAN_POINT('Ctrl Pts',(-3.67447191242615,-19.0310659770756,
1.88483002313483));
#79558=CARTESIAN_POINT('Ctrl Pts',(-3.67001185511461,-19.0335821317326,
1.90386841060097));
#79559=CARTESIAN_POINT('Ctrl Pts',(-3.66482382726056,-19.0350816807103,
1.92275500216907));
#79560=CARTESIAN_POINT('Ctrl Pts',(-3.65901330345387,-19.0356459181985,
1.94133377213654));
#79561=CARTESIAN_POINT('Ctrl Pts',(-3.65432965714411,-19.0361007289725,
1.95630942498522));
#79562=CARTESIAN_POINT('Ctrl Pts',(-3.64924205643322,-19.0359489177316,
1.97108592139919));
#79563=CARTESIAN_POINT('Ctrl Pts',(-3.64380874651171,-19.0352461876269,
1.98560194762267));
#79564=CARTESIAN_POINT('Ctrl Pts',(-3.636611460834,-19.0343153095082,2.00483073985879));
#79565=CARTESIAN_POINT('Ctrl Pts',(-3.62880017214108,-19.0324130278275,
2.02361561274625));
#79566=CARTESIAN_POINT('Ctrl Pts',(-3.62049718169822,-19.0296723870873,
2.04186416513173));
#79567=CARTESIAN_POINT('Ctrl Pts',(-3.61264412060128,-19.027080258465,2.05912384979597));
#79568=CARTESIAN_POINT('Ctrl Pts',(-3.60435188602754,-19.0237393408979,
2.07590422321751));
#79569=CARTESIAN_POINT('Ctrl Pts',(-3.59570735538278,-19.0197564272955,
2.09216768631108));
#79570=CARTESIAN_POINT('Ctrl Pts',(-3.58793996124586,-19.0161776488708,
2.10678094098853));
#79571=CARTESIAN_POINT('Ctrl Pts',(-3.57988831651865,-19.0120810419503,
2.12097740580257));
#79572=CARTESIAN_POINT('Ctrl Pts',(-3.57159642781692,-19.0075286801433,
2.13475630859865));
#79573=CARTESIAN_POINT('Ctrl Pts',(-3.56060098950043,-19.0014920321319,
2.15302778825944));
#79574=CARTESIAN_POINT('Ctrl Pts',(-3.5491896971999,-18.9946593716137,2.17055724509778));
#79575=CARTESIAN_POINT('Ctrl Pts',(-3.53746128646186,-18.987172096478,2.187346950558));
#79576=CARTESIAN_POINT('Ctrl Pts',(-3.52445129523402,-18.9788666759046,
2.2059712915394));
#79577=CARTESIAN_POINT('Ctrl Pts',(-3.5110510390571,-18.9697558575544,2.22368578081534));
#79578=CARTESIAN_POINT('Ctrl Pts',(-3.49735539490297,-18.9599880019219,
2.24052062372232));
#79579=CARTESIAN_POINT('Ctrl Pts',(-3.48177128506724,-18.9488732757123,
2.25967679030909));
#79580=CARTESIAN_POINT('Ctrl Pts',(-3.46580843265995,-18.9369119359418,
2.27769158122885));
#79581=CARTESIAN_POINT('Ctrl Pts',(-3.44957385322151,-18.9242777572026,
2.29462021847525));
#79582=CARTESIAN_POINT('Ctrl Pts',(-3.43869249211144,-18.9158095944324,
2.30596677757017));
#79583=CARTESIAN_POINT('Ctrl Pts',(-3.4276880862854,-18.9070380273395,2.31682600136214));
#79584=CARTESIAN_POINT('Ctrl Pts',(-3.41658548099764,-18.8980052477675,
2.32721594002643));
#79585=CARTESIAN_POINT('Ctrl Pts',(-3.40159501320036,-18.8858094083421,
2.34124418267092));
#79586=CARTESIAN_POINT('Ctrl Pts',(-3.38642762053579,-18.8731390420533,
2.35441545122519));
#79587=CARTESIAN_POINT('Ctrl Pts',(-3.37113079773101,-18.8600780989522,
2.36677042601625));
#79588=CARTESIAN_POINT('',(-3.69310717902964,-18.8681378087753,1.39646426604976));
#79589=CARTESIAN_POINT('Origin',(-3.69310715296,-21.2594877202,0.729452270839));
#79590=CARTESIAN_POINT('Ctrl Pts',(-3.6100371473659,-18.6956696732068,1.17326396103852));
#79591=CARTESIAN_POINT('Ctrl Pts',(-3.61657749559202,-18.705910653501,1.17922394382632));
#79592=CARTESIAN_POINT('Ctrl Pts',(-3.62290464780229,-18.7160628008001,
1.18578600728785));
#79593=CARTESIAN_POINT('Ctrl Pts',(-3.62897495461051,-18.7260771573293,
1.19299524943752));
#79594=CARTESIAN_POINT('Ctrl Pts',(-3.6355512914387,-18.7369263258697,1.20080546499171));
#79595=CARTESIAN_POINT('Ctrl Pts',(-3.64182562246628,-18.7476133476187,
1.20937651984719));
#79596=CARTESIAN_POINT('Ctrl Pts',(-3.64770746228359,-18.7580240682704,
1.21875450143649));
#79597=CARTESIAN_POINT('Ctrl Pts',(-3.65261309355745,-18.7667069223432,
1.22657602007674));
#79598=CARTESIAN_POINT('Ctrl Pts',(-3.65724475415457,-18.7751962949054,
1.23495899770559));
#79599=CARTESIAN_POINT('Ctrl Pts',(-3.66153876063084,-18.78340609774,1.24391468191898));
#79600=CARTESIAN_POINT('Ctrl Pts',(-3.66633688812616,-18.7925797403346,
1.25392177317539));
#79601=CARTESIAN_POINT('Ctrl Pts',(-3.67071998458647,-18.8014160030125,
1.26465261682475));
#79602=CARTESIAN_POINT('Ctrl Pts',(-3.67458836821826,-18.8097703758799,
1.2760889058583));
#79603=CARTESIAN_POINT('Ctrl Pts',(-3.67745768618513,-18.8159671118947,
1.2845716088996));
#79604=CARTESIAN_POINT('Ctrl Pts',(-3.6800436539183,-18.8218982880675,1.2934417126838));
#79605=CARTESIAN_POINT('Ctrl Pts',(-3.68230789365157,-18.8275029762944,
1.30267319568792));
#79606=CARTESIAN_POINT('Ctrl Pts',(-3.68499199445435,-18.8341469495223,
1.31361648520723));
#79607=CARTESIAN_POINT('Ctrl Pts',(-3.68722236982464,-18.8403304069624,
1.32506993521974));
#79608=CARTESIAN_POINT('Ctrl Pts',(-3.68894069456791,-18.8459471700852,
1.33694694132116));
#79609=CARTESIAN_POINT('Ctrl Pts',(-3.68931992656701,-18.8471867822806,
1.33956818086555));
#79610=CARTESIAN_POINT('Ctrl Pts',(-3.68967428152814,-18.84839882896,1.34220986509019));
#79611=CARTESIAN_POINT('Ctrl Pts',(-3.69000325102315,-18.8495822432019,
1.34487073876146));
#79612=CARTESIAN_POINT('Ctrl Pts',(-3.69147094096868,-18.8548620190185,
1.3567421663343));
#79613=CARTESIAN_POINT('Ctrl Pts',(-3.69243036931968,-18.8595676287777,
1.36899573143837));
#79614=CARTESIAN_POINT('Ctrl Pts',(-3.69285480927325,-18.8636259589294,
1.38150306134678));
#79615=CARTESIAN_POINT('Ctrl Pts',(-3.69302282682337,-18.8652324775522,
1.38645417613242));
#79616=CARTESIAN_POINT('Ctrl Pts',(-3.69310721706151,-18.8667377203947,
1.39144456789607));
#79617=CARTESIAN_POINT('Ctrl Pts',(-3.69310720833,-18.8681378362,1.39646425696));
#79618=CARTESIAN_POINT('',(-2.19100517774646,-17.3987921007756,1.04094166879275));
#79619=CARTESIAN_POINT('Ctrl Pts',(-2.19100517814,-17.398792101,1.04094166862));
#79620=CARTESIAN_POINT('Ctrl Pts',(-2.23340908046747,-17.4211505588617,
1.01979176987668));
#79621=CARTESIAN_POINT('Ctrl Pts',(-2.27587182040943,-17.4447260821378,
1.00009119561888));
#79622=CARTESIAN_POINT('Ctrl Pts',(-2.31831144523611,-17.4694731033439,
0.981872772926845));
#79623=CARTESIAN_POINT('Ctrl Pts',(-2.36028923173101,-17.4939508214391,
0.963852607546885));
#79624=CARTESIAN_POINT('Ctrl Pts',(-2.40224490185501,-17.5195750573229,
0.947282414042425));
#79625=CARTESIAN_POINT('Ctrl Pts',(-2.4441036705446,-17.5463069780681,0.932244093891202));
#79626=CARTESIAN_POINT('Ctrl Pts',(-2.4689116555243,-17.5621498972243,0.923331494880038));
#79627=CARTESIAN_POINT('Ctrl Pts',(-2.49368565427865,-17.5783819578072,
0.914957918947159));
#79628=CARTESIAN_POINT('Ctrl Pts',(-2.51840978812709,-17.5949951496287,
0.907149090937463));
#79629=CARTESIAN_POINT('Ctrl Pts',(-2.55914933281228,-17.62236977374,0.894281983050483));
#79630=CARTESIAN_POINT('Ctrl Pts',(-2.59975309442327,-17.6507789369978,
0.882945861082856));
#79631=CARTESIAN_POINT('Ctrl Pts',(-2.64014296081438,-17.6801826263446,
0.873295721186059));
#79632=CARTESIAN_POINT('Ctrl Pts',(-2.6795212705324,-17.708849905774,0.863887267243712));
#79633=CARTESIAN_POINT('Ctrl Pts',(-2.71869660392543,-17.7384627806698,
0.85608145628018));
#79634=CARTESIAN_POINT('Ctrl Pts',(-2.7575849771126,-17.7689766998058,0.85006896734053));
#79635=CARTESIAN_POINT('Ctrl Pts',(-2.7851804530791,-17.7906296015127,0.845802460916248));
#79636=CARTESIAN_POINT('Ctrl Pts',(-2.81263120385022,-17.812736071274,0.842439932418081));
#79637=CARTESIAN_POINT('Ctrl Pts',(-2.83990214642615,-17.8352767486052,
0.840064297938821));
#79638=CARTESIAN_POINT('Ctrl Pts',(-2.87328324226734,-17.8628677461742,
0.837156393966854));
#79639=CARTESIAN_POINT('Ctrl Pts',(-2.90639530240287,-17.891109212603,0.835726215071071));
#79640=CARTESIAN_POINT('Ctrl Pts',(-2.93914685009623,-17.9199408622635,
0.835961192073837));
#79641=CARTESIAN_POINT('Ctrl Pts',(-2.96947375622024,-17.9466380657312,
0.836178773409867));
#79642=CARTESIAN_POINT('Ctrl Pts',(-2.99949281327367,-17.9738427332933,
0.837824051866936));
#79643=CARTESIAN_POINT('Ctrl Pts',(-3.02911562216786,-18.0014956493843,
0.841081001191144));
#79644=CARTESIAN_POINT('Ctrl Pts',(-3.05593606414302,-18.0265325536872,
0.844029837700133));
#79645=CARTESIAN_POINT('Ctrl Pts',(-3.08242830728943,-18.0519338760314,
0.848299586612206));
#79646=CARTESIAN_POINT('Ctrl Pts',(-3.1085035339598,-18.0776339030635,0.854055690967447));
#79647=CARTESIAN_POINT('Ctrl Pts',(-3.13266890449484,-18.1014515551147,
0.859390194722339));
#79648=CARTESIAN_POINT('Ctrl Pts',(-3.15647636754392,-18.1255260738493,
0.866001401350056));
#79649=CARTESIAN_POINT('Ctrl Pts',(-3.17982784457826,-18.1497786992006,
0.874045427786549));
#79650=CARTESIAN_POINT('Ctrl Pts',(-3.18918972837626,-18.1595018640351,
0.877270373285958));
#79651=CARTESIAN_POINT('Ctrl Pts',(-3.19847797729243,-18.1692533183757,
0.880725897195602));
#79652=CARTESIAN_POINT('Ctrl Pts',(-3.20768476668501,-18.1790264993383,
0.884423229782778));
#79653=CARTESIAN_POINT('Ctrl Pts',(-3.22918262193891,-18.2018468790326,
0.893056502185938));
#79654=CARTESIAN_POINT('Ctrl Pts',(-3.25024132019591,-18.2247909364654,
0.903007502286362));
#79655=CARTESIAN_POINT('Ctrl Pts',(-3.27073539415306,-18.2477489410748,
0.914432724385656));
#79656=CARTESIAN_POINT('Ctrl Pts',(-3.28355491073038,-18.2621097031804,
0.921579464677882));
#79657=CARTESIAN_POINT('Ctrl Pts',(-3.2961529105563,-18.2764753126739,0.929303427275135));
#79658=CARTESIAN_POINT('Ctrl Pts',(-3.3084919913374,-18.2908119591701,0.937647026553946));
#79659=CARTESIAN_POINT('',(-2.15473684280641,-17.3799083491911,1.05880473008226));
#79660=CARTESIAN_POINT('Origin',(2.6645352591E-15,-19.5917976147,-1.03352917222));
#79661=CARTESIAN_POINT('',(-2.15473684927718,-17.5697153655739,-0.513604050767344));
#79662=CARTESIAN_POINT('Origin',(-2.15473684211,-21.2594877202,0.729452270839));
#79663=CARTESIAN_POINT('Ctrl Pts',(-2.63891667022851,-17.8998816183554,
-0.516206449710607));
#79664=CARTESIAN_POINT('Ctrl Pts',(-2.61310289645698,-17.8776779425526,
-0.511008230762591));
#79665=CARTESIAN_POINT('Ctrl Pts',(-2.58678584252352,-17.8560536455099,
-0.507010684885198));
#79666=CARTESIAN_POINT('Ctrl Pts',(-2.56007862673513,-17.8350057727795,
-0.504006626604018));
#79667=CARTESIAN_POINT('Ctrl Pts',(-2.54018464775287,-17.8193273905386,
-0.501768929017689));
#79668=CARTESIAN_POINT('Ctrl Pts',(-2.52007339480444,-17.8039686517226,
-0.500083506521339));
#79669=CARTESIAN_POINT('Ctrl Pts',(-2.49978049122198,-17.7889257868244,
-0.498879424947764));
#79670=CARTESIAN_POINT('Ctrl Pts',(-2.46921773238009,-17.7662700120947,
-0.497065980429606));
#79671=CARTESIAN_POINT('Ctrl Pts',(-2.43823442114583,-17.744323941143,-0.496342120194636));
#79672=CARTESIAN_POINT('Ctrl Pts',(-2.40693510521941,-17.7230793986878,
-0.496510632439663));
#79673=CARTESIAN_POINT('Ctrl Pts',(-2.38602396458181,-17.7088858739441,
-0.496623215834878));
#79674=CARTESIAN_POINT('Ctrl Pts',(-2.36497297898658,-17.6950065181827,
-0.497135038263675));
#79675=CARTESIAN_POINT('Ctrl Pts',(-2.34379920732961,-17.6814325355428,
-0.497997390597506));
#79676=CARTESIAN_POINT('Ctrl Pts',(-2.30607364552788,-17.6572476085834,
-0.499533854048225));
#79677=CARTESIAN_POINT('Ctrl Pts',(-2.26794946462982,-17.6340259944123,
-0.502181444449583));
#79678=CARTESIAN_POINT('Ctrl Pts',(-2.22952537353873,-17.6117366097388,
-0.505711726429428));
#79679=CARTESIAN_POINT('Ctrl Pts',(-2.2214515349402,-17.6070530664407,-0.506453524767481));
#79680=CARTESIAN_POINT('Ctrl Pts',(-2.21336435003307,-17.6024106613826,
-0.507234449505707));
#79681=CARTESIAN_POINT('Ctrl Pts',(-2.2052645934251,-17.5978090805389,-0.508052596842114));
#79682=CARTESIAN_POINT('Ctrl Pts',(-2.18847673544652,-17.5882716722659,
-0.509748319559959));
#79683=CARTESIAN_POINT('Ctrl Pts',(-2.17163270974699,-17.5789083811218,
-0.511604117245896));
#79684=CARTESIAN_POINT('Ctrl Pts',(-2.1547368444,-17.5697153922,-0.513604062953));
#79685=CARTESIAN_POINT('',(-3.69310715294,-19.4224990402,-0.940557353778));
#79686=CARTESIAN_POINT('Ctrl Pts',(-3.69310715294,-19.4224990402,-0.940557353778));
#79687=CARTESIAN_POINT('Ctrl Pts',(-3.69310715296,-19.4065320759,-0.922993902523));
#79688=CARTESIAN_POINT('Ctrl Pts',(-3.69165304038,-19.3892706346,-0.906800491528));
#79689=CARTESIAN_POINT('Ctrl Pts',(-3.6887805345,-19.3710481782,-0.89227543696));
#79690=CARTESIAN_POINT('Ctrl Pts',(-3.68066808926,-19.3340162227,-0.867105044941));
#79691=CARTESIAN_POINT('Ctrl Pts',(-3.66836754819,-19.2957464376,-0.84852225854));
#79692=CARTESIAN_POINT('Ctrl Pts',(-3.66145077635,-19.2768489319,-0.840929561713));
#79693=CARTESIAN_POINT('Ctrl Pts',(-3.65309699002,-19.2562736874,-0.834189818013));
#79694=CARTESIAN_POINT('Ctrl Pts',(-3.64401528261,-19.235933638,-0.82903655384));
#79695=CARTESIAN_POINT('Ctrl Pts',(-3.64322047583,-19.2341674975,-0.8286005087));
#79696=CARTESIAN_POINT('Ctrl Pts',(-3.64242036464,-19.2324033163,-0.828176257781));
#79697=CARTESIAN_POINT('Ctrl Pts',(-3.64161503967,-19.2306411737,-0.82776370433));
#79698=CARTESIAN_POINT('',(-3.69310715914368,-19.4536303579338,-0.974172892806444));
#79699=CARTESIAN_POINT('Origin',(-3.69310715296,-21.2594877202,0.729452270839));
#79700=CARTESIAN_POINT('Ctrl Pts',(-3.02151310328351,-19.2807402657353,
-1.87007020034346));
#79701=CARTESIAN_POINT('Ctrl Pts',(-3.09553406839226,-19.3510460935362,
-1.83754967268177));
#79702=CARTESIAN_POINT('Ctrl Pts',(-3.17165791739679,-19.4158556004616,
-1.79287227600525));
#79703=CARTESIAN_POINT('Ctrl Pts',(-3.24819012525093,-19.4734829893339,
-1.73672176875692));
#79704=CARTESIAN_POINT('Ctrl Pts',(-3.41578700005397,-19.5829245957743,
-1.58670170203268));
#79705=CARTESIAN_POINT('Ctrl Pts',(-3.56871476432,-19.6239406117,-1.37338573889));
#79706=CARTESIAN_POINT('Ctrl Pts',(-3.64775681814,-19.6269188806,-1.23837648486));
#79707=CARTESIAN_POINT('Ctrl Pts',(-3.69310705761,-19.5585539651,-1.08539296335));
#79708=CARTESIAN_POINT('Ctrl Pts',(-3.69310716493,-19.4536303642,-0.974172886895));
#79709=CARTESIAN_POINT('Origin',(-3.62140732971,-22.5742356128,-0.813060915858));
#79710=CARTESIAN_POINT('Origin',(-3.62140732971,-22.5742356128,-0.813060915858));
#79711=CARTESIAN_POINT('Origin',(-3.62140732971,-22.5742356128,-0.813060915858));
#79712=CARTESIAN_POINT('Origin',(3.06421554797E-14,-20.9451161625,-0.329359384015));
#79713=CARTESIAN_POINT('Origin',(-3.92508992491174,-21.6853542976041,-0.549143341414481));
#79714=CARTESIAN_POINT('Ctrl Pts',(-3.92508992147,-21.7707429986,-0.261552017256));
#79715=CARTESIAN_POINT('Ctrl Pts',(-4.03342461998,-21.7911739897,-0.267618178739));
#79716=CARTESIAN_POINT('Ctrl Pts',(-4.14175931848,-21.7971474542,-0.322377668836));
#79717=CARTESIAN_POINT('Ctrl Pts',(-4.21845505507,-21.7823881416,-0.425097625007));
#79718=CARTESIAN_POINT('Ctrl Pts',(-4.23766395197,-21.7518702125,-0.54115952752));
#79719=CARTESIAN_POINT('Ctrl Pts',(-4.20883136158,-21.7161398512,-0.641571945224));
#79720=CARTESIAN_POINT('Ctrl Pts',(-3.94759644554,-21.7159070143,-0.24527067605));
#79721=CARTESIAN_POINT('Ctrl Pts',(-4.05328464276,-21.7371102811,-0.255805200216));
#79722=CARTESIAN_POINT('Ctrl Pts',(-4.15897283998,-21.7351498417,-0.310328579867));
#79723=CARTESIAN_POINT('Ctrl Pts',(-4.23513914343,-21.7036118067,-0.406713304892));
#79724=CARTESIAN_POINT('Ctrl Pts',(-4.25724960966,-21.6529065911,-0.513996782083));
#79725=CARTESIAN_POINT('Ctrl Pts',(-4.23296486329,-21.5985397884,-0.606655333963));
#79726=CARTESIAN_POINT('Ctrl Pts',(-3.97344038914,-21.6649651461,-0.215923674571));
#79727=CARTESIAN_POINT('Ctrl Pts',(-4.07632734574,-21.6845810666,-0.231225393142));
#79728=CARTESIAN_POINT('Ctrl Pts',(-4.17921430233,-21.6739831683,-0.283645658503));
#79729=CARTESIAN_POINT('Ctrl Pts',(-4.25480701452,-21.6274260446,-0.369684305774));
#79730=CARTESIAN_POINT('Ctrl Pts',(-4.28000999959,-21.5595174516,-0.463325016282));
#79731=CARTESIAN_POINT('Ctrl Pts',(-4.26067703305,-21.4892929177,-0.543718994175));
#79732=CARTESIAN_POINT('Ctrl Pts',(-4.00108738171,-21.6214550864,-0.174510379657));
#79733=CARTESIAN_POINT('Ctrl Pts',(-4.10130066591,-21.6370722475,-0.193345955876));
#79734=CARTESIAN_POINT('Ctrl Pts',(-4.20151395011,-21.6177478772,-0.241119104285));
#79735=CARTESIAN_POINT('Ctrl Pts',(-4.27654182968,-21.5590499941,-0.31352875262));
#79736=CARTESIAN_POINT('Ctrl Pts',(-4.30472727966,-21.4781628509,-0.390049652199));
#79737=CARTESIAN_POINT('Ctrl Pts',(-4.2903226061,-21.3959799196,-0.454903382914));
#79738=CARTESIAN_POINT('Ctrl Pts',(-4.02839244452,-21.5894619149,-0.1235267805));
#79739=CARTESIAN_POINT('Ctrl Pts',(-4.1262158112,-21.6002037523,-0.143534649036));
#79740=CARTESIAN_POINT('Ctrl Pts',(-4.22403917788,-21.5735622712,-0.18407007299));
#79741=CARTESIAN_POINT('Ctrl Pts',(-4.2985508016,-21.5064407622,-0.240681885995));
#79742=CARTESIAN_POINT('Ctrl Pts',(-4.32942734489,-21.4172155069,-0.298160451165));
#79743=CARTESIAN_POINT('Ctrl Pts',(-4.31960153738,-21.3273684168,-0.345566059647));
#79744=CARTESIAN_POINT('Ctrl Pts',(-4.0532699684,-21.5710708632,-0.0674504949952));
#79745=CARTESIAN_POINT('Ctrl Pts',(-4.14906265325,-21.5773628865,-0.0866355663445));
#79746=CARTESIAN_POINT('Ctrl Pts',(-4.2448553381,-21.545710571,-0.11826504072));
#79747=CARTESIAN_POINT('Ctrl Pts',(-4.31892158577,-21.4741377326,-0.158167701262));
#79748=CARTESIAN_POINT('Ctrl Pts',(-4.35210057067,-21.3811601556,-0.196020790393));
#79749=CARTESIAN_POINT('Ctrl Pts',(-4.34627743719,-21.2879273681,-0.225306170569));
#79750=CARTESIAN_POINT('Origin',(4.36983782492E-13,-22.5742356128,0.729452270839));
#79751=CARTESIAN_POINT('Origin',(2.45,0.,0.));
#79752=CARTESIAN_POINT('',(2.45,-0.730765926094,-8.94930152316968E-17));
#79753=CARTESIAN_POINT('Origin',(2.45,0.,0.));
#79754=CARTESIAN_POINT('Origin',(0.,0.,0.));
#79755=CARTESIAN_POINT('',(4.,-0.730765926094,-8.94930152316968E-17));
#79756=CARTESIAN_POINT('',(0.,-0.730765926094,-8.94930152316968E-17));
#79757=CARTESIAN_POINT('Origin',(4.,0.,0.));
#79758=CARTESIAN_POINT('Origin',(4.,0.,0.));
#79759=CARTESIAN_POINT('',(4.,-6.41575007864,3.96554608849));
#79760=CARTESIAN_POINT('',(4.,-8.14391944342,-3.85542016568));
#79761=CARTESIAN_POINT('Origin',(4.,-9.17423561284,0.47366156039));
#79762=CARTESIAN_POINT('',(4.,2.8773238354,-3.85542016568));
#79763=CARTESIAN_POINT('',(4.,-3.42065492897,-3.85542016568));
#79764=CARTESIAN_POINT('',(4.,3.0773238354,-3.65542016568));
#79765=CARTESIAN_POINT('Origin',(4.,2.8773238354,-3.65542016568));
#79766=CARTESIAN_POINT('',(4.,3.0773238354,1.84387696505));
#79767=CARTESIAN_POINT('',(4.,3.0773238354,0.47366156039));
#79768=CARTESIAN_POINT('',(4.,2.8773238354,2.04387696505));
#79769=CARTESIAN_POINT('Origin',(4.,2.8773238354,1.84387696505));
#79770=CARTESIAN_POINT('',(4.,-2.12788809108,2.04387696505));
#79771=CARTESIAN_POINT('',(4.,-2.74845588872,2.04387696505));
#79772=CARTESIAN_POINT('',(4.,-2.69184369587,2.1725725316));
#79773=CARTESIAN_POINT('Origin',(4.,-2.12788809108,3.34387696505));
#79774=CARTESIAN_POINT('',(4.,-2.74845588872,2.19982997428));
#79775=CARTESIAN_POINT('Origin',(4.3,-2.74845588872,2.19982997428));
#79776=CARTESIAN_POINT('',(4.3,-2.56170009476,2.4428735547));
#79777=CARTESIAN_POINT('Origin',(4.3,-2.69184369587,2.1725725316));
#79778=CARTESIAN_POINT('',(4.3,-6.28560647753,4.2358471116));
#79779=CARTESIAN_POINT('',(4.3,-4.42365328615,3.33936033315));
#79780=CARTESIAN_POINT('Origin',(4.29787870950426,-6.41482982759964,3.96745737345475));
#79781=CARTESIAN_POINT('Origin',(4.3,-2.12788809108,3.34387696505));
#79782=CARTESIAN_POINT('',(4.3,-2.12788809108,2.34387696505));
#79783=CARTESIAN_POINT('Origin',(4.3,-2.12788809108,2.04387696505));
#79784=CARTESIAN_POINT('Origin',(4.3,-2.12788809108,3.34387696505));
#79785=CARTESIAN_POINT('Origin',(4.3,-2.74845588872,2.04387696505));
#79786=CARTESIAN_POINT('',(4.3,2.8773238354,2.34387696505));
#79787=CARTESIAN_POINT('Origin',(4.3,2.8773238354,2.04387696505));
#79788=CARTESIAN_POINT('',(4.3,0.374717872161,2.34387696505));
#79789=CARTESIAN_POINT('Ctrl Pts',(4.,3.0773238354,1.84387696505));
#79790=CARTESIAN_POINT('Ctrl Pts',(4.,3.0773238354,2.04387696505));
#79791=CARTESIAN_POINT('Ctrl Pts',(4.,2.8773238354,2.04387696505));
#79792=CARTESIAN_POINT('Ctrl Pts',(4.,3.3773238354,1.84387696505));
#79793=CARTESIAN_POINT('Ctrl Pts',(4.,3.3773238354,2.34387696505));
#79794=CARTESIAN_POINT('Ctrl Pts',(4.,2.8773238354,2.34387696505));
#79795=CARTESIAN_POINT('Ctrl Pts',(4.3,3.3773238354,1.84387696505));
#79796=CARTESIAN_POINT('Ctrl Pts',(4.3,3.3773238354,2.34387696505));
#79797=CARTESIAN_POINT('Ctrl Pts',(4.3,2.8773238354,2.34387696505));
#79798=CARTESIAN_POINT('',(4.3,3.3773238354,1.84387696505));
#79799=CARTESIAN_POINT('Origin',(4.3,3.0773238354,1.84387696505));
#79800=CARTESIAN_POINT('Origin',(4.3,2.8773238354,1.84387696505));
#79801=CARTESIAN_POINT('Origin',(4.3,3.0773238354,0.47366156039));
#79802=CARTESIAN_POINT('',(4.3,3.3773238354,-3.65542016568));
#79803=CARTESIAN_POINT('Origin',(4.3,3.0773238354,-3.65542016568));
#79804=CARTESIAN_POINT('',(4.3,3.3773238354,-0.905771600316));
#79805=CARTESIAN_POINT('Ctrl Pts',(4.,2.8773238354,-3.85542016568));
#79806=CARTESIAN_POINT('Ctrl Pts',(4.,3.0773238354,-3.85542016568));
#79807=CARTESIAN_POINT('Ctrl Pts',(4.,3.0773238354,-3.65542016568));
#79808=CARTESIAN_POINT('Ctrl Pts',(4.,2.8773238354,-4.15542016568));
#79809=CARTESIAN_POINT('Ctrl Pts',(4.,3.3773238354,-4.15542016568));
#79810=CARTESIAN_POINT('Ctrl Pts',(4.,3.3773238354,-3.65542016568));
#79811=CARTESIAN_POINT('Ctrl Pts',(4.3,2.8773238354,-4.15542016568));
#79812=CARTESIAN_POINT('Ctrl Pts',(4.3,3.3773238354,-4.15542016568));
#79813=CARTESIAN_POINT('Ctrl Pts',(4.3,3.3773238354,-3.65542016568));
#79814=CARTESIAN_POINT('',(4.3,2.8773238354,-4.15542016568));
#79815=CARTESIAN_POINT('Origin',(4.3,2.8773238354,-3.85542016568));
#79816=CARTESIAN_POINT('Origin',(4.3,2.8773238354,-3.65542016568));
#79817=CARTESIAN_POINT('Origin',(4.3,-3.42065492897,-3.85542016568));
#79818=CARTESIAN_POINT('',(4.3,-8.14391944342,-4.15542016568));
#79819=CARTESIAN_POINT('Origin',(4.3,-8.14391944342,-3.85542016568));
#79820=CARTESIAN_POINT('',(4.3,-2.63329780401,-4.15542016568));
#79821=CARTESIAN_POINT('Origin',(3.7,-9.17423561284,0.47366156039));
#79822=CARTESIAN_POINT('',(3.99616160125331,-8.70088467100253,-3.90297923453123));
#79823=CARTESIAN_POINT('Ctrl Pts',(4.,-8.14391944342,-3.85542016568));
#79824=CARTESIAN_POINT('Ctrl Pts',(4.,-8.22339027599,-3.86461668513));
#79825=CARTESIAN_POINT('Ctrl Pts',(3.99962763899,-8.3031200968,-3.87300735474));
#79826=CARTESIAN_POINT('Ctrl Pts',(3.99902875837,-8.38309753718,-3.88055924261));
#79827=CARTESIAN_POINT('Ctrl Pts',(3.99803977235,-8.49460012163,-3.88985328888));
#79828=CARTESIAN_POINT('Ctrl Pts',(3.99700563085,-8.6064155396,-3.89742302488));
#79829=CARTESIAN_POINT('Ctrl Pts',(3.99671653073,-8.63788417864,-3.89941416203));
#79830=CARTESIAN_POINT('Ctrl Pts',(3.99643383471,-8.66937471516,-3.90126651862));
#79831=CARTESIAN_POINT('Ctrl Pts',(3.99616160126,-8.700884671,-3.90297923457));
#79832=CARTESIAN_POINT('',(3.99951365737889,-8.00613533634358,4.74991748852224));
#79833=CARTESIAN_POINT('Ctrl Pts',(3.99951362599666,-8.00613533213075,4.74991748884671));
#79834=CARTESIAN_POINT('Ctrl Pts',(3.99912970651189,-7.93705421321271,4.72406529283756));
#79835=CARTESIAN_POINT('Ctrl Pts',(3.99857561954119,-7.86817196474413,4.69734499917644));
#79836=CARTESIAN_POINT('Ctrl Pts',(3.9980140143817,-7.79955119479,4.66974300961157));
#79837=CARTESIAN_POINT('Ctrl Pts',(3.99745667146121,-7.73145121442678,4.64235050223209));
#79838=CARTESIAN_POINT('Ctrl Pts',(3.99689185763882,-7.66360880560323,4.6140896699695));
#79839=CARTESIAN_POINT('Ctrl Pts',(3.99642772185445,-7.59608259133466,4.58495963619982));
#79840=CARTESIAN_POINT('Ctrl Pts',(3.99596348780259,-7.52854208031863,4.55582343497737));
#79841=CARTESIAN_POINT('Ctrl Pts',(3.99559997461198,-7.461317947509,4.52581768640237));
#79842=CARTESIAN_POINT('Ctrl Pts',(3.99539475488255,-7.39446554448369,4.49495354860779));
#79843=CARTESIAN_POINT('Ctrl Pts',(3.99518950133484,-7.32760212481346,4.46408432469467));
#79844=CARTESIAN_POINT('Ctrl Pts',(3.9951425932134,-7.26111060723937,4.43235645100427));
#79845=CARTESIAN_POINT('Ctrl Pts',(3.99526097596942,-7.1950423146551,4.39979279428734));
#79846=CARTESIAN_POINT('Ctrl Pts',(3.99538088048154,-7.12812474443087,4.36681054667843));
#79847=CARTESIAN_POINT('Ctrl Pts',(3.99567046299158,-7.06164141244719,4.33297088933084));
#79848=CARTESIAN_POINT('Ctrl Pts',(3.99608398850385,-6.99564062204421,4.29830946415507));
#79849=CARTESIAN_POINT('Ctrl Pts',(3.99649234912136,-6.93046417530672,4.26408095692022));
#79850=CARTESIAN_POINT('Ctrl Pts',(3.9970214669193,-6.86575833052573,4.22905112782395));
#79851=CARTESIAN_POINT('Ctrl Pts',(3.99757632607106,-6.80156401020727,4.19326539858406));
#79852=CARTESIAN_POINT('Ctrl Pts',(3.99814171190807,-6.73615180711144,4.15680074910478));
#79853=CARTESIAN_POINT('Ctrl Pts',(3.99873399116725,-6.67127079573283,4.11955123467727));
#79854=CARTESIAN_POINT('Ctrl Pts',(3.99919856363035,-6.6069575312888,4.08157632337734));
#79855=CARTESIAN_POINT('Ctrl Pts',(3.99966313609345,-6.54264426684478,4.04360141207741));
#79856=CARTESIAN_POINT('Ctrl Pts',(4.,-6.47889880397702,4.00490112886999));
#79857=CARTESIAN_POINT('Ctrl Pts',(4.,-6.41575007864,3.96554608849));
#79858=CARTESIAN_POINT('',(3.99944937669,-8.31076354672,4.82056300746));
#79859=CARTESIAN_POINT('Ctrl Pts',(3.99944937669,-8.31076354672,4.82056300746));
#79860=CARTESIAN_POINT('Ctrl Pts',(3.99959839809,-8.28592729564,4.81813395331));
#79861=CARTESIAN_POINT('Ctrl Pts',(3.99969341422,-8.26106714699,4.8150399126));
#79862=CARTESIAN_POINT('Ctrl Pts',(3.99975395169,-8.23622932864,4.81128563568));
#79863=CARTESIAN_POINT('Ctrl Pts',(3.99984876957,-8.17436353389,4.80027772376));
#79864=CARTESIAN_POINT('Ctrl Pts',(3.99983052524,-8.11319387748,4.78525185918));
#79865=CARTESIAN_POINT('Ctrl Pts',(3.99979379772,-8.07691196013,4.77482737361));
#79866=CARTESIAN_POINT('Ctrl Pts',(3.99970844997,-8.04117830882,4.76303153489));
#79867=CARTESIAN_POINT('Ctrl Pts',(3.99951367307,-8.00613533845,4.74991748836));
#79868=CARTESIAN_POINT('',(3.99616169506664,-8.70088460854749,4.85030293274176));
#79869=CARTESIAN_POINT('Ctrl Pts',(3.99616169511,-8.70088460852,4.850302933));
#79870=CARTESIAN_POINT('Ctrl Pts',(3.99683804383,-8.62256210931,4.84604483372));
#79871=CARTESIAN_POINT('Ctrl Pts',(3.99757933996,-8.54435185028,4.84092376899));
#79872=CARTESIAN_POINT('Ctrl Pts',(3.99832332564,-8.46629167717,4.83495432364));
#79873=CARTESIAN_POINT('Ctrl Pts',(3.99898336569,-8.38842527481,4.8281587616));
#79874=CARTESIAN_POINT('Ctrl Pts',(3.99944937669,-8.31076354672,4.82056300746));
#79875=CARTESIAN_POINT('',(3.7,-8.7279990537,4.59960059693));
#79876=CARTESIAN_POINT('Origin',(3.7,-8.69574098918,4.89786125018));
#79877=CARTESIAN_POINT('',(3.7,-8.7279990537,-3.65227747616));
#79878=CARTESIAN_POINT('Origin',(3.7,-9.17423561284,0.47366156039));
#79879=CARTESIAN_POINT('Origin',(3.7,-8.69574098918,-3.9505381294));
#79880=CARTESIAN_POINT('Origin',(0.,-2.35608968258,2.34387696505));
#79881=CARTESIAN_POINT('',(4.35,-2.56170009476,2.4428735547));
#79882=CARTESIAN_POINT('',(4.35,-7.88049121843,5.00374669681));
#79883=CARTESIAN_POINT('',(4.35,2.08731990915,0.204479493281));
#79884=CARTESIAN_POINT('',(4.2990272509,-7.88049121843,5.00374669681));
#79885=CARTESIAN_POINT('',(3.225,-7.88049121843,5.00374669681));
#79886=CARTESIAN_POINT('Ctrl Pts',(4.2990272509,-7.88049121843,5.00374669681));
#79887=CARTESIAN_POINT('Ctrl Pts',(4.29860194904898,-7.84336279989873,4.98587023435574));
#79888=CARTESIAN_POINT('Ctrl Pts',(4.29807036319667,-7.8063193049477,4.96803466061349));
#79889=CARTESIAN_POINT('Ctrl Pts',(4.29749123915026,-7.76934684031188,4.95023328629991));
#79890=CARTESIAN_POINT('Ctrl Pts',(4.29661357039136,-7.71331467008551,4.92325511090297));
#79891=CARTESIAN_POINT('Ctrl Pts',(4.29562842420427,-7.65745144851057,4.89635828031341));
#79892=CARTESIAN_POINT('Ctrl Pts',(4.29470009048654,-7.60171026056881,4.86952020595908));
#79893=CARTESIAN_POINT('Ctrl Pts',(4.29377028407366,-7.54588064561534,4.84263955607304));
#79894=CARTESIAN_POINT('Ctrl Pts',(4.29289746676361,-7.49017341724383,4.8158178323467));
#79895=CARTESIAN_POINT('Ctrl Pts',(4.29219442747521,-7.43454058879187,4.78903193034465));
#79896=CARTESIAN_POINT('Ctrl Pts',(4.29149095408814,-7.3788734092915,4.76222948911851));
#79897=CARTESIAN_POINT('Ctrl Pts',(4.29095746147181,-7.32328068911448,4.73546289822188));
#79898=CARTESIAN_POINT('Ctrl Pts',(4.29065473399492,-7.26771400724003,4.7087088442481));
#79899=CARTESIAN_POINT('Ctrl Pts',(4.29035187162506,-7.21212256529347,4.68194286888037));
#79900=CARTESIAN_POINT('Ctrl Pts',(4.29027997715909,-7.15655715410882,4.65518942682211));
#79901=CARTESIAN_POINT('Ctrl Pts',(4.29044774917812,-7.10096941674446,4.6284252355263));
#79902=CARTESIAN_POINT('Ctrl Pts',(4.29052775589753,-7.07446086941765,4.61566199195374));
#79903=CARTESIAN_POINT('Ctrl Pts',(4.29066150240974,-7.04794724961644,4.6028963061693));
#79904=CARTESIAN_POINT('Ctrl Pts',(4.29084575810665,-7.02142335390664,4.59012567283795));
#79905=CARTESIAN_POINT('Ctrl Pts',(4.29123152417027,-6.96589172578971,4.56338849709526));
#79906=CARTESIAN_POINT('Ctrl Pts',(4.29184075891047,-6.91031984610482,4.53663194126546));
#79907=CARTESIAN_POINT('Ctrl Pts',(4.29260245682323,-6.85466578564437,4.50983581716746));
#79908=CARTESIAN_POINT('Ctrl Pts',(4.29336407793749,-6.79901733652759,4.48304239479976));
#79909=CARTESIAN_POINT('Ctrl Pts',(4.29427813122767,-6.74328668363906,4.45620939309286));
#79910=CARTESIAN_POINT('Ctrl Pts',(4.29522152510374,-6.68743327543012,4.42931728747705));
#79911=CARTESIAN_POINT('Ctrl Pts',(4.29540155763234,-6.67677449274567,4.42418533369164));
#79912=CARTESIAN_POINT('Ctrl Pts',(4.29558250634003,-6.66611124458006,4.41905122987873));
#79913=CARTESIAN_POINT('Ctrl Pts',(4.29576330024143,-6.65544325666937,4.41391484398757));
#79914=CARTESIAN_POINT('Ctrl Pts',(4.29671133096125,-6.59950342584761,4.38698112788367));
#79915=CARTESIAN_POINT('Ctrl Pts',(4.29766075533132,-6.54342366948845,4.35998004088301));
#79916=CARTESIAN_POINT('Ctrl Pts',(4.29842842934662,-6.48716607127935,4.33289332720474));
#79917=CARTESIAN_POINT('Ctrl Pts',(4.29919717698267,-6.43082979472131,4.30576873174731));
#79918=CARTESIAN_POINT('Ctrl Pts',(4.29978365749905,-6.37431514200558,4.27855825235265));
#79919=CARTESIAN_POINT('Ctrl Pts',(4.29995176543971,-6.31758659819914,4.25124478941713));
#79920=CARTESIAN_POINT('Ctrl Pts',(4.29998333258852,-6.30693416633443,4.24611589339078));
#79921=CARTESIAN_POINT('Ctrl Pts',(4.3,-6.29627420060992,4.24098336998769));
#79922=CARTESIAN_POINT('Ctrl Pts',(4.3,-6.28560647753,4.2358471116));
#79923=CARTESIAN_POINT('',(4.225,-2.56170009476,2.4428735547));
#79924=CARTESIAN_POINT('Ctrl Pts',(4.2990272509,-7.88049121843,5.00374669681));
#79925=CARTESIAN_POINT('Ctrl Pts',(4.20814466399,-7.88133645067,5.00415365756));
#79926=CARTESIAN_POINT('Ctrl Pts',(4.11726207707,-7.8971129981,4.97354910689));
#79927=CARTESIAN_POINT('Ctrl Pts',(4.04405123536,-7.92782451085,4.91150498201));
#79928=CARTESIAN_POINT('Ctrl Pts',(4.00460089543,-7.96672185122,4.83165605064));
#79929=CARTESIAN_POINT('Ctrl Pts',(3.99951361632,-8.0061354071,4.74991733337));
#79930=CARTESIAN_POINT('Ctrl Pts',(4.29534152276,-7.55873090479,4.8488266546));
#79931=CARTESIAN_POINT('Ctrl Pts',(4.21089110293,-7.56075677108,4.84980205594));
#79932=CARTESIAN_POINT('Ctrl Pts',(4.12644068311,-7.57560508753,4.82414594128));
#79933=CARTESIAN_POINT('Ctrl Pts',(4.05583695285,-7.60300935451,4.77146524893));
#79934=CARTESIAN_POINT('Ctrl Pts',(4.01210473647,-7.6379921895,4.70122601239));
#79935=CARTESIAN_POINT('Ctrl Pts',(3.99767078695,-7.67454601586,4.62582683568));
#79936=CARTESIAN_POINT('Ctrl Pts',(4.28495419985,-7.24223776902,4.69644263496));
#79937=CARTESIAN_POINT('Ctrl Pts',(4.20364197507,-7.24265108624,4.69664162775));
#79938=CARTESIAN_POINT('Ctrl Pts',(4.12232975028,-7.25504442659,4.67195877864));
#79939=CARTESIAN_POINT('Ctrl Pts',(4.05372035815,-7.27955010958,4.62221233106));
#79940=CARTESIAN_POINT('Ctrl Pts',(4.00967965098,-7.31194178404,4.55622127864));
#79941=CARTESIAN_POINT('Ctrl Pts',(3.99247722227,-7.34677145748,4.48508959035));
#79942=CARTESIAN_POINT('Ctrl Pts',(4.28719359971,-6.92729615453,4.54480563642));
#79943=CARTESIAN_POINT('Ctrl Pts',(4.20516486744,-6.92619358841,4.54427477668));
#79944=CARTESIAN_POINT('Ctrl Pts',(4.12313613516,-6.93728087775,4.51842626492));
#79945=CARTESIAN_POINT('Ctrl Pts',(4.05411385932,-6.96067605503,4.46706057541));
#79946=CARTESIAN_POINT('Ctrl Pts',(4.01020087277,-6.99204699421,4.39931666036));
#79947=CARTESIAN_POINT('Ctrl Pts',(3.99359726714,-7.02607103842,4.32667666396));
#79948=CARTESIAN_POINT('Ctrl Pts',(4.3,-6.60947733541,4.39178333134));
#79949=CARTESIAN_POINT('Ctrl Pts',(4.21340350799,-6.60705721212,4.39061809876));
#79950=CARTESIAN_POINT('Ctrl Pts',(4.12680701597,-6.61808600203,4.3615202213));
#79951=CARTESIAN_POINT('Ctrl Pts',(4.0550389398,-6.64318599408,4.30449502667));
#79952=CARTESIAN_POINT('Ctrl Pts',(4.01201861445,-6.67775474512,4.23026617343));
#79953=CARTESIAN_POINT('Ctrl Pts',(4.,-6.71532134284,4.1522424388));
#79954=CARTESIAN_POINT('Ctrl Pts',(4.3,-6.28560647753,4.2358471116));
#79955=CARTESIAN_POINT('Ctrl Pts',(4.20575222039,-6.28560647753,4.2358471116));
#79956=CARTESIAN_POINT('Ctrl Pts',(4.11150444078,-6.30166230076,4.20250005951));
#79957=CARTESIAN_POINT('Ctrl Pts',(4.0370110165,-6.33397844241,4.13538123018));
#79958=CARTESIAN_POINT('Ctrl Pts',(4.,-6.37486426052,4.05046365934));
#79959=CARTESIAN_POINT('Ctrl Pts',(4.,-6.41575007864,3.96554608849));
#79960=CARTESIAN_POINT('Origin',(4.29708331441242,-8.00976085385706,4.7353069832235));
#79961=CARTESIAN_POINT('Origin',(4.225,-2.12788809108,3.34387696505));
#79962=CARTESIAN_POINT('',(4.35,-2.12788809108,2.34387696505));
#79963=CARTESIAN_POINT('',(4.325,-2.12788809108,2.34387696505));
#79964=CARTESIAN_POINT('Origin',(4.35,-2.12788809108,3.34387696505));
#79965=CARTESIAN_POINT('Origin',(0.,3.3773238354,2.34387696505));
#79966=CARTESIAN_POINT('',(4.35,2.8773238354,2.34387696505));
#79967=CARTESIAN_POINT('',(4.35,-1.95899712601,2.34387696505));
#79968=CARTESIAN_POINT('',(4.225,2.8773238354,2.34387696505));
#79969=CARTESIAN_POINT('Origin',(4.225,2.8773238354,1.84387696505));
#79970=CARTESIAN_POINT('',(4.35,3.3773238354,1.84387696505));
#79971=CARTESIAN_POINT('Origin',(4.35,2.8773238354,1.84387696505));
#79972=CARTESIAN_POINT('',(4.325,3.3773238354,1.84387696505));
#79973=CARTESIAN_POINT('Origin',(0.,3.3773238354,-4.15542016568));
#79974=CARTESIAN_POINT('',(4.35,3.3773238354,-3.65542016568));
#79975=CARTESIAN_POINT('',(4.35,3.3773238354,0.294579834316));
#79976=CARTESIAN_POINT('',(3.225,3.3773238354,-3.65542016568));
#79977=CARTESIAN_POINT('Origin',(3.225,2.8773238354,-3.65542016568));
#79978=CARTESIAN_POINT('',(4.35,2.8773238354,-4.15542016568));
#79979=CARTESIAN_POINT('Origin',(4.35,2.8773238354,-3.65542016568));
#79980=CARTESIAN_POINT('',(4.325,2.8773238354,-4.15542016568));
#79981=CARTESIAN_POINT('Ctrl Pts',(4.29232316291,-8.70602833393,-4.15542016568));
#79982=CARTESIAN_POINT('Ctrl Pts',(4.20764023978,-8.70455758206,-4.15542016896));
#79983=CARTESIAN_POINT('Ctrl Pts',(4.12295731665,-8.70308683019,-4.12553116451));
#79984=CARTESIAN_POINT('Ctrl Pts',(4.05251768323,-8.70186345223,-4.06549009434));
#79985=CARTESIAN_POINT('Ctrl Pts',(4.00958634297,-8.70111783143,-3.98660373227));
#79986=CARTESIAN_POINT('Ctrl Pts',(3.99616158804,-8.70088467363,-3.90297907486));
#79987=CARTESIAN_POINT('Ctrl Pts',(4.2942593567,-8.59454665965,-4.15542016568));
#79988=CARTESIAN_POINT('Ctrl Pts',(4.20834579354,-8.59289747109,-4.15542016627));
#79989=CARTESIAN_POINT('Ctrl Pts',(4.12243223039,-8.59124828254,-4.12466052278));
#79990=CARTESIAN_POINT('Ctrl Pts',(4.05139392587,-8.58988386074,-4.06285702325));
#79991=CARTESIAN_POINT('Ctrl Pts',(4.00903053768,-8.58906847866,-3.98200796497));
#79992=CARTESIAN_POINT('Ctrl Pts',(3.99712968313,-8.58883688841,-3.89688931333));
#79993=CARTESIAN_POINT('Ctrl Pts',(4.29645983294,-8.48273103918,-4.15542016568));
#79994=CARTESIAN_POINT('Ctrl Pts',(4.20896023779,-8.48105918371,-4.15542015758));
#79995=CARTESIAN_POINT('Ctrl Pts',(4.12146064264,-8.47938732823,-4.12352488429));
#79996=CARTESIAN_POINT('Ctrl Pts',(4.04967388507,-8.47801593608,-4.05942126033));
#79997=CARTESIAN_POINT('Ctrl Pts',(4.00810176319,-8.47722229641,-3.97603783242));
#79998=CARTESIAN_POINT('Ctrl Pts',(3.99822990786,-8.47703468918,-3.88903180855));
#79999=CARTESIAN_POINT('Ctrl Pts',(4.29855844641,-8.37042692805,-4.15542016568));
#80000=CARTESIAN_POINT('Ctrl Pts',(4.20912872342,-8.36895891499,-4.15542016568));
#80001=CARTESIAN_POINT('Ctrl Pts',(4.11969900043,-8.36749090194,-4.12211547602));
#80002=CARTESIAN_POINT('Ctrl Pts',(4.04704750378,-8.36630239191,-4.05515458588));
#80003=CARTESIAN_POINT('Ctrl Pts',(4.00655550671,-8.36564940222,-3.96867720994));
#80004=CARTESIAN_POINT('Ctrl Pts',(3.99927927276,-8.3655474023,-3.87944960348));
#80005=CARTESIAN_POINT('Ctrl Pts',(4.3,-8.25752787941,-4.15542016568));
#80006=CARTESIAN_POINT('Ctrl Pts',(4.20831114128,-8.25657123296,-4.15542016568));
#80007=CARTESIAN_POINT('Ctrl Pts',(4.11662228256,-8.2556145865,-4.12041892129));
#80008=CARTESIAN_POINT('Ctrl Pts',(4.04304033238,-8.25485845437,-4.05001401514));
#80009=CARTESIAN_POINT('Ctrl Pts',(4.00401954353,-8.25448277917,-3.95990362884));
#80010=CARTESIAN_POINT('Ctrl Pts',(4.,-8.25448277917,-3.86821477012));
#80011=CARTESIAN_POINT('Ctrl Pts',(4.3,-8.14391944342,-4.15542016568));
#80012=CARTESIAN_POINT('Ctrl Pts',(4.20575222039,-8.14391944342,-4.15542016568));
#80013=CARTESIAN_POINT('Ctrl Pts',(4.11150444078,-8.14391944342,-4.11840914918));
#80014=CARTESIAN_POINT('Ctrl Pts',(4.0370110165,-8.14391944342,-4.0439157249));
#80015=CARTESIAN_POINT('Ctrl Pts',(4.,-8.14391944342,-3.94966794529));
#80016=CARTESIAN_POINT('Ctrl Pts',(4.,-8.14391944342,-3.85542016568));
#80017=CARTESIAN_POINT('',(4.29232316258844,-8.70602835244453,-4.15542016568));
#80018=CARTESIAN_POINT('Origin',(4.29069091406768,-8.70599998041311,-3.85733575579212));
#80019=CARTESIAN_POINT('Ctrl Pts',(4.3,-8.14391944342,-4.15542016568));
#80020=CARTESIAN_POINT('Ctrl Pts',(4.3,-8.20648904053108,-4.15542016568));
#80021=CARTESIAN_POINT('Ctrl Pts',(4.29947971883186,-8.26880371250586,-4.15542016568));
#80022=CARTESIAN_POINT('Ctrl Pts',(4.29869536600186,-8.33090046659907,-4.15542016568));
#80023=CARTESIAN_POINT('Ctrl Pts',(4.29790074267177,-8.39381033016885,-4.15542016568));
#80024=CARTESIAN_POINT('Ctrl Pts',(4.29683500095811,-8.45649622088276,-4.15542016568));
#80025=CARTESIAN_POINT('Ctrl Pts',(4.29571075913684,-8.51899937638185,-4.15542016568));
#80026=CARTESIAN_POINT('Ctrl Pts',(4.29458651731557,-8.58150253188095,-4.15542016568));
#80027=CARTESIAN_POINT('Ctrl Pts',(4.2934034804918,-8.64382608258768,-4.15542016568));
#80028=CARTESIAN_POINT('Ctrl Pts',(4.29232316291,-8.70602833393,-4.15542016568));
#80029=CARTESIAN_POINT('Origin',(0.,3.3773238354,-4.15542016568));
#80030=CARTESIAN_POINT('',(3.69999999774,-9.41827086749,-4.15542016568));
#80031=CARTESIAN_POINT('Ctrl Pts',(4.29232316225885,-8.70602837142191,-4.15542016568));
#80032=CARTESIAN_POINT('Ctrl Pts',(4.29205120071452,-8.72168753702626,-4.15542016568));
#80033=CARTESIAN_POINT('Ctrl Pts',(4.29158720532918,-8.73740648674787,-4.15542016568278));
#80034=CARTESIAN_POINT('Ctrl Pts',(4.29086254081513,-8.75324772180714,-4.15542016514087));
#80035=CARTESIAN_POINT('Ctrl Pts',(4.29008645301039,-8.77021307488149,-4.15542016456051));
#80036=CARTESIAN_POINT('Ctrl Pts',(4.28901119399487,-8.7873184421748,-4.15542016334628));
#80037=CARTESIAN_POINT('Ctrl Pts',(4.28754966268177,-8.80457940448153,-4.15542016341833));
#80038=CARTESIAN_POINT('Ctrl Pts',(4.28677487233489,-8.81372982558667,-4.15542016345652));
#80039=CARTESIAN_POINT('Ctrl Pts',(4.28589150051295,-8.8229229964194,-4.15542016392521));
#80040=CARTESIAN_POINT('Ctrl Pts',(4.28488660862881,-8.83215545542406,-4.15542016457497));
#80041=CARTESIAN_POINT('Ctrl Pts',(4.28275134959082,-8.85177317932411,-4.15542016595563));
#80042=CARTESIAN_POINT('Ctrl Pts',(4.28003832504559,-8.87155237324264,-4.15542016566606));
#80043=CARTESIAN_POINT('Ctrl Pts',(4.27662963897357,-8.89139030340002,-4.15542016567672));
#80044=CARTESIAN_POINT('Ctrl Pts',(4.27453046995187,-8.90360708357898,-4.15542016568329));
#80045=CARTESIAN_POINT('Ctrl Pts',(4.27216774709283,-8.91584486940965,-4.15542016568));
#80046=CARTESIAN_POINT('Ctrl Pts',(4.26951780859382,-8.92807096217797,-4.15542016568));
#80047=CARTESIAN_POINT('Ctrl Pts',(4.26468368982784,-8.95037426638974,-4.15542016568));
#80048=CARTESIAN_POINT('Ctrl Pts',(4.25889294909336,-8.97263030125832,-4.15542016568));
#80049=CARTESIAN_POINT('Ctrl Pts',(4.25202546552033,-8.99462871319934,-4.15542016568));
#80050=CARTESIAN_POINT('Ctrl Pts',(4.24866331428397,-9.00539859522655,-4.15542016568));
#80051=CARTESIAN_POINT('Ctrl Pts',(4.24504378092221,-9.01610634900063,-4.15542016568));
#80052=CARTESIAN_POINT('Ctrl Pts',(4.24115737109246,-9.02672676812152,-4.15542016568));
#80053=CARTESIAN_POINT('Ctrl Pts',(4.23426685680616,-9.04555652434511,-4.15542016568));
#80054=CARTESIAN_POINT('Ctrl Pts',(4.22653159494977,-9.06411864425602,-4.15542016568));
#80055=CARTESIAN_POINT('Ctrl Pts',(4.21793147778923,-9.08227287068491,-4.15542016568));
#80056=CARTESIAN_POINT('Ctrl Pts',(4.2100789353958,-9.0988490207526,-4.15542016568));
#80057=CARTESIAN_POINT('Ctrl Pts',(4.2015054941613,-9.11508438284678,-4.15542016568));
#80058=CARTESIAN_POINT('Ctrl Pts',(4.1922309596074,-9.13089839049763,-4.15542016568));
#80059=CARTESIAN_POINT('Ctrl Pts',(4.18815592541805,-9.13784673075918,-4.15542016568));
#80060=CARTESIAN_POINT('Ctrl Pts',(4.1839460127474,-9.14471414658231,-4.15542016568));
#80061=CARTESIAN_POINT('Ctrl Pts',(4.17960523291625,-9.1514961102524,-4.15542016568));
#80062=CARTESIAN_POINT('Ctrl Pts',(4.16634611145727,-9.17221194554702,-4.15542016568));
#80063=CARTESIAN_POINT('Ctrl Pts',(4.15184518108592,-9.19211860151861,-4.15542016617984));
#80064=CARTESIAN_POINT('Ctrl Pts',(4.13618163257724,-9.21102766582222,-4.15542016179659));
#80065=CARTESIAN_POINT('Ctrl Pts',(4.11973553103685,-9.23088142957176,-4.15542015719435));
#80066=CARTESIAN_POINT('Ctrl Pts',(4.10200809428551,-9.24963529413492,-4.15542014577611));
#80067=CARTESIAN_POINT('Ctrl Pts',(4.08313350202983,-9.26711150454399,-4.15542013374396));
#80068=CARTESIAN_POINT('Ctrl Pts',(4.07176321009623,-9.27763939365293,-4.15542012649563));
#80069=CARTESIAN_POINT('Ctrl Pts',(4.05997740445791,-9.28770440729055,-4.15542011955517));
#80070=CARTESIAN_POINT('Ctrl Pts',(4.04781138042469,-9.29727441845877,-4.15542011643421));
#80071=CARTESIAN_POINT('Ctrl Pts',(4.02659799740219,-9.31396124333162,-4.15542011099231));
#80072=CARTESIAN_POINT('Ctrl Pts',(4.00423092936188,-9.32913206089668,-4.15542011535558));
#80073=CARTESIAN_POINT('Ctrl Pts',(3.98091614962384,-9.34262747027809,-4.15542012343284));
#80074=CARTESIAN_POINT('Ctrl Pts',(3.95650110095926,-9.3567597537694,-4.15542013189127));
#80075=CARTESIAN_POINT('Ctrl Pts',(3.93104736555546,-9.36905451674416,-4.15542014341187));
#80076=CARTESIAN_POINT('Ctrl Pts',(3.90483049009711,-9.37937035892166,-4.15542015118524));
#80077=CARTESIAN_POINT('Ctrl Pts',(3.89672696602562,-9.38255894161665,-4.15542015358796));
#80078=CARTESIAN_POINT('Ctrl Pts',(3.88855076480426,-9.38555876112294,-4.15542015568561));
#80079=CARTESIAN_POINT('Ctrl Pts',(3.88031058139973,-9.38836645220462,-4.1554201574361));
#80080=CARTESIAN_POINT('Ctrl Pts',(3.85132370712238,-9.39824319698063,-4.15542016359385));
#80081=CARTESIAN_POINT('Ctrl Pts',(3.82154088715569,-9.40573335220575,-4.15542016471136));
#80082=CARTESIAN_POINT('Ctrl Pts',(3.79135695696281,-9.41074020445555,-4.15542016528016));
#80083=CARTESIAN_POINT('Ctrl Pts',(3.76117302676992,-9.41574705670534,-4.15542016584896));
#80084=CARTESIAN_POINT('Ctrl Pts',(3.73058948857333,-9.41827087355667,-4.15542016568));
#80085=CARTESIAN_POINT('Ctrl Pts',(3.69999999774,-9.41827086749,-4.15542016568));
#80086=CARTESIAN_POINT('',(2.3,-9.41827086707,-4.15542016568));
#80087=CARTESIAN_POINT('',(3.225,-9.41827086707,-4.15542016568));
#80088=CARTESIAN_POINT('',(2.3,-10.0779006799,-4.15542016568));
#80089=CARTESIAN_POINT('',(2.3,-8.20939783898,-4.15542016568));
#80090=CARTESIAN_POINT('',(4.35,-10.0779006799,-4.15542016568));
#80091=CARTESIAN_POINT('',(3.225,-10.0779006799,-4.15542016568));
#80092=CARTESIAN_POINT('',(4.35,-1.95899712601,-4.15542016568));
#80093=CARTESIAN_POINT('Ctrl Pts',(4.29232279844,-8.70602816471,5.10274328646));
#80094=CARTESIAN_POINT('Ctrl Pts',(4.20763985549,-8.70455745139,5.10274332142));
#80095=CARTESIAN_POINT('Ctrl Pts',(4.12295691253,-8.70308673807,5.07285428042));
#80096=CARTESIAN_POINT('Ctrl Pts',(4.05251729593,-8.70186339274,5.01281309848));
#80097=CARTESIAN_POINT('Ctrl Pts',(4.00958603902,-8.70111779311,4.93392659864));
#80098=CARTESIAN_POINT('Ctrl Pts',(3.99616141568,-8.70088464377,4.85030182916));
#80099=CARTESIAN_POINT('Ctrl Pts',(4.29367604164,-8.62810126572,5.10274328646));
#80100=CARTESIAN_POINT('Ctrl Pts',(4.20813285855,-8.6265058463,5.10274333195));
#80101=CARTESIAN_POINT('Ctrl Pts',(4.12258967546,-8.62491042687,5.07224568401));
#80102=CARTESIAN_POINT('Ctrl Pts',(4.0517315901,-8.62358850977,5.01097248773));
#80103=CARTESIAN_POINT('Ctrl Pts',(4.00919737959,-8.62279415849,4.93071397417));
#80104=CARTESIAN_POINT('Ctrl Pts',(3.99683804383,-8.62256210931,4.84604483372));
#80105=CARTESIAN_POINT('Ctrl Pts',(4.29515862692,-8.55000353482,5.10274328646));
#80106=CARTESIAN_POINT('Ctrl Pts',(4.20858147867,-8.54835950303,5.10274332811));
#80107=CARTESIAN_POINT('Ctrl Pts',(4.12200433041,-8.54671547124,5.07150754218));
#80108=CARTESIAN_POINT('Ctrl Pts',(4.05065454881,-8.5453604781,5.00873951265));
#80109=CARTESIAN_POINT('Ctrl Pts',(4.0086265191,-8.54456207669,4.92682955987));
#80110=CARTESIAN_POINT('Ctrl Pts',(3.99757933996,-8.54435185028,4.84092376899));
#80111=CARTESIAN_POINT('Ctrl Pts',(4.2966466112,-8.47169636018,5.10274328646));
#80112=CARTESIAN_POINT('Ctrl Pts',(4.20886559395,-8.47010372313,5.10274328646));
#80113=CARTESIAN_POINT('Ctrl Pts',(4.12108457671,-8.46851108607,5.0706369892));
#80114=CARTESIAN_POINT('Ctrl Pts',(4.049181176,-8.4672075164,5.00610503411));
#80115=CARTESIAN_POINT('Ctrl Pts',(4.00779063879,-8.46645935943,4.92226864646));
#80116=CARTESIAN_POINT('Ctrl Pts',(3.99832332564,-8.46629167717,4.83495432364));
#80117=CARTESIAN_POINT('Ctrl Pts',(4.29796673138,-8.39314927373,5.10274328646));
#80118=CARTESIAN_POINT('Ctrl Pts',(4.20881731963,-8.39173518355,5.10274328646));
#80119=CARTESIAN_POINT('Ctrl Pts',(4.11966790787,-8.39032109337,5.06963007213));
#80120=CARTESIAN_POINT('Ctrl Pts',(4.04716501903,-8.3891735059,5.00305604873));
#80121=CARTESIAN_POINT('Ctrl Pts',(4.00657458492,-8.38853640885,4.91702461127));
#80122=CARTESIAN_POINT('Ctrl Pts',(3.99898336569,-8.38842527481,4.8281587616));
#80123=CARTESIAN_POINT('Ctrl Pts',(4.29889875178,-8.31430322211,5.10274328646));
#80124=CARTESIAN_POINT('Ctrl Pts',(4.20822334583,-8.31323136973,5.10274328646));
#80125=CARTESIAN_POINT('Ctrl Pts',(4.11754793987,-8.31215951735,5.06848004433));
#80126=CARTESIAN_POINT('Ctrl Pts',(4.04442178691,-8.31129511051,4.99957103487));
#80127=CARTESIAN_POINT('Ctrl Pts',(4.00483540394,-8.3108271693,4.91108461112));
#80128=CARTESIAN_POINT('Ctrl Pts',(3.99944937589,-8.31076350235,4.82056298519));
#80129=CARTESIAN_POINT('',(4.29889875895,-8.31430322211008,5.10274332057));
#80130=CARTESIAN_POINT('Origin',(4.29696586920653,-8.31428039305215,4.80479476356497));
#80131=CARTESIAN_POINT('',(4.29232279670749,-8.70602826446416,5.10274328645992));
#80132=CARTESIAN_POINT('Ctrl Pts',(4.29232279844,-8.70602816471,5.10274328646));
#80133=CARTESIAN_POINT('Ctrl Pts',(4.29367604164,-8.62810126572,5.10274328646));
#80134=CARTESIAN_POINT('Ctrl Pts',(4.29515862692,-8.55000353482,5.10274328646));
#80135=CARTESIAN_POINT('Ctrl Pts',(4.2966466112,-8.47169636018,5.10274328646));
#80136=CARTESIAN_POINT('Ctrl Pts',(4.29796673138,-8.39314927373,5.10274328646));
#80137=CARTESIAN_POINT('Ctrl Pts',(4.29889875178,-8.31430322211,5.10274328646));
#80138=CARTESIAN_POINT('Origin',(4.29068847369796,-8.70599943725965,4.80466191947753));
#80139=CARTESIAN_POINT('Ctrl Pts',(4.29889876134,-8.31430322282,5.1027434229));
#80140=CARTESIAN_POINT('Ctrl Pts',(4.2082233452,-8.31323138881,5.10274342246));
#80141=CARTESIAN_POINT('Ctrl Pts',(4.11754792907,-8.31215955225,5.0684801702));
#80142=CARTESIAN_POINT('Ctrl Pts',(4.04442177042,-8.31129515513,4.99957114081));
#80143=CARTESIAN_POINT('Ctrl Pts',(4.00483538997,-8.31082721545,4.91108469399));
#80144=CARTESIAN_POINT('Ctrl Pts',(3.99944937087,-8.31076354298,4.8205630482));
#80145=CARTESIAN_POINT('Ctrl Pts',(4.29964314059,-8.22434260602,5.1027436292));
#80146=CARTESIAN_POINT('Ctrl Pts',(4.20780699632,-8.22403023518,5.10264720521));
#80147=CARTESIAN_POINT('Ctrl Pts',(4.11597085206,-8.22680019636,5.06741723002));
#80148=CARTESIAN_POINT('Ctrl Pts',(4.0423682592,-8.23275280902,4.99666339283));
#80149=CARTESIAN_POINT('Ctrl Pts',(4.00353912359,-8.24059165767,4.90627699718));
#80150=CARTESIAN_POINT('Ctrl Pts',(3.99982155439,-8.24873700866,4.81449657867));
#80151=CARTESIAN_POINT('Ctrl Pts',(4.29971371834,-8.13469356333,5.09262744205));
#80152=CARTESIAN_POINT('Ctrl Pts',(4.20724144925,-8.13466365636,5.09260573663));
#80153=CARTESIAN_POINT('Ctrl Pts',(4.11476918016,-8.14098347585,5.05729879766));
#80154=CARTESIAN_POINT('Ctrl Pts',(4.04093270982,-8.15373242653,4.98629044613));
#80155=CARTESIAN_POINT('Ctrl Pts',(4.00258694952,-8.1700271987,4.89579754059));
#80156=CARTESIAN_POINT('Ctrl Pts',(3.99985686503,-8.18656139935,4.80428277208));
#80157=CARTESIAN_POINT('Ctrl Pts',(4.29971786827,-8.04665414995,5.07253279403));
#80158=CARTESIAN_POINT('Ctrl Pts',(4.20720101416,-8.04666571693,5.07252348963));
#80159=CARTESIAN_POINT('Ctrl Pts',(4.11468416006,-8.05626571803,5.0379315222));
#80160=CARTESIAN_POINT('Ctrl Pts',(4.04083150668,-8.07556834767,4.96834669024));
#80161=CARTESIAN_POINT('Ctrl Pts',(4.00251997495,-8.10013935979,4.87966809703));
#80162=CARTESIAN_POINT('Ctrl Pts',(3.9998589855,-8.12494698597,4.78999433407));
#80163=CARTESIAN_POINT('Ctrl Pts',(4.29967705707,-7.96150927709,5.0427549913));
#80164=CARTESIAN_POINT('Ctrl Pts',(4.20771171282,-7.96176972051,5.0427867655));
#80165=CARTESIAN_POINT('Ctrl Pts',(4.11574636857,-7.97452633141,5.00973042736));
#80166=CARTESIAN_POINT('Ctrl Pts',(4.04209470673,-7.99987188278,4.94319135382));
#80167=CARTESIAN_POINT('Ctrl Pts',(4.00335979512,-8.03206135592,4.85814590158));
#80168=CARTESIAN_POINT('Ctrl Pts',(3.99983852853,-8.06458049923,4.77178934946));
#80169=CARTESIAN_POINT('Ctrl Pts',(4.29902733552,-7.88049121843,5.00374669681));
#80170=CARTESIAN_POINT('Ctrl Pts',(4.20814475196,-7.88133646016,5.00415366088));
#80171=CARTESIAN_POINT('Ctrl Pts',(4.1172621684,-7.89711301226,4.97354912353));
#80172=CARTESIAN_POINT('Ctrl Pts',(4.04405132352,-7.92782452293,4.91150502168));
#80173=CARTESIAN_POINT('Ctrl Pts',(4.00460096887,-7.96672185729,4.83165611315));
#80174=CARTESIAN_POINT('Ctrl Pts',(3.99951366776,-8.00613540701,4.74991741048));
#80175=CARTESIAN_POINT('Ctrl Pts',(4.29889876134,-8.31430322211031,5.1027434229));
#80176=CARTESIAN_POINT('Ctrl Pts',(4.29920344163676,-8.27748162914417,5.10274350731409));
#80177=CARTESIAN_POINT('Ctrl Pts',(4.29937856313619,-8.24035941587499,5.10070757013621));
#80178=CARTESIAN_POINT('Ctrl Pts',(4.29948883773587,-8.2031747831764,5.09654944157962));
#80179=CARTESIAN_POINT('Ctrl Pts',(4.29959662290323,-8.16682958790246,5.09248518214244));
#80180=CARTESIAN_POINT('Ctrl Pts',(4.29964284554375,-8.13042504980527,5.08639342033935));
#80181=CARTESIAN_POINT('Ctrl Pts',(4.29965086041858,-8.09420012940637,5.0782197064064));
#80182=CARTESIAN_POINT('Ctrl Pts',(4.29965889627944,-8.05788035824006,5.07002459054819));
#80183=CARTESIAN_POINT('Ctrl Pts',(4.29962900470861,-8.02174138997864,5.05973647485076));
#80184=CARTESIAN_POINT('Ctrl Pts',(4.2995403127252,-7.98603700409252,5.04732841046897));
#80185=CARTESIAN_POINT('Ctrl Pts',(4.2994516207418,-7.9503326182064,5.03492034608718));
#80186=CARTESIAN_POINT('Ctrl Pts',(4.29930451946122,-7.91506308836291,5.02039224105907));
#80187=CARTESIAN_POINT('Ctrl Pts',(4.29902725090631,-7.88049121921695,5.00374669718888));
#80188=CARTESIAN_POINT('Ctrl Pts',(3.7,-9.1392576487296,4.91297769122882));
#80189=CARTESIAN_POINT('Ctrl Pts',(3.7,-9.0282774958267,4.63207689326605));
#80190=CARTESIAN_POINT('Ctrl Pts',(3.7,-8.72799905369119,4.59960059693865));
#80191=CARTESIAN_POINT('Ctrl Pts',(3.95543243199934,-9.1392576487296,4.91297769122882));
#80192=CARTESIAN_POINT('Ctrl Pts',(3.95543243199934,-9.0282774958267,4.63207689326605));
#80193=CARTESIAN_POINT('Ctrl Pts',(3.95543243199934,-8.72799905369119,4.59960059693865));
#80194=CARTESIAN_POINT('Ctrl Pts',(3.99616169510398,-8.90473369905756,5.00563497089039));
#80195=CARTESIAN_POINT('Ctrl Pts',(3.99616169510398,-8.84972402020801,4.86640050166025));
#80196=CARTESIAN_POINT('Ctrl Pts',(3.99616169510398,-8.70088460851816,4.85030293300078));
#80197=CARTESIAN_POINT('',(3.7,-9.13925764671,4.9129776861));
#80198=CARTESIAN_POINT('Origin',(3.7,-8.67423561284,5.09670168568));
#80199=CARTESIAN_POINT('Ctrl Pts',(3.7,-9.13925764671,4.9129776861));
#80200=CARTESIAN_POINT('Ctrl Pts',(3.75706459059,-9.13925765647,4.9129776858));
#80201=CARTESIAN_POINT('Ctrl Pts',(3.81411802643,-9.12422889542,4.91173129034));
#80202=CARTESIAN_POINT('Ctrl Pts',(3.86651403782,-9.0935734628,4.90972003087));
#80203=CARTESIAN_POINT('Ctrl Pts',(3.94373685893,-9.0162718551,4.90110872718));
#80204=CARTESIAN_POINT('Ctrl Pts',(3.98361771521,-8.90210958415,4.88238701109));
#80205=CARTESIAN_POINT('Ctrl Pts',(3.99224364397,-8.84501961539,4.86859296944));
#80206=CARTESIAN_POINT('Ctrl Pts',(3.99540042025,-8.7740131878,4.85347142938));
#80207=CARTESIAN_POINT('Ctrl Pts',(3.99616169511,-8.70088460852,4.850302933));
#80208=CARTESIAN_POINT('Origin',(0.,-9.17423561284,0.47366156039));
#80209=CARTESIAN_POINT('',(2.3,-8.7279990537,4.59960059693));
#80210=CARTESIAN_POINT('',(2.3,-8.7279990537,-3.65227747616));
#80211=CARTESIAN_POINT('Origin',(2.3,-9.17423561284,0.47366156039));
#80212=CARTESIAN_POINT('',(3.,-8.7279990537,-3.65227747616));
#80213=CARTESIAN_POINT('',(3.,-8.7279990537,4.59960059693));
#80214=CARTESIAN_POINT('Ctrl Pts',(3.7,-8.72799905369119,-3.65227747615864));
#80215=CARTESIAN_POINT('Ctrl Pts',(3.7,-9.0282774958225,-3.68475377248559));
#80216=CARTESIAN_POINT('Ctrl Pts',(3.7,-9.13925764872732,-3.96565457044306));
#80217=CARTESIAN_POINT('Ctrl Pts',(3.95543192438937,-8.72799905369119,-3.65227747615864));
#80218=CARTESIAN_POINT('Ctrl Pts',(3.95543192438937,-9.0282774958225,-3.68475377248559));
#80219=CARTESIAN_POINT('Ctrl Pts',(3.95543192438937,-9.13925764872732,-3.96565457044306));
#80220=CARTESIAN_POINT('Ctrl Pts',(3.99616160125782,-8.70088467099341,-3.90297923456964));
#80221=CARTESIAN_POINT('Ctrl Pts',(3.99616160125782,-8.84972443161661,-3.91907684096763));
#80222=CARTESIAN_POINT('Ctrl Pts',(3.99616160125782,-8.90473423943044,-4.05831163661298));
#80223=CARTESIAN_POINT('',(3.7,-9.13925764671,-3.96565456533));
#80224=CARTESIAN_POINT('Origin',(3.7,-8.67423561284,-4.1493785649));
#80225=CARTESIAN_POINT('Ctrl Pts',(3.99616160126,-8.700884671,-3.90297923457));
#80226=CARTESIAN_POINT('Ctrl Pts',(3.99540042025,-8.7740131878,-3.9061483086));
#80227=CARTESIAN_POINT('Ctrl Pts',(3.99224364397,-8.84501961539,-3.92126984866));
#80228=CARTESIAN_POINT('Ctrl Pts',(3.98361771521,-8.90210958415,-3.93506389031));
#80229=CARTESIAN_POINT('Ctrl Pts',(3.94373685893,-9.0162718551,-3.9537856064));
#80230=CARTESIAN_POINT('Ctrl Pts',(3.86651403782,-9.0935734628,-3.96239691009));
#80231=CARTESIAN_POINT('Ctrl Pts',(3.81411802643,-9.12422889542,-3.96440816956));
#80232=CARTESIAN_POINT('Ctrl Pts',(3.75706459059,-9.13925765647,-3.96565456502));
#80233=CARTESIAN_POINT('Ctrl Pts',(3.7,-9.13925764671,-3.96565456533));
#80234=CARTESIAN_POINT('Origin',(4.35,2.13070110951,0.294579834316));
#80235=CARTESIAN_POINT('',(4.45,-2.51831889439,2.53297389574));
#80236=CARTESIAN_POINT('Origin',(4.35,-2.51831889439,2.53297389574));
#80237=CARTESIAN_POINT('',(4.45,-7.83711001806,5.09384703785));
#80238=CARTESIAN_POINT('',(4.45,-5.17771445623,3.81341046679));
#80239=CARTESIAN_POINT('Origin',(4.35,-7.83711001806,5.09384703785));
#80240=CARTESIAN_POINT('Origin',(3.225,-8.31430322211,4.10274328646));
#80241=CARTESIAN_POINT('',(4.35,-8.31430322211,5.10274328646));
#80242=CARTESIAN_POINT('Origin',(4.35,-8.31430322211,4.10274328646));
#80243=CARTESIAN_POINT('',(4.32444937589,-8.31430322211,5.10274328646));
#80244=CARTESIAN_POINT('Origin',(4.35,-2.12788809108,3.34387696505));
#80245=CARTESIAN_POINT('',(4.45,-2.12788809108,2.44387696505));
#80246=CARTESIAN_POINT('Origin',(4.35,-2.12788809108,2.44387696505));
#80247=CARTESIAN_POINT('Origin',(4.45,-2.12788809108,3.34387696505));
#80248=CARTESIAN_POINT('Origin',(4.35,-1.95899712601,2.44387696505));
#80249=CARTESIAN_POINT('',(4.45,2.8773238354,2.44387696505));
#80250=CARTESIAN_POINT('Origin',(4.35,2.8773238354,2.44387696505));
#80251=CARTESIAN_POINT('',(4.45,0.374717872161,2.44387696505));
#80252=CARTESIAN_POINT('Origin',(4.35,2.8773238354,1.84387696505));
#80253=CARTESIAN_POINT('',(4.45,3.4773238354,1.84387696505));
#80254=CARTESIAN_POINT('Origin',(4.35,3.4773238354,1.84387696505));
#80255=CARTESIAN_POINT('Origin',(4.45,2.8773238354,1.84387696505));
#80256=CARTESIAN_POINT('Origin',(4.35,3.4773238354,0.294579834316));
#80257=CARTESIAN_POINT('',(4.45,3.4773238354,-3.65542016568));
#80258=CARTESIAN_POINT('Origin',(4.35,3.4773238354,-3.65542016568));
#80259=CARTESIAN_POINT('',(4.45,3.4773238354,-0.905771600316));
#80260=CARTESIAN_POINT('Origin',(4.35,2.8773238354,-3.65542016568));
#80261=CARTESIAN_POINT('',(4.45,2.8773238354,-4.25542016568));
#80262=CARTESIAN_POINT('Origin',(4.35,2.8773238354,-4.25542016568));
#80263=CARTESIAN_POINT('Origin',(4.45,2.8773238354,-3.65542016568));
#80264=CARTESIAN_POINT('Ctrl Pts',(3.69999999774,-9.41827086749,-4.15542016568));
#80265=CARTESIAN_POINT('Ctrl Pts',(3.69999999833,-9.34659890209,-4.15542016568));
#80266=CARTESIAN_POINT('Ctrl Pts',(3.69999999892,-9.2749269367,-4.13401653812));
#80267=CARTESIAN_POINT('Ctrl Pts',(3.69999999944,-9.21183540432,-4.09110601764));
#80268=CARTESIAN_POINT('Ctrl Pts',(3.69999999982,-9.16559336719,-4.03231265157));
#80269=CARTESIAN_POINT('Ctrl Pts',(3.70000000003,-9.13925764692,-3.96565456539));
#80270=CARTESIAN_POINT('Ctrl Pts',(3.81412909821,-9.41827089013,-4.15542016568));
#80271=CARTESIAN_POINT('Ctrl Pts',(3.79947056194,-9.34659892134,-4.15542016565));
#80272=CARTESIAN_POINT('Ctrl Pts',(3.78481202566,-9.27492695255,-4.13401653803));
#80273=CARTESIAN_POINT('Ctrl Pts',(3.77190837788,-9.21183541723,-4.09110601746));
#80274=CARTESIAN_POINT('Ctrl Pts',(3.76245084042,-9.16559337792,-4.03231265129));
#80275=CARTESIAN_POINT('Ctrl Pts',(3.75706459059,-9.13925765647,-3.96565456502));
#80276=CARTESIAN_POINT('Ctrl Pts',(3.92823594404,-9.38909765086,-4.15542016568));
#80277=CARTESIAN_POINT('Ctrl Pts',(3.89892199959,-9.32091627439,-4.15542016461));
#80278=CARTESIAN_POINT('Ctrl Pts',(3.86960805513,-9.25273489792,-4.13385699888));
#80279=CARTESIAN_POINT('Ctrl Pts',(3.84380320278,-9.19278171906,-4.0906252646));
#80280=CARTESIAN_POINT('Ctrl Pts',(3.82488943837,-9.14898176867,-4.03143501908));
#80281=CARTESIAN_POINT('Ctrl Pts',(3.81411802643,-9.12422889542,-3.96440816956));
#80282=CARTESIAN_POINT('Ctrl Pts',(4.03302804821,-9.33107957038,-4.15542016568));
#80283=CARTESIAN_POINT('Ctrl Pts',(3.99017706972,-9.2696193654,-4.1554201695));
#80284=CARTESIAN_POINT('Ctrl Pts',(3.94732609124,-9.20815916043,-4.13359925186));
#80285=CARTESIAN_POINT('Ctrl Pts',(3.90964076698,-9.15426319663,-4.0898484638));
#80286=CARTESIAN_POINT('Ctrl Pts',(3.8820963349,-9.11520770945,-4.03001850758));
#80287=CARTESIAN_POINT('Ctrl Pts',(3.86651403782,-9.0935734628,-3.96239691009));
#80288=CARTESIAN_POINT('Ctrl Pts',(4.18747374061,-9.18016437508,-4.15542016568));
#80289=CARTESIAN_POINT('Ctrl Pts',(4.12388018645,-9.13700016797,-4.15542016252));
#80290=CARTESIAN_POINT('Ctrl Pts',(4.0602866323,-9.09383596087,-4.13249096908));
#80291=CARTESIAN_POINT('Ctrl Pts',(4.00475631151,-9.05633061601,-4.08650843459));
#80292=CARTESIAN_POINT('Ctrl Pts',(3.96503122609,-9.029900996,-4.02393293739));
#80293=CARTESIAN_POINT('Ctrl Pts',(3.94373685893,-9.0162718551,-3.9537856064));
#80294=CARTESIAN_POINT('Ctrl Pts',(4.26723541157,-8.98063713586,-4.15542016568));
#80295=CARTESIAN_POINT('Ctrl Pts',(4.19077919927,-8.95915602901,-4.1554201683));
#80296=CARTESIAN_POINT('Ctrl Pts',(4.11432298698,-8.93767492216,-4.13000304884));
#80297=CARTESIAN_POINT('Ctrl Pts',(4.04869892936,-8.91937700045,-4.07900263159));
#80298=CARTESIAN_POINT('Ctrl Pts',(4.00420277032,-8.90727654877,-4.01043652908));
#80299=CARTESIAN_POINT('Ctrl Pts',(3.98361771521,-8.90210958415,-3.93506389031));
#80300=CARTESIAN_POINT('Ctrl Pts',(4.28448738522,-8.88291546038,-4.15542016568));
#80301=CARTESIAN_POINT('Ctrl Pts',(4.2038128468,-8.87211558957,-4.15542016079));
#80302=CARTESIAN_POINT('Ctrl Pts',(4.12313830838,-8.86131571876,-4.12815293378));
#80303=CARTESIAN_POINT('Ctrl Pts',(4.05474416619,-8.85231492765,-4.07341965826));
#80304=CARTESIAN_POINT('Ctrl Pts',(4.01023278232,-8.84679291313,-4.00043036345));
#80305=CARTESIAN_POINT('Ctrl Pts',(3.99224364397,-8.84501961539,-3.92126984866));
#80306=CARTESIAN_POINT('Ctrl Pts',(4.2908008405,-8.79368075155,-4.15542016568));
#80307=CARTESIAN_POINT('Ctrl Pts',(4.20683195096,-8.78806573108,-4.15542016568));
#80308=CARTESIAN_POINT('Ctrl Pts',(4.12286306143,-8.78245071061,-4.12598423857));
#80309=CARTESIAN_POINT('Ctrl Pts',(4.05279621082,-8.77777630692,-4.06686040464));
#80310=CARTESIAN_POINT('Ctrl Pts',(4.00960658253,-8.77491887358,-3.98899545804));
#80311=CARTESIAN_POINT('Ctrl Pts',(3.99540042025,-8.7740131878,-3.9061483086));
#80312=CARTESIAN_POINT('Ctrl Pts',(4.29232317424,-8.70602837163,-4.15542016568));
#80313=CARTESIAN_POINT('Ctrl Pts',(4.20764026079,-8.70455761115,-4.15542016568));
#80314=CARTESIAN_POINT('Ctrl Pts',(4.12295734733,-8.70308685067,-4.12553116999));
#80315=CARTESIAN_POINT('Ctrl Pts',(4.05251771609,-8.70186346543,-4.06549012145));
#80316=CARTESIAN_POINT('Ctrl Pts',(4.00958636427,-8.70111783998,-3.98660378483));
#80317=CARTESIAN_POINT('Ctrl Pts',(3.99616158712,-8.70088468041,-3.90297914754));
#80318=CARTESIAN_POINT('Origin',(3.69999999519659,-9.41833116541397,-3.85533150874716));
#80319=CARTESIAN_POINT('Origin',(3.225,-9.41827086707,-3.85542016568));
#80320=CARTESIAN_POINT('',(2.3,-9.13925764673,-3.96565456539));
#80321=CARTESIAN_POINT('Origin',(2.3,-9.41827086707,-3.85542016568));
#80322=CARTESIAN_POINT('',(3.,-9.13925764673,-3.96565456539));
#80323=CARTESIAN_POINT('Origin',(2.3,-8.20939783898,-3.85542016568));
#80324=CARTESIAN_POINT('',(2.,-9.41827086707,-3.85542016568));
#80325=CARTESIAN_POINT('',(2.,-10.0779006799,-3.85542016568));
#80326=CARTESIAN_POINT('',(2.,-9.7480857735,-3.85542016568));
#80327=CARTESIAN_POINT('Origin',(2.3,-10.0779006799,-3.85542016568));
#80328=CARTESIAN_POINT('Origin',(2.3,-9.41827086707,-3.85542016568));
#80329=CARTESIAN_POINT('Origin',(3.225,-10.0779006799,-3.15542016568));
#80330=CARTESIAN_POINT('',(4.35,-10.4977210429,-4.06302738404));
#80331=CARTESIAN_POINT('Origin',(4.35,-10.0779006799,-3.15542016568));
#80332=CARTESIAN_POINT('',(2.3,-10.4977210429,-4.06302738404));
#80333=CARTESIAN_POINT('Origin',(2.3,-10.0779006799,-3.15542016568));
#80334=CARTESIAN_POINT('',(3.325,-10.4977210429,-4.06302738404));
#80335=CARTESIAN_POINT('Origin',(4.35,-1.95899712601,-4.25542016568));
#80336=CARTESIAN_POINT('',(4.45,-10.0779006799,-4.25542016568));
#80337=CARTESIAN_POINT('Origin',(4.35,-10.0779006799,-4.25542016568));
#80338=CARTESIAN_POINT('',(4.45,-3.60028842226,-4.25542016568));
#80339=CARTESIAN_POINT('Origin',(0.,-8.08610163061,5.10274328646));
#80340=CARTESIAN_POINT('',(4.35,-12.9053426461,5.10274328646));
#80341=CARTESIAN_POINT('',(4.35,-1.95899712601,5.10274328646));
#80342=CARTESIAN_POINT('',(2.3,-12.9053426461,5.10274328646));
#80343=CARTESIAN_POINT('',(3.225,-12.9053426461,5.10274328646));
#80344=CARTESIAN_POINT('',(2.3,-9.41827086707,5.10274328646));
#80345=CARTESIAN_POINT('',(2.3,-12.0504559477,5.10274328646));
#80346=CARTESIAN_POINT('',(3.69999999774,-9.41827086749,5.10274328646));
#80347=CARTESIAN_POINT('',(3.225,-9.41827086707,5.10274328646));
#80348=CARTESIAN_POINT('Ctrl Pts',(3.69999999774,-9.41827086749,5.10274328646));
#80349=CARTESIAN_POINT('Ctrl Pts',(3.73058948857333,-9.41827087355667,5.10274328646));
#80350=CARTESIAN_POINT('Ctrl Pts',(3.76117302676985,-9.41574705670535,5.10274328662896));
#80351=CARTESIAN_POINT('Ctrl Pts',(3.79135695696247,-9.41074020445563,5.10274328606016));
#80352=CARTESIAN_POINT('Ctrl Pts',(3.8215408871551,-9.40573335220591,5.10274328549136));
#80353=CARTESIAN_POINT('Ctrl Pts',(3.85132370712135,-9.39824319698092,5.10274328437385));
#80354=CARTESIAN_POINT('Ctrl Pts',(3.880310581398,-9.38836645220521,5.1027432782161));
#80355=CARTESIAN_POINT('Ctrl Pts',(3.90707199290093,-9.37924799297674,5.1027432725311));
#80356=CARTESIAN_POINT('Ctrl Pts',(3.93315644396342,-9.36809987699747,5.10274326252178));
#80357=CARTESIAN_POINT('Ctrl Pts',(3.95827561771127,-9.35505208010836,5.10274325269434));
#80358=CARTESIAN_POINT('Ctrl Pts',(3.98223829836866,-9.34260500707664,5.10274324331936));
#80359=CARTESIAN_POINT('Ctrl Pts',(4.00532196797495,-9.32842939224294,5.10274323477061));
#80360=CARTESIAN_POINT('Ctrl Pts',(4.02730698337273,-9.31267452069528,5.10274323470365));
#80361=CARTESIAN_POINT('Ctrl Pts',(4.0342532243783,-9.30769671500346,5.1027432346825));
#80362=CARTESIAN_POINT('Ctrl Pts',(4.04109006204254,-9.30256152719756,5.10274323548998));
#80363=CARTESIAN_POINT('Ctrl Pts',(4.04781138042469,-9.29727441845877,5.10274323721421));
#80364=CARTESIAN_POINT('Ctrl Pts',(4.06816544935236,-9.28126354535637,5.10274324243566));
#80365=CARTESIAN_POINT('Ctrl Pts',(4.08745353683921,-9.26386507535306,5.10274325797042));
#80366=CARTESIAN_POINT('Ctrl Pts',(4.1055168903408,-9.24523724841711,5.10274326872092));
#80367=CARTESIAN_POINT('Ctrl Pts',(4.12268030159011,-9.22753748661184,5.10274327893581));
#80368=CARTESIAN_POINT('Ctrl Pts',(4.13873762061326,-9.20872790766285,5.10274328434029));
#80369=CARTESIAN_POINT('Ctrl Pts',(4.1535845819758,-9.18897826222551,5.10274328574875));
#80370=CARTESIAN_POINT('Ctrl Pts',(4.16272152564545,-9.17682416594611,5.10274328661553));
#80371=CARTESIAN_POINT('Ctrl Pts',(4.17140072073273,-9.16431470638581,5.10274328646));
#80372=CARTESIAN_POINT('Ctrl Pts',(4.17960523291625,-9.15149611025241,5.10274328646));
#80373=CARTESIAN_POINT('Ctrl Pts',(4.18942766527051,-9.13614970201014,5.10274328646));
#80374=CARTESIAN_POINT('Ctrl Pts',(4.19857745049624,-9.12036311945856,5.10274328646));
#80375=CARTESIAN_POINT('Ctrl Pts',(4.20701878194007,-9.10419983822068,5.10274328646));
#80376=CARTESIAN_POINT('Ctrl Pts',(4.21621021747847,-9.08660027367622,5.10274328646));
#80377=CARTESIAN_POINT('Ctrl Pts',(4.22456152722091,-9.06855481897592,5.10274328646));
#80378=CARTESIAN_POINT('Ctrl Pts',(4.2320738661817,-9.05018712924208,5.10274328646));
#80379=CARTESIAN_POINT('Ctrl Pts',(4.23525034335279,-9.04242063368992,5.10274328646));
#80380=CARTESIAN_POINT('Ctrl Pts',(4.23827738137825,-9.03459693600601,5.10274328646));
#80381=CARTESIAN_POINT('Ctrl Pts',(4.24115737109239,-9.02672676812149,5.10274328646));
#80382=CARTESIAN_POINT('Ctrl Pts',(4.24909569801083,-9.00503364704426,5.10274328646));
#80383=CARTESIAN_POINT('Ctrl Pts',(4.25591706153315,-8.98297603570749,5.10274328646));
#80384=CARTESIAN_POINT('Ctrl Pts',(4.26171659160653,-8.96076940630961,5.10274328646));
#80385=CARTESIAN_POINT('Ctrl Pts',(4.26455589904718,-8.94989758613051,5.10274328646));
#80386=CARTESIAN_POINT('Ctrl Pts',(4.26715114281098,-8.93899011197066,5.10274328646));
#80387=CARTESIAN_POINT('Ctrl Pts',(4.26951780859379,-8.92807096217797,5.10274328646));
#80388=CARTESIAN_POINT('Ctrl Pts',(4.27382084868247,-8.90821790999222,5.10274328646));
#80389=CARTESIAN_POINT('Ctrl Pts',(4.27736537389317,-8.88833607622953,5.10274328652144));
#80390=CARTESIAN_POINT('Ctrl Pts',(4.28025710062774,-8.868557900564,5.10274328639925));
#80391=CARTESIAN_POINT('Ctrl Pts',(4.28203791090249,-8.85637791895645,5.102743286324));
#80392=CARTESIAN_POINT('Ctrl Pts',(4.2835716533847,-8.84423662612072,5.10274328620522));
#80393=CARTESIAN_POINT('Ctrl Pts',(4.2848866086288,-8.83215545542406,5.10274328535497));
#80394=CARTESIAN_POINT('Ctrl Pts',(4.28680275059482,-8.81455087285411,5.102743284116));
#80395=CARTESIAN_POINT('Ctrl Pts',(4.28827698219617,-8.79709218114212,5.10274328404483));
#80396=CARTESIAN_POINT('Ctrl Pts',(4.28939927179632,-8.77979151596189,5.10274328478464));
#80397=CARTESIAN_POINT('Ctrl Pts',(4.29044254900022,-8.76370886706949,5.10274328547236));
#80398=CARTESIAN_POINT('Ctrl Pts',(4.29118189695424,-8.74776302279939,5.10274328622038));
#80399=CARTESIAN_POINT('Ctrl Pts',(4.29168885063704,-8.73191886459746,5.1027432863823));
#80400=CARTESIAN_POINT('Ctrl Pts',(4.29196579590166,-8.72326331136879,5.10274328647075));
#80401=CARTESIAN_POINT('Ctrl Pts',(4.29217335586042,-8.71463728288328,5.10274328645986));
#80402=CARTESIAN_POINT('Ctrl Pts',(4.29232279496067,-8.70602836504273,5.10274328645976));
#80403=CARTESIAN_POINT('Ctrl Pts',(3.69999999774,-9.41827086749,5.10274328646));
#80404=CARTESIAN_POINT('Ctrl Pts',(3.69999999833,-9.34659890209,5.10274328646));
#80405=CARTESIAN_POINT('Ctrl Pts',(3.69999999892,-9.2749269367,5.0813396589));
#80406=CARTESIAN_POINT('Ctrl Pts',(3.69999999944,-9.21183540432,5.03842913842));
#80407=CARTESIAN_POINT('Ctrl Pts',(3.69999999982,-9.16559336719,4.97963577235));
#80408=CARTESIAN_POINT('Ctrl Pts',(3.70000000003,-9.13925764692,4.91297768617));
#80409=CARTESIAN_POINT('Ctrl Pts',(3.81412909821,-9.41827089013,5.10274328646));
#80410=CARTESIAN_POINT('Ctrl Pts',(3.79947056194,-9.34659892134,5.10274328643));
#80411=CARTESIAN_POINT('Ctrl Pts',(3.78481202566,-9.27492695255,5.08133965881));
#80412=CARTESIAN_POINT('Ctrl Pts',(3.77190837788,-9.21183541723,5.03842913824));
#80413=CARTESIAN_POINT('Ctrl Pts',(3.76245084042,-9.16559337792,4.97963577207));
#80414=CARTESIAN_POINT('Ctrl Pts',(3.75706459059,-9.13925765647,4.9129776858));
#80415=CARTESIAN_POINT('Ctrl Pts',(3.92823594404,-9.38909765086,5.10274328646));
#80416=CARTESIAN_POINT('Ctrl Pts',(3.89892199959,-9.32091627439,5.10274328539));
#80417=CARTESIAN_POINT('Ctrl Pts',(3.86960805513,-9.25273489792,5.08118011966));
#80418=CARTESIAN_POINT('Ctrl Pts',(3.84380320278,-9.19278171906,5.03794838538));
#80419=CARTESIAN_POINT('Ctrl Pts',(3.82488943837,-9.14898176867,4.97875813986));
#80420=CARTESIAN_POINT('Ctrl Pts',(3.81411802643,-9.12422889542,4.91173129034));
#80421=CARTESIAN_POINT('Ctrl Pts',(4.03302804821,-9.33107957038,5.10274328646));
#80422=CARTESIAN_POINT('Ctrl Pts',(3.99017706972,-9.2696193654,5.10274329028));
#80423=CARTESIAN_POINT('Ctrl Pts',(3.94732609124,-9.20815916043,5.08092237264));
#80424=CARTESIAN_POINT('Ctrl Pts',(3.90964076698,-9.15426319663,5.03717158458));
#80425=CARTESIAN_POINT('Ctrl Pts',(3.8820963349,-9.11520770945,4.97734162836));
#80426=CARTESIAN_POINT('Ctrl Pts',(3.86651403782,-9.0935734628,4.90972003087));
#80427=CARTESIAN_POINT('Ctrl Pts',(4.18747374061,-9.18016437508,5.10274328646));
#80428=CARTESIAN_POINT('Ctrl Pts',(4.12388018645,-9.13700016797,5.1027432833));
#80429=CARTESIAN_POINT('Ctrl Pts',(4.0602866323,-9.09383596087,5.07981408986));
#80430=CARTESIAN_POINT('Ctrl Pts',(4.00475631151,-9.05633061601,5.03383155537));
#80431=CARTESIAN_POINT('Ctrl Pts',(3.96503122609,-9.029900996,4.97125605817));
#80432=CARTESIAN_POINT('Ctrl Pts',(3.94373685893,-9.0162718551,4.90110872718));
#80433=CARTESIAN_POINT('Ctrl Pts',(4.26723541157,-8.98063713586,5.10274328646));
#80434=CARTESIAN_POINT('Ctrl Pts',(4.19077919927,-8.95915602901,5.10274328908));
#80435=CARTESIAN_POINT('Ctrl Pts',(4.11432298698,-8.93767492216,5.07732616962));
#80436=CARTESIAN_POINT('Ctrl Pts',(4.04869892936,-8.91937700045,5.02632575237));
#80437=CARTESIAN_POINT('Ctrl Pts',(4.00420277032,-8.90727654877,4.95775964986));
#80438=CARTESIAN_POINT('Ctrl Pts',(3.98361771521,-8.90210958415,4.88238701109));
#80439=CARTESIAN_POINT('Ctrl Pts',(4.28448738522,-8.88291546038,5.10274328646));
#80440=CARTESIAN_POINT('Ctrl Pts',(4.2038128468,-8.87211558957,5.10274328157));
#80441=CARTESIAN_POINT('Ctrl Pts',(4.12313830838,-8.86131571876,5.07547605456));
#80442=CARTESIAN_POINT('Ctrl Pts',(4.05474416619,-8.85231492765,5.02074277903));
#80443=CARTESIAN_POINT('Ctrl Pts',(4.01023278232,-8.84679291313,4.94775348423));
#80444=CARTESIAN_POINT('Ctrl Pts',(3.99224364397,-8.84501961539,4.86859296944));
#80445=CARTESIAN_POINT('Ctrl Pts',(4.2908008405,-8.79368075155,5.10274328646));
#80446=CARTESIAN_POINT('Ctrl Pts',(4.20683195096,-8.78806573108,5.10274328646));
#80447=CARTESIAN_POINT('Ctrl Pts',(4.12286306143,-8.78245071061,5.07330735934));
#80448=CARTESIAN_POINT('Ctrl Pts',(4.05279621082,-8.77777630692,5.01418352542));
#80449=CARTESIAN_POINT('Ctrl Pts',(4.00960658253,-8.77491887358,4.93631857882));
#80450=CARTESIAN_POINT('Ctrl Pts',(3.99540042025,-8.7740131878,4.85347142938));
#80451=CARTESIAN_POINT('Ctrl Pts',(4.29232317424,-8.70602837163,5.10274328646));
#80452=CARTESIAN_POINT('Ctrl Pts',(4.20764026079,-8.70455761115,5.10274328646));
#80453=CARTESIAN_POINT('Ctrl Pts',(4.12295734733,-8.70308685067,5.07285429077));
#80454=CARTESIAN_POINT('Ctrl Pts',(4.05251771609,-8.70186346543,5.01281324223));
#80455=CARTESIAN_POINT('Ctrl Pts',(4.00958636427,-8.70111783998,4.93392690561));
#80456=CARTESIAN_POINT('Ctrl Pts',(3.99616158712,-8.70088468041,4.85030226832));
#80457=CARTESIAN_POINT('Origin',(3.69999999356454,-9.41833116526676,4.80265463001755));
#80458=CARTESIAN_POINT('Origin',(3.,-8.67423561284,5.09670168568));
#80459=CARTESIAN_POINT('',(2.3,-9.13925764673,4.91297768617));
#80460=CARTESIAN_POINT('',(3.225,-9.13925764673,4.91297768617));
#80461=CARTESIAN_POINT('Origin',(2.3,-8.67423561284,5.09670168568));
#80462=CARTESIAN_POINT('Origin',(2.3,-9.17423561284,0.47366156039));
#80463=CARTESIAN_POINT('',(2.,-8.76025711822,4.30133994369));
#80464=CARTESIAN_POINT('',(2.,-8.76025711822,-3.35401682291));
#80465=CARTESIAN_POINT('Origin',(2.,-9.17423561284,0.47366156039));
#80466=CARTESIAN_POINT('Origin',(2.3,-8.76025711822,-3.35401682291));
#80467=CARTESIAN_POINT('Origin',(2.3,-8.76025711822,4.30133994369));
#80468=CARTESIAN_POINT('Origin',(3.,-8.67423561284,-4.1493785649));
#80469=CARTESIAN_POINT('Origin',(2.3,-8.67423561284,-4.1493785649));
#80470=CARTESIAN_POINT('Origin',(4.35,-8.31430322211,4.10274328646));
#80471=CARTESIAN_POINT('',(4.45,-8.31430322211,5.20274328646));
#80472=CARTESIAN_POINT('Origin',(4.45,-8.31430322211,4.10274328646));
#80473=CARTESIAN_POINT('Origin',(4.35,-8.31430322211,5.20274328646));
#80474=CARTESIAN_POINT('Origin',(4.45,0.,0.));
#80475=CARTESIAN_POINT('',(4.45,4.7773238354,-4.87121911588));
#80476=CARTESIAN_POINT('',(4.45,4.7773238354,-5.55542016568));
#80477=CARTESIAN_POINT('',(4.45,4.7773238354,0.294579834316));
#80478=CARTESIAN_POINT('',(4.45,4.9773238354,-4.67121911588));
#80479=CARTESIAN_POINT('Origin',(4.45,4.9773238354,-4.87121911588));
#80480=CARTESIAN_POINT('',(4.45,15.177455061,-4.67121911588));
#80481=CARTESIAN_POINT('',(4.45,-1.95899712601,-4.67121911588));
#80482=CARTESIAN_POINT('',(4.45,15.177455061,4.02878088412));
#80483=CARTESIAN_POINT('',(4.45,15.177455061,0.294579834316));
#80484=CARTESIAN_POINT('',(4.45,4.9773238354,4.02878088412));
#80485=CARTESIAN_POINT('',(4.45,-1.95899712601,4.02878088412));
#80486=CARTESIAN_POINT('',(4.45,4.7773238354,4.22878088412));
#80487=CARTESIAN_POINT('Origin',(4.45,4.9773238354,4.22878088412));
#80488=CARTESIAN_POINT('',(4.45,4.7773238354,5.90191320834));
#80489=CARTESIAN_POINT('',(4.45,4.7773238354,0.294579834316));
#80490=CARTESIAN_POINT('',(4.45,4.32269078618,5.90191320834));
#80491=CARTESIAN_POINT('',(4.45,-1.95899712601,5.90191320834));
#80492=CARTESIAN_POINT('',(4.45,2.97160656206,4.00332568658));
#80493=CARTESIAN_POINT('',(4.45,0.332366624557,0.294579834316));
#80494=CARTESIAN_POINT('',(4.45,2.48275227055,3.75120710557));
#80495=CARTESIAN_POINT('Origin',(4.45,2.48275227055,4.35120710557));
#80496=CARTESIAN_POINT('',(4.45,-2.24076213014,3.75120710557));
#80497=CARTESIAN_POINT('',(4.45,-1.95899712601,3.75120710557));
#80498=CARTESIAN_POINT('',(4.45,-2.49116133917,3.80595465384));
#80499=CARTESIAN_POINT('Origin',(4.45,-2.24076213014,4.35120710557));
#80500=CARTESIAN_POINT('',(4.45,-7.50411762961,6.1080814688));
#80501=CARTESIAN_POINT('',(4.45,4.59408048322,0.552161034916));
#80502=CARTESIAN_POINT('',(4.45,-7.67105043563,6.14457983432));
#80503=CARTESIAN_POINT('Origin',(4.45,-7.67105043563,5.74457983432));
#80504=CARTESIAN_POINT('',(4.45,-13.881029587,6.14457983432));
#80505=CARTESIAN_POINT('',(4.45,-1.95899712601,6.14457983432));
#80506=CARTESIAN_POINT('',(4.45,-14.4995104256,5.89840049188));
#80507=CARTESIAN_POINT('Origin',(4.45,-13.881029587,5.24457983432));
#80508=CARTESIAN_POINT('',(4.45,-18.4234397556,2.18656441774));
#80509=CARTESIAN_POINT('',(4.45,-18.85379408,1.77947127938));
#80510=CARTESIAN_POINT('',(4.45,-18.4689834555,1.96054363567));
#80511=CARTESIAN_POINT('Origin',(4.45,-18.2859995693,2.04127093829));
#80512=CARTESIAN_POINT('',(4.45,-18.3216303794,1.54889979527));
#80513=CARTESIAN_POINT('Origin',(4.45,-21.2594877202,0.729452270839));
#80514=CARTESIAN_POINT('',(4.45,-17.889478859,1.2973989265));
#80515=CARTESIAN_POINT('',(4.45,-13.9715079445,-0.982757551184));
#80516=CARTESIAN_POINT('',(4.45,-17.4134008589,1.35252791278));
#80517=CARTESIAN_POINT('Origin',(4.45,-17.6882812316,1.64311487169));
#80518=CARTESIAN_POINT('',(4.45,-13.661263671,4.90185742348));
#80519=CARTESIAN_POINT('',(4.45,-17.907928075,0.88473050722));
#80520=CARTESIAN_POINT('',(4.45,-12.9053426461,5.20274328646));
#80521=CARTESIAN_POINT('Origin',(4.45,-12.9053426461,4.10274328646));
#80522=CARTESIAN_POINT('',(4.45,-1.95899712601,5.20274328646));
#80523=CARTESIAN_POINT('',(4.45,-10.5397030792,-4.15378810588));
#80524=CARTESIAN_POINT('Origin',(4.45,-10.0779006799,-3.15542016568));
#80525=CARTESIAN_POINT('',(4.45,-17.3231001714,-1.01607812301));
#80526=CARTESIAN_POINT('',(4.45,-14.1190276664,-2.49814531564));
#80527=CARTESIAN_POINT('',(4.45,-17.582210652,-0.989652421484));
#80528=CARTESIAN_POINT('Origin',(4.45,-17.4910283166,-1.37912101035));
#80529=CARTESIAN_POINT('',(4.45,-19.0026826744,-1.32221314666));
#80530=CARTESIAN_POINT('',(4.45,-1.95899712601,2.6680522976));
#80531=CARTESIAN_POINT('',(4.45,-19.0409285996,-1.36351104187));
#80532=CARTESIAN_POINT('Origin',(4.45,-21.2594877202,0.729452270839));
#80533=CARTESIAN_POINT('',(4.45,-18.9794133856,-1.68227598146));
#80534=CARTESIAN_POINT('Origin',(4.45,-18.895449313,-1.50075453779));
#80535=CARTESIAN_POINT('',(4.45,-10.7858544195,-5.47226666221));
#80536=CARTESIAN_POINT('',(4.45,-15.667308925,-3.214314146));
#80537=CARTESIAN_POINT('',(4.45,-10.4080160928,-5.55542016568));
#80538=CARTESIAN_POINT('Origin',(4.45,-10.4080160928,-4.65542016568));
#80539=CARTESIAN_POINT('',(4.45,-1.95899712601,-5.55542016568));
#80540=CARTESIAN_POINT('Origin',(2.3,-9.41827086707,-3.85542016568));
#80541=CARTESIAN_POINT('Origin',(2.3,-9.41827086707,-3.85542016568));
#80542=CARTESIAN_POINT('Origin',(2.3,-21.2594877202,0.729452270839));
#80543=CARTESIAN_POINT('',(2.,-17.3209666442,-0.597405571358));
#80544=CARTESIAN_POINT('Origin',(2.3,-17.3209666442,-0.597405571358));
#80545=CARTESIAN_POINT('',(2.,-17.1183636721,1.08100826706));
#80546=CARTESIAN_POINT('Origin',(2.,-21.2594877202,0.729452270839));
#80547=CARTESIAN_POINT('Origin',(2.3,-17.1183636721,1.08100826706));
#80548=CARTESIAN_POINT('Origin',(2.,0.,0.));
#80549=CARTESIAN_POINT('',(2.,-17.1551720262,-0.653035235664));
#80550=CARTESIAN_POINT('Origin',(2.,-17.4910283166,-1.37912101035));
#80551=CARTESIAN_POINT('',(2.,-10.371774934,-3.79074521854));
#80552=CARTESIAN_POINT('',(2.,-13.7337583338,-2.23563518556));
#80553=CARTESIAN_POINT('Origin',(2.,-10.0779006799,-3.15542016568));
#80554=CARTESIAN_POINT('Origin',(2.,-8.67423561284,-4.1493785649));
#80555=CARTESIAN_POINT('',(2.,-9.41827086707,4.80274328646));
#80556=CARTESIAN_POINT('Origin',(2.,-8.67423561284,5.09670168568));
#80557=CARTESIAN_POINT('',(2.,-12.9053426461,4.80274328646));
#80558=CARTESIAN_POINT('',(2.,-12.0504559477,4.80274328646));
#80559=CARTESIAN_POINT('',(2.,-13.3863832983,4.61127046457));
#80560=CARTESIAN_POINT('Origin',(2.,-12.9053426461,4.10274328646));
#80561=CARTESIAN_POINT('',(2.,-16.3982789105,1.76217155265));
#80562=CARTESIAN_POINT('',(2.,-6.22423561284,0.47366156039));
#80563=CARTESIAN_POINT('Origin',(2.,-9.17423561284,0.47366156039));
#80564=CARTESIAN_POINT('Origin',(2.3,-10.0779006799,-3.15542016568));
#80565=CARTESIAN_POINT('Origin',(2.3,-10.371774934,-3.79074521854));
#80566=CARTESIAN_POINT('Origin',(0.,-10.2979776218,-4.15542016568));
#80567=CARTESIAN_POINT('',(2.3,-17.2811181351,-0.925317401172));
#80568=CARTESIAN_POINT('',(2.3,-13.8597044427,-2.50791735107));
#80569=CARTESIAN_POINT('',(4.35,-17.2811181351,-0.925317401172));
#80570=CARTESIAN_POINT('',(3.225,-17.2811181351,-0.925317401172));
#80571=CARTESIAN_POINT('',(4.35,-14.0770456301,-2.4073845938));
#80572=CARTESIAN_POINT('Origin',(4.35,-10.0779006799,-3.15542016568));
#80573=CARTESIAN_POINT('Origin',(4.35,-10.5397030792,-4.15378810588));
#80574=CARTESIAN_POINT('Origin',(2.3,-12.0504559477,4.80274328646));
#80575=CARTESIAN_POINT('Origin',(2.3,-9.41827086707,4.80274328646));
#80576=CARTESIAN_POINT('Origin',(2.3,-12.9053426461,4.80274328646));
#80577=CARTESIAN_POINT('Origin',(3.225,-9.41827086707,4.80274328646));
#80578=CARTESIAN_POINT('Origin',(2.3,-9.41827086707,4.80274328646));
#80579=CARTESIAN_POINT('Origin',(3.225,-12.9053426461,4.10274328646));
#80580=CARTESIAN_POINT('',(4.35,-13.5925435779,4.82921068375));
#80581=CARTESIAN_POINT('Origin',(4.35,-12.9053426461,4.10274328646));
#80582=CARTESIAN_POINT('',(2.3,-13.5925435779,4.82921068375));
#80583=CARTESIAN_POINT('',(3.325,-13.5925435779,4.82921068375));
#80584=CARTESIAN_POINT('Origin',(2.3,-12.9053426461,4.10274328646));
#80585=CARTESIAN_POINT('Origin',(4.35,-1.95899712601,5.20274328646));
#80586=CARTESIAN_POINT('Origin',(4.35,-12.9053426461,5.20274328646));
#80587=CARTESIAN_POINT('Origin',(2.3,-8.67423561284,5.09670168568));
#80588=CARTESIAN_POINT('Origin',(2.3,-9.41827086707,4.80274328646));
#80589=CARTESIAN_POINT('Origin',(2.3,-8.67423561284,-4.1493785649));
#80590=CARTESIAN_POINT('Origin',(4.35,-1.95899712601,-5.55542016568));
#80591=CARTESIAN_POINT('',(4.35,-10.4080160928,-5.65542016568));
#80592=CARTESIAN_POINT('Origin',(4.35,-10.4080160928,-5.55542016568));
#80593=CARTESIAN_POINT('',(4.35,4.8773238354,-5.65542016568));
#80594=CARTESIAN_POINT('',(4.35,-2.7653461287,-5.65542016568));
#80595=CARTESIAN_POINT('Origin',(4.35,4.7773238354,-5.55542016568));
#80596=CARTESIAN_POINT('Origin',(4.35,-10.4080160928,-4.65542016568));
#80597=CARTESIAN_POINT('',(4.35,-10.8278364558,-5.56302738404));
#80598=CARTESIAN_POINT('Origin',(4.35,-10.7858544195,-5.47226666221));
#80599=CARTESIAN_POINT('Origin',(4.35,-10.4080160928,-4.65542016568));
#80600=CARTESIAN_POINT('Origin',(4.35,-15.667308925,-3.214314146));
#80601=CARTESIAN_POINT('',(4.35,-19.0213954219,-1.7730367033));
#80602=CARTESIAN_POINT('Origin',(4.35,-18.9794133856,-1.68227598146));
#80603=CARTESIAN_POINT('',(4.35,-14.9246159388,-3.66803204367));
#80604=CARTESIAN_POINT('Origin',(4.35,-18.895449313,-1.50075453779));
#80605=CARTESIAN_POINT('',(4.35,-19.1136682429,-1.29488929392));
#80606=CARTESIAN_POINT('Origin',(4.35,-19.0409285996,-1.36351104187));
#80607=CARTESIAN_POINT('Origin',(4.35,-18.895449313,-1.50075453779));
#80608=CARTESIAN_POINT('Origin',(4.35,-21.2594877202,0.729452270839));
#80609=CARTESIAN_POINT('',(4.35,-19.0766762825,-1.25494542806));
#80610=CARTESIAN_POINT('Origin',(4.35,-19.0026826744,-1.32221314666));
#80611=CARTESIAN_POINT('Origin',(4.35,-21.2594877202,0.729452270839));
#80612=CARTESIAN_POINT('Origin',(4.35,-1.95899712601,2.6680522976));
#80613=CARTESIAN_POINT('',(4.35,-19.0254782583,-1.22484599945));
#80614=CARTESIAN_POINT('Origin',(4.35,-19.0026826744,-1.32221314666));
#80615=CARTESIAN_POINT('',(4.35,-17.6050062358,-0.892285274267));
#80616=CARTESIAN_POINT('Origin',(4.35,-17.582210652,-0.989652421484));
#80617=CARTESIAN_POINT('',(4.35,-18.246704933,-1.04251968981));
#80618=CARTESIAN_POINT('Origin',(4.35,-17.4910283166,-1.37912101035));
#80619=CARTESIAN_POINT('Origin',(4.35,-17.3231001714,-1.01607812301));
#80620=CARTESIAN_POINT('Origin',(4.35,-17.4910283166,-1.37912101035));
#80621=CARTESIAN_POINT('Origin',(4.35,-14.1190276664,-2.49814531564));
#80622=CARTESIAN_POINT('Origin',(4.35,-12.9053426461,4.10274328646));
#80623=CARTESIAN_POINT('Origin',(4.35,-13.661263671,4.90185742348));
#80624=CARTESIAN_POINT('Origin',(4.35,-17.907928075,0.88473050722));
#80625=CARTESIAN_POINT('',(4.35,-17.3446807657,1.27988117305));
#80626=CARTESIAN_POINT('Origin',(4.35,-17.4134008589,1.35252791278));
#80627=CARTESIAN_POINT('',(4.35,-15.4686121718,3.0545459284));
#80628=CARTESIAN_POINT('Origin',(4.35,-17.6882812316,1.64311487169));
#80629=CARTESIAN_POINT('',(4.35,-17.9397782658,1.2109699402));
#80630=CARTESIAN_POINT('Origin',(4.35,-17.889478859,1.2973989265));
#80631=CARTESIAN_POINT('Origin',(4.35,-17.6882812316,1.64311487169));
#80632=CARTESIAN_POINT('Origin',(4.35,-13.9715079445,-0.982757551184));
#80633=CARTESIAN_POINT('',(4.35,-18.3719297863,1.46247080897));
#80634=CARTESIAN_POINT('Origin',(4.35,-18.3216303794,1.54889979527));
#80635=CARTESIAN_POINT('',(4.35,-18.0119156597,1.25295201451));
#80636=CARTESIAN_POINT('Origin',(4.35,-21.2594877202,0.729452270839));
#80637=CARTESIAN_POINT('',(4.35,-18.4179535709,1.52203266332));
#80638=CARTESIAN_POINT('Origin',(4.35,-18.3216303794,1.54889979527));
#80639=CARTESIAN_POINT('',(4.35,-18.5604753986,1.92017998437));
#80640=CARTESIAN_POINT('Origin',(4.35,-18.4689834555,1.96054363567));
#80641=CARTESIAN_POINT('Origin',(4.35,-21.2594877202,0.729452270839));
#80642=CARTESIAN_POINT('Origin',(4.35,-18.2859995693,2.04127093829));
#80643=CARTESIAN_POINT('',(4.35,-18.4921598488,2.25921115747));
#80644=CARTESIAN_POINT('Origin',(4.35,-18.4234397556,2.18656441774));
#80645=CARTESIAN_POINT('Origin',(4.35,-18.2859995693,2.04127093829));
#80646=CARTESIAN_POINT('Origin',(4.35,-18.85379408,1.77947127938));
#80647=CARTESIAN_POINT('',(4.35,-14.5682305188,5.97104723161));
#80648=CARTESIAN_POINT('Origin',(4.35,-14.4995104256,5.89840049188));
#80649=CARTESIAN_POINT('',(4.35,-16.5301951838,4.11512919454));
#80650=CARTESIAN_POINT('Origin',(4.35,-13.881029587,5.24457983432));
#80651=CARTESIAN_POINT('',(4.35,-13.881029587,6.24457983432));
#80652=CARTESIAN_POINT('Origin',(4.35,-13.881029587,6.14457983432));
#80653=CARTESIAN_POINT('Origin',(4.35,-13.881029587,5.24457983432));
#80654=CARTESIAN_POINT('Origin',(4.35,-1.95899712601,6.14457983432));
#80655=CARTESIAN_POINT('',(4.35,-7.67105043563,6.24457983432));
#80656=CARTESIAN_POINT('Origin',(4.35,-7.67105043563,6.14457983432));
#80657=CARTESIAN_POINT('',(4.35,-10.7760400113,6.24457983432));
#80658=CARTESIAN_POINT('Origin',(4.35,-7.67105043563,5.74457983432));
#80659=CARTESIAN_POINT('',(4.35,-7.46238442811,6.19895687742));
#80660=CARTESIAN_POINT('Origin',(4.35,-7.50411762961,6.1080814688));
#80661=CARTESIAN_POINT('Origin',(4.35,-7.67105043563,5.74457983432));
#80662=CARTESIAN_POINT('Origin',(4.35,4.59408048322,0.552161034916));
#80663=CARTESIAN_POINT('',(4.35,-2.44942813767,3.89683006246));
#80664=CARTESIAN_POINT('Origin',(4.35,-2.49116133917,3.80595465384));
#80665=CARTESIAN_POINT('',(4.35,-4.95590628289,5.04789346994));
#80666=CARTESIAN_POINT('Origin',(4.35,-2.24076213014,4.35120710557));
#80667=CARTESIAN_POINT('',(4.35,-2.24076213014,3.85120710557));
#80668=CARTESIAN_POINT('Origin',(4.35,-2.24076213014,3.75120710557));
#80669=CARTESIAN_POINT('Origin',(4.35,-2.24076213014,4.35120710557));
#80670=CARTESIAN_POINT('Origin',(4.35,-1.95899712601,3.75120710557));
#80671=CARTESIAN_POINT('',(4.35,2.48275227055,3.85120710557));
#80672=CARTESIAN_POINT('Origin',(4.35,2.48275227055,3.75120710557));
#80673=CARTESIAN_POINT('',(4.35,0.120995070207,3.85120710557));
#80674=CARTESIAN_POINT('Origin',(4.35,2.48275227055,4.35120710557));
#80675=CARTESIAN_POINT('',(4.35,2.89013084681,4.06130592308));
#80676=CARTESIAN_POINT('Origin',(4.35,2.97160656206,4.00332568658));
#80677=CARTESIAN_POINT('Origin',(4.35,2.48275227055,4.35120710557));
#80678=CARTESIAN_POINT('Origin',(4.35,0.332366624557,0.294579834316));
#80679=CARTESIAN_POINT('',(4.35,4.24121507093,5.95989344484));
#80680=CARTESIAN_POINT('Origin',(4.35,4.32269078618,5.90191320834));
#80681=CARTESIAN_POINT('',(4.35,3.56567295887,5.01059968396));
#80682=CARTESIAN_POINT('Origin',(4.35,-1.95899712601,5.90191320834));
#80683=CARTESIAN_POINT('',(4.35,4.32269078618,6.00191320834));
#80684=CARTESIAN_POINT('Origin',(4.35,4.32269078618,5.90191320834));
#80685=CARTESIAN_POINT('',(4.35,4.7773238354,6.00191320834));
#80686=CARTESIAN_POINT('Origin',(4.35,4.7773238354,5.90191320834));
#80687=CARTESIAN_POINT('',(4.35,4.55000731079,6.00191320834));
#80688=CARTESIAN_POINT('Origin',(4.35,4.7773238354,0.294579834316));
#80689=CARTESIAN_POINT('',(4.35,4.8773238354,5.90191320834));
#80690=CARTESIAN_POINT('Origin',(4.35,4.7773238354,5.90191320834));
#80691=CARTESIAN_POINT('',(4.35,4.8773238354,4.22878088412));
#80692=CARTESIAN_POINT('Origin',(4.35,4.7773238354,4.22878088412));
#80693=CARTESIAN_POINT('',(4.35,4.8773238354,5.06534704623));
#80694=CARTESIAN_POINT('Origin',(4.35,4.9773238354,4.22878088412));
#80695=CARTESIAN_POINT('',(4.35,4.9773238354,4.12878088412));
#80696=CARTESIAN_POINT('Origin',(4.35,4.9773238354,4.02878088412));
#80697=CARTESIAN_POINT('Origin',(4.35,4.9773238354,4.22878088412));
#80698=CARTESIAN_POINT('Origin',(4.35,-1.95899712601,4.02878088412));
#80699=CARTESIAN_POINT('',(4.35,15.177455061,4.12878088412));
#80700=CARTESIAN_POINT('Origin',(4.35,15.177455061,4.02878088412));
#80701=CARTESIAN_POINT('',(4.35,10.0773894482,4.12878088412));
#80702=CARTESIAN_POINT('Origin',(4.35,15.177455061,0.294579834316));
#80703=CARTESIAN_POINT('',(4.35,15.277455061,4.02878088412));
#80704=CARTESIAN_POINT('Origin',(4.35,15.177455061,4.02878088412));
#80705=CARTESIAN_POINT('',(4.35,15.277455061,-4.67121911588));
#80706=CARTESIAN_POINT('Origin',(4.35,15.177455061,-4.67121911588));
#80707=CARTESIAN_POINT('',(4.35,15.277455061,-0.32121911588));
#80708=CARTESIAN_POINT('Origin',(4.35,-1.95899712601,-4.67121911588));
#80709=CARTESIAN_POINT('',(4.35,15.177455061,-4.77121911588));
#80710=CARTESIAN_POINT('Origin',(4.35,15.177455061,-4.67121911588));
#80711=CARTESIAN_POINT('',(4.35,4.9773238354,-4.77121911588));
#80712=CARTESIAN_POINT('Origin',(4.35,4.9773238354,-4.67121911588));
#80713=CARTESIAN_POINT('',(4.35,10.0773894482,-4.77121911588));
#80714=CARTESIAN_POINT('Origin',(4.35,4.9773238354,-4.87121911588));
#80715=CARTESIAN_POINT('',(4.35,4.8773238354,-4.87121911588));
#80716=CARTESIAN_POINT('Origin',(4.35,4.7773238354,-4.87121911588));
#80717=CARTESIAN_POINT('Origin',(4.35,4.9773238354,-4.87121911588));
#80718=CARTESIAN_POINT('Origin',(4.35,4.7773238354,0.294579834316));
#80719=CARTESIAN_POINT('',(4.35,4.8773238354,-5.26331964078));
#80720=CARTESIAN_POINT('Origin',(2.3,-9.17423561284,0.47366156039));
#80721=CARTESIAN_POINT('',(2.3,-6.52423561284,0.47366156039));
#80722=CARTESIAN_POINT('',(2.3,-11.82423561284,0.47366156039));
#80723=CARTESIAN_POINT('Origin',(2.3,-9.17423561284,0.47366156039));
#80724=CARTESIAN_POINT('Origin',(2.3,-9.17423561284,0.47366156039));
#80725=CARTESIAN_POINT('Origin',(2.3,-6.22423561284,0.473661560390001));
#80726=CARTESIAN_POINT('Origin',(2.3,-12.9053426461,4.10274328646));
#80727=CARTESIAN_POINT('Origin',(2.3,-13.3863832983,4.61127046457));
#80728=CARTESIAN_POINT('Origin',(3.94208066889,-21.2594877202,0.729452270839));
#80729=CARTESIAN_POINT('',(3.94208066889,-18.4179535709,1.52203266332));
#80730=CARTESIAN_POINT('Origin',(3.94208066889002,-18.7069231459878,1.44143126945959));
#80731=CARTESIAN_POINT('',(3.94208067709125,-18.560475400287,1.92017998362573));
#80732=CARTESIAN_POINT('Origin',(3.94208066889,-21.2594877202,0.729452270839));
#80733=CARTESIAN_POINT('Origin',(3.94208070435522,-18.8349512373474,1.79908900499315));
#80734=CARTESIAN_POINT('Origin',(-0.660000000086,-21.2594877202,0.729452270839));
#80735=CARTESIAN_POINT('',(2.225,-18.4179535709,1.52203266332));
#80736=CARTESIAN_POINT('',(2.225,-18.5604753986,1.92017998437));
#80737=CARTESIAN_POINT('Origin',(-3.94208066889,-21.2594877202,0.729452270839));
#80738=CARTESIAN_POINT('',(-3.94208066889,-18.5604753986,1.92017998437));
#80739=CARTESIAN_POINT('Origin',(-3.94208066888998,-18.8349512391587,1.79908905596751));
#80740=CARTESIAN_POINT('',(-3.94208069869828,-18.4179535709075,1.5220326633179));
#80741=CARTESIAN_POINT('Origin',(-3.94208066889,-21.2594877202,0.729452270839));
#80742=CARTESIAN_POINT('Origin',(-3.94208081057025,-18.7069232411033,1.44143132952455));
#80743=CARTESIAN_POINT('Origin',(-0.660000000086,-21.2594877202,0.729452270839));
#80744=CARTESIAN_POINT('',(-4.35,-18.5604753986,1.92017998437));
#80745=CARTESIAN_POINT('',(2.225,-18.5604753986,1.92017998437));
#80746=CARTESIAN_POINT('',(-4.35,-18.4179535709,1.52203266332));
#80747=CARTESIAN_POINT('Origin',(-4.35,-21.2594877202,0.729452270839));
#80748=CARTESIAN_POINT('',(-2.225,-18.4179535709,1.52203266332));
#80749=CARTESIAN_POINT('Origin',(3.94208066889,-21.2594877202,0.729452270839));
#80750=CARTESIAN_POINT('',(3.94208066889,-19.1136682429,-1.29488929392));
#80751=CARTESIAN_POINT('Origin',(3.94208066888998,-19.3318871727915,-1.089024050049));
#80752=CARTESIAN_POINT('',(3.94208068754125,-19.076676282417,-1.25494542798173));
#80753=CARTESIAN_POINT('Origin',(3.94208066889,-21.2594877202,0.729452270839));
#80754=CARTESIAN_POINT('Ctrl Pts',(3.69310716476821,-19.4224990726068,-0.940557363285379));
#80755=CARTESIAN_POINT('Ctrl Pts',(3.62071554431345,-19.3428165984805,-1.0129966546369));
#80756=CARTESIAN_POINT('Ctrl Pts',(3.60654669651459,-19.2341736857703,-1.11176422863347));
#80757=CARTESIAN_POINT('Ctrl Pts',(3.68256352205708,-19.1285867907532,-1.20775351544384));
#80758=CARTESIAN_POINT('Ctrl Pts',(3.81232210935313,-19.0766762800567,-1.25494542441243));
#80759=CARTESIAN_POINT('Ctrl Pts',(3.94208069665,-19.0766762825,-1.25494542806));
#80760=CARTESIAN_POINT('Origin',(-0.660000000086,-21.2594877202,0.729452270839));
#80761=CARTESIAN_POINT('',(2.225,-19.1136682429,-1.29488929392));
#80762=CARTESIAN_POINT('',(2.225,-19.0766762825,-1.25494542806));
#80763=CARTESIAN_POINT('Origin',(-3.94208066889,-21.2594877202,0.729452270839));
#80764=CARTESIAN_POINT('',(-3.94208066889,-19.0766762825,-1.25494542806));
#80765=CARTESIAN_POINT('Ctrl Pts',(-3.69310715294,-19.4224990402,-0.940557353778));
#80766=CARTESIAN_POINT('Ctrl Pts',(-3.66294397113573,-19.3892980535193,
-0.970740428832556));
#80767=CARTESIAN_POINT('Ctrl Pts',(-3.64523980863271,-19.3499675246131,
-1.00649588150467));
#80768=CARTESIAN_POINT('Ctrl Pts',(-3.63970736237874,-19.2700614290135,
-1.07913865288026));
#80769=CARTESIAN_POINT('Ctrl Pts',(-3.65188684851974,-19.229598084238,-1.1159239504417));
#80770=CARTESIAN_POINT('Ctrl Pts',(-3.70272651915015,-19.1589820790244,
-1.18012108438481));
#80771=CARTESIAN_POINT('Ctrl Pts',(-3.74131530326262,-19.1289285932923,
-1.20744276086762));
#80772=CARTESIAN_POINT('Ctrl Pts',(-3.834024439204,-19.087746776693,-1.24488122241778));
#80773=CARTESIAN_POINT('Ctrl Pts',(-3.88801458823712,-19.0766762824954,
-1.25494542806764));
#80774=CARTESIAN_POINT('Ctrl Pts',(-3.94208066889,-19.0766762825,-1.25494542806));
#80775=CARTESIAN_POINT('',(-3.94208067884,-19.1136682460366,-1.2948892935186));
#80776=CARTESIAN_POINT('Origin',(-3.94208066889,-21.2594877202,0.729452270839));
#80777=CARTESIAN_POINT('Origin',(-3.94208070251596,-19.3318871781364,-1.08902402959631));
#80778=CARTESIAN_POINT('Origin',(-0.660000000086,-21.2594877202,0.729452270839));
#80779=CARTESIAN_POINT('',(-4.35,-19.0766762825,-1.25494542806));
#80780=CARTESIAN_POINT('',(-2.225,-19.0766762825,-1.25494542806));
#80781=CARTESIAN_POINT('',(-4.35,-19.1136682429,-1.29488929392));
#80782=CARTESIAN_POINT('Origin',(-4.35,-21.2594877202,0.729452270839));
#80783=CARTESIAN_POINT('',(2.225,-19.1136682429,-1.29488929392));
#80784=CARTESIAN_POINT('Origin',(2.3,-17.1183636721,1.08100826706));
#80785=CARTESIAN_POINT('',(2.3,-17.3245239517,1.29894848625));
#80786=CARTESIAN_POINT('Origin',(2.3,-17.1183636721,1.08100826706));
#80787=CARTESIAN_POINT('Origin',(2.3,-17.1183636721,1.08100826706));
#80788=CARTESIAN_POINT('Origin',(2.3,-16.3982789105,1.76217155265));
#80789=CARTESIAN_POINT('',(2.3,-15.4585337648,3.064079585));
#80790=CARTESIAN_POINT('Origin',(2.3,-17.3209666442,-0.597405571358));
#80791=CARTESIAN_POINT('',(2.3,-17.3847397713,-0.890548860981));
#80792=CARTESIAN_POINT('Ctrl Pts',(2.15473698243741,-17.5697154200519,-0.5136040068197));
#80793=CARTESIAN_POINT('Ctrl Pts',(2.153925136701,-17.5747914639389,-0.530078530556508));
#80794=CARTESIAN_POINT('Ctrl Pts',(2.15383645219206,-17.5786293167837,-0.546970861777752));
#80795=CARTESIAN_POINT('Ctrl Pts',(2.15447419324571,-17.5811678664151,-0.56402768389419));
#80796=CARTESIAN_POINT('Ctrl Pts',(2.15512887051018,-17.5837738312011,-0.581537476590885));
#80797=CARTESIAN_POINT('Ctrl Pts',(2.15654900948215,-17.5850105747796,-0.599220153813188));
#80798=CARTESIAN_POINT('Ctrl Pts',(2.1587115129593,-17.5848603759444,-0.616799144345278));
#80799=CARTESIAN_POINT('Ctrl Pts',(2.16090081423076,-17.5847083158416,-0.634595974144406));
#80800=CARTESIAN_POINT('Ctrl Pts',(2.16385085219413,-17.5831348715607,-0.652286011369867));
#80801=CARTESIAN_POINT('Ctrl Pts',(2.167512339514,-17.5801692679682,-0.669587219172914));
#80802=CARTESIAN_POINT('Ctrl Pts',(2.17122230575012,-17.5771643991166,-0.687117498861475));
#80803=CARTESIAN_POINT('Ctrl Pts',(2.17566252859434,-17.5727304261426,-0.704248013442034));
#80804=CARTESIAN_POINT('Ctrl Pts',(2.18075816140222,-17.5669439862781,-0.720698733481176));
#80805=CARTESIAN_POINT('Ctrl Pts',(2.18420668827234,-17.5630279479552,-0.731831943472297));
#80806=CARTESIAN_POINT('Ctrl Pts',(2.18795490743752,-17.5584934329078,-0.742654087325353));
#80807=CARTESIAN_POINT('Ctrl Pts',(2.19197420126701,-17.5533753341438,-0.753083793143141));
#80808=CARTESIAN_POINT('Ctrl Pts',(2.19792273800431,-17.5458005710601,-0.768519710706872));
#80809=CARTESIAN_POINT('Ctrl Pts',(2.20446775346183,-17.5369433267012,-0.783099680208059));
#80810=CARTESIAN_POINT('Ctrl Pts',(2.21150225048338,-17.526947526872,-0.796581344453743));
#80811=CARTESIAN_POINT('Ctrl Pts',(2.21844404117408,-17.5170834598339,-0.809885336348122));
#80812=CARTESIAN_POINT('Ctrl Pts',(2.22586226006111,-17.5061109844372,-0.822119321309216));
#80813=CARTESIAN_POINT('Ctrl Pts',(2.23363909862176,-17.4942031712295,-0.833083573826689));
#80814=CARTESIAN_POINT('Ctrl Pts',(2.24132171377096,-17.482439631916,-0.843914984538571));
#80815=CARTESIAN_POINT('Ctrl Pts',(2.24935409459707,-17.4697635897432,-0.85350682681502));
#80816=CARTESIAN_POINT('Ctrl Pts',(2.2576112830013,-17.4563713159729,-0.861705619751016));
#80817=CARTESIAN_POINT('Ctrl Pts',(2.26568317060648,-17.4432795802197,-0.869720422349396));
#80818=CARTESIAN_POINT('Ctrl Pts',(2.27396968242377,-17.4295037165625,-0.876403714059283));
#80819=CARTESIAN_POINT('Ctrl Pts',(2.28234627169755,-17.4152507016175,-0.881654697950748));
#80820=CARTESIAN_POINT('Ctrl Pts',(2.28820169603079,-17.4052875235503,-0.885325253811452));
#80821=CARTESIAN_POINT('Ctrl Pts',(2.29410097189801,-17.3950916835449,-0.888296809376953));
#80822=CARTESIAN_POINT('Ctrl Pts',(2.3,-17.3847397713,-0.890548860981));
#80823=CARTESIAN_POINT('Origin',(2.3,-17.3209666442,-0.597405571358));
#80824=CARTESIAN_POINT('Origin',(2.3,-17.4910283166,-1.37912101035));
#80825=CARTESIAN_POINT('Origin',(2.3,-17.4910283166,-1.37912101035));
#80826=CARTESIAN_POINT('Origin',(2.3,-17.1551720262,-0.653035235664));
#80827=CARTESIAN_POINT('Origin',(2.3,-13.7337583338,-2.23563518556));
#80828=CARTESIAN_POINT('Ctrl Pts',(2.81682319433,-17.6050062023,-0.8922852285));
#80829=CARTESIAN_POINT('Ctrl Pts',(2.73612057106,-17.6939545409,-0.913109799));
#80830=CARTESIAN_POINT('Ctrl Pts',(2.65541794779,-17.7970156063,-0.873654435323));
#80831=CARTESIAN_POINT('Ctrl Pts',(2.60386284676,-17.8824681957,-0.76467039312));
#80832=CARTESIAN_POINT('Ctrl Pts',(2.60303393697,-17.9145456614,-0.631773538218));
#80833=CARTESIAN_POINT('Ctrl Pts',(2.6389185661,-17.8998831563,-0.516206719759));
#80834=CARTESIAN_POINT('Ctrl Pts',(2.72069356298,-17.5533276597,-0.880186363154));
#80835=CARTESIAN_POINT('Ctrl Pts',(2.6490925352,-17.6461138775,-0.891949880027));
#80836=CARTESIAN_POINT('Ctrl Pts',(2.57749150742,-17.7455086998,-0.846656393229));
#80837=CARTESIAN_POINT('Ctrl Pts',(2.52927175372,-17.8208769651,-0.739254396207));
#80838=CARTESIAN_POINT('Ctrl Pts',(2.52277338275,-17.8437268617,-0.610802571589));
#80839=CARTESIAN_POINT('Ctrl Pts',(2.54886029091,-17.8224196827,-0.498071213161));
#80840=CARTESIAN_POINT('Ctrl Pts',(2.61903613259,-17.5055395511,-0.876231590027));
#80841=CARTESIAN_POINT('Ctrl Pts',(2.55466919521,-17.5985472492,-0.878691004377));
#80842=CARTESIAN_POINT('Ctrl Pts',(2.49030225783,-17.6924862639,-0.828223972158));
#80843=CARTESIAN_POINT('Ctrl Pts',(2.44518237715,-17.7592388707,-0.723287859423));
#80844=CARTESIAN_POINT('Ctrl Pts',(2.43496771469,-17.7758070822,-0.600493912801));
#80845=CARTESIAN_POINT('Ctrl Pts',(2.45362336528,-17.7507876789,-0.492143392024));
#80846=CARTESIAN_POINT('Ctrl Pts',(2.51472500067,-17.4617307335,-0.877425549754));
#80847=CARTESIAN_POINT('Ctrl Pts',(2.45636381292,-17.5531913881,-0.871873917305));
#80848=CARTESIAN_POINT('Ctrl Pts',(2.39800262518,-17.6413431422,-0.817577061761));
#80849=CARTESIAN_POINT('Ctrl Pts',(2.35572686839,-17.7007047271,-0.715372409906));
#80850=CARTESIAN_POINT('Ctrl Pts',(2.34300336711,-17.7124820027,-0.59796369171));
#80851=CARTESIAN_POINT('Ctrl Pts',(2.35590021222,-17.685120806,-0.493932666461));
#80852=CARTESIAN_POINT('Ctrl Pts',(2.40817475382,-17.4215258268,-0.882546079144));
#80853=CARTESIAN_POINT('Ctrl Pts',(2.35497665859,-17.5103013085,-0.869969077284));
#80854=CARTESIAN_POINT('Ctrl Pts',(2.30177856336,-17.5925785463,-0.812746623601));
#80855=CARTESIAN_POINT('Ctrl Pts',(2.26216009393,-17.6454952576,-0.713450485069));
#80856=CARTESIAN_POINT('Ctrl Pts',(2.24774850121,-17.6535758491,-0.601299591245));
#80857=CARTESIAN_POINT('Ctrl Pts',(2.25607950621,-17.6248557047,-0.501608274656));
#80858=CARTESIAN_POINT('Ctrl Pts',(2.3,-17.3847397713,-0.890548860981));
#80859=CARTESIAN_POINT('Ctrl Pts',(2.25132255745,-17.4701614043,-0.871965441699));
#80860=CARTESIAN_POINT('Ctrl Pts',(2.20264511489,-17.5467153022,-0.812620072364));
#80861=CARTESIAN_POINT('Ctrl Pts',(2.16552232472,-17.5939868159,-0.716289768713));
#80862=CARTESIAN_POINT('Ctrl Pts',(2.15003006929,-17.5991454925,-0.609120539761));
#80863=CARTESIAN_POINT('Ctrl Pts',(2.15473684211,-17.5697153437,-0.51360402343));
#80864=CARTESIAN_POINT('Ctrl Pts',(2.3,-17.3847397713,-0.890548860981));
#80865=CARTESIAN_POINT('Ctrl Pts',(2.35860678773143,-17.4046696761071,-0.886213123483853));
#80866=CARTESIAN_POINT('Ctrl Pts',(2.41441920873521,-17.4250473814612,-0.883061314204722));
#80867=CARTESIAN_POINT('Ctrl Pts',(2.4674733429775,-17.4457070088102,-0.881183259835285));
#80868=CARTESIAN_POINT('Ctrl Pts',(2.52048805585001,-17.4663512852195,-0.879306600936282));
#80869=CARTESIAN_POINT('Ctrl Pts',(2.5707537492287,-17.4872788063911,-0.878699456805005));
#80870=CARTESIAN_POINT('Ctrl Pts',(2.61828660044749,-17.5083273649553,-0.879426979284592));
#80871=CARTESIAN_POINT('Ctrl Pts',(2.66936649605086,-17.5309466302949,-0.880208791680725));
#80872=CARTESIAN_POINT('Ctrl Pts',(2.71729027753892,-17.5537057811945,-0.882532787234766));
#80873=CARTESIAN_POINT('Ctrl Pts',(2.76201517433812,-17.5763925505084,-0.886462553872128));
#80874=CARTESIAN_POINT('Ctrl Pts',(2.78085443261086,-17.5859487918207,-0.888117871020545));
#80875=CARTESIAN_POINT('Ctrl Pts',(2.79912544466328,-17.5954920661211,-0.890057799537561));
#80876=CARTESIAN_POINT('Ctrl Pts',(2.81682316876698,-17.6050062304749,-0.8922852350963));
#80877=CARTESIAN_POINT('Origin',(3.225,-17.4910283166,-1.37912101035));
#80878=CARTESIAN_POINT('',(0.,-17.6050062358,-0.892285274267));
#80879=CARTESIAN_POINT('Origin',(2.3,-9.41827086707,4.80274328646));
#80880=CARTESIAN_POINT('Origin',(3.5527136788E-15,-19.4793690683,-1.15238185378));
#80881=CARTESIAN_POINT('',(2.33871339884049,-17.3446807699512,1.27988117280792));
#80882=CARTESIAN_POINT('Origin',(-7.3871464501E-14,-19.6855293478,-0.934441634591));
#80883=CARTESIAN_POINT('Origin',(2.33871339630113,-17.1385204882708,1.06194095191296));
#80884=CARTESIAN_POINT('Origin',(0.,-13.3033814002,5.10274328646));
#80885=CARTESIAN_POINT('',(3.225,-17.3446807657,1.27988117305));
#80886=CARTESIAN_POINT('Origin',(0.,4.8773238354,-5.65542016568));
#80887=CARTESIAN_POINT('',(-4.35,-10.4080160928,-5.65542016568));
#80888=CARTESIAN_POINT('',(2.225,-10.4080160928,-5.65542016568));
#80889=CARTESIAN_POINT('',(-4.35,4.8773238354,-5.65542016568));
#80890=CARTESIAN_POINT('',(-4.35,-1.95899712601,-5.65542016568));
#80891=CARTESIAN_POINT('',(0.,4.8773238354,-5.65542016568));
#80892=CARTESIAN_POINT('Origin',(2.225,-10.4080160928,-4.65542016568));
#80893=CARTESIAN_POINT('',(-4.35,-10.8278364558,-5.56302738404));
#80894=CARTESIAN_POINT('',(0.,-10.8278364558,-5.56302738404));
#80895=CARTESIAN_POINT('Origin',(-4.35,-10.4080160928,-4.65542016568));
#80896=CARTESIAN_POINT('Origin',(-7.89279752667E-12,-21.944500351,-0.751472579896));
#80897=CARTESIAN_POINT('',(-3.22521062834,-19.0213954219,-1.7730367033));
#80898=CARTESIAN_POINT('Origin',(-3.22521062833671,-19.1473415307962,-2.04531886881308));
#80899=CARTESIAN_POINT('',(3.22521062098,-19.021395423127,-1.77303669765361));
#80900=CARTESIAN_POINT('Origin',(1.8168799798E-13,-21.8185542421,-0.479190414391));
#80901=CARTESIAN_POINT('Origin',(3.22521057681892,-19.147341526537,-2.04531877209608));
#80902=CARTESIAN_POINT('Origin',(0.,-10.6280930347,-5.65542016568));
#80903=CARTESIAN_POINT('',(-4.35,-19.0213954219,-1.7730367033));
#80904=CARTESIAN_POINT('',(2.225,-19.0213954219,-1.7730367033));
#80905=CARTESIAN_POINT('',(-4.35,-15.7092909613,-3.30507486784));
#80906=CARTESIAN_POINT('',(2.225,-19.0213954219,-1.7730367033));
#80907=CARTESIAN_POINT('Ctrl Pts',(-3.94208068481,-19.1136682541,-1.29488929088));
#80908=CARTESIAN_POINT('Ctrl Pts',(-3.87720138886,-19.1136682521,-1.29488929001));
#80909=CARTESIAN_POINT('Ctrl Pts',(-3.81231526299,-19.1264162883,-1.28286293457));
#80910=CARTESIAN_POINT('Ctrl Pts',(-3.75378202546,-19.1519793642,-1.2587470166));
#80911=CARTESIAN_POINT('Ctrl Pts',(-3.66183898411,-19.2232952003,-1.1914684627));
#80912=CARTESIAN_POINT('Ctrl Pts',(-3.63176681562,-19.3185856291,-1.10157255296));
#80913=CARTESIAN_POINT('Ctrl Pts',(-3.63525640094,-19.3681821774,-1.0547837327));
#80914=CARTESIAN_POINT('Ctrl Pts',(-3.65691135058,-19.4144643621,-1.01112164612));
#80915=CARTESIAN_POINT('Ctrl Pts',(-3.69310716742,-19.4536303609,-0.974172889134));
#80916=CARTESIAN_POINT('Ctrl Pts',(-3.94208056753,-19.1696667267,-1.35424827581));
#80917=CARTESIAN_POINT('Ctrl Pts',(-3.87720126336,-19.159682392,-1.34366478855));
#80918=CARTESIAN_POINT('Ctrl Pts',(-3.81231512925,-19.1657164022,-1.32452150068));
#80919=CARTESIAN_POINT('Ctrl Pts',(-3.7537818851,-19.1888316549,-1.29781086364));
#80920=CARTESIAN_POINT('Ctrl Pts',(-3.66183883688,-19.2642991186,-1.23493306563));
#80921=CARTESIAN_POINT('Ctrl Pts',(-3.63176667561,-19.3794148126,-1.16605211769));
#80922=CARTESIAN_POINT('Ctrl Pts',(-3.63525626847,-19.4422756684,-1.13332358746));
#80923=CARTESIAN_POINT('Ctrl Pts',(-3.65691122872,-19.5037671225,-1.10578347233));
#80924=CARTESIAN_POINT('Ctrl Pts',(-3.69310705761,-19.5585539651,-1.08539296335));
#80925=CARTESIAN_POINT('Ctrl Pts',(-3.89367300212,-19.2061538294,-1.43589684659));
#80926=CARTESIAN_POINT('Ctrl Pts',(-3.83628934638,-19.1945998508,-1.40628312124));
#80927=CARTESIAN_POINT('Ctrl Pts',(-3.77890147363,-19.200140113,-1.37392209869));
#80928=CARTESIAN_POINT('Ctrl Pts',(-3.72658265001,-19.2238991299,-1.34173819539));
#80929=CARTESIAN_POINT('Ctrl Pts',(-3.64204616206,-19.3031632688,-1.28411031556));
#80930=CARTESIAN_POINT('Ctrl Pts',(-3.60813176427,-19.4272069341,-1.24772986945));
#80931=CARTESIAN_POINT('Ctrl Pts',(-3.60653309604,-19.4958412996,-1.23685475493));
#80932=CARTESIAN_POINT('Ctrl Pts',(-3.62053660286,-19.5643236317,-1.23399666395));
#80933=CARTESIAN_POINT('Ctrl Pts',(-3.64775681814,-19.6269188806,-1.23837648486));
#80934=CARTESIAN_POINT('Ctrl Pts',(-3.80930230156,-19.2045641287,-1.50795234761));
#80935=CARTESIAN_POINT('Ctrl Pts',(-3.75987784682,-19.2054688076,-1.4752752232));
#80936=CARTESIAN_POINT('Ctrl Pts',(-3.71045096623,-19.2208549013,-1.44349482057));
#80937=CARTESIAN_POINT('Ctrl Pts',(-3.66483648247,-19.250546929,-1.41519005469));
#80938=CARTESIAN_POINT('Ctrl Pts',(-3.58875746632,-19.3333975541,-1.37014271634));
#80939=CARTESIAN_POINT('Ctrl Pts',(-3.5517176612,-19.4476835822,-1.35267289918));
#80940=CARTESIAN_POINT('Ctrl Pts',(-3.54520036865,-19.5088551603,-1.35199065903));
#80941=CARTESIAN_POINT('Ctrl Pts',(-3.55129886954,-19.5690125364,-1.35930367043));
#80942=CARTESIAN_POINT('Ctrl Pts',(-3.56871476432,-19.6239406117,-1.37338573889));
#80943=CARTESIAN_POINT('Ctrl Pts',(-3.64606474778,-19.1826736184,-1.62180070384));
#80944=CARTESIAN_POINT('Ctrl Pts',(-3.60648671327,-19.1958948229,-1.58929946191));
#80945=CARTESIAN_POINT('Ctrl Pts',(-3.56690777206,-19.2195650029,-1.56181889209));
#80946=CARTESIAN_POINT('Ctrl Pts',(-3.52971312193,-19.2528311608,-1.5413518596));
#80947=CARTESIAN_POINT('Ctrl Pts',(-3.46482449341,-19.3342203712,-1.5169589309));
#80948=CARTESIAN_POINT('Ctrl Pts',(-3.42528173585,-19.4342377637,-1.52616144186));
#80949=CARTESIAN_POINT('Ctrl Pts',(-3.41345573834,-19.4861495298,-1.53932474796));
#80950=CARTESIAN_POINT('Ctrl Pts',(-3.41038172025,-19.5366455777,-1.56008532149));
#80951=CARTESIAN_POINT('Ctrl Pts',(-3.41578699493,-19.5829245944,-1.58670170918));
#80952=CARTESIAN_POINT('Ctrl Pts',(-3.4671692423,-19.1242637155,-1.70186764332));
#80953=CARTESIAN_POINT('Ctrl Pts',(-3.43450859846,-19.1460253867,-1.67828450814));
#80954=CARTESIAN_POINT('Ctrl Pts',(-3.40184766079,-19.1740199682,-1.6606153876));
#80955=CARTESIAN_POINT('Ctrl Pts',(-3.37068117107,-19.2071483267,-1.64991354979));
#80956=CARTESIAN_POINT('Ctrl Pts',(-3.31431449303,-19.2803854864,-1.64335673091));
#80957=CARTESIAN_POINT('Ctrl Pts',(-3.27435380127,-19.3605444526,-1.6655744582));
#80958=CARTESIAN_POINT('Ctrl Pts',(-3.2596011797,-19.4005949558,-1.68366210416));
#80959=CARTESIAN_POINT('Ctrl Pts',(-3.25082353853,-19.4387529418,-1.70783034438));
#80960=CARTESIAN_POINT('Ctrl Pts',(-3.24819011402,-19.473482982,-1.73672177881));
#80961=CARTESIAN_POINT('Ctrl Pts',(-3.38547751269,-19.0935072946,-1.73183570145));
#80962=CARTESIAN_POINT('Ctrl Pts',(-3.35512154584,-19.1165078816,-1.71264403289));
#80963=CARTESIAN_POINT('Ctrl Pts',(-3.32476535702,-19.1442415397,-1.69929570405));
#80964=CARTESIAN_POINT('Ctrl Pts',(-3.29564414506,-19.1757570958,-1.69255186303));
#80965=CARTESIAN_POINT('Ctrl Pts',(-3.24233287408,-19.2436848784,-1.6927859443));
#80966=CARTESIAN_POINT('Ctrl Pts',(-3.20268173876,-19.3157439579,-1.71926217841));
#80967=CARTESIAN_POINT('Ctrl Pts',(-3.18722650592,-19.3513922741,-1.73877210954));
#80968=CARTESIAN_POINT('Ctrl Pts',(-3.17680955904,-19.3851723952,-1.76371055191));
#80969=CARTESIAN_POINT('Ctrl Pts',(-3.17165790098,-19.4158555881,-1.79287228805));
#80970=CARTESIAN_POINT('Ctrl Pts',(-3.30422173516,-19.0589182003,-1.75568026745));
#80971=CARTESIAN_POINT('Ctrl Pts',(-3.27596559888,-19.0824576484,-1.74095218972));
#80972=CARTESIAN_POINT('Ctrl Pts',(-3.24770931985,-19.1094046865,-1.73175819756));
#80973=CARTESIAN_POINT('Ctrl Pts',(-3.22045811805,-19.1389197877,-1.72861076563));
#80974=CARTESIAN_POINT('Ctrl Pts',(-3.16997041597,-19.2009235168,-1.73461137249));
#80975=CARTESIAN_POINT('Ctrl Pts',(-3.13070946984,-19.2644437842,-1.7638921058));
#80976=CARTESIAN_POINT('Ctrl Pts',(-3.11468881656,-19.2954758049,-1.78403275906));
#80977=CARTESIAN_POINT('Ctrl Pts',(-3.10287409283,-19.3246516908,-1.80892678684));
#80978=CARTESIAN_POINT('Ctrl Pts',(-3.09553404662,-19.351046075,-1.83754968546));
#80979=CARTESIAN_POINT('Ctrl Pts',(-3.22521062834,-19.0213954219,-1.7730367033));
#80980=CARTESIAN_POINT('Ctrl Pts',(-3.19874622208,-19.044347457,-1.76242007146));
#80981=CARTESIAN_POINT('Ctrl Pts',(-3.17228172271,-19.0696431519,-1.75686997245));
#80982=CARTESIAN_POINT('Ctrl Pts',(-3.14663842378,-19.096571511,-1.75671868196));
#80983=CARTESIAN_POINT('Ctrl Pts',(-3.09863298495,-19.1519725754,-1.76722316791));
#80984=CARTESIAN_POINT('Ctrl Pts',(-3.05987676099,-19.2070352425,-1.79804851641));
#80985=CARTESIAN_POINT('Ctrl Pts',(-3.04348517182,-19.2336251131,-1.81822356982));
#80986=CARTESIAN_POINT('Ctrl Pts',(-3.03060394682,-19.2584238423,-1.84251642021));
#80987=CARTESIAN_POINT('Ctrl Pts',(-3.02151311497,-19.2807402375,-1.87007016525));
#80988=CARTESIAN_POINT('Ctrl Pts',(-3.22521062834,-19.0213954219,-1.7730367033));
#80989=CARTESIAN_POINT('Ctrl Pts',(-3.24772444597292,-19.0320873489464,
-1.76809107416998));
#80990=CARTESIAN_POINT('Ctrl Pts',(-3.27028135195154,-19.0424883596232,
-1.76251507821921));
#80991=CARTESIAN_POINT('Ctrl Pts',(-3.2928662202311,-19.0525235172448,-1.75634535752002));
#80992=CARTESIAN_POINT('Ctrl Pts',(-3.30614125710113,-19.0584220279545,
-1.75271889095197));
#80993=CARTESIAN_POINT('Ctrl Pts',(-3.31942721657902,-19.064194344846,-1.74888731162803));
#80994=CARTESIAN_POINT('Ctrl Pts',(-3.33272883036821,-19.0698263727899,
-1.74485946562232));
#80995=CARTESIAN_POINT('Ctrl Pts',(-3.35069467910696,-19.0774332815256,
-1.73941924812477));
#80996=CARTESIAN_POINT('Ctrl Pts',(-3.36868359493464,-19.0847837961097,
-1.7336209772335));
#80997=CARTESIAN_POINT('Ctrl Pts',(-3.38669558519312,-19.0918460227535,
-1.72749125982607));
#80998=CARTESIAN_POINT('Ctrl Pts',(-3.39570158032236,-19.0953771360754,
-1.72442640112235));
#80999=CARTESIAN_POINT('Ctrl Pts',(-3.40431105974672,-19.0986840050788,
-1.72141745792359));
#81000=CARTESIAN_POINT('Ctrl Pts',(-3.41311378877424,-19.1020038683847,
-1.71825795819223));
#81001=CARTESIAN_POINT('Ctrl Pts',(-3.42128496560172,-19.1050855479446,
-1.71532513691481));
#81002=CARTESIAN_POINT('Ctrl Pts',(-3.4296228773541,-19.1081784742,-1.71226240285957));
#81003=CARTESIAN_POINT('Ctrl Pts',(-3.43860354554371,-19.111447523279,-1.70886309082487));
#81004=CARTESIAN_POINT('Ctrl Pts',(-3.43929766352361,-19.1117001888596,
-1.70860035718938));
#81005=CARTESIAN_POINT('Ctrl Pts',(-3.43999562251229,-19.1119538925657,
-1.70833559083555));
#81006=CARTESIAN_POINT('Ctrl Pts',(-3.44069764286074,-19.1122087031213,
-1.70806868482413));
#81007=CARTESIAN_POINT('Ctrl Pts',(-3.4661961713137,-19.1214638396967,-1.69837422149201));
#81008=CARTESIAN_POINT('Ctrl Pts',(-3.49111096758992,-19.130046569157,-1.68809291431738));
#81009=CARTESIAN_POINT('Ctrl Pts',(-3.51542366771508,-19.1379196799265,
-1.67729049519577));
#81010=CARTESIAN_POINT('Ctrl Pts',(-3.52843047035992,-19.1421316348904,
-1.67151141953251));
#81011=CARTESIAN_POINT('Ctrl Pts',(-3.5412644137341,-19.1461398298069,-1.66558344175602));
#81012=CARTESIAN_POINT('Ctrl Pts',(-3.55391844673925,-19.1499344256496,
-1.65951839712039));
#81013=CARTESIAN_POINT('Ctrl Pts',(-3.57553475391646,-19.1564165605797,
-1.64915775811827));
#81014=CARTESIAN_POINT('Ctrl Pts',(-3.59663453427806,-19.1622797228512,
-1.63839506557308));
#81015=CARTESIAN_POINT('Ctrl Pts',(-3.6171612881736,-19.1674726055405,-1.62725042901185));
#81016=CARTESIAN_POINT('Ctrl Pts',(-3.62193563094114,-19.1686804244698,
-1.62465828437789));
#81017=CARTESIAN_POINT('Ctrl Pts',(-3.62667885762862,-19.1698518313957,
-1.62204542253218));
#81018=CARTESIAN_POINT('Ctrl Pts',(-3.63138996488376,-19.1709858783566,
-1.61941203301298));
#81019=CARTESIAN_POINT('Ctrl Pts',(-3.63591728936824,-19.1720756855493,
-1.61688137340329));
#81020=CARTESIAN_POINT('Ctrl Pts',(-3.64041501866186,-19.1731310191457,
-1.61433172446812));
#81021=CARTESIAN_POINT('Ctrl Pts',(-3.64488244879203,-19.1741521328984,
-1.61176395184423));
#81022=CARTESIAN_POINT('Ctrl Pts',(-3.64540287798236,-19.1742710866118,
-1.61146482151904));
#81023=CARTESIAN_POINT('Ctrl Pts',(-3.64592666721413,-19.1743904272115,
-1.61116326385945));
#81024=CARTESIAN_POINT('Ctrl Pts',(-3.64643164572595,-19.1745051343925,
-1.61087208357338));
#81025=CARTESIAN_POINT('Ctrl Pts',(-3.64916151036296,-19.1751252302375,
-1.60929799131533));
#81026=CARTESIAN_POINT('Ctrl Pts',(-3.65147817017146,-19.1756436403,-1.60795197344029));
#81027=CARTESIAN_POINT('Ctrl Pts',(-3.65436417184066,-19.1762780377711,
-1.60626030924236));
#81028=CARTESIAN_POINT('Ctrl Pts',(-3.6555270412225,-19.1765336583422,-1.60557867952568));
#81029=CARTESIAN_POINT('Ctrl Pts',(-3.65678220408794,-19.1768077686339,
-1.60484061205229));
#81030=CARTESIAN_POINT('Ctrl Pts',(-3.6581932018563,-19.1771128584525,-1.60400694268519));
#81031=CARTESIAN_POINT('Ctrl Pts',(-3.6742877471575,-19.1805928653082,-1.59449769348881));
#81032=CARTESIAN_POINT('Ctrl Pts',(-3.68966114213862,-19.1835569868908,
-1.58492691989271));
#81033=CARTESIAN_POINT('Ctrl Pts',(-3.70433248725225,-19.1860351129862,
-1.57533948257634));
#81034=CARTESIAN_POINT('Ctrl Pts',(-3.72775122383417,-19.1899907545306,
-1.56003579588171));
#81035=CARTESIAN_POINT('Ctrl Pts',(-3.74937546375535,-19.1927024574446,
-1.54469005867433));
#81036=CARTESIAN_POINT('Ctrl Pts',(-3.76916732977652,-19.1942216676716,
-1.52951153228472));
#81037=CARTESIAN_POINT('Ctrl Pts',(-3.78526285634382,-19.1954571493864,
-1.51716775557892));
#81038=CARTESIAN_POINT('Ctrl Pts',(-3.80015850434429,-19.1959035366658,
-1.50492975762664));
#81039=CARTESIAN_POINT('Ctrl Pts',(-3.81385444633577,-19.1956091287661,
-1.49289560584265));
#81040=CARTESIAN_POINT('Ctrl Pts',(-3.82070241733151,-19.1954619248163,
-1.48687852995065));
#81041=CARTESIAN_POINT('Ctrl Pts',(-3.82725045890622,-19.1951299577511,
-1.48091230974744));
#81042=CARTESIAN_POINT('Ctrl Pts',(-3.83349856779365,-19.1946218274872,
-1.47500806817809));
#81043=CARTESIAN_POINT('Ctrl Pts',(-3.83662262223736,-19.1943677623552,
-1.47205594739341));
#81044=CARTESIAN_POINT('Ctrl Pts',(-3.83967169317361,-19.1940696838623,
-1.4691193204789));
#81045=CARTESIAN_POINT('Ctrl Pts',(-3.84264577876859,-19.1937288068363,
-1.46619944749653));
#81046=CARTESIAN_POINT('Ctrl Pts',(-3.84427530786577,-19.1935420371504,
-1.46459962199289));
#81047=CARTESIAN_POINT('Ctrl Pts',(-3.84558853566292,-19.1933790227199,
-1.46329651293835));
#81048=CARTESIAN_POINT('Ctrl Pts',(-3.84707135142737,-19.1931828234745,
-1.46181166623411));
#81049=CARTESIAN_POINT('Ctrl Pts',(-3.84829485186967,-19.1930209356195,
-1.46058649002345));
#81050=CARTESIAN_POINT('Ctrl Pts',(-3.84963382677702,-19.192836412323,-1.45923751109255));
#81051=CARTESIAN_POINT('Ctrl Pts',(-3.85134307689286,-19.1925790828302,
-1.45749132327324));
#81052=CARTESIAN_POINT('Ctrl Pts',(-3.86750161951162,-19.1901463963916,
-1.44098358690551));
#81053=CARTESIAN_POINT('Ctrl Pts',(-3.88146163353687,-19.1863177603114,
-1.42482655476048));
#81054=CARTESIAN_POINT('Ctrl Pts',(-3.8932591846746,-19.1812263066711,-1.40917519080981));
#81055=CARTESIAN_POINT('Ctrl Pts',(-3.90503537655242,-19.1761440710185,
-1.39355216337972));
#81056=CARTESIAN_POINT('Ctrl Pts',(-3.91466188565638,-19.1698056445851,
-1.37843033478599));
#81057=CARTESIAN_POINT('Ctrl Pts',(-3.9221775305533,-19.1623488557789,-1.36395201741712));
#81058=CARTESIAN_POINT('Ctrl Pts',(-3.92828814640728,-19.1562860930322,
-1.35218038146748));
#81059=CARTESIAN_POINT('Ctrl Pts',(-3.93300430884911,-19.1494837461493,
-1.34083267762417));
#81060=CARTESIAN_POINT('Ctrl Pts',(-3.93631580667821,-19.1420117931894,
-1.33000380907411));
#81061=CARTESIAN_POINT('Ctrl Pts',(-3.93919658915514,-19.1355116919464,
-1.320583414928));
#81062=CARTESIAN_POINT('Ctrl Pts',(-3.94101431043189,-19.1285042561885,
-1.31155499950984));
#81063=CARTESIAN_POINT('Ctrl Pts',(-3.94173213759005,-19.1210385047908,
-1.30300892857622));
#81064=CARTESIAN_POINT('Ctrl Pts',(-3.94196382899028,-19.1186288015978,
-1.30025053316233));
#81065=CARTESIAN_POINT('Ctrl Pts',(-3.9420806794518,-19.1161714145093,-1.29754266791182));
#81066=CARTESIAN_POINT('Ctrl Pts',(-3.94208068480999,-19.1136682541,-1.29488929088));
#81067=CARTESIAN_POINT('Origin',(2.225,-18.895449313,-1.50075453779));
#81068=CARTESIAN_POINT('Origin',(-4.35,-18.895449313,-1.50075453779));
#81069=CARTESIAN_POINT('Ctrl Pts',(3.22521062098,-19.0213954214,-1.77303668325));
#81070=CARTESIAN_POINT('Ctrl Pts',(3.19874621439,-19.0443474533,-1.7624200523));
#81071=CARTESIAN_POINT('Ctrl Pts',(3.1722817147,-19.0696431447,-1.75686995397));
#81072=CARTESIAN_POINT('Ctrl Pts',(3.14663841544,-19.0965715001,-1.75671866391));
#81073=CARTESIAN_POINT('Ctrl Pts',(3.09863297604,-19.1519725569,-1.76722315022));
#81074=CARTESIAN_POINT('Ctrl Pts',(3.05987675166,-19.2070352164,-1.79804849807));
#81075=CARTESIAN_POINT('Ctrl Pts',(3.04348516232,-19.2336250834,-1.81822355091));
#81076=CARTESIAN_POINT('Ctrl Pts',(3.03060393721,-19.2584238091,-1.84251640048));
#81077=CARTESIAN_POINT('Ctrl Pts',(3.0215131053,-19.2807402012,-1.87007014451));
#81078=CARTESIAN_POINT('Ctrl Pts',(3.31887229845,-19.0658758373,-1.75246199623));
#81079=CARTESIAN_POINT('Ctrl Pts',(3.29028393291,-19.089524209,-1.73697155779));
#81080=CARTESIAN_POINT('Ctrl Pts',(3.2616954154,-19.1167774494,-1.72710190069));
#81081=CARTESIAN_POINT('Ctrl Pts',(3.23414607027,-19.1467721985,-1.72339891277));
#81082=CARTESIAN_POINT('Ctrl Pts',(3.18319809785,-19.2100002284,-1.72856439386));
#81083=CARTESIAN_POINT('Ctrl Pts',(3.14384356469,-19.2750887468,-1.75755872073));
#81084=CARTESIAN_POINT('Ctrl Pts',(3.12789169205,-19.3069444531,-1.77769299668));
#81085=CARTESIAN_POINT('Ctrl Pts',(3.11627472338,-19.3369319732,-1.80269849863));
#81086=CARTESIAN_POINT('Ctrl Pts',(3.10925931489,-19.3640825186,-1.83151964554));
#81087=CARTESIAN_POINT('Ctrl Pts',(3.41573924533,-19.1062581898,-1.72274306856));
#81088=CARTESIAN_POINT('Ctrl Pts',(3.38458474557,-19.1289876528,-1.70187932147));
#81089=CARTESIAN_POINT('Ctrl Pts',(3.3534299924,-19.1569566778,-1.68696468886));
#81090=CARTESIAN_POINT('Ctrl Pts',(3.32359852403,-19.1891775057,-1.67885768802));
#81091=CARTESIAN_POINT('Ctrl Pts',(3.26921872731,-19.2592689985,-1.67689652144));
#81092=CARTESIAN_POINT('Ctrl Pts',(3.22943107032,-19.334526867,-1.70228745871));
#81093=CARTESIAN_POINT('Ctrl Pts',(3.21419840626,-19.3719160959,-1.72154573558));
#81094=CARTESIAN_POINT('Ctrl Pts',(3.20432114725,-19.4074383872,-1.74648676951));
#81095=CARTESIAN_POINT('Ctrl Pts',(3.20000833496,-19.4397458552,-1.77583596615));
#81096=CARTESIAN_POINT('Ctrl Pts',(3.51291896248,-19.1413289289,-1.68469422833));
#81097=CARTESIAN_POINT('Ctrl Pts',(3.4789462662,-19.1620682059,-1.65842751755));
#81098=CARTESIAN_POINT('Ctrl Pts',(3.44497324706,-19.1899424465,-1.63811566301));
#81099=CARTESIAN_POINT('Ctrl Pts',(3.41264252321,-19.2237987455,-1.62501908412));
#81100=CARTESIAN_POINT('Ctrl Pts',(3.35453777244,-19.2998586458,-1.61444987467));
#81101=CARTESIAN_POINT('Ctrl Pts',(3.31440978178,-19.3847471634,-1.63435949598));
#81102=CARTESIAN_POINT('Ctrl Pts',(3.30006468822,-19.4274328561,-1.65176034228));
#81103=CARTESIAN_POINT('Ctrl Pts',(3.2922329623,-19.4682507262,-1.67564817155));
#81104=CARTESIAN_POINT('Ctrl Pts',(3.29105041121,-19.5054576982,-1.70454430458));
#81105=CARTESIAN_POINT('Ctrl Pts',(3.69283515033,-19.1942585079,-1.59547606027));
#81106=CARTESIAN_POINT('Ctrl Pts',(3.65105292983,-19.2042463076,-1.56116545001));
#81107=CARTESIAN_POINT('Ctrl Pts',(3.60926958339,-19.2259574623,-1.5312745857));
#81108=CARTESIAN_POINT('Ctrl Pts',(3.57016835315,-19.258655952,-1.50808432834));
#81109=CARTESIAN_POINT('Ctrl Pts',(3.50264897247,-19.341385442,-1.47818397612));
#81110=CARTESIAN_POINT('Ctrl Pts',(3.46343047149,-19.446443377,-1.48240833377));
#81111=CARTESIAN_POINT('Ctrl Pts',(3.45265831019,-19.501492664,-1.49338380489));
#81112=CARTESIAN_POINT('Ctrl Pts',(3.45153181921,-19.5552861337,-1.51230581401));
#81113=CARTESIAN_POINT('Ctrl Pts',(3.4596034448,-19.6046311185,-1.53737756014));
#81114=CARTESIAN_POINT('Ctrl Pts',(3.84656205857,-19.2016706385,-1.47236182198));
#81115=CARTESIAN_POINT('Ctrl Pts',(3.79361941084,-19.1984204408,-1.44241491043));
#81116=CARTESIAN_POINT('Ctrl Pts',(3.74067352441,-19.2105079959,-1.41147096078));
#81117=CARTESIAN_POINT('Ctrl Pts',(3.69209672656,-19.2381656965,-1.38207884));
#81118=CARTESIAN_POINT('Ctrl Pts',(3.61228551508,-19.3195355041,-1.33161378879));
#81119=CARTESIAN_POINT('Ctrl Pts',(3.57663385678,-19.4363429733,-1.30393743154));
#81120=CARTESIAN_POINT('Ctrl Pts',(3.57229261138,-19.4994985456,-1.29737816529));
#81121=CARTESIAN_POINT('Ctrl Pts',(3.58188180677,-19.5617860447,-1.29857025048));
#81122=CARTESIAN_POINT('Ctrl Pts',(3.60362130644,-19.6185190275,-1.30670041311));
#81123=CARTESIAN_POINT('Ctrl Pts',(3.90904845134,-19.1941294458,-1.40944736849));
#81124=CARTESIAN_POINT('Ctrl Pts',(3.84915166913,-19.1827174766,-1.3858993254));
#81125=CARTESIAN_POINT('Ctrl Pts',(3.78924978079,-19.1880794399,-1.35771639625));
#81126=CARTESIAN_POINT('Ctrl Pts',(3.734849471,-19.2113827948,-1.32722087289));
#81127=CARTESIAN_POINT('Ctrl Pts',(3.64784164979,-19.2891777792,-1.2678039989));
#81128=CARTESIAN_POINT('Ctrl Pts',(3.61523677607,-19.410557809,-1.22097222058));
#81129=CARTESIAN_POINT('Ctrl Pts',(3.61535581634,-19.4775453686,-1.20309998859));
#81130=CARTESIAN_POINT('Ctrl Pts',(3.63193270005,-19.5440428904,-1.19235380158));
#81131=CARTESIAN_POINT('Ctrl Pts',(3.66216118733,-19.6043893474,-1.18881869517));
#81132=CARTESIAN_POINT('Ctrl Pts',(3.94208066889,-19.1605170316,-1.34454941301));
#81133=CARTESIAN_POINT('Ctrl Pts',(3.87720137211,-19.1521640582,-1.33569518932));
#81134=CARTESIAN_POINT('Ctrl Pts',(3.81231524539,-19.1592950835,-1.31771475291));
#81135=CARTESIAN_POINT('Ctrl Pts',(3.7537820072,-19.1828102836,-1.29142806828));
#81136=CARTESIAN_POINT('Ctrl Pts',(3.66183896524,-19.2575993834,-1.2278312033));
#81137=CARTESIAN_POINT('Ctrl Pts',(3.63176679768,-19.3694757596,-1.15551654247));
#81138=CARTESIAN_POINT('Ctrl Pts',(3.6352563839,-19.4301693195,-1.12049065176));
#81139=CARTESIAN_POINT('Ctrl Pts',(3.65691133475,-19.4891756884,-1.09031631225));
#81140=CARTESIAN_POINT('Ctrl Pts',(3.69310715296,-19.5414102009,-1.06722029503));
#81141=CARTESIAN_POINT('Ctrl Pts',(3.94208066889,-19.1136682429,-1.29488929392));
#81142=CARTESIAN_POINT('Ctrl Pts',(3.87720137211,-19.1136682429,-1.29488929392));
#81143=CARTESIAN_POINT('Ctrl Pts',(3.81231524539,-19.1264162816,-1.28286293996));
#81144=CARTESIAN_POINT('Ctrl Pts',(3.7537820072,-19.15197936,-1.258747024));
#81145=CARTESIAN_POINT('Ctrl Pts',(3.66183896524,-19.223295201,-1.19146847485));
#81146=CARTESIAN_POINT('Ctrl Pts',(3.63176679768,-19.3185856331,-1.10157257054));
#81147=CARTESIAN_POINT('Ctrl Pts',(3.6352563839,-19.3681821823,-1.05478375298));
#81148=CARTESIAN_POINT('Ctrl Pts',(3.65691133475,-19.4144643672,-1.01112166887));
#81149=CARTESIAN_POINT('Ctrl Pts',(3.69310715296,-19.4536303653,-0.974172913988));
#81150=CARTESIAN_POINT('Ctrl Pts',(3.94208066889,-19.1136682429,-1.29488929392));
#81151=CARTESIAN_POINT('Ctrl Pts',(3.94208066889,-19.1213935505688,-1.30307818651436));
#81152=CARTESIAN_POINT('Ctrl Pts',(3.94100547669129,-19.1286717217873,-1.31174595495687));
#81153=CARTESIAN_POINT('Ctrl Pts',(3.93888533927808,-19.1354553093415,-1.32081024079185));
#81154=CARTESIAN_POINT('Ctrl Pts',(3.93647580748577,-19.1431648425896,-1.33111178292677));
#81155=CARTESIAN_POINT('Ctrl Pts',(3.93271701109205,-19.1502369295743,-1.34192670736547));
#81156=CARTESIAN_POINT('Ctrl Pts',(3.92760682263043,-19.1566129713568,-1.35318346930748));
#81157=CARTESIAN_POINT('Ctrl Pts',(3.92418283215508,-19.160885124233,-1.360725861523));
#81158=CARTESIAN_POINT('Ctrl Pts',(3.9201493937171,-19.1648460281206,-1.36847027143733));
#81159=CARTESIAN_POINT('Ctrl Pts',(3.91550264816662,-19.1684724142439,-1.37639078404052));
#81160=CARTESIAN_POINT('Ctrl Pts',(3.90804917436684,-19.1742892108954,-1.38909544637408));
#81161=CARTESIAN_POINT('Ctrl Pts',(3.89901903058555,-19.1792414439433,-1.40224844154212));
#81162=CARTESIAN_POINT('Ctrl Pts',(3.88841602773183,-19.1832466824446,-1.41573314937972));
#81163=CARTESIAN_POINT('Ctrl Pts',(3.88311452630497,-19.1852493016953,-1.42247550329852));
#81164=CARTESIAN_POINT('Ctrl Pts',(3.87742029106335,-19.1870154827717,-1.42930055218608));
#81165=CARTESIAN_POINT('Ctrl Pts',(3.87133657591744,-19.1885374657265,-1.43619304513296));
#81166=CARTESIAN_POINT('Ctrl Pts',(3.86981564713096,-19.1889179614652,-1.43791616836967));
#81167=CARTESIAN_POINT('Ctrl Pts',(3.86827038117942,-19.1892832054479,-1.43964351009775));
#81168=CARTESIAN_POINT('Ctrl Pts',(3.86670084145296,-19.1896330966815,-1.44137483565682));
#81169=CARTESIAN_POINT('Ctrl Pts',(3.8655236866581,-19.1898955151067,-1.44267332982611));
#81170=CARTESIAN_POINT('Ctrl Pts',(3.86433287805002,-19.1901492977467,-1.44397406482564));
#81171=CARTESIAN_POINT('Ctrl Pts',(3.86312844582096,-19.1903944045625,-1.44527694032169));
#81172=CARTESIAN_POINT('Ctrl Pts',(3.862820679794,-19.1904570361901,-1.44560986134903));
#81173=CARTESIAN_POINT('Ctrl Pts',(3.86251175890315,-19.1905191679455,-1.44594322302894));
#81174=CARTESIAN_POINT('Ctrl Pts',(3.86219392101923,-19.1905822995663,-1.44628533346112));
#81175=CARTESIAN_POINT('Ctrl Pts',(3.86025365777512,-19.1909676908916,-1.44837377014711));
#81176=CARTESIAN_POINT('Ctrl Pts',(3.85806644600599,-19.1913687357961,-1.45069123929498));
#81177=CARTESIAN_POINT('Ctrl Pts',(3.85604432062616,-19.191709360832,-1.45280045778785));
#81178=CARTESIAN_POINT('Ctrl Pts',(3.85450871101005,-19.191968032765,-1.45440220624145));
#81179=CARTESIAN_POINT('Ctrl Pts',(3.85306958970826,-19.1921930668317,-1.45588408049776));
#81180=CARTESIAN_POINT('Ctrl Pts',(3.85192149540446,-19.1923651413728,-1.4570580131927));
#81181=CARTESIAN_POINT('Ctrl Pts',(3.84000156819927,-19.1941516810292,-1.46924620385017));
#81182=CARTESIAN_POINT('Ctrl Pts',(3.82674560647647,-19.1952061457583,-1.48176044555951));
#81183=CARTESIAN_POINT('Ctrl Pts',(3.81213319489629,-19.1954494376464,-1.49450176335358));
#81184=CARTESIAN_POINT('Ctrl Pts',(3.79903811735577,-19.1956674664175,-1.50592003908214));
#81185=CARTESIAN_POINT('Ctrl Pts',(3.78485595743091,-19.1952349372733,-1.51751939205409));
#81186=CARTESIAN_POINT('Ctrl Pts',(3.7695910419071,-19.194107055607,-1.52921902692643));
#81187=CARTESIAN_POINT('Ctrl Pts',(3.7565253000351,-19.1931416646952,-1.5392331281509));
#81188=CARTESIAN_POINT('Ctrl Pts',(3.74266668945736,-19.1916672093887,-1.54932575197495));
#81189=CARTESIAN_POINT('Ctrl Pts',(3.72802076749187,-19.1896517157489,-1.55943647497926));
#81190=CARTESIAN_POINT('Ctrl Pts',(3.72456428981541,-19.1891760537326,-1.56182263328596));
#81191=CARTESIAN_POINT('Ctrl Pts',(3.72106378520022,-19.1886701887527,-1.56420988691519));
#81192=CARTESIAN_POINT('Ctrl Pts',(3.71751888906543,-19.1881335052326,-1.56659763778155));
#81193=CARTESIAN_POINT('Ctrl Pts',(3.71330638744845,-19.187495748833,-1.56943507053078));
#81194=CARTESIAN_POINT('Ctrl Pts',(3.70903224195872,-19.1868146164059,-1.57227260091458));
#81195=CARTESIAN_POINT('Ctrl Pts',(3.70469541744933,-19.186088937794,-1.57510915486651));
#81196=CARTESIAN_POINT('Ctrl Pts',(3.69947554797873,-19.1852154997234,-1.57852327534644));
#81197=CARTESIAN_POINT('Ctrl Pts',(3.69416478422523,-19.1842774765037,-1.58193601403412));
#81198=CARTESIAN_POINT('Ctrl Pts',(3.68876462401809,-19.1832745138145,-1.5853441458696));
#81199=CARTESIAN_POINT('Ctrl Pts',(3.68382123617734,-19.18235638669,-1.58846400099036));
#81200=CARTESIAN_POINT('Ctrl Pts',(3.6788023431847,-19.1813837619823,-1.59158029219753));
#81201=CARTESIAN_POINT('Ctrl Pts',(3.67370794478431,-19.180356266959,-1.59469101971277));
#81202=CARTESIAN_POINT('Ctrl Pts',(3.67073041486801,-19.1797557255544,-1.59650915082662));
#81203=CARTESIAN_POINT('Ctrl Pts',(3.66714567548281,-19.1790161110558,-1.59867569128098));
#81204=CARTESIAN_POINT('Ctrl Pts',(3.66397164750743,-19.1783453305908,-1.60057321268494));
#81205=CARTESIAN_POINT('Ctrl Pts',(3.66171507915125,-19.1778684406632,-1.60192225144219));
#81206=CARTESIAN_POINT('Ctrl Pts',(3.65966673795962,-19.1774276304334,-1.60313640354589));
#81207=CARTESIAN_POINT('Ctrl Pts',(3.65819753823164,-19.1771090035203,-1.60400401677888));
#81208=CARTESIAN_POINT('Ctrl Pts',(3.64039240413172,-19.1732475850841,-1.61451856402934));
#81209=CARTESIAN_POINT('Ctrl Pts',(3.62101617997714,-19.1686042876446,-1.62534500838972));
#81210=CARTESIAN_POINT('Ctrl Pts',(3.60005819365773,-19.1630368846854,-1.63633013020167));
#81211=CARTESIAN_POINT('Ctrl Pts',(3.58772155265733,-19.1597597066891,-1.64279637662794));
#81212=CARTESIAN_POINT('Ctrl Pts',(3.57483761059001,-19.1561624128229,-1.64931684911771));
#81213=CARTESIAN_POINT('Ctrl Pts',(3.56140967667491,-19.1522164502068,-1.65585401051031));
#81214=CARTESIAN_POINT('Ctrl Pts',(3.54328975021503,-19.1468916881943,-1.66467538872375));
#81215=CARTESIAN_POINT('Ctrl Pts',(3.52417557959925,-19.1409320159719,-1.6735269623939));
#81216=CARTESIAN_POINT('Ctrl Pts',(3.50406715587264,-19.1342760287435,-1.68229465773077));
#81217=CARTESIAN_POINT('Ctrl Pts',(3.49401294400934,-19.1309480351293,-1.6866785053992));
#81218=CARTESIAN_POINT('Ctrl Pts',(3.48371016856777,-19.127446123929,-1.69104102801887));
#81219=CARTESIAN_POINT('Ctrl Pts',(3.4731588282599,-19.1237639580102,-1.69536587194679));
#81220=CARTESIAN_POINT('Ctrl Pts',(3.46788315810597,-19.1219228750509,-1.69752829391075));
#81221=CARTESIAN_POINT('Ctrl Pts',(3.4625453467471,-19.1200367283689,-1.69968129414405));
#81222=CARTESIAN_POINT('Ctrl Pts',(3.45714539413792,-19.1181048645026,-1.70182267645465));
#81223=CARTESIAN_POINT('Ctrl Pts',(3.4533090413257,-19.1167323873879,-1.70334400425951));
#81224=CARTESIAN_POINT('Ctrl Pts',(3.44887872706727,-19.1151331100681,-1.70507852129202));
#81225=CARTESIAN_POINT('Ctrl Pts',(3.4450536379338,-19.1137401653745,-1.70655720634178));
#81226=CARTESIAN_POINT('Ctrl Pts',(3.44349462892571,-19.1131724365584,-1.7071598807455));
#81227=CARTESIAN_POINT('Ctrl Pts',(3.44203611491941,-19.112639349284,-1.70772063898745));
#81228=CARTESIAN_POINT('Ctrl Pts',(3.44075911260381,-19.1121714939915,-1.70820976488904));
#81229=CARTESIAN_POINT('Ctrl Pts',(3.40930114555862,-19.1006462397352,-1.72025900419344));
#81230=CARTESIAN_POINT('Ctrl Pts',(3.37748624251822,-19.0881949128326,-1.73126263301116));
#81231=CARTESIAN_POINT('Ctrl Pts',(3.34544565726412,-19.0748903340227,-1.74118643674611));
#81232=CARTESIAN_POINT('Ctrl Pts',(3.3214711174372,-19.0649351115439,-1.74861197613596));
#81233=CARTESIAN_POINT('Ctrl Pts',(3.29736784319479,-19.0545004799544,-1.75543361106648));
#81234=CARTESIAN_POINT('Ctrl Pts',(3.27320280002085,-19.0436061687958,-1.76161889253852));
#81235=CARTESIAN_POINT('Ctrl Pts',(3.25722224928904,-19.036401667198,-1.76570927233396));
#81236=CARTESIAN_POINT('Ctrl Pts',(3.2412149341913,-19.0289959526638,-1.76952101126774));
#81237=CARTESIAN_POINT('Ctrl Pts',(3.22521062098,-19.0213954214,-1.77303668325));
#81238=CARTESIAN_POINT('Origin',(2.225,-18.895449313,-1.50075453779));
#81239=CARTESIAN_POINT('Origin',(4.35,-19.0026826744,-1.32221314666));
#81240=CARTESIAN_POINT('Origin',(4.35,-19.0026826744,-1.32221314666));
#81241=CARTESIAN_POINT('Origin',(-4.4408920985E-16,-17.4373752488,-0.853039529372));
#81242=CARTESIAN_POINT('',(2.225,-19.0254782583,-1.22484599945));
#81243=CARTESIAN_POINT('Ctrl Pts',(2.33871339945,-17.3446807781,1.27988117638));
#81244=CARTESIAN_POINT('Ctrl Pts',(2.30368136515,-17.3797447944,1.24671241384));
#81245=CARTESIAN_POINT('Ctrl Pts',(2.26864933085,-17.4046242188,1.20277711487));
#81246=CARTESIAN_POINT('Ctrl Pts',(2.23651128313,-17.4163976498,1.15078915349));
#81247=CARTESIAN_POINT('Ctrl Pts',(2.21010974441,-17.4140237598,1.09534672271));
#81248=CARTESIAN_POINT('Ctrl Pts',(2.19100518783,-17.3987921062,1.04094168425));
#81249=CARTESIAN_POINT('Ctrl Pts',(2.46656348386,-17.3868132718,1.24002603887));
#81250=CARTESIAN_POINT('Ctrl Pts',(2.42844748972,-17.4291544248,1.20768003199));
#81251=CARTESIAN_POINT('Ctrl Pts',(2.39033149557,-17.4606361606,1.16135256604));
#81252=CARTESIAN_POINT('Ctrl Pts',(2.35591441479,-17.4771747692,1.10419328591));
#81253=CARTESIAN_POINT('Ctrl Pts',(2.32881040502,-17.477098625,1.04217993252));
#81254=CARTESIAN_POINT('Ctrl Pts',(2.31078053575,-17.4619464725,0.981200951561));
#81255=CARTESIAN_POINT('Ctrl Pts',(2.59487812775,-17.4343620581,1.20661041268));
#81256=CARTESIAN_POINT('Ctrl Pts',(2.55330984454,-17.4840818306,1.17681423799));
#81257=CARTESIAN_POINT('Ctrl Pts',(2.51174156132,-17.5227993839,1.12922208024));
#81258=CARTESIAN_POINT('Ctrl Pts',(2.47489289955,-17.5449043891,1.06729320786));
#81259=CARTESIAN_POINT('Ctrl Pts',(2.44734293975,-17.5477841071,0.998707070211));
#81260=CARTESIAN_POINT('Ctrl Pts',(2.43099106691,-17.5332197496,0.93111255917));
#81261=CARTESIAN_POINT('Ctrl Pts',(2.72261491105,-17.4869576367,1.17969475941));
#81262=CARTESIAN_POINT('Ctrl Pts',(2.67711454496,-17.5437282683,1.15424808256));
#81263=CARTESIAN_POINT('Ctrl Pts',(2.63161417887,-17.5901493824,1.10663321957));
#81264=CARTESIAN_POINT('Ctrl Pts',(2.59215946779,-17.6186952055,1.0403312197));
#81265=CARTESIAN_POINT('Ctrl Pts',(2.56454650279,-17.6253471943,0.965088224411));
#81266=CARTESIAN_POINT('Ctrl Pts',(2.55066029792,-17.6120575799,0.890767574454));
#81267=CARTESIAN_POINT('Ctrl Pts',(2.97172474664,-17.6000943145,1.1412362125));
#81268=CARTESIAN_POINT('Ctrl Pts',(2.91735433119,-17.6692765139,1.12809880562));
#81269=CARTESIAN_POINT('Ctrl Pts',(2.86298391574,-17.7315429739,1.08325341223));
#81270=CARTESIAN_POINT('Ctrl Pts',(2.8179996123,-17.7746943065,1.00928125711));
#81271=CARTESIAN_POINT('Ctrl Pts',(2.79121040663,-17.7907023387,0.920813266721));
#81272=CARTESIAN_POINT('Ctrl Pts',(2.78403685548,-17.7816436282,0.833120105007));
#81273=CARTESIAN_POINT('Ctrl Pts',(3.21130945297,-17.7305299504,1.13861871946));
#81274=CARTESIAN_POINT('Ctrl Pts',(3.14443125953,-17.8051039402,1.14445298434));
#81275=CARTESIAN_POINT('Ctrl Pts',(3.07755306609,-17.8822389016,1.10879949478));
#81276=CARTESIAN_POINT('Ctrl Pts',(3.02603277475,-17.9446380869,1.03007665658));
#81277=CARTESIAN_POINT('Ctrl Pts',(3.0034518946,-17.976136713,0.929176763913));
#81278=CARTESIAN_POINT('Ctrl Pts',(3.00848992062,-17.9771596623,0.8291967484));
#81279=CARTESIAN_POINT('Ctrl Pts',(3.325392695,-17.7982565946,1.14774886529));
#81280=CARTESIAN_POINT('Ctrl Pts',(3.2513090753,-17.8730342715,1.1640276349));
#81281=CARTESIAN_POINT('Ctrl Pts',(3.1772254556,-17.9567834794,1.13437155799));
#81282=CARTESIAN_POINT('Ctrl Pts',(3.12223578852,-18.0298580146,1.05431482767));
#81283=CARTESIAN_POINT('Ctrl Pts',(3.10275958695,-18.0708463807,0.948032090962));
#81284=CARTESIAN_POINT('Ctrl Pts',(3.1153678987,-18.0786783194,0.842882322279));
#81285=CARTESIAN_POINT('Ctrl Pts',(3.43467455982,-17.8694391349,1.1700344079));
#81286=CARTESIAN_POINT('Ctrl Pts',(3.35146956174,-17.9400304974,1.19792357011));
#81287=CARTESIAN_POINT('Ctrl Pts',(3.26826456366,-18.0285526893,1.17642640861));
#81288=CARTESIAN_POINT('Ctrl Pts',(3.20940399066,-18.1140150626,1.09643232242));
#81289=CARTESIAN_POINT('Ctrl Pts',(3.19494098605,-18.1676222846,0.985546029641));
#81290=CARTESIAN_POINT('Ctrl Pts',(3.21774774552,-18.1853772775,0.876287149069));
#81291=CARTESIAN_POINT('Ctrl Pts',(3.53153633351,-17.9397782658,1.2109699402));
#81292=CARTESIAN_POINT('Ctrl Pts',(3.43735910775,-18.0003263168,1.24620732043));
#81293=CARTESIAN_POINT('Ctrl Pts',(3.34318188199,-18.0897485104,1.23183053971));
#81294=CARTESIAN_POINT('Ctrl Pts',(3.28035125045,-18.1886331584,1.15483676411));
#81295=CARTESIAN_POINT('Ctrl Pts',(3.27308199046,-18.2588703505,1.04489921328));
#81296=CARTESIAN_POINT('Ctrl Pts',(3.3084919335,-18.2908119326,0.937647357484));
#81297=CARTESIAN_POINT('Ctrl Pts',(3.53153633351,-17.9397782658,1.2109699402));
#81298=CARTESIAN_POINT('Ctrl Pts',(3.50556811491538,-17.9209206519348,1.19999530273144));
#81299=CARTESIAN_POINT('Ctrl Pts',(3.47707465175054,-17.9009947410055,1.19005350125579));
#81300=CARTESIAN_POINT('Ctrl Pts',(3.44603904201575,-17.8801221407561,1.18138128795028));
#81301=CARTESIAN_POINT('Ctrl Pts',(3.40908705834256,-17.8552705592913,1.17105587507089));
#81302=CARTESIAN_POINT('Ctrl Pts',(3.3685335775199,-17.8290766670107,1.16252994367687));
#81303=CARTESIAN_POINT('Ctrl Pts',(3.32439190884036,-17.8017986399993,1.15617041085934));
#81304=CARTESIAN_POINT('Ctrl Pts',(3.31431861168232,-17.7955736901913,1.15471914121381));
#81305=CARTESIAN_POINT('Ctrl Pts',(3.30405849594343,-17.7892924725729,1.15338059333593));
#81306=CARTESIAN_POINT('Ctrl Pts',(3.29361170856435,-17.7829583723188,1.15215898525626));
#81307=CARTESIAN_POINT('Ctrl Pts',(3.25114950591464,-17.7572126728199,1.14719361475952));
#81308=CARTESIAN_POINT('Ctrl Pts',(3.20559642908899,-17.7306009301782,1.14416617105331));
#81309=CARTESIAN_POINT('Ctrl Pts',(3.1569521793853,-17.703441631524,1.14334279135102));
#81310=CARTESIAN_POINT('Ctrl Pts',(3.15136773655507,-17.7003236977175,1.14324826595689));
#81311=CARTESIAN_POINT('Ctrl Pts',(3.14574255851777,-17.6971985681436,1.14318273767508));
#81312=CARTESIAN_POINT('Ctrl Pts',(3.14007665104147,-17.6940667421653,1.14314657180127));
#81313=CARTESIAN_POINT('Ctrl Pts',(3.11256676654638,-17.6788606747737,1.14297097433246));
#81314=CARTESIAN_POINT('Ctrl Pts',(3.08409652814019,-17.6634980322924,1.14348805625532));
#81315=CARTESIAN_POINT('Ctrl Pts',(3.0546659359017,-17.6480454008806,1.14473598939578));
#81316=CARTESIAN_POINT('Ctrl Pts',(3.03995063978245,-17.6403190851746,1.14535995596601));
#81317=CARTESIAN_POINT('Ctrl Pts',(3.02499521890932,-17.632570287484,1.14616660890463));
#81318=CARTESIAN_POINT('Ctrl Pts',(3.00979681525875,-17.6248116462183,1.14715957583797));
#81319=CARTESIAN_POINT('Ctrl Pts',(3.00219761343346,-17.6209323255855,1.14765605930464));
#81320=CARTESIAN_POINT('Ctrl Pts',(2.99453711990554,-17.6170512120295,1.14819899664201));
#81321=CARTESIAN_POINT('Ctrl Pts',(2.98681744787082,-17.6131669151875,1.14878923028722));
#81322=CARTESIAN_POINT('Ctrl Pts',(2.9845683002017,-17.6120352146245,1.14896119648233));
#81323=CARTESIAN_POINT('Ctrl Pts',(2.98231412808812,-17.6109032447226,1.149137179012));
#81324=CARTESIAN_POINT('Ctrl Pts',(2.98005493497421,-17.6097710297417,1.14931719275426));
#81325=CARTESIAN_POINT('Ctrl Pts',(2.97846279508803,-17.608973114495,1.1494440553307));
#81326=CARTESIAN_POINT('Ctrl Pts',(2.97686816150228,-17.6081750775378,1.14957292003385));
#81327=CARTESIAN_POINT('Ctrl Pts',(2.97527103558563,-17.607376927504,1.1497037920794));
#81328=CARTESIAN_POINT('Ctrl Pts',(2.97491126692257,-17.6071971361879,1.14973327232286));
#81329=CARTESIAN_POINT('Ctrl Pts',(2.97454370653952,-17.6070135083179,1.14976348226065));
#81330=CARTESIAN_POINT('Ctrl Pts',(2.974167052028,-17.6068254014812,1.14979454198035));
#81331=CARTESIAN_POINT('Ctrl Pts',(2.97384315794509,-17.6066636439833,1.14982125096464));
#81332=CARTESIAN_POINT('Ctrl Pts',(2.97351352309312,-17.6064990661748,1.1498485076559));
#81333=CARTESIAN_POINT('Ctrl Pts',(2.97317996049783,-17.6063325774542,1.14987616875897));
#81334=CARTESIAN_POINT('Ctrl Pts',(2.96968027511006,-17.6045858044311,1.15016638462728));
#81335=CARTESIAN_POINT('Ctrl Pts',(2.96574739989838,-17.6026302164279,1.15050426861635));
#81336=CARTESIAN_POINT('Ctrl Pts',(2.96348100707217,-17.6015054896627,1.15070247652069));
#81337=CARTESIAN_POINT('Ctrl Pts',(2.92803905491366,-17.5839169623146,1.15380206057428));
#81338=CARTESIAN_POINT('Ctrl Pts',(2.88987049590359,-17.5655398311131,1.15801219935198));
#81339=CARTESIAN_POINT('Ctrl Pts',(2.84895815223916,-17.5465854691076,1.16361465647827));
#81340=CARTESIAN_POINT('Ctrl Pts',(2.83971491844516,-17.5423031527272,1.16488040701712));
#81341=CARTESIAN_POINT('Ctrl Pts',(2.83033174950334,-17.5379915451762,1.16621721245778));
#81342=CARTESIAN_POINT('Ctrl Pts',(2.82080866325753,-17.5336533934426,1.16762830374947));
#81343=CARTESIAN_POINT('Ctrl Pts',(2.79497160771564,-17.5218835675274,1.17145673112451));
#81344=CARTESIAN_POINT('Ctrl Pts',(2.76810639391988,-17.5099151377531,1.17583291465314));
#81345=CARTESIAN_POINT('Ctrl Pts',(2.74021302188449,-17.4978111868782,1.18082044452999));
#81346=CARTESIAN_POINT('Ctrl Pts',(2.72626633586679,-17.4917592114407,1.18331420946842));
#81347=CARTESIAN_POINT('Ctrl Pts',(2.71206261028851,-17.4856733693343,1.18596084863352));
#81348=CARTESIAN_POINT('Ctrl Pts',(2.69760184513937,-17.4795629428546,1.18876792472649));
#81349=CARTESIAN_POINT('Ctrl Pts',(2.6903714625648,-17.4765077296148,1.19017146277297));
#81350=CARTESIAN_POINT('Ctrl Pts',(2.68307682009751,-17.4734463704891,1.19161511116579));
#81351=CARTESIAN_POINT('Ctrl Pts',(2.67571791773619,-17.4703800732671,1.19309980222432));
#81352=CARTESIAN_POINT('Ctrl Pts',(2.67203846655553,-17.4688469246562,1.19384214775358));
#81353=CARTESIAN_POINT('Ctrl Pts',(2.66834295040137,-17.4673125415659,1.19459475404243));
#81354=CARTESIAN_POINT('Ctrl Pts',(2.6646313692736,-17.4657770799259,1.19535773587256));
#81355=CARTESIAN_POINT('Ctrl Pts',(2.66277557870971,-17.4650093491059,1.19573922678762));
#81356=CARTESIAN_POINT('Ctrl Pts',(2.66091577190243,-17.4642413486511,1.1961233115932));
#81357=CARTESIAN_POINT('Ctrl Pts',(2.65905194885173,-17.4634730983855,1.19651000450817));
#81358=CARTESIAN_POINT('Ctrl Pts',(2.65718812580103,-17.4627048481199,1.19689669742315));
#81359=CARTESIAN_POINT('Ctrl Pts',(2.65385512538322,-17.4613346385436,1.19759276935488));
#81360=CARTESIAN_POINT('Ctrl Pts',(2.65344843096939,-17.4611676180876,1.19767792176957));
#81361=CARTESIAN_POINT('Ctrl Pts',(2.64868306052613,-17.4592105851962,1.19867568024947));
#81362=CARTESIAN_POINT('Ctrl Pts',(2.64128756638981,-17.4561782064591,1.2002330735104));
#81363=CARTESIAN_POINT('Ctrl Pts',(2.63125348900647,-17.4521133445083,1.20241115568425));
#81364=CARTESIAN_POINT('Ctrl Pts',(2.62114362876218,-17.4480177824884,1.20460568793041));
#81365=CARTESIAN_POINT('Ctrl Pts',(2.60835491676642,-17.442873956329,1.20743048208744));
#81366=CARTESIAN_POINT('Ctrl Pts',(2.59287672241144,-17.4367582258099,1.21098967640617));
#81367=CARTESIAN_POINT('Ctrl Pts',(2.57741059224131,-17.4306472620809,1.21454609657843));
#81368=CARTESIAN_POINT('Ctrl Pts',(2.5592587583199,-17.4235657759116,1.21883599503214));
#81369=CARTESIAN_POINT('Ctrl Pts',(2.53841370144026,-17.4156241624524,1.22400164543882));
#81370=CARTESIAN_POINT('Ctrl Pts',(2.51788460629228,-17.4078029250591,1.22908899681004));
#81371=CARTESIAN_POINT('Ctrl Pts',(2.49474277554049,-17.3991473310975,1.23502591824219));
#81372=CARTESIAN_POINT('Ctrl Pts',(2.46899103022168,-17.3897976559456,1.24198241379793));
#81373=CARTESIAN_POINT('Ctrl Pts',(2.44461188735642,-17.3809463309791,1.24856811884025));
#81374=CARTESIAN_POINT('Ctrl Pts',(2.41789312181659,-17.3714729933677,1.25606770645213));
#81375=CARTESIAN_POINT('Ctrl Pts',(2.38885356688222,-17.3615281457323,1.26465399261196));
#81376=CARTESIAN_POINT('Ctrl Pts',(2.37284312652012,-17.3560452314681,1.26938788825205));
#81377=CARTESIAN_POINT('Ctrl Pts',(2.35612757048598,-17.3504195498407,1.27445259817871));
#81378=CARTESIAN_POINT('Ctrl Pts',(2.33871339945,-17.3446807781,1.27988117638));
#81379=CARTESIAN_POINT('Origin',(3.225,-17.6882812316,1.64311487169));
#81380=CARTESIAN_POINT('',(0.,-17.9397782658,1.2109699402));
#81381=CARTESIAN_POINT('Origin',(-4.4408920985E-16,-18.4073812884,1.48310265486));
#81382=CARTESIAN_POINT('',(2.225,-18.3719297863,1.46247080897));
#81383=CARTESIAN_POINT('Origin',(4.35,-18.3216303794,1.54889979527));
#81384=CARTESIAN_POINT('Origin',(4.35,-18.3216303794,1.54889979527));
#81385=CARTESIAN_POINT('Ctrl Pts',(3.94208068347,-18.560475405,1.92017998057));
#81386=CARTESIAN_POINT('Ctrl Pts',(3.87720138837,-18.5604754047,1.92017997921));
#81387=CARTESIAN_POINT('Ctrl Pts',(3.81231526335,-18.5765098903,1.91310601594));
#81388=CARTESIAN_POINT('Ctrl Pts',(3.7537820265,-18.6086631358,1.8989209116));
#81389=CARTESIAN_POINT('Ctrl Pts',(3.66183898589,-18.6983642164,1.85934732843));
#81390=CARTESIAN_POINT('Ctrl Pts',(3.63176681675,-18.8182205442,1.80647010407));
#81391=CARTESIAN_POINT('Ctrl Pts',(3.63525640136,-18.8806030959,1.77894868584));
#81392=CARTESIAN_POINT('Ctrl Pts',(3.65691134997,-18.9388168398,1.75326642816));
#81393=CARTESIAN_POINT('Ctrl Pts',(3.69310716565,-18.9880798429,1.73153298464));
#81394=CARTESIAN_POINT('Ctrl Pts',(3.94208074492,-18.5766887246,1.9569305147));
#81395=CARTESIAN_POINT('Ctrl Pts',(3.87720145143,-18.573797947,1.95037801966));
#81396=CARTESIAN_POINT('Ctrl Pts',(3.81231532801,-18.5878885088,1.93889778448));
#81397=CARTESIAN_POINT('Ctrl Pts',(3.75378209234,-18.6193330273,1.92310621435));
#81398=CARTESIAN_POINT('Ctrl Pts',(3.66183905239,-18.7102361193,1.88625721169));
#81399=CARTESIAN_POINT('Ctrl Pts',(3.63176688029,-18.8358324651,1.84639081277));
#81400=CARTESIAN_POINT('Ctrl Pts',(3.63525646243,-18.902055441,1.82757443591));
#81401=CARTESIAN_POINT('Ctrl Pts',(3.65691140785,-18.9646727386,1.81187365705));
#81402=CARTESIAN_POINT('Ctrl Pts',(3.69310722012,-19.0184584616,1.80039180405));
#81403=CARTESIAN_POINT('Ctrl Pts',(3.9309703758,-18.5868132355,1.99657589927));
#81404=CARTESIAN_POINT('Ctrl Pts',(3.86765536306,-18.583214534,1.98238806807));
#81405=CARTESIAN_POINT('Ctrl Pts',(3.80433403936,-18.5969151126,1.96571696787));
#81406=CARTESIAN_POINT('Ctrl Pts',(3.747100735,-18.6283553041,1.94794658657));
#81407=CARTESIAN_POINT('Ctrl Pts',(3.65672049689,-18.7201473882,1.91392916105));
#81408=CARTESIAN_POINT('Ctrl Pts',(3.62587466002,-18.8484282953,1.88855630444));
#81409=CARTESIAN_POINT('Ctrl Pts',(3.62831693429,-18.9164444968,1.87945311729));
#81410=CARTESIAN_POINT('Ctrl Pts',(3.64838248883,-18.9812381625,1.8748423295));
#81411=CARTESIAN_POINT('Ctrl Pts',(3.68269856573,-19.037428697,1.87467495374));
#81412=CARTESIAN_POINT('Ctrl Pts',(3.90873107927,-18.5892873009,2.03559195441));
#81413=CARTESIAN_POINT('Ctrl Pts',(3.84843942238,-18.5881253798,2.01531034459));
#81414=CARTESIAN_POINT('Ctrl Pts',(3.78814242491,-18.6037700715,1.99484202289));
#81415=CARTESIAN_POINT('Ctrl Pts',(3.73342452262,-18.6363892469,1.97609984706));
#81416=CARTESIAN_POINT('Ctrl Pts',(3.64608120201,-18.728999463,1.94582805337));
#81417=CARTESIAN_POINT('Ctrl Pts',(3.61376485716,-18.855867862,1.93373053153));
#81418=CARTESIAN_POINT('Ctrl Pts',(3.61419481888,-18.9228203826,1.93320496012));
#81419=CARTESIAN_POINT('Ctrl Pts',(3.63119178412,-18.9865881277,1.93820769667));
#81420=CARTESIAN_POINT('Ctrl Pts',(3.6618638453,-19.0420643013,1.94777851272));
#81421=CARTESIAN_POINT('Ctrl Pts',(3.84485695788,-18.5827804967,2.11566725872));
#81422=CARTESIAN_POINT('Ctrl Pts',(3.79152009507,-18.5888985515,2.08692370546));
#81423=CARTESIAN_POINT('Ctrl Pts',(3.73817980644,-18.6098769483,2.06216975114));
#81424=CARTESIAN_POINT('Ctrl Pts',(3.68928525628,-18.6452122306,2.04386917313));
#81425=CARTESIAN_POINT('Ctrl Pts',(3.60913704956,-18.7381762607,2.02344540596));
#81426=CARTESIAN_POINT('Ctrl Pts',(3.57378597362,-18.8578355373,2.03575440104));
#81427=CARTESIAN_POINT('Ctrl Pts',(3.56976842438,-18.9199130291,2.05024905768));
#81428=CARTESIAN_POINT('Ctrl Pts',(3.57980389627,-18.9786742001,2.07169908381));
#81429=CARTESIAN_POINT('Ctrl Pts',(3.60202389653,-19.0298725019,2.09781456345));
#81430=CARTESIAN_POINT('Ctrl Pts',(3.75754974665,-18.5555835484,2.18057996716));
#81431=CARTESIAN_POINT('Ctrl Pts',(3.71097917267,-18.570346009,2.15154816967));
#81432=CARTESIAN_POINT('Ctrl Pts',(3.66440657994,-18.5969345937,2.12885177485));
#81433=CARTESIAN_POINT('Ctrl Pts',(3.6212405898,-18.6342490738,2.11465497547));
#81434=CARTESIAN_POINT('Ctrl Pts',(3.54845228546,-18.7244284924,2.10544382014));
#81435=CARTESIAN_POINT('Ctrl Pts',(3.5107816715,-18.8312096705,2.13301209303));
#81436=CARTESIAN_POINT('Ctrl Pts',(3.50278189077,-18.8851477119,2.15564806317));
#81437=CARTESIAN_POINT('Ctrl Pts',(3.50627219288,-18.9354336643,2.18531444577));
#81438=CARTESIAN_POINT('Ctrl Pts',(3.52023080346,-18.9789141355,2.21944021466));
#81439=CARTESIAN_POINT('Ctrl Pts',(3.70638924491,-18.5368582595,2.21099047066));
#81440=CARTESIAN_POINT('Ctrl Pts',(3.66291643405,-18.5553781779,2.18355413245));
#81441=CARTESIAN_POINT('Ctrl Pts',(3.61944208646,-18.5840852858,2.16319877519));
#81442=CARTESIAN_POINT('Ctrl Pts',(3.57892432105,-18.6217121176,2.15180573279));
#81443=CARTESIAN_POINT('Ctrl Pts',(3.50965240858,-18.709332499,2.14854765445));
#81444=CARTESIAN_POINT('Ctrl Pts',(3.47118766711,-18.80892295,2.18210077644));
#81445=CARTESIAN_POINT('Ctrl Pts',(3.46151440616,-18.8585337116,2.20756445935));
#81446=CARTESIAN_POINT('Ctrl Pts',(3.46211782876,-18.9043879244,2.23984745237));
#81447=CARTESIAN_POINT('Ctrl Pts',(3.47230150547,-18.9438289149,2.27642005797));
#81448=CARTESIAN_POINT('Ctrl Pts',(3.653040134,-18.5154874832,2.23714441069));
#81449=CARTESIAN_POINT('Ctrl Pts',(3.6123450469,-18.5369866519,2.2120117706));
#81450=CARTESIAN_POINT('Ctrl Pts',(3.57164880036,-18.5671228869,2.19437159188));
#81451=CARTESIAN_POINT('Ctrl Pts',(3.53351916143,-18.6045418784,2.18582044714));
#81452=CARTESIAN_POINT('Ctrl Pts',(3.46747923522,-18.6889362982,2.18800948694));
#81453=CARTESIAN_POINT('Ctrl Pts',(3.42846086971,-18.7812883476,2.22611332253));
#81454=CARTESIAN_POINT('Ctrl Pts',(3.4173813101,-18.8266730185,2.25351528442));
#81455=CARTESIAN_POINT('Ctrl Pts',(3.4154812712,-18.8682463624,2.28742585674));
#81456=CARTESIAN_POINT('Ctrl Pts',(3.42232180975,-18.9037867018,2.32542426548));
#81457=CARTESIAN_POINT('Ctrl Pts',(3.59839803273,-18.4921598488,2.25921115747));
#81458=CARTESIAN_POINT('Ctrl Pts',(3.56014406941,-18.515804635,2.23684440141));
#81459=CARTESIAN_POINT('Ctrl Pts',(3.52188922088,-18.5466712753,2.22211105827));
#81460=CARTESIAN_POINT('Ctrl Pts',(3.48587211338,-18.5833900306,2.21633478685));
#81461=CARTESIAN_POINT('Ctrl Pts',(3.42275307116,-18.6640035029,2.22340619898));
#81462=CARTESIAN_POINT('Ctrl Pts',(3.38341089221,-18.7492623786,2.26482681385));
#81463=CARTESIAN_POINT('Ctrl Pts',(3.37119264755,-18.7906308355,2.29343152682));
#81464=CARTESIAN_POINT('Ctrl Pts',(3.36718144669,-18.8281878268,2.32816820766));
#81465=CARTESIAN_POINT('Ctrl Pts',(3.37113078856,-18.8600780815,2.3667703805));
#81466=CARTESIAN_POINT('Ctrl Pts',(3.59839803273,-18.4921598488,2.25921115747));
#81467=CARTESIAN_POINT('Ctrl Pts',(3.62233696850021,-18.5023797841465,2.2495436223255));
#81468=CARTESIAN_POINT('Ctrl Pts',(3.64495292720081,-18.5117286768719,2.23933546288846));
#81469=CARTESIAN_POINT('Ctrl Pts',(3.66623232550782,-18.5202015158469,2.22875537729148));
#81470=CARTESIAN_POINT('Ctrl Pts',(3.68905088268763,-18.5292872032258,2.21741002416266));
#81471=CARTESIAN_POINT('Ctrl Pts',(3.71033413511391,-18.537364597701,2.20563343890839));
#81472=CARTESIAN_POINT('Ctrl Pts',(3.73009481200645,-18.5444472306444,2.19361958363631));
#81473=CARTESIAN_POINT('Ctrl Pts',(3.74918903963728,-18.5512909944679,2.18201090805619));
#81474=CARTESIAN_POINT('Ctrl Pts',(3.76685603736808,-18.5572088969338,2.1701786682227));
#81475=CARTESIAN_POINT('Ctrl Pts',(3.78307881567319,-18.5622509716294,2.15826715051219));
#81476=CARTESIAN_POINT('Ctrl Pts',(3.79119020482575,-18.5647720089771,2.15231139165694));
#81477=CARTESIAN_POINT('Ctrl Pts',(3.79893297411376,-18.5670759749598,2.1463313197106));
#81478=CARTESIAN_POINT('Ctrl Pts',(3.80632114933958,-18.5691671180339,2.14035234406015));
#81479=CARTESIAN_POINT('Ctrl Pts',(3.80945469991699,-18.5700540356269,2.13781647802705));
#81480=CARTESIAN_POINT('Ctrl Pts',(3.81252449773391,-18.5709027096732,2.13528080883013));
#81481=CARTESIAN_POINT('Ctrl Pts',(3.81553100219335,-18.571713764473,2.13274675851501));
#81482=CARTESIAN_POINT('Ctrl Pts',(3.8160401777717,-18.5718511230907,2.13231759682503));
#81483=CARTESIAN_POINT('Ctrl Pts',(3.81654753806618,-18.5719874027859,2.13188848151232));
#81484=CARTESIAN_POINT('Ctrl Pts',(3.81705308543795,-18.5721226066858,2.13145941941345));
#81485=CARTESIAN_POINT('Ctrl Pts',(3.81733124428043,-18.5721969976577,2.13122334377853));
#81486=CARTESIAN_POINT('Ctrl Pts',(3.81760298733007,-18.5722694927627,2.13099226077464));
#81487=CARTESIAN_POINT('Ctrl Pts',(3.81786543179076,-18.5723393509092,2.13076869253328));
#81488=CARTESIAN_POINT('Ctrl Pts',(3.81964637454033,-18.5728134068644,2.12925156301398));
#81489=CARTESIAN_POINT('Ctrl Pts',(3.82107546829223,-18.5731881952949,2.12802006423603));
#81490=CARTESIAN_POINT('Ctrl Pts',(3.82282441905364,-18.5736398446241,2.12649540116583));
#81491=CARTESIAN_POINT('Ctrl Pts',(3.82355222464133,-18.5738277932575,2.12586093030117));
#81492=CARTESIAN_POINT('Ctrl Pts',(3.82433507104321,-18.574028724121,2.12517540037968));
#81493=CARTESIAN_POINT('Ctrl Pts',(3.82521946282455,-18.5742535657944,2.12439558589974));
#81494=CARTESIAN_POINT('Ctrl Pts',(3.82562558266263,-18.574356814904,2.12403748880182));
#81495=CARTESIAN_POINT('Ctrl Pts',(3.82605309574868,-18.5744650878723,2.12365949439501));
#81496=CARTESIAN_POINT('Ctrl Pts',(3.82650638208159,-18.5745793301371,2.12325732390271));
#81497=CARTESIAN_POINT('Ctrl Pts',(3.82680114447219,-18.5746536194342,2.1229958010481));
#81498=CARTESIAN_POINT('Ctrl Pts',(3.82710680368985,-18.5747304313617,2.12272405375829));
#81499=CARTESIAN_POINT('Ctrl Pts',(3.82742454124706,-18.5748100050847,2.12244088867393));
#81500=CARTESIAN_POINT('Ctrl Pts',(3.82766950334125,-18.5748713530286,2.12222258048061));
#81501=CARTESIAN_POINT('Ctrl Pts',(3.82791424023572,-18.5749324874447,2.122004082586));
#81502=CARTESIAN_POINT('Ctrl Pts',(3.82815850400271,-18.5749933462999,2.12178561640277));
#81503=CARTESIAN_POINT('Ctrl Pts',(3.83453725872146,-18.5765826270799,2.11608054514195));
#81504=CARTESIAN_POINT('Ctrl Pts',(3.84064962774462,-18.5779981016353,2.11034704654695));
#81505=CARTESIAN_POINT('Ctrl Pts',(3.84649530522882,-18.5792406016356,2.10459310610884));
#81506=CARTESIAN_POINT('Ctrl Pts',(3.85801299017752,-18.5816886880363,2.09325616982407));
#81507=CARTESIAN_POINT('Ctrl Pts',(3.86849909477289,-18.5834662492265,2.08183660805855));
#81508=CARTESIAN_POINT('Ctrl Pts',(3.87795597733478,-18.5845827583383,2.07038887555791));
#81509=CARTESIAN_POINT('Ctrl Pts',(3.89182600413462,-18.5862202970516,2.05359894975076));
#81510=CARTESIAN_POINT('Ctrl Pts',(3.9034754532728,-18.5864319067783,2.03675151545631));
#81511=CARTESIAN_POINT('Ctrl Pts',(3.91286084283373,-18.5852514849807,2.02007879637055));
#81512=CARTESIAN_POINT('Ctrl Pts',(3.92152399525822,-18.584161900591,2.00468909881638));
#81513=CARTESIAN_POINT('Ctrl Pts',(3.92825680658283,-18.5818861450572,1.98944950741741));
#81514=CARTESIAN_POINT('Ctrl Pts',(3.9330579411577,-18.5784837796564,1.97454056755214));
#81515=CARTESIAN_POINT('Ctrl Pts',(3.93739051868325,-18.5754134612474,1.96108663561528));
#81516=CARTESIAN_POINT('Ctrl Pts',(3.94015054802317,-18.5714255692593,1.9479005209682));
#81517=CARTESIAN_POINT('Ctrl Pts',(3.94136360670749,-18.5665912520027,1.93512016333239));
#81518=CARTESIAN_POINT('Ctrl Pts',(3.94184262224495,-18.5646822651509,1.93007342490078));
#81519=CARTESIAN_POINT('Ctrl Pts',(3.94208069165379,-18.5626416312864,1.92509013935795));
#81520=CARTESIAN_POINT('Ctrl Pts',(3.94208068347,-18.5604754053606,1.9201799813874));
#81521=CARTESIAN_POINT('Origin',(2.225,-18.2859995693,2.04127093829));
#81522=CARTESIAN_POINT('',(3.97419901637,-18.4921598488,2.25921115747));
#81523=CARTESIAN_POINT('Ctrl Pts',(-3.59839802628,-18.4921598689,2.25921118379));
#81524=CARTESIAN_POINT('Ctrl Pts',(-3.56014406419,-18.5158046533,2.23684443014));
#81525=CARTESIAN_POINT('Ctrl Pts',(-3.52188921689,-18.5466712915,2.22211108998));
#81526=CARTESIAN_POINT('Ctrl Pts',(-3.48587211043,-18.5833900444,2.21633482189));
#81527=CARTESIAN_POINT('Ctrl Pts',(-3.4227530696,-18.6640035122,2.22340624095));
#81528=CARTESIAN_POINT('Ctrl Pts',(-3.38341089028,-18.7492623846,2.26482686261));
#81529=CARTESIAN_POINT('Ctrl Pts',(-3.37119264491,-18.7906308404,2.29343157878));
#81530=CARTESIAN_POINT('Ctrl Pts',(-3.36718144281,-18.8281878313,2.32816826251));
#81531=CARTESIAN_POINT('Ctrl Pts',(-3.37113078303,-18.8600780864,2.36677043789));
#81532=CARTESIAN_POINT('Ctrl Pts',(-3.64436692045,-18.5117847779,2.24064705327));
#81533=CARTESIAN_POINT('Ctrl Pts',(-3.60405930901,-18.5336245127,2.21595343871));
#81534=CARTESIAN_POINT('Ctrl Pts',(-3.56375058165,-18.5638766801,2.19877465942));
#81535=CARTESIAN_POINT('Ctrl Pts',(-3.52595626142,-18.6011845215,2.19066396874));
#81536=CARTESIAN_POINT('Ctrl Pts',(-3.46037996228,-18.6849787943,2.19362798662));
#81537=CARTESIAN_POINT('Ctrl Pts',(-3.42131019803,-18.7762049571,2.23225829761));
#81538=CARTESIAN_POINT('Ctrl Pts',(-3.41004989653,-18.8209521428,2.25985117454));
#81539=CARTESIAN_POINT('Ctrl Pts',(-3.40781475601,-18.8618879807,2.29389287788));
#81540=CARTESIAN_POINT('Ctrl Pts',(-3.41419637926,-18.896848952,2.3319871249));
#81541=CARTESIAN_POINT('Ctrl Pts',(-3.68942267786,-18.5300289855,2.21919802164));
#81542=CARTESIAN_POINT('Ctrl Pts',(-3.64682650884,-18.549477242,2.19249708165));
#81543=CARTESIAN_POINT('Ctrl Pts',(-3.60422892213,-18.5786239197,2.17300240599));
#81544=CARTESIAN_POINT('Ctrl Pts',(-3.56446501193,-18.6161750191,2.16250612538));
#81545=CARTESIAN_POINT('Ctrl Pts',(-3.49621412217,-18.7027600572,2.16096091912));
#81546=CARTESIAN_POINT('Ctrl Pts',(-3.4575770292,-18.8000544061,2.19593478233));
#81547=CARTESIAN_POINT('Ctrl Pts',(-3.44746147233,-18.8483268457,2.22200085189));
#81548=CARTESIAN_POINT('Ctrl Pts',(-3.44727650114,-18.8928262827,2.25478702366));
#81549=CARTESIAN_POINT('Ctrl Pts',(-3.45640650501,-18.9310329775,2.29179836087));
#81550=CARTESIAN_POINT('Ctrl Pts',(-3.73299942942,-18.5464475453,2.19473372054));
#81551=CARTESIAN_POINT('Ctrl Pts',(-3.68788926215,-18.5629624494,2.16652139764));
#81552=CARTESIAN_POINT('Ctrl Pts',(-3.64277730184,-18.5905259818,2.14497410893));
#81553=CARTESIAN_POINT('Ctrl Pts',(-3.60086046205,-18.6279613042,2.13211990982));
#81554=CARTESIAN_POINT('Ctrl Pts',(-3.52973391166,-18.716878496,2.12570951285));
#81555=CARTESIAN_POINT('Ctrl Pts',(-3.49169746784,-18.8202109654,2.15601350401));
#81556=CARTESIAN_POINT('Ctrl Pts',(-3.48291402379,-18.8720796182,2.17992329081));
#81557=CARTESIAN_POINT('Ctrl Pts',(-3.48504860923,-18.9202474297,2.21075381154));
#81558=CARTESIAN_POINT('Ctrl Pts',(-3.49723105271,-18.9617959389,2.2459600962));
#81559=CARTESIAN_POINT('Ctrl Pts',(-3.82298172564,-18.5768059901,2.13424066669));
#81560=CARTESIAN_POINT('Ctrl Pts',(-3.77156381879,-18.5854424673,2.10496507054));
#81561=CARTESIAN_POINT('Ctrl Pts',(-3.72014291975,-18.60813878,2.08044622543));
#81562=CARTESIAN_POINT('Ctrl Pts',(-3.67286687834,-18.6441962696,2.06309541364));
#81563=CARTESIAN_POINT('Ctrl Pts',(-3.59477049484,-18.736716632,2.04570253954));
#81564=CARTESIAN_POINT('Ctrl Pts',(-3.55869501022,-18.8530757831,2.06267614809));
#81565=CARTESIAN_POINT('Ctrl Pts',(-3.5535101442,-18.9130111236,2.07975240645));
#81566=CARTESIAN_POINT('Ctrl Pts',(-3.56165956977,-18.9695241648,2.10386975363));
#81567=CARTESIAN_POINT('Ctrl Pts',(-3.58153023859,-19.0186783852,2.13261506243));
#81568=CARTESIAN_POINT('Ctrl Pts',(-3.89478846084,-18.5899476448,2.05800806562));
#81569=CARTESIAN_POINT('Ctrl Pts',(-3.83630626947,-18.590413213,2.03451887228));
#81570=CARTESIAN_POINT('Ctrl Pts',(-3.77781929644,-18.6073285136,2.01213169523));
#81571=CARTESIAN_POINT('Ctrl Pts',(-3.72460903492,-18.6406872183,1.99301884559));
#81572=CARTESIAN_POINT('Ctrl Pts',(-3.63909548341,-18.7337132711,1.96507082573));
#81573=CARTESIAN_POINT('Ctrl Pts',(-3.60591816557,-18.8594295314,1.9603907779));
#81574=CARTESIAN_POINT('Ctrl Pts',(-3.6051532526,-18.9255461021,1.96459768824));
#81575=CARTESIAN_POINT('Ctrl Pts',(-3.62031734938,-18.9884767792,1.97487408281));
#81576=CARTESIAN_POINT('Ctrl Pts',(-3.64880183242,-19.0433013389,1.98977942023));
#81577=CARTESIAN_POINT('Ctrl Pts',(-3.92614909738,-18.5904810042,2.0121443256));
#81578=CARTESIAN_POINT('Ctrl Pts',(-3.86354641755,-18.5867461784,1.99488079923));
#81579=CARTESIAN_POINT('Ctrl Pts',(-3.80093767134,-18.6004023618,1.97610614456));
#81580=CARTESIAN_POINT('Ctrl Pts',(-3.74429549879,-18.6318988452,1.95751630482));
#81581=CARTESIAN_POINT('Ctrl Pts',(-3.65462232559,-18.7240449536,1.92457929667));
#81582=CARTESIAN_POINT('Ctrl Pts',(-3.62341697818,-18.8532013091,1.90495660993));
#81583=CARTESIAN_POINT('Ctrl Pts',(-3.62537876376,-18.9217952194,1.89971595229));
#81584=CARTESIAN_POINT('Ctrl Pts',(-3.64471917587,-18.9873022527,1.89951609703));
#81585=CARTESIAN_POINT('Ctrl Pts',(-3.67818178874,-19.0443009521,1.90384525985));
#81586=CARTESIAN_POINT('Ctrl Pts',(-3.94208066889,-18.5798348566,1.96406190215));
#81587=CARTESIAN_POINT('Ctrl Pts',(-3.87720137211,-18.5763831337,1.95623791132));
#81588=CARTESIAN_POINT('Ctrl Pts',(-3.81231524539,-18.5900964858,1.94390265508));
#81589=CARTESIAN_POINT('Ctrl Pts',(-3.7537820072,-18.6214034822,1.92779936516));
#81590=CARTESIAN_POINT('Ctrl Pts',(-3.66183896524,-18.712539831,1.89147909198));
#81591=CARTESIAN_POINT('Ctrl Pts',(-3.63176679768,-18.8392500191,1.8541374553));
#81592=CARTESIAN_POINT('Ctrl Pts',(-3.6352563839,-18.9062182215,1.8370102935));
#81593=CARTESIAN_POINT('Ctrl Pts',(-3.65691133475,-18.9696900169,1.8232464184));
#81594=CARTESIAN_POINT('Ctrl Pts',(-3.69310715296,-19.0243533592,1.81375388105));
#81595=CARTESIAN_POINT('Ctrl Pts',(-3.94208066889,-18.5604753986,1.92017998437));
#81596=CARTESIAN_POINT('Ctrl Pts',(-3.87720137211,-18.5604753986,1.92017998437));
#81597=CARTESIAN_POINT('Ctrl Pts',(-3.81231524539,-18.5765098851,1.91310602353));
#81598=CARTESIAN_POINT('Ctrl Pts',(-3.7537820072,-18.6086631321,1.89892092257));
#81599=CARTESIAN_POINT('Ctrl Pts',(-3.66183896524,-18.6983642163,1.85934734744));
#81600=CARTESIAN_POINT('Ctrl Pts',(-3.63176679768,-18.8182205477,1.80647013222));
#81601=CARTESIAN_POINT('Ctrl Pts',(-3.6352563839,-18.8806031007,1.77894871848));
#81602=CARTESIAN_POINT('Ctrl Pts',(-3.65691133475,-18.9388168454,1.75326646482));
#81603=CARTESIAN_POINT('Ctrl Pts',(-3.69310715296,-18.9880798485,1.73153302458));
#81604=CARTESIAN_POINT('Ctrl Pts',(-3.94208066889,-18.5604753986,1.92017998437));
#81605=CARTESIAN_POINT('Ctrl Pts',(-3.94208066889,-18.5657281416406,1.93208633206972));
#81606=CARTESIAN_POINT('Ctrl Pts',(-3.94065119988507,-18.5702315992113,
1.94441093072267));
#81607=CARTESIAN_POINT('Ctrl Pts',(-3.93779591447238,-18.5739224805057,
1.95702353188134));
#81608=CARTESIAN_POINT('Ctrl Pts',(-3.93380262854624,-18.579084396811,1.97466300234372));
#81609=CARTESIAN_POINT('Ctrl Pts',(-3.92702066882058,-18.5826580874444,
1.99286811843331));
#81610=CARTESIAN_POINT('Ctrl Pts',(-3.91744476193116,-18.584517276425,2.01138446283056));
#81611=CARTESIAN_POINT('Ctrl Pts',(-3.91616044782598,-18.5847666295839,
2.01386786232058));
#81612=CARTESIAN_POINT('Ctrl Pts',(-3.91482587460073,-18.5849851799538,
2.0163569188334));
#81613=CARTESIAN_POINT('Ctrl Pts',(-3.91344104111079,-18.5851726554105,
2.01885104891104));
#81614=CARTESIAN_POINT('Ctrl Pts',(-3.90562472234754,-18.5862308100119,
2.03292849278095));
#81615=CARTESIAN_POINT('Ctrl Pts',(-3.89620941410297,-18.5862950059314,
2.04715128243047));
#81616=CARTESIAN_POINT('Ctrl Pts',(-3.88517509792813,-18.5853373319509,
2.06136781888637));
#81617=CARTESIAN_POINT('Ctrl Pts',(-3.88273253357344,-18.5851253405333,
2.06451480186602));
#81618=CARTESIAN_POINT('Ctrl Pts',(-3.88021078432442,-18.5848634083244,
2.0676614064857));
#81619=CARTESIAN_POINT('Ctrl Pts',(-3.87760986289313,-18.5845514594247,
2.07080589867206));
#81620=CARTESIAN_POINT('Ctrl Pts',(-3.8704345540156,-18.5836908683731,2.07948078689767));
#81621=CARTESIAN_POINT('Ctrl Pts',(-3.86265400859441,-18.5824497275828,
2.0881389299267));
#81622=CARTESIAN_POINT('Ctrl Pts',(-3.85428553574451,-18.5808265237171,
2.09675428436504));
#81623=CARTESIAN_POINT('Ctrl Pts',(-3.85010129931957,-18.5800149217843,
2.10106196158421));
#81624=CARTESIAN_POINT('Ctrl Pts',(-3.84577002421308,-18.5791077857091,
2.10535901184153));
#81625=CARTESIAN_POINT('Ctrl Pts',(-3.84129246804519,-18.5781049463998,
2.10964170600792));
#81626=CARTESIAN_POINT('Ctrl Pts',(-3.83919880205726,-18.5776360275355,
2.11164425623325));
#81627=CARTESIAN_POINT('Ctrl Pts',(-3.83677005848046,-18.5770763899686,
2.11392889126115));
#81628=CARTESIAN_POINT('Ctrl Pts',(-3.83442653236003,-18.5765193810966,
2.11609139417422));
#81629=CARTESIAN_POINT('Ctrl Pts',(-3.83175814641062,-18.5758851595983,
2.11855366346087));
#81630=CARTESIAN_POINT('Ctrl Pts',(-3.82920065543799,-18.5752546318829,
2.12085758181794));
#81631=CARTESIAN_POINT('Ctrl Pts',(-3.82742157038535,-18.5748090672012,
2.12244296878305));
#81632=CARTESIAN_POINT('Ctrl Pts',(-3.82259073759956,-18.5735992045984,
2.12674784409964));
#81633=CARTESIAN_POINT('Ctrl Pts',(-3.81757758328911,-18.5722826572169,
2.13106343755174));
#81634=CARTESIAN_POINT('Ctrl Pts',(-3.81237820924604,-18.5708553930854,
2.13538342234656));
#81635=CARTESIAN_POINT('Ctrl Pts',(-3.79392163837841,-18.5657889367444,
2.15071836552475));
#81636=CARTESIAN_POINT('Ctrl Pts',(-3.77311289509145,-18.5593227106784,
2.16610956974355));
#81637=CARTESIAN_POINT('Ctrl Pts',(-3.74993785221099,-18.5513665587327,
2.1812003601061));
#81638=CARTESIAN_POINT('Ctrl Pts',(-3.72815451567081,-18.5438881891654,
2.19538491919496));
#81639=CARTESIAN_POINT('Ctrl Pts',(-3.70428289127466,-18.5350948765864,
2.20930315692247));
#81640=CARTESIAN_POINT('Ctrl Pts',(-3.67832404689165,-18.5249399314279,
2.22267762482839));
#81641=CARTESIAN_POINT('Ctrl Pts',(-3.65783608400393,-18.5169251624935,
2.23323339526471));
#81642=CARTESIAN_POINT('Ctrl Pts',(-3.6360461079442,-18.5080622310107,2.24345293909897));
#81643=CARTESIAN_POINT('Ctrl Pts',(-3.61296616496511,-18.4983387101615,
2.25319561885508));
#81644=CARTESIAN_POINT('Ctrl Pts',(-3.60816568166547,-18.4963162788455,
2.25522203510339));
#81645=CARTESIAN_POINT('Ctrl Pts',(-3.60330951103741,-18.4942566687393,
2.25722772150755));
#81646=CARTESIAN_POINT('Ctrl Pts',(-3.59839802627999,-18.4921598714318,
2.25921118139502));
#81647=CARTESIAN_POINT('Origin',(2.225,-18.2859995693,2.04127093829));
#81648=CARTESIAN_POINT('',(-4.35,-18.4921598488,2.25921115747));
#81649=CARTESIAN_POINT('',(-3.97419901637,-18.4921598488,2.25921115747));
#81650=CARTESIAN_POINT('Origin',(-4.35,-18.2859995693,2.04127093829));
#81651=CARTESIAN_POINT('Origin',(0.,-14.2790683411,6.24457983432));
#81652=CARTESIAN_POINT('',(-4.35,-14.5682305188,5.97104723161));
#81653=CARTESIAN_POINT('',(2.225,-14.5682305188,5.97104723161));
#81654=CARTESIAN_POINT('',(-4.35,-18.9225141731,1.85211801911));
#81655=CARTESIAN_POINT('Origin',(2.225,-13.881029587,5.24457983432));
#81656=CARTESIAN_POINT('',(-4.35,-13.881029587,6.24457983432));
#81657=CARTESIAN_POINT('',(0.,-13.881029587,6.24457983432));
#81658=CARTESIAN_POINT('Origin',(-4.35,-13.881029587,5.24457983432));
#81659=CARTESIAN_POINT('Origin',(0.,-7.56172990606,6.24457983432));
#81660=CARTESIAN_POINT('',(-4.35,-7.67105043563,6.24457983432));
#81661=CARTESIAN_POINT('',(2.225,-7.67105043563,6.24457983432));
#81662=CARTESIAN_POINT('',(-4.35,-1.95899712601,6.24457983432));
#81663=CARTESIAN_POINT('Origin',(2.225,-7.67105043563,5.74457983432));
#81664=CARTESIAN_POINT('',(-4.35,-7.46238442811,6.19895687742));
#81665=CARTESIAN_POINT('',(0.,-7.46238442811,6.19895687742));
#81666=CARTESIAN_POINT('Origin',(-4.35,-7.67105043563,5.74457983432));
#81667=CARTESIAN_POINT('Origin',(0.,-2.35008265971,3.85120710557));
#81668=CARTESIAN_POINT('',(-4.35,-2.44942813767,3.89683006246));
#81669=CARTESIAN_POINT('',(2.225,-2.44942813767,3.89683006246));
#81670=CARTESIAN_POINT('',(-4.35,4.63581368472,0.643036443538));
#81671=CARTESIAN_POINT('Origin',(2.225,-2.24076213014,4.35120710557));
#81672=CARTESIAN_POINT('',(-4.35,-2.24076213014,3.85120710557));
#81673=CARTESIAN_POINT('',(0.,-2.24076213014,3.85120710557));
#81674=CARTESIAN_POINT('Origin',(-4.35,-2.24076213014,4.35120710557));
#81675=CARTESIAN_POINT('Origin',(0.,2.74061906787,3.85120710557));
#81676=CARTESIAN_POINT('',(-4.35,2.48275227055,3.85120710557));
#81677=CARTESIAN_POINT('',(2.225,2.48275227055,3.85120710557));
#81678=CARTESIAN_POINT('',(-4.35,-1.95899712601,3.85120710557));
#81679=CARTESIAN_POINT('Origin',(2.225,2.48275227055,4.35120710557));
#81680=CARTESIAN_POINT('',(-4.35,2.89013084681,4.06130592308));
#81681=CARTESIAN_POINT('',(0.,2.89013084681,4.06130592308));
#81682=CARTESIAN_POINT('Origin',(-4.35,2.48275227055,4.35120710557));
#81683=CARTESIAN_POINT('Origin',(0.,4.27111742671,6.00191320834));
#81684=CARTESIAN_POINT('',(-4.35,4.24121507093,5.95989344484));
#81685=CARTESIAN_POINT('',(2.225,4.24121507093,5.95989344484));
#81686=CARTESIAN_POINT('',(-4.35,0.250890909306,0.352560070814));
#81687=CARTESIAN_POINT('Origin',(4.35,4.32269078618,5.90191320834));
#81688=CARTESIAN_POINT('Origin',(4.35,4.32269078618,5.90191320834));
#81689=CARTESIAN_POINT('Origin',(0.,4.8773238354,6.00191320834));
#81690=CARTESIAN_POINT('',(-4.35,4.7773238354,6.00191320834));
#81691=CARTESIAN_POINT('',(2.225,4.7773238354,6.00191320834));
#81692=CARTESIAN_POINT('',(-4.35,4.32269078618,6.00191320834));
#81693=CARTESIAN_POINT('',(-4.35,-1.95899712601,6.00191320834));
#81694=CARTESIAN_POINT('',(2.225,4.32269078618,6.00191320834));
#81695=CARTESIAN_POINT('Origin',(4.35,4.7773238354,5.90191320834));
#81696=CARTESIAN_POINT('Origin',(4.35,4.7773238354,5.90191320834));
#81697=CARTESIAN_POINT('Origin',(0.,4.8773238354,4.12878088412));
#81698=CARTESIAN_POINT('',(-4.35,4.8773238354,4.22878088412));
#81699=CARTESIAN_POINT('',(2.225,4.8773238354,4.22878088412));
#81700=CARTESIAN_POINT('',(-4.35,4.8773238354,5.90191320834));
#81701=CARTESIAN_POINT('',(-4.35,4.8773238354,0.294579834316));
#81702=CARTESIAN_POINT('',(2.225,4.8773238354,5.90191320834));
#81703=CARTESIAN_POINT('Origin',(2.225,4.9773238354,4.22878088412));
#81704=CARTESIAN_POINT('',(-4.35,4.9773238354,4.12878088412));
#81705=CARTESIAN_POINT('',(0.,4.9773238354,4.12878088412));
#81706=CARTESIAN_POINT('Origin',(-4.35,4.9773238354,4.22878088412));
#81707=CARTESIAN_POINT('Origin',(0.,15.277455061,4.12878088412));
#81708=CARTESIAN_POINT('',(-4.35,15.177455061,4.12878088412));
#81709=CARTESIAN_POINT('',(2.225,15.177455061,4.12878088412));
#81710=CARTESIAN_POINT('',(-4.35,-1.95899712601,4.12878088412));
#81711=CARTESIAN_POINT('Origin',(4.35,15.177455061,4.02878088412));
#81712=CARTESIAN_POINT('Origin',(4.35,15.177455061,4.02878088412));
#81713=CARTESIAN_POINT('Origin',(0.,15.277455061,-4.77121911588));
#81714=CARTESIAN_POINT('',(-4.35,15.277455061,-4.67121911588));
#81715=CARTESIAN_POINT('',(2.225,15.277455061,-4.67121911588));
#81716=CARTESIAN_POINT('',(-4.35,15.277455061,4.02878088412));
#81717=CARTESIAN_POINT('',(-4.35,15.277455061,0.294579834316));
#81718=CARTESIAN_POINT('',(2.225,15.277455061,4.02878088412));
#81719=CARTESIAN_POINT('Origin',(4.35,15.177455061,-4.67121911588));
#81720=CARTESIAN_POINT('Origin',(4.35,15.177455061,-4.67121911588));
#81721=CARTESIAN_POINT('Origin',(0.,15.277455061,-4.77121911588));
#81722=CARTESIAN_POINT('',(-4.35,4.9773238354,-4.77121911588));
#81723=CARTESIAN_POINT('',(2.225,4.9773238354,-4.77121911588));
#81724=CARTESIAN_POINT('',(-4.35,15.177455061,-4.77121911588));
#81725=CARTESIAN_POINT('',(-4.35,-1.95899712601,-4.77121911588));
#81726=CARTESIAN_POINT('',(2.225,15.177455061,-4.77121911588));
#81727=CARTESIAN_POINT('Origin',(2.225,4.9773238354,-4.87121911588));
#81728=CARTESIAN_POINT('',(-4.35,4.8773238354,-4.87121911588));
#81729=CARTESIAN_POINT('',(0.,4.8773238354,-4.87121911588));
#81730=CARTESIAN_POINT('Origin',(-4.35,4.9773238354,-4.87121911588));
#81731=CARTESIAN_POINT('Origin',(0.,4.8773238354,4.12878088412));
#81732=CARTESIAN_POINT('',(-4.35,4.8773238354,0.294579834316));
#81733=CARTESIAN_POINT('Origin',(0.,-9.17423561284,0.47366156039));
#81734=CARTESIAN_POINT('',(4.35,-11.8242356128,0.47366156039));
#81735=CARTESIAN_POINT('Origin',(4.35,-9.17423561284,0.473661560389999));
#81736=CARTESIAN_POINT('',(0.,-11.82423561284,0.47366156039));
#81737=CARTESIAN_POINT('Origin',(-4.35,-21.2594877202,0.729452270839));
#81738=CARTESIAN_POINT('',(-4.45,-18.4689834555,1.96054363567));
#81739=CARTESIAN_POINT('Origin',(-4.35,-18.4689834555,1.96054363567));
#81740=CARTESIAN_POINT('',(-4.45,-18.3216303794,1.54889979527));
#81741=CARTESIAN_POINT('Origin',(-4.45,-21.2594877202,0.729452270839));
#81742=CARTESIAN_POINT('Origin',(-4.35,-18.3216303794,1.54889979527));
#81743=CARTESIAN_POINT('Ctrl Pts',(-3.94234877308934,-18.4179622929748,
1.5220634491669));
#81744=CARTESIAN_POINT('Ctrl Pts',(-3.87741592322529,-18.4179021372523,
1.52206354967647));
#81745=CARTESIAN_POINT('Ctrl Pts',(-3.81246043986878,-18.4347523597789,
1.51735270773294));
#81746=CARTESIAN_POINT('Ctrl Pts',(-3.75385806626735,-18.4686084523042,
1.50790595663289));
#81747=CARTESIAN_POINT('Ctrl Pts',(-3.66185147225803,-18.5630744293574,
1.48156577864178));
#81748=CARTESIAN_POINT('Ctrl Pts',(-3.63176687268071,-18.6893211886786,
1.44638791408526));
#81749=CARTESIAN_POINT('Ctrl Pts',(-3.63525645057377,-18.7550039506979,
1.42809073665793));
#81750=CARTESIAN_POINT('Ctrl Pts',(-3.65691138925993,-18.8162985856091,
1.41102067506232));
#81751=CARTESIAN_POINT('Ctrl Pts',(-3.69310719334021,-18.8681699604421,
1.39657949980758));
#81752=CARTESIAN_POINT('Ctrl Pts',(-3.94236571798829,-18.4133876700544,
1.50564227215289));
#81753=CARTESIAN_POINT('Ctrl Pts',(-3.87742949734126,-18.4156210030371,
1.51388530750485));
#81754=CARTESIAN_POINT('Ctrl Pts',(-3.8124706399661,-18.4339647887765,1.51454343666174));
#81755=CARTESIAN_POINT('Ctrl Pts',(-3.75386547213153,-18.4682850893703,
1.50676707768882));
#81756=CARTESIAN_POINT('Ctrl Pts',(-3.66185555985532,-18.5615234559633,
1.47602152543541));
#81757=CARTESIAN_POINT('Ctrl Pts',(-3.63177274765737,-18.682852077315,1.4231810522504));
#81758=CARTESIAN_POINT('Ctrl Pts',(-3.63526465905675,-18.7453003527305,
1.39326767740239));
#81759=CARTESIAN_POINT('Ctrl Pts',(-3.65692311167227,-18.8029268266872,
1.36302496574797));
#81760=CARTESIAN_POINT('Ctrl Pts',(-3.69312305426809,-18.8510626926684,
1.33517080589476));
#81761=CARTESIAN_POINT('Ctrl Pts',(-3.93117743481258,-18.4053199263241,
1.49021851431677));
#81762=CARTESIAN_POINT('Ctrl Pts',(-3.86848432428731,-18.4133496508806,
1.50572009052338));
#81763=CARTESIAN_POINT('Ctrl Pts',(-3.80577072397423,-18.4356439814143,
1.51105797007258));
#81764=CARTESIAN_POINT('Ctrl Pts',(-3.74902487427037,-18.4714835809575,
1.50465788542018));
#81765=CARTESIAN_POINT('Ctrl Pts',(-3.65922237266646,-18.5627831102452,
1.46971354377953));
#81766=CARTESIAN_POINT('Ctrl Pts',(-3.62794841541813,-18.6740098368393,
1.40067791306863));
#81767=CARTESIAN_POINT('Ctrl Pts',(-3.62988637637911,-18.7297933802063,
1.36011859423275));
#81768=CARTESIAN_POINT('Ctrl Pts',(-3.64920524301539,-18.7800386429644,
1.31775397033819));
#81769=CARTESIAN_POINT('Ctrl Pts',(-3.68265005904169,-18.8209194717089,
1.277483839591));
#81770=CARTESIAN_POINT('Ctrl Pts',(-3.90937039764836,-18.3946473544159,
1.47823990790765));
#81771=CARTESIAN_POINT('Ctrl Pts',(-3.85079941235044,-18.4100260311796,
1.4954773509941));
#81772=CARTESIAN_POINT('Ctrl Pts',(-3.79221048551906,-18.4371226818621,
1.50112267759752));
#81773=CARTESIAN_POINT('Ctrl Pts',(-3.73888775605576,-18.4745486886345,
1.49356057393109));
#81774=CARTESIAN_POINT('Ctrl Pts',(-3.65317282634548,-18.5626874259432,
1.45356159969605));
#81775=CARTESIAN_POINT('Ctrl Pts',(-3.6197569336771,-18.6607011526531,1.37482011528626));
#81776=CARTESIAN_POINT('Ctrl Pts',(-3.61885954013509,-18.7079919198437,
1.32845104766779));
#81777=CARTESIAN_POINT('Ctrl Pts',(-3.63388281316495,-18.7490375736454,
1.27962425360384));
#81778=CARTESIAN_POINT('Ctrl Pts',(-3.66223622907347,-18.7810400637854,
1.23262277310423));
#81779=CARTESIAN_POINT('Ctrl Pts',(-3.88313625536304,-18.3833905207368,
1.46911853484485));
#81780=CARTESIAN_POINT('Ctrl Pts',(-3.82827635921413,-18.4040707835055,
1.48560034168476));
#81781=CARTESIAN_POINT('Ctrl Pts',(-3.77340110703683,-18.4341185642061,
1.48981511758575));
#81782=CARTESIAN_POINT('Ctrl Pts',(-3.72318353452304,-18.4717817689888,
1.48031522313803));
#81783=CARTESIAN_POINT('Ctrl Pts',(-3.64128193973745,-18.5553892025893,
1.4356866604964));
#81784=CARTESIAN_POINT('Ctrl Pts',(-3.60614533962705,-18.6412407365273,
1.35102616050676));
#81785=CARTESIAN_POINT('Ctrl Pts',(-3.60279817951113,-18.6811249203593,
1.30143857220328));
#81786=CARTESIAN_POINT('Ctrl Pts',(-3.61399030710223,-18.7143667021278,
1.24912958467003));
#81787=CARTESIAN_POINT('Ctrl Pts',(-3.63767337026233,-18.738937433864,1.19843010357245));
#81788=CARTESIAN_POINT('Ctrl Pts',(-3.85356722871327,-18.3718068169226,
1.46239916841677));
#81789=CARTESIAN_POINT('Ctrl Pts',(-3.80215086093377,-18.3963222194477,
1.47671313353459));
#81790=CARTESIAN_POINT('Ctrl Pts',(-3.75072128784765,-18.4280665581311,
1.47861300783342));
#81791=CARTESIAN_POINT('Ctrl Pts',(-3.70340064135175,-18.4651002965507,
1.46690668481873));
#81792=CARTESIAN_POINT('Ctrl Pts',(-3.62512643672596,-18.5433562230935,
1.41831938308649));
#81793=CARTESIAN_POINT('Ctrl Pts',(-3.58854128012704,-18.6178411571792,
1.3304346488623));
#81794=CARTESIAN_POINT('Ctrl Pts',(-3.58299778663471,-18.6510735894616,
1.27938625857796));
#81795=CARTESIAN_POINT('Ctrl Pts',(-3.59067473503819,-18.6774630701226,
1.22558481182393));
#81796=CARTESIAN_POINT('Ctrl Pts',(-3.60998517910906,-18.6955883056329,
1.17321662092078));
#81797=CARTESIAN_POINT('Ctrl Pts',(-3.85341043799,-18.3719297862815,1.46247080900171));
#81798=CARTESIAN_POINT('Ctrl Pts',(-3.87059142535003,-18.3786553513643,
1.46638491177223));
#81799=CARTESIAN_POINT('Ctrl Pts',(-3.88527563788033,-18.3848432456902,
1.47104121504505));
#81800=CARTESIAN_POINT('Ctrl Pts',(-3.89746307558087,-18.3903663596056,
1.47626808714481));
#81801=CARTESIAN_POINT('Ctrl Pts',(-3.90983341714612,-18.3959723620578,
1.48157340191077));
#81802=CARTESIAN_POINT('Ctrl Pts',(-3.91963148047731,-18.4008934150417,
1.48746561968176));
#81803=CARTESIAN_POINT('Ctrl Pts',(-3.92685726557444,-18.4050492008162,
1.49375181041533));
#81804=CARTESIAN_POINT('Ctrl Pts',(-3.93425454899559,-18.4093036208963,
1.50018719893999));
#81805=CARTESIAN_POINT('Ctrl Pts',(-3.93895600318521,-18.4127561162088,
1.50703457317492));
#81806=CARTESIAN_POINT('Ctrl Pts',(-3.94096162814328,-18.4153751057879,
1.51408706377056));
#81807=CARTESIAN_POINT('Ctrl Pts',(-3.94170771372341,-18.4163493608956,
1.51671056599425));
#81808=CARTESIAN_POINT('Ctrl Pts',(-3.94208074657565,-18.4172087969225,
1.51936252321673));
#81809=CARTESIAN_POINT('Ctrl Pts',(-3.9420807267,-18.4179535709002,1.52203266331995));
#81810=CARTESIAN_POINT('Origin',(-2.225,-18.3216303794,1.54889979527));
#81811=CARTESIAN_POINT('',(-4.35,-18.3719297863,1.46247080897));
#81812=CARTESIAN_POINT('Origin',(-4.35,-18.3216303794,1.54889979527));
#81813=CARTESIAN_POINT('',(0.,-18.3719297863,1.46247080897));
#81814=CARTESIAN_POINT('Origin',(-2.3,-21.2594877202,0.729452270839));
#81815=CARTESIAN_POINT('',(-2.,-17.1183636721,1.08100826706));
#81816=CARTESIAN_POINT('Origin',(-2.3,-17.1183636721,1.08100826706));
#81817=CARTESIAN_POINT('',(-2.,-17.3209666442,-0.597405571358));
#81818=CARTESIAN_POINT('Origin',(-2.,-21.2594877202,0.729452270839));
#81819=CARTESIAN_POINT('Origin',(-2.3,-17.3209666442,-0.597405571358));
#81820=CARTESIAN_POINT('Origin',(-2.,0.,0.));
#81821=CARTESIAN_POINT('',(-2.,-13.3863832983,4.61127046457));
#81822=CARTESIAN_POINT('',(-2.,-16.3982789105,1.76217155265));
#81823=CARTESIAN_POINT('',(-2.,-12.9053426461,4.80274328646));
#81824=CARTESIAN_POINT('Origin',(-2.,-12.9053426461,4.10274328646));
#81825=CARTESIAN_POINT('',(-2.,-9.41827086707,4.80274328646));
#81826=CARTESIAN_POINT('',(-2.,-12.0504559477,4.80274328646));
#81827=CARTESIAN_POINT('',(-2.,-8.76025711822,4.30133994369));
#81828=CARTESIAN_POINT('Origin',(-2.,-8.67423561284,5.09670168568));
#81829=CARTESIAN_POINT('',(-2.,-8.76025711822,-3.35401682291));
#81830=CARTESIAN_POINT('Origin',(-2.,-9.17423561284,0.47366156039));
#81831=CARTESIAN_POINT('',(-2.,-9.41827086707,-3.85542016568));
#81832=CARTESIAN_POINT('Origin',(-2.,-8.67423561284,-4.1493785649));
#81833=CARTESIAN_POINT('',(-2.,-10.0779006799,-3.85542016568));
#81834=CARTESIAN_POINT('',(-2.,-8.20939783898,-3.85542016568));
#81835=CARTESIAN_POINT('',(-2.,-10.371774934,-3.79074521854));
#81836=CARTESIAN_POINT('Origin',(-2.,-10.0779006799,-3.15542016568));
#81837=CARTESIAN_POINT('',(-2.,-17.1551720262,-0.653035235664));
#81838=CARTESIAN_POINT('',(-2.,-13.7337583338,-2.23563518556));
#81839=CARTESIAN_POINT('Origin',(-2.,-17.4910283166,-1.37912101035));
#81840=CARTESIAN_POINT('',(-2.,-12.12423561284,0.47366156039));
#81841=CARTESIAN_POINT('Origin',(-2.,-9.17423561284,0.47366156039));
#81842=CARTESIAN_POINT('Ctrl Pts',(-3.88718266259547,-19.025433934838,-1.22483561091038));
#81843=CARTESIAN_POINT('Ctrl Pts',(-3.77580408384224,-19.0736898839023,
-1.23616597952645));
#81844=CARTESIAN_POINT('Ctrl Pts',(-3.66440778333474,-19.1360641780841,
-1.18720219522702));
#81845=CARTESIAN_POINT('Ctrl Pts',(-3.59323386373744,-19.1955274355822,
-1.07211980399972));
#81846=CARTESIAN_POINT('Ctrl Pts',(-3.59207872644302,-19.2271844940609,
-0.939102859271506));
#81847=CARTESIAN_POINT('Ctrl Pts',(-3.64159979814485,-19.2306078238278,
-0.827755898096201));
#81848=CARTESIAN_POINT('Ctrl Pts',(-3.90640659993754,-19.0359515024118,
-1.22729295147926));
#81849=CARTESIAN_POINT('Ctrl Pts',(-3.78964355915635,-19.0775118594821,
-1.24255434458416));
#81850=CARTESIAN_POINT('Ctrl Pts',(-3.67286110812766,-19.1403096158138,
-1.19644007340445));
#81851=CARTESIAN_POINT('Ctrl Pts',(-3.60013346101267,-19.2091455215151,
-1.0813755662174));
#81852=CARTESIAN_POINT('Ctrl Pts',(-3.60331125265511,-19.2540269422902,
-0.947808006978175));
#81853=CARTESIAN_POINT('Ctrl Pts',(-3.65960588543438,-19.2700026746203,
-0.836975235851294));
#81854=CARTESIAN_POINT('Ctrl Pts',(-3.92284970227234,-19.0467428229707,
-1.23131164661682));
#81855=CARTESIAN_POINT('Ctrl Pts',(-3.80072845787408,-19.0792180125451,
-1.24870207523215));
#81856=CARTESIAN_POINT('Ctrl Pts',(-3.67858607893163,-19.1408694654263,
-1.20498533022795));
#81857=CARTESIAN_POINT('Ctrl Pts',(-3.60441223261194,-19.2195874016009,
-1.09137878321749));
#81858=CARTESIAN_POINT('Ctrl Pts',(-3.61202763612795,-19.2797027732923,
-0.959801768378248));
#81859=CARTESIAN_POINT('Ctrl Pts',(-3.67500679368465,-19.3104167222716,
-0.852040651816825));
#81860=CARTESIAN_POINT('Ctrl Pts',(-3.93558612334475,-19.0576343352439,
-1.23716860991036));
#81861=CARTESIAN_POINT('Ctrl Pts',(-3.80845043726328,-19.0782994500631,
-1.25360431235422));
#81862=CARTESIAN_POINT('Ctrl Pts',(-3.68129195135629,-19.1367502302322,
-1.21109032580039));
#81863=CARTESIAN_POINT('Ctrl Pts',(-3.60588177835506,-19.2256755686209,
-1.10083932805995));
#81864=CARTESIAN_POINT('Ctrl Pts',(-3.61778081899953,-19.303262871619,-0.974970009523419));
#81865=CARTESIAN_POINT('Ctrl Pts',(-3.68693535426574,-19.3511979302931,
-0.873985633650477));
#81866=CARTESIAN_POINT('Ctrl Pts',(-3.94218039631734,-19.0678943136438,
-1.24528320682825));
#81867=CARTESIAN_POINT('Ctrl Pts',(-3.8124009667551,-19.0766778004732,-1.25501049679676));
#81868=CARTESIAN_POINT('Ctrl Pts',(-3.68259785626293,-19.1312303113916,
-1.21075865244405));
#81869=CARTESIAN_POINT('Ctrl Pts',(-3.60654295125758,-19.2294718799634,
-1.10665750700906));
#81870=CARTESIAN_POINT('Ctrl Pts',(-3.62070686959814,-19.3242869156647,
-0.992634050237943));
#81871=CARTESIAN_POINT('Ctrl Pts',(-3.69311133654807,-19.3896139653707,
-0.904376164438057));
#81872=CARTESIAN_POINT('Ctrl Pts',(-3.94217592748915,-19.076683734755,-1.25495360386885));
#81873=CARTESIAN_POINT('Ctrl Pts',(-3.81239828953171,-19.0766457743704,
-1.25497310675431));
#81874=CARTESIAN_POINT('Ctrl Pts',(-3.68259697124399,-19.1285379948036,
-1.20779327228567));
#81875=CARTESIAN_POINT('Ctrl Pts',(-3.60654249737104,-19.2341457609791,
-1.1117975978063));
#81876=CARTESIAN_POINT('Ctrl Pts',(-3.62070488664521,-19.3428206630258,
-1.01302463080287));
#81877=CARTESIAN_POINT('Ctrl Pts',(-3.69310715118846,-19.4225269040689,
-0.940588007021057));
#81878=CARTESIAN_POINT('Ctrl Pts',(-3.94208066889,-19.0766762824804,-1.25494542807784));
#81879=CARTESIAN_POINT('Ctrl Pts',(-3.94208066889,-19.0715553844833,-1.24931250745258));
#81880=CARTESIAN_POINT('Ctrl Pts',(-3.9393205736673,-19.0657379583168,-1.2442116228788));
#81881=CARTESIAN_POINT('Ctrl Pts',(-3.9338003832219,-19.0593444548702,-1.23981507244739));
#81882=CARTESIAN_POINT('Ctrl Pts',(-3.92838645285692,-19.0530740222121,
-1.23550315275601));
#81883=CARTESIAN_POINT('Ctrl Pts',(-3.9203176646309,-19.0462498198137,-1.23186946682268));
#81884=CARTESIAN_POINT('Ctrl Pts',(-3.90959401854385,-19.0390290035994,
-1.22905229461513));
#81885=CARTESIAN_POINT('Ctrl Pts',(-3.90308103832551,-19.0346434585356,
-1.22734129196635));
#81886=CARTESIAN_POINT('Ctrl Pts',(-3.89558875789756,-19.0301124511698,
-1.22593095609068));
#81887=CARTESIAN_POINT('Ctrl Pts',(-3.88711717726,-19.0254782582987,-1.22484599945563));
#81888=CARTESIAN_POINT('Origin',(-2.225,-19.0026826744,-1.32221314666));
#81889=CARTESIAN_POINT('',(-4.35,-19.0254782583,-1.22484599945));
#81890=CARTESIAN_POINT('',(0.,-19.0254782583,-1.22484599945));
#81891=CARTESIAN_POINT('Origin',(-4.35,-19.0026826744,-1.32221314666));
#81892=CARTESIAN_POINT('Origin',(-2.3,-9.41827086707,-3.85542016568));
#81893=CARTESIAN_POINT('',(-2.3,-9.13925764673,-3.96565456539));
#81894=CARTESIAN_POINT('Origin',(-2.3,-9.41827086707,-3.85542016568));
#81895=CARTESIAN_POINT('',(-2.3,-9.41827086707,-4.15542016568));
#81896=CARTESIAN_POINT('Origin',(-2.3,-9.41827086707,-3.85542016568));
#81897=CARTESIAN_POINT('Origin',(-2.3,-9.41827086707,-3.85542016568));
#81898=CARTESIAN_POINT('Ctrl Pts',(3.85357127529058,-18.3718036312809,1.46239723758686));
#81899=CARTESIAN_POINT('Ctrl Pts',(3.80215397592704,-18.3963191316518,1.47671247492689));
#81900=CARTESIAN_POINT('Ctrl Pts',(3.75072320422429,-18.4280638952455,1.47861315152616));
#81901=CARTESIAN_POINT('Ctrl Pts',(3.70340133340925,-18.4650983039147,1.46690700156938));
#81902=CARTESIAN_POINT('Ctrl Pts',(3.62512602082281,-18.5433548310396,1.41831937899194));
#81903=CARTESIAN_POINT('Ctrl Pts',(3.58854039733859,-18.6178399766783,1.33043350136151));
#81904=CARTESIAN_POINT('Ctrl Pts',(3.5829967928236,-18.6510720638893,1.27938501876718));
#81905=CARTESIAN_POINT('Ctrl Pts',(3.59067356313336,-18.6774611898981,1.22558347765477));
#81906=CARTESIAN_POINT('Ctrl Pts',(3.60998378544702,-18.6955860923029,1.17321518442684));
#81907=CARTESIAN_POINT('Ctrl Pts',(3.88315087732857,-18.3833917237588,1.46911854700638));
#81908=CARTESIAN_POINT('Ctrl Pts',(3.82828881190557,-18.4040705718358,1.4856024608897));
#81909=CARTESIAN_POINT('Ctrl Pts',(3.7734110869559,-18.4341180636217,1.48981892272446));
#81910=CARTESIAN_POINT('Ctrl Pts',(3.72319120146361,-18.4717821126652,1.48032002015744));
#81911=CARTESIAN_POINT('Ctrl Pts',(3.64128717554319,-18.5553919914991,1.4356925004318));
#81912=CARTESIAN_POINT('Ctrl Pts',(3.60615060806008,-18.6412476903878,1.35103186316354));
#81913=CARTESIAN_POINT('Ctrl Pts',(3.6028040762687,-18.6811337590432,1.30144459840769));
#81914=CARTESIAN_POINT('Ctrl Pts',(3.6139972125595,-18.7143774757967,1.24913593326059));
#81915=CARTESIAN_POINT('Ctrl Pts',(3.63768153388863,-18.738950023906,1.1984368256642));
#81916=CARTESIAN_POINT('Ctrl Pts',(3.90939559357203,-18.3946540094753,1.4782446449377));
#81917=CARTESIAN_POINT('Ctrl Pts',(3.85082074009429,-18.4100283850775,1.49548402094887));
#81918=CARTESIAN_POINT('Ctrl Pts',(3.7922276215467,-18.4371229831985,1.50113134358345));
#81919=CARTESIAN_POINT('Ctrl Pts',(3.73890110215105,-18.4745494045097,1.49357102698152));
#81920=CARTESIAN_POINT('Ctrl Pts',(3.65318201219449,-18.5626922931479,1.45357539566712));
#81921=CARTESIAN_POINT('Ctrl Pts',(3.61976694585612,-18.6607156097194,1.37483737433787));
#81922=CARTESIAN_POINT('Ctrl Pts',(3.61887128440298,-18.7080115525041,1.32847064540805));
#81923=CARTESIAN_POINT('Ctrl Pts',(3.63389722882754,-18.7490626081558,1.27964638891813));
#81924=CARTESIAN_POINT('Ctrl Pts',(3.66225393957856,-18.7810702739468,1.23264761022329));
#81925=CARTESIAN_POINT('Ctrl Pts',(3.93117576959292,-18.4053110180947,1.49019805486829));
#81926=CARTESIAN_POINT('Ctrl Pts',(3.86848316971063,-18.4133452763836,1.50571006544666));
#81927=CARTESIAN_POINT('Ctrl Pts',(3.80576973439363,-18.43564302456,1.5110547043985));
#81928=CARTESIAN_POINT('Ctrl Pts',(3.74902367655503,-18.4714843750673,1.50465682308547));
#81929=CARTESIAN_POINT('Ctrl Pts',(3.65922142539151,-18.5627826491134,1.46970715178544));
#81930=CARTESIAN_POINT('Ctrl Pts',(3.62794609617334,-18.6740004978667,1.40065049328273));
#81931=CARTESIAN_POINT('Ctrl Pts',(3.62988278031609,-18.729777409853,1.36007776743956));
#81932=CARTESIAN_POINT('Ctrl Pts',(3.64919964740062,-18.7800152939447,1.31769811801765));
#81933=CARTESIAN_POINT('Ctrl Pts',(3.68264216713878,-18.8208888431934,1.27741247157079));
#81934=CARTESIAN_POINT('Ctrl Pts',(3.9423729901106,-18.4133858070116,1.50563516198861));
#81935=CARTESIAN_POINT('Ctrl Pts',(3.87743527118537,-18.4156185427818,1.51388218351694));
#81936=CARTESIAN_POINT('Ctrl Pts',(3.81247450205661,-18.4339621657064,1.51454292609738));
#81937=CARTESIAN_POINT('Ctrl Pts',(3.75386744558497,-18.4682828070917,1.50676736425539));
#81938=CARTESIAN_POINT('Ctrl Pts',(3.66185577629033,-18.5615214174088,1.47602002943265));
#81939=CARTESIAN_POINT('Ctrl Pts',(3.63177269714063,-18.6828496357294,1.4231722323832));
#81940=CARTESIAN_POINT('Ctrl Pts',(3.63526468072322,-18.7452967881311,1.39325441889084));
#81941=CARTESIAN_POINT('Ctrl Pts',(3.65692324111908,-18.8029219813393,1.36300667854291));
#81942=CARTESIAN_POINT('Ctrl Pts',(3.69312330991489,-18.8510565319363,1.33514740419474));
#81943=CARTESIAN_POINT('Ctrl Pts',(3.94235571266733,-18.4179625115314,1.5220642680868));
#81944=CARTESIAN_POINT('Ctrl Pts',(3.87742145776479,-18.4179007841395,1.52206437062455));
#81945=CARTESIAN_POINT('Ctrl Pts',(3.81246415607458,-18.4347501956728,1.51735346837426));
#81946=CARTESIAN_POINT('Ctrl Pts',(3.753859970967,-18.4686064148437,1.50790658895422));
#81947=CARTESIAN_POINT('Ctrl Pts',(3.66185171063921,-18.5630731192789,1.48156642851933));
#81948=CARTESIAN_POINT('Ctrl Pts',(3.63176679199362,-18.6893214659412,1.4463890385369));
#81949=CARTESIAN_POINT('Ctrl Pts',(3.63525637590299,-18.7550043776421,1.42809242464829));
#81950=CARTESIAN_POINT('Ctrl Pts',(3.65691132327402,-18.8162991820994,1.41102300383918));
#81951=CARTESIAN_POINT('Ctrl Pts',(3.69310713738719,-18.8681707290433,1.39658248257056));
#81952=CARTESIAN_POINT('Ctrl Pts',(3.94208066889,-18.4179535709002,1.52203266331995));
#81953=CARTESIAN_POINT('Ctrl Pts',(3.94208066889,-18.4159570093382,1.51487465397101));
#81954=CARTESIAN_POINT('Ctrl Pts',(3.93939976457242,-18.4131329107994,1.50784646200859));
#81955=CARTESIAN_POINT('Ctrl Pts',(3.93403795593725,-18.4094935804964,1.50114984350989));
#81956=CARTESIAN_POINT('Ctrl Pts',(3.92876493073444,-18.4059145119927,1.49456411087376));
#81957=CARTESIAN_POINT('Ctrl Pts',(3.9208990495868,-18.4015467557532,1.48829988745783));
#81958=CARTESIAN_POINT('Ctrl Pts',(3.91044031249432,-18.3964516676079,1.48255392252034));
#81959=CARTESIAN_POINT('Ctrl Pts',(3.90021604344847,-18.3914708031355,1.47693677286552));
#81960=CARTESIAN_POINT('Ctrl Pts',(3.88751387064069,-18.3857948927057,1.47181575064448));
#81961=CARTESIAN_POINT('Ctrl Pts',(3.87233379407099,-18.3795304027369,1.46736705768817));
#81962=CARTESIAN_POINT('Ctrl Pts',(3.86640409230692,-18.3770833427996,1.46562929158734));
#81963=CARTESIAN_POINT('Ctrl Pts',(3.86009629442993,-18.3745470069084,1.46399396287509));
#81964=CARTESIAN_POINT('Ctrl Pts',(3.85341040044,-18.3719297862815,1.46247080900171));
#81965=CARTESIAN_POINT('Origin',(2.225,-18.3216303794,1.54889979527));
#81966=CARTESIAN_POINT('Ctrl Pts',(3.94217663519884,-19.0766837901707,-1.2549536550141));
#81967=CARTESIAN_POINT('Ctrl Pts',(3.81239886354541,-19.076645554116,-1.25497330040668));
#81968=CARTESIAN_POINT('Ctrl Pts',(3.68259724249823,-19.1285376451827,-1.20779355502293));
#81969=CARTESIAN_POINT('Ctrl Pts',(3.60654250007182,-19.2341455692012,-1.1117978356177));
#81970=CARTESIAN_POINT('Ctrl Pts',(3.62070484051499,-19.3428207129455,-1.01302482729591));
#81971=CARTESIAN_POINT('Ctrl Pts',(3.69310717754101,-19.4225271378534,-0.94058821884175));
#81972=CARTESIAN_POINT('Ctrl Pts',(3.94218096368045,-19.0678969965114,-1.24528619924438));
#81973=CARTESIAN_POINT('Ctrl Pts',(3.8124013649262,-19.0766775490856,-1.25501070217547));
#81974=CARTESIAN_POINT('Ctrl Pts',(3.68259791616145,-19.1312291346839,-1.21075808335523));
#81975=CARTESIAN_POINT('Ctrl Pts',(3.60654273595517,-19.2294730875314,-1.10665936685993));
#81976=CARTESIAN_POINT('Ctrl Pts',(3.62070664165137,-19.324292537579,-0.992640516836252));
#81977=CARTESIAN_POINT('Ctrl Pts',(3.6931112295076,-19.3896240982595,-0.904387480917484));
#81978=CARTESIAN_POINT('Ctrl Pts',(3.93559125826023,-19.0576325988436,-1.23716461215919));
#81979=CARTESIAN_POINT('Ctrl Pts',(3.80845383863766,-19.0782981623898,-1.25360525685934));
#81980=CARTESIAN_POINT('Ctrl Pts',(3.68129345587565,-19.1367489342405,-1.21109305480358));
#81981=CARTESIAN_POINT('Ctrl Pts',(3.60588262725552,-19.2256736017137,-1.10083844359046));
#81982=CARTESIAN_POINT('Ctrl Pts',(3.61778298506652,-19.303259371832,-0.974962537597518));
#81983=CARTESIAN_POINT('Ctrl Pts',(3.68693955445337,-19.3511924443395,-0.873971611157963));
#81984=CARTESIAN_POINT('Ctrl Pts',(3.92284245621784,-19.0467376773103,-1.23131009492543));
#81985=CARTESIAN_POINT('Ctrl Pts',(3.80072347300955,-19.0792164390004,-1.24869960618928));
#81986=CARTESIAN_POINT('Ctrl Pts',(3.67858320514373,-19.1408681690318,-1.20498191179878));
#81987=CARTESIAN_POINT('Ctrl Pts',(3.60440977323658,-19.2195819167867,-1.09137485002728));
#81988=CARTESIAN_POINT('Ctrl Pts',(3.61202315176679,-19.2796909254035,-0.959797114573344));
#81989=CARTESIAN_POINT('Ctrl Pts',(3.67499936923216,-19.3103986831458,-0.852034828687459));
#81990=CARTESIAN_POINT('Ctrl Pts',(3.90640478505367,-19.0359499558752,-1.22729253742374));
#81991=CARTESIAN_POINT('Ctrl Pts',(3.78964230727276,-19.0775111308421,-1.24255371131931));
#81992=CARTESIAN_POINT('Ctrl Pts',(3.67286028089071,-19.1403088898408,-1.19643924561693));
#81993=CARTESIAN_POINT('Ctrl Pts',(3.60013259824114,-19.2091437100303,-1.08137464614068));
#81994=CARTESIAN_POINT('Ctrl Pts',(3.60330978482216,-19.2540235088518,-0.947806978160459));
#81995=CARTESIAN_POINT('Ctrl Pts',(3.65960361600605,-19.269997643815,-0.836974012631725));
#81996=CARTESIAN_POINT('Ctrl Pts',(3.8871831332344,-19.0254336179556,-1.22483553825469));
#81997=CARTESIAN_POINT('Ctrl Pts',(3.7758044692101,-19.0736895981168,-1.23616614954179));
#81998=CARTESIAN_POINT('Ctrl Pts',(3.66440795692671,-19.1360639649269,-1.18720250561116));
#81999=CARTESIAN_POINT('Ctrl Pts',(3.59323382499553,-19.195527288658,-1.07212003077549));
#82000=CARTESIAN_POINT('Ctrl Pts',(3.5920786079709,-19.2271843326888,-0.939102925829812));
#82001=CARTESIAN_POINT('Ctrl Pts',(3.64159969192542,-19.2306075924216,-0.827755843337992));
#82002=CARTESIAN_POINT('Ctrl Pts',(3.88711718104,-19.0254782582987,-1.22484599945563));
#82003=CARTESIAN_POINT('Ctrl Pts',(3.90102713913336,-19.0330874010163,-1.22662745096361));
#82004=CARTESIAN_POINT('Ctrl Pts',(3.91229688764402,-19.0404164069268,-1.22928808656999));
#82005=CARTESIAN_POINT('Ctrl Pts',(3.92092642657198,-19.0472854309651,-1.23271122429632));
#82006=CARTESIAN_POINT('Ctrl Pts',(3.92972882390163,-19.0542920485095,-1.23620293093707));
#82007=CARTESIAN_POINT('Ctrl Pts',(3.93578418014501,-19.0608195794311,-1.24048724663272));
#82008=CARTESIAN_POINT('Ctrl Pts',(3.93909249530211,-19.0667202939656,-1.24540700575729));
#82009=CARTESIAN_POINT('Ctrl Pts',(3.94108457006763,-19.0702733606974,-1.24836939825591));
#82010=CARTESIAN_POINT('Ctrl Pts',(3.94208063718359,-19.0736000363802,-1.25156159772694));
#82011=CARTESIAN_POINT('Ctrl Pts',(3.94208069665,-19.0766762824038,-1.25494542799359));
#82012=CARTESIAN_POINT('Origin',(2.225,-19.0026826744,-1.32221314666));
#82013=CARTESIAN_POINT('Origin',(-4.35,-1.95899712601,-5.55542016568));
#82014=CARTESIAN_POINT('',(-4.45,4.7773238354,-5.55542016568));
#82015=CARTESIAN_POINT('Origin',(-4.35,4.7773238354,-5.55542016568));
#82016=CARTESIAN_POINT('',(-4.45,-10.4080160928,-5.55542016568));
#82017=CARTESIAN_POINT('Origin',(-4.35,-10.4080160928,-5.55542016568));
#82018=CARTESIAN_POINT('',(-4.45,-2.8153461287,-5.55542016568));
#82019=CARTESIAN_POINT('Origin',(-4.35,-10.4080160928,-4.65542016568));
#82020=CARTESIAN_POINT('',(-4.45,-10.7858544195,-5.47226666221));
#82021=CARTESIAN_POINT('Origin',(-4.35,-10.7858544195,-5.47226666221));
#82022=CARTESIAN_POINT('Origin',(-4.45,-10.4080160928,-4.65542016568));
#82023=CARTESIAN_POINT('Origin',(-4.35,-15.667308925,-3.214314146));
#82024=CARTESIAN_POINT('',(-4.45,-18.9794133856,-1.68227598146));
#82025=CARTESIAN_POINT('Origin',(-4.35,-18.9794133856,-1.68227598146));
#82026=CARTESIAN_POINT('',(-4.45,-14.8826339026,-3.57727132183));
#82027=CARTESIAN_POINT('Origin',(-4.35,-18.895449313,-1.50075453779));
#82028=CARTESIAN_POINT('',(-4.45,-19.0409285996,-1.36351104187));
#82029=CARTESIAN_POINT('Origin',(-4.35,-19.0409285996,-1.36351104187));
#82030=CARTESIAN_POINT('Origin',(-4.45,-18.895449313,-1.50075453779));
#82031=CARTESIAN_POINT('Origin',(-4.35,-18.2859995693,2.04127093829));
#82032=CARTESIAN_POINT('',(-4.45,-18.4234397556,2.18656441774));
#82033=CARTESIAN_POINT('Origin',(-4.35,-18.4234397556,2.18656441774));
#82034=CARTESIAN_POINT('Origin',(-4.45,-18.2859995693,2.04127093829));
#82035=CARTESIAN_POINT('Origin',(-4.35,-18.85379408,1.77947127938));
#82036=CARTESIAN_POINT('',(-4.45,-14.4995104256,5.89840049188));
#82037=CARTESIAN_POINT('Origin',(-4.35,-14.4995104256,5.89840049188));
#82038=CARTESIAN_POINT('',(-4.45,-16.4614750906,4.04248245481));
#82039=CARTESIAN_POINT('Origin',(-4.35,-13.881029587,5.24457983432));
#82040=CARTESIAN_POINT('',(-4.45,-13.881029587,6.14457983432));
#82041=CARTESIAN_POINT('Origin',(-4.35,-13.881029587,6.14457983432));
#82042=CARTESIAN_POINT('Origin',(-4.45,-13.881029587,5.24457983432));
#82043=CARTESIAN_POINT('Origin',(-4.35,-1.95899712601,6.14457983432));
#82044=CARTESIAN_POINT('',(-4.45,-7.67105043563,6.14457983432));
#82045=CARTESIAN_POINT('Origin',(-4.35,-7.67105043563,6.14457983432));
#82046=CARTESIAN_POINT('',(-4.45,-10.7760400113,6.14457983432));
#82047=CARTESIAN_POINT('Origin',(-4.35,-7.67105043563,5.74457983432));
#82048=CARTESIAN_POINT('',(-4.45,-7.50411762961,6.1080814688));
#82049=CARTESIAN_POINT('Origin',(-4.35,-7.50411762961,6.1080814688));
#82050=CARTESIAN_POINT('Origin',(-4.45,-7.67105043563,5.74457983432));
#82051=CARTESIAN_POINT('Origin',(-4.35,4.59408048322,0.552161034916));
#82052=CARTESIAN_POINT('',(-4.45,-2.49116133917,3.80595465384));
#82053=CARTESIAN_POINT('Origin',(-4.35,-2.49116133917,3.80595465384));
#82054=CARTESIAN_POINT('',(-4.45,-4.99763948439,4.95701806132));
#82055=CARTESIAN_POINT('Origin',(-4.35,-2.24076213014,4.35120710557));
#82056=CARTESIAN_POINT('',(-4.45,-2.24076213014,3.75120710557));
#82057=CARTESIAN_POINT('Origin',(-4.35,-2.24076213014,3.75120710557));
#82058=CARTESIAN_POINT('Origin',(-4.45,-2.24076213014,4.35120710557));
#82059=CARTESIAN_POINT('Origin',(-4.35,-1.95899712601,3.75120710557));
#82060=CARTESIAN_POINT('',(-4.45,2.48275227055,3.75120710557));
#82061=CARTESIAN_POINT('Origin',(-4.35,2.48275227055,3.75120710557));
#82062=CARTESIAN_POINT('',(-4.45,0.120995070207,3.75120710557));
#82063=CARTESIAN_POINT('Origin',(-4.35,2.48275227055,4.35120710557));
#82064=CARTESIAN_POINT('',(-4.45,2.97160656206,4.00332568658));
#82065=CARTESIAN_POINT('Origin',(-4.35,2.97160656206,4.00332568658));
#82066=CARTESIAN_POINT('Origin',(-4.45,2.48275227055,4.35120710557));
#82067=CARTESIAN_POINT('Origin',(-4.35,0.332366624557,0.294579834316));
#82068=CARTESIAN_POINT('',(-4.45,4.32269078618,5.90191320834));
#82069=CARTESIAN_POINT('Origin',(-4.35,4.32269078618,5.90191320834));
#82070=CARTESIAN_POINT('',(-4.45,3.64714867412,4.95261944746));
#82071=CARTESIAN_POINT('Origin',(2.225,4.32269078618,5.90191320834));
#82072=CARTESIAN_POINT('Origin',(-4.35,4.32269078618,5.90191320834));
#82073=CARTESIAN_POINT('Origin',(-4.35,-1.95899712601,5.90191320834));
#82074=CARTESIAN_POINT('',(-4.45,4.7773238354,5.90191320834));
#82075=CARTESIAN_POINT('Origin',(-4.35,4.7773238354,5.90191320834));
#82076=CARTESIAN_POINT('',(-4.45,4.55000731079,5.90191320834));
#82077=CARTESIAN_POINT('Origin',(-4.35,4.32269078618,5.90191320834));
#82078=CARTESIAN_POINT('Origin',(2.225,4.7773238354,5.90191320834));
#82079=CARTESIAN_POINT('Origin',(-4.35,4.7773238354,5.90191320834));
#82080=CARTESIAN_POINT('Origin',(-4.35,4.7773238354,0.294579834316));
#82081=CARTESIAN_POINT('',(-4.45,4.7773238354,4.22878088412));
#82082=CARTESIAN_POINT('Origin',(-4.35,4.7773238354,4.22878088412));
#82083=CARTESIAN_POINT('',(-4.45,4.7773238354,5.06534704623));
#82084=CARTESIAN_POINT('Origin',(-4.35,4.7773238354,5.90191320834));
#82085=CARTESIAN_POINT('Origin',(-4.35,4.9773238354,4.22878088412));
#82086=CARTESIAN_POINT('',(-4.45,4.9773238354,4.02878088412));
#82087=CARTESIAN_POINT('Origin',(-4.35,4.9773238354,4.02878088412));
#82088=CARTESIAN_POINT('Origin',(-4.45,4.9773238354,4.22878088412));
#82089=CARTESIAN_POINT('Origin',(-4.35,-1.95899712601,4.02878088412));
#82090=CARTESIAN_POINT('',(-4.45,15.177455061,4.02878088412));
#82091=CARTESIAN_POINT('Origin',(-4.35,15.177455061,4.02878088412));
#82092=CARTESIAN_POINT('',(-4.45,10.0773894482,4.02878088412));
#82093=CARTESIAN_POINT('Origin',(2.225,15.177455061,4.02878088412));
#82094=CARTESIAN_POINT('Origin',(-4.35,15.177455061,4.02878088412));
#82095=CARTESIAN_POINT('Origin',(-4.35,15.177455061,0.294579834316));
#82096=CARTESIAN_POINT('',(-4.45,15.177455061,-4.67121911588));
#82097=CARTESIAN_POINT('Origin',(-4.35,15.177455061,-4.67121911588));
#82098=CARTESIAN_POINT('',(-4.45,15.177455061,-0.32121911588));
#82099=CARTESIAN_POINT('Origin',(-4.35,15.177455061,4.02878088412));
#82100=CARTESIAN_POINT('Origin',(2.225,15.177455061,-4.67121911588));
#82101=CARTESIAN_POINT('Origin',(-4.35,15.177455061,-4.67121911588));
#82102=CARTESIAN_POINT('Origin',(-4.35,-1.95899712601,-4.67121911588));
#82103=CARTESIAN_POINT('',(-4.45,4.9773238354,-4.67121911588));
#82104=CARTESIAN_POINT('Origin',(-4.35,4.9773238354,-4.67121911588));
#82105=CARTESIAN_POINT('',(-4.45,10.0773894482,-4.67121911588));
#82106=CARTESIAN_POINT('Origin',(-4.35,15.177455061,-4.67121911588));
#82107=CARTESIAN_POINT('Origin',(-4.35,4.9773238354,-4.87121911588));
#82108=CARTESIAN_POINT('',(-4.45,4.7773238354,-4.87121911588));
#82109=CARTESIAN_POINT('Origin',(-4.35,4.7773238354,-4.87121911588));
#82110=CARTESIAN_POINT('Origin',(-4.45,4.9773238354,-4.87121911588));
#82111=CARTESIAN_POINT('Origin',(-4.35,4.7773238354,0.294579834316));
#82112=CARTESIAN_POINT('',(-4.45,4.7773238354,-5.21331964078));
#82113=CARTESIAN_POINT('Origin',(4.35,0.,0.));
#82114=CARTESIAN_POINT('',(4.35,-10.5742356128,0.47366156039));
#82115=CARTESIAN_POINT('Origin',(4.35,-9.17423561284,0.47366156039));
#82116=CARTESIAN_POINT('Origin',(-4.35,-18.3216303794,1.54889979527));
#82117=CARTESIAN_POINT('Origin',(-4.35,-18.3216303794,1.54889979527));
#82118=CARTESIAN_POINT('Origin',(-7.44184532531,-9.17423561283998,0.473661560388455));
#82119=CARTESIAN_POINT('',(-5.0771333862,-11.8030366882,0.47366156039));
#82120=CARTESIAN_POINT('Origin',(-5.0771333862,-9.17423561284,0.47366156039));
#82121=CARTESIAN_POINT('',(-5.31156614753,-11.6198777414,0.47366156039));
#82122=CARTESIAN_POINT('',(-7.44184532530999,-9.95552123934695,0.473661560388455));
#82123=CARTESIAN_POINT('',(-5.31156614753,-6.74197323652571,0.218191104751761));
#82124=CARTESIAN_POINT('Origin',(-5.31156614753,-9.17423561284,0.473661560391));
#82125=CARTESIAN_POINT('Origin',(-5.31156614753,-9.17423561284,0.473661560391));
#82126=CARTESIAN_POINT('Origin',(4.4408920985E-16,-18.4073812884,1.48310265486));
#82127=CARTESIAN_POINT('',(-4.35,-17.9397782658,1.2109699402));
#82128=CARTESIAN_POINT('',(-4.35,-14.0218073513,-1.06918653748));
#82129=CARTESIAN_POINT('',(-3.225,-17.9397782658,1.2109699402));
#82130=CARTESIAN_POINT('Origin',(-2.3,-9.17423561284,0.47366156039));
#82131=CARTESIAN_POINT('',(-2.3,-11.82423561284,0.47366156039));
#82132=CARTESIAN_POINT('Origin',(-2.3,-9.17423561284,0.47366156039));
#82133=CARTESIAN_POINT('Origin',(-2.3,-12.12423561284,0.47366156039));
#82134=CARTESIAN_POINT('Origin',(-2.3,-12.0504559477,4.80274328646));
#82135=CARTESIAN_POINT('',(-2.3,-12.9053426461,5.10274328646));
#82136=CARTESIAN_POINT('Origin',(-2.3,-12.9053426461,4.80274328646));
#82137=CARTESIAN_POINT('',(-2.3,-9.41827086707,5.10274328646));
#82138=CARTESIAN_POINT('',(-2.3,-11.1618067566,5.10274328646));
#82139=CARTESIAN_POINT('Origin',(-2.3,-9.41827086707,4.80274328646));
#82140=CARTESIAN_POINT('Origin',(-2.3,-12.9053426461,4.10274328646));
#82141=CARTESIAN_POINT('',(-2.3,-13.5925435779,4.82921068375));
#82142=CARTESIAN_POINT('Origin',(-2.3,-13.3863832983,4.61127046457));
#82143=CARTESIAN_POINT('Origin',(-2.3,-12.9053426461,4.10274328646));
#82144=CARTESIAN_POINT('Origin',(-2.3,-10.0779006799,-3.15542016568));
#82145=CARTESIAN_POINT('',(-2.3,-10.0779006799,-4.15542016568));
#82146=CARTESIAN_POINT('Origin',(-2.3,-10.0779006799,-3.85542016568));
#82147=CARTESIAN_POINT('',(-2.3,-10.4977210429,-4.06302738404));
#82148=CARTESIAN_POINT('Origin',(-2.3,-10.0779006799,-3.15542016568));
#82149=CARTESIAN_POINT('Origin',(-2.3,-10.371774934,-3.79074521854));
#82150=CARTESIAN_POINT('Origin',(-2.3,-8.20939783898,-3.85542016568));
#82151=CARTESIAN_POINT('',(-2.3,-9.7480857735,-4.15542016568));
#82152=CARTESIAN_POINT('Origin',(-2.3,-8.67423561284,-4.1493785649));
#82153=CARTESIAN_POINT('',(-2.3,-8.7279990537,-3.65227747616));
#82154=CARTESIAN_POINT('Origin',(-2.3,-8.76025711822,-3.35401682291));
#82155=CARTESIAN_POINT('Origin',(-2.3,-8.67423561284,-4.1493785649));
#82156=CARTESIAN_POINT('Origin',(-2.3,-17.1183636721,1.08100826706));
#82157=CARTESIAN_POINT('',(-2.3,-17.3245239517,1.29894848625));
#82158=CARTESIAN_POINT('Origin',(-2.3,-17.1183636721,1.08100826706));
#82159=CARTESIAN_POINT('Origin',(-2.3,-17.1183636721,1.08100826706));
#82160=CARTESIAN_POINT('Origin',(-2.3,-16.3982789105,1.76217155265));
#82161=CARTESIAN_POINT('',(-2.3,-15.4585337648,3.064079585));
#82162=CARTESIAN_POINT('Origin',(-2.3,-17.3209666442,-0.597405571358));
#82163=CARTESIAN_POINT('',(-2.30000000000001,-17.3847397931138,-0.890548863178005));
#82164=CARTESIAN_POINT('Origin',(-2.3,-17.3209666442,-0.597405571358));
#82165=CARTESIAN_POINT('Ctrl Pts',(-2.15473685769753,-17.5697153662214,
-0.513604063130804));
#82166=CARTESIAN_POINT('Ctrl Pts',(-2.15395405942168,-17.574609993053,-0.529489742692386));
#82167=CARTESIAN_POINT('Ctrl Pts',(-2.15388324244328,-17.5783881601095,
-0.545799682384687));
#82168=CARTESIAN_POINT('Ctrl Pts',(-2.15451525157936,-17.5809692196611,
-0.562293625661652));
#82169=CARTESIAN_POINT('Ctrl Pts',(-2.1551503423395,-17.5835628642447,-0.578867992036593));
#82170=CARTESIAN_POINT('Ctrl Pts',(-2.1564949444798,-17.5849474880118,-0.595627317314118));
#82171=CARTESIAN_POINT('Ctrl Pts',(-2.15851501242277,-17.5850869864651,
-0.612320097566757));
#82172=CARTESIAN_POINT('Ctrl Pts',(-2.16056754790439,-17.5852287270071,
-0.629281172502292));
#82173=CARTESIAN_POINT('Ctrl Pts',(-2.16331716225515,-17.5840849489386,
-0.646172685370115));
#82174=CARTESIAN_POINT('Ctrl Pts',(-2.1667060874432,-17.5816670068449,-0.662735914936609));
#82175=CARTESIAN_POINT('Ctrl Pts',(-2.17014082128786,-17.5792163810321,
-0.679523032388902));
#82176=CARTESIAN_POINT('Ctrl Pts',(-2.17423187430862,-17.5754571498334,
-0.695972148081803));
#82177=CARTESIAN_POINT('Ctrl Pts',(-2.1789017592561,-17.5704498287427,-0.711831777793248));
#82178=CARTESIAN_POINT('Ctrl Pts',(-2.18365732878883,-17.5653506316774,
-0.727982405207925));
#82179=CARTESIAN_POINT('Ctrl Pts',(-2.18901271728734,-17.5589575689096,
-0.743521087226289));
#82180=CARTESIAN_POINT('Ctrl Pts',(-2.19487469522746,-17.5513795105412,
-0.758211607690351));
#82181=CARTESIAN_POINT('Ctrl Pts',(-2.20088007215961,-17.5436160734589,
-0.773261495905079));
#82182=CARTESIAN_POINT('Ctrl Pts',(-2.20741666432177,-17.5346095538899,
-0.787420812647958));
#82183=CARTESIAN_POINT('Ctrl Pts',(-2.21437945983172,-17.5245157190218,
-0.800474272147822));
#82184=CARTESIAN_POINT('Ctrl Pts',(-2.22171459988143,-17.5138821032147,
-0.814225782360628));
#82185=CARTESIAN_POINT('Ctrl Pts',(-2.22952228939455,-17.5020423686272,
-0.826749707962301));
#82186=CARTESIAN_POINT('Ctrl Pts',(-2.23768186400214,-17.4892117556151,
-0.837842740719717));
#82187=CARTESIAN_POINT('Ctrl Pts',(-2.24617531542753,-17.4758561343214,
-0.84938968273771));
#82188=CARTESIAN_POINT('Ctrl Pts',(-2.25504971643787,-17.4614274905277,
-0.859386461572597));
#82189=CARTESIAN_POINT('Ctrl Pts',(-2.26417755548704,-17.4461935944183,
-0.867655388024234));
#82190=CARTESIAN_POINT('Ctrl Pts',(-2.27393424211809,-17.4299101838862,
-0.876493988675408));
#82191=CARTESIAN_POINT('Ctrl Pts',(-2.28398040584175,-17.4127068136573,
-0.883358866726679));
#82192=CARTESIAN_POINT('Ctrl Pts',(-2.29417357219113,-17.3949324822234,
-0.888085993031839));
#82193=CARTESIAN_POINT('Ctrl Pts',(-2.29611068012178,-17.3915546507232,
-0.888984335464508));
#82194=CARTESIAN_POINT('Ctrl Pts',(-2.29805313306564,-17.3881562612702,
-0.88980560552101));
#82195=CARTESIAN_POINT('Ctrl Pts',(-2.3,-17.3847398009031,-0.890548854556042));
#82196=CARTESIAN_POINT('Origin',(-2.3,-17.4910283166,-1.37912101035));
#82197=CARTESIAN_POINT('',(-2.3,-17.2811181351,-0.925317401172));
#82198=CARTESIAN_POINT('Origin',(-2.3,-17.1551720262,-0.653035235664));
#82199=CARTESIAN_POINT('Origin',(-2.3,-17.4910283166,-1.37912101035));
#82200=CARTESIAN_POINT('Origin',(-2.3,-13.7337583338,-2.23563518556));
#82201=CARTESIAN_POINT('',(-2.3,-13.889419589,-2.49417239261));
#82202=CARTESIAN_POINT('Origin',(-2.3,-8.67423561284,5.09670168568));
#82203=CARTESIAN_POINT('',(-2.3,-9.13925764673,4.91297768617));
#82204=CARTESIAN_POINT('Origin',(-2.3,-9.41827086707,4.80274328646));
#82205=CARTESIAN_POINT('',(-2.3,-8.7279990537,4.59960059693));
#82206=CARTESIAN_POINT('Origin',(-2.3,-8.67423561284,5.09670168568));
#82207=CARTESIAN_POINT('Origin',(-2.3,-8.76025711822,4.30133994369));
#82208=CARTESIAN_POINT('Origin',(-2.3,-9.17423561284,0.47366156039));
#82209=CARTESIAN_POINT('Origin',(-2.3,-9.17423561284,0.47366156039));
#82210=CARTESIAN_POINT('Origin',(4.4408920985E-16,-17.4373752488,-0.853039529372));
#82211=CARTESIAN_POINT('',(-4.35,-17.6050062358,-0.892285274267));
#82212=CARTESIAN_POINT('',(-3.225,-17.6050062358,-0.892285274267));
#82213=CARTESIAN_POINT('',(-4.35,-1.98179270986,2.76541944482));
#82214=CARTESIAN_POINT('Origin',(-5.25,-9.17423561284,0.473661560391));
#82215=CARTESIAN_POINT('',(-5.35,-6.82034320266343,0.226422622515883));
#82216=CARTESIAN_POINT('Origin',(-5.25,-6.82034320266825,0.226422622516389));
#82217=CARTESIAN_POINT('',(-5.35,-6.8073945597,0.473677431302));
#82218=CARTESIAN_POINT('Origin',(-5.35,-9.17423561282425,0.473661560374535));
#82219=CARTESIAN_POINT('',(-5.35,-11.541076666,0.47366441431));
#82220=CARTESIAN_POINT('Origin',(-5.35,-9.17423561282426,0.47366156039));
#82221=CARTESIAN_POINT('Origin',(-5.35,-9.17423561282425,0.473661560374535));
#82222=CARTESIAN_POINT('Origin',(-4.35,4.32269078618,5.90191320834));
#82223=CARTESIAN_POINT('Origin',(-4.35,4.7773238354,5.90191320834));
#82224=CARTESIAN_POINT('Origin',(-4.35,15.177455061,4.02878088412));
#82225=CARTESIAN_POINT('Origin',(-4.35,15.177455061,-4.67121911588));
#82226=CARTESIAN_POINT('Origin',(0.,-9.17423561284,0.47366156039));
#82227=CARTESIAN_POINT('',(-5.35,-10.5742356128,0.47366156039));
#82228=CARTESIAN_POINT('Origin',(-5.35,-9.17423561284,0.47366156039));
#82229=CARTESIAN_POINT('',(0.,-10.57423561284,0.473661560390001));
#82230=CARTESIAN_POINT('Origin',(-4.35,-13.9715079445,-0.982757551184));
#82231=CARTESIAN_POINT('',(-4.45,-17.889478859,1.2973989265));
#82232=CARTESIAN_POINT('',(-4.45,-18.1055546192,1.42314936088));
#82233=CARTESIAN_POINT('Origin',(-4.35,-17.889478859,1.2973989265));
#82234=CARTESIAN_POINT('Origin',(-4.35,-17.6882812316,1.64311487169));
#82235=CARTESIAN_POINT('',(-4.35,-17.3446807657,1.27988117305));
#82236=CARTESIAN_POINT('Origin',(-4.35,-17.6882812316,1.64311487169));
#82237=CARTESIAN_POINT('',(-4.45,-17.4134008589,1.35252791278));
#82238=CARTESIAN_POINT('Origin',(-4.45,-17.6882812316,1.64311487169));
#82239=CARTESIAN_POINT('Origin',(-4.35,-17.4134008589,1.35252791278));
#82240=CARTESIAN_POINT('Origin',(-4.35,-17.907928075,0.88473050722));
#82241=CARTESIAN_POINT('',(-4.35,-13.5925435779,4.82921068375));
#82242=CARTESIAN_POINT('',(-4.35,-15.4686121718,3.0545459284));
#82243=CARTESIAN_POINT('',(-4.45,-13.661263671,4.90185742348));
#82244=CARTESIAN_POINT('',(-4.45,-15.537332265,3.12719266813));
#82245=CARTESIAN_POINT('Origin',(-4.35,-13.661263671,4.90185742348));
#82246=CARTESIAN_POINT('Origin',(-4.35,-12.9053426461,4.10274328646));
#82247=CARTESIAN_POINT('',(-4.35,-12.9053426461,5.10274328646));
#82248=CARTESIAN_POINT('Origin',(-4.35,-12.9053426461,4.10274328646));
#82249=CARTESIAN_POINT('',(-4.45,-12.9053426461,5.20274328646));
#82250=CARTESIAN_POINT('Origin',(-4.45,-12.9053426461,4.10274328646));
#82251=CARTESIAN_POINT('Origin',(-4.35,-12.9053426461,5.20274328646));
#82252=CARTESIAN_POINT('Origin',(-4.35,-1.95899712601,5.20274328646));
#82253=CARTESIAN_POINT('',(-4.35,-8.31430322211,5.10274328646));
#82254=CARTESIAN_POINT('',(-4.35,-10.6098229341,5.10274328646));
#82255=CARTESIAN_POINT('',(-4.45,-8.31430322211,5.20274328646));
#82256=CARTESIAN_POINT('',(-4.45,-10.6098229341,5.20274328646));
#82257=CARTESIAN_POINT('Origin',(-4.35,-8.31430322211,5.20274328646));
#82258=CARTESIAN_POINT('Origin',(-2.3,-9.41827086707,4.80274328646));
#82259=CARTESIAN_POINT('Origin',(-2.3,-9.41827086707,4.80274328646));
#82260=CARTESIAN_POINT('Origin',(3.225,-12.9053426461,4.10274328646));
#82261=CARTESIAN_POINT('',(-3.325,-12.9053426461,5.10274328646));
#82262=CARTESIAN_POINT('',(-3.325,-13.5925435779,4.82921068375));
#82263=CARTESIAN_POINT('Origin',(2.6645352591E-15,-19.4793690683,-1.15238185378));
#82264=CARTESIAN_POINT('',(-2.33871339239,-17.3446807657,1.27988117305));
#82265=CARTESIAN_POINT('Origin',(-2.33872773956445,-17.1384751807674,1.06192182456203));
#82266=CARTESIAN_POINT('Origin',(9.50350909079E-14,-19.6855293478,-0.934441634591));
#82267=CARTESIAN_POINT('Origin',(0.,-13.3033814002,5.10274328646));
#82268=CARTESIAN_POINT('',(-3.225,-17.3446807657,1.27988117305));
#82269=CARTESIAN_POINT('Origin',(-5.01556723867,-9.17423561284,0.47366156039));
#82270=CARTESIAN_POINT('',(-5.01556723867,-11.8242356128,0.47366156039));
#82271=CARTESIAN_POINT('Origin',(-5.01556723867,-11.72423561284,0.47366156039));
#82272=CARTESIAN_POINT('Origin',(-5.01556723867,-9.17423561284,0.47366156039));
#82273=CARTESIAN_POINT('Origin',(-5.35,0.,0.));
#82274=CARTESIAN_POINT('Origin',(-4.3,-2.12788809108,3.34387696505));
#82275=CARTESIAN_POINT('',(-4.,-2.69184369587,2.1725725316));
#82276=CARTESIAN_POINT('',(-4.3,-2.56170009476,2.4428735547));
#82277=CARTESIAN_POINT('Origin',(-4.3,-2.69184369587,2.1725725316));
#82278=CARTESIAN_POINT('',(-4.3,-2.12788809108,2.34387696505));
#82279=CARTESIAN_POINT('Origin',(-4.3,-2.12788809108,3.34387696505));
#82280=CARTESIAN_POINT('',(-4.,-2.12788809108,2.04387696505));
#82281=CARTESIAN_POINT('Origin',(-4.3,-2.12788809108,2.04387696505));
#82282=CARTESIAN_POINT('Origin',(-4.,-2.12788809108,3.34387696505));
#82283=CARTESIAN_POINT('Origin',(3.225,-9.41827086707,-3.85542016568));
#82284=CARTESIAN_POINT('',(-3.7,-9.13925764671,-3.96565456533));
#82285=CARTESIAN_POINT('',(3.,-9.13925764673,-3.96565456539));
#82286=CARTESIAN_POINT('',(-3.69999999774,-9.41827086749,-4.15542016568));
#82287=CARTESIAN_POINT('Origin',(-3.69999999887,-9.41827086707,-3.85542016568));
#82288=CARTESIAN_POINT('',(-3.,-9.41827086707,-4.15542016568));
#82289=CARTESIAN_POINT('Ctrl Pts',(-4.,2.8773238354,2.04387696505));
#82290=CARTESIAN_POINT('Ctrl Pts',(-4.,3.0773238354,2.04387696505));
#82291=CARTESIAN_POINT('Ctrl Pts',(-4.,3.0773238354,1.84387696505));
#82292=CARTESIAN_POINT('Ctrl Pts',(-4.,2.8773238354,2.34387696505));
#82293=CARTESIAN_POINT('Ctrl Pts',(-4.,3.3773238354,2.34387696505));
#82294=CARTESIAN_POINT('Ctrl Pts',(-4.,3.3773238354,1.84387696505));
#82295=CARTESIAN_POINT('Ctrl Pts',(-4.3,2.8773238354,2.34387696505));
#82296=CARTESIAN_POINT('Ctrl Pts',(-4.3,3.3773238354,2.34387696505));
#82297=CARTESIAN_POINT('Ctrl Pts',(-4.3,3.3773238354,1.84387696505));
#82298=CARTESIAN_POINT('',(-4.,2.8773238354,2.04387696505));
#82299=CARTESIAN_POINT('',(-4.3,2.8773238354,2.34387696505));
#82300=CARTESIAN_POINT('Origin',(-4.3,2.8773238354,2.04387696505));
#82301=CARTESIAN_POINT('',(-4.3,3.3773238354,1.84387696505));
#82302=CARTESIAN_POINT('Origin',(-4.3,2.8773238354,1.84387696505));
#82303=CARTESIAN_POINT('',(-4.,3.0773238354,1.84387696505));
#82304=CARTESIAN_POINT('Origin',(-4.3,3.0773238354,1.84387696505));
#82305=CARTESIAN_POINT('Origin',(-4.,2.8773238354,1.84387696505));
#82306=CARTESIAN_POINT('Origin',(-4.3,-2.74845588872,2.04387696505));
#82307=CARTESIAN_POINT('',(-4.3,0.374717872161,2.34387696505));
#82308=CARTESIAN_POINT('',(-4.,0.374717872161,2.04387696505));
#82309=CARTESIAN_POINT('Ctrl Pts',(-3.53153643377,-17.9397782186,1.21096972349));
#82310=CARTESIAN_POINT('Ctrl Pts',(-3.43735921762,-18.0003262942,1.24620711182));
#82311=CARTESIAN_POINT('Ctrl Pts',(-3.34318200148,-18.0897485133,1.23183031842));
#82312=CARTESIAN_POINT('Ctrl Pts',(-3.28035136998,-18.1886331834,1.15483650889));
#82313=CARTESIAN_POINT('Ctrl Pts',(-3.27308209541,-18.2588703936,1.04489890981));
#82314=CARTESIAN_POINT('Ctrl Pts',(-3.30849201868,-18.2908119879,0.937647001707));
#82315=CARTESIAN_POINT('Ctrl Pts',(-3.44407910476,-17.8762683682,1.17400854083));
#82316=CARTESIAN_POINT('Ctrl Pts',(-3.35980883034,-17.945884643,1.20261112942));
#82317=CARTESIAN_POINT('Ctrl Pts',(-3.27553855592,-18.0344942384,1.18180525286));
#82318=CARTESIAN_POINT('Ctrl Pts',(-3.21629253048,-18.1212598109,1.10210242162));
#82319=CARTESIAN_POINT('Ctrl Pts',(-3.20252794116,-18.1764816782,0.991308189139));
#82320=CARTESIAN_POINT('Ctrl Pts',(-3.22655830802,-18.1956140888,0.882244113432));
#82321=CARTESIAN_POINT('Ctrl Pts',(-3.3464798887,-17.8120594694,1.15225334483));
#82322=CARTESIAN_POINT('Ctrl Pts',(-3.27061651551,-17.8859816006,1.17073218793));
#82323=CARTESIAN_POINT('Ctrl Pts',(-3.19475314232,-17.9706270502,1.14263777494));
#82324=CARTESIAN_POINT('Ctrl Pts',(-3.13901290586,-18.0461110452,1.06262258853));
#82325=CARTESIAN_POINT('Ctrl Pts',(-3.12052271368,-18.0895777918,0.955511460449));
#82326=CARTESIAN_POINT('Ctrl Pts',(-3.1351232828,-18.0993679319,0.849634347569));
#82327=CARTESIAN_POINT('Ctrl Pts',(-3.24445759626,-17.7503923647,1.14165798595));
#82328=CARTESIAN_POINT('Ctrl Pts',(-3.17540943486,-17.8248792216,1.15059278692));
#82329=CARTESIAN_POINT('Ctrl Pts',(-3.10636127346,-17.9038800164,1.11677030553));
#82330=CARTESIAN_POINT('Ctrl Pts',(-3.05381470327,-17.9694500338,1.03769631264));
#82331=CARTESIAN_POINT('Ctrl Pts',(-3.03220663125,-18.0038208707,0.935228982262));
#82332=CARTESIAN_POINT('Ctrl Pts',(-3.03954447223,-18.006932574,0.833752309795));
#82333=CARTESIAN_POINT('Ctrl Pts',(-3.00710650148,-17.6178055192,1.13794464306));
#82334=CARTESIAN_POINT('Ctrl Pts',(-2.95127328323,-17.6885112346,1.12719077166));
#82335=CARTESIAN_POINT('Ctrl Pts',(-2.89544006498,-17.7531454598,1.08321253997));
#82336=CARTESIAN_POINT('Ctrl Pts',(-2.84959649515,-17.7987006574,1.00827828536));
#82337=CARTESIAN_POINT('Ctrl Pts',(-2.82308648415,-17.8163636325,0.917856141561));
#82338=CARTESIAN_POINT('Ctrl Pts',(-2.81718400147,-17.8081915572,0.828186375887));
#82339=CARTESIAN_POINT('Ctrl Pts',(-2.75866817858,-17.5019383088,1.17227759984));
#82340=CARTESIAN_POINT('Ctrl Pts',(-2.71204809217,-17.5606955711,1.14808808045));
#82341=CARTESIAN_POINT('Ctrl Pts',(-2.66542800575,-17.6093034777,1.10048544899));
#82342=CARTESIAN_POINT('Ctrl Pts',(-2.62523407894,-17.6396878429,1.03296291179));
#82343=CARTESIAN_POINT('Ctrl Pts',(-2.59761061232,-17.6474253317,0.955854949617));
#82344=CARTESIAN_POINT('Ctrl Pts',(-2.5844364843,-17.6345130992,0.879649456437));
#82345=CARTESIAN_POINT('Ctrl Pts',(-2.61902164686,-17.4433557891,1.20037711022));
#82346=CARTESIAN_POINT('Ctrl Pts',(-2.5768009727,-17.4944653366,1.17107895197));
#82347=CARTESIAN_POINT('Ctrl Pts',(-2.53458029853,-17.5345510327,1.12326065353));
#82348=CARTESIAN_POINT('Ctrl Pts',(-2.49727274202,-17.5577104896,1.06043707681));
#82349=CARTESIAN_POINT('Ctrl Pts',(-2.46964074457,-17.5611511175,0.990611628682));
#82350=CARTESIAN_POINT('Ctrl Pts',(-2.45360974016,-17.5467007921,0.921769238571));
#82351=CARTESIAN_POINT('Ctrl Pts',(-2.47860839712,-17.3907825954,1.23627120452));
#82352=CARTESIAN_POINT('Ctrl Pts',(-2.44020185655,-17.4338093447,1.20400270366));
#82353=CARTESIAN_POINT('Ctrl Pts',(-2.40179531599,-17.4659130997,1.15744985931));
#82354=CARTESIAN_POINT('Ctrl Pts',(-2.36716352241,-17.4829006471,1.09980337157));
#82355=CARTESIAN_POINT('Ctrl Pts',(-2.3399933307,-17.4830409793,1.03717095186));
#82356=CARTESIAN_POINT('Ctrl Pts',(-2.32206470888,-17.4678963173,0.975572621049));
#82357=CARTESIAN_POINT('Ctrl Pts',(-2.33871339239,-17.3446807657,1.27988117305));
#82358=CARTESIAN_POINT('Ctrl Pts',(-2.30368135741,-17.3797447841,1.24671240841));
#82359=CARTESIAN_POINT('Ctrl Pts',(-2.26864932242,-17.4046242104,1.20277710693));
#82360=CARTESIAN_POINT('Ctrl Pts',(-2.23651127409,-17.416397643,1.15078914283));
#82361=CARTESIAN_POINT('Ctrl Pts',(-2.21010973495,-17.414023754,1.09534670941));
#82362=CARTESIAN_POINT('Ctrl Pts',(-2.19100517814,-17.398792101,1.04094166862));
#82363=CARTESIAN_POINT('Ctrl Pts',(-2.33871339239,-17.3446807657,1.27988117305));
#82364=CARTESIAN_POINT('Ctrl Pts',(-2.37085722385345,-17.3552736346009,
1.26986086187324));
#82365=CARTESIAN_POINT('Ctrl Pts',(-2.40060138748257,-17.3654931419459,
1.26106505972869));
#82366=CARTESIAN_POINT('Ctrl Pts',(-2.42792441532416,-17.3751539348591,
1.25330473292905));
#82367=CARTESIAN_POINT('Ctrl Pts',(-2.45683268599488,-17.3853752331006,
1.24509416311528));
#82368=CARTESIAN_POINT('Ctrl Pts',(-2.48303144889736,-17.3949709404682,
1.23804288922432));
#82369=CARTESIAN_POINT('Ctrl Pts',(-2.50652519652193,-17.4037561126913,
1.23196427011995));
#82370=CARTESIAN_POINT('Ctrl Pts',(-2.52430430947977,-17.4104043738289,
1.22736421833548));
#82371=CARTESIAN_POINT('Ctrl Pts',(-2.54053497856681,-17.4165891620293,
1.22332190980238));
#82372=CARTESIAN_POINT('Ctrl Pts',(-2.55522602630707,-17.4222434165849,
1.2197694487075));
#82373=CARTESIAN_POINT('Ctrl Pts',(-2.57438046892142,-17.4296155316531,
1.21513768837394));
#82374=CARTESIAN_POINT('Ctrl Pts',(-2.59090554108931,-17.4360979659964,
1.21132852184931));
#82375=CARTESIAN_POINT('Ctrl Pts',(-2.6048009567519,-17.441601809986,1.20820745071824));
#82376=CARTESIAN_POINT('Ctrl Pts',(-2.60993120718498,-17.443633854129,1.20705513711276));
#82377=CARTESIAN_POINT('Ctrl Pts',(-2.61470302832676,-17.4455328588739,
1.20599698877206));
#82378=CARTESIAN_POINT('Ctrl Pts',(-2.61911644276473,-17.4472955559474,
1.2050275628334));
#82379=CARTESIAN_POINT('Ctrl Pts',(-2.62730007342115,-17.4505640597353,
1.20322999228066));
#82380=CARTESIAN_POINT('Ctrl Pts',(-2.63425131799992,-17.4533635882907,
1.20173688910744));
#82381=CARTESIAN_POINT('Ctrl Pts',(-2.63997017640731,-17.4556785810865,
1.20052048671079));
#82382=CARTESIAN_POINT('Ctrl Pts',(-2.642829605611,-17.4568360774844,1.19991228551246));
#82383=CARTESIAN_POINT('Ctrl Pts',(-2.64538093825375,-17.4578725207325,
1.19937341434368));
#82384=CARTESIAN_POINT('Ctrl Pts',(-2.64762417435145,-17.4587865567906,
1.1989012763582));
#82385=CARTESIAN_POINT('Ctrl Pts',(-2.6487457924003,-17.4592435748197,1.19866520736547));
#82386=CARTESIAN_POINT('Ctrl Pts',(-2.64979038631128,-17.4596699961906,
1.19844583132589));
#82387=CARTESIAN_POINT('Ctrl Pts',(-2.65075795608283,-17.4600656805176,
1.198242882505));
#82388=CARTESIAN_POINT('Ctrl Pts',(-2.65124174096861,-17.460263522681,1.19814140809456));
#82389=CARTESIAN_POINT('Ctrl Pts',(-2.65170626964839,-17.4604536819025,
1.19804404256586));
#82390=CARTESIAN_POINT('Ctrl Pts',(-2.65214192053663,-17.460632254491,1.19795273829656));
#82391=CARTESIAN_POINT('Ctrl Pts',(-2.65257757142488,-17.4608108270794,
1.19786143402726));
#82392=CARTESIAN_POINT('Ctrl Pts',(-2.65300365773986,-17.4609851971307,
1.19777165882951));
#82393=CARTESIAN_POINT('Ctrl Pts',(-2.65483063319514,-17.461736156073,1.19739003540087));
#82394=CARTESIAN_POINT('Ctrl Pts',(-2.68950642668481,-17.4759892743222,
1.19014686463782));
#82395=CARTESIAN_POINT('Ctrl Pts',(-2.72323913489447,-17.490340247288,1.18371785132662));
#82396=CARTESIAN_POINT('Ctrl Pts',(-2.75572764050077,-17.5045738471626,
1.17809425967101));
#82397=CARTESIAN_POINT('Ctrl Pts',(-2.77801459302075,-17.5143380255597,
1.17423650389304));
#82398=CARTESIAN_POINT('Ctrl Pts',(-2.79971637818909,-17.5240463924571,
1.17075696072237));
#82399=CARTESIAN_POINT('Ctrl Pts',(-2.8207410235801,-17.5336236381446,1.16764089921239));
#82400=CARTESIAN_POINT('Ctrl Pts',(-2.84657754344982,-17.5453928116027,
1.16381167005678));
#82401=CARTESIAN_POINT('Ctrl Pts',(-2.87138972981263,-17.556965111084,1.16052926742677));
#82402=CARTESIAN_POINT('Ctrl Pts',(-2.89517608835571,-17.5682913708109,
1.15772838507829));
#82403=CARTESIAN_POINT('Ctrl Pts',(-2.90706926762725,-17.5739545006744,
1.15632794390404));
#82404=CARTESIAN_POINT('Ctrl Pts',(-2.91870376450622,-17.5795588671794,
1.15504729109772));
#82405=CARTESIAN_POINT('Ctrl Pts',(-2.93008295529788,-17.585095124209,1.15387927549878));
#82406=CARTESIAN_POINT('Ctrl Pts',(-2.93577255069372,-17.5878632527238,
1.15329526769931));
#82407=CARTESIAN_POINT('Ctrl Pts',(-2.94139832389838,-17.5906143505413,
1.15273941070078));
#82408=CARTESIAN_POINT('Ctrl Pts',(-2.94696039348753,-17.5933476575522,
1.15221069698343));
#82409=CARTESIAN_POINT('Ctrl Pts',(-2.94974142828211,-17.5947143110577,
1.15194634012475));
#82410=CARTESIAN_POINT('Ctrl Pts',(-2.95250653708668,-17.5960765170342,
1.15168876905108));
#82411=CARTESIAN_POINT('Ctrl Pts',(-2.95525573651771,-17.5974341826461,
1.15143785739361));
#82412=CARTESIAN_POINT('Ctrl Pts',(-2.95780061870979,-17.598690948161,1.15120559319273));
#82413=CARTESIAN_POINT('Ctrl Pts',(-2.95930210470662,-17.5994332235654,
1.15106977482125));
#82414=CARTESIAN_POINT('Ctrl Pts',(-2.9626199252829,-17.6010788586254,1.15077824350422));
#82415=CARTESIAN_POINT('Ctrl Pts',(-2.96288629829677,-17.6012109793234,
1.15075483775524));
#82416=CARTESIAN_POINT('Ctrl Pts',(-2.96316437249295,-17.6013489348644,
1.15073045290619));
#82417=CARTESIAN_POINT('Ctrl Pts',(-2.96345562364545,-17.601493466588,1.15070497409997));
#82418=CARTESIAN_POINT('Ctrl Pts',(-2.98660845975514,-17.6129829294787,
1.1486795516434));
#82419=CARTESIAN_POINT('Ctrl Pts',(-3.00924236604217,-17.6244510594205,
1.14707287507716));
#82420=CARTESIAN_POINT('Ctrl Pts',(-3.03135622106119,-17.6358748807149,
1.14586888188318));
#82421=CARTESIAN_POINT('Ctrl Pts',(-3.07548657744149,-17.658672231268,1.14346619593431));
#82422=CARTESIAN_POINT('Ctrl Pts',(-3.11754201398305,-17.6812897018117,
1.14266734811753));
#82423=CARTESIAN_POINT('Ctrl Pts',(-3.15750338943099,-17.703545586087,1.14334632593646));
#82424=CARTESIAN_POINT('Ctrl Pts',(-3.20904005267743,-17.7322481520094,
1.1442219777581));
#82425=CARTESIAN_POINT('Ctrl Pts',(-3.25709852006457,-17.7603520183409,
1.14755784233417));
#82426=CARTESIAN_POINT('Ctrl Pts',(-3.30167585169498,-17.7875179004328,
1.15305956494331));
#82427=CARTESIAN_POINT('Ctrl Pts',(-3.34214685945926,-17.8121813467373,
1.15805448613505));
#82428=CARTESIAN_POINT('Ctrl Pts',(-3.37974752021567,-17.836071417311,1.16483514835252));
#82429=CARTESIAN_POINT('Ctrl Pts',(-3.41447735425161,-17.8589510516284,
1.17314411559556));
#82430=CARTESIAN_POINT('Ctrl Pts',(-3.44443398255037,-17.8786861502802,
1.18031111337011));
#82431=CARTESIAN_POINT('Ctrl Pts',(-3.47225349205163,-17.8976688837122,
1.18861468802206));
#82432=CARTESIAN_POINT('Ctrl Pts',(-3.49795473249979,-17.9157683536315,
1.19786218814635));
#82433=CARTESIAN_POINT('Ctrl Pts',(-3.5095802536272,-17.9239553425189,1.20204513831513));
#82434=CARTESIAN_POINT('Ctrl Pts',(-3.5207727482244,-17.9319619744418,1.20642085871186));
#82435=CARTESIAN_POINT('Ctrl Pts',(-3.53153633920471,-17.9397782793976,
1.21096975887257));
#82436=CARTESIAN_POINT('Origin',(-3.225,-17.6882812316,1.64311487169));
#82437=CARTESIAN_POINT('Origin',(0.,-9.17423561284,0.47366156039));
#82438=CARTESIAN_POINT('',(0.,-11.82423561284,0.47366156039));
#82439=CARTESIAN_POINT('Origin',(-4.3,3.0773238354,0.47366156039));
#82440=CARTESIAN_POINT('',(-4.3,3.3773238354,-3.65542016568));
#82441=CARTESIAN_POINT('',(-4.3,3.3773238354,-0.905771600316));
#82442=CARTESIAN_POINT('',(-4.,3.0773238354,-3.65542016568));
#82443=CARTESIAN_POINT('Origin',(-4.3,3.0773238354,-3.65542016568));
#82444=CARTESIAN_POINT('',(-4.,3.0773238354,-0.905771600316));
#82445=CARTESIAN_POINT('Origin',(-4.35,-10.0779006799,-3.15542016568));
#82446=CARTESIAN_POINT('',(-4.35,-10.4977210429,-4.06302738404));
#82447=CARTESIAN_POINT('',(-4.35,-10.0779006799,-4.15542016568));
#82448=CARTESIAN_POINT('Origin',(-4.35,-10.0779006799,-3.15542016568));
#82449=CARTESIAN_POINT('',(-4.45,-10.0779006799,-4.25542016568));
#82450=CARTESIAN_POINT('Origin',(-4.35,-10.0779006799,-4.25542016568));
#82451=CARTESIAN_POINT('',(-4.45,-10.5397030792,-4.15378810588));
#82452=CARTESIAN_POINT('Origin',(-4.45,-10.0779006799,-3.15542016568));
#82453=CARTESIAN_POINT('Origin',(-4.35,-10.5397030792,-4.15378810588));
#82454=CARTESIAN_POINT('Origin',(-4.35,-14.1190276664,-2.49814531564));
#82455=CARTESIAN_POINT('',(-4.35,-17.2811181351,-0.925317401172));
#82456=CARTESIAN_POINT('',(-4.35,-13.889419589,-2.49417239261));
#82457=CARTESIAN_POINT('',(-4.45,-17.3231001714,-1.01607812301));
#82458=CARTESIAN_POINT('',(-4.45,-13.9314016253,-2.58493311444));
#82459=CARTESIAN_POINT('Origin',(-4.35,-17.3231001714,-1.01607812301));
#82460=CARTESIAN_POINT('Origin',(-4.45,0.,0.));
#82461=CARTESIAN_POINT('',(-4.45,-19.0026826744,-1.32221314666));
#82462=CARTESIAN_POINT('Origin',(-4.45,-21.2594877202,0.729452270839));
#82463=CARTESIAN_POINT('',(-4.45,-17.582210652,-0.989652421484));
#82464=CARTESIAN_POINT('',(-4.45,-1.95899712601,2.6680522976));
#82465=CARTESIAN_POINT('Origin',(-4.45,-17.4910283166,-1.37912101035));
#82466=CARTESIAN_POINT('',(-4.45,2.8773238354,-4.25542016568));
#82467=CARTESIAN_POINT('',(-4.45,-1.95899712601,-4.25542016568));
#82468=CARTESIAN_POINT('',(-4.45,3.4773238354,-3.65542016568));
#82469=CARTESIAN_POINT('Origin',(-4.45,2.8773238354,-3.65542016568));
#82470=CARTESIAN_POINT('',(-4.45,3.4773238354,1.84387696505));
#82471=CARTESIAN_POINT('',(-4.45,3.4773238354,0.294579834316));
#82472=CARTESIAN_POINT('',(-4.45,2.8773238354,2.44387696505));
#82473=CARTESIAN_POINT('Origin',(-4.45,2.8773238354,1.84387696505));
#82474=CARTESIAN_POINT('',(-4.45,-2.12788809108,2.44387696505));
#82475=CARTESIAN_POINT('',(-4.45,-1.95899712601,2.44387696505));
#82476=CARTESIAN_POINT('',(-4.45,-2.51831889439,2.53297389574));
#82477=CARTESIAN_POINT('Origin',(-4.45,-2.12788809108,3.34387696505));
#82478=CARTESIAN_POINT('',(-4.45,-7.83711001806,5.09384703785));
#82479=CARTESIAN_POINT('',(-4.45,2.13070110951,0.294579834316));
#82480=CARTESIAN_POINT('Origin',(-4.45,-8.31430322211,4.10274328646));
#82481=CARTESIAN_POINT('Origin',(-4.35,-21.2594877202,0.729452270839));
#82482=CARTESIAN_POINT('Origin',(-4.35,-19.0026826744,-1.32221314666));
#82483=CARTESIAN_POINT('Origin',(-4.35,-19.0026826744,-1.32221314666));
#82484=CARTESIAN_POINT('Origin',(-4.35,-19.0026826744,-1.32221314666));
#82485=CARTESIAN_POINT('Origin',(-4.35,-1.95899712601,2.6680522976));
#82486=CARTESIAN_POINT('Origin',(-4.35,-17.582210652,-0.989652421484));
#82487=CARTESIAN_POINT('Origin',(-4.35,-17.4910283166,-1.37912101035));
#82488=CARTESIAN_POINT('Origin',(-4.35,-17.4910283166,-1.37912101035));
#82489=CARTESIAN_POINT('Ctrl Pts',(-2.30026150234977,-17.3820580265551,
-0.891121645497691));
#82490=CARTESIAN_POINT('Ctrl Pts',(-2.2511020282712,-17.4685660559916,-0.873172032485047));
#82491=CARTESIAN_POINT('Ctrl Pts',(-2.2017503487722,-17.5463291774412,-0.813547788890955));
#82492=CARTESIAN_POINT('Ctrl Pts',(-2.16413757728291,-17.5942001577229,
-0.71591120019767));
#82493=CARTESIAN_POINT('Ctrl Pts',(-2.14871234024909,-17.5988806949977,
-0.607385187645706));
#82494=CARTESIAN_POINT('Ctrl Pts',(-2.15387724303736,-17.5683659671124,
-0.511132105859265));
#82495=CARTESIAN_POINT('Ctrl Pts',(-2.40878057050813,-17.418797425994,-0.882916394445839));
#82496=CARTESIAN_POINT('Ctrl Pts',(-2.35504797194602,-17.5086551346987,
-0.87112727920342));
#82497=CARTESIAN_POINT('Ctrl Pts',(-2.30108940419278,-17.5922280790055,
-0.813709700010545));
#82498=CARTESIAN_POINT('Ctrl Pts',(-2.26093305392475,-17.6458395466711,
-0.713034714408869));
#82499=CARTESIAN_POINT('Ctrl Pts',(-2.24664268994449,-17.6534402243889,
-0.599427746817492));
#82500=CARTESIAN_POINT('Ctrl Pts',(-2.25552652731881,-17.6235908872705,
-0.498965911082793));
#82501=CARTESIAN_POINT('Ctrl Pts',(-2.51566402719547,-17.4589771799051,
-0.877572242965746));
#82502=CARTESIAN_POINT('Ctrl Pts',(-2.45670878457325,-17.5514899225794,
-0.872981025895007));
#82503=CARTESIAN_POINT('Ctrl Pts',(-2.39748577966448,-17.6410198701621,
-0.818594729897352));
#82504=CARTESIAN_POINT('Ctrl Pts',(-2.35461942392657,-17.7011884981179,
-0.714934954500043));
#82505=CARTESIAN_POINT('Ctrl Pts',(-2.34208969093556,-17.7124931079571,
-0.595961003183311));
#82506=CARTESIAN_POINT('Ctrl Pts',(-2.35565283813046,-17.683962733608,-0.491125495637028));
#82507=CARTESIAN_POINT('Ctrl Pts',(-2.62041115594089,-17.5028395885339,
-0.87613658390424));
#82508=CARTESIAN_POINT('Ctrl Pts',(-2.5553750193492,-17.5968327517438,-0.879749872744001));
#82509=CARTESIAN_POINT('Ctrl Pts',(-2.49001831660964,-17.69222510147,-0.82932513722258));
#82510=CARTESIAN_POINT('Ctrl Pts',(-2.44424641281096,-17.7599256351865,
-0.722853057106192));
#82511=CARTESIAN_POINT('Ctrl Pts',(-2.43432528251228,-17.7760500789645,
-0.598373539580247));
#82512=CARTESIAN_POINT('Ctrl Pts',(-2.4537889856892,-17.7498341449337,-0.489185387248891));
#82513=CARTESIAN_POINT('Ctrl Pts',(-2.7224545911624,-17.5507108773925,-0.879827372138517));
#82514=CARTESIAN_POINT('Ctrl Pts',(-2.65009743783106,-17.6443621840397,
-0.892953323240521));
#82515=CARTESIAN_POINT('Ctrl Pts',(-2.57735067987483,-17.7452621208078,
-0.84787026250574));
#82516=CARTESIAN_POINT('Ctrl Pts',(-2.5284103961115,-17.821745215291,-0.738849741797549));
#82517=CARTESIAN_POINT('Ctrl Pts',(-2.52234106163441,-17.8441995989119,
-0.608578431302329));
#82518=CARTESIAN_POINT('Ctrl Pts',(-2.54940634153372,-17.8216799279534,
-0.494979618252563));
#82519=CARTESIAN_POINT('Ctrl Pts',(-2.81901489023132,-17.6025946693237,
-0.891701921170512));
#82520=CARTESIAN_POINT('Ctrl Pts',(-2.73744075495876,-17.6921936758885,
-0.914074996544492));
#82521=CARTESIAN_POINT('Ctrl Pts',(-2.65538058640039,-17.7967415471119,
-0.875010275347337));
#82522=CARTESIAN_POINT('Ctrl Pts',(-2.60302630158974,-17.8835187867793,
-0.764336819213081));
#82523=CARTESIAN_POINT('Ctrl Pts',(-2.60282559743216,-17.9153183318905,
-0.629507557784543));
#82524=CARTESIAN_POINT('Ctrl Pts',(-2.63990390140954,-17.8994711764097,
-0.513073271338585));
#82525=CARTESIAN_POINT('Ctrl Pts',(-2.81682310404,-17.6050062358,-0.892285274267));
#82526=CARTESIAN_POINT('Ctrl Pts',(-2.77238544150798,-17.5811167968899,
-0.886692281931633));
#82527=CARTESIAN_POINT('Ctrl Pts',(-2.7243400982194,-17.5570466401642,-0.882915995356844));
#82528=CARTESIAN_POINT('Ctrl Pts',(-2.67274747304574,-17.5330452228065,
-0.880894863642099));
#82529=CARTESIAN_POINT('Ctrl Pts',(-2.62668804079532,-17.5116179034371,
-0.87909049375452));
#82530=CARTESIAN_POINT('Ctrl Pts',(-2.57780359900481,-17.4902459976349,
-0.878683248104142));
#82531=CARTESIAN_POINT('Ctrl Pts',(-2.52610297724738,-17.4691042792122,
-0.879609375083118));
#82532=CARTESIAN_POINT('Ctrl Pts',(-2.47295527054473,-17.4473708104119,
-0.880561424079336));
#82533=CARTESIAN_POINT('Ctrl Pts',(-2.41683107761332,-17.4258804100421,
-0.882923772785761));
#82534=CARTESIAN_POINT('Ctrl Pts',(-2.35768503181644,-17.4048159349658,
-0.886610023581458));
#82535=CARTESIAN_POINT('Ctrl Pts',(-2.33876680496398,-17.3980783329393,
-0.887789093591101));
#82536=CARTESIAN_POINT('Ctrl Pts',(-2.319539086922,-17.3913842780576,-0.889103366281777));
#82537=CARTESIAN_POINT('Ctrl Pts',(-2.30000000000002,-17.3847398066618,
-0.890548881027004));
#82538=CARTESIAN_POINT('Origin',(-3.225,-17.4910283166,-1.37912101035));
#82539=CARTESIAN_POINT('',(-3.325,-17.2811181351,-0.925317401172));
#82540=CARTESIAN_POINT('Origin',(0.,-10.2979776218,-4.15542016568));
#82541=CARTESIAN_POINT('',(3.225,-10.4977210429,-4.06302738404));
#82542=CARTESIAN_POINT('Origin',(3.225,-10.0779006799,-3.15542016568));
#82543=CARTESIAN_POINT('',(-3.325,-10.0779006799,-4.15542016568));
#82544=CARTESIAN_POINT('Origin',(0.,3.3773238354,-4.15542016568));
#82545=CARTESIAN_POINT('',(-4.35,2.8773238354,-4.15542016568));
#82546=CARTESIAN_POINT('',(-4.35,-1.95899712601,-4.15542016568));
#82547=CARTESIAN_POINT('',(-4.29232316258844,-8.70602835244453,-4.15542016568));
#82548=CARTESIAN_POINT('Ctrl Pts',(-4.29232316225885,-8.70602837142191,
-4.15542016568));
#82549=CARTESIAN_POINT('Ctrl Pts',(-4.29205120071452,-8.72168753702626,
-4.15542016568));
#82550=CARTESIAN_POINT('Ctrl Pts',(-4.29158720532918,-8.73740648674787,
-4.15542016568278));
#82551=CARTESIAN_POINT('Ctrl Pts',(-4.29086254081513,-8.75324772180714,
-4.15542016514087));
#82552=CARTESIAN_POINT('Ctrl Pts',(-4.29008645301039,-8.77021307488149,
-4.15542016456051));
#82553=CARTESIAN_POINT('Ctrl Pts',(-4.28901119399487,-8.7873184421748,-4.15542016334628));
#82554=CARTESIAN_POINT('Ctrl Pts',(-4.28754966268177,-8.80457940448153,
-4.15542016341833));
#82555=CARTESIAN_POINT('Ctrl Pts',(-4.28677487233489,-8.81372982558667,
-4.15542016345652));
#82556=CARTESIAN_POINT('Ctrl Pts',(-4.28589150051295,-8.8229229964194,-4.15542016392521));
#82557=CARTESIAN_POINT('Ctrl Pts',(-4.28488660862881,-8.83215545542406,
-4.15542016457497));
#82558=CARTESIAN_POINT('Ctrl Pts',(-4.28275134959082,-8.85177317932411,
-4.15542016595563));
#82559=CARTESIAN_POINT('Ctrl Pts',(-4.28003832504559,-8.87155237324264,
-4.15542016566606));
#82560=CARTESIAN_POINT('Ctrl Pts',(-4.27662963897357,-8.89139030340002,
-4.15542016567672));
#82561=CARTESIAN_POINT('Ctrl Pts',(-4.27453046995187,-8.90360708357898,
-4.15542016568329));
#82562=CARTESIAN_POINT('Ctrl Pts',(-4.27216774709283,-8.91584486940965,
-4.15542016568));
#82563=CARTESIAN_POINT('Ctrl Pts',(-4.26951780859382,-8.92807096217797,
-4.15542016568));
#82564=CARTESIAN_POINT('Ctrl Pts',(-4.26468368982784,-8.95037426638974,
-4.15542016568));
#82565=CARTESIAN_POINT('Ctrl Pts',(-4.25889294909336,-8.97263030125832,
-4.15542016568));
#82566=CARTESIAN_POINT('Ctrl Pts',(-4.25202546552033,-8.99462871319934,
-4.15542016568));
#82567=CARTESIAN_POINT('Ctrl Pts',(-4.24866331428397,-9.00539859522655,
-4.15542016568));
#82568=CARTESIAN_POINT('Ctrl Pts',(-4.24504378092221,-9.01610634900063,
-4.15542016568));
#82569=CARTESIAN_POINT('Ctrl Pts',(-4.24115737109246,-9.02672676812152,
-4.15542016568));
#82570=CARTESIAN_POINT('Ctrl Pts',(-4.23426685680616,-9.04555652434511,
-4.15542016568));
#82571=CARTESIAN_POINT('Ctrl Pts',(-4.22653159494977,-9.06411864425602,
-4.15542016568));
#82572=CARTESIAN_POINT('Ctrl Pts',(-4.21793147778923,-9.08227287068491,
-4.15542016568));
#82573=CARTESIAN_POINT('Ctrl Pts',(-4.2100789353958,-9.0988490207526,-4.15542016568));
#82574=CARTESIAN_POINT('Ctrl Pts',(-4.2015054941613,-9.11508438284678,-4.15542016568));
#82575=CARTESIAN_POINT('Ctrl Pts',(-4.1922309596074,-9.13089839049763,-4.15542016568));
#82576=CARTESIAN_POINT('Ctrl Pts',(-4.18815592541805,-9.13784673075918,
-4.15542016568));
#82577=CARTESIAN_POINT('Ctrl Pts',(-4.1839460127474,-9.14471414658231,-4.15542016568));
#82578=CARTESIAN_POINT('Ctrl Pts',(-4.17960523291625,-9.1514961102524,-4.15542016568));
#82579=CARTESIAN_POINT('Ctrl Pts',(-4.16634611145727,-9.17221194554702,
-4.15542016568));
#82580=CARTESIAN_POINT('Ctrl Pts',(-4.15184518108592,-9.19211860151861,
-4.15542016617984));
#82581=CARTESIAN_POINT('Ctrl Pts',(-4.13618163257724,-9.21102766582222,
-4.15542016179659));
#82582=CARTESIAN_POINT('Ctrl Pts',(-4.11973553103685,-9.23088142957176,
-4.15542015719435));
#82583=CARTESIAN_POINT('Ctrl Pts',(-4.10200809428551,-9.24963529413492,
-4.15542014577611));
#82584=CARTESIAN_POINT('Ctrl Pts',(-4.08313350202983,-9.26711150454399,
-4.15542013374396));
#82585=CARTESIAN_POINT('Ctrl Pts',(-4.07176321009623,-9.27763939365293,
-4.15542012649563));
#82586=CARTESIAN_POINT('Ctrl Pts',(-4.05997740445791,-9.28770440729055,
-4.15542011955517));
#82587=CARTESIAN_POINT('Ctrl Pts',(-4.04781138042469,-9.29727441845877,
-4.15542011643421));
#82588=CARTESIAN_POINT('Ctrl Pts',(-4.02659799740219,-9.31396124333162,
-4.15542011099231));
#82589=CARTESIAN_POINT('Ctrl Pts',(-4.00423092936188,-9.32913206089668,
-4.15542011535558));
#82590=CARTESIAN_POINT('Ctrl Pts',(-3.98091614962384,-9.34262747027809,
-4.15542012343284));
#82591=CARTESIAN_POINT('Ctrl Pts',(-3.95650110095926,-9.3567597537694,-4.15542013189127));
#82592=CARTESIAN_POINT('Ctrl Pts',(-3.93104736555546,-9.36905451674416,
-4.15542014341187));
#82593=CARTESIAN_POINT('Ctrl Pts',(-3.90483049009711,-9.37937035892166,
-4.15542015118524));
#82594=CARTESIAN_POINT('Ctrl Pts',(-3.89672696602562,-9.38255894161665,
-4.15542015358796));
#82595=CARTESIAN_POINT('Ctrl Pts',(-3.88855076480426,-9.38555876112294,
-4.15542015568561));
#82596=CARTESIAN_POINT('Ctrl Pts',(-3.88031058139973,-9.38836645220462,
-4.1554201574361));
#82597=CARTESIAN_POINT('Ctrl Pts',(-3.85132370712238,-9.39824319698063,
-4.15542016359385));
#82598=CARTESIAN_POINT('Ctrl Pts',(-3.82154088715569,-9.40573335220575,
-4.15542016471136));
#82599=CARTESIAN_POINT('Ctrl Pts',(-3.79135695696281,-9.41074020445555,
-4.15542016528016));
#82600=CARTESIAN_POINT('Ctrl Pts',(-3.76117302676992,-9.41574705670534,
-4.15542016584896));
#82601=CARTESIAN_POINT('Ctrl Pts',(-3.73058948857333,-9.41827087355667,
-4.15542016568));
#82602=CARTESIAN_POINT('Ctrl Pts',(-3.69999999774,-9.41827086749,-4.15542016568));
#82603=CARTESIAN_POINT('',(-4.3,-8.14391944342,-4.15542016568));
#82604=CARTESIAN_POINT('Ctrl Pts',(-4.3,-8.14391944342,-4.15542016568));
#82605=CARTESIAN_POINT('Ctrl Pts',(-4.3,-8.20648904053108,-4.15542016568));
#82606=CARTESIAN_POINT('Ctrl Pts',(-4.29947971883186,-8.26880371250586,
-4.15542016568));
#82607=CARTESIAN_POINT('Ctrl Pts',(-4.29869536600186,-8.33090046659907,
-4.15542016568));
#82608=CARTESIAN_POINT('Ctrl Pts',(-4.29790074267177,-8.39381033016885,
-4.15542016568));
#82609=CARTESIAN_POINT('Ctrl Pts',(-4.29683500095811,-8.45649622088276,
-4.15542016568));
#82610=CARTESIAN_POINT('Ctrl Pts',(-4.29571075913684,-8.51899937638185,
-4.15542016568));
#82611=CARTESIAN_POINT('Ctrl Pts',(-4.29458651731557,-8.58150253188095,
-4.15542016568));
#82612=CARTESIAN_POINT('Ctrl Pts',(-4.2934034804918,-8.64382608258768,-4.15542016568));
#82613=CARTESIAN_POINT('Ctrl Pts',(-4.29232316291,-8.70602833393,-4.15542016568));
#82614=CARTESIAN_POINT('',(-4.3,2.8773238354,-4.15542016568));
#82615=CARTESIAN_POINT('',(-4.3,-3.42065492897,-4.15542016568));
#82616=CARTESIAN_POINT('',(3.225,2.8773238354,-4.15542016568));
#82617=CARTESIAN_POINT('Origin',(-4.35,-1.95899712601,-4.25542016568));
#82618=CARTESIAN_POINT('Origin',(-4.35,2.8773238354,-4.25542016568));
#82619=CARTESIAN_POINT('Origin',(-4.35,2.8773238354,-3.65542016568));
#82620=CARTESIAN_POINT('',(-4.35,3.3773238354,-3.65542016568));
#82621=CARTESIAN_POINT('Origin',(-4.35,2.8773238354,-3.65542016568));
#82622=CARTESIAN_POINT('Origin',(-4.35,3.4773238354,-3.65542016568));
#82623=CARTESIAN_POINT('Origin',(-4.35,3.4773238354,0.294579834316));
#82624=CARTESIAN_POINT('',(-4.35,3.3773238354,1.84387696505));
#82625=CARTESIAN_POINT('',(-4.35,3.3773238354,-0.905771600316));
#82626=CARTESIAN_POINT('Origin',(-4.35,3.4773238354,1.84387696505));
#82627=CARTESIAN_POINT('Origin',(-4.35,2.8773238354,1.84387696505));
#82628=CARTESIAN_POINT('',(-4.35,2.8773238354,2.34387696505));
#82629=CARTESIAN_POINT('Origin',(-4.35,2.8773238354,1.84387696505));
#82630=CARTESIAN_POINT('Origin',(-4.35,2.8773238354,2.44387696505));
#82631=CARTESIAN_POINT('Origin',(-4.35,-1.95899712601,2.44387696505));
#82632=CARTESIAN_POINT('',(-4.35,-2.12788809108,2.34387696505));
#82633=CARTESIAN_POINT('',(-4.35,0.374717872161,2.34387696505));
#82634=CARTESIAN_POINT('Origin',(-4.35,-2.12788809108,2.44387696505));
#82635=CARTESIAN_POINT('Origin',(-4.35,-2.12788809108,3.34387696505));
#82636=CARTESIAN_POINT('',(-4.35,-2.56170009476,2.4428735547));
#82637=CARTESIAN_POINT('Origin',(-4.35,-2.12788809108,3.34387696505));
#82638=CARTESIAN_POINT('Origin',(-4.35,-2.51831889439,2.53297389574));
#82639=CARTESIAN_POINT('Origin',(-4.35,2.13070110951,0.294579834316));
#82640=CARTESIAN_POINT('',(-4.35,-7.88049121843,5.00374669681));
#82641=CARTESIAN_POINT('',(-4.35,-5.22109565659,3.72331012576));
#82642=CARTESIAN_POINT('Origin',(-4.35,-7.83711001806,5.09384703785));
#82643=CARTESIAN_POINT('Origin',(-4.35,-8.31430322211,4.10274328646));
#82644=CARTESIAN_POINT('Origin',(-4.35,-8.31430322211,4.10274328646));
#82645=CARTESIAN_POINT('Origin',(3.225,-8.31430322211,4.10274328646));
#82646=CARTESIAN_POINT('',(-4.2990272509,-7.88049121843,5.00374669681));
#82647=CARTESIAN_POINT('',(-4.32451362545,-7.88049121843,5.00374669681));
#82648=CARTESIAN_POINT('',(-4.29889875895,-8.31430322211008,5.10274332057));
#82649=CARTESIAN_POINT('Ctrl Pts',(-4.29889876134,-8.31430322211031,5.1027434229));
#82650=CARTESIAN_POINT('Ctrl Pts',(-4.2992163598671,-8.2759204184726,5.10274351089319));
#82651=CARTESIAN_POINT('Ctrl Pts',(-4.29939095950142,-8.23760601837549,
5.10053256059037));
#82652=CARTESIAN_POINT('Ctrl Pts',(-4.29949929792767,-8.199577020703,5.09614052938043));
#82653=CARTESIAN_POINT('Ctrl Pts',(-4.29956041494064,-8.17812370239259,
5.09366285052106));
#82654=CARTESIAN_POINT('Ctrl Pts',(-4.29959953479425,-8.15676118602362,
5.09049130118834));
#82655=CARTESIAN_POINT('Ctrl Pts',(-4.29962336909445,-8.13552816410012,
5.08663315284131));
#82656=CARTESIAN_POINT('Ctrl Pts',(-4.29966559839581,-8.09790777356408,
5.07979733606101));
#82657=CARTESIAN_POINT('Ctrl Pts',(-4.29966269432202,-8.06069331187253,
5.07080520434682));
#82658=CARTESIAN_POINT('Ctrl Pts',(-4.29961270179433,-8.02409853669487,
5.05970769169322));
#82659=CARTESIAN_POINT('Ctrl Pts',(-4.2995627202886,-7.98751182964539,5.04861262573191));
#82660=CARTESIAN_POINT('Ctrl Pts',(-4.2994656683763,-7.95154459699327,5.0354131084642));
#82661=CARTESIAN_POINT('Ctrl Pts',(-4.2992694321813,-7.91640705990306,5.02017373353442));
#82662=CARTESIAN_POINT('Ctrl Pts',(-4.29920200874686,-7.9043343970172,5.01493774230241));
#82663=CARTESIAN_POINT('Ctrl Pts',(-4.29912244160228,-7.89235964547437,
5.00946106597536));
#82664=CARTESIAN_POINT('Ctrl Pts',(-4.29902725090631,-7.88049121921695,
5.00374669718888));
#82665=CARTESIAN_POINT('',(-4.32444937589,-8.31430322211,5.10274328646));
#82666=CARTESIAN_POINT('Origin',(0.,-2.35608968258,2.34387696505));
#82667=CARTESIAN_POINT('',(4.225,-2.56170009476,2.4428735547));
#82668=CARTESIAN_POINT('',(-4.3,-6.28560647753,4.2358471116));
#82669=CARTESIAN_POINT('',(-4.3,-2.61831228762,2.47013099738));
#82670=CARTESIAN_POINT('Ctrl Pts',(-4.2990272509,-7.88049121843,5.00374669681));
#82671=CARTESIAN_POINT('Ctrl Pts',(-4.29860194904898,-7.84336279989873,
4.98587023435574));
#82672=CARTESIAN_POINT('Ctrl Pts',(-4.29807036319667,-7.8063193049477,4.96803466061349));
#82673=CARTESIAN_POINT('Ctrl Pts',(-4.29749123915026,-7.76934684031188,
4.95023328629991));
#82674=CARTESIAN_POINT('Ctrl Pts',(-4.29661357039136,-7.71331467008551,
4.92325511090297));
#82675=CARTESIAN_POINT('Ctrl Pts',(-4.29562842420427,-7.65745144851057,
4.89635828031341));
#82676=CARTESIAN_POINT('Ctrl Pts',(-4.29470009048654,-7.60171026056881,
4.86952020595908));
#82677=CARTESIAN_POINT('Ctrl Pts',(-4.29377028407366,-7.54588064561534,
4.84263955607304));
#82678=CARTESIAN_POINT('Ctrl Pts',(-4.29289746676361,-7.49017341724383,
4.8158178323467));
#82679=CARTESIAN_POINT('Ctrl Pts',(-4.29219442747521,-7.43454058879187,
4.78903193034465));
#82680=CARTESIAN_POINT('Ctrl Pts',(-4.29149095408814,-7.3788734092915,4.76222948911851));
#82681=CARTESIAN_POINT('Ctrl Pts',(-4.29095746147181,-7.32328068911448,
4.73546289822188));
#82682=CARTESIAN_POINT('Ctrl Pts',(-4.29065473399492,-7.26771400724003,
4.7087088442481));
#82683=CARTESIAN_POINT('Ctrl Pts',(-4.29035187162506,-7.21212256529347,
4.68194286888037));
#82684=CARTESIAN_POINT('Ctrl Pts',(-4.29027997715909,-7.15655715410882,
4.65518942682211));
#82685=CARTESIAN_POINT('Ctrl Pts',(-4.29044774917812,-7.10096941674446,
4.6284252355263));
#82686=CARTESIAN_POINT('Ctrl Pts',(-4.29052775589753,-7.07446086941765,
4.61566199195374));
#82687=CARTESIAN_POINT('Ctrl Pts',(-4.29066150240974,-7.04794724961644,
4.6028963061693));
#82688=CARTESIAN_POINT('Ctrl Pts',(-4.29084575810665,-7.02142335390664,
4.59012567283795));
#82689=CARTESIAN_POINT('Ctrl Pts',(-4.29123152417027,-6.96589172578971,
4.56338849709526));
#82690=CARTESIAN_POINT('Ctrl Pts',(-4.29184075891047,-6.91031984610482,
4.53663194126546));
#82691=CARTESIAN_POINT('Ctrl Pts',(-4.29260245682323,-6.85466578564437,
4.50983581716746));
#82692=CARTESIAN_POINT('Ctrl Pts',(-4.29336407793749,-6.79901733652759,
4.48304239479976));
#82693=CARTESIAN_POINT('Ctrl Pts',(-4.29427813122767,-6.74328668363906,
4.45620939309286));
#82694=CARTESIAN_POINT('Ctrl Pts',(-4.29522152510374,-6.68743327543012,
4.42931728747705));
#82695=CARTESIAN_POINT('Ctrl Pts',(-4.29540155763234,-6.67677449274567,
4.42418533369164));
#82696=CARTESIAN_POINT('Ctrl Pts',(-4.29558250634003,-6.66611124458006,
4.41905122987873));
#82697=CARTESIAN_POINT('Ctrl Pts',(-4.29576330024143,-6.65544325666937,
4.41391484398757));
#82698=CARTESIAN_POINT('Ctrl Pts',(-4.29671133096125,-6.59950342584761,
4.38698112788367));
#82699=CARTESIAN_POINT('Ctrl Pts',(-4.29766075533132,-6.54342366948845,
4.35998004088301));
#82700=CARTESIAN_POINT('Ctrl Pts',(-4.29842842934662,-6.48716607127935,
4.33289332720474));
#82701=CARTESIAN_POINT('Ctrl Pts',(-4.29919717698267,-6.43082979472131,
4.30576873174731));
#82702=CARTESIAN_POINT('Ctrl Pts',(-4.29978365749905,-6.37431514200558,
4.27855825235265));
#82703=CARTESIAN_POINT('Ctrl Pts',(-4.29995176543971,-6.31758659819914,
4.25124478941713));
#82704=CARTESIAN_POINT('Ctrl Pts',(-4.29998333258852,-6.30693416633443,
4.24611589339078));
#82705=CARTESIAN_POINT('Ctrl Pts',(-4.3,-6.29627420060992,4.24098336998769));
#82706=CARTESIAN_POINT('Ctrl Pts',(-4.3,-6.28560647753,4.2358471116));
#82707=CARTESIAN_POINT('Origin',(4.225,-2.12788809108,3.34387696505));
#82708=CARTESIAN_POINT('',(-4.325,-2.12788809108,2.34387696505));
#82709=CARTESIAN_POINT('Origin',(0.,3.3773238354,2.34387696505));
#82710=CARTESIAN_POINT('',(4.225,2.8773238354,2.34387696505));
#82711=CARTESIAN_POINT('Origin',(4.225,2.8773238354,1.84387696505));
#82712=CARTESIAN_POINT('',(-4.325,3.3773238354,1.84387696505));
#82713=CARTESIAN_POINT('Origin',(0.,3.3773238354,-4.15542016568));
#82714=CARTESIAN_POINT('',(3.225,3.3773238354,-3.65542016568));
#82715=CARTESIAN_POINT('Origin',(3.225,2.8773238354,-3.65542016568));
#82716=CARTESIAN_POINT('Origin',(-4.3,2.8773238354,-3.65542016568));
#82717=CARTESIAN_POINT('Ctrl Pts',(-4.,3.0773238354,-3.65542016568));
#82718=CARTESIAN_POINT('Ctrl Pts',(-4.,3.0773238354,-3.85542016568));
#82719=CARTESIAN_POINT('Ctrl Pts',(-4.,2.8773238354,-3.85542016568));
#82720=CARTESIAN_POINT('Ctrl Pts',(-4.,3.3773238354,-3.65542016568));
#82721=CARTESIAN_POINT('Ctrl Pts',(-4.,3.3773238354,-4.15542016568));
#82722=CARTESIAN_POINT('Ctrl Pts',(-4.,2.8773238354,-4.15542016568));
#82723=CARTESIAN_POINT('Ctrl Pts',(-4.3,3.3773238354,-3.65542016568));
#82724=CARTESIAN_POINT('Ctrl Pts',(-4.3,3.3773238354,-4.15542016568));
#82725=CARTESIAN_POINT('Ctrl Pts',(-4.3,2.8773238354,-4.15542016568));
#82726=CARTESIAN_POINT('',(-4.,2.8773238354,-3.85542016568));
#82727=CARTESIAN_POINT('Origin',(-4.3,2.8773238354,-3.85542016568));
#82728=CARTESIAN_POINT('Origin',(-4.,2.8773238354,-3.65542016568));
#82729=CARTESIAN_POINT('Origin',(-4.3,-3.42065492897,-3.85542016568));
#82730=CARTESIAN_POINT('',(-4.,-8.14391944342,-3.85542016568));
#82731=CARTESIAN_POINT('Origin',(-4.29787870966756,-8.14391943179286,-3.85754145569448));
#82732=CARTESIAN_POINT('',(-4.,-2.63329780401,-3.85542016568));
#82733=CARTESIAN_POINT('Ctrl Pts',(-4.29232316291,-8.70602833393,-4.15542016568));
#82734=CARTESIAN_POINT('Ctrl Pts',(-4.20764023978,-8.70455758206,-4.15542016896));
#82735=CARTESIAN_POINT('Ctrl Pts',(-4.12295731665,-8.70308683019,-4.12553116451));
#82736=CARTESIAN_POINT('Ctrl Pts',(-4.05251768323,-8.70186345223,-4.06549009434));
#82737=CARTESIAN_POINT('Ctrl Pts',(-4.00958634297,-8.70111783143,-3.98660373227));
#82738=CARTESIAN_POINT('Ctrl Pts',(-3.99616158804,-8.70088467363,-3.90297907486));
#82739=CARTESIAN_POINT('Ctrl Pts',(-4.2942593567,-8.59454665965,-4.15542016568));
#82740=CARTESIAN_POINT('Ctrl Pts',(-4.20834579354,-8.59289747109,-4.15542016627));
#82741=CARTESIAN_POINT('Ctrl Pts',(-4.12243223039,-8.59124828254,-4.12466052278));
#82742=CARTESIAN_POINT('Ctrl Pts',(-4.05139392587,-8.58988386074,-4.06285702325));
#82743=CARTESIAN_POINT('Ctrl Pts',(-4.00903053768,-8.58906847866,-3.98200796497));
#82744=CARTESIAN_POINT('Ctrl Pts',(-3.99712968313,-8.58883688841,-3.89688931333));
#82745=CARTESIAN_POINT('Ctrl Pts',(-4.29645983294,-8.48273103918,-4.15542016568));
#82746=CARTESIAN_POINT('Ctrl Pts',(-4.20896023779,-8.48105918371,-4.15542015758));
#82747=CARTESIAN_POINT('Ctrl Pts',(-4.12146064264,-8.47938732823,-4.12352488429));
#82748=CARTESIAN_POINT('Ctrl Pts',(-4.04967388507,-8.47801593608,-4.05942126033));
#82749=CARTESIAN_POINT('Ctrl Pts',(-4.00810176319,-8.47722229641,-3.97603783242));
#82750=CARTESIAN_POINT('Ctrl Pts',(-3.99822990786,-8.47703468918,-3.88903180855));
#82751=CARTESIAN_POINT('Ctrl Pts',(-4.29855844641,-8.37042692805,-4.15542016568));
#82752=CARTESIAN_POINT('Ctrl Pts',(-4.20912872342,-8.36895891499,-4.15542016568));
#82753=CARTESIAN_POINT('Ctrl Pts',(-4.11969900043,-8.36749090194,-4.12211547602));
#82754=CARTESIAN_POINT('Ctrl Pts',(-4.04704750378,-8.36630239191,-4.05515458588));
#82755=CARTESIAN_POINT('Ctrl Pts',(-4.00655550671,-8.36564940222,-3.96867720994));
#82756=CARTESIAN_POINT('Ctrl Pts',(-3.99927927276,-8.3655474023,-3.87944960348));
#82757=CARTESIAN_POINT('Ctrl Pts',(-4.3,-8.25752787941,-4.15542016568));
#82758=CARTESIAN_POINT('Ctrl Pts',(-4.20831114128,-8.25657123296,-4.15542016568));
#82759=CARTESIAN_POINT('Ctrl Pts',(-4.11662228256,-8.2556145865,-4.12041892129));
#82760=CARTESIAN_POINT('Ctrl Pts',(-4.04304033238,-8.25485845437,-4.05001401514));
#82761=CARTESIAN_POINT('Ctrl Pts',(-4.00401954353,-8.25448277917,-3.95990362884));
#82762=CARTESIAN_POINT('Ctrl Pts',(-4.,-8.25448277917,-3.86821477012));
#82763=CARTESIAN_POINT('Ctrl Pts',(-4.3,-8.14391944342,-4.15542016568));
#82764=CARTESIAN_POINT('Ctrl Pts',(-4.20575222039,-8.14391944342,-4.15542016568));
#82765=CARTESIAN_POINT('Ctrl Pts',(-4.11150444078,-8.14391944342,-4.11840914918));
#82766=CARTESIAN_POINT('Ctrl Pts',(-4.0370110165,-8.14391944342,-4.0439157249));
#82767=CARTESIAN_POINT('Ctrl Pts',(-4.,-8.14391944342,-3.94966794529));
#82768=CARTESIAN_POINT('Ctrl Pts',(-4.,-8.14391944342,-3.85542016568));
#82769=CARTESIAN_POINT('',(-3.99616160426685,-8.70088467346877,-3.90297923414786));
#82770=CARTESIAN_POINT('Origin',(-4.290691026855,-8.70599993058013,-3.85733562503364));
#82771=CARTESIAN_POINT('Ctrl Pts',(-4.,-8.14391944342,-3.85542016568));
#82772=CARTESIAN_POINT('Ctrl Pts',(-4.,-8.21619147164719,-3.86378362547669));
#82773=CARTESIAN_POINT('Ctrl Pts',(-3.99963494167047,-8.28873626415572,
-3.87134899206184));
#82774=CARTESIAN_POINT('Ctrl Pts',(-3.99911352626311,-8.36160108492365,
-3.87807113866823));
#82775=CARTESIAN_POINT('Ctrl Pts',(-3.99857374958904,-8.43703178769067,
-3.88503000080881));
#82776=CARTESIAN_POINT('Ctrl Pts',(-3.99786619096606,-8.51280461194599,
-3.89108515684303));
#82777=CARTESIAN_POINT('Ctrl Pts',(-3.99716685654696,-8.58897211220517,
-3.89618805925311));
#82778=CARTESIAN_POINT('Ctrl Pts',(-3.99682523423041,-8.62617965865753,
-3.89868080849417));
#82779=CARTESIAN_POINT('Ctrl Pts',(-3.9964847718308,-8.66348146771974,-3.9009463498971));
#82780=CARTESIAN_POINT('Ctrl Pts',(-3.99616161341551,-8.70088467121112,
-3.90297923261801));
#82781=CARTESIAN_POINT('Ctrl Pts',(-3.69999999774,-9.41827086749,-4.15542016568));
#82782=CARTESIAN_POINT('Ctrl Pts',(-3.69999999833,-9.34659890209,-4.15542016568));
#82783=CARTESIAN_POINT('Ctrl Pts',(-3.69999999892,-9.2749269367,-4.13401653812));
#82784=CARTESIAN_POINT('Ctrl Pts',(-3.69999999944,-9.21183540432,-4.09110601764));
#82785=CARTESIAN_POINT('Ctrl Pts',(-3.69999999982,-9.16559336719,-4.03231265157));
#82786=CARTESIAN_POINT('Ctrl Pts',(-3.70000000003,-9.13925764692,-3.96565456539));
#82787=CARTESIAN_POINT('Ctrl Pts',(-3.81412909821,-9.41827089013,-4.15542016568));
#82788=CARTESIAN_POINT('Ctrl Pts',(-3.79947056194,-9.34659892134,-4.15542016565));
#82789=CARTESIAN_POINT('Ctrl Pts',(-3.78481202566,-9.27492695255,-4.13401653803));
#82790=CARTESIAN_POINT('Ctrl Pts',(-3.77190837788,-9.21183541723,-4.09110601746));
#82791=CARTESIAN_POINT('Ctrl Pts',(-3.76245084042,-9.16559337792,-4.03231265129));
#82792=CARTESIAN_POINT('Ctrl Pts',(-3.75706459059,-9.13925765647,-3.96565456502));
#82793=CARTESIAN_POINT('Ctrl Pts',(-3.92823594404,-9.38909765086,-4.15542016568));
#82794=CARTESIAN_POINT('Ctrl Pts',(-3.89892199959,-9.32091627439,-4.15542016461));
#82795=CARTESIAN_POINT('Ctrl Pts',(-3.86960805513,-9.25273489792,-4.13385699888));
#82796=CARTESIAN_POINT('Ctrl Pts',(-3.84380320278,-9.19278171906,-4.0906252646));
#82797=CARTESIAN_POINT('Ctrl Pts',(-3.82488943837,-9.14898176867,-4.03143501908));
#82798=CARTESIAN_POINT('Ctrl Pts',(-3.81411802643,-9.12422889542,-3.96440816956));
#82799=CARTESIAN_POINT('Ctrl Pts',(-4.03302804821,-9.33107957038,-4.15542016568));
#82800=CARTESIAN_POINT('Ctrl Pts',(-3.99017706972,-9.2696193654,-4.1554201695));
#82801=CARTESIAN_POINT('Ctrl Pts',(-3.94732609124,-9.20815916043,-4.13359925186));
#82802=CARTESIAN_POINT('Ctrl Pts',(-3.90964076698,-9.15426319663,-4.0898484638));
#82803=CARTESIAN_POINT('Ctrl Pts',(-3.8820963349,-9.11520770945,-4.03001850758));
#82804=CARTESIAN_POINT('Ctrl Pts',(-3.86651403782,-9.0935734628,-3.96239691009));
#82805=CARTESIAN_POINT('Ctrl Pts',(-4.18747374061,-9.18016437508,-4.15542016568));
#82806=CARTESIAN_POINT('Ctrl Pts',(-4.12388018645,-9.13700016797,-4.15542016252));
#82807=CARTESIAN_POINT('Ctrl Pts',(-4.0602866323,-9.09383596087,-4.13249096908));
#82808=CARTESIAN_POINT('Ctrl Pts',(-4.00475631151,-9.05633061601,-4.08650843459));
#82809=CARTESIAN_POINT('Ctrl Pts',(-3.96503122609,-9.029900996,-4.02393293739));
#82810=CARTESIAN_POINT('Ctrl Pts',(-3.94373685893,-9.0162718551,-3.9537856064));
#82811=CARTESIAN_POINT('Ctrl Pts',(-4.26723541157,-8.98063713586,-4.15542016568));
#82812=CARTESIAN_POINT('Ctrl Pts',(-4.19077919927,-8.95915602901,-4.1554201683));
#82813=CARTESIAN_POINT('Ctrl Pts',(-4.11432298698,-8.93767492216,-4.13000304884));
#82814=CARTESIAN_POINT('Ctrl Pts',(-4.04869892936,-8.91937700045,-4.07900263159));
#82815=CARTESIAN_POINT('Ctrl Pts',(-4.00420277032,-8.90727654877,-4.01043652908));
#82816=CARTESIAN_POINT('Ctrl Pts',(-3.98361771521,-8.90210958415,-3.93506389031));
#82817=CARTESIAN_POINT('Ctrl Pts',(-4.28448738522,-8.88291546038,-4.15542016568));
#82818=CARTESIAN_POINT('Ctrl Pts',(-4.2038128468,-8.87211558957,-4.15542016079));
#82819=CARTESIAN_POINT('Ctrl Pts',(-4.12313830838,-8.86131571876,-4.12815293378));
#82820=CARTESIAN_POINT('Ctrl Pts',(-4.05474416619,-8.85231492765,-4.07341965826));
#82821=CARTESIAN_POINT('Ctrl Pts',(-4.01023278232,-8.84679291313,-4.00043036345));
#82822=CARTESIAN_POINT('Ctrl Pts',(-3.99224364397,-8.84501961539,-3.92126984866));
#82823=CARTESIAN_POINT('Ctrl Pts',(-4.2908008405,-8.79368075155,-4.15542016568));
#82824=CARTESIAN_POINT('Ctrl Pts',(-4.20683195096,-8.78806573108,-4.15542016568));
#82825=CARTESIAN_POINT('Ctrl Pts',(-4.12286306143,-8.78245071061,-4.12598423857));
#82826=CARTESIAN_POINT('Ctrl Pts',(-4.05279621082,-8.77777630692,-4.06686040464));
#82827=CARTESIAN_POINT('Ctrl Pts',(-4.00960658253,-8.77491887358,-3.98899545804));
#82828=CARTESIAN_POINT('Ctrl Pts',(-3.99540042025,-8.7740131878,-3.9061483086));
#82829=CARTESIAN_POINT('Ctrl Pts',(-4.29232317424,-8.70602837163,-4.15542016568));
#82830=CARTESIAN_POINT('Ctrl Pts',(-4.20764026079,-8.70455761115,-4.15542016568));
#82831=CARTESIAN_POINT('Ctrl Pts',(-4.12295734733,-8.70308685067,-4.12553116999));
#82832=CARTESIAN_POINT('Ctrl Pts',(-4.05251771609,-8.70186346543,-4.06549012145));
#82833=CARTESIAN_POINT('Ctrl Pts',(-4.00958636427,-8.70111783998,-3.98660378483));
#82834=CARTESIAN_POINT('Ctrl Pts',(-3.99616158712,-8.70088468041,-3.90297914754));
#82835=CARTESIAN_POINT('Ctrl Pts',(-3.99616160115866,-8.70088468065382,
-3.90297923498851));
#82836=CARTESIAN_POINT('Ctrl Pts',(-3.99604551141223,-8.71203767637363,
-3.9034625548241));
#82837=CARTESIAN_POINT('Ctrl Pts',(-3.99586488182614,-8.72292685065226,
-3.90426647885834));
#82838=CARTESIAN_POINT('Ctrl Pts',(-3.99560115130509,-8.73359011569891,
-3.90528436153708));
#82839=CARTESIAN_POINT('Ctrl Pts',(-3.99529801267143,-8.74584674638279,
-3.90645434202788));
#82840=CARTESIAN_POINT('Ctrl Pts',(-3.99488561757464,-8.75780627735821,
-3.90790775425564));
#82841=CARTESIAN_POINT('Ctrl Pts',(-3.99432792915694,-8.76955639086698,
-3.90954414641858));
#82842=CARTESIAN_POINT('Ctrl Pts',(-3.99368017119247,-8.78320420811978,
-3.91144482432923));
#82843=CARTESIAN_POINT('Ctrl Pts',(-3.99283783198393,-8.79657147264791,
-3.91359388993806));
#82844=CARTESIAN_POINT('Ctrl Pts',(-3.99171828615615,-8.80980380168097,
-3.91589197001634));
#82845=CARTESIAN_POINT('Ctrl Pts',(-3.99064600082351,-8.82247754132309,
-3.9180930389677));
#82846=CARTESIAN_POINT('Ctrl Pts',(-3.98932011806426,-8.83502840719307,
-3.92043291784419));
#82847=CARTESIAN_POINT('Ctrl Pts',(-3.98763067900264,-8.84756915200607,
-3.92284258058646));
#82848=CARTESIAN_POINT('Ctrl Pts',(-3.98684406614188,-8.85340819727119,
-3.92396453387038));
#82849=CARTESIAN_POINT('Ctrl Pts',(-3.98597803251126,-8.85924475074751,
-3.92510169021808));
#82850=CARTESIAN_POINT('Ctrl Pts',(-3.98501789856444,-8.86508845323168,
-3.92624698376165));
#82851=CARTESIAN_POINT('Ctrl Pts',(-3.98252059670421,-8.880287883616,-3.92922588447268));
#82852=CARTESIAN_POINT('Ctrl Pts',(-3.97939450198513,-8.89550115214628,
-3.93225214634863));
#82853=CARTESIAN_POINT('Ctrl Pts',(-3.97537936433567,-8.91066978033972,
-3.93515747744907));
#82854=CARTESIAN_POINT('Ctrl Pts',(-3.97262832208053,-8.92106283302081,
-3.93714811620677));
#82855=CARTESIAN_POINT('Ctrl Pts',(-3.96945852442506,-8.93143598728981,
-3.93908154714824));
#82856=CARTESIAN_POINT('Ctrl Pts',(-3.96577774861011,-8.941769529366,-3.94091664769336));
#82857=CARTESIAN_POINT('Ctrl Pts',(-3.96216893175439,-8.95190105127839,
-3.94271587212651));
#82858=CARTESIAN_POINT('Ctrl Pts',(-3.95807061154141,-8.96198653511246,
-3.94441767599072));
#82859=CARTESIAN_POINT('Ctrl Pts',(-3.95341373784437,-8.97197051163173,
-3.94600679205796));
#82860=CARTESIAN_POINT('Ctrl Pts',(-3.94932091006251,-8.9807452173957,-3.94740343255365));
#82861=CARTESIAN_POINT('Ctrl Pts',(-3.94479769632574,-8.98944092795093,
-3.94871261919628));
#82862=CARTESIAN_POINT('Ctrl Pts',(-3.93980261645734,-8.99801101188341,
-3.94995603040284));
#82863=CARTESIAN_POINT('Ctrl Pts',(-3.93763249450409,-9.00173430115467,
-3.95049623276745));
#82864=CARTESIAN_POINT('Ctrl Pts',(-3.93537324066519,-9.00543373618864,
-3.95102461961947));
#82865=CARTESIAN_POINT('Ctrl Pts',(-3.93302131928633,-9.00910465172099,
-3.95154035015494));
#82866=CARTESIAN_POINT('Ctrl Pts',(-3.93266333651296,-9.00966339681123,
-3.9516188488025));
#82867=CARTESIAN_POINT('Ctrl Pts',(-3.93230320820075,-9.01022147916087,
-3.95169705425756));
#82868=CARTESIAN_POINT('Ctrl Pts',(-3.93194092287047,-9.01077888093755,
-3.95177496369907));
#82869=CARTESIAN_POINT('Ctrl Pts',(-3.93176419291978,-9.01105079255052,
-3.95181296946581));
#82870=CARTESIAN_POINT('Ctrl Pts',(-3.93158234635872,-9.01132962742367,
-3.95185189524054));
#82871=CARTESIAN_POINT('Ctrl Pts',(-3.93139478338652,-9.01161613949368,
-3.95189183812612));
#82872=CARTESIAN_POINT('Ctrl Pts',(-3.93028310063817,-9.01331429196849,
-3.95212857897266));
#82873=CARTESIAN_POINT('Ctrl Pts',(-3.92899148176813,-9.0152425934793,-3.95239515355946));
#82874=CARTESIAN_POINT('Ctrl Pts',(-3.92785226325583,-9.01690526443413,
-3.95262308942227));
#82875=CARTESIAN_POINT('Ctrl Pts',(-3.92698904941135,-9.01816511104963,
-3.95279580202334));
#82876=CARTESIAN_POINT('Ctrl Pts',(-3.92621450008615,-9.01927362386826,
-3.95294664455499));
#82877=CARTESIAN_POINT('Ctrl Pts',(-3.92568436011083,-9.0200266935362,-3.95304883021392));
#82878=CARTESIAN_POINT('Ctrl Pts',(-3.9185903818677,-9.03010376768366,-3.95441621029272));
#82879=CARTESIAN_POINT('Ctrl Pts',(-3.91069606779733,-9.04001012485587,
-3.95571759994867));
#82880=CARTESIAN_POINT('Ctrl Pts',(-3.90191649924126,-9.04958397296082,
-3.95692033378577));
#82881=CARTESIAN_POINT('Ctrl Pts',(-3.89352540383185,-9.05873420310834,
-3.95806984976879));
#82882=CARTESIAN_POINT('Ctrl Pts',(-3.88432499148419,-9.06758068841357,
-3.9591292538823));
#82883=CARTESIAN_POINT('Ctrl Pts',(-3.87427212029623,-9.07594769332381,
-3.9600791735614));
#82884=CARTESIAN_POINT('Ctrl Pts',(-3.86461090920672,-9.08398871952552,
-3.9609920843474));
#82885=CARTESIAN_POINT('Ctrl Pts',(-3.85416187252658,-9.09158662465468,
-3.96180401029878));
#82886=CARTESIAN_POINT('Ctrl Pts',(-3.84292435692288,-9.09855486626783,
-3.96250537695381));
#82887=CARTESIAN_POINT('Ctrl Pts',(-3.84110078825937,-9.0996856381834,-3.96261919127886));
#82888=CARTESIAN_POINT('Ctrl Pts',(-3.83925654865879,-9.10079976768752,
-3.96273010799853));
#82889=CARTESIAN_POINT('Ctrl Pts',(-3.83739174650389,-9.10189638836945,
-3.96283810094468));
#82890=CARTESIAN_POINT('Ctrl Pts',(-3.82591638674565,-9.10864461997696,
-3.96350265289469));
#82891=CARTESIAN_POINT('Ctrl Pts',(-3.81364052793048,-9.11472436781836,
-3.96401517490357));
#82892=CARTESIAN_POINT('Ctrl Pts',(-3.80060602177208,-9.119932670966,-3.96441142708227));
#82893=CARTESIAN_POINT('Ctrl Pts',(-3.78769322884257,-9.12509234017344,
-3.96480397914901));
#82894=CARTESIAN_POINT('Ctrl Pts',(-3.77403546873179,-9.12939595950774,
-3.96508294623434));
#82895=CARTESIAN_POINT('Ctrl Pts',(-3.75971878916075,-9.13262369144836,
-3.96527859680989));
#82896=CARTESIAN_POINT('Ctrl Pts',(-3.7460532179828,-9.13570462934035,-3.96546534939123));
#82897=CARTESIAN_POINT('Ctrl Pts',(-3.73178737468922,-9.13780386141483,
-3.96557697803066));
#82898=CARTESIAN_POINT('Ctrl Pts',(-3.71703967484152,-9.13872606991317,
-3.9656262756991));
#82899=CARTESIAN_POINT('Ctrl Pts',(-3.71142639112646,-9.13907708179971,
-3.96564503942513));
#82900=CARTESIAN_POINT('Ctrl Pts',(-3.7057437580401,-9.13925764788124,-3.96565456535276));
#82901=CARTESIAN_POINT('Ctrl Pts',(-3.70000000003,-9.13925764692,-3.96565456539));
#82902=CARTESIAN_POINT('Ctrl Pts',(-3.7,-9.13925764782849,-3.96565456816803));
#82903=CARTESIAN_POINT('Ctrl Pts',(-3.7,-9.02827749416282,-3.68475377230609));
#82904=CARTESIAN_POINT('Ctrl Pts',(-3.7,-8.72799905369119,-3.65227747615864));
#82905=CARTESIAN_POINT('Ctrl Pts',(-3.95543192421952,-9.13925764782849,
-3.96565456816803));
#82906=CARTESIAN_POINT('Ctrl Pts',(-3.95543192421952,-9.02827749416282,
-3.68475377230609));
#82907=CARTESIAN_POINT('Ctrl Pts',(-3.95543192421952,-8.72799905369119,
-3.65227747615864));
#82908=CARTESIAN_POINT('Ctrl Pts',(-3.99616160122642,-8.90473423916573,
-4.05831163541388));
#82909=CARTESIAN_POINT('Ctrl Pts',(-3.99616160122642,-8.84972443093161,
-3.919076840698));
#82910=CARTESIAN_POINT('Ctrl Pts',(-3.99616160122642,-8.70088467101431,
-3.90297923437636));
#82911=CARTESIAN_POINT('',(-3.7,-8.7279990537,-3.65227747616));
#82912=CARTESIAN_POINT('Origin',(-3.7,-8.67423561284,-4.1493785649));
#82913=CARTESIAN_POINT('Origin',(-3.7,-8.69574098918,-3.9505381294));
#82914=CARTESIAN_POINT('Origin',(3.,-8.67423561284,-4.1493785649));
#82915=CARTESIAN_POINT('',(0.,-8.7279990537,-3.65227747616));
#82916=CARTESIAN_POINT('Origin',(0.,-9.17423561284,0.47366156039));
#82917=CARTESIAN_POINT('',(-3.7,-8.7279990537,4.59960059693));
#82918=CARTESIAN_POINT('',(3.,-8.7279990537,4.59960059693));
#82919=CARTESIAN_POINT('Origin',(-3.7,-9.17423561284,0.47366156039));
#82920=CARTESIAN_POINT('Origin',(3.,-8.67423561284,5.09670168568));
#82921=CARTESIAN_POINT('',(-3.7,-9.13925764671,4.9129776861));
#82922=CARTESIAN_POINT('',(3.225,-9.13925764673,4.91297768617));
#82923=CARTESIAN_POINT('Origin',(-3.7,-8.67423561284,5.09670168568));
#82924=CARTESIAN_POINT('Origin',(3.225,-9.41827086707,4.80274328646));
#82925=CARTESIAN_POINT('',(-3.69999999774,-9.41827086749,5.10274328646));
#82926=CARTESIAN_POINT('',(-3.,-9.41827086707,5.10274328646));
#82927=CARTESIAN_POINT('Origin',(-3.69999999763766,-9.41833116541154,4.80265462953655));
#82928=CARTESIAN_POINT('Origin',(0.,-8.08610163061,5.10274328646));
#82929=CARTESIAN_POINT('',(-4.29232279670749,-8.70602826446416,5.10274328645992));
#82930=CARTESIAN_POINT('Ctrl Pts',(-4.29232279844,-8.70602816471,5.10274328646));
#82931=CARTESIAN_POINT('Ctrl Pts',(-4.29367604164,-8.62810126572,5.10274328646));
#82932=CARTESIAN_POINT('Ctrl Pts',(-4.29515862692,-8.55000353482,5.10274328646));
#82933=CARTESIAN_POINT('Ctrl Pts',(-4.2966466112,-8.47169636018,5.10274328646));
#82934=CARTESIAN_POINT('Ctrl Pts',(-4.29796673138,-8.39314927373,5.10274328646));
#82935=CARTESIAN_POINT('Ctrl Pts',(-4.29889875178,-8.31430322211,5.10274328646));
#82936=CARTESIAN_POINT('Ctrl Pts',(-3.69999999774,-9.41827086749,5.10274328646));
#82937=CARTESIAN_POINT('Ctrl Pts',(-3.73058948857333,-9.41827087355667,
5.10274328646));
#82938=CARTESIAN_POINT('Ctrl Pts',(-3.76117302676985,-9.41574705670535,
5.10274328662896));
#82939=CARTESIAN_POINT('Ctrl Pts',(-3.79135695696247,-9.41074020445563,
5.10274328606016));
#82940=CARTESIAN_POINT('Ctrl Pts',(-3.8215408871551,-9.40573335220591,5.10274328549136));
#82941=CARTESIAN_POINT('Ctrl Pts',(-3.85132370712135,-9.39824319698092,
5.10274328437385));
#82942=CARTESIAN_POINT('Ctrl Pts',(-3.880310581398,-9.38836645220521,5.1027432782161));
#82943=CARTESIAN_POINT('Ctrl Pts',(-3.90707199290093,-9.37924799297674,
5.1027432725311));
#82944=CARTESIAN_POINT('Ctrl Pts',(-3.93315644396342,-9.36809987699747,
5.10274326252178));
#82945=CARTESIAN_POINT('Ctrl Pts',(-3.95827561771127,-9.35505208010836,
5.10274325269434));
#82946=CARTESIAN_POINT('Ctrl Pts',(-3.98223829836866,-9.34260500707664,
5.10274324331936));
#82947=CARTESIAN_POINT('Ctrl Pts',(-4.00532196797495,-9.32842939224294,
5.10274323477061));
#82948=CARTESIAN_POINT('Ctrl Pts',(-4.02730698337273,-9.31267452069528,
5.10274323470365));
#82949=CARTESIAN_POINT('Ctrl Pts',(-4.0342532243783,-9.30769671500346,5.1027432346825));
#82950=CARTESIAN_POINT('Ctrl Pts',(-4.04109006204254,-9.30256152719756,
5.10274323548998));
#82951=CARTESIAN_POINT('Ctrl Pts',(-4.04781138042469,-9.29727441845877,
5.10274323721421));
#82952=CARTESIAN_POINT('Ctrl Pts',(-4.06816544935236,-9.28126354535637,
5.10274324243566));
#82953=CARTESIAN_POINT('Ctrl Pts',(-4.08745353683921,-9.26386507535306,
5.10274325797042));
#82954=CARTESIAN_POINT('Ctrl Pts',(-4.1055168903408,-9.24523724841711,5.10274326872092));
#82955=CARTESIAN_POINT('Ctrl Pts',(-4.12268030159011,-9.22753748661184,
5.10274327893581));
#82956=CARTESIAN_POINT('Ctrl Pts',(-4.13873762061326,-9.20872790766285,
5.10274328434029));
#82957=CARTESIAN_POINT('Ctrl Pts',(-4.1535845819758,-9.18897826222551,5.10274328574875));
#82958=CARTESIAN_POINT('Ctrl Pts',(-4.16272152564545,-9.17682416594611,
5.10274328661553));
#82959=CARTESIAN_POINT('Ctrl Pts',(-4.17140072073273,-9.16431470638581,
5.10274328646));
#82960=CARTESIAN_POINT('Ctrl Pts',(-4.17960523291625,-9.15149611025241,
5.10274328646));
#82961=CARTESIAN_POINT('Ctrl Pts',(-4.18942766527051,-9.13614970201014,
5.10274328646));
#82962=CARTESIAN_POINT('Ctrl Pts',(-4.19857745049624,-9.12036311945856,
5.10274328646));
#82963=CARTESIAN_POINT('Ctrl Pts',(-4.20701878194007,-9.10419983822068,
5.10274328646));
#82964=CARTESIAN_POINT('Ctrl Pts',(-4.21621021747847,-9.08660027367622,
5.10274328646));
#82965=CARTESIAN_POINT('Ctrl Pts',(-4.22456152722091,-9.06855481897592,
5.10274328646));
#82966=CARTESIAN_POINT('Ctrl Pts',(-4.2320738661817,-9.05018712924208,5.10274328646));
#82967=CARTESIAN_POINT('Ctrl Pts',(-4.23525034335279,-9.04242063368992,
5.10274328646));
#82968=CARTESIAN_POINT('Ctrl Pts',(-4.23827738137825,-9.03459693600601,
5.10274328646));
#82969=CARTESIAN_POINT('Ctrl Pts',(-4.24115737109239,-9.02672676812149,
5.10274328646));
#82970=CARTESIAN_POINT('Ctrl Pts',(-4.24909569801083,-9.00503364704426,
5.10274328646));
#82971=CARTESIAN_POINT('Ctrl Pts',(-4.25591706153315,-8.98297603570749,
5.10274328646));
#82972=CARTESIAN_POINT('Ctrl Pts',(-4.26171659160653,-8.96076940630961,
5.10274328646));
#82973=CARTESIAN_POINT('Ctrl Pts',(-4.26455589904718,-8.94989758613051,
5.10274328646));
#82974=CARTESIAN_POINT('Ctrl Pts',(-4.26715114281098,-8.93899011197066,
5.10274328646));
#82975=CARTESIAN_POINT('Ctrl Pts',(-4.26951780859379,-8.92807096217797,
5.10274328646));
#82976=CARTESIAN_POINT('Ctrl Pts',(-4.27382084868247,-8.90821790999222,
5.10274328646));
#82977=CARTESIAN_POINT('Ctrl Pts',(-4.27736537389317,-8.88833607622953,
5.10274328652144));
#82978=CARTESIAN_POINT('Ctrl Pts',(-4.28025710062774,-8.868557900564,5.10274328639925));
#82979=CARTESIAN_POINT('Ctrl Pts',(-4.28203791090249,-8.85637791895645,
5.102743286324));
#82980=CARTESIAN_POINT('Ctrl Pts',(-4.2835716533847,-8.84423662612072,5.10274328620522));
#82981=CARTESIAN_POINT('Ctrl Pts',(-4.2848866086288,-8.83215545542406,5.10274328535497));
#82982=CARTESIAN_POINT('Ctrl Pts',(-4.28680275059482,-8.81455087285411,
5.102743284116));
#82983=CARTESIAN_POINT('Ctrl Pts',(-4.28827698219617,-8.79709218114212,
5.10274328404483));
#82984=CARTESIAN_POINT('Ctrl Pts',(-4.28939927179632,-8.77979151596189,
5.10274328478464));
#82985=CARTESIAN_POINT('Ctrl Pts',(-4.29044254900022,-8.76370886706949,
5.10274328547236));
#82986=CARTESIAN_POINT('Ctrl Pts',(-4.29118189695424,-8.74776302279939,
5.10274328622038));
#82987=CARTESIAN_POINT('Ctrl Pts',(-4.29168885063704,-8.73191886459746,
5.1027432863823));
#82988=CARTESIAN_POINT('Ctrl Pts',(-4.29196579590166,-8.72326331136879,
5.10274328647075));
#82989=CARTESIAN_POINT('Ctrl Pts',(-4.29217335586042,-8.71463728288328,
5.10274328645986));
#82990=CARTESIAN_POINT('Ctrl Pts',(-4.29232279496067,-8.70602836504273,
5.10274328645976));
#82991=CARTESIAN_POINT('Ctrl Pts',(-4.29232279844,-8.70602816471,5.10274328646));
#82992=CARTESIAN_POINT('Ctrl Pts',(-4.20763985549,-8.70455745139,5.10274332142));
#82993=CARTESIAN_POINT('Ctrl Pts',(-4.12295691253,-8.70308673807,5.07285428042));
#82994=CARTESIAN_POINT('Ctrl Pts',(-4.05251729593,-8.70186339274,5.01281309848));
#82995=CARTESIAN_POINT('Ctrl Pts',(-4.00958603902,-8.70111779311,4.93392659864));
#82996=CARTESIAN_POINT('Ctrl Pts',(-3.99616141568,-8.70088464377,4.85030182916));
#82997=CARTESIAN_POINT('Ctrl Pts',(-4.29367604164,-8.62810126572,5.10274328646));
#82998=CARTESIAN_POINT('Ctrl Pts',(-4.20813285855,-8.6265058463,5.10274333195));
#82999=CARTESIAN_POINT('Ctrl Pts',(-4.12258967546,-8.62491042687,5.07224568401));
#83000=CARTESIAN_POINT('Ctrl Pts',(-4.0517315901,-8.62358850977,5.01097248773));
#83001=CARTESIAN_POINT('Ctrl Pts',(-4.00919737959,-8.62279415849,4.93071397417));
#83002=CARTESIAN_POINT('Ctrl Pts',(-3.99683804383,-8.62256210931,4.84604483372));
#83003=CARTESIAN_POINT('Ctrl Pts',(-4.29515862692,-8.55000353482,5.10274328646));
#83004=CARTESIAN_POINT('Ctrl Pts',(-4.20858147867,-8.54835950303,5.10274332811));
#83005=CARTESIAN_POINT('Ctrl Pts',(-4.12200433041,-8.54671547124,5.07150754218));
#83006=CARTESIAN_POINT('Ctrl Pts',(-4.05065454881,-8.5453604781,5.00873951265));
#83007=CARTESIAN_POINT('Ctrl Pts',(-4.0086265191,-8.54456207669,4.92682955987));
#83008=CARTESIAN_POINT('Ctrl Pts',(-3.99757933996,-8.54435185028,4.84092376899));
#83009=CARTESIAN_POINT('Ctrl Pts',(-4.2966466112,-8.47169636018,5.10274328646));
#83010=CARTESIAN_POINT('Ctrl Pts',(-4.20886559395,-8.47010372313,5.10274328646));
#83011=CARTESIAN_POINT('Ctrl Pts',(-4.12108457671,-8.46851108607,5.0706369892));
#83012=CARTESIAN_POINT('Ctrl Pts',(-4.049181176,-8.4672075164,5.00610503411));
#83013=CARTESIAN_POINT('Ctrl Pts',(-4.00779063879,-8.46645935943,4.92226864646));
#83014=CARTESIAN_POINT('Ctrl Pts',(-3.99832332564,-8.46629167717,4.83495432364));
#83015=CARTESIAN_POINT('Ctrl Pts',(-4.29796673138,-8.39314927373,5.10274328646));
#83016=CARTESIAN_POINT('Ctrl Pts',(-4.20881731963,-8.39173518355,5.10274328646));
#83017=CARTESIAN_POINT('Ctrl Pts',(-4.11966790787,-8.39032109337,5.06963007213));
#83018=CARTESIAN_POINT('Ctrl Pts',(-4.04716501903,-8.3891735059,5.00305604873));
#83019=CARTESIAN_POINT('Ctrl Pts',(-4.00657458492,-8.38853640885,4.91702461127));
#83020=CARTESIAN_POINT('Ctrl Pts',(-3.99898336569,-8.38842527481,4.8281587616));
#83021=CARTESIAN_POINT('Ctrl Pts',(-4.29889875178,-8.31430322211,5.10274328646));
#83022=CARTESIAN_POINT('Ctrl Pts',(-4.20822334583,-8.31323136973,5.10274328646));
#83023=CARTESIAN_POINT('Ctrl Pts',(-4.11754793987,-8.31215951735,5.06848004433));
#83024=CARTESIAN_POINT('Ctrl Pts',(-4.04442178691,-8.31129511051,4.99957103487));
#83025=CARTESIAN_POINT('Ctrl Pts',(-4.00483540394,-8.3108271693,4.91108461112));
#83026=CARTESIAN_POINT('Ctrl Pts',(-3.99944937589,-8.31076350235,4.82056298519));
#83027=CARTESIAN_POINT('',(-3.9961616700265,-8.70088464035681,4.85030293837252));
#83028=CARTESIAN_POINT('Origin',(-4.2906912681792,-8.70600002892326,4.80465840215202));
#83029=CARTESIAN_POINT('',(-3.9994493766888,-8.31076354696256,4.82056300748371));
#83030=CARTESIAN_POINT('Origin',(-4.29696517402085,-8.31428035436309,4.80479513966836));
#83031=CARTESIAN_POINT('Ctrl Pts',(-3.9961615961339,-8.70088460680108,4.85030294889421));
#83032=CARTESIAN_POINT('Ctrl Pts',(-3.99678390426082,-8.62885486806307,
4.846388344858));
#83033=CARTESIAN_POINT('Ctrl Pts',(-3.99747548605133,-8.5569395249013,4.84159514513512));
#83034=CARTESIAN_POINT('Ctrl Pts',(-3.99810969192043,-8.48520158611709,
4.83595601816904));
#83035=CARTESIAN_POINT('Ctrl Pts',(-3.99862484060351,-8.42693075247652,
4.83137550421942));
#83036=CARTESIAN_POINT('Ctrl Pts',(-3.99910126161364,-8.36877776894241,
4.8262371302703));
#83037=CARTESIAN_POINT('Ctrl Pts',(-3.9994493766893,-8.31076354696257,4.82056300748368));
#83038=CARTESIAN_POINT('Ctrl Pts',(-3.69999999774,-9.41827086749,5.10274328646));
#83039=CARTESIAN_POINT('Ctrl Pts',(-3.69999999833,-9.34659890209,5.10274328646));
#83040=CARTESIAN_POINT('Ctrl Pts',(-3.69999999892,-9.2749269367,5.0813396589));
#83041=CARTESIAN_POINT('Ctrl Pts',(-3.69999999944,-9.21183540432,5.03842913842));
#83042=CARTESIAN_POINT('Ctrl Pts',(-3.69999999982,-9.16559336719,4.97963577235));
#83043=CARTESIAN_POINT('Ctrl Pts',(-3.70000000003,-9.13925764692,4.91297768617));
#83044=CARTESIAN_POINT('Ctrl Pts',(-3.81412909821,-9.41827089013,5.10274328646));
#83045=CARTESIAN_POINT('Ctrl Pts',(-3.79947056194,-9.34659892134,5.10274328643));
#83046=CARTESIAN_POINT('Ctrl Pts',(-3.78481202566,-9.27492695255,5.08133965881));
#83047=CARTESIAN_POINT('Ctrl Pts',(-3.77190837788,-9.21183541723,5.03842913824));
#83048=CARTESIAN_POINT('Ctrl Pts',(-3.76245084042,-9.16559337792,4.97963577207));
#83049=CARTESIAN_POINT('Ctrl Pts',(-3.75706459059,-9.13925765647,4.9129776858));
#83050=CARTESIAN_POINT('Ctrl Pts',(-3.92823594404,-9.38909765086,5.10274328646));
#83051=CARTESIAN_POINT('Ctrl Pts',(-3.89892199959,-9.32091627439,5.10274328539));
#83052=CARTESIAN_POINT('Ctrl Pts',(-3.86960805513,-9.25273489792,5.08118011966));
#83053=CARTESIAN_POINT('Ctrl Pts',(-3.84380320278,-9.19278171906,5.03794838538));
#83054=CARTESIAN_POINT('Ctrl Pts',(-3.82488943837,-9.14898176867,4.97875813986));
#83055=CARTESIAN_POINT('Ctrl Pts',(-3.81411802643,-9.12422889542,4.91173129034));
#83056=CARTESIAN_POINT('Ctrl Pts',(-4.03302804821,-9.33107957038,5.10274328646));
#83057=CARTESIAN_POINT('Ctrl Pts',(-3.99017706972,-9.2696193654,5.10274329028));
#83058=CARTESIAN_POINT('Ctrl Pts',(-3.94732609124,-9.20815916043,5.08092237264));
#83059=CARTESIAN_POINT('Ctrl Pts',(-3.90964076698,-9.15426319663,5.03717158458));
#83060=CARTESIAN_POINT('Ctrl Pts',(-3.8820963349,-9.11520770945,4.97734162836));
#83061=CARTESIAN_POINT('Ctrl Pts',(-3.86651403782,-9.0935734628,4.90972003087));
#83062=CARTESIAN_POINT('Ctrl Pts',(-4.18747374061,-9.18016437508,5.10274328646));
#83063=CARTESIAN_POINT('Ctrl Pts',(-4.12388018645,-9.13700016797,5.1027432833));
#83064=CARTESIAN_POINT('Ctrl Pts',(-4.0602866323,-9.09383596087,5.07981408986));
#83065=CARTESIAN_POINT('Ctrl Pts',(-4.00475631151,-9.05633061601,5.03383155537));
#83066=CARTESIAN_POINT('Ctrl Pts',(-3.96503122609,-9.029900996,4.97125605817));
#83067=CARTESIAN_POINT('Ctrl Pts',(-3.94373685893,-9.0162718551,4.90110872718));
#83068=CARTESIAN_POINT('Ctrl Pts',(-4.26723541157,-8.98063713586,5.10274328646));
#83069=CARTESIAN_POINT('Ctrl Pts',(-4.19077919927,-8.95915602901,5.10274328908));
#83070=CARTESIAN_POINT('Ctrl Pts',(-4.11432298698,-8.93767492216,5.07732616962));
#83071=CARTESIAN_POINT('Ctrl Pts',(-4.04869892936,-8.91937700045,5.02632575237));
#83072=CARTESIAN_POINT('Ctrl Pts',(-4.00420277032,-8.90727654877,4.95775964986));
#83073=CARTESIAN_POINT('Ctrl Pts',(-3.98361771521,-8.90210958415,4.88238701109));
#83074=CARTESIAN_POINT('Ctrl Pts',(-4.28448738522,-8.88291546038,5.10274328646));
#83075=CARTESIAN_POINT('Ctrl Pts',(-4.2038128468,-8.87211558957,5.10274328157));
#83076=CARTESIAN_POINT('Ctrl Pts',(-4.12313830838,-8.86131571876,5.07547605456));
#83077=CARTESIAN_POINT('Ctrl Pts',(-4.05474416619,-8.85231492765,5.02074277903));
#83078=CARTESIAN_POINT('Ctrl Pts',(-4.01023278232,-8.84679291313,4.94775348423));
#83079=CARTESIAN_POINT('Ctrl Pts',(-3.99224364397,-8.84501961539,4.86859296944));
#83080=CARTESIAN_POINT('Ctrl Pts',(-4.2908008405,-8.79368075155,5.10274328646));
#83081=CARTESIAN_POINT('Ctrl Pts',(-4.20683195096,-8.78806573108,5.10274328646));
#83082=CARTESIAN_POINT('Ctrl Pts',(-4.12286306143,-8.78245071061,5.07330735934));
#83083=CARTESIAN_POINT('Ctrl Pts',(-4.05279621082,-8.77777630692,5.01418352542));
#83084=CARTESIAN_POINT('Ctrl Pts',(-4.00960658253,-8.77491887358,4.93631857882));
#83085=CARTESIAN_POINT('Ctrl Pts',(-3.99540042025,-8.7740131878,4.85347142938));
#83086=CARTESIAN_POINT('Ctrl Pts',(-4.29232317424,-8.70602837163,5.10274328646));
#83087=CARTESIAN_POINT('Ctrl Pts',(-4.20764026079,-8.70455761115,5.10274328646));
#83088=CARTESIAN_POINT('Ctrl Pts',(-4.12295734733,-8.70308685067,5.07285429077));
#83089=CARTESIAN_POINT('Ctrl Pts',(-4.05251771609,-8.70186346543,5.01281324223));
#83090=CARTESIAN_POINT('Ctrl Pts',(-4.00958636427,-8.70111783998,4.93392690561));
#83091=CARTESIAN_POINT('Ctrl Pts',(-3.99616158712,-8.70088468041,4.85030226832));
#83092=CARTESIAN_POINT('Ctrl Pts',(-3.70000000003,-9.13925764692,4.91297768617));
#83093=CARTESIAN_POINT('Ctrl Pts',(-3.71529015207103,-9.13925764947887,
4.91297768607086));
#83094=CARTESIAN_POINT('Ctrl Pts',(-3.73014416026747,-9.13797639510877,
4.91291207427923));
#83095=CARTESIAN_POINT('Ctrl Pts',(-3.74442150434438,-9.1356118541454,4.91277684154045));
#83096=CARTESIAN_POINT('Ctrl Pts',(-3.75913917708147,-9.13317438819342,
4.91263743807842));
#83097=CARTESIAN_POINT('Ctrl Pts',(-3.77324400464638,-9.12958776148789,
4.91242293557063));
#83098=CARTESIAN_POINT('Ctrl Pts',(-3.78663328576126,-9.12507402641783,
4.91210731666113));
#83099=CARTESIAN_POINT('Ctrl Pts',(-3.8002070348353,-9.12049810432745,4.91178734937955));
#83100=CARTESIAN_POINT('Ctrl Pts',(-3.81304573279602,-9.11497046038793,
4.91136276950297));
#83101=CARTESIAN_POINT('Ctrl Pts',(-3.8250917003685,-9.10870418173369,4.91079849724977));
#83102=CARTESIAN_POINT('Ctrl Pts',(-3.8292814570418,-9.10652468202556,4.9106022354365));
#83103=CARTESIAN_POINT('Ctrl Pts',(-3.83337571956335,-9.10425559637984,
4.91038904836799));
#83104=CARTESIAN_POINT('Ctrl Pts',(-3.83737329592438,-9.10190509538605,
4.91015742089567));
#83105=CARTESIAN_POINT('Ctrl Pts',(-3.8488097273671,-9.09518068513249,4.90949477146307));
#83106=CARTESIAN_POINT('Ctrl Pts',(-3.8594617959262,-9.08779972523566,4.9087105172242));
#83107=CARTESIAN_POINT('Ctrl Pts',(-3.86933226327774,-9.07995068541308,
4.90782345834443));
#83108=CARTESIAN_POINT('Ctrl Pts',(-3.87578520446725,-9.07481927769292,
4.90724353253354));
#83109=CARTESIAN_POINT('Ctrl Pts',(-3.88190505349891,-9.06948713729174,
4.90661977297618));
#83110=CARTESIAN_POINT('Ctrl Pts',(-3.88770139233235,-9.0639990067157,4.90595898381691));
#83111=CARTESIAN_POINT('Ctrl Pts',(-3.89503262347501,-9.05705759853542,
4.90512321520462));
#83112=CARTESIAN_POINT('Ctrl Pts',(-3.90184468314376,-9.0498682586582,4.90422830374491));
#83113=CARTESIAN_POINT('Ctrl Pts',(-3.90816884420435,-9.04251720447913,
4.90330690801195));
#83114=CARTESIAN_POINT('Ctrl Pts',(-3.91133092473464,-9.0388416773896,4.90284621014547));
#83115=CARTESIAN_POINT('Ctrl Pts',(-3.91436903980901,-9.03512384425042,
4.90237127730828));
#83116=CARTESIAN_POINT('Ctrl Pts',(-3.9172869481511,-9.03137248254924,4.90188194411826));
#83117=CARTESIAN_POINT('Ctrl Pts',(-3.91874590232215,-9.02949680169865,
4.90163727752325));
#83118=CARTESIAN_POINT('Ctrl Pts',(-3.92017480408882,-9.02761274156667,
4.90138901495576));
#83119=CARTESIAN_POINT('Ctrl Pts',(-3.92157419015545,-9.02572141015965,
4.90113729933359));
#83120=CARTESIAN_POINT('Ctrl Pts',(-3.92238337566387,-9.0246277605924,4.90099174648113));
#83121=CARTESIAN_POINT('Ctrl Pts',(-3.92290954425151,-9.02390648865029,
4.90089521932563));
#83122=CARTESIAN_POINT('Ctrl Pts',(-3.92362915257453,-9.02291017871459,
4.90076221167712));
#83123=CARTESIAN_POINT('Ctrl Pts',(-3.92415401767594,-9.0221834940742,4.90066519907917));
#83124=CARTESIAN_POINT('Ctrl Pts',(-3.92478177136042,-9.0213104522166,4.90054877457427));
#83125=CARTESIAN_POINT('Ctrl Pts',(-3.9256856428377,-9.02002767016122,4.90037663508057));
#83126=CARTESIAN_POINT('Ctrl Pts',(-3.93076928149868,-9.01281292712051,
4.8994084720095));
#83127=CARTESIAN_POINT('Ctrl Pts',(-3.93546808728794,-9.0054636078729,4.89838345132082));
#83128=CARTESIAN_POINT('Ctrl Pts',(-3.93981071245734,-8.99801619371013,
4.89730809585987));
#83129=CARTESIAN_POINT('Ctrl Pts',(-3.94482881368225,-8.98941036735518,
4.89606547363361));
#83130=CARTESIAN_POINT('Ctrl Pts',(-3.9493701033765,-8.98067630776327,4.89475285872136));
#83131=CARTESIAN_POINT('Ctrl Pts',(-3.95347304747733,-8.9718716535676,4.8933511552548));
#83132=CARTESIAN_POINT('Ctrl Pts',(-3.95830199337999,-8.96150904619162,
4.89170142519629));
#83133=CARTESIAN_POINT('Ctrl Pts',(-3.9625243731347,-8.95104726054702,4.88992847546876));
#83134=CARTESIAN_POINT('Ctrl Pts',(-3.96622543769305,-8.94053252013442,
4.88804954732827));
#83135=CARTESIAN_POINT('Ctrl Pts',(-3.97105362982472,-8.92681560541267,
4.88559840768431));
#83136=CARTESIAN_POINT('Ctrl Pts',(-3.97499639173049,-8.91300578021216,
4.88296736034851));
#83137=CARTESIAN_POINT('Ctrl Pts',(-3.97825803337248,-8.89916845917825,
4.88026821014047));
#83138=CARTESIAN_POINT('Ctrl Pts',(-3.98093354530121,-8.8878177586564,4.87805410774305));
#83139=CARTESIAN_POINT('Ctrl Pts',(-3.98315132864282,-8.87644764305007,
4.87579638200634));
#83140=CARTESIAN_POINT('Ctrl Pts',(-3.98501607995159,-8.8650995212513,4.87357227374489));
#83141=CARTESIAN_POINT('Ctrl Pts',(-3.98704683592159,-8.85274116226647,
4.87115016999914));
#83142=CARTESIAN_POINT('Ctrl Pts',(-3.98865981875432,-8.84041605363061,
4.86876464610217));
#83143=CARTESIAN_POINT('Ctrl Pts',(-3.98998120246124,-8.82802685533874,
4.86648143874877));
#83144=CARTESIAN_POINT('Ctrl Pts',(-3.99138671146833,-8.81484890430245,
4.86405287202475));
#83145=CARTESIAN_POINT('Ctrl Pts',(-3.99246174015616,-8.80159798477713,
4.86173834904854));
#83146=CARTESIAN_POINT('Ctrl Pts',(-3.99330779305355,-8.78813311929187,
4.85962424523925));
#83147=CARTESIAN_POINT('Ctrl Pts',(-3.99408249088382,-8.77580386410155,
4.85768844236086));
#83148=CARTESIAN_POINT('Ctrl Pts',(-3.99466399994344,-8.76329376004554,
4.85591896163928));
#83149=CARTESIAN_POINT('Ctrl Pts',(-3.99510413495378,-8.75049000131564,
4.85441263397948));
#83150=CARTESIAN_POINT('Ctrl Pts',(-3.99546774267706,-8.73991246157952,
4.85316821497618));
#83151=CARTESIAN_POINT('Ctrl Pts',(-3.99573425864729,-8.72913360479011,
4.8521030453621));
#83152=CARTESIAN_POINT('Ctrl Pts',(-3.99592511106015,-8.71810107884211,
4.85130447744043));
#83153=CARTESIAN_POINT('Ctrl Pts',(-3.9960232071946,-8.71243047645101,4.85089402192122));
#83154=CARTESIAN_POINT('Ctrl Pts',(-3.99610122682654,-8.70669311547007,
4.85055459128874));
#83155=CARTESIAN_POINT('Ctrl Pts',(-3.99616169433912,-8.70088468227217,
4.8503029361967));
#83156=CARTESIAN_POINT('Ctrl Pts',(-3.7,-8.72799905369119,4.59960059693865));
#83157=CARTESIAN_POINT('Ctrl Pts',(-3.7,-9.02827749416229,4.63207689308604));
#83158=CARTESIAN_POINT('Ctrl Pts',(-3.7,-9.13925764782821,4.91297768894732));
#83159=CARTESIAN_POINT('Ctrl Pts',(-3.95543243018288,-8.72799905369119,
4.59960059693865));
#83160=CARTESIAN_POINT('Ctrl Pts',(-3.95543243018288,-9.02827749416229,
4.63207689308604));
#83161=CARTESIAN_POINT('Ctrl Pts',(-3.95543243018288,-9.13925764782821,
4.91297768894732));
#83162=CARTESIAN_POINT('Ctrl Pts',(-3.99616169476815,-8.70088460874173,
4.85030293093368));
#83163=CARTESIAN_POINT('Ctrl Pts',(-3.99616169476815,-8.84972402085523,
4.86640049963897));
#83164=CARTESIAN_POINT('Ctrl Pts',(-3.99616169476815,-8.90473370054448,
5.00563496899553));
#83165=CARTESIAN_POINT('Origin',(-3.7,-8.69574098918,4.89786125018));
#83166=CARTESIAN_POINT('Origin',(-3.7,-9.17423561284,0.47366156039));
#83167=CARTESIAN_POINT('',(-3.99951365747597,-8.00613534473186,4.74991749256093));
#83168=CARTESIAN_POINT('Ctrl Pts',(-3.99944937669,-8.31076354672,4.82056300746));
#83169=CARTESIAN_POINT('Ctrl Pts',(-3.99959839809,-8.28592729564,4.81813395331));
#83170=CARTESIAN_POINT('Ctrl Pts',(-3.99969341422,-8.26106714699,4.8150399126));
#83171=CARTESIAN_POINT('Ctrl Pts',(-3.99975395169,-8.23622932864,4.81128563568));
#83172=CARTESIAN_POINT('Ctrl Pts',(-3.99984876957,-8.17436353389,4.80027772376));
#83173=CARTESIAN_POINT('Ctrl Pts',(-3.99983052524,-8.11319387748,4.78525185918));
#83174=CARTESIAN_POINT('Ctrl Pts',(-3.99979379772,-8.07691196013,4.77482737361));
#83175=CARTESIAN_POINT('Ctrl Pts',(-3.99970844997,-8.04117830882,4.76303153489));
#83176=CARTESIAN_POINT('Ctrl Pts',(-3.99951367307,-8.00613533845,4.74991748836));
#83177=CARTESIAN_POINT('',(-4.,-6.41575007864,3.96554608849));
#83178=CARTESIAN_POINT('Ctrl Pts',(-3.99951362599666,-8.00613533213075,
4.74991748884671));
#83179=CARTESIAN_POINT('Ctrl Pts',(-3.99912775537927,-7.93670347374554,
4.72393400135952));
#83180=CARTESIAN_POINT('Ctrl Pts',(-3.99857222013012,-7.86774756468867,
4.69717811451172));
#83181=CARTESIAN_POINT('Ctrl Pts',(-3.99801113590394,-7.79918725181215,
4.66959751880907));
#83182=CARTESIAN_POINT('Ctrl Pts',(-3.99744761007927,-7.730328593788,4.64189690415447));
#83183=CARTESIAN_POINT('Ctrl Pts',(-3.99687800868216,-7.66186886095888,
4.61336445780402));
#83184=CARTESIAN_POINT('Ctrl Pts',(-3.99641199162889,-7.59372678110788,
4.58394586052179));
#83185=CARTESIAN_POINT('Ctrl Pts',(-3.99594125784065,-7.52489500947846,
4.55422950648306));
#83186=CARTESIAN_POINT('Ctrl Pts',(-3.995576066866,-7.45638723799201,4.52360898626897));
#83187=CARTESIAN_POINT('Ctrl Pts',(-3.99537650648205,-7.3881216373169,4.49202632379195));
#83188=CARTESIAN_POINT('Ctrl Pts',(-3.99518351319893,-7.32210250998592,
4.46148297846278));
#83189=CARTESIAN_POINT('Ctrl Pts',(-3.99514521891445,-7.25630980867474,
4.43003972020292));
#83190=CARTESIAN_POINT('Ctrl Pts',(-3.99526985343324,-7.19067264205082,
4.39764258740694));
#83191=CARTESIAN_POINT('Ctrl Pts',(-3.99539848691283,-7.12292947414796,
4.36420597642182));
#83192=CARTESIAN_POINT('Ctrl Pts',(-3.99570001270616,-7.05585580407319,
4.33000186128198));
#83193=CARTESIAN_POINT('Ctrl Pts',(-3.99612402104634,-6.98939603026552,
4.29503064588602));
#83194=CARTESIAN_POINT('Ctrl Pts',(-3.9965462561408,-6.92321419794775,4.26020568364672));
#83195=CARTESIAN_POINT('Ctrl Pts',(-3.99708992828748,-6.85764109095415,
4.22461998892733));
#83196=CARTESIAN_POINT('Ctrl Pts',(-3.99765401687659,-6.79262048515617,
4.18827520267667));
#83197=CARTESIAN_POINT('Ctrl Pts',(-3.99820754909831,-6.72881667653507,
4.1526105736279));
#83198=CARTESIAN_POINT('Ctrl Pts',(-3.998780787767,-6.66554485798596,4.11621493441839));
#83199=CARTESIAN_POINT('Ctrl Pts',(-3.99922880371063,-6.60275116879257,
4.07909177039002));
#83200=CARTESIAN_POINT('Ctrl Pts',(-3.99967681965425,-6.53995747959918,
4.04196860636165));
#83201=CARTESIAN_POINT('Ctrl Pts',(-4.,-6.47764191894906,4.00411781442964));
#83202=CARTESIAN_POINT('Ctrl Pts',(-4.,-6.41575007864,3.96554608849));
#83203=CARTESIAN_POINT('Origin',(-4.,-9.17423561284,0.47366156039));
#83204=CARTESIAN_POINT('Ctrl Pts',(-4.29889876134,-8.31430322282,5.1027434229));
#83205=CARTESIAN_POINT('Ctrl Pts',(-4.2082233452,-8.31323138881,5.10274342246));
#83206=CARTESIAN_POINT('Ctrl Pts',(-4.11754792907,-8.31215955225,5.0684801702));
#83207=CARTESIAN_POINT('Ctrl Pts',(-4.04442177042,-8.31129515513,4.99957114081));
#83208=CARTESIAN_POINT('Ctrl Pts',(-4.00483538997,-8.31082721545,4.91108469399));
#83209=CARTESIAN_POINT('Ctrl Pts',(-3.99944937087,-8.31076354298,4.8205630482));
#83210=CARTESIAN_POINT('Ctrl Pts',(-4.29964314059,-8.22434260602,5.1027436292));
#83211=CARTESIAN_POINT('Ctrl Pts',(-4.20780699632,-8.22403023518,5.10264720521));
#83212=CARTESIAN_POINT('Ctrl Pts',(-4.11597085206,-8.22680019636,5.06741723002));
#83213=CARTESIAN_POINT('Ctrl Pts',(-4.0423682592,-8.23275280902,4.99666339283));
#83214=CARTESIAN_POINT('Ctrl Pts',(-4.00353912359,-8.24059165767,4.90627699718));
#83215=CARTESIAN_POINT('Ctrl Pts',(-3.99982155439,-8.24873700866,4.81449657867));
#83216=CARTESIAN_POINT('Ctrl Pts',(-4.29971371834,-8.13469356333,5.09262744205));
#83217=CARTESIAN_POINT('Ctrl Pts',(-4.20724144925,-8.13466365636,5.09260573663));
#83218=CARTESIAN_POINT('Ctrl Pts',(-4.11476918016,-8.14098347585,5.05729879766));
#83219=CARTESIAN_POINT('Ctrl Pts',(-4.04093270982,-8.15373242653,4.98629044613));
#83220=CARTESIAN_POINT('Ctrl Pts',(-4.00258694952,-8.1700271987,4.89579754059));
#83221=CARTESIAN_POINT('Ctrl Pts',(-3.99985686503,-8.18656139935,4.80428277208));
#83222=CARTESIAN_POINT('Ctrl Pts',(-4.29971786827,-8.04665414995,5.07253279403));
#83223=CARTESIAN_POINT('Ctrl Pts',(-4.20720101416,-8.04666571693,5.07252348963));
#83224=CARTESIAN_POINT('Ctrl Pts',(-4.11468416006,-8.05626571803,5.0379315222));
#83225=CARTESIAN_POINT('Ctrl Pts',(-4.04083150668,-8.07556834767,4.96834669024));
#83226=CARTESIAN_POINT('Ctrl Pts',(-4.00251997495,-8.10013935979,4.87966809703));
#83227=CARTESIAN_POINT('Ctrl Pts',(-3.9998589855,-8.12494698597,4.78999433407));
#83228=CARTESIAN_POINT('Ctrl Pts',(-4.29967705707,-7.96150927709,5.0427549913));
#83229=CARTESIAN_POINT('Ctrl Pts',(-4.20771171282,-7.96176972051,5.0427867655));
#83230=CARTESIAN_POINT('Ctrl Pts',(-4.11574636857,-7.97452633141,5.00973042736));
#83231=CARTESIAN_POINT('Ctrl Pts',(-4.04209470673,-7.99987188278,4.94319135382));
#83232=CARTESIAN_POINT('Ctrl Pts',(-4.00335979512,-8.03206135592,4.85814590158));
#83233=CARTESIAN_POINT('Ctrl Pts',(-3.99983852853,-8.06458049923,4.77178934946));
#83234=CARTESIAN_POINT('Ctrl Pts',(-4.29902733552,-7.88049121843,5.00374669681));
#83235=CARTESIAN_POINT('Ctrl Pts',(-4.20814475196,-7.88133646016,5.00415366088));
#83236=CARTESIAN_POINT('Ctrl Pts',(-4.1172621684,-7.89711301226,4.97354912353));
#83237=CARTESIAN_POINT('Ctrl Pts',(-4.04405132352,-7.92782452293,4.91150502168));
#83238=CARTESIAN_POINT('Ctrl Pts',(-4.00460096887,-7.96672185729,4.83165611315));
#83239=CARTESIAN_POINT('Ctrl Pts',(-3.99951366776,-8.00613540701,4.74991741048));
#83240=CARTESIAN_POINT('Origin',(-4.29708374629736,-8.00976110076321,4.73530658527947));
#83241=CARTESIAN_POINT('Ctrl Pts',(-4.2990272509,-7.88049121843,5.00374669681));
#83242=CARTESIAN_POINT('Ctrl Pts',(-4.20814466399,-7.88133645067,5.00415365756));
#83243=CARTESIAN_POINT('Ctrl Pts',(-4.11726207707,-7.8971129981,4.97354910689));
#83244=CARTESIAN_POINT('Ctrl Pts',(-4.04405123536,-7.92782451085,4.91150498201));
#83245=CARTESIAN_POINT('Ctrl Pts',(-4.00460089543,-7.96672185122,4.83165605064));
#83246=CARTESIAN_POINT('Ctrl Pts',(-3.99951361632,-8.0061354071,4.74991733337));
#83247=CARTESIAN_POINT('Ctrl Pts',(-4.29534152276,-7.55873090479,4.8488266546));
#83248=CARTESIAN_POINT('Ctrl Pts',(-4.21089110293,-7.56075677108,4.84980205594));
#83249=CARTESIAN_POINT('Ctrl Pts',(-4.12644068311,-7.57560508753,4.82414594128));
#83250=CARTESIAN_POINT('Ctrl Pts',(-4.05583695285,-7.60300935451,4.77146524893));
#83251=CARTESIAN_POINT('Ctrl Pts',(-4.01210473647,-7.6379921895,4.70122601239));
#83252=CARTESIAN_POINT('Ctrl Pts',(-3.99767078695,-7.67454601586,4.62582683568));
#83253=CARTESIAN_POINT('Ctrl Pts',(-4.28495419985,-7.24223776902,4.69644263496));
#83254=CARTESIAN_POINT('Ctrl Pts',(-4.20364197507,-7.24265108624,4.69664162775));
#83255=CARTESIAN_POINT('Ctrl Pts',(-4.12232975028,-7.25504442659,4.67195877864));
#83256=CARTESIAN_POINT('Ctrl Pts',(-4.05372035815,-7.27955010958,4.62221233106));
#83257=CARTESIAN_POINT('Ctrl Pts',(-4.00967965098,-7.31194178404,4.55622127864));
#83258=CARTESIAN_POINT('Ctrl Pts',(-3.99247722227,-7.34677145748,4.48508959035));
#83259=CARTESIAN_POINT('Ctrl Pts',(-4.28719359971,-6.92729615453,4.54480563642));
#83260=CARTESIAN_POINT('Ctrl Pts',(-4.20516486744,-6.92619358841,4.54427477668));
#83261=CARTESIAN_POINT('Ctrl Pts',(-4.12313613516,-6.93728087775,4.51842626492));
#83262=CARTESIAN_POINT('Ctrl Pts',(-4.05411385932,-6.96067605503,4.46706057541));
#83263=CARTESIAN_POINT('Ctrl Pts',(-4.01020087277,-6.99204699421,4.39931666036));
#83264=CARTESIAN_POINT('Ctrl Pts',(-3.99359726714,-7.02607103842,4.32667666396));
#83265=CARTESIAN_POINT('Ctrl Pts',(-4.3,-6.60947733541,4.39178333134));
#83266=CARTESIAN_POINT('Ctrl Pts',(-4.21340350799,-6.60705721212,4.39061809876));
#83267=CARTESIAN_POINT('Ctrl Pts',(-4.12680701597,-6.61808600203,4.3615202213));
#83268=CARTESIAN_POINT('Ctrl Pts',(-4.0550389398,-6.64318599408,4.30449502667));
#83269=CARTESIAN_POINT('Ctrl Pts',(-4.01201861445,-6.67775474512,4.23026617343));
#83270=CARTESIAN_POINT('Ctrl Pts',(-4.,-6.71532134284,4.1522424388));
#83271=CARTESIAN_POINT('Ctrl Pts',(-4.3,-6.28560647753,4.2358471116));
#83272=CARTESIAN_POINT('Ctrl Pts',(-4.20575222039,-6.28560647753,4.2358471116));
#83273=CARTESIAN_POINT('Ctrl Pts',(-4.11150444078,-6.30166230076,4.20250005951));
#83274=CARTESIAN_POINT('Ctrl Pts',(-4.0370110165,-6.33397844241,4.13538123018));
#83275=CARTESIAN_POINT('Ctrl Pts',(-4.,-6.37486426052,4.05046365934));
#83276=CARTESIAN_POINT('Ctrl Pts',(-4.,-6.41575007864,3.96554608849));
#83277=CARTESIAN_POINT('Origin',(-4.29787865889067,-6.41482978920342,3.96745741146091));
#83278=CARTESIAN_POINT('Origin',(-4.3,-2.74845588872,2.19982997428));
#83279=CARTESIAN_POINT('',(-4.,-4.55379688725,3.06905931004));
#83280=CARTESIAN_POINT('Origin',(-4.,0.,0.));
#83281=CARTESIAN_POINT('',(0.,0.,0.));
#83282=CARTESIAN_POINT('Ctrl Pts',(-11.2571565141535,-6.63753909988913,
0.));
#83283=CARTESIAN_POINT('Ctrl Pts',(-11.2571565141535,-6.63753909988913,
22.5143130283071));
#83284=CARTESIAN_POINT('Ctrl Pts',(11.2571565141535,-6.63753909988913,22.5143130283071));
#83285=CARTESIAN_POINT('Ctrl Pts',(11.2571565141535,-6.63753909988913,1.37860406925589E-15));
#83286=CARTESIAN_POINT('Ctrl Pts',(-11.2316061906402,-5.55581078583997,
0.));
#83287=CARTESIAN_POINT('Ctrl Pts',(-11.2316061906402,-5.55581078583997,
22.4632123812804));
#83288=CARTESIAN_POINT('Ctrl Pts',(11.2316061906402,-5.55581078583997,22.4632123812804));
#83289=CARTESIAN_POINT('Ctrl Pts',(11.2316061906402,-5.55581078583997,1.37547505706511E-15));
#83290=CARTESIAN_POINT('Ctrl Pts',(-11.1603664914423,-4.97414426866896,
0.));
#83291=CARTESIAN_POINT('Ctrl Pts',(-11.1603664914423,-4.97414426866896,
22.3207329828847));
#83292=CARTESIAN_POINT('Ctrl Pts',(11.1603664914423,-4.97414426866896,22.3207329828847));
#83293=CARTESIAN_POINT('Ctrl Pts',(11.1603664914423,-4.97414426866896,1.36675071010562E-15));
#83294=CARTESIAN_POINT('Ctrl Pts',(-10.527435261753,-4.27423561284,0.));
#83295=CARTESIAN_POINT('Ctrl Pts',(-10.527435261753,-4.27423561284,21.054870523506));
#83296=CARTESIAN_POINT('Ctrl Pts',(10.527435261753,-4.27423561284,21.054870523506));
#83297=CARTESIAN_POINT('Ctrl Pts',(10.527435261753,-4.27423561284,1.28923898965368E-15));
#83298=CARTESIAN_POINT('Ctrl Pts',(-10.5228448600506,-4.26915945016304,
0.));
#83299=CARTESIAN_POINT('Ctrl Pts',(-10.5228448600506,-4.26915945016304,
21.0456897201012));
#83300=CARTESIAN_POINT('Ctrl Pts',(10.5228448600506,-4.26915945016304,21.0456897201012));
#83301=CARTESIAN_POINT('Ctrl Pts',(10.5228448600506,-4.26915945016304,1.28867682757851E-15));
#83302=CARTESIAN_POINT('Ctrl Pts',(-10.5182544583482,-4.26408328748608,
0.));
#83303=CARTESIAN_POINT('Ctrl Pts',(-10.5182544583482,-4.26408328748608,
21.0365089166964));
#83304=CARTESIAN_POINT('Ctrl Pts',(10.5182544583482,-4.26408328748608,21.0365089166964));
#83305=CARTESIAN_POINT('Ctrl Pts',(10.5182544583482,-4.26408328748608,1.28811466550335E-15));
#83306=CARTESIAN_POINT('Ctrl Pts',(-10.5136640566458,-4.25900712480911,
0.));
#83307=CARTESIAN_POINT('Ctrl Pts',(-10.5136640566458,-4.25900712480911,
21.0273281132916));
#83308=CARTESIAN_POINT('Ctrl Pts',(10.5136640566458,-4.25900712480911,21.0273281132916));
#83309=CARTESIAN_POINT('Ctrl Pts',(10.5136640566458,-4.25900712480911,1.28755250342819E-15));
#83310=CARTESIAN_POINT('',(11.0953289065065,-6.63753909988913,1.90190673814221));
#83311=CARTESIAN_POINT('',(11.2571565141535,-6.63753909988913,1.37860406925589E-15));
#83312=CARTESIAN_POINT('Origin',(0.,-6.63753909988913,0.));
#83313=CARTESIAN_POINT('',(10.527435261753,-4.27423561284,1.28923898965368E-15));
#83314=CARTESIAN_POINT('Ctrl Pts',(11.2571565141535,-6.63753909988913,1.37860406925589E-15));
#83315=CARTESIAN_POINT('Ctrl Pts',(11.2316061906402,-5.55581078583997,1.37547505706511E-15));
#83316=CARTESIAN_POINT('Ctrl Pts',(11.1603664914423,-4.97414426866896,1.36675071010562E-15));
#83317=CARTESIAN_POINT('Ctrl Pts',(10.527435261753,-4.27423561284,1.28923898965368E-15));
#83318=CARTESIAN_POINT('',(-10.527435261753,-4.27423561284,0.));
#83319=CARTESIAN_POINT('Origin',(0.,-4.27423561284,0.));
#83320=CARTESIAN_POINT('',(-11.2571565141535,-6.63753909988913,0.));
#83321=CARTESIAN_POINT('Ctrl Pts',(-11.2571565141535,-6.63753909988913,
0.));
#83322=CARTESIAN_POINT('Ctrl Pts',(-11.2316061906402,-5.55581078583997,
0.));
#83323=CARTESIAN_POINT('Ctrl Pts',(-11.1603664914423,-4.97414426866896,
0.));
#83324=CARTESIAN_POINT('Ctrl Pts',(-10.527435261753,-4.27423561284,0.));
#83325=CARTESIAN_POINT('',(-11.0953289065065,-6.63753909988913,1.90190673814229));
#83326=CARTESIAN_POINT('Origin',(0.,-6.63753909988913,0.));
#83327=CARTESIAN_POINT('',(-7.19476400411325,-6.63753909988913,8.65788332730729));
#83328=CARTESIAN_POINT('Ctrl Pts',(-7.19476400411324,-6.63753909988912,
8.6578833273073));
#83329=CARTESIAN_POINT('Ctrl Pts',(-7.20793342429833,-6.25115677756972,
8.6350732224405));
#83330=CARTESIAN_POINT('Ctrl Pts',(-7.22957597298833,-5.92703963684568,
8.59758722850414));
#83331=CARTESIAN_POINT('Ctrl Pts',(-7.33264605094298,-5.48248933517018,
8.4190646167466));
#83332=CARTESIAN_POINT('Ctrl Pts',(-7.38587885165345,-5.33005160890817,
8.32686270128687));
#83333=CARTESIAN_POINT('Ctrl Pts',(-7.55351534711913,-5.02205392516935,
8.03650777393752));
#83334=CARTESIAN_POINT('Ctrl Pts',(-7.68241549558843,-4.85741613145636,
7.81324616768553));
#83335=CARTESIAN_POINT('Ctrl Pts',(-8.0780580468698,-4.55925658398769,7.12797316723002));
#83336=CARTESIAN_POINT('Ctrl Pts',(-8.29873608204807,-4.4610264457769,6.74574759818678));
#83337=CARTESIAN_POINT('Ctrl Pts',(-8.61875324812282,-4.36808225563914,
6.19146160725111));
#83338=CARTESIAN_POINT('Ctrl Pts',(-8.73033406055842,-4.34507072735131,
5.99819797096284));
#83339=CARTESIAN_POINT('Ctrl Pts',(-8.89953062521159,-4.32271936364378,
5.70514092451745));
#83340=CARTESIAN_POINT('Ctrl Pts',(-8.95774725247859,-4.31728665962078,
5.60430676824569));
#83341=CARTESIAN_POINT('Ctrl Pts',(-9.05873727376953,-4.31167125033784,
5.42938692031232));
#83342=CARTESIAN_POINT('Ctrl Pts',(-9.10160080381226,-4.31047752426154,
5.35514510848656));
#83343=CARTESIAN_POINT('Ctrl Pts',(-9.18843216468573,-4.31045476730958,
5.20474877976337));
#83344=CARTESIAN_POINT('Ctrl Pts',(-9.23245827883183,-4.31169063776259,
5.12849331320241));
#83345=CARTESIAN_POINT('Ctrl Pts',(-9.33992086438237,-4.31777109093092,
4.94236265511615));
#83346=CARTESIAN_POINT('Ctrl Pts',(-9.40346807156986,-4.32398244074387,
4.8322956635884));
#83347=CARTESIAN_POINT('Ctrl Pts',(-9.59164397495291,-4.35037319724938,
4.5063654381688));
#83348=CARTESIAN_POINT('Ctrl Pts',(-9.71718683007748,-4.37846636964579,
4.28891883456579));
#83349=CARTESIAN_POINT('Ctrl Pts',(-10.0959505184891,-4.50027701908412,
3.6328808821747));
#83350=CARTESIAN_POINT('Ctrl Pts',(-10.3416323810422,-4.63190537710756,
3.20734741373457));
#83351=CARTESIAN_POINT('Ctrl Pts',(-10.7018033055645,-4.9692390378482,2.58351307305293));
#83352=CARTESIAN_POINT('Ctrl Pts',(-10.8039037926249,-5.13032755417158,
2.40666984198668));
#83353=CARTESIAN_POINT('Ctrl Pts',(-10.9344613444127,-5.41302767928393,
2.18053752897839));
#83354=CARTESIAN_POINT('Ctrl Pts',(-10.9804393462863,-5.56176401030116,
2.10090129370282));
#83355=CARTESIAN_POINT('Ctrl Pts',(-11.0647640875135,-5.99351761929468,
1.95484655756219));
#83356=CARTESIAN_POINT('Ctrl Pts',(-11.0834813101589,-6.28993823923336,
1.92242737696384));
#83357=CARTESIAN_POINT('Ctrl Pts',(-11.0953289065065,-6.63753909988913,
1.90190673814229));
#83358=CARTESIAN_POINT('',(-3.90056490239319,-6.63753909988913,10.5597900654496));
#83359=CARTESIAN_POINT('Origin',(0.,-6.63753909988913,0.));
#83360=CARTESIAN_POINT('',(3.90056490239326,-6.63753909988913,10.5597900654496));
#83361=CARTESIAN_POINT('Ctrl Pts',(3.90056490239325,-6.63753909988913,10.5597900654496));
#83362=CARTESIAN_POINT('Ctrl Pts',(3.88650640714011,-6.43130549325031,10.5597900654496));
#83363=CARTESIAN_POINT('Ctrl Pts',(3.86750921833427,-6.24077478304519,10.5597900654496));
#83364=CARTESIAN_POINT('Ctrl Pts',(3.79603527122585,-5.88328867547875,10.5597900654496));
#83365=CARTESIAN_POINT('Ctrl Pts',(3.74111739908575,-5.70969285765482,10.5597900656594));
#83366=CARTESIAN_POINT('Ctrl Pts',(3.56226471943089,-5.38996752638001,10.5597900656594));
#83367=CARTESIAN_POINT('Ctrl Pts',(3.43858592823323,-5.23989257637326,10.5597900654496));
#83368=CARTESIAN_POINT('Ctrl Pts',(2.92900810424278,-4.84096372109964,10.5597900654496));
#83369=CARTESIAN_POINT('Ctrl Pts',(2.50413756504136,-4.6858650511529,10.5597900654496));
#83370=CARTESIAN_POINT('Ctrl Pts',(1.80048019244854,-4.48301709563196,10.5597900654496));
#83371=CARTESIAN_POINT('Ctrl Pts',(1.40703076126875,-4.41160065323694,10.5597900654496));
#83372=CARTESIAN_POINT('Ctrl Pts',(0.841933717031905,-4.34702984071186,
10.5597900654496));
#83373=CARTESIAN_POINT('Ctrl Pts',(0.658043722812898,-4.33203279124676,
10.5597900654496));
#83374=CARTESIAN_POINT('Ctrl Pts',(0.382154538654409,-4.31786065829337,
10.5597900654496));
#83375=CARTESIAN_POINT('Ctrl Pts',(0.289586349001999,-4.31451406956158,
10.5597900654496));
#83376=CARTESIAN_POINT('Ctrl Pts',(0.131799833370187,-4.31116993398485,
10.5597900654496));
#83377=CARTESIAN_POINT('Ctrl Pts',(0.0664976322661047,-4.31047485185275,
10.5597900654496));
#83378=CARTESIAN_POINT('Ctrl Pts',(-0.0639173571933893,-4.31045776213067,
10.5597900654496));
#83379=CARTESIAN_POINT('Ctrl Pts',(-0.129079361026244,-4.31113280201933,
10.5597900654496));
#83380=CARTESIAN_POINT('Ctrl Pts',(-0.286057044143298,-4.31441138123185,
10.5597900654496));
#83381=CARTESIAN_POINT('Ctrl Pts',(-0.377955322537848,-4.31769531886315,
10.5597900654496));
#83382=CARTESIAN_POINT('Ctrl Pts',(-0.651486594053972,-4.33160004901355,
10.5597900654496));
#83383=CARTESIAN_POINT('Ctrl Pts',(-0.833670646936046,-4.34630752826427,
10.5597900654496));
#83384=CARTESIAN_POINT('Ctrl Pts',(-1.3930903593616,-4.40956151168579,10.5597900654496));
#83385=CARTESIAN_POINT('Ctrl Pts',(-1.78195277809543,-4.47937544741227,
10.5597900654496));
#83386=CARTESIAN_POINT('Ctrl Pts',(-2.48599710360177,-4.67915031046562,
10.5597900654496));
#83387=CARTESIAN_POINT('Ctrl Pts',(-2.91820462596571,-4.83459622286678,
10.5597900654496));
#83388=CARTESIAN_POINT('Ctrl Pts',(-3.43432853419096,-5.23545667439743,
10.5597900654496));
#83389=CARTESIAN_POINT('Ctrl Pts',(-3.55892444433017,-5.38544981580468,
10.5597900657021));
#83390=CARTESIAN_POINT('Ctrl Pts',(-3.73882514968007,-5.70415223222546,
10.5597900657021));
#83391=CARTESIAN_POINT('Ctrl Pts',(-3.79423029833334,-5.87690202689054,
10.5597900654496));
#83392=CARTESIAN_POINT('Ctrl Pts',(-3.86701620951239,-6.23579968922602,
10.5597900654496));
#83393=CARTESIAN_POINT('Ctrl Pts',(-3.88632393679757,-6.42862871197633,
10.5597900654496));
#83394=CARTESIAN_POINT('Ctrl Pts',(-3.90056490239319,-6.63753909988913,
10.5597900654496));
#83395=CARTESIAN_POINT('',(7.1947640041133,-6.63753909988913,8.65788332730725));
#83396=CARTESIAN_POINT('Origin',(0.,-6.63753909988913,0.));
#83397=CARTESIAN_POINT('Ctrl Pts',(11.0953289065065,-6.63753909988913,1.90190673814222));
#83398=CARTESIAN_POINT('Ctrl Pts',(11.0835931462191,-6.29321943734551,1.92223367122543));
#83399=CARTESIAN_POINT('Ctrl Pts',(11.0651161129459,-5.99918609364608,1.95423683162777));
#83400=CARTESIAN_POINT('Ctrl Pts',(10.9824464115036,-5.56957898521084,2.09742495477241));
#83401=CARTESIAN_POINT('Ctrl Pts',(10.9371509020333,-5.42068513211763,2.17587907852961));
#83402=CARTESIAN_POINT('Ctrl Pts',(10.8075382554254,-5.13626438454726,2.40037476775806));
#83403=CARTESIAN_POINT('Ctrl Pts',(10.706766468623,-4.97635007968677,2.57491662246921));
#83404=CARTESIAN_POINT('Ctrl Pts',(10.3498218261676,-4.6366205362042,3.19316287869144));
#83405=CARTESIAN_POINT('Ctrl Pts',(10.102224520358,-4.50300238908698,3.62201399217098));
#83406=CARTESIAN_POINT('Ctrl Pts',(9.72143984871376,-4.37950172223957,4.2815523902022));
#83407=CARTESIAN_POINT('Ctrl Pts',(9.59502849226354,-4.3509924062512,4.50050328222767));
#83408=CARTESIAN_POINT('Ctrl Pts',(9.4056501266249,-4.32421736597006,4.82851623336816));
#83409=CARTESIAN_POINT('Ctrl Pts',(9.34174413003697,-4.31791520443557,4.93920466636667));
#83410=CARTESIAN_POINT('Ctrl Pts',(9.23384225124111,-4.3117414707732,5.12609620267325));
#83411=CARTESIAN_POINT('Ctrl Pts',(9.18973415909192,-4.31047784978131,5.20249365930066));
#83412=CARTESIAN_POINT('Ctrl Pts',(9.1028760836397,-4.31045508582793,5.35293625903157));
#83413=CARTESIAN_POINT('Ctrl Pts',(9.06006776325592,-4.31162331048586,5.42708244492296));
#83414=CARTESIAN_POINT('Ctrl Pts',(8.95941636902022,-4.31715957848669,5.60141577359183));
#83415=CARTESIAN_POINT('Ctrl Pts',(8.90148409311069,-4.32252007109623,5.70175741886524));
#83416=CARTESIAN_POINT('Ctrl Pts',(8.73325091212282,-4.34457631956746,5.99314583585518));
#83417=CARTESIAN_POINT('Ctrl Pts',(8.62236299560943,-4.36727979901887,6.18520934120182));
#83418=CARTESIAN_POINT('Ctrl Pts',(8.30433573130963,-4.45894533929482,6.73604872116122));
#83419=CARTESIAN_POINT('Ctrl Pts',(8.08539249003287,-4.55566580971443,7.11526953902639));
#83420=CARTESIAN_POINT('Ctrl Pts',(7.68947767855933,-4.85020226805387,7.80101410796761));
#83421=CARTESIAN_POINT('Ctrl Pts',(7.55829760823951,-5.01478805334236,8.02822465470201));
#83422=CARTESIAN_POINT('Ctrl Pts',(7.38777942464449,-5.32531557816686,8.32357081230295));
#83423=CARTESIAN_POINT('Ctrl Pts',(7.33403218269023,-5.47793756447169,8.41666376613443));
#83424=CARTESIAN_POINT('Ctrl Pts',(7.22979823884862,-5.92365652676787,8.59720225274137));
#83425=CARTESIAN_POINT('Ctrl Pts',(7.20800124955009,-6.24916682828626,8.63495574565847));
#83426=CARTESIAN_POINT('Ctrl Pts',(7.19476400411331,-6.63753909988913,8.65788332730724));
#83427=CARTESIAN_POINT('Origin',(0.,-14.6742356128,0.));
#83428=CARTESIAN_POINT('',(-8.34200437171315,-15.6742356128,-15.2699365768925));
#83429=CARTESIAN_POINT('',(-2.1308854305164E-15,-15.6742356128,17.4));
#83430=CARTESIAN_POINT('Origin',(0.,-15.6742356128,0.));
#83431=CARTESIAN_POINT('Origin',(0.,-15.6742356128,0.));
#83432=CARTESIAN_POINT('',(-2.00842075060166E-15,-14.6742356128,16.4));
#83433=CARTESIAN_POINT('',(-2.00842075060166E-15,-14.6742356128,16.4));
#83434=CARTESIAN_POINT('Origin',(0.,-14.6742356128,0.));
#83435=CARTESIAN_POINT('Origin',(0.,-18.0242356128,0.));
#83436=CARTESIAN_POINT('',(-2.0870381674,-16.6742356128,10.8001977615));
#83437=CARTESIAN_POINT('',(2.0870381674,-16.6742356128,10.8001977615));
#83438=CARTESIAN_POINT('Origin',(-5.49560397189452E-14,-16.6742356128,-4.21884749357559E-14));
#83439=CARTESIAN_POINT('',(2.08703816887115,-19.5762208096,10.800197769113));
#83440=CARTESIAN_POINT('',(2.0870381674,-18.0242356128,10.8001977615));
#83441=CARTESIAN_POINT('',(2.03267803765,-19.6742356128,10.8105605773));
#83442=CARTESIAN_POINT('Ctrl Pts',(2.08703816739882,-19.5762208096,10.8001977614939));
#83443=CARTESIAN_POINT('Ctrl Pts',(2.07857179402344,-19.5911991209122,10.8018331158543));
#83444=CARTESIAN_POINT('Ctrl Pts',(2.07030745035201,-19.605954198511,10.8034201368899));
#83445=CARTESIAN_POINT('Ctrl Pts',(2.0621770638366,-19.6206102877713,10.8049722242346));
#83446=CARTESIAN_POINT('Ctrl Pts',(2.05414457024727,-19.6350899121785,10.8065056238611));
#83447=CARTESIAN_POINT('Ctrl Pts',(2.04624300011735,-19.6494727516023,10.8080049411755));
#83448=CARTESIAN_POINT('Ctrl Pts',(2.03836798365886,-19.6638468112158,10.8094895879609));
#83449=CARTESIAN_POINT('Ctrl Pts',(2.03647058914484,-19.6673100753243,10.8098472965042));
#83450=CARTESIAN_POINT('Ctrl Pts',(2.03457454933455,-19.670772688533,10.8102041831093));
#83451=CARTESIAN_POINT('Ctrl Pts',(2.03267803765,-19.6742356128,10.8105605773));
#83452=CARTESIAN_POINT('',(2.03267803765,-20.5742356128,10.8105605773));
#83453=CARTESIAN_POINT('',(2.03267803765,-18.0242356128,10.8105605773));
#83454=CARTESIAN_POINT('',(-2.03267803765,-20.5742356128,10.8105605773));
#83455=CARTESIAN_POINT('Origin',(0.,-20.5742356128,0.));
#83456=CARTESIAN_POINT('',(-2.03267803765,-19.6742356128,10.8105605773));
#83457=CARTESIAN_POINT('',(-2.03267803765,-18.0242356128,10.8105605773));
#83458=CARTESIAN_POINT('',(-2.08703816887115,-19.5762208096,10.800197769113));
#83459=CARTESIAN_POINT('Ctrl Pts',(-2.08703816739882,-19.5762208096,10.8001977614939));
#83460=CARTESIAN_POINT('Ctrl Pts',(-2.07851836458347,-19.5912936327508,
10.8018434362202));
#83461=CARTESIAN_POINT('Ctrl Pts',(-2.07020057505286,-19.6061447702175,
10.803440661169));
#83462=CARTESIAN_POINT('Ctrl Pts',(-2.06201879505428,-19.6208943062105,
10.8050024359317));
#83463=CARTESIAN_POINT('Ctrl Pts',(-2.05455817949112,-19.6343437778167,
10.8064265516013));
#83464=CARTESIAN_POINT('Ctrl Pts',(-2.04721036756645,-19.6477083057653,
10.8078212728186));
#83465=CARTESIAN_POINT('Ctrl Pts',(-2.03989637952827,-19.6610552454502,
10.8092013212638));
#83466=CARTESIAN_POINT('Ctrl Pts',(-2.03748869684149,-19.6654489080366,
10.8096556177066));
#83467=CARTESIAN_POINT('Ctrl Pts',(-2.03508470198871,-19.6698411784241,
10.8101083147612));
#83468=CARTESIAN_POINT('Ctrl Pts',(-2.03267803765,-19.6742356128,10.8105605773));
#83469=CARTESIAN_POINT('',(-2.0870381674,-18.7742356128,10.8001977615));
#83470=CARTESIAN_POINT('Origin',(0.,-4.27423561284,11.15));
#83471=CARTESIAN_POINT('Origin',(0.,-4.27423561284,0.));
#83472=CARTESIAN_POINT('',(-4.38674367823,-4.27423561284,-8.0298804413));
#83473=CARTESIAN_POINT('Origin',(0.,-4.27423561284,0.));
#83474=CARTESIAN_POINT('Origin',(0.,-32.7742356128,2.4));
#83475=CARTESIAN_POINT('',(-16.2234398325,-32.7742356128,2.4));
#83476=CARTESIAN_POINT('',(-17.2336879396,-32.7742356128,2.4));
#83477=CARTESIAN_POINT('',(-16.7285638861,-32.7742356128,2.4));
#83478=CARTESIAN_POINT('',(-17.2336879396,-32.7742356128,-2.4));
#83479=CARTESIAN_POINT('Origin',(0.,-32.7742356128,0.));
#83480=CARTESIAN_POINT('',(-16.2234398325,-32.7742356128,-2.4));
#83481=CARTESIAN_POINT('',(-16.7285638861,-32.7742356128,-2.4));
#83482=CARTESIAN_POINT('Origin',(0.,-32.7742356128,0.));
#83483=CARTESIAN_POINT('Origin',(0.,-34.4742356128,-2.4));
#83484=CARTESIAN_POINT('',(-16.2234398325,-34.4742356128,-2.4));
#83485=CARTESIAN_POINT('',(-16.2234398325,-27.9742356128,-2.4));
#83486=CARTESIAN_POINT('',(-17.2336879396,-34.4742356128,-2.4));
#83487=CARTESIAN_POINT('',(-17.2336879396,-26.9742356128,-2.4));
#83488=CARTESIAN_POINT('',(-16.7285638861,-34.4742356128,-2.4));
#83489=CARTESIAN_POINT('Origin',(0.,-34.4742356128,2.4));
#83490=CARTESIAN_POINT('',(-16.2234398325,-34.4742356128,2.4));
#83491=CARTESIAN_POINT('',(-17.2336879396,-34.4742356128,2.4));
#83492=CARTESIAN_POINT('',(-16.7285638861,-34.4742356128,2.4));
#83493=CARTESIAN_POINT('',(-17.2336879396,-26.9742356128,2.4));
#83494=CARTESIAN_POINT('',(-16.2234398325,-27.9742356128,2.4));
#83495=CARTESIAN_POINT('Origin',(0.,-34.4742356128,-2.4));
#83496=CARTESIAN_POINT('Origin',(0.,-34.4742356128,0.));
#83497=CARTESIAN_POINT('Origin',(0.,-34.4742356128,0.));
#83498=CARTESIAN_POINT('Origin',(0.,-32.7742356128,2.4));
#83499=CARTESIAN_POINT('',(17.2336879396,-32.7742356128,-2.4));
#83500=CARTESIAN_POINT('',(16.2234398325,-32.7742356128,-2.4));
#83501=CARTESIAN_POINT('',(16.7285638861,-32.7742356128,-2.4));
#83502=CARTESIAN_POINT('',(17.2336879396,-32.7742356128,2.4));
#83503=CARTESIAN_POINT('Origin',(0.,-32.7742356128,0.));
#83504=CARTESIAN_POINT('',(16.2234398325,-32.7742356128,2.4));
#83505=CARTESIAN_POINT('',(16.7285638861,-32.7742356128,2.4));
#83506=CARTESIAN_POINT('Origin',(0.,-32.7742356128,0.));
#83507=CARTESIAN_POINT('Origin',(0.,-34.4742356128,2.4));
#83508=CARTESIAN_POINT('',(17.2336879396,-34.4742356128,2.4));
#83509=CARTESIAN_POINT('',(17.2336879396,-26.9742356128,2.4));
#83510=CARTESIAN_POINT('',(16.2234398325,-34.4742356128,2.4));
#83511=CARTESIAN_POINT('',(16.7285638861,-34.4742356128,2.4));
#83512=CARTESIAN_POINT('',(16.2234398325,-27.9742356128,2.4));
#83513=CARTESIAN_POINT('Origin',(0.,-34.4742356128,-2.4));
#83514=CARTESIAN_POINT('',(16.2234398325,-34.4742356128,-2.4));
#83515=CARTESIAN_POINT('',(16.2234398325,-27.9742356128,-2.4));
#83516=CARTESIAN_POINT('',(17.2336879396,-34.4742356128,-2.4));
#83517=CARTESIAN_POINT('',(16.7285638861,-34.4742356128,-2.4));
#83518=CARTESIAN_POINT('',(17.2336879396,-26.9742356128,-2.4));
#83519=CARTESIAN_POINT('Origin',(0.,-34.4742356128,-2.4));
#83520=CARTESIAN_POINT('Origin',(0.,-34.4742356128,0.));
#83521=CARTESIAN_POINT('Origin',(0.,-34.4742356128,0.));
#83522=CARTESIAN_POINT('Origin',(0.,-21.7742356128,0.));
#83523=CARTESIAN_POINT('',(-4.5,-39.2742356128,15.7705421594));
#83524=CARTESIAN_POINT('',(-7.86257883310895,-39.2742356128016,-14.3923540150021));
#83525=CARTESIAN_POINT('Origin',(0.,-39.2742356128,0.));
#83526=CARTESIAN_POINT('',(-7.86257883310895,-16.6742356128,-14.3923540150021));
#83527=CARTESIAN_POINT('',(-7.86257883310895,-21.7742356128,-14.3923540150021));
#83528=CARTESIAN_POINT('',(-15.9289440371,-16.6742356128,-3.90240206319));
#83529=CARTESIAN_POINT('Origin',(1.22124532708767E-14,-16.6742356128,-4.44089209850063E-15));
#83530=CARTESIAN_POINT('',(-15.9289440371,-19.3742356128,-3.90240206319));
#83531=CARTESIAN_POINT('',(-15.9289440371,-18.0242356128,-3.90240206319));
#83532=CARTESIAN_POINT('',(-16.2336455538,-19.3742356128,-2.32996824702));
#83533=CARTESIAN_POINT('Origin',(0.,-19.3742356128,0.));
#83534=CARTESIAN_POINT('',(-16.2336455538,-16.6742356128,-2.32996824702));
#83535=CARTESIAN_POINT('',(-16.2336455538,-18.0242356128,-2.32996824702));
#83536=CARTESIAN_POINT('',(-16.2336455538,-16.6742356128,2.32996824702));
#83537=CARTESIAN_POINT('Origin',(3.5527136788005E-14,-16.6742356128,-2.91433543964104E-14));
#83538=CARTESIAN_POINT('',(-16.2336455538,-19.3742356128,2.32996824702));
#83539=CARTESIAN_POINT('',(-16.2336455538,-18.0242356128,2.32996824702));
#83540=CARTESIAN_POINT('',(-15.9289440371,-19.3742356128,3.90240206319));
#83541=CARTESIAN_POINT('Origin',(0.,-19.3742356128,0.));
#83542=CARTESIAN_POINT('',(-15.9289440371,-16.6742356128,3.90240206319));
#83543=CARTESIAN_POINT('',(-15.9289440371,-18.0242356128,3.90240206319));
#83544=CARTESIAN_POINT('',(-7.49224433422,-16.6742356128,14.5885665792));
#83545=CARTESIAN_POINT('Origin',(-8.88178419700125E-15,-16.6742356128,3.44169137633799E-14));
#83546=CARTESIAN_POINT('',(-7.49224433422,-19.0742356128,14.5885665792));
#83547=CARTESIAN_POINT('',(-7.49224433422,-17.8742356128,14.5885665792));
#83548=CARTESIAN_POINT('',(-7.19123109516,-19.3742356128,14.739273908));
#83549=CARTESIAN_POINT('Ctrl Pts',(-7.19123109512951,-19.3742356128,14.7392739080473));
#83550=CARTESIAN_POINT('Ctrl Pts',(-7.22952132866876,-19.3742356127946,
14.7205922606481));
#83551=CARTESIAN_POINT('Ctrl Pts',(-7.27057773529867,-19.3666953834606,
14.7003573162235));
#83552=CARTESIAN_POINT('Ctrl Pts',(-7.34666159172428,-19.3348937450062,
14.6624816891679));
#83553=CARTESIAN_POINT('Ctrl Pts',(-7.38168615217903,-19.3106128070347,
14.6448516028746));
#83554=CARTESIAN_POINT('Ctrl Pts',(-7.43385501333582,-19.2559632146065,
14.618431778239));
#83555=CARTESIAN_POINT('Ctrl Pts',(-7.45563951291232,-19.2234139907703,
14.6073169516831));
#83556=CARTESIAN_POINT('Ctrl Pts',(-7.48484529484258,-19.1512739974414,
14.5923733499151));
#83557=CARTESIAN_POINT('Ctrl Pts',(-7.4922443341904,-19.111669668748,14.5885665792357));
#83558=CARTESIAN_POINT('Ctrl Pts',(-7.4922443341904,-19.0742356128,14.5885665792357));
#83559=CARTESIAN_POINT('',(-6.24926904222,-19.3742356128,15.1626724702));
#83560=CARTESIAN_POINT('Origin',(0.,-19.3742356128,0.));
#83561=CARTESIAN_POINT('',(-5.92151655781,-19.0742356128,15.2936471012));
#83562=CARTESIAN_POINT('Ctrl Pts',(-5.92151655783295,-19.0742356128,15.293647101176));
#83563=CARTESIAN_POINT('Ctrl Pts',(-5.92151655783295,-19.1116715424785,
15.293647101176));
#83564=CARTESIAN_POINT('Ctrl Pts',(-5.92976192802622,-19.1510542471533,
15.2904615732935));
#83565=CARTESIAN_POINT('Ctrl Pts',(-5.96159367196029,-19.2224116359375,
15.2780788235699));
#83566=CARTESIAN_POINT('Ctrl Pts',(-5.98511656924299,-19.2544169262194,
15.2688949021608));
#83567=CARTESIAN_POINT('Ctrl Pts',(-6.04180004067785,-19.309437956177,15.2465652051803));
#83568=CARTESIAN_POINT('Ctrl Pts',(-6.08040370020595,-19.3341462543713,
15.2312408052802));
#83569=CARTESIAN_POINT('Ctrl Pts',(-6.16349766956827,-19.3665421888705,
15.1978058318927));
#83570=CARTESIAN_POINT('Ctrl Pts',(-6.20798298226436,-19.3742356128,15.1796884478622));
#83571=CARTESIAN_POINT('Ctrl Pts',(-6.24926904224182,-19.3742356128,15.1626724701709));
#83572=CARTESIAN_POINT('',(-5.92151655781,-16.6742356128,15.2936471012));
#83573=CARTESIAN_POINT('',(-5.92151655781,-18.0242356128,15.2936471012));
#83574=CARTESIAN_POINT('',(-1.02442996075,-16.6742356128,16.3679730955));
#83575=CARTESIAN_POINT('Origin',(-1.18793863634892E-13,-16.6742356128,3.99680288865056E-14));
#83576=CARTESIAN_POINT('',(-1.02442996075,-20.5742356128,16.3679730955));
#83577=CARTESIAN_POINT('',(-1.02442996075,-18.7742356128,16.3679730955));
#83578=CARTESIAN_POINT('',(-0.703933081317,-20.8742356128,16.3848856638));
#83579=CARTESIAN_POINT('Ctrl Pts',(-0.703933081313263,-20.8742356128,16.3848856638377));
#83580=CARTESIAN_POINT('Ctrl Pts',(-0.74430255434404,-20.8742356127994,
16.3831512966822));
#83581=CARTESIAN_POINT('Ctrl Pts',(-0.787517237531629,-20.8666318008058,
16.3811299589766));
#83582=CARTESIAN_POINT('Ctrl Pts',(-0.867468556859285,-20.8352672300064,
16.377090719509));
#83583=CARTESIAN_POINT('Ctrl Pts',(-0.904202386296281,-20.8114982977688,
16.3750807377873));
#83584=CARTESIAN_POINT('Ctrl Pts',(-0.96040637329737,-20.7575520580267,
16.371876958888));
#83585=CARTESIAN_POINT('Ctrl Pts',(-0.984367443611667,-20.7245301270092,
16.3704391530226));
#83586=CARTESIAN_POINT('Ctrl Pts',(-1.01639053666175,-20.6516587395374,
16.3684821411247));
#83587=CARTESIAN_POINT('Ctrl Pts',(-1.02442996074781,-20.6117990817782,
16.3679730955156));
#83588=CARTESIAN_POINT('Ctrl Pts',(-1.02442996074781,-20.5742356128,16.3679730955156));
#83589=CARTESIAN_POINT('',(0.703933081317,-20.8742356128,16.3848856638));
#83590=CARTESIAN_POINT('Origin',(0.,-20.8742356128,0.));
#83591=CARTESIAN_POINT('',(1.02442996075,-20.5742356128,16.3679730955));
#83592=CARTESIAN_POINT('Ctrl Pts',(0.703933081313263,-20.8742356128,16.3848856638377));
#83593=CARTESIAN_POINT('Ctrl Pts',(0.74430255434404,-20.8742356127994,16.3831512966822));
#83594=CARTESIAN_POINT('Ctrl Pts',(0.787517237531627,-20.8666318008058,
16.3811299589766));
#83595=CARTESIAN_POINT('Ctrl Pts',(0.867468556859283,-20.8352672300064,
16.377090719509));
#83596=CARTESIAN_POINT('Ctrl Pts',(0.904202386296281,-20.8114982977688,
16.3750807377873));
#83597=CARTESIAN_POINT('Ctrl Pts',(0.96040637329737,-20.7575520580267,16.371876958888));
#83598=CARTESIAN_POINT('Ctrl Pts',(0.984367443611667,-20.7245301270092,
16.3704391530226));
#83599=CARTESIAN_POINT('Ctrl Pts',(1.01639053666175,-20.6516587395374,16.3684821411247));
#83600=CARTESIAN_POINT('Ctrl Pts',(1.02442996074781,-20.6117990817782,16.3679730955156));
#83601=CARTESIAN_POINT('Ctrl Pts',(1.02442996074781,-20.5742356128,16.3679730955156));
#83602=CARTESIAN_POINT('',(1.02442996075,-16.6742356128,16.3679730955));
#83603=CARTESIAN_POINT('',(1.02442996075,-18.7742356128,16.3679730955));
#83604=CARTESIAN_POINT('',(5.92151655781,-16.6742356128,15.2936471012));
#83605=CARTESIAN_POINT('Origin',(-1.0172418463128E-13,-16.6742356128,-8.21565038222616E-14));
#83606=CARTESIAN_POINT('',(5.92151655781,-19.0742356128,15.2936471012));
#83607=CARTESIAN_POINT('',(5.92151655781,-18.0242356128,15.2936471012));
#83608=CARTESIAN_POINT('',(6.24926904222,-19.3742356128,15.1626724702));
#83609=CARTESIAN_POINT('Ctrl Pts',(5.92151655783295,-19.0742356128,15.293647101176));
#83610=CARTESIAN_POINT('Ctrl Pts',(5.92151655783295,-19.1116715424785,15.293647101176));
#83611=CARTESIAN_POINT('Ctrl Pts',(5.92976192802622,-19.1510542471533,15.2904615732935));
#83612=CARTESIAN_POINT('Ctrl Pts',(5.96159367196029,-19.2224116359375,15.2780788235699));
#83613=CARTESIAN_POINT('Ctrl Pts',(5.985116569243,-19.2544169262194,15.2688949021608));
#83614=CARTESIAN_POINT('Ctrl Pts',(6.04180004067786,-19.309437956177,15.2465652051803));
#83615=CARTESIAN_POINT('Ctrl Pts',(6.08040370020595,-19.3341462543713,15.2312408052802));
#83616=CARTESIAN_POINT('Ctrl Pts',(6.16349766956827,-19.3665421888705,15.1978058318927));
#83617=CARTESIAN_POINT('Ctrl Pts',(6.20798298226436,-19.3742356128,15.1796884478622));
#83618=CARTESIAN_POINT('Ctrl Pts',(6.24926904224182,-19.3742356128,15.1626724701709));
#83619=CARTESIAN_POINT('',(7.19123109516,-19.3742356128,14.739273908));
#83620=CARTESIAN_POINT('Origin',(0.,-19.3742356128,0.));
#83621=CARTESIAN_POINT('',(7.49224433422,-19.0742356128,14.5885665792));
#83622=CARTESIAN_POINT('Ctrl Pts',(7.19123109512951,-19.3742356128,14.7392739080473));
#83623=CARTESIAN_POINT('Ctrl Pts',(7.22952132866876,-19.3742356127946,14.7205922606481));
#83624=CARTESIAN_POINT('Ctrl Pts',(7.27057773529867,-19.3666953834606,14.7003573162235));
#83625=CARTESIAN_POINT('Ctrl Pts',(7.34666159172428,-19.3348937450062,14.6624816891679));
#83626=CARTESIAN_POINT('Ctrl Pts',(7.38168615217903,-19.3106128070347,14.6448516028746));
#83627=CARTESIAN_POINT('Ctrl Pts',(7.43385501333582,-19.2559632146065,14.618431778239));
#83628=CARTESIAN_POINT('Ctrl Pts',(7.45563951291232,-19.2234139907703,14.6073169516831));
#83629=CARTESIAN_POINT('Ctrl Pts',(7.48484529484258,-19.1512739974414,14.5923733499151));
#83630=CARTESIAN_POINT('Ctrl Pts',(7.4922443341904,-19.111669668748,14.5885665792357));
#83631=CARTESIAN_POINT('Ctrl Pts',(7.4922443341904,-19.0742356128,14.5885665792357));
#83632=CARTESIAN_POINT('',(7.49224433422,-16.6742356128,14.5885665792));
#83633=CARTESIAN_POINT('',(7.49224433422,-17.8742356128,14.5885665792));
#83634=CARTESIAN_POINT('',(15.9289440371,-16.6742356128,3.90240206319));
#83635=CARTESIAN_POINT('Origin',(5.36126698591488E-12,-16.6742356128,1.11088915843993E-11));
#83636=CARTESIAN_POINT('',(15.9289440371,-19.3742356128,3.90240206319));
#83637=CARTESIAN_POINT('',(15.9289440371,-18.0242356128,3.90240206319));
#83638=CARTESIAN_POINT('',(16.2336455538,-19.3742356128,2.32996824702));
#83639=CARTESIAN_POINT('Origin',(0.,-19.3742356128,0.));
#83640=CARTESIAN_POINT('',(16.2336455538,-16.6742356128,2.32996824702));
#83641=CARTESIAN_POINT('',(16.2336455538,-18.0242356128,2.32996824702));
#83642=CARTESIAN_POINT('',(16.2336455538,-16.6742356128,-2.32996824702));
#83643=CARTESIAN_POINT('Origin',(1.90958360235527E-13,-16.6742356128,5.16253706450698E-14));
#83644=CARTESIAN_POINT('',(16.2336455538,-19.3742356128,-2.32996824702));
#83645=CARTESIAN_POINT('',(16.2336455538,-18.0242356128,-2.32996824702));
#83646=CARTESIAN_POINT('',(15.9289440371,-19.3742356128,-3.90240206319));
#83647=CARTESIAN_POINT('Origin',(0.,-19.3742356128,0.));
#83648=CARTESIAN_POINT('',(15.9289440371,-16.6742356128,-3.90240206319));
#83649=CARTESIAN_POINT('',(15.9289440371,-18.0242356128,-3.90240206319));
#83650=CARTESIAN_POINT('Origin',(1.22124532708767E-14,-16.6742356128,-4.44089209850063E-15));
#83651=CARTESIAN_POINT('',(-5.5,-39.2742356128,-15.4502427165));
#83652=CARTESIAN_POINT('Origin',(0.,-39.2742356128,0.));
#83653=CARTESIAN_POINT('',(-5.,-38.7742356128,-15.6192189305));
#83654=CARTESIAN_POINT('Ctrl Pts',(-5.,-38.7742356128,-15.6192189305355));
#83655=CARTESIAN_POINT('Ctrl Pts',(-5.,-38.8368018315904,-15.6192189305355));
#83656=CARTESIAN_POINT('Ctrl Pts',(-5.01248103067696,-38.9033171525403,
-15.6152401633624));
#83657=CARTESIAN_POINT('Ctrl Pts',(-5.06252926091632,-39.0251462300073,
-15.5990861568434));
#83658=CARTESIAN_POINT('Ctrl Pts',(-5.10007609417628,-39.0804660078343,
-15.5868932416425));
#83659=CARTESIAN_POINT('Ctrl Pts',(-5.18809492268901,-39.1703688520033,
-15.5578261400603));
#83660=CARTESIAN_POINT('Ctrl Pts',(-5.24538280864814,-39.2098107413741,
-15.5386709530016));
#83661=CARTESIAN_POINT('Ctrl Pts',(-5.3699886467473,-39.2617319238639,-15.4960497459829));
#83662=CARTESIAN_POINT('Ctrl Pts',(-5.43729042387462,-39.2742356128,-15.4725661631692));
#83663=CARTESIAN_POINT('Ctrl Pts',(-5.5,-39.2742356128,-15.4502427165401));
#83664=CARTESIAN_POINT('',(-5.,-35.2742356128,-15.6192189305));
#83665=CARTESIAN_POINT('',(-5.,-37.0242356128,-15.6192189305));
#83666=CARTESIAN_POINT('',(-4.,-34.2742356128,-15.9047162817));
#83667=CARTESIAN_POINT('Ctrl Pts',(-5.,-35.2742356128,-15.6192189305355));
#83668=CARTESIAN_POINT('Ctrl Pts',(-5.,-35.1487422268978,-15.6192189305355));
#83669=CARTESIAN_POINT('Ctrl Pts',(-4.97490968370107,-35.0153658897602,
-15.6273177607417));
#83670=CARTESIAN_POINT('Ctrl Pts',(-4.87420273104728,-34.7710139518027,
-15.6590208655925));
#83671=CARTESIAN_POINT('Ctrl Pts',(-4.79862638132674,-34.6600074810144,
-15.6825150669345));
#83672=CARTESIAN_POINT('Ctrl Pts',(-4.62282043142789,-34.4815119728997,
-15.7352562259596));
#83673=CARTESIAN_POINT('Ctrl Pts',(-4.50949514531374,-34.4033230413762,
-15.7683552560566));
#83674=CARTESIAN_POINT('Ctrl Pts',(-4.26139179450132,-34.2996852813123,
-15.837206632462));
#83675=CARTESIAN_POINT('Ctrl Pts',(-4.126591817014,-34.2742356128,-15.8728787273686));
#83676=CARTESIAN_POINT('Ctrl Pts',(-4.,-34.2742356128,-15.9047162816568));
#83677=CARTESIAN_POINT('',(4.,-34.2742356128,-15.9047162817));
#83678=CARTESIAN_POINT('Origin',(0.,-34.2742356128,0.));
#83679=CARTESIAN_POINT('',(5.,-35.2742356128,-15.6192189305));
#83680=CARTESIAN_POINT('Ctrl Pts',(4.,-34.2742356128,-15.9047162816568));
#83681=CARTESIAN_POINT('Ctrl Pts',(4.12659181701402,-34.2742356127987,-15.8728787273687));
#83682=CARTESIAN_POINT('Ctrl Pts',(4.26139179450132,-34.2996852813123,-15.837206632462));
#83683=CARTESIAN_POINT('Ctrl Pts',(4.50949514531374,-34.4033230413762,-15.7683552560566));
#83684=CARTESIAN_POINT('Ctrl Pts',(4.62282043142789,-34.4815119728997,-15.7352562259596));
#83685=CARTESIAN_POINT('Ctrl Pts',(4.79862638132674,-34.6600074810144,-15.6825150669345));
#83686=CARTESIAN_POINT('Ctrl Pts',(4.87420273104728,-34.7710139518027,-15.6590208655925));
#83687=CARTESIAN_POINT('Ctrl Pts',(4.97490968370107,-35.0153658897602,-15.6273177607417));
#83688=CARTESIAN_POINT('Ctrl Pts',(5.,-35.1487422268978,-15.6192189305355));
#83689=CARTESIAN_POINT('Ctrl Pts',(5.,-35.2742356128,-15.6192189305355));
#83690=CARTESIAN_POINT('',(5.,-38.7742356128,-15.6192189305));
#83691=CARTESIAN_POINT('',(5.,-37.0242356128,-15.6192189305));
#83692=CARTESIAN_POINT('',(5.5,-39.2742356128,-15.4502427165));
#83693=CARTESIAN_POINT('Ctrl Pts',(5.5,-39.2742356128,-15.4502427165401));
#83694=CARTESIAN_POINT('Ctrl Pts',(5.43729042387464,-39.2742356128016,-15.4725661631693));
#83695=CARTESIAN_POINT('Ctrl Pts',(5.3699886467473,-39.2617319238639,-15.4960497459829));
#83696=CARTESIAN_POINT('Ctrl Pts',(5.24538280864814,-39.2098107413741,-15.5386709530016));
#83697=CARTESIAN_POINT('Ctrl Pts',(5.18809492268901,-39.1703688520033,-15.5578261400603));
#83698=CARTESIAN_POINT('Ctrl Pts',(5.10007609417628,-39.0804660078343,-15.5868932416425));
#83699=CARTESIAN_POINT('Ctrl Pts',(5.06252926091632,-39.0251462300073,-15.5990861568434));
#83700=CARTESIAN_POINT('Ctrl Pts',(5.01248103067696,-38.9033171525403,-15.6152401633624));
#83701=CARTESIAN_POINT('Ctrl Pts',(5.,-38.8368018315904,-15.6192189305355));
#83702=CARTESIAN_POINT('Ctrl Pts',(5.,-38.7742356128,-15.6192189305355));
#83703=CARTESIAN_POINT('',(4.5,-39.2742356128,15.7705421594));
#83704=CARTESIAN_POINT('Origin',(0.,-39.2742356128,0.));
#83705=CARTESIAN_POINT('',(4.,-38.7742356128,15.9047162817));
#83706=CARTESIAN_POINT('Ctrl Pts',(4.,-38.7742356128,15.9047162816568));
#83707=CARTESIAN_POINT('Ctrl Pts',(4.,-38.836872188068,15.9047162816568));
#83708=CARTESIAN_POINT('Ctrl Pts',(4.01250244639384,-38.9035481102566,15.9015879733306));
#83709=CARTESIAN_POINT('Ctrl Pts',(4.06290022618683,-39.0258690198089,15.8887859105305));
#83710=CARTESIAN_POINT('Ctrl Pts',(4.10078344949377,-39.0815169257637,15.8790923795176));
#83711=CARTESIAN_POINT('Ctrl Pts',(4.18908794953576,-39.1710308075913,15.8560306789731));
#83712=CARTESIAN_POINT('Ctrl Pts',(4.24601666452162,-39.2101357988612,15.8409431205528));
#83713=CARTESIAN_POINT('Ctrl Pts',(4.37012998316081,-39.2617294942499,15.8071534564237));
#83714=CARTESIAN_POINT('Ctrl Pts',(4.43730220859644,-39.2742356128,15.7884324803388));
#83715=CARTESIAN_POINT('Ctrl Pts',(4.5,-39.2742356128,15.7705421593552));
#83716=CARTESIAN_POINT('',(4.,-35.2742356128,15.9047162817));
#83717=CARTESIAN_POINT('',(4.,-36.7742356128,15.9047162817));
#83718=CARTESIAN_POINT('',(3.,-34.2742356128,16.1232751015));
#83719=CARTESIAN_POINT('Ctrl Pts',(4.,-35.2742356128,15.9047162816568));
#83720=CARTESIAN_POINT('Ctrl Pts',(4.,-35.1486858517753,15.9047162816568));
#83721=CARTESIAN_POINT('Ctrl Pts',(3.97489679058695,-35.0150679349663,15.9110940851556));
#83722=CARTESIAN_POINT('Ctrl Pts',(3.87362953483757,-34.7698913888191,15.9360507557735));
#83723=CARTESIAN_POINT('Ctrl Pts',(3.79749048511181,-34.6583124843852,15.9545317615642));
#83724=CARTESIAN_POINT('Ctrl Pts',(3.62103634952688,-34.4802687438727,15.9955146214762));
#83725=CARTESIAN_POINT('Ctrl Pts',(3.50813186616486,-34.4025975216227,16.0208922692526));
#83726=CARTESIAN_POINT('Ctrl Pts',(3.26076324768218,-34.2995800372216,16.0730644662099));
#83727=CARTESIAN_POINT('Ctrl Pts',(3.12628134821427,-34.2742356128,16.0997783837685));
#83728=CARTESIAN_POINT('Ctrl Pts',(3.,-34.2742356128,16.1232751015419));
#83729=CARTESIAN_POINT('',(-3.,-34.2742356128,16.1232751015));
#83730=CARTESIAN_POINT('Origin',(0.,-34.2742356128,0.));
#83731=CARTESIAN_POINT('',(-4.,-35.2742356128,15.9047162817));
#83732=CARTESIAN_POINT('Ctrl Pts',(-3.,-34.2742356128,16.1232751015419));
#83733=CARTESIAN_POINT('Ctrl Pts',(-3.12628134821426,-34.274235612801,16.0997783837685));
#83734=CARTESIAN_POINT('Ctrl Pts',(-3.26076324768218,-34.2995800372216,
16.0730644662099));
#83735=CARTESIAN_POINT('Ctrl Pts',(-3.50813186616486,-34.4025975216227,
16.0208922692526));
#83736=CARTESIAN_POINT('Ctrl Pts',(-3.62103634952688,-34.4802687438727,
15.9955146214762));
#83737=CARTESIAN_POINT('Ctrl Pts',(-3.79749048511181,-34.6583124843852,
15.9545317615642));
#83738=CARTESIAN_POINT('Ctrl Pts',(-3.87362953483757,-34.7698913888191,
15.9360507557735));
#83739=CARTESIAN_POINT('Ctrl Pts',(-3.97489679058695,-35.0150679349663,
15.9110940851556));
#83740=CARTESIAN_POINT('Ctrl Pts',(-4.,-35.1486858517753,15.9047162816568));
#83741=CARTESIAN_POINT('Ctrl Pts',(-4.,-35.2742356128,15.9047162816568));
#83742=CARTESIAN_POINT('',(-4.,-38.7742356128,15.9047162817));
#83743=CARTESIAN_POINT('',(-4.,-36.7742356128,15.9047162817));
#83744=CARTESIAN_POINT('Ctrl Pts',(-4.5,-39.2742356128,15.7705421593552));
#83745=CARTESIAN_POINT('Ctrl Pts',(-4.43730220859643,-39.2742356127985,
15.7884324803387));
#83746=CARTESIAN_POINT('Ctrl Pts',(-4.37012998316081,-39.2617294942499,
15.8071534564237));
#83747=CARTESIAN_POINT('Ctrl Pts',(-4.24601666452162,-39.2101357988612,
15.8409431205528));
#83748=CARTESIAN_POINT('Ctrl Pts',(-4.18908794953576,-39.1710308075913,
15.8560306789731));
#83749=CARTESIAN_POINT('Ctrl Pts',(-4.10078344949377,-39.0815169257637,
15.8790923795176));
#83750=CARTESIAN_POINT('Ctrl Pts',(-4.06290022618683,-39.0258690198089,
15.8887859105305));
#83751=CARTESIAN_POINT('Ctrl Pts',(-4.01250244639384,-38.9035481102566,
15.9015879733306));
#83752=CARTESIAN_POINT('Ctrl Pts',(-4.,-38.836872188068,15.9047162816568));
#83753=CARTESIAN_POINT('Ctrl Pts',(-4.,-38.7742356128,15.9047162816568));
#83754=CARTESIAN_POINT('Origin',(0.,-21.7742356128,0.));
#83755=CARTESIAN_POINT('',(-8.34200437171315,-39.2742356128003,-15.2699365768925));
#83756=CARTESIAN_POINT('',(-8.34200437171315,-21.7742356128,-15.2699365768925));
#83757=CARTESIAN_POINT('',(-4.5,-39.2742356128,16.8080337934));
#83758=CARTESIAN_POINT('Origin',(0.,-39.2742356128,0.));
#83759=CARTESIAN_POINT('',(-4.,-38.7742356128,16.9339894886));
#83760=CARTESIAN_POINT('Ctrl Pts',(-4.,-38.7742356128,16.9339894885996));
#83761=CARTESIAN_POINT('Ctrl Pts',(-4.,-38.8368887914994,16.9339894885996));
#83762=CARTESIAN_POINT('Ctrl Pts',(-4.01250760002811,-38.903598396939,16.9310500506214));
#83763=CARTESIAN_POINT('Ctrl Pts',(-4.06297796817314,-39.0260198677362,
16.9190095185695));
#83764=CARTESIAN_POINT('Ctrl Pts',(-4.10093014199565,-39.0817342544231,
16.9098896615843));
#83765=CARTESIAN_POINT('Ctrl Pts',(-4.18928809817478,-39.1711621467437,
16.8882209976741));
#83766=CARTESIAN_POINT('Ctrl Pts',(-4.24613535186385,-39.2101954912713,
16.8740756815564));
#83767=CARTESIAN_POINT('Ctrl Pts',(-4.37014285930182,-39.2617244815659,
16.8423854285274));
#83768=CARTESIAN_POINT('Ctrl Pts',(-4.43729208625343,-39.2742356128,16.8248225276024));
#83769=CARTESIAN_POINT('Ctrl Pts',(-4.5,-39.2742356128,16.8080337933977));
#83770=CARTESIAN_POINT('',(-4.,-35.2742356128,16.9339894886));
#83771=CARTESIAN_POINT('',(-4.,-36.7742356128,16.9339894886));
#83772=CARTESIAN_POINT('',(-3.,-34.2742356128,17.1394282285));
#83773=CARTESIAN_POINT('Ctrl Pts',(-4.,-35.2742356128,16.9339894885996));
#83774=CARTESIAN_POINT('Ctrl Pts',(-4.,-35.1486855593285,16.9339894885996));
#83775=CARTESIAN_POINT('Ctrl Pts',(-3.97489818350414,-35.0150317313568,
16.9399790550091));
#83776=CARTESIAN_POINT('Ctrl Pts',(-3.87354117753779,-34.7697170783414,
16.9634425952617));
#83777=CARTESIAN_POINT('Ctrl Pts',(-3.79730805944039,-34.6580384861345,
16.9808260582146));
#83778=CARTESIAN_POINT('Ctrl Pts',(-3.6207263799214,-34.4800481242703,17.0193617118533));
#83779=CARTESIAN_POINT('Ctrl Pts',(-3.5078727043035,-34.4024577097155,17.0432013993171));
#83780=CARTESIAN_POINT('Ctrl Pts',(-3.26061624783525,-34.2995507541585,
17.0922282494331));
#83781=CARTESIAN_POINT('Ctrl Pts',(-3.12619777878762,-34.2742356128,17.1173391989672));
#83782=CARTESIAN_POINT('Ctrl Pts',(-3.,-34.2742356128,17.1394282285029));
#83783=CARTESIAN_POINT('',(3.,-34.2742356128,17.1394282285));
#83784=CARTESIAN_POINT('Origin',(0.,-34.2742356128,0.));
#83785=CARTESIAN_POINT('',(4.,-35.2742356128,16.9339894886));
#83786=CARTESIAN_POINT('Ctrl Pts',(3.,-34.2742356128,17.1394282285029));
#83787=CARTESIAN_POINT('Ctrl Pts',(3.12619777878762,-34.2742356128001,17.1173391989672));
#83788=CARTESIAN_POINT('Ctrl Pts',(3.26061624783525,-34.2995507541585,17.0922282494331));
#83789=CARTESIAN_POINT('Ctrl Pts',(3.5078727043035,-34.4024577097155,17.0432013993171));
#83790=CARTESIAN_POINT('Ctrl Pts',(3.6207263799214,-34.4800481242703,17.0193617118533));
#83791=CARTESIAN_POINT('Ctrl Pts',(3.79730805944039,-34.6580384861345,16.9808260582146));
#83792=CARTESIAN_POINT('Ctrl Pts',(3.87354117753779,-34.7697170783414,16.9634425952617));
#83793=CARTESIAN_POINT('Ctrl Pts',(3.97489818350414,-35.0150317313568,16.9399790550091));
#83794=CARTESIAN_POINT('Ctrl Pts',(4.,-35.1486855593285,16.9339894885996));
#83795=CARTESIAN_POINT('Ctrl Pts',(4.,-35.2742356128,16.9339894885996));
#83796=CARTESIAN_POINT('',(4.,-38.7742356128,16.9339894886));
#83797=CARTESIAN_POINT('',(4.,-36.7742356128,16.9339894886));
#83798=CARTESIAN_POINT('',(4.5,-39.2742356128,16.8080337934));
#83799=CARTESIAN_POINT('Ctrl Pts',(4.5,-39.2742356128,16.8080337933977));
#83800=CARTESIAN_POINT('Ctrl Pts',(4.43729208625343,-39.2742356127999,16.8248225276024));
#83801=CARTESIAN_POINT('Ctrl Pts',(4.37014285930182,-39.2617244815659,16.8423854285274));
#83802=CARTESIAN_POINT('Ctrl Pts',(4.24613535186385,-39.2101954912713,16.8740756815564));
#83803=CARTESIAN_POINT('Ctrl Pts',(4.18928809817478,-39.1711621467437,16.8882209976741));
#83804=CARTESIAN_POINT('Ctrl Pts',(4.10093014199565,-39.0817342544231,16.9098896615843));
#83805=CARTESIAN_POINT('Ctrl Pts',(4.06297796817314,-39.0260198677362,16.9190095185695));
#83806=CARTESIAN_POINT('Ctrl Pts',(4.0125076000281,-38.903598396939,16.9310500506214));
#83807=CARTESIAN_POINT('Ctrl Pts',(4.,-38.8368887914994,16.9339894885996));
#83808=CARTESIAN_POINT('Ctrl Pts',(4.,-38.7742356128,16.9339894885996));
#83809=CARTESIAN_POINT('',(5.5,-39.2742356128,-16.5078769077));
#83810=CARTESIAN_POINT('Origin',(0.,-39.2742356128,0.));
#83811=CARTESIAN_POINT('',(5.,-38.7742356128,-16.6661333248));
#83812=CARTESIAN_POINT('Ctrl Pts',(5.,-38.7742356128,-16.6661333247997));
#83813=CARTESIAN_POINT('Ctrl Pts',(5.,-38.8368267820667,-16.6661333247997));
#83814=CARTESIAN_POINT('Ctrl Pts',(5.01248880952419,-38.9033956100947,-16.6624020649352));
#83815=CARTESIAN_POINT('Ctrl Pts',(5.06265202735881,-39.0253853950253,-16.647229231688));
#83816=CARTESIAN_POINT('Ctrl Pts',(5.10030872977378,-39.0808115065366,-16.6357705740154));
#83817=CARTESIAN_POINT('Ctrl Pts',(5.18841286970923,-39.1705785286071,-16.6085103506913));
#83818=CARTESIAN_POINT('Ctrl Pts',(5.24557566629518,-39.2099085842528,-16.5906059126269));
#83819=CARTESIAN_POINT('Ctrl Pts',(5.37001700861689,-39.2617262283776,-16.5507457822022));
#83820=CARTESIAN_POINT('Ctrl Pts',(5.43728107900467,-39.2742356128,-16.5287732390402));
#83821=CARTESIAN_POINT('Ctrl Pts',(5.5,-39.2742356128,-16.5078769077068));
#83822=CARTESIAN_POINT('',(5.,-35.2742356128,-16.6661333248));
#83823=CARTESIAN_POINT('',(5.,-37.0242356128,-16.6661333248));
#83824=CARTESIAN_POINT('',(4.,-34.2742356128,-16.9339894886));
#83825=CARTESIAN_POINT('Ctrl Pts',(5.,-35.2742356128,-16.6661333247997));
#83826=CARTESIAN_POINT('Ctrl Pts',(5.,-35.1487369636031,-16.6661333247997));
#83827=CARTESIAN_POINT('Ctrl Pts',(4.97490998956982,-35.0152959233024,-16.6737229014171));
#83828=CARTESIAN_POINT('Ctrl Pts',(4.87404705295522,-34.7707070374517,-16.7034855674542));
#83829=CARTESIAN_POINT('Ctrl Pts',(4.79830954261467,-34.6595323663436,-16.7255581246326));
#83830=CARTESIAN_POINT('Ctrl Pts',(4.62229972372855,-34.481143286089,-16.7750706933282));
#83831=CARTESIAN_POINT('Ctrl Pts',(4.50907276305283,-34.403095624184,-16.8060902401953));
#83832=CARTESIAN_POINT('Ctrl Pts',(4.2611669496739,-34.299642472023,-16.8706509231256));
#83833=CARTESIAN_POINT('Ctrl Pts',(4.12646889394831,-34.2742356128,-16.9041161042955));
#83834=CARTESIAN_POINT('Ctrl Pts',(4.,-34.2742356128,-16.9339894885996));
#83835=CARTESIAN_POINT('',(-4.,-34.2742356128,-16.9339894886));
#83836=CARTESIAN_POINT('Origin',(0.,-34.2742356128,0.));
#83837=CARTESIAN_POINT('',(-5.,-35.2742356128,-16.6661333248));
#83838=CARTESIAN_POINT('Ctrl Pts',(-4.,-34.2742356128,-16.9339894885996));
#83839=CARTESIAN_POINT('Ctrl Pts',(-4.12646889394831,-34.2742356128,-16.9041161042955));
#83840=CARTESIAN_POINT('Ctrl Pts',(-4.26116694967389,-34.299642472023,-16.8706509231256));
#83841=CARTESIAN_POINT('Ctrl Pts',(-4.50907276305283,-34.403095624184,-16.8060902401953));
#83842=CARTESIAN_POINT('Ctrl Pts',(-4.62229972372855,-34.481143286089,-16.7750706933282));
#83843=CARTESIAN_POINT('Ctrl Pts',(-4.79830954261467,-34.6595323663436,
-16.7255581246326));
#83844=CARTESIAN_POINT('Ctrl Pts',(-4.87404705295522,-34.7707070374517,
-16.7034855674542));
#83845=CARTESIAN_POINT('Ctrl Pts',(-4.97490998956982,-35.0152959233024,
-16.6737229014171));
#83846=CARTESIAN_POINT('Ctrl Pts',(-5.,-35.1487369636031,-16.6661333247997));
#83847=CARTESIAN_POINT('Ctrl Pts',(-5.,-35.2742356128,-16.6661333247997));
#83848=CARTESIAN_POINT('',(-5.,-38.7742356128,-16.6661333248));
#83849=CARTESIAN_POINT('',(-5.,-37.0242356128,-16.6661333248));
#83850=CARTESIAN_POINT('',(-5.5,-39.2742356128,-16.5078769077));
#83851=CARTESIAN_POINT('Ctrl Pts',(-5.5,-39.2742356128,-16.5078769077068));
#83852=CARTESIAN_POINT('Ctrl Pts',(-5.43728107900467,-39.2742356128003,
-16.5287732390402));
#83853=CARTESIAN_POINT('Ctrl Pts',(-5.37001700861689,-39.2617262283776,
-16.5507457822022));
#83854=CARTESIAN_POINT('Ctrl Pts',(-5.24557566629518,-39.2099085842528,
-16.5906059126269));
#83855=CARTESIAN_POINT('Ctrl Pts',(-5.18841286970923,-39.1705785286071,
-16.6085103506913));
#83856=CARTESIAN_POINT('Ctrl Pts',(-5.10030872977378,-39.0808115065366,
-16.6357705740154));
#83857=CARTESIAN_POINT('Ctrl Pts',(-5.06265202735881,-39.0253853950253,
-16.647229231688));
#83858=CARTESIAN_POINT('Ctrl Pts',(-5.01248880952419,-38.9033956100947,
-16.6624020649352));
#83859=CARTESIAN_POINT('Ctrl Pts',(-5.,-38.8368267820667,-16.6661333247997));
#83860=CARTESIAN_POINT('Ctrl Pts',(-5.,-38.7742356128,-16.6661333247997));
#83861=CARTESIAN_POINT('Origin',(0.,-39.2742356128,0.));
#83862=CARTESIAN_POINT('Origin',(14.0872311983,-16.6742356128,-1.01503102594));
#83863=CARTESIAN_POINT('',(14.9221240862,-16.6742356128,-1.52650344091));
#83864=CARTESIAN_POINT('',(14.9221240862,-16.6742356128,-1.52650344091));
#83865=CARTESIAN_POINT('',(14.9221240862,-19.3742356128,-1.52650344091));
#83866=CARTESIAN_POINT('',(14.9221240862,-18.0242356128,-1.52650344091));
#83867=CARTESIAN_POINT('',(15.57788482,-19.3742356128,-1.92823584397));
#83868=CARTESIAN_POINT('Origin',(13.4419608479,-16.6742356128,0.619725245787));
#83869=CARTESIAN_POINT('',(14.8362431871,-19.3742356128,1.4738910501));
#83870=CARTESIAN_POINT('',(15.5349443705,-19.3742356128,1.90192964856));
#83871=CARTESIAN_POINT('',(14.8362431871,-16.6742356128,1.4738910501));
#83872=CARTESIAN_POINT('',(14.8362431871,-18.0242356128,1.4738910501));
#83873=CARTESIAN_POINT('',(14.8362431871,-16.6742356128,1.4738910501));
#83874=CARTESIAN_POINT('Origin',(0.,-18.0242356128,0.));
#83875=CARTESIAN_POINT('',(14.976285439,-19.3742356128,0.843133708384));
#83876=CARTESIAN_POINT('Origin',(0.,-19.3742356128,0.));
#83877=CARTESIAN_POINT('',(14.976285439,-16.6742356128,0.843133708384));
#83878=CARTESIAN_POINT('Origin',(-3.5527136788005E-13,-16.6742356128,-5.24580379135386E-14));
#83879=CARTESIAN_POINT('',(14.976285439,-18.0242356128,0.843133708384));
#83880=CARTESIAN_POINT('Origin',(12.9794473804,-18.0242356128,0.730715880599));
#83881=CARTESIAN_POINT('Origin',(12.9794473804,-16.6742356128,0.730715880599));
#83882=CARTESIAN_POINT('Origin',(12.9794473804,-19.3742356128,0.730715880599));
#83883=CARTESIAN_POINT('Origin',(0.,-18.0242356128,0.));
#83884=CARTESIAN_POINT('',(13.4786568951,-19.3742356128,0.758820337546));
#83885=CARTESIAN_POINT('',(13.4786568951,-16.6742356128,0.758820337546));
#83886=CARTESIAN_POINT('',(13.4786568951,-18.0242356128,0.758820337546));
#83887=CARTESIAN_POINT('',(13.3555478213,-16.6742356128,-1.96960462883));
#83888=CARTESIAN_POINT('Origin',(1.04360964314765E-13,-16.6742356128,1.24761312392252E-13));
#83889=CARTESIAN_POINT('',(13.3555478213,-19.3742356128,-1.96960462883));
#83890=CARTESIAN_POINT('',(13.3555478213,-18.0242356128,-1.96960462883));
#83891=CARTESIAN_POINT('Origin',(0.,-19.3742356128,0.));
#83892=CARTESIAN_POINT('Origin',(12.9794473804,-18.0242356128,0.730715880599));
#83893=CARTESIAN_POINT('',(13.1249762208,-16.6742356128,1.20906863394));
#83894=CARTESIAN_POINT('',(13.1249762208,-19.3742356128,1.20906863394));
#83895=CARTESIAN_POINT('',(13.1249762208,-18.0242356128,1.20906863394));
#83896=CARTESIAN_POINT('Origin',(12.9794473804,-16.6742356128,0.730715880598998));
#83897=CARTESIAN_POINT('Origin',(12.9794473804,-19.3742356128,0.730715880599));
#83898=CARTESIAN_POINT('Origin',(13.2705050612,-18.0242356128,1.68742138727));
#83899=CARTESIAN_POINT('',(13.0093116937,-19.3742356128,2.11377572911));
#83900=CARTESIAN_POINT('Origin',(13.2705050612,-19.3742356128,1.68742138727));
#83901=CARTESIAN_POINT('',(13.0093116937,-16.6742356128,2.11377572911));
#83902=CARTESIAN_POINT('',(13.0093116937,-18.0242356128,2.11377572911));
#83903=CARTESIAN_POINT('Origin',(13.2705050612,-16.6742356128,1.68742138727));
#83904=CARTESIAN_POINT('Origin',(12.6583807456,-16.6742356128,1.8987882713));
#83905=CARTESIAN_POINT('',(14.4691278654,-19.3742356128,3.00808889615));
#83906=CARTESIAN_POINT('',(15.9289440371,-16.6742356128,3.90240206319));
#83907=CARTESIAN_POINT('Origin',(13.8501977406,-18.0242356128,-2.04255294841));
#83908=CARTESIAN_POINT('',(13.5890043731,-19.3742356128,-2.46890729025));
#83909=CARTESIAN_POINT('Origin',(13.8501977406,-19.3742356128,-2.04255294841));
#83910=CARTESIAN_POINT('',(13.5890043731,-16.6742356128,-2.46890729025));
#83911=CARTESIAN_POINT('Origin',(13.8501977406,-16.6742356128,-2.04255294841));
#83912=CARTESIAN_POINT('',(13.5890043731,-18.0242356128,-2.46890729025));
#83913=CARTESIAN_POINT('Origin',(0.,-19.3742356128,0.));
#83914=CARTESIAN_POINT('',(14.7589742051,-19.3742356128,-3.18565467672));
#83915=CARTESIAN_POINT('Origin',(13.303651096,-16.6742356128,-2.29409405145));
#83916=CARTESIAN_POINT('',(13.5890043731,-16.6742356128,-2.46890729025));
#83917=CARTESIAN_POINT('Origin',(0.212376136953,-18.7742356128,15.2985259544));
#83918=CARTESIAN_POINT('',(0.213764216279,-16.6742356128,15.3985163201));
#83919=CARTESIAN_POINT('',(0.30759325472,-16.6742356128,15.3290824673));
#83920=CARTESIAN_POINT('Origin',(0.212376136952997,-16.6742356128,15.2985259544));
#83921=CARTESIAN_POINT('',(0.30759325472,-20.8742356128,15.3290824673));
#83922=CARTESIAN_POINT('',(0.30759325472,-18.7742356128,15.3290824673));
#83923=CARTESIAN_POINT('',(0.213764216279,-20.8742356128,15.3985163201));
#83924=CARTESIAN_POINT('Origin',(0.212376136953,-20.8742356128,15.2985259544));
#83925=CARTESIAN_POINT('',(0.213764216279,-18.7742356128,15.3985163201));
#83926=CARTESIAN_POINT('Origin',(1.82391441117,-19.3742356128,10.6040757126));
#83927=CARTESIAN_POINT('',(1.188848049,-16.6742356128,12.5830053333));
#83928=CARTESIAN_POINT('',(0.30759325472,-16.6742356128,15.3290824673));
#83929=CARTESIAN_POINT('',(1.188848049,-20.8742356128,12.5830053333));
#83930=CARTESIAN_POINT('',(1.188848049,-18.7742356128,12.5830053333));
#83931=CARTESIAN_POINT('',(0.748220651862,-20.8742356128,13.9560439003));
#83932=CARTESIAN_POINT('Origin',(2.12507249391,-18.7742356128,11.3019496944));
#83933=CARTESIAN_POINT('',(2.60115808275,-20.5742356128,11.4547322592));
#83934=CARTESIAN_POINT('Origin',(2.12507249391,-20.5742356128,11.3019496944));
#83935=CARTESIAN_POINT('',(2.60115808275,-19.6742356128,11.4547322592));
#83936=CARTESIAN_POINT('Origin',(2.12507249391,-19.6742356128,11.3019496944));
#83937=CARTESIAN_POINT('',(2.60115808275,-18.7742356128,11.4547322592));
#83938=CARTESIAN_POINT('Ctrl Pts',(2.03267803763261,-20.5742356128,10.8105605772543));
#83939=CARTESIAN_POINT('Ctrl Pts',(2.31194217506952,-20.5742356128,10.7580513595367));
#83940=CARTESIAN_POINT('Ctrl Pts',(2.49996449209242,-20.5742356128,10.9711083582602));
#83941=CARTESIAN_POINT('Ctrl Pts',(2.68798680911532,-20.5742356128,11.1841653569836));
#83942=CARTESIAN_POINT('Ctrl Pts',(2.60115808268513,-20.5742356128,11.454732259376));
#83943=CARTESIAN_POINT('Ctrl Pts',(2.03267803763261,-20.6984996815293,10.8105605772543));
#83944=CARTESIAN_POINT('Ctrl Pts',(2.31194217506952,-20.6984996815293,10.7580513595367));
#83945=CARTESIAN_POINT('Ctrl Pts',(2.49996449209242,-20.6984996815293,10.9711083582602));
#83946=CARTESIAN_POINT('Ctrl Pts',(2.68798680911532,-20.6984996815293,11.1841653569836));
#83947=CARTESIAN_POINT('Ctrl Pts',(2.60115808268513,-20.6984996815293,11.454732259376));
#83948=CARTESIAN_POINT('Ctrl Pts',(2.04891506345624,-20.7863676471769,10.8969153014013));
#83949=CARTESIAN_POINT('Ctrl Pts',(2.27910245761361,-20.7863676471769,10.8536338399628));
#83950=CARTESIAN_POINT('Ctrl Pts',(2.43408249764367,-20.7863676471769,11.0292490685892));
#83951=CARTESIAN_POINT('Ctrl Pts',(2.58906253767373,-20.7863676471769,11.2048642972156));
#83952=CARTESIAN_POINT('Ctrl Pts',(2.51749273834894,-20.7863676471769,11.4278828730289));
#83953=CARTESIAN_POINT('Ctrl Pts',(2.06515208927988,-20.8742356128246,10.9832700255484));
#83954=CARTESIAN_POINT('Ctrl Pts',(2.24626274015771,-20.8742356128246,10.9492163203888));
#83955=CARTESIAN_POINT('Ctrl Pts',(2.36820050319492,-20.8742356128246,11.0873897789182));
#83956=CARTESIAN_POINT('Ctrl Pts',(2.49013826623214,-20.8742356128246,11.2255632374475));
#83957=CARTESIAN_POINT('Ctrl Pts',(2.43382739401276,-20.8742356128246,11.4010334866819));
#83958=CARTESIAN_POINT('Ctrl Pts',(2.08811471141,-20.8742356128,11.1053940476));
#83959=CARTESIAN_POINT('Ctrl Pts',(2.19982036635165,-20.8742356128,11.0843903605192));
#83960=CARTESIAN_POINT('Ctrl Pts',(2.27502929313851,-20.8742356128,11.1696131599833));
#83961=CARTESIAN_POINT('Ctrl Pts',(2.35023821992538,-20.8742356128,11.2548359594474));
#83962=CARTESIAN_POINT('Ctrl Pts',(2.3155067293636,-20.8742356128,11.3630627203723));
#83963=CARTESIAN_POINT('',(2.31550672945,-20.8742356128,11.3630627204));
#83964=CARTESIAN_POINT('',(2.08811471141,-20.8742356128,11.1053940476));
#83965=CARTESIAN_POINT('Origin',(2.12507249391,-20.8742356128,11.3019496944));
#83966=CARTESIAN_POINT('Origin',(2.08811471141,-20.5742356128,11.1053940476));
#83967=CARTESIAN_POINT('Origin',(2.31550672945,-20.5742356128,11.3630627204));
#83968=CARTESIAN_POINT('Origin',(1.59732923672,-20.5742356128,13.6009748472));
#83969=CARTESIAN_POINT('',(1.50971990538,-20.8742356128,13.8739741921));
#83970=CARTESIAN_POINT('',(1.94732913984,-20.5742356128,13.4921279379));
#83971=CARTESIAN_POINT('Origin',(2.77608558884,-19.3742356128,10.9096408422));
#83972=CARTESIAN_POINT('',(2.30669397219696,-19.6742353176957,12.3723115634183));
#83973=CARTESIAN_POINT('',(1.91660155908,-19.6742356128,13.5878781199));
#83974=CARTESIAN_POINT('',(2.11321243347333,-19.0742355019,12.9752191818));
#83975=CARTESIAN_POINT('Origin',(2.30675324894277,-19.0740005634869,12.37212685105));
#83976=CARTESIAN_POINT('',(2.11321243752,-16.6742356128,12.9752191692));
#83977=CARTESIAN_POINT('',(2.11321243752,-18.7742356128,12.9752191692));
#83978=CARTESIAN_POINT('',(1.02442996075,-16.6742356128,16.3679730955));
#83979=CARTESIAN_POINT('Origin',(2.39886379082,-18.7742356128,13.066888708));
#83980=CARTESIAN_POINT('',(2.57699954471655,-19.074235612975,12.8255017742882));
#83981=CARTESIAN_POINT('Ctrl Pts',(2.57699954611,-19.0742356128,12.8255017724));
#83982=CARTESIAN_POINT('Ctrl Pts',(2.48546463599,-19.0742356274384,12.7579519823));
#83983=CARTESIAN_POINT('Ctrl Pts',(2.36191078436,-19.0742356216407,12.7337901943));
#83984=CARTESIAN_POINT('Ctrl Pts',(2.23407965787,-19.0742355909528,12.7750559918));
#83985=CARTESIAN_POINT('Ctrl Pts',(2.14797389499,-19.0742355464704,12.8668990358));
#83986=CARTESIAN_POINT('Ctrl Pts',(2.11321243145,-19.0742355019,12.9752191881));
#83987=CARTESIAN_POINT('',(2.576999541,-16.6742356128,12.8255017686));
#83988=CARTESIAN_POINT('',(2.576999541,-18.0242356128,12.8255017686));
#83989=CARTESIAN_POINT('Origin',(2.39886379082,-16.6742356128,13.066888708));
#83990=CARTESIAN_POINT('Origin',(1.40932124909,-16.6742356128,11.9637929743));
#83991=CARTESIAN_POINT('',(4.11574708991,-19.0742356128,13.9610476671));
#83992=CARTESIAN_POINT('',(2.576999541,-16.6742356128,12.8255017686));
#83993=CARTESIAN_POINT('Origin',(1.09363093124,-18.7742356128,12.5524488203));
#83994=CARTESIAN_POINT('',(1.08495132067,-16.6742356128,12.4528262106));
#83995=CARTESIAN_POINT('Origin',(1.09363093124,-16.6742356128,12.5524488203));
#83996=CARTESIAN_POINT('',(1.08495132067,-20.8742356128,12.4528262106));
#83997=CARTESIAN_POINT('',(1.08495132067,-18.7742356128,12.4528262106));
#83998=CARTESIAN_POINT('Origin',(1.09363093124,-20.8742356128,12.5524488203));
#83999=CARTESIAN_POINT('Ctrl Pts',(2.11321243145,-19.0742355019,12.9752191881));
#84000=CARTESIAN_POINT('Ctrl Pts',(2.14797389499,-19.0742355464,12.8668990358));
#84001=CARTESIAN_POINT('Ctrl Pts',(2.23407965787,-19.0742355909,12.7750559918));
#84002=CARTESIAN_POINT('Ctrl Pts',(2.36191078436,-19.0742356216,12.7337901943));
#84003=CARTESIAN_POINT('Ctrl Pts',(2.48546463599,-19.0742356274,12.7579519823));
#84004=CARTESIAN_POINT('Ctrl Pts',(2.57699954053,-19.0742356132,12.82550178));
#84005=CARTESIAN_POINT('Ctrl Pts',(2.11321242505,-19.1612543019,12.975219208));
#84006=CARTESIAN_POINT('Ctrl Pts',(2.14797389154,-19.1438426701,12.8668990456));
#84007=CARTESIAN_POINT('Ctrl Pts',(2.23407965879,-19.1264310382,12.7750559919));
#84008=CARTESIAN_POINT('Ctrl Pts',(2.36191078991,-19.1144387816,12.7337901893));
#84009=CARTESIAN_POINT('Ctrl Pts',(2.48546464338,-19.112181627,12.7579519792));
#84010=CARTESIAN_POINT('Ctrl Pts',(2.57699954662,-19.1177450086,12.825501783));
#84011=CARTESIAN_POINT('Ctrl Pts',(2.11829710106,-19.248306695,12.9593748545));
#84012=CARTESIAN_POINT('Ctrl Pts',(2.15187949666,-19.2134621794,12.8547287833));
#84013=CARTESIAN_POINT('Ctrl Pts',(2.23632644193,-19.1786176639,12.7664058619));
#84014=CARTESIAN_POINT('Ctrl Pts',(2.3624655556,-19.1546253192,12.7270177415));
#84015=CARTESIAN_POINT('Ctrl Pts',(2.48537378308,-19.1501233479,12.7505876284));
#84016=CARTESIAN_POINT('Ctrl Pts',(2.57740280629,-19.1612710822,12.8160010902));
#84017=CARTESIAN_POINT('Ctrl Pts',(2.1284939378,-19.3306965513,12.9276005023));
#84018=CARTESIAN_POINT('Ctrl Pts',(2.15970428933,-19.2801076689,12.8303459527));
#84019=CARTESIAN_POINT('Ctrl Pts',(2.24081540097,-19.2295187866,12.7491052593));
#84020=CARTESIAN_POINT('Ctrl Pts',(2.36355540449,-19.1943772592,12.7134885287));
#84021=CARTESIAN_POINT('Ctrl Pts',(2.48517594342,-19.1870911735,12.7358510743));
#84022=CARTESIAN_POINT('Ctrl Pts',(2.5782116467,-19.2024661641,12.796948158));
#84023=CARTESIAN_POINT('Ctrl Pts',(2.16109563614,-19.4975344726,12.8260103845));
#84024=CARTESIAN_POINT('Ctrl Pts',(2.18524115037,-19.4177125414,12.7507705807));
#84025=CARTESIAN_POINT('Ctrl Pts',(2.25630596622,-19.3378906101,12.6905878411));
#84026=CARTESIAN_POINT('Ctrl Pts',(2.36852442786,-19.2809552961,12.6666894295));
#84027=CARTESIAN_POINT('Ctrl Pts',(2.48552961718,-19.2657636574,12.6866327467));
#84028=CARTESIAN_POINT('Ctrl Pts',(2.58079725879,-19.2858849393,12.7360320273));
#84029=CARTESIAN_POINT('Ctrl Pts',(2.21060765367,-19.6106096232,12.6717260389));
#84030=CARTESIAN_POINT('Ctrl Pts',(2.22542521735,-19.5162497602,12.6255530347));
#84031=CARTESIAN_POINT('Ctrl Pts',(2.28292923485,-19.4218898972,12.5930787142));
#84032=CARTESIAN_POINT('Ctrl Pts',(2.38019466467,-19.3518501373,12.5859609253));
#84033=CARTESIAN_POINT('Ctrl Pts',(2.48889752329,-19.3268991358,12.6060157728));
#84034=CARTESIAN_POINT('Ctrl Pts',(2.58472445083,-19.3424227485,12.6435184464));
#84035=CARTESIAN_POINT('Ctrl Pts',(2.24157751669,-19.6529683202,12.5752208815));
#84036=CARTESIAN_POINT('Ctrl Pts',(2.25115370883,-19.5552809276,12.5453805297));
#84037=CARTESIAN_POINT('Ctrl Pts',(2.30089868661,-19.4575935349,12.5284309064));
#84038=CARTESIAN_POINT('Ctrl Pts',(2.3892638599,-19.383367284,12.5313593346));
#84039=CARTESIAN_POINT('Ctrl Pts',(2.49223570108,-19.3530489966,12.553066847));
#84040=CARTESIAN_POINT('Ctrl Pts',(2.58718049198,-19.36360193,12.5856515981));
#84041=CARTESIAN_POINT('Ctrl Pts',(2.27413005219,-19.6742347534,12.47378396));
#84042=CARTESIAN_POINT('Ctrl Pts',(2.2787229772,-19.5767604829,12.4594719462));
#84043=CARTESIAN_POINT('Ctrl Pts',(2.32096970846,-19.4792862125,12.4572435686));
#84044=CARTESIAN_POINT('Ctrl Pts',(2.40043923714,-19.4036435793,12.4702692455));
#84045=CARTESIAN_POINT('Ctrl Pts',(2.49695035202,-19.3691668211,12.4950419018));
#84046=CARTESIAN_POINT('Ctrl Pts',(2.58976267699,-19.3742352023,12.5248266884));
#84047=CARTESIAN_POINT('Ctrl Pts',(2.30669397214,-19.6742350234,12.3723115634));
#84048=CARTESIAN_POINT('Ctrl Pts',(2.30669398607,-19.579987326,12.3723115185));
#84049=CARTESIAN_POINT('Ctrl Pts',(2.34193483095,-19.4857396287,12.3836207521));
#84050=CARTESIAN_POINT('Ctrl Pts',(2.41286534931,-19.4112462739,12.4063833145));
#84051=CARTESIAN_POINT('Ctrl Pts',(2.50260539009,-19.374235302,12.4351821369));
#84052=CARTESIAN_POINT('Ctrl Pts',(2.5923454193,-19.3742353183,12.4639809751));
#84053=CARTESIAN_POINT('',(2.59234532544548,-19.3742354655498,12.4639811022925));
#84054=CARTESIAN_POINT('Origin',(2.59032542786042,-19.6721136845399,12.4633329506423));
#84055=CARTESIAN_POINT('Ctrl Pts',(2.57699954051151,-19.0742356132,12.8255017799864));
#84056=CARTESIAN_POINT('Ctrl Pts',(2.57699954076031,-19.090097926119,12.8255017796252));
#84057=CARTESIAN_POINT('Ctrl Pts',(2.57701922698783,-19.1061952220878,12.8239491830546));
#84058=CARTESIAN_POINT('Ctrl Pts',(2.57709880509,-19.12230194734,12.8207578866714));
#84059=CARTESIAN_POINT('Ctrl Pts',(2.57717957791688,-19.138650486634,12.8175186786076));
#84060=CARTESIAN_POINT('Ctrl Pts',(2.57732193153449,-19.1550088429505,12.8125913121783));
#84061=CARTESIAN_POINT('Ctrl Pts',(2.57756630925782,-19.1711234874925,12.8059362580234));
#84062=CARTESIAN_POINT('Ctrl Pts',(2.57765386220267,-19.1768968639105,12.8035519589085));
#84063=CARTESIAN_POINT('Ctrl Pts',(2.57775450453884,-19.1826387868041,12.8009463571809));
#84064=CARTESIAN_POINT('Ctrl Pts',(2.57787008290454,-19.1883370166356,12.7981191469069));
#84065=CARTESIAN_POINT('Ctrl Pts',(2.57817481420733,-19.2033608404254,12.7906649882946));
#84066=CARTESIAN_POINT('Ctrl Pts',(2.57857607419071,-19.2180779034073,12.7816630814634));
#84067=CARTESIAN_POINT('Ctrl Pts',(2.57906577997038,-19.2322424680007,12.7711186642919));
#84068=CARTESIAN_POINT('Ctrl Pts',(2.57918353240181,-19.23564841498,12.7685832015478));
#84069=CARTESIAN_POINT('Ctrl Pts',(2.57930638722896,-19.2390223625536,12.7659587844579));
#84070=CARTESIAN_POINT('Ctrl Pts',(2.57943420930647,-19.2423608205184,12.7632459251213));
#84071=CARTESIAN_POINT('Ctrl Pts',(2.57976391192748,-19.2509719960097,12.7562484106769));
#84072=CARTESIAN_POINT('Ctrl Pts',(2.58012584519649,-19.2593468309819,12.7486613252388));
#84073=CARTESIAN_POINT('Ctrl Pts',(2.58051138970481,-19.2674240519412,12.7404963491802));
#84074=CARTESIAN_POINT('Ctrl Pts',(2.58056816614879,-19.2686135277951,12.7392939502465));
#84075=CARTESIAN_POINT('Ctrl Pts',(2.58062545046643,-19.269796552749,12.73807903108));
#84076=CARTESIAN_POINT('Ctrl Pts',(2.58068320201332,-19.2709729333731,12.7368516370555));
#84077=CARTESIAN_POINT('Ctrl Pts',(2.58082153347369,-19.2737907011809,12.7339116775742));
#84078=CARTESIAN_POINT('Ctrl Pts',(2.58096254608146,-19.2765703481791,12.7309001375071));
#84079=CARTESIAN_POINT('Ctrl Pts',(2.58110567068349,-19.2793091646015,12.7278178308886));
#84080=CARTESIAN_POINT('Ctrl Pts',(2.58120710929444,-19.2812502825475,12.7256332665479));
#84081=CARTESIAN_POINT('Ctrl Pts',(2.58130960682343,-19.2831708968851,12.7234131488369));
#84082=CARTESIAN_POINT('Ctrl Pts',(2.5814129424722,-19.2850700547872,12.7211577769492));
#84083=CARTESIAN_POINT('Ctrl Pts',(2.58147759529574,-19.2862582790078,12.7197466844325));
#84084=CARTESIAN_POINT('Ctrl Pts',(2.58155841255508,-19.2877354635363,12.7179601732247));
#84085=CARTESIAN_POINT('Ctrl Pts',(2.58162455597423,-19.2889406945427,12.7164741655177));
#84086=CARTESIAN_POINT('Ctrl Pts',(2.58166413064681,-19.2896618036579,12.7155850631821));
#84087=CARTESIAN_POINT('Ctrl Pts',(2.58169840521701,-19.2902866388584,12.7148046420957));
#84088=CARTESIAN_POINT('Ctrl Pts',(2.58172051136112,-19.290701337284,12.7142838635621));
#84089=CARTESIAN_POINT('Ctrl Pts',(2.58205066174859,-19.2968947668227,12.7065061510011));
#84090=CARTESIAN_POINT('Ctrl Pts',(2.58236159329862,-19.3033427590597,12.6976710607334));
#84091=CARTESIAN_POINT('Ctrl Pts',(2.58269944763325,-19.3098398763417,12.687678603169));
#84092=CARTESIAN_POINT('Ctrl Pts',(2.58301649266678,-19.3159368197739,12.6783016062834));
#84093=CARTESIAN_POINT('Ctrl Pts',(2.58335731531155,-19.3220767709619,12.6679046408337));
#84094=CARTESIAN_POINT('Ctrl Pts',(2.58375973823555,-19.3280499192408,12.6564230442139));
#84095=CARTESIAN_POINT('Ctrl Pts',(2.58415576141217,-19.3339280763109,12.6451240398706));
#84096=CARTESIAN_POINT('Ctrl Pts',(2.58461157955433,-19.3396446663915,12.6327736690589));
#84097=CARTESIAN_POINT('Ctrl Pts',(2.58516141713524,-19.3449612196282,12.6193410240067));
#84098=CARTESIAN_POINT('Ctrl Pts',(2.58566365303769,-19.3498174972007,12.607071297738));
#84099=CARTESIAN_POINT('Ctrl Pts',(2.5862673264569,-19.3543409250383,12.5939094274449));
#84100=CARTESIAN_POINT('Ctrl Pts',(2.58693635426293,-19.3583167707245,12.5798423788928));
#84101=CARTESIAN_POINT('Ctrl Pts',(2.58758944940851,-19.3621979330527,12.5661103321239));
#84102=CARTESIAN_POINT('Ctrl Pts',(2.58830473859446,-19.3655569150395,12.5515153321523));
#84103=CARTESIAN_POINT('Ctrl Pts',(2.58904729022186,-19.3681783800973,12.5360915504371));
#84104=CARTESIAN_POINT('Ctrl Pts',(2.58976947620421,-19.3707279473572,12.5210907901685));
#84105=CARTESIAN_POINT('Ctrl Pts',(2.59051733423415,-19.3725797009973,12.5053059280041));
#84106=CARTESIAN_POINT('Ctrl Pts',(2.59125889447743,-19.373524845373,12.4888164992638));
#84107=CARTESIAN_POINT('Ctrl Pts',(2.59162376646249,-19.3739898874349,12.4807031589771));
#84108=CARTESIAN_POINT('Ctrl Pts',(2.59198712693089,-19.3742352985182,12.4724200069811));
#84109=CARTESIAN_POINT('Ctrl Pts',(2.59234532544022,-19.3742353182997,12.4639811022993));
#84110=CARTESIAN_POINT('Origin',(4.29388284009,-19.0742356128,13.7196607277));
#84111=CARTESIAN_POINT('',(4.42080718383,-19.3742356128,13.8133267862));
#84112=CARTESIAN_POINT('Ctrl Pts',(2.03267803765,-19.6742356128,10.8105605773));
#84113=CARTESIAN_POINT('Ctrl Pts',(2.03267803765,-19.6742356128,10.8105605773));
#84114=CARTESIAN_POINT('Ctrl Pts',(2.03267803765,-19.6742356128,10.8105605773));
#84115=CARTESIAN_POINT('Ctrl Pts',(2.03267803765,-19.6742356128,10.8105605773));
#84116=CARTESIAN_POINT('Ctrl Pts',(2.03267803765,-19.6742356128,10.8105605773));
#84117=CARTESIAN_POINT('Ctrl Pts',(2.03267803765,-19.6742356128,10.8105605773));
#84118=CARTESIAN_POINT('Ctrl Pts',(2.05894886759,-19.6259152622,10.8056234563));
#84119=CARTESIAN_POINT('Ctrl Pts',(2.06734285289645,-19.6307029517914,10.8040622488486));
#84120=CARTESIAN_POINT('Ctrl Pts',(2.07573485238451,-19.6354906438259,10.802501411656));
#84121=CARTESIAN_POINT('Ctrl Pts',(2.08416049881215,-19.6403007330939,10.8009343190103));
#84122=CARTESIAN_POINT('Ctrl Pts',(2.09265549117115,-19.6451556121481,10.7993543328483));
#84123=CARTESIAN_POINT('Ctrl Pts',(2.10125198398,-19.6500754685,10.7977554742));
#84124=CARTESIAN_POINT('Ctrl Pts',(2.0870381674,-19.5762206261,10.8001977615));
#84125=CARTESIAN_POINT('Ctrl Pts',(2.1034870056,-19.586196795,10.7970191759));
#84126=CARTESIAN_POINT('Ctrl Pts',(2.1202364023,-19.596172964,10.7953959482));
#84127=CARTESIAN_POINT('Ctrl Pts',(2.13714159915,-19.6060613319,10.795356101));
#84128=CARTESIAN_POINT('Ctrl Pts',(2.15405252281,-19.6157741162,10.796899988));
#84129=CARTESIAN_POINT('Ctrl Pts',(2.17082159168,-19.6252281195,10.8000002758));
#84130=CARTESIAN_POINT('',(2.17082158289334,-19.625228208562,10.8000002947161));
#84131=CARTESIAN_POINT('Origin',(2.15163545644867,-19.6372754487651,11.5156625316905));
#84132=CARTESIAN_POINT('Origin',(2.14395737416692,-19.5762206558258,11.0947491984194));
#84133=CARTESIAN_POINT('Origin',(2.12507249391,-19.6742356128,11.3019496944));
#84134=CARTESIAN_POINT('',(2.86720992902818,-19.3749426154318,11.5401120404683));
#84135=CARTESIAN_POINT('Origin',(2.88680943605,-19.6742356128,11.5464017981));
#84136=CARTESIAN_POINT('',(2.49881053590011,-19.5594863527756,10.9363631916917));
#84137=CARTESIAN_POINT('Ctrl Pts',(2.49881057490515,-19.5594863753635,10.9363631535376));
#84138=CARTESIAN_POINT('Ctrl Pts',(2.48189321230393,-19.5616279484725,10.9203363430907));
#84139=CARTESIAN_POINT('Ctrl Pts',(2.46385740336137,-19.5640380169532,10.9055168337234));
#84140=CARTESIAN_POINT('Ctrl Pts',(2.44489566614884,-19.5667483129689,10.8920449861814));
#84141=CARTESIAN_POINT('Ctrl Pts',(2.43732153123321,-19.5678309219859,10.8866637497629));
#84142=CARTESIAN_POINT('Ctrl Pts',(2.42960011206188,-19.5689617226717,10.8814972313772));
#84143=CARTESIAN_POINT('Ctrl Pts',(2.42174516216224,-19.5701438338236,10.8765530967493));
#84144=CARTESIAN_POINT('Ctrl Pts',(2.40085003502617,-19.5732883940211,10.8634010941334));
#84145=CARTESIAN_POINT('Ctrl Pts',(2.37900647676366,-19.576794631005,10.851824341331));
#84146=CARTESIAN_POINT('Ctrl Pts',(2.35649261223513,-19.5807393452508,10.8419423005584));
#84147=CARTESIAN_POINT('Ctrl Pts',(2.34862227224651,-19.5821183285094,10.8384877616646));
#84148=CARTESIAN_POINT('Ctrl Pts',(2.34067012527774,-19.5835511190477,10.8352399234243));
#84149=CARTESIAN_POINT('Ctrl Pts',(2.33264814825159,-19.5850416728663,10.8322025543555));
#84150=CARTESIAN_POINT('Ctrl Pts',(2.31659588540332,-19.5880243243507,10.8261246702505));
#84151=CARTESIAN_POINT('Ctrl Pts',(2.30026230264194,-19.5912378419647,10.8208866290135));
#84152=CARTESIAN_POINT('Ctrl Pts',(2.28377162562935,-19.5947588383549,10.8165105761754));
#84153=CARTESIAN_POINT('Ctrl Pts',(2.27121598386632,-19.5974396482021,10.8131787450001));
#84154=CARTESIAN_POINT('Ctrl Pts',(2.25856722444482,-19.6002954429563,10.8103468853162));
#84155=CARTESIAN_POINT('Ctrl Pts',(2.24588993027475,-19.6033758386239,10.8080180359072));
#84156=CARTESIAN_POINT('Ctrl Pts',(2.24191676821981,-19.6043412584538,10.8072881564882));
#84157=CARTESIAN_POINT('Ctrl Pts',(2.23794098212931,-19.6053290264032,10.8066076133275));
#84158=CARTESIAN_POINT('Ctrl Pts',(2.23396517538284,-19.6063416556388,10.8059762733988));
#84159=CARTESIAN_POINT('Ctrl Pts',(2.22528476776626,-19.6085525363706,10.8045978643677));
#84160=CARTESIAN_POINT('Ctrl Pts',(2.21660055076944,-19.6108808098985,10.8034535416467));
#84161=CARTESIAN_POINT('Ctrl Pts',(2.20794528221928,-19.6133598336687,10.8025389750823));
#84162=CARTESIAN_POINT('Ctrl Pts',(2.19929001366913,-19.6158388574389,10.8016244085179));
#84163=CARTESIAN_POINT('Ctrl Pts',(2.19066341384667,-19.6184721846969,10.8009406384501));
#84164=CARTESIAN_POINT('Ctrl Pts',(2.18211944040195,-19.6213167700468,10.8004807714098));
#84165=CARTESIAN_POINT('Ctrl Pts',(2.17833689867943,-19.622576109491,10.8002771815604));
#84166=CARTESIAN_POINT('Ctrl Pts',(2.17456948674399,-19.6238775578788,10.800117324421));
#84167=CARTESIAN_POINT('Ctrl Pts',(2.17082158489314,-19.6252282072342,10.800000304529));
#84168=CARTESIAN_POINT('Ctrl Pts',(2.86720992947,-19.3749426154,11.5401120406));
#84169=CARTESIAN_POINT('Ctrl Pts',(2.83073115845,-19.3783306343,11.4925686116));
#84170=CARTESIAN_POINT('Ctrl Pts',(2.796245355,-19.3917000854,11.4409843867));
#84171=CARTESIAN_POINT('Ctrl Pts',(2.76681414133,-19.4133420624,11.3857731806));
#84172=CARTESIAN_POINT('Ctrl Pts',(2.71098021085,-19.4644758001,11.2604631973));
#84173=CARTESIAN_POINT('Ctrl Pts',(2.64928177187,-19.5134920611,11.1278449523));
#84174=CARTESIAN_POINT('Ctrl Pts',(2.60971873368,-19.5351693857,11.0585616091));
#84175=CARTESIAN_POINT('Ctrl Pts',(2.55903583297,-19.5518626834,10.9934181309));
#84176=CARTESIAN_POINT('Ctrl Pts',(2.49881045789,-19.5594863076,10.936363268));
#84177=CARTESIAN_POINT('Origin',(2.20225291238,-19.6742356128,13.6795476588));
#84178=CARTESIAN_POINT('',(2.8825676448599,-19.3742356866711,11.5596196699867));
#84179=CARTESIAN_POINT('',(2.7374564764,-19.3742356128,12.011800398));
#84180=CARTESIAN_POINT('Ctrl Pts',(2.88256762736,-19.3742356128,11.5596196937));
#84181=CARTESIAN_POINT('Ctrl Pts',(2.87949410326,-19.3742359194,11.555715524));
#84182=CARTESIAN_POINT('Ctrl Pts',(2.87642049893,-19.3743066351,11.5518113974));
#84183=CARTESIAN_POINT('Ctrl Pts',(2.87334791066,-19.3744480562,11.5479085637));
#84184=CARTESIAN_POINT('Ctrl Pts',(2.87027737467,-19.3746601605,11.544008339));
#84185=CARTESIAN_POINT('Ctrl Pts',(2.86720992947,-19.3749426154,11.5401120406));
#84186=CARTESIAN_POINT('Origin',(0.,-19.3742356128,0.));
#84187=CARTESIAN_POINT('',(4.88509763285,-19.3742356128,13.0374220375));
#84188=CARTESIAN_POINT('Ctrl Pts',(2.47879655924,-19.4447372417,10.8888042378));
#84189=CARTESIAN_POINT('Ctrl Pts',(2.4861493729,-19.4683844343,10.8942303744));
#84190=CARTESIAN_POINT('Ctrl Pts',(2.49191208452,-19.4920316269,10.9018112135));
#84191=CARTESIAN_POINT('Ctrl Pts',(2.49597515407,-19.5153269748,10.9114662072));
#84192=CARTESIAN_POINT('Ctrl Pts',(2.49827725138,-19.5379188455,10.9230496178));
#84193=CARTESIAN_POINT('Ctrl Pts',(2.49881059449,-19.5594864256,10.9363632033));
#84194=CARTESIAN_POINT('Ctrl Pts',(2.44089425171,-19.4520187736,10.8608335));
#84195=CARTESIAN_POINT('Ctrl Pts',(2.44963136368,-19.4748973849,10.8662112305));
#84196=CARTESIAN_POINT('Ctrl Pts',(2.45702223689,-19.4977759963,10.8738380918));
#84197=CARTESIAN_POINT('Ctrl Pts',(2.46293957656,-19.5203232432,10.8836363306));
#84198=CARTESIAN_POINT('Ctrl Pts',(2.4672956606,-19.5422079505,10.8954618457));
#84199=CARTESIAN_POINT('Ctrl Pts',(2.47004984489,-19.5631271909,10.9091164123));
#84200=CARTESIAN_POINT('Ctrl Pts',(2.40004991429,-19.4606048121,10.8375867107));
#84201=CARTESIAN_POINT('Ctrl Pts',(2.41019998813,-19.4825787168,10.8426296142));
#84202=CARTESIAN_POINT('Ctrl Pts',(2.41925749864,-19.5045526216,10.8499715311));
#84203=CARTESIAN_POINT('Ctrl Pts',(2.42707877395,-19.5262185084,10.8595420691));
#84204=CARTESIAN_POINT('Ctrl Pts',(2.43355105359,-19.5472685228,10.8712051552));
#84205=CARTESIAN_POINT('Ctrl Pts',(2.43860186298,-19.5674202148,10.8847702011));
#84206=CARTESIAN_POINT('Ctrl Pts',(2.35714755108,-19.4705790255,10.8194836801));
#84207=CARTESIAN_POINT('Ctrl Pts',(2.36865799258,-19.4915042786,10.8238986479));
#84208=CARTESIAN_POINT('Ctrl Pts',(2.3793283911,-19.5124295317,10.8306149778));
#84209=CARTESIAN_POINT('Ctrl Pts',(2.38900185162,-19.5330726947,10.839573774));
#84210=CARTESIAN_POINT('Ctrl Pts',(2.3975442085,-19.5531518159,10.850652948));
#84211=CARTESIAN_POINT('Ctrl Pts',(2.40485476239,-19.5724073147,10.863676829));
#84212=CARTESIAN_POINT('Ctrl Pts',(2.27560738165,-19.4921831081,10.7955818101));
#84213=CARTESIAN_POINT('Ctrl Pts',(2.2893900823,-19.510844473,10.7983487664));
#84214=CARTESIAN_POINT('Ctrl Pts',(2.30277704132,-19.5295058379,10.8033357254));
#84215=CARTESIAN_POINT('Ctrl Pts',(2.31559552336,-19.5479374484,10.8105100727));
#84216=CARTESIAN_POINT('Ctrl Pts',(2.32768219961,-19.5659096429,10.8197835155));
#84217=CARTESIAN_POINT('Ctrl Pts',(2.33889513807,-19.5832093643,10.8310183547));
#84218=CARTESIAN_POINT('Ctrl Pts',(2.19384540622,-19.5207627351,10.7891484524));
#84219=CARTESIAN_POINT('Ctrl Pts',(2.2092243494,-19.5364515236,10.7895844661));
#84220=CARTESIAN_POINT('Ctrl Pts',(2.22456910998,-19.5521403122,10.7920171276));
#84221=CARTESIAN_POINT('Ctrl Pts',(2.23970912867,-19.56765722,10.7964428));
#84222=CARTESIAN_POINT('Ctrl Pts',(2.25447433499,-19.5828304221,10.8028133883));
#84223=CARTESIAN_POINT('Ctrl Pts',(2.26870622615,-19.5974991706,10.8110393571));
#84224=CARTESIAN_POINT('Ctrl Pts',(2.15676147687,-19.5361420848,10.7897230447));
#84225=CARTESIAN_POINT('Ctrl Pts',(2.17269814184,-19.5502379741,10.7889802082));
#84226=CARTESIAN_POINT('Ctrl Pts',(2.18874339027,-19.5643338633,10.7901046703));
#84227=CARTESIAN_POINT('Ctrl Pts',(2.20473176783,-19.578285603,10.7931055871));
#84228=CARTESIAN_POINT('Ctrl Pts',(2.22049530483,-19.591949083,10.7979533276));
#84229=CARTESIAN_POINT('Ctrl Pts',(2.23587372456,-19.6051888511,10.8045811578));
#84230=CARTESIAN_POINT('Ctrl Pts',(2.12065129512,-19.5532237866,10.7937022943));
#84231=CARTESIAN_POINT('Ctrl Pts',(2.13693992507,-19.565556494,10.7917229743));
#84232=CARTESIAN_POINT('Ctrl Pts',(2.15344959477,-19.5778892014,10.7914591884));
#84233=CARTESIAN_POINT('Ctrl Pts',(2.1700239605,-19.5901054864,10.7929309325));
#84234=CARTESIAN_POINT('Ctrl Pts',(2.18650229981,-19.6020889553,10.7961251723));
#84235=CARTESIAN_POINT('Ctrl Pts',(2.20272856722,-19.6137296999,10.8009965235));
#84236=CARTESIAN_POINT('Ctrl Pts',(2.08703817283,-19.5762208096,10.800197792));
#84237=CARTESIAN_POINT('Ctrl Pts',(2.10348700925,-19.5861969598,10.7970192075));
#84238=CARTESIAN_POINT('Ctrl Pts',(2.12023640403,-19.59617311,10.7953959802));
#84239=CARTESIAN_POINT('Ctrl Pts',(2.13714159891,-19.6060614593,10.7953561328));
#84240=CARTESIAN_POINT('Ctrl Pts',(2.1540525206,-19.6157742254,10.7969000191));
#84241=CARTESIAN_POINT('Ctrl Pts',(2.17082158758,-19.625228211,10.8000003054));
#84242=CARTESIAN_POINT('',(2.47879649228767,-19.4447371256487,10.8888042456754));
#84243=CARTESIAN_POINT('Ctrl Pts',(2.47879653467763,-19.4447372464188,10.8888042196737));
#84244=CARTESIAN_POINT('Ctrl Pts',(2.46236153595402,-19.4478946260502,10.876675697395));
#84245=CARTESIAN_POINT('Ctrl Pts',(2.44568006662651,-19.4512658354645,10.8659214494554));
#84246=CARTESIAN_POINT('Ctrl Pts',(2.42898429620936,-19.4548281576759,10.8564327768725));
#84247=CARTESIAN_POINT('Ctrl Pts',(2.41178359825752,-19.4584982146326,10.8466571398709));
#84248=CARTESIAN_POINT('Ctrl Pts',(2.39456825807104,-19.4623715596554,10.838223851903));
#84249=CARTESIAN_POINT('Ctrl Pts',(2.37754518539451,-19.4664312188039,10.8309864958141));
#84250=CARTESIAN_POINT('Ctrl Pts',(2.36024497993418,-19.4705569685263,10.8236313167752));
#84251=CARTESIAN_POINT('Ctrl Pts',(2.34314342187394,-19.4748754849818,10.8175104777587));
#84252=CARTESIAN_POINT('Ctrl Pts',(2.32640542393977,-19.479370938867,10.8124560770319));
#84253=CARTESIAN_POINT('Ctrl Pts',(2.30916927320829,-19.4840001855115,10.8072512482867));
#84254=CARTESIAN_POINT('Ctrl Pts',(2.29231853163633,-19.4888172941262,10.8031765684167));
#84255=CARTESIAN_POINT('Ctrl Pts',(2.2759784968436,-19.4938026368773,10.8000457865001));
#84256=CARTESIAN_POINT('Ctrl Pts',(2.27375428601186,-19.4944812433483,10.7996196234509));
#84257=CARTESIAN_POINT('Ctrl Pts',(2.27153945952708,-19.4951629606774,10.7992109544957));
#84258=CARTESIAN_POINT('Ctrl Pts',(2.26933426098062,-19.4958477329477,10.7988193163431));
#84259=CARTESIAN_POINT('Ctrl Pts',(2.26467629109108,-19.4972941553671,10.7979920716827));
#84260=CARTESIAN_POINT('Ctrl Pts',(2.26006131757016,-19.4987542761252,10.7972407987156));
#84261=CARTESIAN_POINT('Ctrl Pts',(2.255491916587,-19.5002289809292,10.7965609749296));
#84262=CARTESIAN_POINT('Ctrl Pts',(2.23931624507815,-19.5054494333626,10.7941543999131));
#84263=CARTESIAN_POINT('Ctrl Pts',(2.22369167515068,-19.510863007211,10.7926392347204));
#84264=CARTESIAN_POINT('Ctrl Pts',(2.20872066031686,-19.5164597190796,10.7918341279312));
#84265=CARTESIAN_POINT('Ctrl Pts',(2.19296963644529,-19.522348026801,10.7909870740477));
#84266=CARTESIAN_POINT('Ctrl Pts',(2.17794021198136,-19.5284338048858,10.790926179143));
#84267=CARTESIAN_POINT('Ctrl Pts',(2.16371391624849,-19.5347195389631,10.791444877268));
#84268=CARTESIAN_POINT('Ctrl Pts',(2.14831679595182,-19.5415225891428,10.7920062642642));
#84269=CARTESIAN_POINT('Ctrl Pts',(2.13386025331722,-19.5485602758314,10.7932458031077));
#84270=CARTESIAN_POINT('Ctrl Pts',(2.12042184758101,-19.5558955782218,10.7949111398957));
#84271=CARTESIAN_POINT('Ctrl Pts',(2.10847797481028,-19.5624150955072,10.7963912686481));
#84272=CARTESIAN_POINT('Ctrl Pts',(2.09733850824266,-19.5691736498683,10.7982073251794));
#84273=CARTESIAN_POINT('Ctrl Pts',(2.08703817327717,-19.5762208095999,10.8001977919136));
#84274=CARTESIAN_POINT('Origin',(2.30065980503153,-19.4447369552491,11.1301922502066));
#84275=CARTESIAN_POINT('Origin',(2.18190353865,-18.7742356128,11.2911158416));
#84276=CARTESIAN_POINT('',(2.47879645562,-16.6742356128,10.8888042759));
#84277=CARTESIAN_POINT('Origin',(2.18190353865,-16.6742356128,11.2911158416));
#84278=CARTESIAN_POINT('',(2.47879645562,-18.0594863082,10.8888042759));
#84279=CARTESIAN_POINT('Ctrl Pts',(2.47879645562,-19.4447370035,10.8888042759));
#84280=CARTESIAN_POINT('Ctrl Pts',(2.48614926363,-19.4683842219,10.8942304132));
#84281=CARTESIAN_POINT('Ctrl Pts',(2.4919119687,-19.4920314402,10.901811256));
#84282=CARTESIAN_POINT('Ctrl Pts',(2.49597503074,-19.515326813,10.9114662563));
#84283=CARTESIAN_POINT('Ctrl Pts',(2.49827711961,-19.5379187068,10.9230496761));
#84284=CARTESIAN_POINT('Ctrl Pts',(2.49881045348,-19.5594863076,10.9363632729));
#84285=CARTESIAN_POINT('Ctrl Pts',(2.510543559,-19.4294897509,10.9122326109));
#84286=CARTESIAN_POINT('Ctrl Pts',(2.52509315654,-19.4549860554,10.9229697266));
#84287=CARTESIAN_POINT('Ctrl Pts',(2.53743184504,-19.4804823599,10.9367027854));
#84288=CARTESIAN_POINT('Ctrl Pts',(2.54730011106,-19.5054619039,10.9532408984));
#84289=CARTESIAN_POINT('Ctrl Pts',(2.55452473408,-19.52940842,10.9722767674));
#84290=CARTESIAN_POINT('Ctrl Pts',(2.55903583297,-19.5518626834,10.9934181309));
#84291=CARTESIAN_POINT('Ctrl Pts',(2.54358798483,-19.3961031493,10.9366183279));
#84292=CARTESIAN_POINT('Ctrl Pts',(2.56490210185,-19.4257202286,10.9523474783));
#84293=CARTESIAN_POINT('Ctrl Pts',(2.58262930917,-19.4553373078,10.972937153));
#84294=CARTESIAN_POINT('Ctrl Pts',(2.59620857289,-19.4840367355,10.997975939));
#84295=CARTESIAN_POINT('Ctrl Pts',(2.60527727222,-19.5109029172,11.0267904888));
#84296=CARTESIAN_POINT('Ctrl Pts',(2.60971873368,-19.5351693857,11.0585616091));
#84297=CARTESIAN_POINT('Ctrl Pts',(2.57980368735,-19.3527485635,10.9633443444));
#84298=CARTESIAN_POINT('Ctrl Pts',(2.60698188591,-19.3880359645,10.9834009889));
#84299=CARTESIAN_POINT('Ctrl Pts',(2.62854104782,-19.4233233655,11.011071838));
#84300=CARTESIAN_POINT('Ctrl Pts',(2.64323454282,-19.4570166595,11.0454386344));
#84301=CARTESIAN_POINT('Ctrl Pts',(2.65023339726,-19.4875204033,11.0850019677));
#84302=CARTESIAN_POINT('Ctrl Pts',(2.64928177187,-19.5134920611,11.1278449523));
#84303=CARTESIAN_POINT('Ctrl Pts',(2.66373575496,-19.2547159387,11.0252834944));
#84304=CARTESIAN_POINT('Ctrl Pts',(2.69872898986,-19.3050683152,11.0511073573));
#84305=CARTESIAN_POINT('Ctrl Pts',(2.72330881282,-19.3554206917,11.0910421533));
#84306=CARTESIAN_POINT('Ctrl Pts',(2.73408042005,-19.4013898853,11.1426264261));
#84307=CARTESIAN_POINT('Ctrl Pts',(2.72955068062,-19.4386199009,11.2009208948));
#84308=CARTESIAN_POINT('Ctrl Pts',(2.71098021085,-19.4644758001,11.2604631973));
#84309=CARTESIAN_POINT('Ctrl Pts',(2.78975290654,-19.1524485557,11.1182800744));
#84310=CARTESIAN_POINT('Ctrl Pts',(2.82090969201,-19.2230604651,11.1412727847));
#84311=CARTESIAN_POINT('Ctrl Pts',(2.83638207721,-19.2936723745,11.1855190018));
#84312=CARTESIAN_POINT('Ctrl Pts',(2.83135807356,-19.3541924937,11.2476786502));
#84313=CARTESIAN_POINT('Ctrl Pts',(2.80630726796,-19.3949915084,11.3177423125));
#84314=CARTESIAN_POINT('Ctrl Pts',(2.76681414133,-19.4133420624,11.3857731806));
#84315=CARTESIAN_POINT('Ctrl Pts',(2.86129530492,-19.1091646129,11.1710760494));
#84316=CARTESIAN_POINT('Ctrl Pts',(2.88687394597,-19.1898640218,11.1899522282));
#84317=CARTESIAN_POINT('Ctrl Pts',(2.89447935536,-19.2705634307,11.2331834474));
#84318=CARTESIAN_POINT('Ctrl Pts',(2.87932742318,-19.3377754042,11.2975635634));
#84319=CARTESIAN_POINT('Ctrl Pts',(2.84388765021,-19.3788647517,11.3707877234));
#84320=CARTESIAN_POINT('Ctrl Pts',(2.796245355,-19.3917000854,11.4409843867));
#84321=CARTESIAN_POINT('Ctrl Pts',(2.94208651244,-19.0824256558,11.2306973462));
#84322=CARTESIAN_POINT('Ctrl Pts',(2.95834742078,-19.1709113574,11.2426973703));
#84323=CARTESIAN_POINT('Ctrl Pts',(2.9547674495,-19.2593970589,11.2815832341));
#84324=CARTESIAN_POINT('Ctrl Pts',(2.92789987303,-19.3312626769,11.3452494815));
#84325=CARTESIAN_POINT('Ctrl Pts',(2.88323668464,-19.3712611943,11.4201106412));
#84326=CARTESIAN_POINT('Ctrl Pts',(2.83073115845,-19.3783306343,11.4925686116));
#84327=CARTESIAN_POINT('Ctrl Pts',(3.0257458739,-19.0756496396,11.2924352478));
#84328=CARTESIAN_POINT('Ctrl Pts',(3.03060872632,-19.1683851734,11.2960238755));
#84329=CARTESIAN_POINT('Ctrl Pts',(3.01410418365,-19.2611207071,11.3285668827));
#84330=CARTESIAN_POINT('Ctrl Pts',(2.97498276954,-19.334976222,11.3896852328));
#84331=CARTESIAN_POINT('Ctrl Pts',(2.92227176474,-19.372909531,11.465275844));
#84332=CARTESIAN_POINT('Ctrl Pts',(2.86720977988,-19.3749426262,11.5401119926));
#84333=CARTESIAN_POINT('',(3.0257458739,-19.0756502088,11.2924352478));
#84334=CARTESIAN_POINT('Ctrl Pts',(3.02574587389968,-19.0756502088,11.2924352478004));
#84335=CARTESIAN_POINT('Ctrl Pts',(3.00675351565961,-19.0771882002878,11.2784195019978));
#84336=CARTESIAN_POINT('Ctrl Pts',(2.98794556110458,-19.0799656124685,11.2645398401506));
#84337=CARTESIAN_POINT('Ctrl Pts',(2.96946444777136,-19.0838689703512,11.2509013765509));
#84338=CARTESIAN_POINT('Ctrl Pts',(2.95255124090799,-19.0874411739377,11.2384199771892));
#84339=CARTESIAN_POINT('Ctrl Pts',(2.93591148075212,-19.0919553471003,11.2261403726466));
#84340=CARTESIAN_POINT('Ctrl Pts',(2.91963473242905,-19.0972951829733,11.2141286590785));
#84341=CARTESIAN_POINT('Ctrl Pts',(2.90097606500497,-19.1034164437851,11.2003591662896));
#84342=CARTESIAN_POINT('Ctrl Pts',(2.88279745671413,-19.1106246716873,11.1869439416157));
#84343=CARTESIAN_POINT('Ctrl Pts',(2.86521289932878,-19.1187068763404,11.1739671072852));
#84344=CARTESIAN_POINT('Ctrl Pts',(2.85069831160009,-19.1253780632181,11.16325581122));
#84345=CARTESIAN_POINT('Ctrl Pts',(2.83658785784503,-19.1326436742646,11.1528427529497));
#84346=CARTESIAN_POINT('Ctrl Pts',(2.82292669530417,-19.140371437611,11.142761257057));
#84347=CARTESIAN_POINT('Ctrl Pts',(2.80596470462133,-19.1499663933469,11.1302438568071));
#84348=CARTESIAN_POINT('Ctrl Pts',(2.78969874364794,-19.1602717602212,11.1182401039592));
#84349=CARTESIAN_POINT('Ctrl Pts',(2.7741716633805,-19.1710306210649,11.1067816211666));
#84350=CARTESIAN_POINT('Ctrl Pts',(2.76433010714757,-19.1778499285053,11.0995188711321));
#84351=CARTESIAN_POINT('Ctrl Pts',(2.75478457692901,-19.1848513153056,11.0924745787183));
#84352=CARTESIAN_POINT('Ctrl Pts',(2.74553729325106,-19.1919708669864,11.0856503826122));
#84353=CARTESIAN_POINT('Ctrl Pts',(2.73213768965327,-19.2022873202974,11.075761908777));
#84354=CARTESIAN_POINT('Ctrl Pts',(2.7193444588255,-19.2128634993548,11.0663209183868));
#84355=CARTESIAN_POINT('Ctrl Pts',(2.70715916076948,-19.2235067787786,11.0573285627176));
#84356=CARTESIAN_POINT('Ctrl Pts',(2.69769192270529,-19.2317759618241,11.0503420473704));
#84357=CARTESIAN_POINT('Ctrl Pts',(2.68859091957648,-19.2400856488052,11.0436258015626));
#84358=CARTESIAN_POINT('Ctrl Pts',(2.67984102302334,-19.2483550306415,11.0371686610452));
#84359=CARTESIAN_POINT('Ctrl Pts',(2.66553704813159,-19.2618734796242,11.026612790439));
#84360=CARTESIAN_POINT('Ctrl Pts',(2.65214757506909,-19.2753062681188,11.0167317926194));
#84361=CARTESIAN_POINT('Ctrl Pts',(2.63954076934534,-19.2884074477262,11.0074283780573));
#84362=CARTESIAN_POINT('Ctrl Pts',(2.63452172045956,-19.2936233178166,11.0037244824381));
#84363=CARTESIAN_POINT('Ctrl Pts',(2.62962657043066,-19.2987872244217,11.0001120201687));
#84364=CARTESIAN_POINT('Ctrl Pts',(2.6248465335031,-19.3038857598675,10.9965845076172));
#84365=CARTESIAN_POINT('Ctrl Pts',(2.60806283236651,-19.3217877753653,10.9841986793659));
#84366=CARTESIAN_POINT('Ctrl Pts',(2.59269322531019,-19.3388823165721,10.972856406431));
#84367=CARTESIAN_POINT('Ctrl Pts',(2.57833633556526,-19.3547066387323,10.9622614863181));
#84368=CARTESIAN_POINT('Ctrl Pts',(2.56468487008995,-19.3697534344852,10.9521871464922));
#84369=CARTESIAN_POINT('Ctrl Pts',(2.55194665981057,-19.3836622157048,10.9427867595277));
#84370=CARTESIAN_POINT('Ctrl Pts',(2.53980373411162,-19.396024813606,10.9338256733092));
#84371=CARTESIAN_POINT('Ctrl Pts',(2.53017587314596,-19.4058268478701,10.926720623476));
#84372=CARTESIAN_POINT('Ctrl Pts',(2.52092740821589,-19.4146616173831,10.9198955559181));
#84373=CARTESIAN_POINT('Ctrl Pts',(2.51192137185923,-19.4222801308466,10.9132493927221));
#84374=CARTESIAN_POINT('Ctrl Pts',(2.50956800534002,-19.4242709238882,10.9115126844381));
#84375=CARTESIAN_POINT('Ctrl Pts',(2.50723135998009,-19.4261785010644,10.9097883158081));
#84376=CARTESIAN_POINT('Ctrl Pts',(2.50490937729373,-19.4279980029771,10.9080747677192));
#84377=CARTESIAN_POINT('Ctrl Pts',(2.49828731261426,-19.43318704225,10.9031878982596));
#84378=CARTESIAN_POINT('Ctrl Pts',(2.49177954925272,-19.4376614176956,10.8983853790159));
#84379=CARTESIAN_POINT('Ctrl Pts',(2.48534852651507,-19.4413044184337,10.8936394922355));
#84380=CARTESIAN_POINT('Ctrl Pts',(2.48315653562045,-19.44254612209,10.8920218738514));
#84381=CARTESIAN_POINT('Ctrl Pts',(2.48097305807628,-19.4436916418333,10.8904105380807));
#84382=CARTESIAN_POINT('Ctrl Pts',(2.47879645562,-19.4447370035,10.8888042759));
#84383=CARTESIAN_POINT('Origin',(2.84896336685575,-19.0776976706847,11.5322131892507));
#84384=CARTESIAN_POINT('Ctrl Pts',(3.02574587396,-19.0756502088,11.2924352478));
#84385=CARTESIAN_POINT('Ctrl Pts',(3.03060876213,-19.1683856419,11.2960239029));
#84386=CARTESIAN_POINT('Ctrl Pts',(3.0141042599,-19.261121075,11.3285669311));
#84387=CARTESIAN_POINT('Ctrl Pts',(2.97498288462,-19.3349765133,11.3896852899));
#84388=CARTESIAN_POINT('Ctrl Pts',(2.9222719047,-19.3729097939,11.465275899));
#84389=CARTESIAN_POINT('Ctrl Pts',(2.86720992778,-19.3749429031,11.5401120401));
#84390=CARTESIAN_POINT('Ctrl Pts',(3.03447355616,-19.0749433453,11.2988759949));
#84391=CARTESIAN_POINT('Ctrl Pts',(3.03813896473,-19.1681049521,11.3015809487));
#84392=CARTESIAN_POINT('Ctrl Pts',(3.02028592653,-19.2612665588,11.3334449681));
#84393=CARTESIAN_POINT('Ctrl Pts',(2.97989655367,-19.3353233942,11.3942703053));
#84394=CARTESIAN_POINT('Ctrl Pts',(2.92636073645,-19.3730546128,11.4699120931));
#84395=CARTESIAN_POINT('Ctrl Pts',(2.87104425856,-19.3745894729,11.5449824418));
#84396=CARTESIAN_POINT('Ctrl Pts',(3.04321296595,-19.0744719442,11.3053253965));
#84397=CARTESIAN_POINT('Ctrl Pts',(3.04566841653,-19.1680282232,11.3071374404));
#84398=CARTESIAN_POINT('Ctrl Pts',(3.02645347241,-19.2615845022,11.3383144504));
#84399=CARTESIAN_POINT('Ctrl Pts',(2.9847889853,-19.3358150142,11.3988454565));
#84400=CARTESIAN_POINT('Ctrl Pts',(2.93043564473,-19.3733247573,11.4745447401));
#84401=CARTESIAN_POINT('Ctrl Pts',(2.87488373803,-19.3743537743,11.5498593869));
#84402=CARTESIAN_POINT('Ctrl Pts',(3.05195820325,-19.0742362318,11.3117790986));
#84403=CARTESIAN_POINT('Ctrl Pts',(3.0531916857,-19.1681548312,11.3126893695));
#84404=CARTESIAN_POINT('Ctrl Pts',(3.03260202102,-19.2620734306,11.3431715971));
#84405=CARTESIAN_POINT('Ctrl Pts',(2.98965603461,-19.3364495577,11.4034071424));
#84406=CARTESIAN_POINT('Ctrl Pts',(2.93449336502,-19.3737189989,11.4791704265));
#84407=CARTESIAN_POINT('Ctrl Pts',(2.87872577363,-19.3742359202,11.5547395826));
#84408=CARTESIAN_POINT('Ctrl Pts',(3.06070337749,-19.0742362041,11.3182327542));
#84409=CARTESIAN_POINT('Ctrl Pts',(3.06070341502,-19.1684838804,11.3182327825));
#84410=CARTESIAN_POINT('Ctrl Pts',(3.0387268402,-19.2627315566,11.3480127241));
#84411=CARTESIAN_POINT('Ctrl Pts',(2.9944937393,-19.3372249046,11.4079518654));
#84412=CARTESIAN_POINT('Ctrl Pts',(2.93853076799,-19.3742358919,11.4837858067));
#84413=CARTESIAN_POINT('Ctrl Pts',(2.88256777785,-19.3742359083,11.5596197419));
#84414=CARTESIAN_POINT('',(3.06070337744086,-19.0742359088556,11.3182327542666));
#84415=CARTESIAN_POINT('Origin',(3.06701733419236,-19.6773931794005,11.3228922010275));
#84416=CARTESIAN_POINT('Origin',(2.88382729685578,-19.0763575401806,11.5579128499525));
#84417=CARTESIAN_POINT('Origin',(4.88509763285,-19.0742356128,13.0374220375));
#84418=CARTESIAN_POINT('',(5.27647385588,-19.0742356128,12.9533996668));
#84419=CARTESIAN_POINT('Origin',(2.3,-16.6742356128,10.7568582774));
#84420=CARTESIAN_POINT('',(7.49224433422,-16.6742356128,14.5885665792));
#84421=CARTESIAN_POINT('Origin',(0.,-18.1642356128,0.));
#84422=CARTESIAN_POINT('',(-0.213764216279,-20.8742356128,15.3985163201));
#84423=CARTESIAN_POINT('',(-0.213764216279,-16.6742356128,15.3985163201));
#84424=CARTESIAN_POINT('',(-0.213764216279,-18.7742356128,15.3985163201));
#84425=CARTESIAN_POINT('Origin',(0.,-16.6742356128,0.));
#84426=CARTESIAN_POINT('Origin',(0.,-20.8742356128,0.));
#84427=CARTESIAN_POINT('Origin',(-0.212376136953,-18.7742356128,15.2985259544));
#84428=CARTESIAN_POINT('',(-0.30759325472,-20.8742356128,15.3290824673));
#84429=CARTESIAN_POINT('Origin',(-0.212376136953,-20.8742356128,15.2985259544));
#84430=CARTESIAN_POINT('',(-0.30759325472,-16.6742356128,15.3290824673));
#84431=CARTESIAN_POINT('',(-0.30759325472,-18.7742356128,15.3290824673));
#84432=CARTESIAN_POINT('Origin',(-0.212376136952999,-16.6742356128,15.2985259544));
#84433=CARTESIAN_POINT('Origin',(-1.82391441117,-19.3742356128,10.6040757126));
#84434=CARTESIAN_POINT('',(-1.188848049,-20.8742356128,12.5830053333));
#84435=CARTESIAN_POINT('',(-0.748220651862,-20.8742356128,13.9560439003));
#84436=CARTESIAN_POINT('',(-1.188848049,-16.6742356128,12.5830053333));
#84437=CARTESIAN_POINT('',(-1.188848049,-18.7742356128,12.5830053333));
#84438=CARTESIAN_POINT('',(-0.30759325472,-16.6742356128,15.3290824673));
#84439=CARTESIAN_POINT('Origin',(-2.12507249391,-18.7742356128,11.3019496944));
#84440=CARTESIAN_POINT('',(-2.60115808275,-19.6742356128,11.4547322592));
#84441=CARTESIAN_POINT('',(-2.60115808275,-20.5742356128,11.4547322592));
#84442=CARTESIAN_POINT('',(-2.60115808275,-18.7742356128,11.4547322592));
#84443=CARTESIAN_POINT('Origin',(-2.12507249391,-19.6742356128,11.3019496944));
#84444=CARTESIAN_POINT('Origin',(-2.12507249391,-20.5742356128,11.3019496944));
#84445=CARTESIAN_POINT('Ctrl Pts',(-2.60115808268513,-20.5742356128,11.454732259376));
#84446=CARTESIAN_POINT('Ctrl Pts',(-2.68798680911532,-20.5742356128,11.1841653569836));
#84447=CARTESIAN_POINT('Ctrl Pts',(-2.49996449209242,-20.5742356128,10.9711083582602));
#84448=CARTESIAN_POINT('Ctrl Pts',(-2.31194217506952,-20.5742356128,10.7580513595367));
#84449=CARTESIAN_POINT('Ctrl Pts',(-2.03267803763261,-20.5742356128,10.8105605772543));
#84450=CARTESIAN_POINT('Ctrl Pts',(-2.60115808268513,-20.6984996815293,
11.454732259376));
#84451=CARTESIAN_POINT('Ctrl Pts',(-2.68798680911532,-20.6984996815293,
11.1841653569836));
#84452=CARTESIAN_POINT('Ctrl Pts',(-2.49996449209242,-20.6984996815293,
10.9711083582602));
#84453=CARTESIAN_POINT('Ctrl Pts',(-2.31194217506952,-20.6984996815293,
10.7580513595367));
#84454=CARTESIAN_POINT('Ctrl Pts',(-2.03267803763261,-20.6984996815293,
10.8105605772543));
#84455=CARTESIAN_POINT('Ctrl Pts',(-2.51749273834894,-20.7863676471769,
11.4278828730289));
#84456=CARTESIAN_POINT('Ctrl Pts',(-2.58906253767373,-20.7863676471769,
11.2048642972156));
#84457=CARTESIAN_POINT('Ctrl Pts',(-2.43408249764367,-20.7863676471769,
11.0292490685892));
#84458=CARTESIAN_POINT('Ctrl Pts',(-2.27910245761361,-20.7863676471769,
10.8536338399628));
#84459=CARTESIAN_POINT('Ctrl Pts',(-2.04891506345624,-20.7863676471769,
10.8969153014013));
#84460=CARTESIAN_POINT('Ctrl Pts',(-2.43382739401276,-20.8742356128246,
11.4010334866819));
#84461=CARTESIAN_POINT('Ctrl Pts',(-2.49013826623214,-20.8742356128246,
11.2255632374475));
#84462=CARTESIAN_POINT('Ctrl Pts',(-2.36820050319492,-20.8742356128246,
11.0873897789182));
#84463=CARTESIAN_POINT('Ctrl Pts',(-2.24626274015771,-20.8742356128246,
10.9492163203888));
#84464=CARTESIAN_POINT('Ctrl Pts',(-2.06515208927988,-20.8742356128246,
10.9832700255484));
#84465=CARTESIAN_POINT('Ctrl Pts',(-2.3155067293636,-20.8742356128,11.3630627203723));
#84466=CARTESIAN_POINT('Ctrl Pts',(-2.35023821992538,-20.8742356128,11.2548359594474));
#84467=CARTESIAN_POINT('Ctrl Pts',(-2.27502929313851,-20.8742356128,11.1696131599833));
#84468=CARTESIAN_POINT('Ctrl Pts',(-2.19982036635165,-20.8742356128,11.0843903605192));
#84469=CARTESIAN_POINT('Ctrl Pts',(-2.08811471141,-20.8742356128,11.1053940476));
#84470=CARTESIAN_POINT('',(-2.31550672945,-20.8742356128,11.3630627204));
#84471=CARTESIAN_POINT('Origin',(-2.31550672945,-20.5742356128,11.3630627204));
#84472=CARTESIAN_POINT('',(-2.08811471141,-20.8742356128,11.1053940476));
#84473=CARTESIAN_POINT('Origin',(-2.08811471141,-20.5742356128,11.1053940476));
#84474=CARTESIAN_POINT('Origin',(-2.12507249391,-20.8742356128,11.3019496944));
#84475=CARTESIAN_POINT('Origin',(0.,-20.8742356128,0.));
#84476=CARTESIAN_POINT('',(-1.59732923672,-20.8742356128,13.6009748472));
#84477=CARTESIAN_POINT('Origin',(7.1054273576E-15,-20.8742356128,4.4408920985E-16));
#84478=CARTESIAN_POINT('',(-1.08495132067,-20.8742356128,12.4528262106));
#84479=CARTESIAN_POINT('Origin',(0.,-20.8742356128,0.));
#84480=CARTESIAN_POINT('Origin',(-1.09363093124,-20.8742356128,12.5524488203));
#84481=CARTESIAN_POINT('Origin',(-1.59732923672,-20.5742356128,13.6009748472));
#84482=CARTESIAN_POINT('',(-1.94732913984,-20.5742356128,13.4921279379));
#84483=CARTESIAN_POINT('Origin',(-2.77608558884,-19.3742356128,10.9096408422));
#84484=CARTESIAN_POINT('',(-2.11321243752,-16.6742356128,12.9752191692));
#84485=CARTESIAN_POINT('',(-1.02442996075,-16.6742356128,16.3679730955));
#84486=CARTESIAN_POINT('',(-2.11321243436594,-19.0742355019,12.9752191789979));
#84487=CARTESIAN_POINT('',(-2.11321243752,-18.7742356128,12.9752191692));
#84488=CARTESIAN_POINT('',(-2.30669397219695,-19.6742353176957,12.3723115634183));
#84489=CARTESIAN_POINT('Origin',(-2.30675324894277,-19.0740005634869,12.37212685105));
#84490=CARTESIAN_POINT('',(-1.91660155908,-19.6742356128,13.5878781199));
#84491=CARTESIAN_POINT('Origin',(-2.39886379082,-18.7742356128,13.066888708));
#84492=CARTESIAN_POINT('',(-2.576999541,-16.6742356128,12.8255017686));
#84493=CARTESIAN_POINT('Origin',(-2.39886379082,-16.6742356128,13.066888708));
#84494=CARTESIAN_POINT('',(-2.57699954471655,-19.074235612975,12.8255017742882));
#84495=CARTESIAN_POINT('',(-2.576999541,-18.0242356128,12.8255017686));
#84496=CARTESIAN_POINT('Origin',(-2.39886379082,-19.07423555735,13.066888708));
#84497=CARTESIAN_POINT('Origin',(-1.40932124909,-16.6742356128,11.9637929743));
#84498=CARTESIAN_POINT('',(-2.576999541,-16.6742356128,12.8255017686));
#84499=CARTESIAN_POINT('',(-4.11574708991,-19.0742356128,13.9610476671));
#84500=CARTESIAN_POINT('Origin',(-1.09363093124,-18.7742356128,12.5524488203));
#84501=CARTESIAN_POINT('',(-1.08495132067,-16.6742356128,12.4528262106));
#84502=CARTESIAN_POINT('',(-1.08495132067,-18.7742356128,12.4528262106));
#84503=CARTESIAN_POINT('Origin',(-1.09363093124,-16.6742356128,12.5524488203));
#84504=CARTESIAN_POINT('Origin',(0.,-18.1642356128,0.));
#84505=CARTESIAN_POINT('Origin',(-3.01622616368355E-13,-16.6742356128,-1.06581410364015E-13));
#84506=CARTESIAN_POINT('Origin',(7.1054273576E-15,-20.5742356128,4.4408920985E-16));
#84507=CARTESIAN_POINT('Ctrl Pts',(-2.11321243145,-19.0742355019,12.9752191881));
#84508=CARTESIAN_POINT('Ctrl Pts',(-2.14797389499,-19.0742355464,12.8668990358));
#84509=CARTESIAN_POINT('Ctrl Pts',(-2.23407965787,-19.0742355909,12.7750559918));
#84510=CARTESIAN_POINT('Ctrl Pts',(-2.36191078436,-19.0742356216,12.7337901943));
#84511=CARTESIAN_POINT('Ctrl Pts',(-2.48546463599,-19.0742356274,12.7579519823));
#84512=CARTESIAN_POINT('Ctrl Pts',(-2.57699954053,-19.0742356132,12.82550178));
#84513=CARTESIAN_POINT('Ctrl Pts',(-2.11321242505,-19.1612543019,12.975219208));
#84514=CARTESIAN_POINT('Ctrl Pts',(-2.14797389154,-19.1438426701,12.8668990456));
#84515=CARTESIAN_POINT('Ctrl Pts',(-2.23407965879,-19.1264310382,12.7750559919));
#84516=CARTESIAN_POINT('Ctrl Pts',(-2.36191078991,-19.1144387816,12.7337901893));
#84517=CARTESIAN_POINT('Ctrl Pts',(-2.48546464338,-19.112181627,12.7579519792));
#84518=CARTESIAN_POINT('Ctrl Pts',(-2.57699954662,-19.1177450086,12.825501783));
#84519=CARTESIAN_POINT('Ctrl Pts',(-2.11829710106,-19.248306695,12.9593748545));
#84520=CARTESIAN_POINT('Ctrl Pts',(-2.15187949666,-19.2134621794,12.8547287833));
#84521=CARTESIAN_POINT('Ctrl Pts',(-2.23632644193,-19.1786176639,12.7664058619));
#84522=CARTESIAN_POINT('Ctrl Pts',(-2.3624655556,-19.1546253192,12.7270177415));
#84523=CARTESIAN_POINT('Ctrl Pts',(-2.48537378308,-19.1501233479,12.7505876284));
#84524=CARTESIAN_POINT('Ctrl Pts',(-2.57740280629,-19.1612710822,12.8160010902));
#84525=CARTESIAN_POINT('Ctrl Pts',(-2.1284939378,-19.3306965513,12.9276005023));
#84526=CARTESIAN_POINT('Ctrl Pts',(-2.15970428933,-19.2801076689,12.8303459527));
#84527=CARTESIAN_POINT('Ctrl Pts',(-2.24081540097,-19.2295187866,12.7491052593));
#84528=CARTESIAN_POINT('Ctrl Pts',(-2.36355540449,-19.1943772592,12.7134885287));
#84529=CARTESIAN_POINT('Ctrl Pts',(-2.48517594342,-19.1870911735,12.7358510743));
#84530=CARTESIAN_POINT('Ctrl Pts',(-2.5782116467,-19.2024661641,12.796948158));
#84531=CARTESIAN_POINT('Ctrl Pts',(-2.16109563614,-19.4975344726,12.8260103845));
#84532=CARTESIAN_POINT('Ctrl Pts',(-2.18524115037,-19.4177125414,12.7507705807));
#84533=CARTESIAN_POINT('Ctrl Pts',(-2.25630596622,-19.3378906101,12.6905878411));
#84534=CARTESIAN_POINT('Ctrl Pts',(-2.36852442786,-19.2809552961,12.6666894295));
#84535=CARTESIAN_POINT('Ctrl Pts',(-2.48552961718,-19.2657636574,12.6866327467));
#84536=CARTESIAN_POINT('Ctrl Pts',(-2.58079725879,-19.2858849393,12.7360320273));
#84537=CARTESIAN_POINT('Ctrl Pts',(-2.21060765367,-19.6106096232,12.6717260389));
#84538=CARTESIAN_POINT('Ctrl Pts',(-2.22542521735,-19.5162497602,12.6255530347));
#84539=CARTESIAN_POINT('Ctrl Pts',(-2.28292923485,-19.4218898972,12.5930787142));
#84540=CARTESIAN_POINT('Ctrl Pts',(-2.38019466467,-19.3518501373,12.5859609253));
#84541=CARTESIAN_POINT('Ctrl Pts',(-2.48889752329,-19.3268991358,12.6060157728));
#84542=CARTESIAN_POINT('Ctrl Pts',(-2.58472445083,-19.3424227485,12.6435184464));
#84543=CARTESIAN_POINT('Ctrl Pts',(-2.24157751669,-19.6529683202,12.5752208815));
#84544=CARTESIAN_POINT('Ctrl Pts',(-2.25115370883,-19.5552809276,12.5453805297));
#84545=CARTESIAN_POINT('Ctrl Pts',(-2.30089868661,-19.4575935349,12.5284309064));
#84546=CARTESIAN_POINT('Ctrl Pts',(-2.3892638599,-19.383367284,12.5313593346));
#84547=CARTESIAN_POINT('Ctrl Pts',(-2.49223570108,-19.3530489966,12.553066847));
#84548=CARTESIAN_POINT('Ctrl Pts',(-2.58718049198,-19.36360193,12.5856515981));
#84549=CARTESIAN_POINT('Ctrl Pts',(-2.27413005219,-19.6742347534,12.47378396));
#84550=CARTESIAN_POINT('Ctrl Pts',(-2.2787229772,-19.5767604829,12.4594719462));
#84551=CARTESIAN_POINT('Ctrl Pts',(-2.32096970846,-19.4792862125,12.4572435686));
#84552=CARTESIAN_POINT('Ctrl Pts',(-2.40043923714,-19.4036435793,12.4702692455));
#84553=CARTESIAN_POINT('Ctrl Pts',(-2.49695035202,-19.3691668211,12.4950419018));
#84554=CARTESIAN_POINT('Ctrl Pts',(-2.58976267699,-19.3742352023,12.5248266884));
#84555=CARTESIAN_POINT('Ctrl Pts',(-2.30669397214,-19.6742350234,12.3723115634));
#84556=CARTESIAN_POINT('Ctrl Pts',(-2.30669398607,-19.579987326,12.3723115185));
#84557=CARTESIAN_POINT('Ctrl Pts',(-2.34193483095,-19.4857396287,12.3836207521));
#84558=CARTESIAN_POINT('Ctrl Pts',(-2.41286534931,-19.4112462739,12.4063833145));
#84559=CARTESIAN_POINT('Ctrl Pts',(-2.50260539009,-19.374235302,12.4351821369));
#84560=CARTESIAN_POINT('Ctrl Pts',(-2.5923454193,-19.3742353183,12.4639809751));
#84561=CARTESIAN_POINT('',(-2.59234532544548,-19.3742354655498,12.4639811022925));
#84562=CARTESIAN_POINT('Origin',(-2.59234284839811,-19.0742335195363,12.4640390914794));
#84563=CARTESIAN_POINT('Origin',(-2.59032547075745,-19.6721137326376,12.4633329753833));
#84564=CARTESIAN_POINT('Origin',(-4.29388284009,-19.0742356128,13.7196607277));
#84565=CARTESIAN_POINT('',(-4.42080718383,-19.3742356128,13.8133267862));
#84566=CARTESIAN_POINT('Ctrl Pts',(-2.03267803765,-19.6742356128,10.8105605773));
#84567=CARTESIAN_POINT('Ctrl Pts',(-2.03267803765,-19.6742356128,10.8105605773));
#84568=CARTESIAN_POINT('Ctrl Pts',(-2.03267803765,-19.6742356128,10.8105605773));
#84569=CARTESIAN_POINT('Ctrl Pts',(-2.03267803765,-19.6742356128,10.8105605773));
#84570=CARTESIAN_POINT('Ctrl Pts',(-2.03267803765,-19.6742356128,10.8105605773));
#84571=CARTESIAN_POINT('Ctrl Pts',(-2.03267803765,-19.6742356128,10.8105605773));
#84572=CARTESIAN_POINT('Ctrl Pts',(-2.05894886759,-19.6259152622,10.8056234563));
#84573=CARTESIAN_POINT('Ctrl Pts',(-2.06734285289645,-19.6307029517914,
10.8040622488486));
#84574=CARTESIAN_POINT('Ctrl Pts',(-2.07573485238451,-19.6354906438259,
10.802501411656));
#84575=CARTESIAN_POINT('Ctrl Pts',(-2.08416049881215,-19.6403007330939,
10.8009343190103));
#84576=CARTESIAN_POINT('Ctrl Pts',(-2.09265549117115,-19.6451556121481,
10.7993543328483));
#84577=CARTESIAN_POINT('Ctrl Pts',(-2.10125198398,-19.6500754685,10.7977554742));
#84578=CARTESIAN_POINT('Ctrl Pts',(-2.0870381674,-19.5762206261,10.8001977615));
#84579=CARTESIAN_POINT('Ctrl Pts',(-2.1034870056,-19.586196795,10.7970191759));
#84580=CARTESIAN_POINT('Ctrl Pts',(-2.1202364023,-19.596172964,10.7953959482));
#84581=CARTESIAN_POINT('Ctrl Pts',(-2.13714159915,-19.6060613319,10.795356101));
#84582=CARTESIAN_POINT('Ctrl Pts',(-2.15405252281,-19.6157741162,10.796899988));
#84583=CARTESIAN_POINT('Ctrl Pts',(-2.17082159168,-19.6252281195,10.8000002758));
#84584=CARTESIAN_POINT('',(-2.17082156040968,-19.6252281736439,10.8000002868487));
#84585=CARTESIAN_POINT('Origin',(-2.14395737416692,-19.5762206558258,11.0947491984194));
#84586=CARTESIAN_POINT('Origin',(-2.12965350097472,-20.4077533044672,22.8291553975983));
#84587=CARTESIAN_POINT('Origin',(-2.12507249391,-19.6742356128,11.3019496944));
#84588=CARTESIAN_POINT('',(-2.86720989586223,-19.3749426183134,11.5401120066422));
#84589=CARTESIAN_POINT('',(-2.49881049555799,-19.5594863294135,10.9363632311538));
#84590=CARTESIAN_POINT('Ctrl Pts',(-2.86720983507867,-19.3749426241618,
11.5401119175781));
#84591=CARTESIAN_POINT('Ctrl Pts',(-2.85794042079669,-19.3758035323584,
11.5280309646887));
#84592=CARTESIAN_POINT('Ctrl Pts',(-2.84902123015658,-19.3774209880109,
11.5158588629276));
#84593=CARTESIAN_POINT('Ctrl Pts',(-2.84047942817318,-19.3796414951876,
11.5036349549176));
#84594=CARTESIAN_POINT('Ctrl Pts',(-2.83321900805626,-19.3815288972846,
11.4932447927721));
#84595=CARTESIAN_POINT('Ctrl Pts',(-2.82622945323719,-19.3838515544305,
11.4828167136796));
#84596=CARTESIAN_POINT('Ctrl Pts',(-2.8194993801726,-19.3865184502639,11.4723681225865));
#84597=CARTESIAN_POINT('Ctrl Pts',(-2.81420528569115,-19.3886163173121,
11.4641489208165));
#84598=CARTESIAN_POINT('Ctrl Pts',(-2.80919033263759,-19.3908762665008,
11.4560955502276));
#84599=CARTESIAN_POINT('Ctrl Pts',(-2.80431578664454,-19.393298788564,11.4480166929727));
#84600=CARTESIAN_POINT('Ctrl Pts',(-2.79896751651414,-19.3959567391525,
11.4391527062535));
#84601=CARTESIAN_POINT('Ctrl Pts',(-2.79378806281648,-19.398811001587,11.4302582445943));
#84602=CARTESIAN_POINT('Ctrl Pts',(-2.78861324655873,-19.4019174204448,
11.4210514196961));
#84603=CARTESIAN_POINT('Ctrl Pts',(-2.78545482629351,-19.4038134058835,
11.4154320854264));
#84604=CARTESIAN_POINT('Ctrl Pts',(-2.7822985437128,-19.4058043481332,11.4096958180335));
#84605=CARTESIAN_POINT('Ctrl Pts',(-2.77911013539142,-19.407909997777,11.4037733452569));
#84606=CARTESIAN_POINT('Ctrl Pts',(-2.77158501758046,-19.4128796440837,
11.3897954287283));
#84607=CARTESIAN_POINT('Ctrl Pts',(-2.76424601720805,-19.4182523799667,
11.3754630858337));
#84608=CARTESIAN_POINT('Ctrl Pts',(-2.7570614996732,-19.4238657810566,11.36086736767));
#84609=CARTESIAN_POINT('Ctrl Pts',(-2.74942930372377,-19.4298289618621,
11.3453621677025));
#84610=CARTESIAN_POINT('Ctrl Pts',(-2.74197085693992,-19.4360617673903,
11.3295591468001));
#84611=CARTESIAN_POINT('Ctrl Pts',(-2.73459878949584,-19.4423636392851,
11.3136025882499));
#84612=CARTESIAN_POINT('Ctrl Pts',(-2.72722672205175,-19.44866551118,11.2976460296998));
#84613=CARTESIAN_POINT('Ctrl Pts',(-2.71993933440834,-19.4550345102455,
11.2815360940162));
#84614=CARTESIAN_POINT('Ctrl Pts',(-2.71261970911949,-19.4612950594277,
11.2654542758801));
#84615=CARTESIAN_POINT('Ctrl Pts',(-2.71002476272399,-19.4635145431981,
11.2597529654498));
#84616=CARTESIAN_POINT('Ctrl Pts',(-2.70742557195454,-19.4657207814632,
11.2540555471212));
#84617=CARTESIAN_POINT('Ctrl Pts',(-2.70481758415677,-19.4679080407443,
11.2483697897688));
#84618=CARTESIAN_POINT('Ctrl Pts',(-2.69382295878758,-19.4771289797386,
11.2244000564427));
#84619=CARTESIAN_POINT('Ctrl Pts',(-2.68254235207586,-19.4861201933903,
11.2003269705257));
#84620=CARTESIAN_POINT('Ctrl Pts',(-2.67024406741993,-19.4948015724197,
11.1759168881403));
#84621=CARTESIAN_POINT('Ctrl Pts',(-2.66232922858485,-19.5003886699545,
11.1602072283432));
#84622=CARTESIAN_POINT('Ctrl Pts',(-2.65399319767008,-19.5058487044407,
11.1443575461923));
#84623=CARTESIAN_POINT('Ctrl Pts',(-2.64502082159231,-19.5111479090135,
11.128321463775));
#84624=CARTESIAN_POINT('Ctrl Pts',(-2.63719041285278,-19.5157726524973,
11.1143263883546));
#84625=CARTESIAN_POINT('Ctrl Pts',(-2.62887529120171,-19.5202752745558,
11.1001890144411));
#84626=CARTESIAN_POINT('Ctrl Pts',(-2.61991334581597,-19.5246145322958,
11.085897506031));
#84627=CARTESIAN_POINT('Ctrl Pts',(-2.60762140935298,-19.5305661285332,
11.0662957001981));
#84628=CARTESIAN_POINT('Ctrl Pts',(-2.59474731925378,-19.5358925855985,
11.0474288525336));
#84629=CARTESIAN_POINT('Ctrl Pts',(-2.58122541698925,-19.5405628662028,
11.0293309608975));
#84630=CARTESIAN_POINT('Ctrl Pts',(-2.56761875949697,-19.5452624201067,
11.0111196317512));
#84631=CARTESIAN_POINT('Ctrl Pts',(-2.55335737438676,-19.5492990339476,
10.9936859098735));
#84632=CARTESIAN_POINT('Ctrl Pts',(-2.53841802417724,-19.5526197567307,
10.9770558858659));
#84633=CARTESIAN_POINT('Ctrl Pts',(-2.52570452319816,-19.5554457171482,
10.962903608589));
#84634=CARTESIAN_POINT('Ctrl Pts',(-2.51250080576092,-19.5577533139566,
10.9493329054815));
#84635=CARTESIAN_POINT('Ctrl Pts',(-2.49881045387518,-19.5594863052749,
10.9363632719275));
#84636=CARTESIAN_POINT('Ctrl Pts',(-2.49881057490516,-19.5594863753635,
10.9363631535376));
#84637=CARTESIAN_POINT('Ctrl Pts',(-2.48189321230394,-19.5616279484725,
10.9203363430907));
#84638=CARTESIAN_POINT('Ctrl Pts',(-2.46385740336138,-19.5640380169532,
10.9055168337234));
#84639=CARTESIAN_POINT('Ctrl Pts',(-2.44489566614884,-19.5667483129689,
10.8920449861814));
#84640=CARTESIAN_POINT('Ctrl Pts',(-2.43732153123321,-19.5678309219859,
10.8866637497629));
#84641=CARTESIAN_POINT('Ctrl Pts',(-2.42960011206188,-19.5689617226717,
10.8814972313772));
#84642=CARTESIAN_POINT('Ctrl Pts',(-2.42174516216224,-19.5701438338236,
10.8765530967493));
#84643=CARTESIAN_POINT('Ctrl Pts',(-2.40085003502617,-19.5732883940211,
10.8634010941334));
#84644=CARTESIAN_POINT('Ctrl Pts',(-2.37900647676366,-19.576794631005,10.851824341331));
#84645=CARTESIAN_POINT('Ctrl Pts',(-2.35649261223513,-19.5807393452508,
10.8419423005584));
#84646=CARTESIAN_POINT('Ctrl Pts',(-2.34862227224651,-19.5821183285094,
10.8384877616646));
#84647=CARTESIAN_POINT('Ctrl Pts',(-2.34067012527774,-19.5835511190477,
10.8352399234243));
#84648=CARTESIAN_POINT('Ctrl Pts',(-2.33264814825159,-19.5850416728663,
10.8322025543555));
#84649=CARTESIAN_POINT('Ctrl Pts',(-2.31659588540332,-19.5880243243507,
10.8261246702505));
#84650=CARTESIAN_POINT('Ctrl Pts',(-2.30026230264194,-19.5912378419647,
10.8208866290135));
#84651=CARTESIAN_POINT('Ctrl Pts',(-2.28377162562935,-19.5947588383549,
10.8165105761754));
#84652=CARTESIAN_POINT('Ctrl Pts',(-2.27121598386632,-19.5974396482021,
10.8131787450001));
#84653=CARTESIAN_POINT('Ctrl Pts',(-2.25856722444482,-19.6002954429563,
10.8103468853162));
#84654=CARTESIAN_POINT('Ctrl Pts',(-2.24588993027475,-19.6033758386239,
10.8080180359072));
#84655=CARTESIAN_POINT('Ctrl Pts',(-2.24191676821981,-19.6043412584538,
10.8072881564882));
#84656=CARTESIAN_POINT('Ctrl Pts',(-2.23794098212931,-19.6053290264032,
10.8066076133275));
#84657=CARTESIAN_POINT('Ctrl Pts',(-2.23396517538284,-19.6063416556388,
10.8059762733988));
#84658=CARTESIAN_POINT('Ctrl Pts',(-2.22528476776626,-19.6085525363706,
10.8045978643677));
#84659=CARTESIAN_POINT('Ctrl Pts',(-2.21660055076944,-19.6108808098985,
10.8034535416467));
#84660=CARTESIAN_POINT('Ctrl Pts',(-2.20794528221928,-19.6133598336687,
10.8025389750823));
#84661=CARTESIAN_POINT('Ctrl Pts',(-2.19929001366913,-19.6158388574389,
10.8016244085179));
#84662=CARTESIAN_POINT('Ctrl Pts',(-2.19066341384667,-19.6184721846969,
10.8009406384501));
#84663=CARTESIAN_POINT('Ctrl Pts',(-2.18211944040195,-19.6213167700468,
10.8004807714098));
#84664=CARTESIAN_POINT('Ctrl Pts',(-2.17833689867943,-19.622576109491,10.8002771815604));
#84665=CARTESIAN_POINT('Ctrl Pts',(-2.17456948674399,-19.6238775578788,
10.800117324421));
#84666=CARTESIAN_POINT('Ctrl Pts',(-2.17082158489314,-19.6252282072342,
10.800000304529));
#84667=CARTESIAN_POINT('Origin',(-2.88680943605,-19.6742356128,11.5464017981));
#84668=CARTESIAN_POINT('Origin',(-2.20225291238,-19.6742356128,13.6795476588));
#84669=CARTESIAN_POINT('',(-2.8825676448599,-19.3742356866711,11.5596196699867));
#84670=CARTESIAN_POINT('Ctrl Pts',(-2.88256762736,-19.3742356128,11.5596196937));
#84671=CARTESIAN_POINT('Ctrl Pts',(-2.87949410326,-19.3742359194,11.555715524));
#84672=CARTESIAN_POINT('Ctrl Pts',(-2.87642049893,-19.3743066351,11.5518113974));
#84673=CARTESIAN_POINT('Ctrl Pts',(-2.87334791066,-19.3744480562,11.5479085637));
#84674=CARTESIAN_POINT('Ctrl Pts',(-2.87027737467,-19.3746601605,11.544008339));
#84675=CARTESIAN_POINT('Ctrl Pts',(-2.86720992947,-19.3749426154,11.5401120406));
#84676=CARTESIAN_POINT('',(-2.7374564764,-19.3742356128,12.011800398));
#84677=CARTESIAN_POINT('Origin',(0.,-19.3742356128,0.));
#84678=CARTESIAN_POINT('',(-4.88509763285,-19.3742356128,13.0374220375));
#84679=CARTESIAN_POINT('Ctrl Pts',(-2.47879655924,-19.4447372417,10.8888042378));
#84680=CARTESIAN_POINT('Ctrl Pts',(-2.4861493729,-19.4683844343,10.8942303744));
#84681=CARTESIAN_POINT('Ctrl Pts',(-2.49191208452,-19.4920316269,10.9018112135));
#84682=CARTESIAN_POINT('Ctrl Pts',(-2.49597515407,-19.5153269748,10.9114662072));
#84683=CARTESIAN_POINT('Ctrl Pts',(-2.49827725138,-19.5379188455,10.9230496178));
#84684=CARTESIAN_POINT('Ctrl Pts',(-2.49881059449,-19.5594864256,10.9363632033));
#84685=CARTESIAN_POINT('Ctrl Pts',(-2.44089425171,-19.4520187736,10.8608335));
#84686=CARTESIAN_POINT('Ctrl Pts',(-2.44963136368,-19.4748973849,10.8662112305));
#84687=CARTESIAN_POINT('Ctrl Pts',(-2.45702223689,-19.4977759963,10.8738380918));
#84688=CARTESIAN_POINT('Ctrl Pts',(-2.46293957656,-19.5203232432,10.8836363306));
#84689=CARTESIAN_POINT('Ctrl Pts',(-2.4672956606,-19.5422079505,10.8954618457));
#84690=CARTESIAN_POINT('Ctrl Pts',(-2.47004984489,-19.5631271909,10.9091164123));
#84691=CARTESIAN_POINT('Ctrl Pts',(-2.40004991429,-19.4606048121,10.8375867107));
#84692=CARTESIAN_POINT('Ctrl Pts',(-2.41019998813,-19.4825787168,10.8426296142));
#84693=CARTESIAN_POINT('Ctrl Pts',(-2.41925749864,-19.5045526216,10.8499715311));
#84694=CARTESIAN_POINT('Ctrl Pts',(-2.42707877395,-19.5262185084,10.8595420691));
#84695=CARTESIAN_POINT('Ctrl Pts',(-2.43355105359,-19.5472685228,10.8712051552));
#84696=CARTESIAN_POINT('Ctrl Pts',(-2.43860186298,-19.5674202148,10.8847702011));
#84697=CARTESIAN_POINT('Ctrl Pts',(-2.35714755108,-19.4705790255,10.8194836801));
#84698=CARTESIAN_POINT('Ctrl Pts',(-2.36865799258,-19.4915042786,10.8238986479));
#84699=CARTESIAN_POINT('Ctrl Pts',(-2.3793283911,-19.5124295317,10.8306149778));
#84700=CARTESIAN_POINT('Ctrl Pts',(-2.38900185162,-19.5330726947,10.839573774));
#84701=CARTESIAN_POINT('Ctrl Pts',(-2.3975442085,-19.5531518159,10.850652948));
#84702=CARTESIAN_POINT('Ctrl Pts',(-2.40485476239,-19.5724073147,10.863676829));
#84703=CARTESIAN_POINT('Ctrl Pts',(-2.27560738165,-19.4921831081,10.7955818101));
#84704=CARTESIAN_POINT('Ctrl Pts',(-2.2893900823,-19.510844473,10.7983487664));
#84705=CARTESIAN_POINT('Ctrl Pts',(-2.30277704132,-19.5295058379,10.8033357254));
#84706=CARTESIAN_POINT('Ctrl Pts',(-2.31559552336,-19.5479374484,10.8105100727));
#84707=CARTESIAN_POINT('Ctrl Pts',(-2.32768219961,-19.5659096429,10.8197835155));
#84708=CARTESIAN_POINT('Ctrl Pts',(-2.33889513807,-19.5832093643,10.8310183547));
#84709=CARTESIAN_POINT('Ctrl Pts',(-2.19384540622,-19.5207627351,10.7891484524));
#84710=CARTESIAN_POINT('Ctrl Pts',(-2.2092243494,-19.5364515236,10.7895844661));
#84711=CARTESIAN_POINT('Ctrl Pts',(-2.22456910998,-19.5521403122,10.7920171276));
#84712=CARTESIAN_POINT('Ctrl Pts',(-2.23970912867,-19.56765722,10.7964428));
#84713=CARTESIAN_POINT('Ctrl Pts',(-2.25447433499,-19.5828304221,10.8028133883));
#84714=CARTESIAN_POINT('Ctrl Pts',(-2.26870622615,-19.5974991706,10.8110393571));
#84715=CARTESIAN_POINT('Ctrl Pts',(-2.15676147687,-19.5361420848,10.7897230447));
#84716=CARTESIAN_POINT('Ctrl Pts',(-2.17269814184,-19.5502379741,10.7889802082));
#84717=CARTESIAN_POINT('Ctrl Pts',(-2.18874339027,-19.5643338633,10.7901046703));
#84718=CARTESIAN_POINT('Ctrl Pts',(-2.20473176783,-19.578285603,10.7931055871));
#84719=CARTESIAN_POINT('Ctrl Pts',(-2.22049530483,-19.591949083,10.7979533276));
#84720=CARTESIAN_POINT('Ctrl Pts',(-2.23587372456,-19.6051888511,10.8045811578));
#84721=CARTESIAN_POINT('Ctrl Pts',(-2.12065129512,-19.5532237866,10.7937022943));
#84722=CARTESIAN_POINT('Ctrl Pts',(-2.13693992507,-19.565556494,10.7917229743));
#84723=CARTESIAN_POINT('Ctrl Pts',(-2.15344959477,-19.5778892014,10.7914591884));
#84724=CARTESIAN_POINT('Ctrl Pts',(-2.1700239605,-19.5901054864,10.7929309325));
#84725=CARTESIAN_POINT('Ctrl Pts',(-2.18650229981,-19.6020889553,10.7961251723));
#84726=CARTESIAN_POINT('Ctrl Pts',(-2.20272856722,-19.6137296999,10.8009965235));
#84727=CARTESIAN_POINT('Ctrl Pts',(-2.08703817283,-19.5762208096,10.800197792));
#84728=CARTESIAN_POINT('Ctrl Pts',(-2.10348700925,-19.5861969598,10.7970192075));
#84729=CARTESIAN_POINT('Ctrl Pts',(-2.12023640403,-19.59617311,10.7953959802));
#84730=CARTESIAN_POINT('Ctrl Pts',(-2.13714159891,-19.6060614593,10.7953561328));
#84731=CARTESIAN_POINT('Ctrl Pts',(-2.1540525206,-19.6157742254,10.7969000191));
#84732=CARTESIAN_POINT('Ctrl Pts',(-2.17082158758,-19.625228211,10.8000003054));
#84733=CARTESIAN_POINT('',(-2.47879649228766,-19.4447371256487,10.8888042456754));
#84734=CARTESIAN_POINT('Origin',(-2.3006596926964,-19.4447370092007,11.1301921673071));
#84735=CARTESIAN_POINT('Ctrl Pts',(-2.47879653467762,-19.4447372464188,
10.8888042196737));
#84736=CARTESIAN_POINT('Ctrl Pts',(-2.46045463077369,-19.4482609676597,
10.8752684601721));
#84737=CARTESIAN_POINT('Ctrl Pts',(-2.44128408623476,-19.4521492663384,
10.8630639844833));
#84738=CARTESIAN_POINT('Ctrl Pts',(-2.42151329003282,-19.4564348686664,
10.8522709465103));
#84739=CARTESIAN_POINT('Ctrl Pts',(-2.40132346561323,-19.4608113013426,
10.8412491576352));
#84740=CARTESIAN_POINT('Ctrl Pts',(-2.38050875266403,-19.465602185527,10.8316993192422));
#84741=CARTESIAN_POINT('Ctrl Pts',(-2.35932627610263,-19.4708664875248,
10.8236593330656));
#84742=CARTESIAN_POINT('Ctrl Pts',(-2.33803965795491,-19.4761566709515,
10.8155798190788));
#84743=CARTESIAN_POINT('Ctrl Pts',(-2.31638283441941,-19.4819251433216,
10.8090249582489));
#84744=CARTESIAN_POINT('Ctrl Pts',(-2.29461341099357,-19.4882532179105,
10.803986219452));
#84745=CARTESIAN_POINT('Ctrl Pts',(-2.28619925943151,-19.4906990970524,
10.80203868455));
#84746=CARTESIAN_POINT('Ctrl Pts',(-2.27776815634791,-19.4932287863165,
10.8003171566218));
#84747=CARTESIAN_POINT('Ctrl Pts',(-2.2693342610873,-19.4958477330895,10.798819316362));
#84748=CARTESIAN_POINT('Ctrl Pts',(-2.25070834978327,-19.5016315694778,
10.7955113976644));
#84749=CARTESIAN_POINT('Ctrl Pts',(-2.23207171544287,-19.5078569454259,
10.7932947524955));
#84750=CARTESIAN_POINT('Ctrl Pts',(-2.213592013128,-19.5146534541264,10.7921199499763));
#84751=CARTESIAN_POINT('Ctrl Pts',(-2.20119473891072,-19.5192129530103,
10.7913318231584));
#84752=CARTESIAN_POINT('Ctrl Pts',(-2.18886677146711,-19.5240260825368,
10.791012665294));
#84753=CARTESIAN_POINT('Ctrl Pts',(-2.17665894379668,-19.52914744962,10.7911409237761));
#84754=CARTESIAN_POINT('Ctrl Pts',(-2.16571136803727,-19.5337401220962,
10.7912559417374));
#84755=CARTESIAN_POINT('Ctrl Pts',(-2.15486008673492,-19.5385797109364,
10.7917308495758));
#84756=CARTESIAN_POINT('Ctrl Pts',(-2.14414981251461,-19.5437418168646,
10.7925427409177));
#84757=CARTESIAN_POINT('Ctrl Pts',(-2.13433303459833,-19.5484732781172,
10.7932869008553));
#84758=CARTESIAN_POINT('Ctrl Pts',(-2.1246345745427,-19.5534752730665,10.7943141938894));
#84759=CARTESIAN_POINT('Ctrl Pts',(-2.11509897207031,-19.5588469738143,
10.7955997371279));
#84760=CARTESIAN_POINT('Ctrl Pts',(-2.10556336959791,-19.5642186745621,
10.7968852803664));
#84761=CARTESIAN_POINT('Ctrl Pts',(-2.09619036471992,-19.5699591730014,
10.7984291957784));
#84762=CARTESIAN_POINT('Ctrl Pts',(-2.08703817327717,-19.5762208095999,
10.8001977919136));
#84763=CARTESIAN_POINT('Origin',(-2.18190353865,-18.7742356128,11.2911158416));
#84764=CARTESIAN_POINT('',(-2.47879645562,-16.6742356128,10.8888042759));
#84765=CARTESIAN_POINT('',(-2.47879645562,-18.0594863082,10.8888042759));
#84766=CARTESIAN_POINT('Origin',(-2.18190353865,-16.6742356128,11.2911158416));
#84767=CARTESIAN_POINT('Ctrl Pts',(-2.47879645562,-19.4447370035,10.8888042759));
#84768=CARTESIAN_POINT('Ctrl Pts',(-2.48614926363,-19.4683842219,10.8942304132));
#84769=CARTESIAN_POINT('Ctrl Pts',(-2.4919119687,-19.4920314402,10.901811256));
#84770=CARTESIAN_POINT('Ctrl Pts',(-2.49597503074,-19.515326813,10.9114662563));
#84771=CARTESIAN_POINT('Ctrl Pts',(-2.49827711961,-19.5379187068,10.9230496761));
#84772=CARTESIAN_POINT('Ctrl Pts',(-2.49881045348,-19.5594863076,10.9363632729));
#84773=CARTESIAN_POINT('Ctrl Pts',(-2.510543559,-19.4294897509,10.9122326109));
#84774=CARTESIAN_POINT('Ctrl Pts',(-2.52509315654,-19.4549860554,10.9229697266));
#84775=CARTESIAN_POINT('Ctrl Pts',(-2.53743184504,-19.4804823599,10.9367027854));
#84776=CARTESIAN_POINT('Ctrl Pts',(-2.54730011106,-19.5054619039,10.9532408984));
#84777=CARTESIAN_POINT('Ctrl Pts',(-2.55452473408,-19.52940842,10.9722767674));
#84778=CARTESIAN_POINT('Ctrl Pts',(-2.55903583297,-19.5518626834,10.9934181309));
#84779=CARTESIAN_POINT('Ctrl Pts',(-2.54358798483,-19.3961031493,10.9366183279));
#84780=CARTESIAN_POINT('Ctrl Pts',(-2.56490210185,-19.4257202286,10.9523474783));
#84781=CARTESIAN_POINT('Ctrl Pts',(-2.58262930917,-19.4553373078,10.972937153));
#84782=CARTESIAN_POINT('Ctrl Pts',(-2.59620857289,-19.4840367355,10.997975939));
#84783=CARTESIAN_POINT('Ctrl Pts',(-2.60527727222,-19.5109029172,11.0267904888));
#84784=CARTESIAN_POINT('Ctrl Pts',(-2.60971873368,-19.5351693857,11.0585616091));
#84785=CARTESIAN_POINT('Ctrl Pts',(-2.57980368735,-19.3527485635,10.9633443444));
#84786=CARTESIAN_POINT('Ctrl Pts',(-2.60698188591,-19.3880359645,10.9834009889));
#84787=CARTESIAN_POINT('Ctrl Pts',(-2.62854104782,-19.4233233655,11.011071838));
#84788=CARTESIAN_POINT('Ctrl Pts',(-2.64323454282,-19.4570166595,11.0454386344));
#84789=CARTESIAN_POINT('Ctrl Pts',(-2.65023339726,-19.4875204033,11.0850019677));
#84790=CARTESIAN_POINT('Ctrl Pts',(-2.64928177187,-19.5134920611,11.1278449523));
#84791=CARTESIAN_POINT('Ctrl Pts',(-2.66373575496,-19.2547159387,11.0252834944));
#84792=CARTESIAN_POINT('Ctrl Pts',(-2.69872898986,-19.3050683152,11.0511073573));
#84793=CARTESIAN_POINT('Ctrl Pts',(-2.72330881282,-19.3554206917,11.0910421533));
#84794=CARTESIAN_POINT('Ctrl Pts',(-2.73408042005,-19.4013898853,11.1426264261));
#84795=CARTESIAN_POINT('Ctrl Pts',(-2.72955068062,-19.4386199009,11.2009208948));
#84796=CARTESIAN_POINT('Ctrl Pts',(-2.71098021085,-19.4644758001,11.2604631973));
#84797=CARTESIAN_POINT('Ctrl Pts',(-2.78975290654,-19.1524485557,11.1182800744));
#84798=CARTESIAN_POINT('Ctrl Pts',(-2.82090969201,-19.2230604651,11.1412727847));
#84799=CARTESIAN_POINT('Ctrl Pts',(-2.83638207721,-19.2936723745,11.1855190018));
#84800=CARTESIAN_POINT('Ctrl Pts',(-2.83135807356,-19.3541924937,11.2476786502));
#84801=CARTESIAN_POINT('Ctrl Pts',(-2.80630726796,-19.3949915084,11.3177423125));
#84802=CARTESIAN_POINT('Ctrl Pts',(-2.76681414133,-19.4133420624,11.3857731806));
#84803=CARTESIAN_POINT('Ctrl Pts',(-2.86129530492,-19.1091646129,11.1710760494));
#84804=CARTESIAN_POINT('Ctrl Pts',(-2.88687394597,-19.1898640218,11.1899522282));
#84805=CARTESIAN_POINT('Ctrl Pts',(-2.89447935536,-19.2705634307,11.2331834474));
#84806=CARTESIAN_POINT('Ctrl Pts',(-2.87932742318,-19.3377754042,11.2975635634));
#84807=CARTESIAN_POINT('Ctrl Pts',(-2.84388765021,-19.3788647517,11.3707877234));
#84808=CARTESIAN_POINT('Ctrl Pts',(-2.796245355,-19.3917000854,11.4409843867));
#84809=CARTESIAN_POINT('Ctrl Pts',(-2.94208651244,-19.0824256558,11.2306973462));
#84810=CARTESIAN_POINT('Ctrl Pts',(-2.95834742078,-19.1709113574,11.2426973703));
#84811=CARTESIAN_POINT('Ctrl Pts',(-2.9547674495,-19.2593970589,11.2815832341));
#84812=CARTESIAN_POINT('Ctrl Pts',(-2.92789987303,-19.3312626769,11.3452494815));
#84813=CARTESIAN_POINT('Ctrl Pts',(-2.88323668464,-19.3712611943,11.4201106412));
#84814=CARTESIAN_POINT('Ctrl Pts',(-2.83073115845,-19.3783306343,11.4925686116));
#84815=CARTESIAN_POINT('Ctrl Pts',(-3.0257458739,-19.0756496396,11.2924352478));
#84816=CARTESIAN_POINT('Ctrl Pts',(-3.03060872632,-19.1683851734,11.2960238755));
#84817=CARTESIAN_POINT('Ctrl Pts',(-3.01410418365,-19.2611207071,11.3285668827));
#84818=CARTESIAN_POINT('Ctrl Pts',(-2.97498276954,-19.334976222,11.3896852328));
#84819=CARTESIAN_POINT('Ctrl Pts',(-2.92227176474,-19.372909531,11.465275844));
#84820=CARTESIAN_POINT('Ctrl Pts',(-2.86720977988,-19.3749426262,11.5401119926));
#84821=CARTESIAN_POINT('',(-3.0257458739,-19.0756502088,11.2924352478));
#84822=CARTESIAN_POINT('Origin',(-2.84896336891823,-19.0776979407904,11.5322135659977));
#84823=CARTESIAN_POINT('Ctrl Pts',(-3.02574587389968,-19.0756502088,11.2924352478004));
#84824=CARTESIAN_POINT('Ctrl Pts',(-3.00675351565961,-19.0771882002878,
11.2784195019978));
#84825=CARTESIAN_POINT('Ctrl Pts',(-2.98794556110458,-19.0799656124685,
11.2645398401506));
#84826=CARTESIAN_POINT('Ctrl Pts',(-2.96946444777136,-19.0838689703512,
11.2509013765509));
#84827=CARTESIAN_POINT('Ctrl Pts',(-2.95255124090799,-19.0874411739377,
11.2384199771892));
#84828=CARTESIAN_POINT('Ctrl Pts',(-2.93591148075212,-19.0919553471003,
11.2261403726466));
#84829=CARTESIAN_POINT('Ctrl Pts',(-2.91963473242905,-19.0972951829733,
11.2141286590785));
#84830=CARTESIAN_POINT('Ctrl Pts',(-2.90097606500497,-19.1034164437851,
11.2003591662896));
#84831=CARTESIAN_POINT('Ctrl Pts',(-2.88279745671413,-19.1106246716873,
11.1869439416157));
#84832=CARTESIAN_POINT('Ctrl Pts',(-2.86521289932878,-19.1187068763404,
11.1739671072852));
#84833=CARTESIAN_POINT('Ctrl Pts',(-2.85069831160009,-19.1253780632181,
11.16325581122));
#84834=CARTESIAN_POINT('Ctrl Pts',(-2.83658785784503,-19.1326436742646,
11.1528427529497));
#84835=CARTESIAN_POINT('Ctrl Pts',(-2.82292669530417,-19.140371437611,11.142761257057));
#84836=CARTESIAN_POINT('Ctrl Pts',(-2.80596470462133,-19.1499663933469,
11.1302438568071));
#84837=CARTESIAN_POINT('Ctrl Pts',(-2.78969874364794,-19.1602717602212,
11.1182401039592));
#84838=CARTESIAN_POINT('Ctrl Pts',(-2.7741716633805,-19.1710306210649,11.1067816211666));
#84839=CARTESIAN_POINT('Ctrl Pts',(-2.76433010714757,-19.1778499285053,
11.0995188711321));
#84840=CARTESIAN_POINT('Ctrl Pts',(-2.75478457692901,-19.1848513153056,
11.0924745787183));
#84841=CARTESIAN_POINT('Ctrl Pts',(-2.74553729325106,-19.1919708669864,
11.0856503826122));
#84842=CARTESIAN_POINT('Ctrl Pts',(-2.73213768965327,-19.2022873202974,
11.075761908777));
#84843=CARTESIAN_POINT('Ctrl Pts',(-2.7193444588255,-19.2128634993548,11.0663209183868));
#84844=CARTESIAN_POINT('Ctrl Pts',(-2.70715916076948,-19.2235067787786,
11.0573285627176));
#84845=CARTESIAN_POINT('Ctrl Pts',(-2.69769192270529,-19.2317759618241,
11.0503420473704));
#84846=CARTESIAN_POINT('Ctrl Pts',(-2.68859091957648,-19.2400856488052,
11.0436258015626));
#84847=CARTESIAN_POINT('Ctrl Pts',(-2.67984102302334,-19.2483550306415,
11.0371686610452));
#84848=CARTESIAN_POINT('Ctrl Pts',(-2.66553704813159,-19.2618734796242,
11.026612790439));
#84849=CARTESIAN_POINT('Ctrl Pts',(-2.65214757506909,-19.2753062681188,
11.0167317926194));
#84850=CARTESIAN_POINT('Ctrl Pts',(-2.63954076934534,-19.2884074477262,
11.0074283780573));
#84851=CARTESIAN_POINT('Ctrl Pts',(-2.63452172045956,-19.2936233178166,
11.0037244824381));
#84852=CARTESIAN_POINT('Ctrl Pts',(-2.62962657043066,-19.2987872244217,
11.0001120201687));
#84853=CARTESIAN_POINT('Ctrl Pts',(-2.6248465335031,-19.3038857598675,10.9965845076172));
#84854=CARTESIAN_POINT('Ctrl Pts',(-2.60806283236651,-19.3217877753653,
10.9841986793659));
#84855=CARTESIAN_POINT('Ctrl Pts',(-2.59269322531019,-19.3388823165721,
10.972856406431));
#84856=CARTESIAN_POINT('Ctrl Pts',(-2.57833633556526,-19.3547066387323,
10.9622614863181));
#84857=CARTESIAN_POINT('Ctrl Pts',(-2.56468487008995,-19.3697534344852,
10.9521871464922));
#84858=CARTESIAN_POINT('Ctrl Pts',(-2.55194665981057,-19.3836622157048,
10.9427867595277));
#84859=CARTESIAN_POINT('Ctrl Pts',(-2.53980373411162,-19.396024813606,10.9338256733092));
#84860=CARTESIAN_POINT('Ctrl Pts',(-2.53017587314596,-19.4058268478701,
10.926720623476));
#84861=CARTESIAN_POINT('Ctrl Pts',(-2.52092740821589,-19.4146616173831,
10.9198955559181));
#84862=CARTESIAN_POINT('Ctrl Pts',(-2.51192137185923,-19.4222801308466,
10.9132493927221));
#84863=CARTESIAN_POINT('Ctrl Pts',(-2.50956800534002,-19.4242709238882,
10.9115126844381));
#84864=CARTESIAN_POINT('Ctrl Pts',(-2.50723135998009,-19.4261785010644,
10.9097883158081));
#84865=CARTESIAN_POINT('Ctrl Pts',(-2.50490937729373,-19.4279980029771,
10.9080747677192));
#84866=CARTESIAN_POINT('Ctrl Pts',(-2.49828731261426,-19.43318704225,10.9031878982596));
#84867=CARTESIAN_POINT('Ctrl Pts',(-2.49177954925272,-19.4376614176956,
10.8983853790159));
#84868=CARTESIAN_POINT('Ctrl Pts',(-2.48534852651507,-19.4413044184337,
10.8936394922355));
#84869=CARTESIAN_POINT('Ctrl Pts',(-2.48315653562045,-19.44254612209,10.8920218738514));
#84870=CARTESIAN_POINT('Ctrl Pts',(-2.48097305807628,-19.4436916418333,
10.8904105380807));
#84871=CARTESIAN_POINT('Ctrl Pts',(-2.47879645562,-19.4447370035,10.8888042759));
#84872=CARTESIAN_POINT('Ctrl Pts',(-3.02574587396,-19.0756502088,11.2924352478));
#84873=CARTESIAN_POINT('Ctrl Pts',(-3.03060876213,-19.1683856419,11.2960239029));
#84874=CARTESIAN_POINT('Ctrl Pts',(-3.0141042599,-19.261121075,11.3285669311));
#84875=CARTESIAN_POINT('Ctrl Pts',(-2.97498288462,-19.3349765133,11.3896852899));
#84876=CARTESIAN_POINT('Ctrl Pts',(-2.9222719047,-19.3729097939,11.465275899));
#84877=CARTESIAN_POINT('Ctrl Pts',(-2.86720992778,-19.3749429031,11.5401120401));
#84878=CARTESIAN_POINT('Ctrl Pts',(-3.03447355616,-19.0749433453,11.2988759949));
#84879=CARTESIAN_POINT('Ctrl Pts',(-3.03813896473,-19.1681049521,11.3015809487));
#84880=CARTESIAN_POINT('Ctrl Pts',(-3.02028592653,-19.2612665588,11.3334449681));
#84881=CARTESIAN_POINT('Ctrl Pts',(-2.97989655367,-19.3353233942,11.3942703053));
#84882=CARTESIAN_POINT('Ctrl Pts',(-2.92636073645,-19.3730546128,11.4699120931));
#84883=CARTESIAN_POINT('Ctrl Pts',(-2.87104425856,-19.3745894729,11.5449824418));
#84884=CARTESIAN_POINT('Ctrl Pts',(-3.04321296595,-19.0744719442,11.3053253965));
#84885=CARTESIAN_POINT('Ctrl Pts',(-3.04566841653,-19.1680282232,11.3071374404));
#84886=CARTESIAN_POINT('Ctrl Pts',(-3.02645347241,-19.2615845022,11.3383144504));
#84887=CARTESIAN_POINT('Ctrl Pts',(-2.9847889853,-19.3358150142,11.3988454565));
#84888=CARTESIAN_POINT('Ctrl Pts',(-2.93043564473,-19.3733247573,11.4745447401));
#84889=CARTESIAN_POINT('Ctrl Pts',(-2.87488373803,-19.3743537743,11.5498593869));
#84890=CARTESIAN_POINT('Ctrl Pts',(-3.05195820325,-19.0742362318,11.3117790986));
#84891=CARTESIAN_POINT('Ctrl Pts',(-3.0531916857,-19.1681548312,11.3126893695));
#84892=CARTESIAN_POINT('Ctrl Pts',(-3.03260202102,-19.2620734306,11.3431715971));
#84893=CARTESIAN_POINT('Ctrl Pts',(-2.98965603461,-19.3364495577,11.4034071424));
#84894=CARTESIAN_POINT('Ctrl Pts',(-2.93449336502,-19.3737189989,11.4791704265));
#84895=CARTESIAN_POINT('Ctrl Pts',(-2.87872577363,-19.3742359202,11.5547395826));
#84896=CARTESIAN_POINT('Ctrl Pts',(-3.06070337749,-19.0742362041,11.3182327542));
#84897=CARTESIAN_POINT('Ctrl Pts',(-3.06070341502,-19.1684838804,11.3182327825));
#84898=CARTESIAN_POINT('Ctrl Pts',(-3.0387268402,-19.2627315566,11.3480127241));
#84899=CARTESIAN_POINT('Ctrl Pts',(-2.9944937393,-19.3372249046,11.4079518654));
#84900=CARTESIAN_POINT('Ctrl Pts',(-2.93853076799,-19.3742358919,11.4837858067));
#84901=CARTESIAN_POINT('Ctrl Pts',(-2.88256777785,-19.3742359083,11.5596197419));
#84902=CARTESIAN_POINT('',(-3.06070337744081,-19.0742359088556,11.3182327542666));
#84903=CARTESIAN_POINT('Origin',(-2.88382717324306,-19.0763574922431,11.5579128187659));
#84904=CARTESIAN_POINT('Origin',(-3.06701733419236,-19.6773931794005,11.3228922010275));
#84905=CARTESIAN_POINT('Origin',(-4.88509763285,-19.0742356128,13.0374220375));
#84906=CARTESIAN_POINT('',(-5.27647385588,-19.0742356128,12.9533996668));
#84907=CARTESIAN_POINT('Origin',(-2.3,-16.6742356128,10.7568582774));
#84908=CARTESIAN_POINT('',(-7.49224433422,-16.6742356128,14.5885665792));
#84909=CARTESIAN_POINT('Origin',(-14.0872311983,-16.6742356128,1.01503102594));
#84910=CARTESIAN_POINT('',(-14.9221240862,-16.6742356128,1.52650344091));
#84911=CARTESIAN_POINT('',(-14.9221240862,-16.6742356128,1.52650344091));
#84912=CARTESIAN_POINT('',(-14.9221240862,-19.3742356128,1.52650344091));
#84913=CARTESIAN_POINT('',(-14.9221240862,-18.0242356128,1.52650344091));
#84914=CARTESIAN_POINT('',(-15.57788482,-19.3742356128,1.92823584397));
#84915=CARTESIAN_POINT('Origin',(-13.4419608479,-16.6742356128,-0.619725245787));
#84916=CARTESIAN_POINT('',(-14.8362431871,-19.3742356128,-1.4738910501));
#84917=CARTESIAN_POINT('',(-15.5349443705,-19.3742356128,-1.90192964856));
#84918=CARTESIAN_POINT('',(-14.8362431871,-16.6742356128,-1.4738910501));
#84919=CARTESIAN_POINT('',(-14.8362431871,-18.0242356128,-1.4738910501));
#84920=CARTESIAN_POINT('',(-14.8362431871,-16.6742356128,-1.4738910501));
#84921=CARTESIAN_POINT('Origin',(0.,-18.0242356128,0.));
#84922=CARTESIAN_POINT('',(-14.976285439,-19.3742356128,-0.843133708384));
#84923=CARTESIAN_POINT('Origin',(0.,-19.3742356128,0.));
#84924=CARTESIAN_POINT('',(-14.976285439,-16.6742356128,-0.843133708384));
#84925=CARTESIAN_POINT('Origin',(3.5527136788005E-13,-16.6742356128,5.24580379135386E-14));
#84926=CARTESIAN_POINT('',(-14.976285439,-18.0242356128,-0.843133708384));
#84927=CARTESIAN_POINT('Origin',(-12.9794473804,-18.0242356128,-0.730715880599));
#84928=CARTESIAN_POINT('Origin',(-12.9794473804,-16.6742356128,-0.730715880599));
#84929=CARTESIAN_POINT('Origin',(-12.9794473804,-19.3742356128,-0.730715880599));
#84930=CARTESIAN_POINT('Origin',(0.,-18.0242356128,0.));
#84931=CARTESIAN_POINT('',(-13.4786568951,-19.3742356128,-0.758820337546));
#84932=CARTESIAN_POINT('',(-13.4786568951,-16.6742356128,-0.758820337546));
#84933=CARTESIAN_POINT('',(-13.4786568951,-18.0242356128,-0.758820337546));
#84934=CARTESIAN_POINT('',(-13.3555478213,-16.6742356128,1.96960462883));
#84935=CARTESIAN_POINT('Origin',(-1.04360964314765E-13,-16.6742356128,-1.24761312392252E-13));
#84936=CARTESIAN_POINT('',(-13.3555478213,-19.3742356128,1.96960462883));
#84937=CARTESIAN_POINT('',(-13.3555478213,-18.0242356128,1.96960462883));
#84938=CARTESIAN_POINT('Origin',(0.,-19.3742356128,0.));
#84939=CARTESIAN_POINT('Origin',(-12.9794473804,-18.0242356128,-0.730715880599));
#84940=CARTESIAN_POINT('',(-13.1249762208,-16.6742356128,-1.20906863394));
#84941=CARTESIAN_POINT('',(-13.1249762208,-19.3742356128,-1.20906863394));
#84942=CARTESIAN_POINT('',(-13.1249762208,-18.0242356128,-1.20906863394));
#84943=CARTESIAN_POINT('Origin',(-12.9794473804,-16.6742356128,-0.730715880598998));
#84944=CARTESIAN_POINT('Origin',(-12.9794473804,-19.3742356128,-0.730715880599));
#84945=CARTESIAN_POINT('Origin',(-13.2705050612,-18.0242356128,-1.68742138727));
#84946=CARTESIAN_POINT('',(-13.0093116937,-19.3742356128,-2.11377572911));
#84947=CARTESIAN_POINT('Origin',(-13.2705050612,-19.3742356128,-1.68742138727));
#84948=CARTESIAN_POINT('',(-13.0093116937,-16.6742356128,-2.11377572911));
#84949=CARTESIAN_POINT('',(-13.0093116937,-18.0242356128,-2.11377572911));
#84950=CARTESIAN_POINT('Origin',(-13.2705050612,-16.6742356128,-1.68742138727));
#84951=CARTESIAN_POINT('Origin',(-12.6583807456,-16.6742356128,-1.8987882713));
#84952=CARTESIAN_POINT('',(-14.4691278654,-19.3742356128,-3.00808889615));
#84953=CARTESIAN_POINT('',(-15.9289440371,-16.6742356128,-3.90240206319));
#84954=CARTESIAN_POINT('Origin',(-13.8501977406,-18.0242356128,2.04255294841));
#84955=CARTESIAN_POINT('',(-13.5890043731,-19.3742356128,2.46890729025));
#84956=CARTESIAN_POINT('Origin',(-13.8501977406,-19.3742356128,2.04255294841));
#84957=CARTESIAN_POINT('',(-13.5890043731,-16.6742356128,2.46890729025));
#84958=CARTESIAN_POINT('Origin',(-13.8501977406,-16.6742356128,2.04255294841));
#84959=CARTESIAN_POINT('',(-13.5890043731,-18.0242356128,2.46890729025));
#84960=CARTESIAN_POINT('Origin',(0.,-19.3742356128,0.));
#84961=CARTESIAN_POINT('',(-14.7589742051,-19.3742356128,3.18565467672));
#84962=CARTESIAN_POINT('Origin',(-13.303651096,-16.6742356128,2.29409405145));
#84963=CARTESIAN_POINT('',(-13.5890043731,-16.6742356128,2.46890729025));
#84964=CARTESIAN_POINT('Origin',(5.,-39.2742356128,0.));
#84965=CARTESIAN_POINT('',(5.,-35.2742356128,-16.5096094653));
#84966=CARTESIAN_POINT('',(5.,-38.7742356128,0.1339280819));
#84967=CARTESIAN_POINT('Origin',(4.,-35.2742356128,-16.5096094653));
#84968=CARTESIAN_POINT('',(4.,-34.2742356128,-16.4193528851));
#84969=CARTESIAN_POINT('Origin',(5.,-34.2742356128,0.));
#84970=CARTESIAN_POINT('',(-4.,-34.2742356128,-16.5096094653));
#84971=CARTESIAN_POINT('Origin',(-4.,-35.2742356128,-16.5096094653));
#84972=CARTESIAN_POINT('',(-5.,-35.2742356128,-16.1426761277));
#84973=CARTESIAN_POINT('Origin',(-5.,-39.2742356128,0.));
#84974=CARTESIAN_POINT('',(-5.,-38.7742356128,0.1339280819));
#84975=CARTESIAN_POINT('Origin',(4.,-39.2742356128,0.));
#84976=CARTESIAN_POINT('',(4.,-35.2742356128,16.6523581408));
#84977=CARTESIAN_POINT('',(4.,-38.7742356128,0.213056290446));
#84978=CARTESIAN_POINT('Origin',(3.,-35.2742356128,16.6523581408));
#84979=CARTESIAN_POINT('',(3.,-34.2742356128,16.631351665));
#84980=CARTESIAN_POINT('Origin',(5.,-34.2742356128,0.));
#84981=CARTESIAN_POINT('',(-3.,-34.2742356128,16.6523581408));
#84982=CARTESIAN_POINT('Origin',(-3.,-35.2742356128,16.6523581408));
#84983=CARTESIAN_POINT('',(-4.,-35.2742356128,16.4206921659));
#84984=CARTESIAN_POINT('Origin',(-4.,-39.2742356128,0.));
#84985=CARTESIAN_POINT('',(-4.,-38.7742356128,0.213056290446));
#84986=CARTESIAN_POINT('Origin',(-5.5,-38.7742356128,0.1339280819));
#84987=CARTESIAN_POINT('',(-5.5,-39.2742356128,-15.9790598121));
#84988=CARTESIAN_POINT('Origin',(-4.5,-38.7742356128,0.213056290446));
#84989=CARTESIAN_POINT('',(-4.5,-39.2742356128,16.2892879764));
#84990=CARTESIAN_POINT('Origin',(0.,-39.2742356128,17.4));
#84991=CARTESIAN_POINT('Origin',(5.5,-38.7742356128,0.1339280819));
#84992=CARTESIAN_POINT('',(5.5,-39.2742356128,-15.9790598121));
#84993=CARTESIAN_POINT('Origin',(4.5,-38.7742356128,0.213056290446));
#84994=CARTESIAN_POINT('',(4.5,-39.2742356128,16.2892879764));
#84995=CARTESIAN_POINT('Origin',(0.,-39.2742356128,17.4));
#84996=CARTESIAN_POINT('Origin',(0.,-21.7742356128,0.));
#84997=CARTESIAN_POINT('',(-4.38674367823,-16.6742356128,-8.0298804413));
#84998=CARTESIAN_POINT('Origin',(-2.22044604925031E-15,-16.6742356128,-2.22044604925031E-15));
#84999=CARTESIAN_POINT('',(-4.38674367822846,-21.7742356128,-8.02988044129691));
#85000=CARTESIAN_POINT('Origin',(0.,-16.6742356128,17.4));
#85001=CARTESIAN_POINT('Origin',(0.,-16.6742356128,17.4));
#85002=CARTESIAN_POINT('Origin',(0.,-16.6742356128,17.4));
#85003=CARTESIAN_POINT('Origin',(0.,-16.6742356128,17.4));
#85004=CARTESIAN_POINT('Origin',(0.,-16.6742356128,17.4));
#85005=CARTESIAN_POINT('Origin',(0.,-16.6742356128,17.4));
#85006=CARTESIAN_POINT('Origin',(0.,-14.6742356128,17.4));
#85007=CARTESIAN_POINT('',(3.90056490239326,-14.6742356128,10.5597900654496));
#85008=CARTESIAN_POINT('',(7.1947640041133,-14.6742356128,8.65788332730725));
#85009=CARTESIAN_POINT('Origin',(0.,-14.6742356128,0.));
#85010=CARTESIAN_POINT('',(-3.90056490239319,-14.6742356128,10.5597900654496));
#85011=CARTESIAN_POINT('',(3.75578649684289E-14,-14.6742356128,10.5597900654496));
#85012=CARTESIAN_POINT('',(-7.19476400411325,-14.6742356128,8.65788332730729));
#85013=CARTESIAN_POINT('Origin',(0.,-14.6742356128,0.));
#85014=CARTESIAN_POINT('',(-11.0953289065065,-14.6742356128,1.9019067381423));
#85015=CARTESIAN_POINT('',(-9.14504645530986,-14.6742356128,5.27989503272479));
#85016=CARTESIAN_POINT('',(-11.0953289065065,-14.6742356128,-1.90190673814234));
#85017=CARTESIAN_POINT('Origin',(0.,-14.6742356128,0.));
#85018=CARTESIAN_POINT('',(-7.1947640041134,-14.6742356128,-8.65788332730717));
#85019=CARTESIAN_POINT('',(-9.14504645530993,-14.6742356128,-5.27989503272475));
#85020=CARTESIAN_POINT('',(-3.90056490239334,-14.6742356128,-10.5597900654495));
#85021=CARTESIAN_POINT('Origin',(0.,-14.6742356128,0.));
#85022=CARTESIAN_POINT('',(3.90056490239312,-14.6742356128,-10.5597900654496));
#85023=CARTESIAN_POINT('',(-1.11171280306549E-13,-14.6742356128,-10.5597900654496));
#85024=CARTESIAN_POINT('',(7.19476400411319,-14.6742356128,-8.65788332730735));
#85025=CARTESIAN_POINT('Origin',(0.,-14.6742356128,0.));
#85026=CARTESIAN_POINT('',(11.0953289065065,-14.6742356128,-1.90190673814237));
#85027=CARTESIAN_POINT('',(9.14504645530982,-14.6742356128,-5.27989503272486));
#85028=CARTESIAN_POINT('',(11.0953289065065,-14.6742356128,1.90190673814221));
#85029=CARTESIAN_POINT('Origin',(0.,-14.6742356128,0.));
#85030=CARTESIAN_POINT('',(9.14504645530989,-14.6742356128,5.27989503272473));
#85031=CARTESIAN_POINT('Origin',(3.75578649684289E-14,26.5953441711815,
10.5597900654496));
#85032=CARTESIAN_POINT('',(3.90056490239326,26.5953441711815,10.5597900654496));
#85033=CARTESIAN_POINT('',(-3.90056490239319,26.5953441711815,10.5597900654496));
#85034=CARTESIAN_POINT('Origin',(0.,26.5953441711815,0.));
#85035=CARTESIAN_POINT('',(7.1947640041133,26.5953441711815,8.65788332730725));
#85036=CARTESIAN_POINT('Origin',(9.14504645530989,26.5953441711815,5.27989503272473));
#85037=CARTESIAN_POINT('',(11.0953289065065,26.5953441711815,1.90190673814221));
#85038=CARTESIAN_POINT('Origin',(0.,26.5953441711815,0.));
#85039=CARTESIAN_POINT('',(11.0953289065065,-6.63753909988913,-1.90190673814237));
#85040=CARTESIAN_POINT('',(11.0953289065065,26.5953441711815,-1.90190673814237));
#85041=CARTESIAN_POINT('Origin',(0.,-6.63753909988913,0.));
#85042=CARTESIAN_POINT('Origin',(9.14504645530982,26.5953441711815,-5.27989503272486));
#85043=CARTESIAN_POINT('',(7.19476400411318,-6.63753909988913,-8.65788332730734));
#85044=CARTESIAN_POINT('',(7.19476400411319,26.5953441711815,-8.65788332730735));
#85045=CARTESIAN_POINT('Ctrl Pts',(7.19476400411318,-6.63753909988913,-8.65788332730735));
#85046=CARTESIAN_POINT('Ctrl Pts',(7.20793342429826,-6.25115677756999,-8.63507322244056));
#85047=CARTESIAN_POINT('Ctrl Pts',(7.22957597298824,-5.92703963684599,-8.59758722850423));
#85048=CARTESIAN_POINT('Ctrl Pts',(7.33264605094296,-5.4824893351699,-8.41906461674658));
#85049=CARTESIAN_POINT('Ctrl Pts',(7.38587885165349,-5.33005160890808,-8.32686270128674));
#85050=CARTESIAN_POINT('Ctrl Pts',(7.55351534711876,-5.02205392516981,-8.03650777393812));
#85051=CARTESIAN_POINT('Ctrl Pts',(7.68241549558792,-4.85741613145686,-7.81324616768638));
#85052=CARTESIAN_POINT('Ctrl Pts',(8.07805804686918,-4.55925658398797,-7.12797316723107));
#85053=CARTESIAN_POINT('Ctrl Pts',(8.2987360820476,-4.46102644577706,-6.74574759818758));
#85054=CARTESIAN_POINT('Ctrl Pts',(8.61875324812248,-4.36808225563921,-6.19146160725169));
#85055=CARTESIAN_POINT('Ctrl Pts',(8.73033406055812,-4.34507072735135,-5.99819797096336));
#85056=CARTESIAN_POINT('Ctrl Pts',(8.89953062521147,-4.32271936364378,-5.70514092451763));
#85057=CARTESIAN_POINT('Ctrl Pts',(8.95774725247859,-4.31728665962078,-5.60430676824569));
#85058=CARTESIAN_POINT('Ctrl Pts',(9.05873727376944,-4.31167125033784,-5.42938692031248));
#85059=CARTESIAN_POINT('Ctrl Pts',(9.10160080381223,-4.31047752426155,-5.35514510848663));
#85060=CARTESIAN_POINT('Ctrl Pts',(9.18843216468531,-4.31045476730958,-5.20474877976411));
#85061=CARTESIAN_POINT('Ctrl Pts',(9.23245827883154,-4.31169063776257,-5.1284933132029));
#85062=CARTESIAN_POINT('Ctrl Pts',(9.33992086438215,-4.3177710909309,-4.94236265511655));
#85063=CARTESIAN_POINT('Ctrl Pts',(9.40346807156964,-4.32398244074384,-4.83229566358879));
#85064=CARTESIAN_POINT('Ctrl Pts',(9.5916439749527,-4.35037319724934,-4.50636543816916));
#85065=CARTESIAN_POINT('Ctrl Pts',(9.71718683007716,-4.37846636964572,-4.28891883456635));
#85066=CARTESIAN_POINT('Ctrl Pts',(10.0959505184882,-4.5002770190838,-3.63288088217621));
#85067=CARTESIAN_POINT('Ctrl Pts',(10.3416323810413,-4.63190537710699,-3.20734741373611));
#85068=CARTESIAN_POINT('Ctrl Pts',(10.7018033055628,-4.96923903784649,-2.58351307305582));
#85069=CARTESIAN_POINT('Ctrl Pts',(10.8039037926238,-5.13032755416942,-2.4066698419886));
#85070=CARTESIAN_POINT('Ctrl Pts',(10.9344613444125,-5.41302767928334,-2.18053752897883));
#85071=CARTESIAN_POINT('Ctrl Pts',(10.9804393462862,-5.56176401030052,-2.10090129370317));
#85072=CARTESIAN_POINT('Ctrl Pts',(11.0647640875135,-5.9935176192942,-1.95484655756232));
#85073=CARTESIAN_POINT('Ctrl Pts',(11.0834813101589,-6.28993823923298,-1.92242737696393));
#85074=CARTESIAN_POINT('Ctrl Pts',(11.0953289065065,-6.63753909988913,-1.90190673814236));
#85075=CARTESIAN_POINT('Origin',(0.,26.5953441711815,0.));
#85076=CARTESIAN_POINT('',(3.90056490239312,-6.63753909988913,-10.5597900654496));
#85077=CARTESIAN_POINT('',(3.90056490239312,26.5953441711815,-10.5597900654496));
#85078=CARTESIAN_POINT('Origin',(0.,-6.63753909988913,0.));
#85079=CARTESIAN_POINT('Origin',(-1.11171280306549E-13,26.5953441711815,
-10.5597900654496));
#85080=CARTESIAN_POINT('',(-3.90056490239334,-6.63753909988913,-10.5597900654495));
#85081=CARTESIAN_POINT('',(-3.90056490239334,26.5953441711815,-10.5597900654495));
#85082=CARTESIAN_POINT('Ctrl Pts',(-3.90056490239333,-6.63753909988912,
-10.5597900654495));
#85083=CARTESIAN_POINT('Ctrl Pts',(-3.88650640714021,-6.43130549325069,
-10.5597900654495));
#85084=CARTESIAN_POINT('Ctrl Pts',(-3.86750921833438,-6.24077478304535,
-10.5597900654495));
#85085=CARTESIAN_POINT('Ctrl Pts',(-3.79603527122593,-5.88328867547882,
-10.5597900654495));
#85086=CARTESIAN_POINT('Ctrl Pts',(-3.74111739908583,-5.70969285765481,
-10.5597900656594));
#85087=CARTESIAN_POINT('Ctrl Pts',(-3.56226471943126,-5.38996752638052,
-10.5597900656594));
#85088=CARTESIAN_POINT('Ctrl Pts',(-3.4385859282338,-5.23989257637364,-10.5597900654495));
#85089=CARTESIAN_POINT('Ctrl Pts',(-2.92900810424285,-4.84096372109965,
-10.5597900654495));
#85090=CARTESIAN_POINT('Ctrl Pts',(-2.50413756504146,-4.6858650511529,-10.5597900654495));
#85091=CARTESIAN_POINT('Ctrl Pts',(-1.80048019244854,-4.48301709563195,
-10.5597900654495));
#85092=CARTESIAN_POINT('Ctrl Pts',(-1.40703076126886,-4.41160065323693,
-10.5597900654495));
#85093=CARTESIAN_POINT('Ctrl Pts',(-0.841933717031831,-4.34702984071184,
-10.5597900654496));
#85094=CARTESIAN_POINT('Ctrl Pts',(-0.658043722812697,-4.33203279124675,
-10.5597900654496));
#85095=CARTESIAN_POINT('Ctrl Pts',(-0.382154538654522,-4.31786065829338,
-10.5597900654496));
#85096=CARTESIAN_POINT('Ctrl Pts',(-0.289586349002193,-4.31451406956158,
-10.5597900654496));
#85097=CARTESIAN_POINT('Ctrl Pts',(-0.131799833370343,-4.31116993398485,
-10.5597900654496));
#85098=CARTESIAN_POINT('Ctrl Pts',(-0.0664976322663677,-4.31047485185275,
-10.5597900654496));
#85099=CARTESIAN_POINT('Ctrl Pts',(0.0639173571934239,-4.31045776213066,
-10.5597900654496));
#85100=CARTESIAN_POINT('Ctrl Pts',(0.129079361026242,-4.31113280201933,
-10.5597900654496));
#85101=CARTESIAN_POINT('Ctrl Pts',(0.28605704414335,-4.31441138123185,-10.5597900654496));
#85102=CARTESIAN_POINT('Ctrl Pts',(0.377955322537869,-4.31769531886316,
-10.5597900654496));
#85103=CARTESIAN_POINT('Ctrl Pts',(0.651486594053966,-4.33160004901355,
-10.5597900654496));
#85104=CARTESIAN_POINT('Ctrl Pts',(0.833670646936078,-4.34630752826428,
-10.5597900654496));
#85105=CARTESIAN_POINT('Ctrl Pts',(1.39309035936172,-4.40956151168582,-10.5597900654496));
#85106=CARTESIAN_POINT('Ctrl Pts',(1.78195277809562,-4.47937544741232,-10.5597900654496));
#85107=CARTESIAN_POINT('Ctrl Pts',(2.48599710360056,-4.67915031046531,-10.5597900654496));
#85108=CARTESIAN_POINT('Ctrl Pts',(2.91820462596513,-4.83459622286637,-10.5597900654496));
#85109=CARTESIAN_POINT('Ctrl Pts',(3.43432853419123,-5.23545667439774,-10.5597900654496));
#85110=CARTESIAN_POINT('Ctrl Pts',(3.55892444433031,-5.38544981580505,-10.5597900657021));
#85111=CARTESIAN_POINT('Ctrl Pts',(3.73882514967999,-5.7041522322255,-10.5597900657021));
#85112=CARTESIAN_POINT('Ctrl Pts',(3.79423029833326,-5.87690202689049,-10.5597900654496));
#85113=CARTESIAN_POINT('Ctrl Pts',(3.86701620951233,-6.23579968922608,-10.5597900654496));
#85114=CARTESIAN_POINT('Ctrl Pts',(3.88632393679749,-6.42862871197637,-10.5597900654496));
#85115=CARTESIAN_POINT('Ctrl Pts',(3.90056490239312,-6.63753909988913,-10.5597900654496));
#85116=CARTESIAN_POINT('Origin',(0.,26.5953441711815,0.));
#85117=CARTESIAN_POINT('',(-7.1947640041134,-6.63753909988913,-8.65788332730716));
#85118=CARTESIAN_POINT('',(-7.1947640041134,26.5953441711815,-8.65788332730717));
#85119=CARTESIAN_POINT('Origin',(0.,-6.63753909988913,0.));
#85120=CARTESIAN_POINT('Origin',(-9.14504645530993,26.5953441711815,-5.27989503272475));
#85121=CARTESIAN_POINT('',(-11.0953289065065,-6.63753909988913,-1.90190673814234));
#85122=CARTESIAN_POINT('',(-11.0953289065065,26.5953441711815,-1.90190673814234));
#85123=CARTESIAN_POINT('Ctrl Pts',(-11.0953289065065,-6.63753909988913,
-1.90190673814234));
#85124=CARTESIAN_POINT('Ctrl Pts',(-11.0835931462191,-6.29321943734551,
-1.92223367122555));
#85125=CARTESIAN_POINT('Ctrl Pts',(-11.0651161129459,-5.99918609364617,
-1.95423683162789));
#85126=CARTESIAN_POINT('Ctrl Pts',(-10.9824464115036,-5.56957898521099,
-2.09742495477247));
#85127=CARTESIAN_POINT('Ctrl Pts',(-10.9371509020334,-5.4206851321178,-2.17587907852964));
#85128=CARTESIAN_POINT('Ctrl Pts',(-10.8075382554253,-5.13626438454722,
-2.4003747677582));
#85129=CARTESIAN_POINT('Ctrl Pts',(-10.706766468623,-4.9763500796868,-2.57491662246939));
#85130=CARTESIAN_POINT('Ctrl Pts',(-10.3498218261682,-4.63662053620469,
-3.1931628786906));
#85131=CARTESIAN_POINT('Ctrl Pts',(-10.1022245203587,-4.50300238908727,
-3.62201399216979));
#85132=CARTESIAN_POINT('Ctrl Pts',(-9.72143984871383,-4.37950172223962,
-4.28155239020215));
#85133=CARTESIAN_POINT('Ctrl Pts',(-9.59502849226356,-4.35099240625125,
-4.50050328222773));
#85134=CARTESIAN_POINT('Ctrl Pts',(-9.40565012662499,-4.32421736597011,
-4.8285162333681));
#85135=CARTESIAN_POINT('Ctrl Pts',(-9.34174413003707,-4.31791520443562,
-4.93920466636659));
#85136=CARTESIAN_POINT('Ctrl Pts',(-9.23384225124107,-4.31174147077324,
-5.12609620267341));
#85137=CARTESIAN_POINT('Ctrl Pts',(-9.18973415909178,-4.31047784978136,
-5.202493659301));
#85138=CARTESIAN_POINT('Ctrl Pts',(-9.1028760836399,-4.31045508582798,-5.35293625903132));
#85139=CARTESIAN_POINT('Ctrl Pts',(-9.06006776325605,-4.3116233104859,-5.42708244492283));
#85140=CARTESIAN_POINT('Ctrl Pts',(-8.95941636902032,-4.31715957848673,
-5.60141577359174));
#85141=CARTESIAN_POINT('Ctrl Pts',(-8.90148409311079,-4.32252007109627,
-5.70175741886518));
#85142=CARTESIAN_POINT('Ctrl Pts',(-8.7332509121229,-4.3445763195675,-5.99314583585513));
#85143=CARTESIAN_POINT('Ctrl Pts',(-8.62236299560954,-4.36727979901891,
-6.18520934120172));
#85144=CARTESIAN_POINT('Ctrl Pts',(-8.30433573130979,-4.45894533929483,
-6.73604872116104));
#85145=CARTESIAN_POINT('Ctrl Pts',(-8.08539249003307,-4.55566580971441,
-7.11526953902613));
#85146=CARTESIAN_POINT('Ctrl Pts',(-7.68947767855954,-4.85020226805379,
-7.80101410796735));
#85147=CARTESIAN_POINT('Ctrl Pts',(-7.55829760823967,-5.01478805334227,
-8.02822465470182));
#85148=CARTESIAN_POINT('Ctrl Pts',(-7.38777942464433,-5.32531557816731,
-8.32357081230331));
#85149=CARTESIAN_POINT('Ctrl Pts',(-7.33403218269018,-5.47793756447234,
-8.4166637661346));
#85150=CARTESIAN_POINT('Ctrl Pts',(-7.22979823884874,-5.92365652676773,
-8.59720225274125));
#85151=CARTESIAN_POINT('Ctrl Pts',(-7.20800124955019,-6.249166828286,-8.63495574565837));
#85152=CARTESIAN_POINT('Ctrl Pts',(-7.1947640041134,-6.63753909988913,-8.65788332730716));
#85153=CARTESIAN_POINT('Origin',(0.,26.5953441711815,0.));
#85154=CARTESIAN_POINT('',(-11.0953289065065,26.5953441711815,1.9019067381423));
#85155=CARTESIAN_POINT('Origin',(0.,-6.63753909988913,0.));
#85156=CARTESIAN_POINT('Origin',(-9.14504645530986,26.5953441711815,5.27989503272479));
#85157=CARTESIAN_POINT('',(-7.19476400411325,26.5953441711815,8.65788332730729));
#85158=CARTESIAN_POINT('Origin',(0.,26.5953441711815,0.));
#85159=CARTESIAN_POINT('Ctrl Pts',(11.2571565141535,-6.63753909988913,1.37860406925589E-15));
#85160=CARTESIAN_POINT('Ctrl Pts',(11.2571565141535,-6.63753909988913,-22.5143130283071));
#85161=CARTESIAN_POINT('Ctrl Pts',(-11.2571565141535,-6.63753909988913,
-22.5143130283071));
#85162=CARTESIAN_POINT('Ctrl Pts',(-11.2571565141535,-6.63753909988913,
-2.75720813851178E-15));
#85163=CARTESIAN_POINT('Ctrl Pts',(11.2316061906402,-5.55581078583997,1.37547505706511E-15));
#85164=CARTESIAN_POINT('Ctrl Pts',(11.2316061906402,-5.55581078583997,-22.4632123812804));
#85165=CARTESIAN_POINT('Ctrl Pts',(-11.2316061906402,-5.55581078583997,
-22.4632123812804));
#85166=CARTESIAN_POINT('Ctrl Pts',(-11.2316061906402,-5.55581078583997,
-2.75095011413023E-15));
#85167=CARTESIAN_POINT('Ctrl Pts',(11.1603664914423,-4.97414426866896,1.36675071010562E-15));
#85168=CARTESIAN_POINT('Ctrl Pts',(11.1603664914423,-4.97414426866896,-22.3207329828847));
#85169=CARTESIAN_POINT('Ctrl Pts',(-11.1603664914423,-4.97414426866896,
-22.3207329828847));
#85170=CARTESIAN_POINT('Ctrl Pts',(-11.1603664914423,-4.97414426866896,
-2.73350142021125E-15));
#85171=CARTESIAN_POINT('Ctrl Pts',(10.527435261753,-4.27423561284,1.28923898965368E-15));
#85172=CARTESIAN_POINT('Ctrl Pts',(10.527435261753,-4.27423561284,-21.054870523506));
#85173=CARTESIAN_POINT('Ctrl Pts',(-10.527435261753,-4.27423561284,-21.054870523506));
#85174=CARTESIAN_POINT('Ctrl Pts',(-10.527435261753,-4.27423561284,-2.57847797930735E-15));
#85175=CARTESIAN_POINT('Ctrl Pts',(10.5228448600506,-4.26915945016302,1.28867682757851E-15));
#85176=CARTESIAN_POINT('Ctrl Pts',(10.5228448600506,-4.26915945016302,-21.0456897201011));
#85177=CARTESIAN_POINT('Ctrl Pts',(-10.5228448600506,-4.26915945016302,
-21.0456897201012));
#85178=CARTESIAN_POINT('Ctrl Pts',(-10.5228448600506,-4.26915945016302,
-2.57735365515702E-15));
#85179=CARTESIAN_POINT('Ctrl Pts',(10.5182544583482,-4.26408328748604,1.28811466550335E-15));
#85180=CARTESIAN_POINT('Ctrl Pts',(10.5182544583482,-4.26408328748604,-21.0365089166963));
#85181=CARTESIAN_POINT('Ctrl Pts',(-10.5182544583482,-4.26408328748604,
-21.0365089166963));
#85182=CARTESIAN_POINT('Ctrl Pts',(-10.5182544583482,-4.26408328748604,
-2.57622933100669E-15));
#85183=CARTESIAN_POINT('Ctrl Pts',(10.5136640566458,-4.25900712480906,1.28755250342818E-15));
#85184=CARTESIAN_POINT('Ctrl Pts',(10.5136640566458,-4.25900712480906,-21.0273281132915));
#85185=CARTESIAN_POINT('Ctrl Pts',(-10.5136640566458,-4.25900712480906,
-21.0273281132915));
#85186=CARTESIAN_POINT('Ctrl Pts',(-10.5136640566458,-4.25900712480906,
-2.57510500685636E-15));
#85187=CARTESIAN_POINT('',(0.,0.,0.));
#85188=CARTESIAN_POINT('Origin',(8.21591479143,-23.2742356128,11.6886688365));
#85189=CARTESIAN_POINT('',(7.99564314217,-23.4742356128,11.4850014593));
#85190=CARTESIAN_POINT('',(8.01224741424,-22.8742356128,11.9089404858));
#85191=CARTESIAN_POINT('Ctrl Pts',(7.99564314217,-23.4742356128,11.4850014593));
#85192=CARTESIAN_POINT('Ctrl Pts',(7.98964252128,-23.4742356128,11.4914912894));
#85193=CARTESIAN_POINT('Ctrl Pts',(7.97859188254,-23.4732430341,11.5041738872));
#85194=CARTESIAN_POINT('Ctrl Pts',(7.97506561416,-23.4709827428,11.5096523074));
#85195=CARTESIAN_POINT('Ctrl Pts',(7.96049908281,-23.4651088112,11.5297325584));
#85196=CARTESIAN_POINT('Ctrl Pts',(7.94999449773,-23.4537301075,11.5494738265));
#85197=CARTESIAN_POINT('Ctrl Pts',(7.9432480685,-23.4460266432,11.5624437668));
#85198=CARTESIAN_POINT('Ctrl Pts',(7.93181038161,-23.4257772831,11.589727728));
#85199=CARTESIAN_POINT('Ctrl Pts',(7.92449811306,-23.4017307742,11.6153459759));
#85200=CARTESIAN_POINT('Ctrl Pts',(7.92150726931,-23.3879026248,11.6287650914));
#85201=CARTESIAN_POINT('Ctrl Pts',(7.91677660432,-23.3563766548,11.6571003353));
#85202=CARTESIAN_POINT('Ctrl Pts',(7.91547477954,-23.3227166577,11.6832984902));
#85203=CARTESIAN_POINT('Ctrl Pts',(7.9155846643,-23.3039994083,11.6969647216));
#85204=CARTESIAN_POINT('Ctrl Pts',(7.91959338184,-23.2114810387,11.7607695014));
#85205=CARTESIAN_POINT('Ctrl Pts',(7.93828028322,-23.1128615217,11.8131880532));
#85206=CARTESIAN_POINT('Ctrl Pts',(7.95813278234,-23.0338190575,11.8499462819));
#85207=CARTESIAN_POINT('Ctrl Pts',(7.9829584197,-22.9540055384,11.8818593216));
#85208=CARTESIAN_POINT('Ctrl Pts',(8.01224741424,-22.8742356128,11.9089404858));
#85209=CARTESIAN_POINT('',(8.03752439844,-23.4742356128,11.4474700229));
#85210=CARTESIAN_POINT('Origin',(8.21591479143,-23.4742356128,11.6886688365));
#85211=CARTESIAN_POINT('',(8.03752439844,-25.4742356128,11.4474700229));
#85212=CARTESIAN_POINT('',(8.03752439844,-22.6642356128,11.4474700229));
#85213=CARTESIAN_POINT('',(8.01224741424,-25.4742356128,11.9089404858));
#85214=CARTESIAN_POINT('Origin',(8.21591479143,-25.4742356128,11.6886688365));
#85215=CARTESIAN_POINT('',(8.01224741424,-24.1742356128,11.9089404858));
#85216=CARTESIAN_POINT('Origin',(7.16045579301E-17,-22.6642356128,0.580061096523));
#85217=CARTESIAN_POINT('',(8.73611663980898,-23.4697909663899,10.8942572011661));
#85218=CARTESIAN_POINT('',(8.73611663424,-25.4742356128,10.8942572059));
#85219=CARTESIAN_POINT('',(8.73611663424,-23.2742356128,10.8942572059));
#85220=CARTESIAN_POINT('Origin',(-1.62597327472E-14,-25.4742356128,0.580061096523));
#85221=CARTESIAN_POINT('',(8.67864985337,-23.4742356128,10.942657873));
#85222=CARTESIAN_POINT('Origin',(2.30650470794E-14,-23.4742356128,0.580061096523));
#85223=CARTESIAN_POINT('Origin',(8.65818093366798,-22.8777633816448,10.9233631052074));
#85224=CARTESIAN_POINT('Origin',(8.93001206801,-23.2742356128,11.1231776304));
#85225=CARTESIAN_POINT('',(9.1336794452,-22.8742356128,10.9029059811));
#85226=CARTESIAN_POINT('Ctrl Pts',(9.1336794452,-22.8742356128,10.9029059811));
#85227=CARTESIAN_POINT('Ctrl Pts',(9.12864186713826,-22.887974922811,10.8982344510715));
#85228=CARTESIAN_POINT('Ctrl Pts',(9.12335771886472,-22.9019293773381,10.8936712120832));
#85229=CARTESIAN_POINT('Ctrl Pts',(9.11787226943502,-22.9159664885182,10.8892648795277));
#85230=CARTESIAN_POINT('Ctrl Pts',(9.11216771025498,-22.9305642954016,10.8846825412613));
#85231=CARTESIAN_POINT('Ctrl Pts',(9.10624538901133,-22.9452518966254,10.8802696612691));
#85232=CARTESIAN_POINT('Ctrl Pts',(9.10013711659066,-22.9599342922501,10.8760617975029));
#85233=CARTESIAN_POINT('Ctrl Pts',(9.09343775296072,-22.9760374881251,10.8714467431089));
#85234=CARTESIAN_POINT('Ctrl Pts',(9.0865147798379,-22.9921346475642,10.8670780600761));
#85235=CARTESIAN_POINT('Ctrl Pts',(9.07938726585101,-23.0081598565969,10.8629836574886));
#85236=CARTESIAN_POINT('Ctrl Pts',(9.07426631747019,-23.0196735861245,10.8600419271266));
#85237=CARTESIAN_POINT('Ctrl Pts',(9.06903926975429,-23.0311515307987,10.8572413388931));
#85238=CARTESIAN_POINT('Ctrl Pts',(9.0637068507804,-23.0425837055347,10.8545884512405));
#85239=CARTESIAN_POINT('Ctrl Pts',(9.05410828995007,-23.0631620631552,10.8498131506434));
#85240=CARTESIAN_POINT('Ctrl Pts',(9.04417029772133,-23.0835899275873,10.8455159152366));
#85241=CARTESIAN_POINT('Ctrl Pts',(9.03386350882102,-23.1038677787328,10.8417281569271));
#85242=CARTESIAN_POINT('Ctrl Pts',(9.0241092043464,-23.1230586572963,10.8381434373616));
#85243=CARTESIAN_POINT('Ctrl Pts',(9.01402344674499,-23.1421190687442,10.8350133981201));
#85244=CARTESIAN_POINT('Ctrl Pts',(9.00355723569183,-23.1610637443997,10.8323801860489));
#85245=CARTESIAN_POINT('Ctrl Pts',(8.99509378474724,-23.1763832647359,10.830250851844));
#85246=CARTESIAN_POINT('Ctrl Pts',(8.98638093349722,-23.1916281008454,10.8284463322577));
#85247=CARTESIAN_POINT('Ctrl Pts',(8.97738730234821,-23.2067889067296,10.8270074448473));
#85248=CARTESIAN_POINT('Ctrl Pts',(8.96872247513198,-23.2213954389821,10.8256211626452));
#85249=CARTESIAN_POINT('Ctrl Pts',(8.95979676807654,-23.2359248322128,10.8245739094458));
#85250=CARTESIAN_POINT('Ctrl Pts',(8.95058185178658,-23.2503385870446,10.823924671162));
#85251=CARTESIAN_POINT('Ctrl Pts',(8.94184683855384,-23.2640016888274,10.8233092445188));
#85252=CARTESIAN_POINT('Ctrl Pts',(8.93285178149626,-23.2775613698534,10.8230512852217));
#85253=CARTESIAN_POINT('Ctrl Pts',(8.92357530042097,-23.2909480014561,10.82322518767));
#85254=CARTESIAN_POINT('Ctrl Pts',(8.91488039725482,-23.3034953741679,10.8233881875119));
#85255=CARTESIAN_POINT('Ctrl Pts',(8.90593815285812,-23.3158909022145,10.8239305650324));
#85256=CARTESIAN_POINT('Ctrl Pts',(8.89673528370321,-23.3280395843762,10.8249366440998));
#85257=CARTESIAN_POINT('Ctrl Pts',(8.88802059732318,-23.3395438178048,10.8258893538904));
#85258=CARTESIAN_POINT('Ctrl Pts',(8.87907214142089,-23.3508268089755,10.8272578606624));
#85259=CARTESIAN_POINT('Ctrl Pts',(8.86988374445289,-23.361770917696,10.8291354703124));
#85260=CARTESIAN_POINT('Ctrl Pts',(8.86073527603326,-23.3726674683521,10.8310049207342));
#85261=CARTESIAN_POINT('Ctrl Pts',(8.85134885107335,-23.3832284587279,10.8333788805503));
#85262=CARTESIAN_POINT('Ctrl Pts',(8.84172478760057,-23.3932960776091,10.8363732226571));
#85263=CARTESIAN_POINT('Ctrl Pts',(8.83247645671033,-23.4029706470832,10.8392506628029));
#85264=CARTESIAN_POINT('Ctrl Pts',(8.82300864068946,-23.4121896919426,10.8427009774483));
#85265=CARTESIAN_POINT('Ctrl Pts',(8.81332846159939,-23.4207716836739,10.8468501500846));
#85266=CARTESIAN_POINT('Ctrl Pts',(8.80383668759135,-23.4291866443162,10.8509185674783));
#85267=CARTESIAN_POINT('Ctrl Pts',(8.79414068539646,-23.4369892804721,10.8556588323708));
#85268=CARTESIAN_POINT('Ctrl Pts',(8.78425456845438,-23.4439657681908,10.8612131542089));
#85269=CARTESIAN_POINT('Ctrl Pts',(8.77462998987335,-23.4507576921243,10.8666205358237));
#85270=CARTESIAN_POINT('Ctrl Pts',(8.76482519042245,-23.4567666850184,10.8727994450304));
#85271=CARTESIAN_POINT('Ctrl Pts',(8.75486086381769,-23.4617528149732,10.8799042056571));
#85272=CARTESIAN_POINT('Ctrl Pts',(8.74867197648696,-23.4648497223439,10.8843170039098));
#85273=CARTESIAN_POINT('Ctrl Pts',(8.74242170151348,-23.4675511927818,10.889087426161));
#85274=CARTESIAN_POINT('Ctrl Pts',(8.73611663424,-23.4697908757,10.8942572059));
#85275=CARTESIAN_POINT('',(9.1336794452,-25.4742356128,10.9029059811));
#85276=CARTESIAN_POINT('',(9.1336794452,-24.1742356128,10.9029059811));
#85277=CARTESIAN_POINT('Origin',(8.93001206801,-25.4742356128,11.1231776304));
#85278=CARTESIAN_POINT('Origin',(10.806321674,-23.2742356128,10.0787147334));
#85279=CARTESIAN_POINT('',(11.0909930576,-25.4742356128,10.1733836478));
#85280=CARTESIAN_POINT('',(11.0909930576,-22.9538972343,10.1733836478));
#85281=CARTESIAN_POINT('',(11.0909930576,-22.6642356128,10.1733836478));
#85282=CARTESIAN_POINT('',(11.031648508,-25.4742356128,10.2767748704));
#85283=CARTESIAN_POINT('Origin',(10.806321674,-25.4742356128,10.0787147334));
#85284=CARTESIAN_POINT('',(11.031648508,-22.9538972343,10.2767748704));
#85285=CARTESIAN_POINT('',(11.031648508,-22.6642356128,10.2767748704));
#85286=CARTESIAN_POINT('Ctrl Pts',(11.0316485080236,-22.9538972342712,10.2767748704012));
#85287=CARTESIAN_POINT('Ctrl Pts',(11.0362618244719,-22.9574629735615,10.2715264443151));
#85288=CARTESIAN_POINT('Ctrl Pts',(11.0409289539567,-22.9603378044225,10.2658423505117));
#85289=CARTESIAN_POINT('Ctrl Pts',(11.0497741877589,-22.9645897469489,10.2541599678227));
#85290=CARTESIAN_POINT('Ctrl Pts',(11.0539505572373,-22.9660452016239,10.2482245763534));
#85291=CARTESIAN_POINT('Ctrl Pts',(11.0609089320228,-22.9675632436939,10.2375072647136));
#85292=CARTESIAN_POINT('Ctrl Pts',(11.0637741673946,-22.9678862078995,10.2328198127542));
#85293=CARTESIAN_POINT('Ctrl Pts',(11.0665081104589,-22.9678862078995,10.2280566842471));
#85294=CARTESIAN_POINT('Ctrl Pts',(11.0691844131435,-22.9678862078995,10.2233939779248));
#85295=CARTESIAN_POINT('Ctrl Pts',(11.0717346751094,-22.9675767047451,10.2186592052973));
#85296=CARTESIAN_POINT('Ctrl Pts',(11.0773589468691,-22.9661256456956,10.2075161455921));
#85297=CARTESIAN_POINT('Ctrl Pts',(11.0803172029966,-22.9647393225438,10.2010842541412));
#85298=CARTESIAN_POINT('Ctrl Pts',(11.0860358359614,-22.9605581903024,10.1874436600315));
#85299=CARTESIAN_POINT('Ctrl Pts',(11.0887021061436,-22.9576018392337,10.1802725862398));
#85300=CARTESIAN_POINT('Ctrl Pts',(11.0909930576014,-22.9538972342539,10.1733836478253));
#85301=CARTESIAN_POINT('Origin',(10.8795671881,-23.2742356128,9.85222376962));
#85302=CARTESIAN_POINT('',(11.0832345653,-25.4742356128,9.63195212036));
#85303=CARTESIAN_POINT('',(11.0832345653,-21.0742356128,9.63195212036));
#85304=CARTESIAN_POINT('',(11.0832345653,-23.2742356128,9.63195212036));
#85305=CARTESIAN_POINT('',(11.1657658425,-25.4742356128,9.94217003248));
#85306=CARTESIAN_POINT('Origin',(10.8795671881,-25.4742356128,9.85222376962));
#85307=CARTESIAN_POINT('',(11.1657658425,-21.0742356128,9.94217003248));
#85308=CARTESIAN_POINT('',(11.1657658425,-22.6642356128,9.94217003248));
#85309=CARTESIAN_POINT('Origin',(10.8795671881,-21.0742356128,9.85222376962));
#85310=CARTESIAN_POINT('Origin',(11.221722051,-23.1742356128,9.76000029674));
#85311=CARTESIAN_POINT('',(10.7039554837,-21.0742356128,9.28126343203));
#85312=CARTESIAN_POINT('',(10.7039554837,-25.4742356128,9.28126343203));
#85313=CARTESIAN_POINT('',(10.7039554837,-23.2742356128,9.28126343203));
#85314=CARTESIAN_POINT('',(11.080905232,-25.4742356128,9.62979837427));
#85315=CARTESIAN_POINT('',(9.20983954971,-21.0742356128,7.89977528084));
#85316=CARTESIAN_POINT('Origin',(10.9076228609,-23.2742356128,9.06099178277));
#85317=CARTESIAN_POINT('',(10.6707879888,-21.0742356128,8.87684715658));
#85318=CARTESIAN_POINT('Origin',(10.9076228609,-21.0742356128,9.06099178277));
#85319=CARTESIAN_POINT('',(10.6707879888,-25.4742356128,8.87684715658));
#85320=CARTESIAN_POINT('',(10.6707879888,-22.6642356128,8.87684715658));
#85321=CARTESIAN_POINT('Origin',(10.9076228609,-25.4742356128,9.06099178277));
#85322=CARTESIAN_POINT('Origin',(7.16045579301E-17,-22.6642356128,0.580061096523));
#85323=CARTESIAN_POINT('',(11.1917725091,-21.0742356128,8.1594148509));
#85324=CARTESIAN_POINT('',(11.1917725091,-25.4742356128,8.1594148509));
#85325=CARTESIAN_POINT('',(11.1917725091,-23.2742356128,8.1594148509));
#85326=CARTESIAN_POINT('Origin',(2.10437608802E-14,-25.4742356128,0.580061096523));
#85327=CARTESIAN_POINT('Origin',(-5.06274711921E-15,-21.0742356128,0.580061096523));
#85328=CARTESIAN_POINT('Origin',(11.4401704731,-23.2742356128,8.32763628675));
#85329=CARTESIAN_POINT('',(11.4067704497,-21.0742356128,8.02950135347));
#85330=CARTESIAN_POINT('Origin',(11.4401704731,-21.0742356128,8.32763628675));
#85331=CARTESIAN_POINT('',(11.4067704324828,-22.8742356736053,8.02950135644609));
#85332=CARTESIAN_POINT('',(11.4067704497,-23.1237854196,8.02950135347));
#85333=CARTESIAN_POINT('',(11.6438378494077,-23.4645367062672,8.107364636655));
#85334=CARTESIAN_POINT('Ctrl Pts',(11.4067704240483,-22.8742356736211,8.02950135948828));
#85335=CARTESIAN_POINT('Ctrl Pts',(11.406804630593,-22.8931971151233,8.02949752860505));
#85336=CARTESIAN_POINT('Ctrl Pts',(11.4072793786485,-22.9119159973912,8.02944297070681));
#85337=CARTESIAN_POINT('Ctrl Pts',(11.4081636215115,-22.9303682802508,8.02934885100158));
#85338=CARTESIAN_POINT('Ctrl Pts',(11.4093015847953,-22.9541151729595,8.02922772503799));
#85339=CARTESIAN_POINT('Ctrl Pts',(11.4111181074154,-22.9774225569164,8.02904008763942));
#85340=CARTESIAN_POINT('Ctrl Pts',(11.4136025576223,-23.0003019569523,8.02882283063887));
#85341=CARTESIAN_POINT('Ctrl Pts',(11.4158839595366,-23.0213114772456,8.0286233295438));
#85342=CARTESIAN_POINT('Ctrl Pts',(11.4187306210101,-23.041963354936,8.02839868544617));
#85343=CARTESIAN_POINT('Ctrl Pts',(11.4221516301857,-23.0622661414509,8.02819479359798));
#85344=CARTESIAN_POINT('Ctrl Pts',(11.4255161960669,-23.0822339519104,8.02799426576521));
#85345=CARTESIAN_POINT('Ctrl Pts',(11.4294208422657,-23.1018555855848,8.02781470906328));
#85346=CARTESIAN_POINT('Ctrl Pts',(11.433865073085,-23.121150855687,8.02771826496776));
#85347=CARTESIAN_POINT('Ctrl Pts',(11.4378046064153,-23.1382549087334,8.02763277329456));
#85348=CARTESIAN_POINT('Ctrl Pts',(11.4421665723171,-23.1550964914925,8.02761253148517));
#85349=CARTESIAN_POINT('Ctrl Pts',(11.4469532894184,-23.171677434704,8.02771668501094));
#85350=CARTESIAN_POINT('Ctrl Pts',(11.4493343026855,-23.1799251428787,8.02776849315448));
#85351=CARTESIAN_POINT('Ctrl Pts',(11.45182061247,-23.1881086229785,8.02785134438343));
#85352=CARTESIAN_POINT('Ctrl Pts',(11.4544133388932,-23.1962268038527,8.02797457619187));
#85353=CARTESIAN_POINT('Ctrl Pts',(11.4560833706917,-23.2014559017182,8.02805395249506));
#85354=CARTESIAN_POINT('Ctrl Pts',(11.4577973958969,-23.2066571892584,8.02815006675177));
#85355=CARTESIAN_POINT('Ctrl Pts',(11.4595579723806,-23.21182985295,8.02826447101687));
#85356=CARTESIAN_POINT('Ctrl Pts',(11.4608371058657,-23.215588012505,8.02834759056758));
#85357=CARTESIAN_POINT('Ctrl Pts',(11.4619902680251,-23.2188887018161,8.02842958664865));
#85358=CARTESIAN_POINT('Ctrl Pts',(11.4632664251937,-23.2224651114436,8.02852793871659));
#85359=CARTESIAN_POINT('Ctrl Pts',(11.4642974173963,-23.2253544502573,8.02860739618285));
#85360=CARTESIAN_POINT('Ctrl Pts',(11.4654089415283,-23.2284235612494,8.02869756181277));
#85361=CARTESIAN_POINT('Ctrl Pts',(11.4667526561535,-23.2320483579825,8.02881620022717));
#85362=CARTESIAN_POINT('Ctrl Pts',(11.4716505862419,-23.2452609856118,8.02924864521855));
#85363=CARTESIAN_POINT('Ctrl Pts',(11.476723057138,-23.2578514126002,8.02981125418537));
#85364=CARTESIAN_POINT('Ctrl Pts',(11.4819567085306,-23.2698805438842,8.03053293688576));
#85365=CARTESIAN_POINT('Ctrl Pts',(11.4891125155748,-23.2863275969878,8.031519670958));
#85366=CARTESIAN_POINT('Ctrl Pts',(11.4965676819051,-23.3017228895861,8.03280495670992));
#85367=CARTESIAN_POINT('Ctrl Pts',(11.5042645117035,-23.3161285879357,8.03446701167399));
#85368=CARTESIAN_POINT('Ctrl Pts',(11.5134123496989,-23.333250051988,8.03644239763791));
#85369=CARTESIAN_POINT('Ctrl Pts',(11.5228989659229,-23.3489714733738,8.03894962022515));
#85370=CARTESIAN_POINT('Ctrl Pts',(11.5326485135102,-23.3633433251174,8.04211213354388));
#85371=CARTESIAN_POINT('Ctrl Pts',(11.5413937056095,-23.3762346519401,8.04494885865768));
#85372=CARTESIAN_POINT('Ctrl Pts',(11.5503523954545,-23.3880408749711,8.04831209101017));
#85373=CARTESIAN_POINT('Ctrl Pts',(11.5594844411486,-23.3987638621671,8.0522969369301));
#85374=CARTESIAN_POINT('Ctrl Pts',(11.5675484360139,-23.4082327278062,8.0558157297738));
#85375=CARTESIAN_POINT('Ctrl Pts',(11.5757495248873,-23.4168566128402,8.05981987129089));
#85376=CARTESIAN_POINT('Ctrl Pts',(11.5840455773726,-23.4246048038136,8.06437911997429));
#85377=CARTESIAN_POINT('Ctrl Pts',(11.5912704990814,-23.4313526002225,8.06834970897998));
#85378=CARTESIAN_POINT('Ctrl Pts',(11.5985685290852,-23.4374349566399,8.07274238219416));
#85379=CARTESIAN_POINT('Ctrl Pts',(11.6058815281764,-23.4428171841118,8.07759494346571));
#85380=CARTESIAN_POINT('Ctrl Pts',(11.6122904881892,-23.4475340561116,8.08184762704481));
#85381=CARTESIAN_POINT('Ctrl Pts',(11.6187115020277,-23.4517117790196,8.08645452510614));
#85382=CARTESIAN_POINT('Ctrl Pts',(11.6250704319617,-23.4553328841096,8.09142084227157));
#85383=CARTESIAN_POINT('Ctrl Pts',(11.6303453144621,-23.4583366762679,8.0955405196039));
#85384=CARTESIAN_POINT('Ctrl Pts',(11.6355773644057,-23.4609566494751,8.09990789774777));
#85385=CARTESIAN_POINT('Ctrl Pts',(11.6406968626537,-23.4632004596753,8.10450322745316));
#85386=CARTESIAN_POINT('Ctrl Pts',(11.6417489768831,-23.4636615878026,8.10544761917633));
#85387=CARTESIAN_POINT('Ctrl Pts',(11.6427962324924,-23.4641069212813,8.10640153774678));
#85388=CARTESIAN_POINT('Ctrl Pts',(11.6438378503,-23.4645366935,8.10736463748));
#85389=CARTESIAN_POINT('',(11.6438378503,-25.4742356128,8.10736463748));
#85390=CARTESIAN_POINT('',(11.6438378503,-24.4693861731,8.10736463748));
#85391=CARTESIAN_POINT('Origin',(11.4401704731,-25.4742356128,8.32763628675));
#85392=CARTESIAN_POINT('Origin',(12.8942551175,-23.1742356128,9.2635243433));
#85393=CARTESIAN_POINT('',(12.7478394283,-25.4742356128,9.12814559847));
#85394=CARTESIAN_POINT('',(12.7478394285276,-23.4742356127672,9.12814559867721));
#85395=CARTESIAN_POINT('',(12.7478394283,-22.5760378048,9.12814559847));
#85396=CARTESIAN_POINT('',(12.1510854644,-25.4742356128,8.57637547707));
#85397=CARTESIAN_POINT('',(11.7384871149,-23.4742356128,8.19487915673));
#85398=CARTESIAN_POINT('Origin',(11.7384707086266,-22.6130235696614,8.19486399662491));
#85399=CARTESIAN_POINT('',(6.46706166421,-23.4742356128,3.32081842676));
#85400=CARTESIAN_POINT('Origin',(8.92072771219,-25.4742356128,12.3403523349));
#85401=CARTESIAN_POINT('',(9.18405109086,-25.4742356128,12.9924125631));
#85402=CARTESIAN_POINT('',(9.38771846805,-25.7742356128,12.7721409138));
#85403=CARTESIAN_POINT('Ctrl Pts',(9.18405109085604,-25.4742356128,12.9924125631043));
#85404=CARTESIAN_POINT('Ctrl Pts',(9.18405109085603,-25.4915889699708,12.9924125631043));
#85405=CARTESIAN_POINT('Ctrl Pts',(9.18506704327817,-25.5091509586982,12.9912971565068));
#85406=CARTESIAN_POINT('Ctrl Pts',(9.18716742200737,-25.5266577240362,12.989007694918));
#85407=CARTESIAN_POINT('Ctrl Pts',(9.18920364301532,-25.5436297314494,12.9867881667352));
#85408=CARTESIAN_POINT('Ctrl Pts',(9.19225937615859,-25.5605494747294,12.9834648633035));
#85409=CARTESIAN_POINT('Ctrl Pts',(9.19637109291018,-25.577145193568,12.9790123784317));
#85410=CARTESIAN_POINT('Ctrl Pts',(9.19702801738436,-25.5797966733586,12.9783010098088));
#85411=CARTESIAN_POINT('Ctrl Pts',(9.19771183581985,-25.582439822218,12.9775608837574));
#85412=CARTESIAN_POINT('Ctrl Pts',(9.19842262451815,-25.5850734653017,12.976791975009));
#85413=CARTESIAN_POINT('Ctrl Pts',(9.20271106230882,-25.6009631587567,12.9721528785487));
#85414=CARTESIAN_POINT('Ctrl Pts',(9.20798244683343,-25.6165082390736,12.966462002305));
#85415=CARTESIAN_POINT('Ctrl Pts',(9.21422564722063,-25.6314368687755,12.9597255814124));
#85416=CARTESIAN_POINT('Ctrl Pts',(9.21507861227714,-25.6334764636448,12.9588052310679));
#85417=CARTESIAN_POINT('Ctrl Pts',(9.21594966634115,-25.6355045241066,12.9578654196439));
#85418=CARTESIAN_POINT('Ctrl Pts',(9.21683873157363,-25.6375203320718,12.9569062165261));
#85419=CARTESIAN_POINT('Ctrl Pts',(9.22053698036576,-25.6459054978619,12.9529162148453));
#85420=CARTESIAN_POINT('Ctrl Pts',(9.22454701548163,-25.6540787107173,12.9485902011535));
#85421=CARTESIAN_POINT('Ctrl Pts',(9.22885958309505,-25.6619871955642,12.9439349706664));
#85422=CARTESIAN_POINT('Ctrl Pts',(9.23101586690176,-25.6659414379876,12.9416073554228));
#85423=CARTESIAN_POINT('Ctrl Pts',(9.2332477536728,-25.6698295357845,12.9391974685992));
#85424=CARTESIAN_POINT('Ctrl Pts',(9.23555354594216,-25.6736446998774,12.9367065617839));
#85425=CARTESIAN_POINT('Ctrl Pts',(9.23661514745997,-25.6754012258428,12.9355597323444));
#85426=CARTESIAN_POINT('Ctrl Pts',(9.23786437853895,-25.6774206517901,12.9342097543335));
#85427=CARTESIAN_POINT('Ctrl Pts',(9.23906757488256,-25.6793122990687,12.9329092711513));
#85428=CARTESIAN_POINT('Ctrl Pts',(9.24047771393935,-25.6815292985829,12.9313851124903));
#85429=CARTESIAN_POINT('Ctrl Pts',(9.24182444870364,-25.6835705571029,12.929929124854));
#85430=CARTESIAN_POINT('Ctrl Pts',(9.24269077028947,-25.6848647673463,12.9289922005395));
#85431=CARTESIAN_POINT('Ctrl Pts',(9.24702851674015,-25.6913449889886,12.9243009401738));
#85432=CARTESIAN_POINT('Ctrl Pts',(9.25189294570965,-25.6980495816226,12.919007545773));
#85433=CARTESIAN_POINT('Ctrl Pts',(9.25736979554345,-25.7047927115736,12.9130403476632));
#85434=CARTESIAN_POINT('Ctrl Pts',(9.26273984236593,-25.7114043450244,12.9071895147536));
#85435=CARTESIAN_POINT('Ctrl Pts',(9.26869935366587,-25.7180531264771,12.9006901484567));
#85436=CARTESIAN_POINT('Ctrl Pts',(9.27531632190389,-25.7245165097648,12.8934885636304));
#85437=CARTESIAN_POINT('Ctrl Pts',(9.28152670348966,-25.7305827435909,12.8867294878444));
#85438=CARTESIAN_POINT('Ctrl Pts',(9.28831672104179,-25.7364852360521,12.8793513061525));
#85439=CARTESIAN_POINT('Ctrl Pts',(9.29572291972933,-25.7420008228083,12.8713309055222));
#85440=CARTESIAN_POINT('Ctrl Pts',(9.29620779517355,-25.7423619220295,12.870805818972));
#85441=CARTESIAN_POINT('Ctrl Pts',(9.29669530270517,-25.7427213495874,12.8702779894634));
#85442=CARTESIAN_POINT('Ctrl Pts',(9.29718544861305,-25.7430790373084,12.8697474147999));
#85443=CARTESIAN_POINT('Ctrl Pts',(9.30425747107762,-25.7482398997328,12.8620920699751));
#85444=CARTESIAN_POINT('Ctrl Pts',(9.31188552467293,-25.7530410399209,12.8538658250417));
#85445=CARTESIAN_POINT('Ctrl Pts',(9.32005647568179,-25.7572618964892,12.8450655815725));
#85446=CARTESIAN_POINT('Ctrl Pts',(9.32798270924704,-25.7613563397148,12.8365289026605));
#85447=CARTESIAN_POINT('Ctrl Pts',(9.33642017572173,-25.7649041797592,12.8274516947767));
#85448=CARTESIAN_POINT('Ctrl Pts',(9.34532707567636,-25.7676848145053,12.8178633707713));
#85449=CARTESIAN_POINT('Ctrl Pts',(9.35386441150747,-25.7703500754572,12.808672884462));
#85450=CARTESIAN_POINT('Ctrl Pts',(9.36283322025893,-25.7723098092211,12.7990126145978));
#85451=CARTESIAN_POINT('Ctrl Pts',(9.37216502621645,-25.7733606539579,12.7889427107013));
#85452=CARTESIAN_POINT('Ctrl Pts',(9.37724758285781,-25.7739329952519,12.7834581499249));
#85453=CARTESIAN_POINT('Ctrl Pts',(9.38243724338762,-25.7742356128009,12.7778526977998));
#85454=CARTESIAN_POINT('Ctrl Pts',(9.38771846805,-25.7742356128,12.7721409138));
#85455=CARTESIAN_POINT('',(8.59814925255,-25.4742356128,12.4506765244));
#85456=CARTESIAN_POINT('',(8.21591479143,-25.7742356128,11.6886688365));
#85457=CARTESIAN_POINT('Origin',(8.21591479143,-25.4742356128,11.6886688365));
#85458=CARTESIAN_POINT('',(8.80181662974,-25.7742356128,12.2304048752));
#85459=CARTESIAN_POINT('Origin',(8.21591479143,-25.4742356128,11.6886688365));
#85460=CARTESIAN_POINT('Origin',(8.21591479143,-25.4742356128,11.6886688365));
#85461=CARTESIAN_POINT('Origin',(-1.62597327472E-14,-25.4742356128,0.580061096523));
#85462=CARTESIAN_POINT('',(8.93001206801,-25.7742356128,11.1231776304));
#85463=CARTESIAN_POINT('Origin',(-3.09260596606E-16,-25.7742356128,0.580061096523));
#85464=CARTESIAN_POINT('Origin',(8.93001206801,-25.4742356128,11.1231776304));
#85465=CARTESIAN_POINT('Origin',(8.93001206801,-25.4742356128,11.1231776304));
#85466=CARTESIAN_POINT('Origin',(8.93001206801,-25.4742356128,11.1231776304));
#85467=CARTESIAN_POINT('Origin',(9.58357319026,-25.4742356128,11.7274727362));
#85468=CARTESIAN_POINT('',(9.39452601497,-25.7742356128,11.5526761045));
#85469=CARTESIAN_POINT('',(9.16226904149,-25.7742356128,11.3379268674));
#85470=CARTESIAN_POINT('',(9.59819339216,-25.4742356128,11.3324044552));
#85471=CARTESIAN_POINT('',(9.36593641868,-25.4742356128,11.1176552182));
#85472=CARTESIAN_POINT('Origin',(9.39452601497,-25.4742356128,11.5526761045));
#85473=CARTESIAN_POINT('Origin',(9.80186076935,-25.4742356128,11.1121328059));
#85474=CARTESIAN_POINT('',(10.2106256241,-25.7742356128,11.5513494877));
#85475=CARTESIAN_POINT('Origin',(9.80186076935,-25.7742356128,11.1121328059));
#85476=CARTESIAN_POINT('',(10.0062431967,-25.4742356128,11.3317411468));
#85477=CARTESIAN_POINT('Origin',(9.80186076935,-25.4742356128,11.1121328059));
#85478=CARTESIAN_POINT('Origin',(10.2106256241,-25.4742356128,11.5513494877));
#85479=CARTESIAN_POINT('Origin',(3.28019248617E-15,-25.4742356128,0.580061096523));
#85480=CARTESIAN_POINT('',(11.256975342,-25.7742356128,10.4748350074));
#85481=CARTESIAN_POINT('Origin',(8.59564264812E-16,-25.7742356128,0.580061096523));
#85482=CARTESIAN_POINT('Origin',(-2.72521192632E-16,-25.4742356128,0.580061096523));
#85483=CARTESIAN_POINT('Origin',(11.256975342,-25.4742356128,10.4748350074));
#85484=CARTESIAN_POINT('Origin',(10.806321674,-25.4742356128,10.0787147334));
#85485=CARTESIAN_POINT('',(11.3756644412,-25.7742356128,10.2680525622));
#85486=CARTESIAN_POINT('Origin',(10.806321674,-25.7742356128,10.0787147334));
#85487=CARTESIAN_POINT('Origin',(11.3756644412,-25.4742356128,10.2680525622));
#85488=CARTESIAN_POINT('Origin',(-2.84607155346,-25.4742356128,5.53854202767));
#85489=CARTESIAN_POINT('',(11.4519644969,-25.7742356128,10.0321162953));
#85490=CARTESIAN_POINT('Origin',(-2.84607155346,-25.7742356128,5.53854202767));
#85491=CARTESIAN_POINT('Origin',(-2.84607155346,-25.4742356128,5.53854202767));
#85492=CARTESIAN_POINT('Origin',(11.4519644969,-25.4742356128,10.0321162953));
#85493=CARTESIAN_POINT('Origin',(10.8795671881,-25.4742356128,9.85222376962));
#85494=CARTESIAN_POINT('',(11.2869019425,-25.7742356128,9.4116804711));
#85495=CARTESIAN_POINT('Origin',(10.8795671881,-25.7742356128,9.85222376962));
#85496=CARTESIAN_POINT('Origin',(11.2869019425,-25.4742356128,9.4116804711));
#85497=CARTESIAN_POINT('Origin',(11.2845726092,-25.4742356128,9.409526725));
#85498=CARTESIAN_POINT('',(10.9076228609,-25.7742356128,9.06099178277));
#85499=CARTESIAN_POINT('',(11.0972624017,-25.7742356128,9.23633612693));
#85500=CARTESIAN_POINT('Origin',(10.9076228609,-25.4742356128,9.06099178277));
#85501=CARTESIAN_POINT('Origin',(10.9076228609,-25.4742356128,9.06099178277));
#85502=CARTESIAN_POINT('Origin',(10.9076228609,-25.4742356128,9.06099178277));
#85503=CARTESIAN_POINT('Origin',(2.10437608802E-14,-25.4742356128,0.580061096523));
#85504=CARTESIAN_POINT('',(11.4401704731,-25.7742356128,8.32763628675));
#85505=CARTESIAN_POINT('Origin',(-3.09260596606E-16,-25.7742356128,0.580061096523));
#85506=CARTESIAN_POINT('Origin',(11.4401704731,-25.4742356128,8.32763628675));
#85507=CARTESIAN_POINT('Origin',(11.4401704731,-25.4742356128,8.32763628675));
#85508=CARTESIAN_POINT('Origin',(11.4401704731,-25.4742356128,8.32763628675));
#85509=CARTESIAN_POINT('Origin',(11.9474180872,-25.4742356128,8.79664712633));
#85510=CARTESIAN_POINT('',(12.5441720511,-25.7742356128,9.34841724773));
#85511=CARTESIAN_POINT('Ctrl Pts',(12.5441720511,-25.7742356128,9.34841724773));
#85512=CARTESIAN_POINT('Ctrl Pts',(12.5539822763409,-25.7742356128001,9.33780722995768));
#85513=CARTESIAN_POINT('Ctrl Pts',(12.5634456430601,-25.7731910200537,9.3275154089535));
#85514=CARTESIAN_POINT('Ctrl Pts',(12.5724911176183,-25.7713070166777,9.31765005053512));
#85515=CARTESIAN_POINT('Ctrl Pts',(12.5817733359601,-25.7693737039942,9.30752648982309));
#85516=CARTESIAN_POINT('Ctrl Pts',(12.590615701935,-25.7665572829415,9.29785179003076));
#85517=CARTESIAN_POINT('Ctrl Pts',(12.5989798508501,-25.7630785008082,9.28870141850777));
#85518=CARTESIAN_POINT('Ctrl Pts',(12.6077176009545,-25.7594443320175,9.27914232761384));
#85519=CARTESIAN_POINT('Ctrl Pts',(12.6159336998732,-25.7550880979871,9.27015519076182));
#85520=CARTESIAN_POINT('Ctrl Pts',(12.623622484751,-25.7502477283811,9.26178486645217));
#85521=CARTESIAN_POINT('Ctrl Pts',(12.6283279817392,-25.7472854469589,9.25666227082029));
#85522=CARTESIAN_POINT('Ctrl Pts',(12.6328367078553,-25.7441415029729,9.2517699072643));
#85523=CARTESIAN_POINT('Ctrl Pts',(12.6371532053515,-25.7408663583315,9.24711174163293));
#85524=CARTESIAN_POINT('Ctrl Pts',(12.6446891080961,-25.7351484883423,9.23897934188115));
#85525=CARTESIAN_POINT('Ctrl Pts',(12.6516265314871,-25.7290305922244,9.23154438354611));
#85526=CARTESIAN_POINT('Ctrl Pts',(12.6579848548716,-25.7227419730146,9.22475891729431));
#85527=CARTESIAN_POINT('Ctrl Pts',(12.662046954928,-25.7187244044039,9.22042393129609));
#85528=CARTESIAN_POINT('Ctrl Pts',(12.665873268387,-25.714636311481,9.2163534156184));
#85529=CARTESIAN_POINT('Ctrl Pts',(12.6694732315878,-25.710528583226,9.21253012695852));
#85530=CARTESIAN_POINT('Ctrl Pts',(12.6740906881256,-25.7052598469562,9.2076262242703));
#85531=CARTESIAN_POINT('Ctrl Pts',(12.6783349748146,-25.6999590815914,9.20312778888616));
#85532=CARTESIAN_POINT('Ctrl Pts',(12.6822277695392,-25.6947156622293,9.19898775635845));
#85533=CARTESIAN_POINT('Ctrl Pts',(12.6841741669014,-25.6920939525483,9.1969177400946));
#85534=CARTESIAN_POINT('Ctrl Pts',(12.6860327378614,-25.6894862802653,9.19493721400768));
#85535=CARTESIAN_POINT('Ctrl Pts',(12.6878063838999,-25.6869020998827,9.19303982266937));
#85536=CARTESIAN_POINT('Ctrl Pts',(12.6887246962375,-25.6855641301432,9.19205744070731));
#85537=CARTESIAN_POINT('Ctrl Pts',(12.6894223110675,-25.6845279385757,9.19131139879719));
#85538=CARTESIAN_POINT('Ctrl Pts',(12.6902095492152,-25.6833392669281,9.19046563803261));
#85539=CARTESIAN_POINT('Ctrl Pts',(12.6909427979048,-25.6822321153875,9.18967788025659));
#85540=CARTESIAN_POINT('Ctrl Pts',(12.6917542381505,-25.6809931412886,9.18880313678734));
#85541=CARTESIAN_POINT('Ctrl Pts',(12.6928755092835,-25.6792284128773,9.18759052905043));
#85542=CARTESIAN_POINT('Ctrl Pts',(12.7010717825987,-25.6663285923428,9.17872660297269));
#85543=CARTESIAN_POINT('Ctrl Pts',(12.7083456542452,-25.6525959016894,9.17086003188428));
#85544=CARTESIAN_POINT('Ctrl Pts',(12.7146889305147,-25.6382910415628,9.16399975905503));
#85545=CARTESIAN_POINT('Ctrl Pts',(12.7215940637009,-25.6227191256968,9.15653183623932));
#85546=CARTESIAN_POINT('Ctrl Pts',(12.7273969802182,-25.6064695638937,9.15025579407772));
#85547=CARTESIAN_POINT('Ctrl Pts',(12.7321138526963,-25.5898298670075,9.14515424664999));
#85548=CARTESIAN_POINT('Ctrl Pts',(12.737124295717,-25.5721545421994,9.13973518713073));
#85549=CARTESIAN_POINT('Ctrl Pts',(12.7409100277816,-25.5540387942889,9.13564058265248));
#85550=CARTESIAN_POINT('Ctrl Pts',(12.7435088166785,-25.5357731503047,9.13282971245183));
#85551=CARTESIAN_POINT('Ctrl Pts',(12.746416898406,-25.5153336349699,9.12968430872993));
#85552=CARTESIAN_POINT('Ctrl Pts',(12.7478394282971,-25.4947060095316,9.12814559847313));
#85553=CARTESIAN_POINT('Ctrl Pts',(12.7478394282971,-25.4742356128,9.12814559847313));
#85554=CARTESIAN_POINT('',(11.9921712621,-25.7742356128,8.83802676724));
#85555=CARTESIAN_POINT('Origin',(-3.18408167778E-16,-25.7742356128,0.729452270839));
#85556=CARTESIAN_POINT('',(12.1784264826,-25.7742356128,9.98548488886));
#85557=CARTESIAN_POINT('Origin',(10.0415172382,-25.7742356128,8.33514586886));
#85558=CARTESIAN_POINT('Origin',(-3.09260596606E-16,-25.7742356128,0.580061096523));
#85559=CARTESIAN_POINT('Origin',(3.39394702409,-23.1742356128,-9.39793292047));
#85560=CARTESIAN_POINT('',(3.39394702409,-21.0742356128,-7.0794205347));
#85561=CARTESIAN_POINT('',(3.39394702409,-25.4742356128,-7.0794205347));
#85562=CARTESIAN_POINT('',(3.39394702409,-23.2742356128,-7.0794205347));
#85563=CARTESIAN_POINT('',(3.39394702409,-25.4742356128,-9.19678210318));
#85564=CARTESIAN_POINT('',(3.39394702409,-25.4742356128,-8.58812386759));
#85565=CARTESIAN_POINT('',(3.39394702409,-23.4742356128,-9.19678210416077));
#85566=CARTESIAN_POINT('',(3.39394702409,-23.2742356128,-9.19678210318));
#85567=CARTESIAN_POINT('',(3.39394702409,-23.4742356128,-7.94679080481));
#85568=CARTESIAN_POINT('',(3.39394702409,-23.4742356128,3.39628270998));
#85569=CARTESIAN_POINT('',(3.39394702409,-22.8742356071,-7.27665075406));
#85570=CARTESIAN_POINT('Ctrl Pts',(3.39394702409,-22.8742356071,-7.27665075406));
#85571=CARTESIAN_POINT('Ctrl Pts',(3.39394702409,-22.8963796807801,-7.27665075202916));
#85572=CARTESIAN_POINT('Ctrl Pts',(3.39394702409,-22.9185266226574,-7.27803164667852));
#85573=CARTESIAN_POINT('Ctrl Pts',(3.39394702409019,-22.9404763729725,-7.28076880448012));
#85574=CARTESIAN_POINT('Ctrl Pts',(3.39394702409038,-22.9635612306701,-7.28364751141022));
#85575=CARTESIAN_POINT('Ctrl Pts',(3.39394702409077,-22.9864277437381,-7.28802596271889));
#85576=CARTESIAN_POINT('Ctrl Pts',(3.39394702409072,-23.0088766193784,-7.29382800372885));
#85577=CARTESIAN_POINT('Ctrl Pts',(3.3939470240907,-23.0181604618048,-7.29622746619418));
#85578=CARTESIAN_POINT('Ctrl Pts',(3.39394702409061,-23.0273732778489,-7.29886989897477));
#85579=CARTESIAN_POINT('Ctrl Pts',(3.39394702409046,-23.0365026587174,-7.30174800896343));
#85580=CARTESIAN_POINT('Ctrl Pts',(3.39394702409007,-23.0599555275722,-7.30914171255472));
#85581=CARTESIAN_POINT('Ctrl Pts',(3.39394702409004,-23.0828466467018,-7.31809082810804));
#85582=CARTESIAN_POINT('Ctrl Pts',(3.39394702409001,-23.1049940708735,-7.32844271008414));
#85583=CARTESIAN_POINT('Ctrl Pts',(3.39394702408999,-23.1281264931002,-7.33925498797506));
#85584=CARTESIAN_POINT('Ctrl Pts',(3.39394702409,-23.1504472805791,-7.35159636510977));
#85585=CARTESIAN_POINT('Ctrl Pts',(3.39394702409,-23.1717995438951,-7.36526779521605));
#85586=CARTESIAN_POINT('Ctrl Pts',(3.39394702409,-23.1802621945299,-7.37068626233385));
#85587=CARTESIAN_POINT('Ctrl Pts',(3.39394702409,-23.1885732730389,-7.37631349194848));
#85588=CARTESIAN_POINT('Ctrl Pts',(3.39394702409,-23.1967252289902,-7.38213675751289));
#85589=CARTESIAN_POINT('Ctrl Pts',(3.39394702409,-23.216964154042,-7.39659422465562));
#85590=CARTESIAN_POINT('Ctrl Pts',(3.39394702409,-23.2362264780343,-7.41226456121671));
#85591=CARTESIAN_POINT('Ctrl Pts',(3.39394702409,-23.2544248664386,-7.42895825046336));
#85592=CARTESIAN_POINT('Ctrl Pts',(3.39394702409,-23.2663051018241,-7.43985619116538));
#85593=CARTESIAN_POINT('Ctrl Pts',(3.39394702409,-23.2777329032204,-7.45119035077379));
#85594=CARTESIAN_POINT('Ctrl Pts',(3.39394702409,-23.2886950564466,-7.46291290030111));
#85595=CARTESIAN_POINT('Ctrl Pts',(3.39394702409,-23.3092436284265,-7.48488683624042));
#85596=CARTESIAN_POINT('Ctrl Pts',(3.39394702407267,-23.3281539933134,-7.5082252168758));
#85597=CARTESIAN_POINT('Ctrl Pts',(3.39394702415533,-23.3453669419493,-7.53263177580096));
#85598=CARTESIAN_POINT('Ctrl Pts',(3.39394702418428,-23.351396654865,-7.54118141750917));
#85599=CARTESIAN_POINT('Ctrl Pts',(3.39394702422707,-23.3572183823464,-7.54986251226728));
#85600=CARTESIAN_POINT('Ctrl Pts',(3.39394702429189,-23.3628304875723,-7.55866347490331));
#85601=CARTESIAN_POINT('Ctrl Pts',(3.39394702449706,-23.3805929863697,-7.58651881295321));
#85602=CARTESIAN_POINT('Ctrl Pts',(3.39394702467124,-23.3962633147006,-7.61557726389403));
#85603=CARTESIAN_POINT('Ctrl Pts',(3.39394702467555,-23.4098082144408,-7.64551044052));
#85604=CARTESIAN_POINT('Ctrl Pts',(3.39394702468063,-23.4257384366872,-7.68071499465771));
#85605=CARTESIAN_POINT('Ctrl Pts',(3.39394702450576,-23.4387297283905,-7.71712955274666));
#85606=CARTESIAN_POINT('Ctrl Pts',(3.3939470243646,-23.448763496914,-7.75428420736052));
#85607=CARTESIAN_POINT('Ctrl Pts',(3.39394702420207,-23.4603148681498,-7.79705848579653));
#85608=CARTESIAN_POINT('Ctrl Pts',(3.39394702411207,-23.4679503272946,-7.84081579026664));
#85609=CARTESIAN_POINT('Ctrl Pts',(3.39394702409605,-23.4716451363039,-7.88490127919122));
#85610=CARTESIAN_POINT('Ctrl Pts',(3.39394702408857,-23.4733699118574,-7.90548084727437));
#85611=CARTESIAN_POINT('Ctrl Pts',(3.39394702409,-23.4742356128,-7.92613251437262));
#85612=CARTESIAN_POINT('Ctrl Pts',(3.39394702409,-23.4742356128,-7.94679080481));
#85613=CARTESIAN_POINT('',(3.39394702409,-21.0742356128,-7.27665075431));
#85614=CARTESIAN_POINT('',(3.39394702409,-23.1223803511,-7.27665075431));
#85615=CARTESIAN_POINT('',(3.39394702409,-21.0742356128,-6.14889144395));
#85616=CARTESIAN_POINT('Origin',(3.09394702409,-23.2742356128,-7.0794205347));
#85617=CARTESIAN_POINT('',(2.96616998276,-21.0742356128,-6.8079927769));
#85618=CARTESIAN_POINT('Origin',(3.09394702409,-21.0742356128,-7.0794205347));
#85619=CARTESIAN_POINT('',(2.96616998276,-25.4742356128,-6.8079927769));
#85620=CARTESIAN_POINT('',(2.96616998276,-22.6642356128,-6.8079927769));
#85621=CARTESIAN_POINT('Origin',(3.09394702409,-25.4742356128,-7.0794205347));
#85622=CARTESIAN_POINT('Origin',(-2.84607155346,-22.6642356128,5.53854202767));
#85623=CARTESIAN_POINT('',(2.60391380109,-21.0742356128,-6.97212274247));
#85624=CARTESIAN_POINT('',(2.60391380109,-25.4742356128,-6.97212274247));
#85625=CARTESIAN_POINT('',(2.60391380109,-23.2742356128,-6.97212274247));
#85626=CARTESIAN_POINT('Origin',(-2.84607155346,-25.4742356128,5.53854202767));
#85627=CARTESIAN_POINT('Origin',(-2.84607155346,-21.0742356128,5.53854202767));
#85628=CARTESIAN_POINT('Origin',(2.72372695744,-23.2742356128,-7.24715875387));
#85629=CARTESIAN_POINT('',(2.42372695744,-21.0742356128,-7.24715875387));
#85630=CARTESIAN_POINT('Origin',(2.72372695744,-21.0742356128,-7.24715875387));
#85631=CARTESIAN_POINT('',(2.42372695744,-25.4742356128,-7.24715875387));
#85632=CARTESIAN_POINT('',(2.42372695744,-23.2742356128,-7.24715875387));
#85633=CARTESIAN_POINT('Origin',(2.72372695744,-25.4742356128,-7.24715875387));
#85634=CARTESIAN_POINT('Origin',(2.42372695744,-23.1742356128,-8.1710440518));
#85635=CARTESIAN_POINT('',(2.42372695744,-21.0742356128,-7.96338790087));
#85636=CARTESIAN_POINT('',(2.42372695744,-21.0742356128,-6.11170048962));
#85637=CARTESIAN_POINT('',(2.42372695744,-25.4742356128,-7.96338790087));
#85638=CARTESIAN_POINT('',(2.42372695744,-23.2742356128,-7.96338790087));
#85639=CARTESIAN_POINT('',(2.42372695744,-25.4742356128,-8.58812386759));
#85640=CARTESIAN_POINT('Origin',(2.12372695744,-23.2742356128,-7.96338790087));
#85641=CARTESIAN_POINT('',(2.22735416732,-25.4742356128,-8.24492191546));
#85642=CARTESIAN_POINT('',(2.22735416732,-21.0742356128,-8.24492191546));
#85643=CARTESIAN_POINT('',(2.22735416732,-22.6642356128,-8.24492191546));
#85644=CARTESIAN_POINT('Origin',(2.12372695744,-25.4742356128,-7.96338790087));
#85645=CARTESIAN_POINT('Ctrl Pts',(2.22735416732076,-21.0742356128,-8.24492191546207));
#85646=CARTESIAN_POINT('Ctrl Pts',(2.24108151060133,-21.0742356128001,-8.23986914666857));
#85647=CARTESIAN_POINT('Ctrl Pts',(2.25402468097048,-21.0741856837446,-8.2339643074798));
#85648=CARTESIAN_POINT('Ctrl Pts',(2.26612777278258,-21.0741202589394,-8.22743715345324));
#85649=CARTESIAN_POINT('Ctrl Pts',(2.27875418582157,-21.0740520052548,-8.22062777416504));
#85650=CARTESIAN_POINT('Ctrl Pts',(2.29046668928501,-21.0739668868197,-8.21314184239419));
#85651=CARTESIAN_POINT('Ctrl Pts',(2.30125680627737,-21.0739039993993,-8.20522080345313));
#85652=CARTESIAN_POINT('Ctrl Pts',(2.31096366691234,-21.0738474254599,-8.19809498441526));
#85653=CARTESIAN_POINT('Ctrl Pts',(2.31992518748148,-21.0738088429042,-8.19061695362599));
#85654=CARTESIAN_POINT('Ctrl Pts',(2.32816585676089,-21.0738167151887,-8.1829436715627));
#85655=CARTESIAN_POINT('Ctrl Pts',(2.33583411214787,-21.0738240406482,-8.17580339150502));
#85656=CARTESIAN_POINT('Ctrl Pts',(2.34299563004193,-21.0738628977486,-8.16837895699461));
#85657=CARTESIAN_POINT('Ctrl Pts',(2.34958037155088,-21.0739142203341,-8.16084735325064));
#85658=CARTESIAN_POINT('Ctrl Pts',(2.35632821361967,-21.0739668141528,-8.15312919567072));
#85659=CARTESIAN_POINT('Ctrl Pts',(2.36247022703321,-21.0740324986314,-8.14529944422524));
#85660=CARTESIAN_POINT('Ctrl Pts',(2.36798314853736,-21.0740907554554,-8.13756859185097));
#85661=CARTESIAN_POINT('Ctrl Pts',(2.37385294559234,-21.0741527834987,-8.12933728754802));
#85662=CARTESIAN_POINT('Ctrl Pts',(2.3790097036189,-21.0742063911124,-8.12121921958259));
#85663=CARTESIAN_POINT('Ctrl Pts',(2.38348457893087,-21.0742268117467,-8.11347446948094));
#85664=CARTESIAN_POINT('Ctrl Pts',(2.38470841967809,-21.0742323966183,-8.11135634549074));
#85665=CARTESIAN_POINT('Ctrl Pts',(2.38588156616565,-21.074235499182,-8.10926612248979));
#85666=CARTESIAN_POINT('Ctrl Pts',(2.38700529704613,-21.0742356128,-8.10720902551531));
#85667=CARTESIAN_POINT('Ctrl Pts',(2.39285425271468,-21.0742362041755,-8.09650195212366));
#85668=CARTESIAN_POINT('Ctrl Pts',(2.39788657480719,-21.0742365265271,-8.08574567897341));
#85669=CARTESIAN_POINT('Ctrl Pts',(2.40220661886468,-21.0742366716414,-8.07496333800916));
#85670=CARTESIAN_POINT('Ctrl Pts',(2.4067318406694,-21.0742368236478,-8.06366889661274));
#85671=CARTESIAN_POINT('Ctrl Pts',(2.41047617380133,-21.0742367811817,-8.05234499029572));
#85672=CARTESIAN_POINT('Ctrl Pts',(2.41351966652779,-21.0742366497387,-8.04097775690518));
#85673=CARTESIAN_POINT('Ctrl Pts',(2.4166090583842,-21.0742365163134,-8.02943909346062));
#85674=CARTESIAN_POINT('Ctrl Pts',(2.41897665741814,-21.0742362912073,-8.0178546901109));
#85675=CARTESIAN_POINT('Ctrl Pts',(2.42065864862612,-21.0742360847615,-8.00618475553654));
#85676=CARTESIAN_POINT('Ctrl Pts',(2.42234140953528,-21.0742358782212,-7.9945094806475));
#85677=CARTESIAN_POINT('Ctrl Pts',(2.42333809291483,-21.0742356903582,-7.98274747425376));
#85678=CARTESIAN_POINT('Ctrl Pts',(2.42363412571554,-21.0742356316651,-7.97085050208861));
#85679=CARTESIAN_POINT('Ctrl Pts',(2.42369587368949,-21.0742356194226,-7.96836897326607));
#85680=CARTESIAN_POINT('Ctrl Pts',(2.42372695744,-21.0742356128,-7.96588157712267));
#85681=CARTESIAN_POINT('Ctrl Pts',(2.42372695744,-21.0742356128,-7.96338790087));
#85682=CARTESIAN_POINT('Origin',(3.09394702409,-23.2742356128,-9.19678210318));
#85683=CARTESIAN_POINT('',(3.20611083607784,-23.4742356128,-9.47502535777846));
#85684=CARTESIAN_POINT('Origin',(3.09394702409,-23.4742356128,-9.19678210318));
#85685=CARTESIAN_POINT('',(3.20611081633,-25.4742356128,-9.47502531282));
#85686=CARTESIAN_POINT('Origin',(3.09394702409,-25.4742356128,-9.19678210318));
#85687=CARTESIAN_POINT('',(3.20611081633,-20.0742356128,-9.47502531282));
#85688=CARTESIAN_POINT('Origin',(3.09394702409,-25.4742356128,-8.58812386759));
#85689=CARTESIAN_POINT('',(3.09394702409,-25.7742356128,-7.0794205347));
#85690=CARTESIAN_POINT('',(3.09394702409,-25.7742356128,-9.19678210318));
#85691=CARTESIAN_POINT('',(3.09394702409,-25.7742356128,-8.13810131894));
#85692=CARTESIAN_POINT('Origin',(3.09394702409,-25.4742356128,-9.19678210318));
#85693=CARTESIAN_POINT('Origin',(3.09394702409,-25.4742356128,-7.0794205347));
#85694=CARTESIAN_POINT('Origin',(3.09394702409,-25.4742356128,-7.0794205347));
#85695=CARTESIAN_POINT('Origin',(3.09394702409,-25.4742356128,-7.0794205347));
#85696=CARTESIAN_POINT('Origin',(-2.84607155346,-25.4742356128,5.53854202767));
#85697=CARTESIAN_POINT('',(2.72372695744,-25.7742356128,-7.24715875387));
#85698=CARTESIAN_POINT('Origin',(-2.84607155346,-25.7742356128,5.53854202767));
#85699=CARTESIAN_POINT('Origin',(2.72372695744,-25.4742356128,-7.24715875387));
#85700=CARTESIAN_POINT('Origin',(2.72372695744,-25.4742356128,-7.24715875387));
#85701=CARTESIAN_POINT('Origin',(2.72372695744,-25.4742356128,-7.24715875387));
#85702=CARTESIAN_POINT('Origin',(2.72372695744,-25.4742356128,-8.58812386759));
#85703=CARTESIAN_POINT('',(2.72372695744,-25.7742356128,-7.96338790087));
#85704=CARTESIAN_POINT('',(2.72372695744,-25.7742356128,-7.60527332737));
#85705=CARTESIAN_POINT('Origin',(2.72372695744,-25.4742356128,-7.96338790087));
#85706=CARTESIAN_POINT('Origin',(2.12372695744,-25.4742356128,-7.96338790087));
#85707=CARTESIAN_POINT('',(2.3309813772,-25.7742356128,-8.52645593005));
#85708=CARTESIAN_POINT('Origin',(2.12372695744,-25.7742356128,-7.96338790087));
#85709=CARTESIAN_POINT('Origin',(2.3309813772,-25.4742356128,-8.52645593005));
#85710=CARTESIAN_POINT('Origin',(-2.84607155346,-25.4742356128,5.53854202767));
#85711=CARTESIAN_POINT('',(-2.3573467526E-14,-25.7742356128,-9.1762777575));
#85712=CARTESIAN_POINT('',(0.207931717439474,-25.4742356128,-8.82796732002595));
#85713=CARTESIAN_POINT('Ctrl Pts',(-2.3573467526E-14,-25.7742356128,-9.1762777575));
#85714=CARTESIAN_POINT('Ctrl Pts',(0.0543179010637,-25.7751862689,-9.07845703679));
#85715=CARTESIAN_POINT('Ctrl Pts',(0.109343357832,-25.7400248661,-8.98386898437));
#85716=CARTESIAN_POINT('Ctrl Pts',(0.16325179783,-25.6940006666,-8.89703057892));
#85717=CARTESIAN_POINT('Ctrl Pts',(0.208904902043,-25.586489454,-8.82655958228));
#85718=CARTESIAN_POINT('Ctrl Pts',(0.207931718075,-25.4742356128,-8.82796731988));
#85719=CARTESIAN_POINT('Origin',(-2.84607155346,-25.7742356128,5.53854202767));
#85720=CARTESIAN_POINT('Origin',(-2.84607155346,-25.4742356128,5.53854202767));
#85721=CARTESIAN_POINT('Origin',(3.09394702409,-25.4742356128,-9.19678210318));
#85722=CARTESIAN_POINT('Origin',(3.09394702409,-25.4742356128,-9.19678210318));
#85723=CARTESIAN_POINT('Origin',(-2.84607155346,-25.4742356128,5.53854202767));
#85724=CARTESIAN_POINT('',(-3.64520546117E-14,-25.7742356128,-10.0919881826));
#85725=CARTESIAN_POINT('',(0.647446102181,-25.4742356128,-10.2675153591));
#85726=CARTESIAN_POINT('Ctrl Pts',(2.77555756156289E-16,-25.7742356128,
-10.0919881826));
#85727=CARTESIAN_POINT('Ctrl Pts',(0.0127666947406751,-25.7742356128,-10.0968936681105));
#85728=CARTESIAN_POINT('Ctrl Pts',(0.0271180838392129,-25.7739854886413,
-10.1023205735565));
#85729=CARTESIAN_POINT('Ctrl Pts',(0.0431487367547728,-25.773293591676,
-10.1082196250995));
#85730=CARTESIAN_POINT('Ctrl Pts',(0.05389738199205,-25.7728296707701,-10.1121749731822));
#85731=CARTESIAN_POINT('Ctrl Pts',(0.065400894022011,-25.7721663394268,
-10.1163419506036));
#85732=CARTESIAN_POINT('Ctrl Pts',(0.0776850226532396,-25.7712351361557,
-10.1206985310685));
#85733=CARTESIAN_POINT('Ctrl Pts',(0.0929874322081948,-25.7700751308952,
-10.1261255483634));
#85734=CARTESIAN_POINT('Ctrl Pts',(0.109500172992918,-25.7684996343647,
-10.1318460369282));
#85735=CARTESIAN_POINT('Ctrl Pts',(0.127205102846768,-25.7663646795551,
-10.1377881312263));
#85736=CARTESIAN_POINT('Ctrl Pts',(0.136057567773693,-25.7652972021504,
-10.1407591783753));
#85737=CARTESIAN_POINT('Ctrl Pts',(0.144896818651612,-25.7641306876289,
-10.1436826499001));
#85738=CARTESIAN_POINT('Ctrl Pts',(0.154175043372714,-25.7627912803035,
-10.1467024954506));
#85739=CARTESIAN_POINT('Ctrl Pts',(0.163453268093816,-25.761451872978,-10.1497223410011));
#85740=CARTESIAN_POINT('Ctrl Pts',(0.173170690817713,-25.7599402451658,
-10.1528388311902));
#85741=CARTESIAN_POINT('Ctrl Pts',(0.183778538386152,-25.7581340314033,
-10.1561762498561));
#85742=CARTESIAN_POINT('Ctrl Pts',(0.201065198147305,-25.7551906064939,
-10.161614942351));
#85743=CARTESIAN_POINT('Ctrl Pts',(0.217387269440654,-25.7520155315348,
-10.1666030373977));
#85744=CARTESIAN_POINT('Ctrl Pts',(0.232709678556698,-25.7487351314624,
-10.1711799585317));
#85745=CARTESIAN_POINT('Ctrl Pts',(0.249222845736503,-25.7451998000141,
-10.1761125682331));
#85746=CARTESIAN_POINT('Ctrl Pts',(0.264575283226697,-25.7415419604595,
-10.1805680336023));
#85747=CARTESIAN_POINT('Ctrl Pts',(0.278780403189311,-25.7379006349803,
-10.1845847080561));
#85748=CARTESIAN_POINT('Ctrl Pts',(0.283747727460943,-25.7366273163121,
-10.1859892808128));
#85749=CARTESIAN_POINT('Ctrl Pts',(0.288575211171245,-25.7353558696552,
-10.1873400786056));
#85750=CARTESIAN_POINT('Ctrl Pts',(0.293264740388737,-25.7340918048577,
-10.1886383529592));
#85751=CARTESIAN_POINT('Ctrl Pts',(0.306688881619296,-25.7304733213002,
-10.1923547640251));
#85752=CARTESIAN_POINT('Ctrl Pts',(0.318964875652885,-25.7269134297011,
-10.1956507029994));
#85753=CARTESIAN_POINT('Ctrl Pts',(0.330098484404839,-25.7235154506728,
-10.1985807972922));
#85754=CARTESIAN_POINT('Ctrl Pts',(0.33163100564525,-25.7230477249649,-10.1989841195069));
#85755=CARTESIAN_POINT('Ctrl Pts',(0.333141857760913,-25.7225830413197,
-10.1993804990849));
#85756=CARTESIAN_POINT('Ctrl Pts',(0.334630964292926,-25.7221216340532,
-10.1997700635937));
#85757=CARTESIAN_POINT('Ctrl Pts',(0.340784620245485,-25.7202148923185,
-10.2013799188375));
#85758=CARTESIAN_POINT('Ctrl Pts',(0.34656837976259,-25.7183638800075,-10.2028735271497));
#85759=CARTESIAN_POINT('Ctrl Pts',(0.35198311466046,-25.7165836270321,-10.2042604508819));
#85760=CARTESIAN_POINT('Ctrl Pts',(0.354690482109395,-25.7156935005444,
-10.2049539127479));
#85761=CARTESIAN_POINT('Ctrl Pts',(0.35730559201964,-25.7148210565333,-10.2056206967166));
#85762=CARTESIAN_POINT('Ctrl Pts',(0.359828577161451,-25.7139680222366,
-10.2062620182685));
#85763=CARTESIAN_POINT('Ctrl Pts',(0.361090069732355,-25.7135415050882,
-10.2065826790445));
#85764=CARTESIAN_POINT('Ctrl Pts',(0.362323886515271,-25.7131202917207,
-10.2068973089369));
#85765=CARTESIAN_POINT('Ctrl Pts',(0.363535529846051,-25.7127040568142,
-10.2072056663922));
#85766=CARTESIAN_POINT('Ctrl Pts',(0.364650472969556,-25.712321041256,-10.2074894141054));
#85767=CARTESIAN_POINT('Ctrl Pts',(0.364770803899085,-25.7122807741327,
-10.2075203139685));
#85768=CARTESIAN_POINT('Ctrl Pts',(0.366590937652134,-25.7116489007287,
-10.2079818068637));
#85769=CARTESIAN_POINT('Ctrl Pts',(0.366748799795484,-25.7115940976738,
-10.2080218326351));
#85770=CARTESIAN_POINT('Ctrl Pts',(0.366919439077047,-25.7115348150142,
-10.2080650866454));
#85771=CARTESIAN_POINT('Ctrl Pts',(0.367104605833077,-25.7114704193595,
-10.2081120060478));
#85772=CARTESIAN_POINT('Ctrl Pts',(0.389501333108037,-25.7036814838767,
-10.2137871125346));
#85773=CARTESIAN_POINT('Ctrl Pts',(0.410401281874009,-25.6955112103493,
-10.2188521723151));
#85774=CARTESIAN_POINT('Ctrl Pts',(0.429803208558037,-25.6871592795531,
-10.2233953578027));
#85775=CARTESIAN_POINT('Ctrl Pts',(0.442559404690514,-25.6816681307071,
-10.2263823686336));
#85776=CARTESIAN_POINT('Ctrl Pts',(0.454670476409811,-25.6760980541835,
-10.2291439086179));
#85777=CARTESIAN_POINT('Ctrl Pts',(0.466122175642957,-25.6704997865415,
-10.2316997585462));
#85778=CARTESIAN_POINT('Ctrl Pts',(0.480556931371571,-25.6634432245178,
-10.2349213825727));
#85779=CARTESIAN_POINT('Ctrl Pts',(0.493936616845627,-25.6563383359936,
-10.2378216347637));
#85780=CARTESIAN_POINT('Ctrl Pts',(0.506275616356922,-25.649249086395,-10.2404322659966));
#85781=CARTESIAN_POINT('Ctrl Pts',(0.512445116112571,-25.6457044615957,
-10.2417375816131));
#85782=CARTESIAN_POINT('Ctrl Pts',(0.518354491225542,-25.6421636198033,
-10.2429701357078));
#85783=CARTESIAN_POINT('Ctrl Pts',(0.524003849100926,-25.638633533667,-10.2441336784079));
#85784=CARTESIAN_POINT('Ctrl Pts',(0.526235482565565,-25.6372390639717,
-10.2445933060124));
#85785=CARTESIAN_POINT('Ctrl Pts',(0.52842660556555,-25.6358463010662,-10.2450421307954));
#85786=CARTESIAN_POINT('Ctrl Pts',(0.53057705908913,-25.6344556231107,-10.2454804579075));
#85787=CARTESIAN_POINT('Ctrl Pts',(0.531148531397364,-25.6340860573738,
-10.2455969411534));
#85788=CARTESIAN_POINT('Ctrl Pts',(0.53171713188043,-25.6337166391242,-10.2457126830695));
#85789=CARTESIAN_POINT('Ctrl Pts',(0.532282888338958,-25.6333473964984,
-10.2458276940714));
#85790=CARTESIAN_POINT('Ctrl Pts',(0.533630238942648,-25.6324680441423,
-10.2461015930973));
#85791=CARTESIAN_POINT('Ctrl Pts',(0.534961368822432,-25.6315896547556,
-10.2463713913334));
#85792=CARTESIAN_POINT('Ctrl Pts',(0.536274157225102,-25.630712658771,-10.2466376811725));
#85793=CARTESIAN_POINT('Ctrl Pts',(0.537260883005261,-25.6300534858644,
-10.2468378315157));
#85794=CARTESIAN_POINT('Ctrl Pts',(0.537698506461127,-25.6297596128986,
-10.2469265405115));
#85795=CARTESIAN_POINT('Ctrl Pts',(0.538805038270017,-25.6290097214713,
-10.2471504943624));
#85796=CARTESIAN_POINT('Ctrl Pts',(0.539170690684045,-25.6287619205419,
-10.2472244997056));
#85797=CARTESIAN_POINT('Ctrl Pts',(0.539609233626648,-25.6284640898016,
-10.2473132167283));
#85798=CARTESIAN_POINT('Ctrl Pts',(0.540163859237224,-25.6280854254163,
-10.2474252657462));
#85799=CARTESIAN_POINT('Ctrl Pts',(0.547924623835747,-25.6227868508452,
-10.2489931451136));
#85800=CARTESIAN_POINT('Ctrl Pts',(0.555251731899524,-25.6174552869425,
-10.2504479415432));
#85801=CARTESIAN_POINT('Ctrl Pts',(0.562169842897244,-25.6120958381659,
-10.2518022325599));
#85802=CARTESIAN_POINT('Ctrl Pts',(0.573305111815716,-25.6034693643494,
-10.2539820753912));
#85803=CARTESIAN_POINT('Ctrl Pts',(0.583378449603745,-25.5947641147587,
-10.2559016411584));
#85804=CARTESIAN_POINT('Ctrl Pts',(0.592367203409916,-25.5859391051817,
-10.2575864731877));
#85805=CARTESIAN_POINT('Ctrl Pts',(0.600561704306696,-25.5778938799534,
-10.2591224322174));
#85806=CARTESIAN_POINT('Ctrl Pts',(0.607850336182629,-25.569747293597,-10.2604624417005));
#85807=CARTESIAN_POINT('Ctrl Pts',(0.614214632612605,-25.5615083372879,
-10.2616195565446));
#85808=CARTESIAN_POINT('Ctrl Pts',(0.621304560947548,-25.5523300077696,
-10.2629086010464));
#85809=CARTESIAN_POINT('Ctrl Pts',(0.627247118265407,-25.5430378679536,
-10.2639706364414));
#85810=CARTESIAN_POINT('Ctrl Pts',(0.632051116031981,-25.5337020589155,
-10.2648221979346));
#85811=CARTESIAN_POINT('Ctrl Pts',(0.637187967973039,-25.5237194004904,
-10.2657327614949));
#85812=CARTESIAN_POINT('Ctrl Pts',(0.641026239505504,-25.5136885666782,
-10.266403109198));
#85813=CARTESIAN_POINT('Ctrl Pts',(0.643589723141555,-25.5037325098279,
-10.266848622649));
#85814=CARTESIAN_POINT('Ctrl Pts',(0.64583883367469,-25.4949974151249,-10.2672395005081));
#85815=CARTESIAN_POINT('Ctrl Pts',(0.64710868213128,-25.4863197852285,-10.2674574760169));
#85816=CARTESIAN_POINT('Ctrl Pts',(0.647387572639472,-25.4777990118003,
-10.2675053229145));
#85817=CARTESIAN_POINT('Ctrl Pts',(0.647426555016346,-25.4766080067597,
-10.2675120107929));
#85818=CARTESIAN_POINT('Ctrl Pts',(0.647446102180999,-25.4754201027178,
-10.2675153591));
#85819=CARTESIAN_POINT('Ctrl Pts',(0.647446102181,-25.4742356128,-10.2675153591));
#85820=CARTESIAN_POINT('Origin',(-2.84607155346,-25.4742356128,5.53854202767));
#85821=CARTESIAN_POINT('Origin',(-2.84607155346,-25.7742356128,5.53854202767));
#85822=CARTESIAN_POINT('Origin',(7.06664156103,-21.0742356128,-3.23658091327));
#85823=CARTESIAN_POINT('',(7.64099403241,-21.0742356128,-4.28030970457));
#85824=CARTESIAN_POINT('',(5.92940140951,-21.0742356128,-2.47090756951));
#85825=CARTESIAN_POINT('',(6.78519772096,-21.0742356128,-3.37560863704));
#85826=CARTESIAN_POINT('',(7.85893479751,-20.7742356128,-4.07415000213));
#85827=CARTESIAN_POINT('Ctrl Pts',(7.85893479751,-20.7742356128,-4.07415000213));
#85828=CARTESIAN_POINT('Ctrl Pts',(7.85183926652127,-20.7742356127998,-4.08086197525167));
#85829=CARTESIAN_POINT('Ctrl Pts',(7.84533191258089,-20.7747094757886,-4.08700495036613));
#85830=CARTESIAN_POINT('Ctrl Pts',(7.83943039491049,-20.7754368206059,-4.09255817936291));
#85831=CARTESIAN_POINT('Ctrl Pts',(7.83330363186861,-20.7761919262575,-4.09832336047068));
#85832=CARTESIAN_POINT('Ctrl Pts',(7.82782908140359,-20.7772197128011,-4.10345363014837));
#85833=CARTESIAN_POINT('Ctrl Pts',(7.82300251618872,-20.7783191472933,-4.10794846284614));
#85834=CARTESIAN_POINT('Ctrl Pts',(7.82041781215545,-20.7789079123134,-4.11035551873072));
#85835=CARTESIAN_POINT('Ctrl Pts',(7.81801860696792,-20.7795180417377,-4.11258065655733));
#85836=CARTESIAN_POINT('Ctrl Pts',(7.81580268710095,-20.7801243597889,-4.11462527537135));
#85837=CARTESIAN_POINT('Ctrl Pts',(7.8115806647721,-20.7812795858371,-4.11852091546893));
#85838=CARTESIAN_POINT('Ctrl Pts',(7.80802846205607,-20.7824184098577,-4.12177047634116));
#85839=CARTESIAN_POINT('Ctrl Pts',(7.80513688118672,-20.783408983068,-4.12440799958011));
#85840=CARTESIAN_POINT('Ctrl Pts',(7.80448775989285,-20.7836313535266,-4.12500008832839));
#85841=CARTESIAN_POINT('Ctrl Pts',(7.80387192759621,-20.7838464613465,-4.12556133630691));
#85842=CARTESIAN_POINT('Ctrl Pts',(7.80328928645214,-20.7840531729096,-4.12609212275007));
#85843=CARTESIAN_POINT('Ctrl Pts',(7.80170024694699,-20.7846169381762,-4.1275397387236));
#85844=CARTESIAN_POINT('Ctrl Pts',(7.80035804175691,-20.785117756612,-4.12876088185069));
#85845=CARTESIAN_POINT('Ctrl Pts',(7.79926085691167,-20.7855373871536,-4.12976226790216));
#85846=CARTESIAN_POINT('Ctrl Pts',(7.79871226448904,-20.7857472024244,-4.13026296092789));
#85847=CARTESIAN_POINT('Ctrl Pts',(7.79853440088772,-20.7858158360464,-4.13042047045815));
#85848=CARTESIAN_POINT('Ctrl Pts',(7.79826256025366,-20.7859215662924,-4.13066808561332));
#85849=CARTESIAN_POINT('Ctrl Pts',(7.7979907196196,-20.7860272965384,-4.13091570076849));
#85850=CARTESIAN_POINT('Ctrl Pts',(7.79762464761794,-20.7861689844856,-4.13125366213504));
#85851=CARTESIAN_POINT('Ctrl Pts',(7.79670305211903,-20.7865412504096,-4.13211202964214));
#85852=CARTESIAN_POINT('Ctrl Pts',(7.79077432765017,-20.7889360777444,-4.13763400153611));
#85853=CARTESIAN_POINT('Ctrl Pts',(7.78442746797871,-20.791913998756,-4.14376377093566));
#85854=CARTESIAN_POINT('Ctrl Pts',(7.77769431332228,-20.7956726711726,-4.15032683375898));
#85855=CARTESIAN_POINT('Ctrl Pts',(7.77605434143871,-20.7965881583992,-4.15192537694558));
#85856=CARTESIAN_POINT('Ctrl Pts',(7.77439162408683,-20.7975500115351,-4.15354946303284));
#85857=CARTESIAN_POINT('Ctrl Pts',(7.77270696753313,-20.7985611469581,-4.15519624304362));
#85858=CARTESIAN_POINT('Ctrl Pts',(7.76840633206434,-20.8011424000059,-4.15940018627946));
#85859=CARTESIAN_POINT('Ctrl Pts',(7.76396141066586,-20.8040448037012,-4.16375080512166));
#85860=CARTESIAN_POINT('Ctrl Pts',(7.75938461841096,-20.8073139488897,-4.16818508401255));
#85861=CARTESIAN_POINT('Ctrl Pts',(7.75745526485453,-20.8086920618877,-4.17005436084921));
#85862=CARTESIAN_POINT('Ctrl Pts',(7.75529472619584,-20.810286165269,-4.17213333375864));
#85863=CARTESIAN_POINT('Ctrl Pts',(7.753170537234,-20.8119177521571,-4.17416630948157));
#85864=CARTESIAN_POINT('Ctrl Pts',(7.75095089065221,-20.8136226599238,-4.17629064384886));
#85865=CARTESIAN_POINT('Ctrl Pts',(7.74877121181608,-20.8153685032777,-4.17836449142159));
#85866=CARTESIAN_POINT('Ctrl Pts',(7.74691494002475,-20.8168980893368,-4.18011674479675));
#85867=CARTESIAN_POINT('Ctrl Pts',(7.74633359759334,-20.8173771211698,-4.18066551100778));
#85868=CARTESIAN_POINT('Ctrl Pts',(7.74578381270852,-20.8178345854507,-4.18118288870584));
#85869=CARTESIAN_POINT('Ctrl Pts',(7.7452739071026,-20.8182617746731,-4.18166091416508));
#85870=CARTESIAN_POINT('Ctrl Pts',(7.73623209499571,-20.8258368329543,-4.1901374171386));
#85871=CARTESIAN_POINT('Ctrl Pts',(7.72791609663171,-20.8340692187894,-4.19800215501873));
#85872=CARTESIAN_POINT('Ctrl Pts',(7.72029634619406,-20.8427229030516,-4.20522725952926));
#85873=CARTESIAN_POINT('Ctrl Pts',(7.71545651995509,-20.8482194515934,-4.20981641906612));
#85874=CARTESIAN_POINT('Ctrl Pts',(7.71089683958716,-20.8538864976655,-4.21414823283737));
#85875=CARTESIAN_POINT('Ctrl Pts',(7.70660331641012,-20.8596698009706,-4.2182216252992));
#85876=CARTESIAN_POINT('Ctrl Pts',(7.70107672530996,-20.8671140259712,-4.22346486577998));
#85877=CARTESIAN_POINT('Ctrl Pts',(7.69599298422546,-20.8747513212587,-4.22828368619705));
#85878=CARTESIAN_POINT('Ctrl Pts',(7.69132291127602,-20.8824884583873,-4.23270372921761));
#85879=CARTESIAN_POINT('Ctrl Pts',(7.68931388380915,-20.8858169119628,-4.23460519583906));
#85880=CARTESIAN_POINT('Ctrl Pts',(7.68727656376502,-20.8893444390518,-4.23653209982262));
#85881=CARTESIAN_POINT('Ctrl Pts',(7.68534941494104,-20.8928381851489,-4.23835441195482));
#85882=CARTESIAN_POINT('Ctrl Pts',(7.68331638715091,-20.8965238802124,-4.24027684324861));
#85883=CARTESIAN_POINT('Ctrl Pts',(7.68140611510582,-20.9001715874312,-4.2420827359796));
#85884=CARTESIAN_POINT('Ctrl Pts',(7.67974560486613,-20.9034727800355,-4.2436530646065));
#85885=CARTESIAN_POINT('Ctrl Pts',(7.67932124059199,-20.904316441321,-4.24405438183538));
#85886=CARTESIAN_POINT('Ctrl Pts',(7.67891301835769,-20.9051373252889,-4.24444047509348));
#85887=CARTESIAN_POINT('Ctrl Pts',(7.67852273949611,-20.9059300251566,-4.24480965903291));
#85888=CARTESIAN_POINT('Ctrl Pts',(7.67352497797012,-20.9160810358573,-4.24953728707039));
#85889=CARTESIAN_POINT('Ctrl Pts',(7.66914206979505,-20.9263164258937,-4.25368328847564));
#85890=CARTESIAN_POINT('Ctrl Pts',(7.66528975762001,-20.9365851464252,-4.25732736873421));
#85891=CARTESIAN_POINT('Ctrl Pts',(7.66128653682442,-20.9472561288658,-4.2611142004366));
#85892=CARTESIAN_POINT('Ctrl Pts',(7.65785582893469,-20.9579639028255,-4.26435945938395));
#85893=CARTESIAN_POINT('Ctrl Pts',(7.65492517216004,-20.9686982280599,-4.26713169346425));
#85894=CARTESIAN_POINT('Ctrl Pts',(7.65187006261451,-20.9798883953195,-4.27002165276431));
#85895=CARTESIAN_POINT('Ctrl Pts',(7.64935794570938,-20.9911083156681,-4.27239796652737));
#85896=CARTESIAN_POINT('Ctrl Pts',(7.64733735079348,-21.0023832268463,-4.27430932661769));
#85897=CARTESIAN_POINT('Ctrl Pts',(7.64522595759957,-21.0141647920359,-4.2763065763653));
#85898=CARTESIAN_POINT('Ctrl Pts',(7.64365080122791,-21.026007495695,-4.27779657458376));
#85899=CARTESIAN_POINT('Ctrl Pts',(7.64259285259056,-21.0379639184472,-4.27879732574037));
#85900=CARTESIAN_POINT('Ctrl Pts',(7.64153490395321,-21.0499203411994,-4.27979807689698));
#85901=CARTESIAN_POINT('Ctrl Pts',(7.64099403240862,-21.0619917936591,-4.28030970457131));
#85902=CARTESIAN_POINT('Ctrl Pts',(7.64099403240862,-21.0742356128,-4.28030970457131));
#85903=CARTESIAN_POINT('',(6.1473421746,-20.7742356128,-2.26474786707));
#85904=CARTESIAN_POINT('',(7.00313848605,-20.7742356128,-3.1694489346));
#85905=CARTESIAN_POINT('Ctrl Pts',(5.92940140950644,-21.0742356128,-2.47090756951336));
#85906=CARTESIAN_POINT('Ctrl Pts',(5.92940140950644,-21.0620465213214,-2.47090756951336));
#85907=CARTESIAN_POINT('Ctrl Pts',(5.92995101839846,-21.0500039028176,-2.47041394631259));
#85908=CARTESIAN_POINT('Ctrl Pts',(5.93101943002766,-21.0380655608985,-2.46943347772656));
#85909=CARTESIAN_POINT('Ctrl Pts',(5.9320858573139,-21.0261493918611,-2.46845483014835));
#85910=CARTESIAN_POINT('Ctrl Pts',(5.93366928149062,-21.0143359647724,-2.46699103089334));
#85911=CARTESIAN_POINT('Ctrl Pts',(5.93577611680437,-21.0025880055739,-2.46501377374376));
#85912=CARTESIAN_POINT('Ctrl Pts',(5.93693874668391,-20.9961050458956,-2.46392264990193));
#85913=CARTESIAN_POINT('Ctrl Pts',(5.93826141371168,-20.9896422032718,-2.46267455482446));
#85914=CARTESIAN_POINT('Ctrl Pts',(5.93974980292276,-20.9831957720588,-2.46126037362452));
#85915=CARTESIAN_POINT('Ctrl Pts',(5.94256096536312,-20.9710202166559,-2.45858936993573));
#85916=CARTESIAN_POINT('Ctrl Pts',(5.94596922600863,-20.9589055034122,-2.45533644285574));
#85917=CARTESIAN_POINT('Ctrl Pts',(5.95004731874438,-20.9468901927177,-2.45145053613956));
#85918=CARTESIAN_POINT('Ctrl Pts',(5.95096515538695,-20.9441859647508,-2.45057595387651));
#85919=CARTESIAN_POINT('Ctrl Pts',(5.95191701489044,-20.9414869353962,-2.44966922051427));
#85920=CARTESIAN_POINT('Ctrl Pts',(5.95290388063803,-20.9387938528556,-2.44872960814046));
#85921=CARTESIAN_POINT('Ctrl Pts',(5.95558971347156,-20.9314644166798,-2.44617237908421));
#85922=CARTESIAN_POINT('Ctrl Pts',(5.95853458616578,-20.9241793796473,-2.44337210772868));
#85923=CARTESIAN_POINT('Ctrl Pts',(5.96175683895069,-20.9169637237193,-2.44031448175405));
#85924=CARTESIAN_POINT('Ctrl Pts',(5.96319285476145,-20.9137480244278,-2.43895183284472));
#85925=CARTESIAN_POINT('Ctrl Pts',(5.96478214034198,-20.9103349058105,-2.43744524137443));
#85926=CARTESIAN_POINT('Ctrl Pts',(5.96640032087268,-20.9070148772088,-2.43591232356138));
#85927=CARTESIAN_POINT('Ctrl Pts',(5.96807093993496,-20.9035872602254,-2.43432973022842));
#85928=CARTESIAN_POINT('Ctrl Pts',(5.96977220807806,-20.9002591791179,-2.43271921754394));
#85929=CARTESIAN_POINT('Ctrl Pts',(5.97133259130416,-20.8973175679299,-2.43124300810494));
#85930=CARTESIAN_POINT('Ctrl Pts',(5.97165222026851,-20.8967150081729,-2.43094062130261));
#85931=CARTESIAN_POINT('Ctrl Pts',(5.97196583563394,-20.8961285551134,-2.43064396641428));
#85932=CARTESIAN_POINT('Ctrl Pts',(5.97227182042976,-20.8955605161796,-2.43035457266878));
#85933=CARTESIAN_POINT('Ctrl Pts',(5.97602931122008,-20.8885850027176,-2.42680081984083));
#85934=CARTESIAN_POINT('Ctrl Pts',(5.98019629816105,-20.8813245480512,-2.42269456354623));
#85935=CARTESIAN_POINT('Ctrl Pts',(5.98491790960405,-20.8738972008456,-2.41798939022611));
#85936=CARTESIAN_POINT('Ctrl Pts',(5.98946154888746,-20.866749813361,-2.41346156946182));
#85937=CARTESIAN_POINT('Ctrl Pts',(5.99451930907194,-20.8594475486382,-2.40837863946706));
#85938=CARTESIAN_POINT('Ctrl Pts',(6.00022051682109,-20.8521423476661,-2.40269924115795));
#85939=CARTESIAN_POINT('Ctrl Pts',(6.00560265299428,-20.8452459867309,-2.39733769384615));
#85940=CARTESIAN_POINT('Ctrl Pts',(6.01155875634439,-20.8383470065419,-2.39144407574847));
#85941=CARTESIAN_POINT('Ctrl Pts',(6.01819022591929,-20.8316177623016,-2.38499059670732));
#85942=CARTESIAN_POINT('Ctrl Pts',(6.02246370269338,-20.8272812772068,-2.38083182126803));
#85943=CARTESIAN_POINT('Ctrl Pts',(6.02701749468084,-20.8230161860919,-2.37644068965293));
#85944=CARTESIAN_POINT('Ctrl Pts',(6.03187524669176,-20.8188792073734,-2.37181306735779));
#85945=CARTESIAN_POINT('Ctrl Pts',(6.03904491973146,-20.8127733409732,-2.36498304830108));
#85946=CARTESIAN_POINT('Ctrl Pts',(6.04690540802277,-20.8069436641881,-2.35765851382944));
#85947=CARTESIAN_POINT('Ctrl Pts',(6.05541988710496,-20.8016210284865,-2.34979781381991));
#85948=CARTESIAN_POINT('Ctrl Pts',(6.06364317348351,-20.796480425375,-2.34220594746024));
#85949=CARTESIAN_POINT('Ctrl Pts',(6.07247680878188,-20.7918134067092,-2.33411365367724));
#85950=CARTESIAN_POINT('Ctrl Pts',(6.08185538094852,-20.7878447886848,-2.32551390647897));
#85951=CARTESIAN_POINT('Ctrl Pts',(6.09099832383897,-20.7839758790783,-2.31713022118987));
#85952=CARTESIAN_POINT('Ctrl Pts',(6.10065940586829,-20.7807714248902,-2.30826403339204));
#85953=CARTESIAN_POINT('Ctrl Pts',(6.11074267212237,-20.7784463041617,-2.29894227287215));
#85954=CARTESIAN_POINT('Ctrl Pts',(6.12050826794062,-20.7761944357004,-2.2899141917665));
#85955=CARTESIAN_POINT('Ctrl Pts',(6.13066992045268,-20.7747681118582,-2.28045873909444));
#85956=CARTESIAN_POINT('Ctrl Pts',(6.14110482235127,-20.774358224677,-2.27063409101451));
#85957=CARTESIAN_POINT('Ctrl Pts',(6.14317369217154,-20.7742769586309,-2.26868621281644));
#85958=CARTESIAN_POINT('Ctrl Pts',(6.14525318677249,-20.7742356128,-2.26672393202862));
#85959=CARTESIAN_POINT('Ctrl Pts',(6.1473421746,-20.7742356128,-2.26474786707));
#85960=CARTESIAN_POINT('Origin',(0.00234331738835,-21.0742356128,3.08191746407));
#85961=CARTESIAN_POINT('',(8.05349668264,-20.7742356128,1.84629187045));
#85962=CARTESIAN_POINT('Origin',(0.00234331738835,-20.7742356128,3.08191746407));
#85963=CARTESIAN_POINT('',(7.75696851341,-21.0742356128,1.89180060423));
#85964=CARTESIAN_POINT('Ctrl Pts',(7.75696851340708,-21.0742356128,1.89180060423045));
#85965=CARTESIAN_POINT('Ctrl Pts',(7.75696851340708,-21.0616661584389,1.89180060423045));
#85966=CARTESIAN_POINT('Ctrl Pts',(7.75774249257575,-21.0492324960412,1.89166508636217));
#85967=CARTESIAN_POINT('Ctrl Pts',(7.75926820201175,-21.0369022993968,1.8914120010612));
#85968=CARTESIAN_POINT('Ctrl Pts',(7.76078851625566,-21.0246157046192,1.89115981071688));
#85969=CARTESIAN_POINT('Ctrl Pts',(7.76305543403818,-21.0124306480291,1.89079084973378));
#85970=CARTESIAN_POINT('Ctrl Pts',(7.76609704294065,-21.0003208010519,1.8903152156623));
#85971=CARTESIAN_POINT('Ctrl Pts',(7.76767607380167,-20.9940340552169,1.89006829342426));
#85972=CARTESIAN_POINT('Ctrl Pts',(7.76946470014536,-20.9877677810365,1.88979249855927));
#85973=CARTESIAN_POINT('Ctrl Pts',(7.7714719062634,-20.9815205326532,1.88948847860383));
#85974=CARTESIAN_POINT('Ctrl Pts',(7.77423444354622,-20.9729223840033,1.88907005298523));
#85975=CARTESIAN_POINT('Ctrl Pts',(7.77736366142895,-20.9644930346671,1.88859926473075));
#85976=CARTESIAN_POINT('Ctrl Pts',(7.78090592895025,-20.9561289601266,1.88806630410627));
#85977=CARTESIAN_POINT('Ctrl Pts',(7.78438936162325,-20.9479038076336,1.88754219562447));
#85978=CARTESIAN_POINT('Ctrl Pts',(7.78827253241698,-20.939741062644,1.8869579179785));
#85979=CARTESIAN_POINT('Ctrl Pts',(7.79264235226126,-20.9315661910541,1.88629756027545));
#85980=CARTESIAN_POINT('Ctrl Pts',(7.79681578785701,-20.9237587066955,1.88566687973438));
#85981=CARTESIAN_POINT('Ctrl Pts',(7.80143350528879,-20.915939583347,1.88496674416322));
#85982=CARTESIAN_POINT('Ctrl Pts',(7.80660547580603,-20.9080749321963,1.88417801872099));
#85983=CARTESIAN_POINT('Ctrl Pts',(7.80995423788519,-20.9029827056549,1.88366733254384));
#85984=CARTESIAN_POINT('Ctrl Pts',(7.81353604563579,-20.897872017984,1.88311940119982));
#85985=CARTESIAN_POINT('Ctrl Pts',(7.81738779919566,-20.892743072491,1.88252794322287));
#85986=CARTESIAN_POINT('Ctrl Pts',(7.82462310241973,-20.8831086357898,1.88141692255628));
#85987=CARTESIAN_POINT('Ctrl Pts',(7.83271540665919,-20.8735443563726,1.88019259901566));
#85988=CARTESIAN_POINT('Ctrl Pts',(7.84175563150046,-20.8642171343037,1.87881827297348));
#85989=CARTESIAN_POINT('Ctrl Pts',(7.84668640059003,-20.8591298296098,1.87806868051459));
#85990=CARTESIAN_POINT('Ctrl Pts',(7.85189894556063,-20.854113854674,1.87727449378871));
#85991=CARTESIAN_POINT('Ctrl Pts',(7.8574054894449,-20.8492024317588,1.87643010692974));
#85992=CARTESIAN_POINT('Ctrl Pts',(7.86520669548291,-20.8422443428183,1.8752338509839));
#85993=CARTESIAN_POINT('Ctrl Pts',(7.8735979524252,-20.8354966552672,1.87393871427795));
#85994=CARTESIAN_POINT('Ctrl Pts',(7.8825978759917,-20.8290738365449,1.87254643281156));
#85995=CARTESIAN_POINT('Ctrl Pts',(7.88709783777494,-20.8258624271837,1.87185029207836));
#85996=CARTESIAN_POINT('Ctrl Pts',(7.89174968103352,-20.822732539534,1.87113009993202));
#85997=CARTESIAN_POINT('Ctrl Pts',(7.89655375328037,-20.8197001322686,1.87038764109567));
#85998=CARTESIAN_POINT('Ctrl Pts',(7.89870392181544,-20.8183429114875,1.87005533726124));
#85999=CARTESIAN_POINT('Ctrl Pts',(7.901185677847,-20.8168201497101,1.86967235116843));
#86000=CARTESIAN_POINT('Ctrl Pts',(7.90359907289843,-20.8153894858188,1.86930032870983));
#86001=CARTESIAN_POINT('Ctrl Pts',(7.90623217468787,-20.8138285794724,1.86889443867501));
#86002=CARTESIAN_POINT('Ctrl Pts',(7.90878358936557,-20.8123773614406,1.86850164745361));
#86003=CARTESIAN_POINT('Ctrl Pts',(7.91070059863892,-20.8113116696728,1.86820712823749));
#86004=CARTESIAN_POINT('Ctrl Pts',(7.9109522801952,-20.8111717564411,1.86816846120771));
#86005=CARTESIAN_POINT('Ctrl Pts',(7.91119299389188,-20.8110384236042,1.86813149309831));
#86006=CARTESIAN_POINT('Ctrl Pts',(7.91142146587712,-20.8109122481099,1.86809642019366));
#86007=CARTESIAN_POINT('Ctrl Pts',(7.91772242298953,-20.8074324937851,1.86712915557353));
#86008=CARTESIAN_POINT('Ctrl Pts',(7.92487299159786,-20.8037803081172,1.86603160716374));
#86009=CARTESIAN_POINT('Ctrl Pts',(7.93293913642026,-20.800148831898,1.86479361588198));
#86010=CARTESIAN_POINT('Ctrl Pts',(7.94056676519282,-20.7967147809225,1.86362292800955));
#86011=CARTESIAN_POINT('Ctrl Pts',(7.9490140035596,-20.7932995377014,1.86232651780251));
#86012=CARTESIAN_POINT('Ctrl Pts',(7.95831982767407,-20.7901088517458,1.86089837350558));
#86013=CARTESIAN_POINT('Ctrl Pts',(7.96730267214303,-20.7870289057532,1.85951979618231));
#86014=CARTESIAN_POINT('Ctrl Pts',(7.97708639509304,-20.7841585184049,1.85801833885613));
#86015=CARTESIAN_POINT('Ctrl Pts',(7.98767748349669,-20.7817192873822,1.85639297870789));
#86016=CARTESIAN_POINT('Ctrl Pts',(7.99768726647839,-20.7794139366714,1.85485682852852));
#86017=CARTESIAN_POINT('Ctrl Pts',(8.00841878677286,-20.7774942736015,1.85320991650343));
#86018=CARTESIAN_POINT('Ctrl Pts',(8.01984167864081,-20.7761741033989,1.85145687957012));
#86019=CARTESIAN_POINT('Ctrl Pts',(8.03048065196714,-20.7749445324868,1.84982414826274));
#86020=CARTESIAN_POINT('Ctrl Pts',(8.04171959731026,-20.7742356128001,1.84809932180418));
#86021=CARTESIAN_POINT('Ctrl Pts',(8.05349668264,-20.7742356128,1.84629187045));
#86022=CARTESIAN_POINT('',(5.92101866809,-21.0742356128,-2.06782739988));
#86023=CARTESIAN_POINT('Origin',(0.00234331738835,-21.0742356128,3.08191746407));
#86024=CARTESIAN_POINT('Origin',(6.14734217460299,-21.0742356128,-2.26474786707535));
#86025=CARTESIAN_POINT('Origin',(-8.59172680003,-21.0742356128,1.84629187045));
#86026=CARTESIAN_POINT('',(11.0596214465,-20.7742356128,1.84629187045));
#86027=CARTESIAN_POINT('',(9.55655906459,-20.7742356128,1.84629187045));
#86028=CARTESIAN_POINT('',(11.0596214465,-21.0742356128,2.14629187045));
#86029=CARTESIAN_POINT('Ctrl Pts',(11.0596214465,-20.7742356128,1.84629187045));
#86030=CARTESIAN_POINT('Ctrl Pts',(11.0596214514713,-20.7742356128,1.86570125826323));
#86031=CARTESIAN_POINT('Ctrl Pts',(11.059621456438,-20.7761238547456,1.88504253295737));
#86032=CARTESIAN_POINT('Ctrl Pts',(11.0596214756218,-20.7798335852751,1.90397589067421));
#86033=CARTESIAN_POINT('Ctrl Pts',(11.0596214903527,-20.7826822310291,1.91851452862674));
#86034=CARTESIAN_POINT('Ctrl Pts',(11.059621513363,-20.786621837117,1.93289102969955));
#86035=CARTESIAN_POINT('Ctrl Pts',(11.0596215459651,-20.7916084043232,1.94689933055417));
#86036=CARTESIAN_POINT('Ctrl Pts',(11.0596215513868,-20.7924376650847,1.94922889591513));
#86037=CARTESIAN_POINT('Ctrl Pts',(11.0596215570631,-20.7932957658107,1.95154830433926));
#86038=CARTESIAN_POINT('Ctrl Pts',(11.0596215629872,-20.7941823691093,1.95385664488059));
#86039=CARTESIAN_POINT('Ctrl Pts',(11.0596215996861,-20.7996747577981,1.9681565053698));
#86040=CARTESIAN_POINT('Ctrl Pts',(11.0596216464123,-20.8062505351596,1.98200383104242));
#86041=CARTESIAN_POINT('Ctrl Pts',(11.0596217085961,-20.8138429039508,1.99527387331651));
#86042=CARTESIAN_POINT('Ctrl Pts',(11.0596217625585,-20.8204314682786,2.00678945291488));
#86043=CARTESIAN_POINT('Ctrl Pts',(11.0596218281764,-20.8277896556534,2.01787429563428));
#86044=CARTESIAN_POINT('Ctrl Pts',(11.0596219124487,-20.835846848425,2.02842038831454));
#86045=CARTESIAN_POINT('Ctrl Pts',(11.059621983873,-20.842675656481,2.03735864320007));
#86046=CARTESIAN_POINT('Ctrl Pts',(11.0596220686938,-20.8500054114903,2.04590963456982));
#86047=CARTESIAN_POINT('Ctrl Pts',(11.0596221745448,-20.8577913720448,2.05402220199404));
#86048=CARTESIAN_POINT('Ctrl Pts',(11.0596222613442,-20.8641759739613,2.06067462633664));
#86049=CARTESIAN_POINT('Ctrl Pts',(11.0596223622858,-20.8708674013712,2.06703237410384));
#86050=CARTESIAN_POINT('Ctrl Pts',(11.0596224948845,-20.8778366192505,2.07306804938344));
#86051=CARTESIAN_POINT('Ctrl Pts',(11.0596225983655,-20.8832754459947,2.07777833290419));
#86052=CARTESIAN_POINT('Ctrl Pts',(11.0596227211269,-20.8888833845846,2.08229251640741));
#86053=CARTESIAN_POINT('Ctrl Pts',(11.0596228734679,-20.8946459379248,2.0865990669219));
#86054=CARTESIAN_POINT('Ctrl Pts',(11.0596229829271,-20.8987864179635,2.0896933873365));
#86055=CARTESIAN_POINT('Ctrl Pts',(11.0596231076574,-20.9030067046001,2.09268053834455));
#86056=CARTESIAN_POINT('Ctrl Pts',(11.0596233102948,-20.9073012235333,2.09555660858332));
#86057=CARTESIAN_POINT('Ctrl Pts',(11.0596234335262,-20.9099128823873,2.09730565531492));
#86058=CARTESIAN_POINT('Ctrl Pts',(11.05962358557,-20.9125519917939,2.09901362387901));
#86059=CARTESIAN_POINT('Ctrl Pts',(11.0596238053652,-20.9152170612572,2.10067956720373));
#86060=CARTESIAN_POINT('Ctrl Pts',(11.0596238835097,-20.9161645813609,2.10127186500815));
#86061=CARTESIAN_POINT('Ctrl Pts',(11.0596239702182,-20.9171153822968,2.10185885195));
#86062=CARTESIAN_POINT('Ctrl Pts',(11.0596243586793,-20.9180695616141,2.10244058594263));
#86063=CARTESIAN_POINT('Ctrl Pts',(11.0596295564672,-20.9308369188505,2.1102244537817));
#86064=CARTESIAN_POINT('Ctrl Pts',(11.0596887741995,-20.9442101040438,2.11706359965047));
#86065=CARTESIAN_POINT('Ctrl Pts',(11.0597786773667,-20.958006572114,2.12286154590208));
#86066=CARTESIAN_POINT('Ctrl Pts',(11.0598685819633,-20.971803259534,2.12865958433516));
#86067=CARTESIAN_POINT('Ctrl Pts',(11.0599892148189,-20.986027642207,2.13342149132777));
#86068=CARTESIAN_POINT('Ctrl Pts',(11.0600749747649,-21.0005419751008,2.13709943925585));
#86069=CARTESIAN_POINT('Ctrl Pts',(11.0601461047687,-21.0125802820666,2.14014995948896));
#86070=CARTESIAN_POINT('Ctrl Pts',(11.0601932330123,-21.0248049323751,2.14245042568098));
#86071=CARTESIAN_POINT('Ctrl Pts',(11.0601138668724,-21.0371032668211,2.14398457510411));
#86072=CARTESIAN_POINT('Ctrl Pts',(11.0600344938244,-21.0494026717346,2.14551885806216));
#86073=CARTESIAN_POINT('Ctrl Pts',(11.0598278725422,-21.0618265078302,2.14629187045));
#86074=CARTESIAN_POINT('Ctrl Pts',(11.0596214465,-21.0742356128,2.14629187045));
#86075=CARTESIAN_POINT('',(8.05349668264,-21.0742356128,2.14629187045));
#86076=CARTESIAN_POINT('',(9.55655906459,-21.0742356128,2.14629187045));
#86077=CARTESIAN_POINT('Origin',(8.05349668264,-21.0742356128,1.84629187045));
#86078=CARTESIAN_POINT('Origin',(-2.84607155346,-21.0742356128,5.53854202767));
#86079=CARTESIAN_POINT('',(11.3495744826,-21.0742356128,1.76930332028));
#86080=CARTESIAN_POINT('',(8.08214906615,-21.0742356128,-4.27458799822));
#86081=CARTESIAN_POINT('Origin',(-2.84607155346,-21.0742356128,5.53854202767));
#86082=CARTESIAN_POINT('Ctrl Pts',(11.0596214465,-20.7742356128,1.84629187045));
#86083=CARTESIAN_POINT('Ctrl Pts',(11.070799043927,-20.7742356127963,1.84332398630273));
#86084=CARTESIAN_POINT('Ctrl Pts',(11.0812745407999,-20.7749023807717,1.84056790739039));
#86085=CARTESIAN_POINT('Ctrl Pts',(11.090984392949,-20.7759944024526,1.83801248606312));
#86086=CARTESIAN_POINT('Ctrl Pts',(11.0983251775274,-20.7768199861785,1.83608055165439));
#86087=CARTESIAN_POINT('Ctrl Pts',(11.105229605784,-20.7778890057565,1.83426296451625));
#86088=CARTESIAN_POINT('Ctrl Pts',(11.1116861224859,-20.7791077535672,1.83255059549683));
#86089=CARTESIAN_POINT('Ctrl Pts',(11.1191844845229,-20.7805231626395,1.83056191283071));
#86090=CARTESIAN_POINT('Ctrl Pts',(11.1260816354282,-20.7821401240567,1.82871994583986));
#86091=CARTESIAN_POINT('Ctrl Pts',(11.1323879808919,-20.7838325871391,1.82702746924725));
#86092=CARTESIAN_POINT('Ctrl Pts',(11.1355411536237,-20.7846788186803,1.82618123095095));
#86093=CARTESIAN_POINT('Ctrl Pts',(11.1385469425801,-20.7855442815937,1.82537246668409));
#86094=CARTESIAN_POINT('Ctrl Pts',(11.1414081485161,-20.7864153809969,1.82460200663818));
#86095=CARTESIAN_POINT('Ctrl Pts',(11.1428387514841,-20.7868509306985,1.82421677661523));
#86096=CARTESIAN_POINT('Ctrl Pts',(11.1437160692069,-20.7871263827825,1.82398021955917));
#86097=CARTESIAN_POINT('Ctrl Pts',(11.1448178401921,-20.7874771225719,1.8236833995488));
#86098=CARTESIAN_POINT('Ctrl Pts',(11.1457920700905,-20.7877872606986,1.82342093944374));
#86099=CARTESIAN_POINT('Ctrl Pts',(11.1469421037944,-20.7881554945431,1.82311127916004));
#86100=CARTESIAN_POINT('Ctrl Pts',(11.1487960782264,-20.7887760313561,1.82261250308688));
#86101=CARTESIAN_POINT('Ctrl Pts',(11.14903879087,-20.7888572687927,1.82254720593001));
#86102=CARTESIAN_POINT('Ctrl Pts',(11.1492935454941,-20.788942900769,1.82247867357926));
#86103=CARTESIAN_POINT('Ctrl Pts',(11.1495615021919,-20.7890334389009,1.82240659421726));
#86104=CARTESIAN_POINT('Ctrl Pts',(11.1563279211354,-20.7913196998364,1.82058645251367));
#86105=CARTESIAN_POINT('Ctrl Pts',(11.1625769168139,-20.7937252051572,1.81886794431943));
#86106=CARTESIAN_POINT('Ctrl Pts',(11.1680845579708,-20.7960314016393,1.81734032689293));
#86107=CARTESIAN_POINT('Ctrl Pts',(11.1757232918988,-20.7992299435943,1.8152216225815));
#86108=CARTESIAN_POINT('Ctrl Pts',(11.1819360774177,-20.8022315964258,1.81347008282657));
#86109=CARTESIAN_POINT('Ctrl Pts',(11.186205818646,-20.8043814218725,1.81230297902011));
#86110=CARTESIAN_POINT('Ctrl Pts',(11.1872827793046,-20.8049236742727,1.81200859938046));
#86111=CARTESIAN_POINT('Ctrl Pts',(11.1882363244331,-20.8054118612248,1.81175134962557));
#86112=CARTESIAN_POINT('Ctrl Pts',(11.1890582182961,-20.8058362808762,1.8115347011105));
#86113=CARTESIAN_POINT('Ctrl Pts',(11.191620679814,-20.8071595162392,1.81085924469486));
#86114=CARTESIAN_POINT('Ctrl Pts',(11.1950125808572,-20.8089466794886,1.81003220731266));
#86115=CARTESIAN_POINT('Ctrl Pts',(11.1991539097921,-20.8112879294087,1.80901917411934));
#86116=CARTESIAN_POINT('Ctrl Pts',(11.2002083640929,-20.8118840523168,1.80876123826724));
#86117=CARTESIAN_POINT('Ctrl Pts',(11.2013112466889,-20.8125163047139,1.80849128555073));
#86118=CARTESIAN_POINT('Ctrl Pts',(11.2024608971286,-20.8131865820199,1.80820883669898));
#86119=CARTESIAN_POINT('Ctrl Pts',(11.2052933264132,-20.814837964914,1.80751295874215));
#86120=CARTESIAN_POINT('Ctrl Pts',(11.208409451306,-20.8167196829706,1.80674007759016));
#86121=CARTESIAN_POINT('Ctrl Pts',(11.2117758887729,-20.8188620521781,1.80587689222197));
#86122=CARTESIAN_POINT('Ctrl Pts',(11.2135389634822,-20.8199840563754,1.805424823735));
#86123=CARTESIAN_POINT('Ctrl Pts',(11.2156745716249,-20.8213772323699,1.80486375185293));
#86124=CARTESIAN_POINT('Ctrl Pts',(11.217695862772,-20.8227376815279,1.80432438855134));
#86125=CARTESIAN_POINT('Ctrl Pts',(11.2195340508706,-20.8239748914441,1.80383388464586));
#86126=CARTESIAN_POINT('Ctrl Pts',(11.221278205261,-20.8251839540792,1.8033611982393));
#86127=CARTESIAN_POINT('Ctrl Pts',(11.2225827407332,-20.8261038737532,1.80299917840933));
#86128=CARTESIAN_POINT('Ctrl Pts',(11.2311650483049,-20.8321558621824,1.80061751413563));
#86129=CARTESIAN_POINT('Ctrl Pts',(11.2388722047358,-20.8382890404485,1.79847325067937));
#86130=CARTESIAN_POINT('Ctrl Pts',(11.2458190592394,-20.8443217970411,1.79659127395651));
#86131=CARTESIAN_POINT('Ctrl Pts',(11.2477404719851,-20.8459903817801,1.79607074282109));
#86132=CARTESIAN_POINT('Ctrl Pts',(11.2496037920806,-20.8476515874104,1.79557025959013));
#86133=CARTESIAN_POINT('Ctrl Pts',(11.2514115713214,-20.8493022441783,1.79509032176336));
#86134=CARTESIAN_POINT('Ctrl Pts',(11.2555834676177,-20.8531115416307,1.79398274690199));
#86135=CARTESIAN_POINT('Ctrl Pts',(11.2594601534398,-20.856864462399,1.79298521059919));
#86136=CARTESIAN_POINT('Ctrl Pts',(11.2630756862055,-20.8605294332295,1.79210639261045));
#86137=CARTESIAN_POINT('Ctrl Pts',(11.2647550735698,-20.8622317841974,1.79169818836465));
#86138=CARTESIAN_POINT('Ctrl Pts',(11.2668542955939,-20.8644074833757,1.79118402619731));
#86139=CARTESIAN_POINT('Ctrl Pts',(11.2689933712148,-20.8667099173455,1.79064579654053));
#86140=CARTESIAN_POINT('Ctrl Pts',(11.2710430014965,-20.868916075155,1.79013007292968));
#86141=CARTESIAN_POINT('Ctrl Pts',(11.2731287735226,-20.8712386651904,1.78959237040092));
#86142=CARTESIAN_POINT('Ctrl Pts',(11.2749530779121,-20.8733356323948,1.78909495732801));
#86143=CARTESIAN_POINT('Ctrl Pts',(11.2753237759261,-20.8737617353974,1.78899388316553));
#86144=CARTESIAN_POINT('Ctrl Pts',(11.2756838044323,-20.8741784050093,1.78889443889188));
#86145=CARTESIAN_POINT('Ctrl Pts',(11.2760308487974,-20.8745826066336,1.78879709845521));
#86146=CARTESIAN_POINT('Ctrl Pts',(11.2786809486211,-20.8776691706615,1.78805378751286));
#86147=CARTESIAN_POINT('Ctrl Pts',(11.280819351248,-20.8802900091605,1.78742118467707));
#86148=CARTESIAN_POINT('Ctrl Pts',(11.2826709372862,-20.8826174977141,1.78686578086445));
#86149=CARTESIAN_POINT('Ctrl Pts',(11.2847855319977,-20.8852755945482,1.78623148467696));
#86150=CARTESIAN_POINT('Ctrl Pts',(11.2865255819466,-20.8875519570998,1.78569800051693));
#86151=CARTESIAN_POINT('Ctrl Pts',(11.2881757877891,-20.8897516108374,1.78522881404554));
#86152=CARTESIAN_POINT('Ctrl Pts',(11.2892652516828,-20.8912038195644,1.78491905770677));
#86153=CARTESIAN_POINT('Ctrl Pts',(11.2903146411927,-20.8926234410485,1.78463756969843));
#86154=CARTESIAN_POINT('Ctrl Pts',(11.2913968729573,-20.8941058380151,1.78437624402163));
#86155=CARTESIAN_POINT('Ctrl Pts',(11.2934752969568,-20.896952778507,1.78387436856746));
#86156=CARTESIAN_POINT('Ctrl Pts',(11.2959003782589,-20.9003586644651,1.78334317638522));
#86157=CARTESIAN_POINT('Ctrl Pts',(11.2985721795118,-20.9043476305441,1.78272589006414));
#86158=CARTESIAN_POINT('Ctrl Pts',(11.2997437831322,-20.9060968201946,1.78245520567554));
#86159=CARTESIAN_POINT('Ctrl Pts',(11.3011892265232,-20.9083082281453,1.78210362596708));
#86160=CARTESIAN_POINT('Ctrl Pts',(11.3025914362365,-20.9105281754296,1.78175149746585));
#86161=CARTESIAN_POINT('Ctrl Pts',(11.3040652188877,-20.9128614353999,1.78138139528274));
#86162=CARTESIAN_POINT('Ctrl Pts',(11.3054908542077,-20.9152040706641,1.78101078849584));
#86163=CARTESIAN_POINT('Ctrl Pts',(11.3065530473484,-20.9169938461998,1.78071892298188));
#86164=CARTESIAN_POINT('Ctrl Pts',(11.3067849034257,-20.9173845193448,1.78065521442402));
#86165=CARTESIAN_POINT('Ctrl Pts',(11.3069996179879,-20.917748743027,1.78059521109814));
#86166=CARTESIAN_POINT('Ctrl Pts',(11.307194142963,-20.9180805322724,1.78053967587823));
#86167=CARTESIAN_POINT('Ctrl Pts',(11.3144962577439,-20.930535298823,1.77845498443932));
#86168=CARTESIAN_POINT('Ctrl Pts',(11.3208213488539,-20.9432998130216,1.77679228846964));
#86169=CARTESIAN_POINT('Ctrl Pts',(11.3262029546748,-20.9562949396764,1.77540952966746));
#86170=CARTESIAN_POINT('Ctrl Pts',(11.3265215026431,-20.9570641471085,1.7753276814196));
#86171=CARTESIAN_POINT('Ctrl Pts',(11.3268367370717,-20.9578341751543,1.77524681580918));
#86172=CARTESIAN_POINT('Ctrl Pts',(11.3271486618196,-20.958605011926,1.77516690410521));
#86173=CARTESIAN_POINT('Ctrl Pts',(11.3290483249791,-20.9632995102861,1.77468023121025));
#86174=CARTESIAN_POINT('Ctrl Pts',(11.3309150432156,-20.9682576704015,1.77420483690388));
#86175=CARTESIAN_POINT('Ctrl Pts',(11.3326433989493,-20.9732472551659,1.77376348769531));
#86176=CARTESIAN_POINT('Ctrl Pts',(11.334434517243,-20.9784180289684,1.7733061115742));
#86177=CARTESIAN_POINT('Ctrl Pts',(11.3360766368962,-20.9836221559145,1.77288540523271));
#86178=CARTESIAN_POINT('Ctrl Pts',(11.337506302503,-20.9885816823008,1.77251239450797));
#86179=CARTESIAN_POINT('Ctrl Pts',(11.3387505506701,-20.9928979934623,1.77218776061571));
#86180=CARTESIAN_POINT('Ctrl Pts',(11.3398351802698,-20.9970284406791,1.77189890714644));
#86181=CARTESIAN_POINT('Ctrl Pts',(11.3407487906881,-21.0007831501905,1.77164502091652));
#86182=CARTESIAN_POINT('Ctrl Pts',(11.3431127849098,-21.0104985731009,1.77098808272004));
#86183=CARTESIAN_POINT('Ctrl Pts',(11.3449694913004,-21.0201442238305,1.77048932883145));
#86184=CARTESIAN_POINT('Ctrl Pts',(11.3463686089709,-21.0298042582066,1.77012153108541));
#86185=CARTESIAN_POINT('Ctrl Pts',(11.3477748237025,-21.03951329336,1.76975186767566));
#86186=CARTESIAN_POINT('Ctrl Pts',(11.3487188980331,-21.0492377497457,1.76951446321259));
#86187=CARTESIAN_POINT('Ctrl Pts',(11.3492020949561,-21.0590740018403,1.76939470728942));
#86188=CARTESIAN_POINT('Ctrl Pts',(11.3494487174911,-21.0640944010007,1.76933358415731));
#86189=CARTESIAN_POINT('Ctrl Pts',(11.3495744826921,-21.0691440165458,1.76930332025556));
#86190=CARTESIAN_POINT('Ctrl Pts',(11.3495744826921,-21.0742356128,1.76930332025556));
#86191=CARTESIAN_POINT('Origin',(-2.84607155346,-20.7742356128,5.53854202767));
#86192=CARTESIAN_POINT('Origin',(7.85893479754359,-21.0742356128,-4.07415000216138));
#86193=CARTESIAN_POINT('Origin',(7.85893479751,-21.0742356128,-4.07415000213));
#86194=CARTESIAN_POINT('Origin',(7.85893479751,-21.0742356128,-4.07415000213));
#86195=CARTESIAN_POINT('Origin',(7.86219292935,-23.1742356128,-4.51414908377));
#86196=CARTESIAN_POINT('',(7.64099403241,-22.8742356128,-4.28030970457));
#86197=CARTESIAN_POINT('',(5.92940140951,-22.8742356128,-2.47090756951));
#86198=CARTESIAN_POINT('',(6.88866980649,-22.8742356128,-3.48499366825));
#86199=CARTESIAN_POINT('',(7.64099403241,-22.1242356128,-4.28030970457));
#86200=CARTESIAN_POINT('',(5.92940140951,-22.1242356128,-2.47090756951));
#86201=CARTESIAN_POINT('Origin',(6.1473421746,-21.0742356128,-2.26474786707));
#86202=CARTESIAN_POINT('Origin',(6.1473421746,-21.0742356128,-2.26474786707));
#86203=CARTESIAN_POINT('Origin',(0.00234331738835,-21.2742356128,3.08191746407));
#86204=CARTESIAN_POINT('',(5.92101866809,-22.8742356128,-2.06782739988));
#86205=CARTESIAN_POINT('',(7.75696851341,-22.8742356128,1.89180060423));
#86206=CARTESIAN_POINT('Origin',(0.00234331738837,-22.8742356128,3.08191746407));
#86207=CARTESIAN_POINT('',(5.92101866809,-22.1242356128,-2.06782739988));
#86208=CARTESIAN_POINT('',(7.75696851341,-22.1242356128,1.89180060423));
#86209=CARTESIAN_POINT('Origin',(8.05349668264,-21.0742356128,1.84629187045));
#86210=CARTESIAN_POINT('Origin',(8.05349668264,-21.0742356128,1.84629187045));
#86211=CARTESIAN_POINT('Origin',(-11.4443506127,-23.1742356128,2.14629187045));
#86212=CARTESIAN_POINT('',(8.05349668264,-22.8742356128,2.14629187045));
#86213=CARTESIAN_POINT('',(8.05349668264,-22.1242356128,2.14629187045));
#86214=CARTESIAN_POINT('',(11.0596214465,-22.8742356128,2.14629187045));
#86215=CARTESIAN_POINT('',(11.0596214465,-22.1242356128,2.14629187045));
#86216=CARTESIAN_POINT('',(-6.6707290414,-22.8742356128,2.14629187045));
#86217=CARTESIAN_POINT('Origin',(11.0596214465,-21.0742356128,1.84629187045));
#86218=CARTESIAN_POINT('Origin',(11.0596214465,-21.0742356128,1.84629187045));
#86219=CARTESIAN_POINT('Origin',(-2.84607155346,-21.2742356128,5.53854202767));
#86220=CARTESIAN_POINT('',(11.3495744826,-22.8742356128,1.76930332028));
#86221=CARTESIAN_POINT('',(11.3495744826,-22.1242356128,1.76930332028));
#86222=CARTESIAN_POINT('',(8.08214906615,-22.8742356128,-4.27458799822));
#86223=CARTESIAN_POINT('',(8.08214906615,-22.1242356128,-4.27458799822));
#86224=CARTESIAN_POINT('Origin',(-2.84607155346,-22.8742356128,5.53854202767));
#86225=CARTESIAN_POINT('Origin',(7.85893479751,-22.1242356128,-4.07415000213));
#86226=CARTESIAN_POINT('Origin',(7.85893479751,-22.8742356128,-4.07415000213));
#86227=CARTESIAN_POINT('Origin',(6.6707290414,-22.8742356128,-3.69115337069));
#86228=CARTESIAN_POINT('',(5.71146064442,-23.1742356128,-2.67706727196));
#86229=CARTESIAN_POINT('Origin',(5.71146064442,-22.8742356128,-2.67706727196));
#86230=CARTESIAN_POINT('',(7.42305326732,-23.1742356128,-4.48646940701));
#86231=CARTESIAN_POINT('',(6.56725695587,-23.1742356128,-3.58176833949));
#86232=CARTESIAN_POINT('Origin',(7.42305326732,-22.8742356128,-4.48646940701));
#86233=CARTESIAN_POINT('Origin',(6.1473421746,-22.1242356128,-2.26474786707));
#86234=CARTESIAN_POINT('Origin',(6.1473421746,-22.8742356128,-2.26474786707));
#86235=CARTESIAN_POINT('Origin',(0.00234331738837,-22.8742356128,3.08191746407));
#86236=CARTESIAN_POINT('',(7.46044034417,-23.1742356128,1.93730933801));
#86237=CARTESIAN_POINT('Origin',(7.46044034417,-22.8742356128,1.93730933801));
#86238=CARTESIAN_POINT('',(5.69469516158,-23.1742356128,-1.87090693268));
#86239=CARTESIAN_POINT('Origin',(0.00234331738835,-23.1742356128,3.08191746407));
#86240=CARTESIAN_POINT('Origin',(5.69469516158,-22.8742356128,-1.87090693268));
#86241=CARTESIAN_POINT('Origin',(8.05349668264,-22.1242356128,1.84629187045));
#86242=CARTESIAN_POINT('Origin',(8.05349668264,-22.8742356128,1.84629187045));
#86243=CARTESIAN_POINT('Origin',(-6.6707290414,-22.8742356128,2.44629187045));
#86244=CARTESIAN_POINT('',(11.0596214465,-23.1742356128,2.44629187045));
#86245=CARTESIAN_POINT('Origin',(11.0596214465,-22.8742356128,2.44629187045));
#86246=CARTESIAN_POINT('',(8.05349668264,-23.1742356128,2.44629187045));
#86247=CARTESIAN_POINT('',(9.55655906459,-23.1742356128,2.44629187045));
#86248=CARTESIAN_POINT('Origin',(8.05349668264,-22.8742356128,2.44629187045));
#86249=CARTESIAN_POINT('Origin',(11.0596214465,-22.1242356128,1.84629187045));
#86250=CARTESIAN_POINT('Origin',(11.0596214465,-22.8742356128,1.84629187045));
#86251=CARTESIAN_POINT('Origin',(-2.84607155346,-22.8742356128,5.53854202767));
#86252=CARTESIAN_POINT('',(8.30536333479,-23.1742356128,-4.4750259943));
#86253=CARTESIAN_POINT('Origin',(8.30536333479,-22.8742356128,-4.4750259943));
#86254=CARTESIAN_POINT('',(11.6395275187,-23.1742356128,1.69231477012));
#86255=CARTESIAN_POINT('Origin',(-2.84607155346,-23.1742356128,5.53854202767));
#86256=CARTESIAN_POINT('Origin',(11.6395275187,-22.8742356128,1.69231477012));
#86257=CARTESIAN_POINT('Origin',(7.85893479751,-22.8742356128,-4.07415000213));
#86258=CARTESIAN_POINT('Origin',(7.85893479751,-23.1742356128,-4.07415000213));
#86259=CARTESIAN_POINT('Origin',(3.41821282746,-21.0742356128,8.06979469543));
#86260=CARTESIAN_POINT('',(3.62188020465,-21.0742356128,7.84952304616));
#86261=CARTESIAN_POINT('',(3.58772315463,-21.0742356128,8.31731489457));
#86262=CARTESIAN_POINT('Origin',(3.41821282746,-21.0742356128,8.06979469543));
#86263=CARTESIAN_POINT('',(3.41821282746,-20.7742356128,8.06979469543));
#86264=CARTESIAN_POINT('Origin',(3.41821282746,-21.0742356128,8.06979469543));
#86265=CARTESIAN_POINT('Origin',(3.41821282746,-21.0742356128,8.06979469543));
#86266=CARTESIAN_POINT('Origin',(6.1473421746,-22.8742356128,-2.26474786707));
#86267=CARTESIAN_POINT('Origin',(6.1473421746,-23.1742356128,-2.26474786707));
#86268=CARTESIAN_POINT('Origin',(8.05349668264,-22.8742356128,1.84629187045));
#86269=CARTESIAN_POINT('Origin',(8.05349668264,-23.1742356128,1.84629187045));
#86270=CARTESIAN_POINT('Origin',(11.0596214465,-22.8742356128,1.84629187045));
#86271=CARTESIAN_POINT('Origin',(11.0596214465,-23.1742356128,1.84629187045));
#86272=CARTESIAN_POINT('Origin',(-2.84607155346,-22.8742356128,5.53854202767));
#86273=CARTESIAN_POINT('',(0.246934184019208,-22.8742356128,-6.59919549797773));
#86274=CARTESIAN_POINT('',(2.37995077076E-13,-23.1742356128,-6.35119542306));
#86275=CARTESIAN_POINT('Ctrl Pts',(0.246934184763,-22.8742356128,-6.59919549778));
#86276=CARTESIAN_POINT('Ctrl Pts',(0.247420066333,-22.976056074,-6.59957097409));
#86277=CARTESIAN_POINT('Ctrl Pts',(0.206909891011,-23.0789305063,-6.56242231995));
#86278=CARTESIAN_POINT('Ctrl Pts',(0.139040717811,-23.1404071843,-6.49840377124));
#86279=CARTESIAN_POINT('Ctrl Pts',(0.0693760469986,-23.1744148412,-6.42641803012));
#86280=CARTESIAN_POINT('Ctrl Pts',(2.37995077076E-13,-23.1742356128,-6.35119542306));
#86281=CARTESIAN_POINT('',(0.530881036642,-22.8742356128,-6.52327988851));
#86282=CARTESIAN_POINT('Origin',(-2.84607155346,-22.8742356128,5.53854202767));
#86283=CARTESIAN_POINT('',(0.45,-23.1742356128,-6.23438845923));
#86284=CARTESIAN_POINT('Origin',(0.45,-22.8742356128,-6.23438845923));
#86285=CARTESIAN_POINT('Origin',(-2.84607155346,-23.1742356128,5.53854202767));
#86286=CARTESIAN_POINT('Origin',(2.93915231795E-16,-20.7742356128,0.729452270839));
#86287=CARTESIAN_POINT('Ctrl Pts',(3.39394702409,-22.8742356071,-7.27665075406));
#86288=CARTESIAN_POINT('Ctrl Pts',(3.3939470242,-22.8742356096,-7.39921133184));
#86289=CARTESIAN_POINT('Ctrl Pts',(3.45653492108,-22.8742356121,-7.52177190961));
#86290=CARTESIAN_POINT('Ctrl Pts',(3.58353228733,-22.8742356136,-7.59954001295));
#86291=CARTESIAN_POINT('Ctrl Pts',(3.72114892405,-22.8742356136,-7.59957667728));
#86292=CARTESIAN_POINT('Ctrl Pts',(3.83031550589,-22.8742356125,-7.54386534431));
#86293=CARTESIAN_POINT('Ctrl Pts',(3.39394702409,-22.9689887672,-7.27665074537));
#86294=CARTESIAN_POINT('Ctrl Pts',(3.3939470273,-22.9472590608,-7.39921132275));
#86295=CARTESIAN_POINT('Ctrl Pts',(3.45653492596,-22.9255293543,-7.52177190012));
#86296=CARTESIAN_POINT('Ctrl Pts',(3.5835322914,-22.9117412055,-7.59954000419));
#86297=CARTESIAN_POINT('Ctrl Pts',(3.72114892639,-22.9117347492,-7.59957667094));
#86298=CARTESIAN_POINT('Ctrl Pts',(3.83031550688,-22.9216122395,-7.54386534051));
#86299=CARTESIAN_POINT('Ctrl Pts',(3.39394702409,-23.0638368546,-7.29765903263));
#86300=CARTESIAN_POINT('Ctrl Pts',(3.39394703709,-23.0202773024,-7.41438252872));
#86301=CARTESIAN_POINT('Ctrl Pts',(3.45551763217,-22.9767177502,-7.53110602482));
#86302=CARTESIAN_POINT('Ctrl Pts',(3.58040884259,-22.9491120295,-7.6059738358));
#86303=CARTESIAN_POINT('Ctrl Pts',(3.71667793436,-22.9491723593,-7.60786209828));
#86304=CARTESIAN_POINT('Ctrl Pts',(3.82588511173,-22.969036255,-7.55663051616));
#86305=CARTESIAN_POINT('Ctrl Pts',(3.39394702409,-23.1509380315,-7.33965594802));
#86306=CARTESIAN_POINT('Ctrl Pts',(3.39394697957,-23.0896047046,-7.44484208723));
#86307=CARTESIAN_POINT('Ctrl Pts',(3.45348987378,-23.0282713776,-7.55002822643));
#86308=CARTESIAN_POINT('Ctrl Pts',(3.57418338496,-22.9885124598,-7.61911093785));
#86309=CARTESIAN_POINT('Ctrl Pts',(3.70775302124,-22.9865706365,-7.62456986686));
#86310=CARTESIAN_POINT('Ctrl Pts',(3.81702777332,-23.0125868459,-7.58214937101));
#86311=CARTESIAN_POINT('Ctrl Pts',(3.39394702409,-23.3144960216,-7.46222952989));
#86312=CARTESIAN_POINT('Ctrl Pts',(3.39394707642,-23.2249734796,-7.53850326899));
#86313=CARTESIAN_POINT('Ctrl Pts',(3.4480237922,-23.1354509376,-7.6147770081));
#86314=CARTESIAN_POINT('Ctrl Pts',(3.55743149517,-23.0743105508,-7.66795137089));
#86315=CARTESIAN_POINT('Ctrl Pts',(3.68302539363,-23.0640733183,-7.67932532721));
#86316=CARTESIAN_POINT('Ctrl Pts',(3.79142259861,-23.0943657893,-7.65641303197));
#86317=CARTESIAN_POINT('Ctrl Pts',(3.39394702409,-23.4183511293,-7.6347947685));
#86318=CARTESIAN_POINT('Ctrl Pts',(3.39394696259,-23.319135779,-7.67899068739));
#86319=CARTESIAN_POINT('Ctrl Pts',(3.44128745287,-23.2199204287,-7.72318660628));
#86320=CARTESIAN_POINT('Ctrl Pts',(3.53685705407,-23.1477285443,-7.75602607095));
#86321=CARTESIAN_POINT('Ctrl Pts',(3.65117651028,-23.1252941134,-7.76773938497));
#86322=CARTESIAN_POINT('Ctrl Pts',(3.75606800489,-23.1462934039,-7.76036589659));
#86323=CARTESIAN_POINT('Ctrl Pts',(3.39394702409,-23.4554260016,-7.73594528854));
#86324=CARTESIAN_POINT('Ctrl Pts',(3.39394732526,-23.3552502828,-7.7641726908));
#86325=CARTESIAN_POINT('Ctrl Pts',(3.43768548772,-23.255074564,-7.79240009306));
#86326=CARTESIAN_POINT('Ctrl Pts',(3.52588291425,-23.1798234897,-7.81406109398));
#86327=CARTESIAN_POINT('Ctrl Pts',(3.63360843235,-23.151042617,-7.82338875536));
#86328=CARTESIAN_POINT('Ctrl Pts',(3.73562880641,-23.1648309328,-7.82105608415));
#86329=CARTESIAN_POINT('Ctrl Pts',(3.39394702409,-23.4742356128,-7.84128512581));
#86330=CARTESIAN_POINT('Ctrl Pts',(3.39394702409,-23.3758453918,-7.85470223468));
#86331=CARTESIAN_POINT('Ctrl Pts',(3.43421150493,-23.2774551707,-7.86811934354));
#86332=CARTESIAN_POINT('Ctrl Pts',(3.51532352314,-23.2014862199,-7.87872422454));
#86333=CARTESIAN_POINT('Ctrl Pts',(3.61626901029,-23.167728681,-7.88399310977));
#86334=CARTESIAN_POINT('Ctrl Pts',(3.71465923135,-23.1742356128,-7.88399310977));
#86335=CARTESIAN_POINT('Ctrl Pts',(3.39394702409,-23.4742356128,-7.94679080481));
#86336=CARTESIAN_POINT('Ctrl Pts',(3.39394702409,-23.3799878332,-7.94679080481));
#86337=CARTESIAN_POINT('Ctrl Pts',(3.4309580406,-23.2857400536,-7.94679080481));
#86338=CARTESIAN_POINT('Ctrl Pts',(3.50545146488,-23.2112466293,-7.94679080481));
#86339=CARTESIAN_POINT('Ctrl Pts',(3.59969924449,-23.1742356128,-7.94679080481));
#86340=CARTESIAN_POINT('Ctrl Pts',(3.69394702409,-23.1742356128,-7.94679080481));
#86341=CARTESIAN_POINT('',(3.8303155059,-22.8742356128,-7.54386534442));
#86342=CARTESIAN_POINT('Ctrl Pts',(3.8303155059,-22.8742356128,-7.54386534442));
#86343=CARTESIAN_POINT('Ctrl Pts',(3.72114892405,-22.8742356145701,-7.59957667728));
#86344=CARTESIAN_POINT('Ctrl Pts',(3.58353228733,-22.8742356145703,-7.59954001295));
#86345=CARTESIAN_POINT('Ctrl Pts',(3.45653492108,-22.874235613427,-7.52177190961));
#86346=CARTESIAN_POINT('Ctrl Pts',(3.3939470242,-22.8742356114892,-7.39921133184));
#86347=CARTESIAN_POINT('Ctrl Pts',(3.39394702409,-22.8742356071,-7.27665075406));
#86348=CARTESIAN_POINT('',(3.69394702409,-23.1742356128,-7.94679080481));
#86349=CARTESIAN_POINT('Origin',(3.69182568282636,-23.4721142715478,-7.94679080481));
#86350=CARTESIAN_POINT('Ctrl Pts',(3.8303155058534,-22.8742356128,-7.54386534432868));
#86351=CARTESIAN_POINT('Ctrl Pts',(3.83031550576691,-22.8891836981438,-7.54386534335005));
#86352=CARTESIAN_POINT('Ctrl Pts',(3.82971372840363,-22.9043888182403,-7.54543077875052));
#86353=CARTESIAN_POINT('Ctrl Pts',(3.82852226081592,-22.9196429501145,-7.54866017859));
#86354=CARTESIAN_POINT('Ctrl Pts',(3.82728294903626,-22.9355096220367,-7.5520192571781));
#86355=CARTESIAN_POINT('Ctrl Pts',(3.8254052437601,-22.9514301757083,-7.55717821794454));
#86356=CARTESIAN_POINT('Ctrl Pts',(3.82292523898896,-22.9671744194393,-7.56419691331168));
#86357=CARTESIAN_POINT('Ctrl Pts',(3.821706622318,-22.9749107746696,-7.56764573699232));
#86358=CARTESIAN_POINT('Ctrl Pts',(3.82034295925121,-22.982604531287,-7.57154287310375));
#86359=CARTESIAN_POINT('Ctrl Pts',(3.81884079211807,-22.9902275607281,-7.5758915167602));
#86360=CARTESIAN_POINT('Ctrl Pts',(3.81607775040317,-23.0042491352088,-7.58389028304987));
#86361=CARTESIAN_POINT('Ctrl Pts',(3.8128308557735,-23.0180209455026,-7.59342190599612));
#86362=CARTESIAN_POINT('Ctrl Pts',(3.80908417075911,-23.031335083101,-7.60449227138444));
#86363=CARTESIAN_POINT('Ctrl Pts',(3.80774703235729,-23.0360867087652,-7.60844312677423));
#86364=CARTESIAN_POINT('Ctrl Pts',(3.80634639550617,-23.0407798967205,-7.61258949584727));
#86365=CARTESIAN_POINT('Ctrl Pts',(3.80488200217345,-23.0454049053476,-7.61693019755438));
#86366=CARTESIAN_POINT('Ctrl Pts',(3.80209817773717,-23.0541970868923,-7.62518190917649));
#86367=CARTESIAN_POINT('Ctrl Pts',(3.79908193039014,-23.0627426525445,-7.63413739357837));
#86368=CARTESIAN_POINT('Ctrl Pts',(3.79582238365986,-23.0709722301392,-7.64378448429961));
#86369=CARTESIAN_POINT('Ctrl Pts',(3.79441196867438,-23.0745331913784,-7.64795880743269));
#86370=CARTESIAN_POINT('Ctrl Pts',(3.79294260755751,-23.0780316640683,-7.65226591558948));
#86371=CARTESIAN_POINT('Ctrl Pts',(3.79142613720875,-23.0814652617517,-7.65670050231454));
#86372=CARTESIAN_POINT('Ctrl Pts',(3.79119028429884,-23.0819992807688,-7.65739020269952));
#86373=CARTESIAN_POINT('Ctrl Pts',(3.79095329160658,-23.082531731389,-7.65808298900307));
#86374=CARTESIAN_POINT('Ctrl Pts',(3.79071520419736,-23.0830626037977,-7.65877884160525));
#86375=CARTESIAN_POINT('Ctrl Pts',(3.78990694113206,-23.0848648182104,-7.66114113350075));
#86376=CARTESIAN_POINT('Ctrl Pts',(3.78898629334184,-23.086868580809,-7.66383305214407));
#86377=CARTESIAN_POINT('Ctrl Pts',(3.78808966118208,-23.0887663855061,-7.6664561297899));
#86378=CARTESIAN_POINT('Ctrl Pts',(3.78710763895836,-23.0908449261523,-7.66932901418814));
#86379=CARTESIAN_POINT('Ctrl Pts',(3.78615456208163,-23.0927963606278,-7.67211893756012));
#86380=CARTESIAN_POINT('Ctrl Pts',(3.78542392434147,-23.0942650558611,-7.67425848985647));
#86381=CARTESIAN_POINT('Ctrl Pts',(3.78536167208538,-23.0943901925558,-7.67444078533636));
#86382=CARTESIAN_POINT('Ctrl Pts',(3.78530104061487,-23.0945118473466,-7.67461834086054));
#86383=CARTESIAN_POINT('Ctrl Pts',(3.78524215234058,-23.0946298108357,-7.67479079697391));
#86384=CARTESIAN_POINT('Ctrl Pts',(3.7815169251505,-23.1020920909291,-7.68570023880042));
#86385=CARTESIAN_POINT('Ctrl Pts',(3.77739994333826,-23.109525749538,-7.69775930932877));
#86386=CARTESIAN_POINT('Ctrl Pts',(3.772875551567,-23.1167109360701,-7.71103970318222));
#86387=CARTESIAN_POINT('Ctrl Pts',(3.77069040030985,-23.1201811747624,-7.71745375191882));
#86388=CARTESIAN_POINT('Ctrl Pts',(3.76841042757223,-23.1235929863598,-7.72415214818587));
#86389=CARTESIAN_POINT('Ctrl Pts',(3.76603516262184,-23.1269190542052,-7.73113960412645));
#86390=CARTESIAN_POINT('Ctrl Pts',(3.76238851748999,-23.1320254273341,-7.74186715356705));
#86391=CARTESIAN_POINT('Ctrl Pts',(3.75852730260589,-23.1369322492204,-7.75327548212248));
#86392=CARTESIAN_POINT('Ctrl Pts',(3.75444904890525,-23.1415316798466,-7.76537128242619));
#86393=CARTESIAN_POINT('Ctrl Pts',(3.75240992205494,-23.1438313951596,-7.77141918257805));
#86394=CARTESIAN_POINT('Ctrl Pts',(3.75031641641447,-23.1460540871329,-7.77763873481617));
#86395=CARTESIAN_POINT('Ctrl Pts',(3.74816743160474,-23.1481853204141,-7.78402931127238));
#86396=CARTESIAN_POINT('Ctrl Pts',(3.74709293919988,-23.1492509370547,-7.78722459950048));
#86397=CARTESIAN_POINT('Ctrl Pts',(3.74600457707861,-23.1502936881539,-7.79046264393566));
#86398=CARTESIAN_POINT('Ctrl Pts',(3.74490214245977,-23.1513117086285,-7.79374324293244));
#86399=CARTESIAN_POINT('Ctrl Pts',(3.74435092515035,-23.1518207188659,-7.79538354243082));
#86400=CARTESIAN_POINT('Ctrl Pts',(3.74379618970325,-23.1523235465235,-7.79703448054263));
#86401=CARTESIAN_POINT('Ctrl Pts',(3.74323790853073,-23.1528199569261,-7.79869602771192));
#86402=CARTESIAN_POINT('Ctrl Pts',(3.74281599488497,-23.153195112552,-7.79995172010905));
#86403=CARTESIAN_POINT('Ctrl Pts',(3.7421707340011,-23.1537585415559,-7.80187200933954));
#86404=CARTESIAN_POINT('Ctrl Pts',(3.74180381131037,-23.154074114798,-7.80296414761389));
#86405=CARTESIAN_POINT('Ctrl Pts',(3.74168521751671,-23.1541761118369,-7.8033171397412));
#86406=CARTESIAN_POINT('Ctrl Pts',(3.74159574384263,-23.1542526471401,-7.80358346296994));
#86407=CARTESIAN_POINT('Ctrl Pts',(3.74155239904321,-23.1542897009319,-7.80371246452033));
#86408=CARTESIAN_POINT('Ctrl Pts',(3.7404152624986,-23.1552617949622,-7.80709677772983));
#86409=CARTESIAN_POINT('Ctrl Pts',(3.73888225575716,-23.1565394420993,-7.81166442353252));
#86410=CARTESIAN_POINT('Ctrl Pts',(3.73694415193971,-23.158023736641,-7.81744798511014));
#86411=CARTESIAN_POINT('Ctrl Pts',(3.73500913445982,-23.1595056675146,-7.82322233664276));
#86412=CARTESIAN_POINT('Ctrl Pts',(3.73267003716621,-23.1611935991109,-7.83020952169269));
#86413=CARTESIAN_POINT('Ctrl Pts',(3.72991761188174,-23.1629377834524,-7.83844583282956));
#86414=CARTESIAN_POINT('Ctrl Pts',(3.72723730229835,-23.1646362687963,-7.84646634615521));
#86415=CARTESIAN_POINT('Ctrl Pts',(3.72416473685366,-23.1663879276109,-7.85567229785107));
#86416=CARTESIAN_POINT('Ctrl Pts',(3.72069556429772,-23.1680073125115,-7.86608830518644));
#86417=CARTESIAN_POINT('Ctrl Pts',(3.71735496001881,-23.1695666826613,-7.87611829306183));
#86418=CARTESIAN_POINT('Ctrl Pts',(3.71364632450648,-23.1710032445205,-7.88727117149701));
#86419=CARTESIAN_POINT('Ctrl Pts',(3.70957386674216,-23.1721096345942,-7.89954781998661));
#86420=CARTESIAN_POINT('Ctrl Pts',(3.705781791046,-23.1731398515176,-7.91097924127122));
#86421=CARTESIAN_POINT('Ctrl Pts',(3.70167409659488,-23.1738836084695,-7.92338559552355));
#86422=CARTESIAN_POINT('Ctrl Pts',(3.69726432338169,-23.1741393298497,-7.93673921986036));
#86423=CARTESIAN_POINT('Ctrl Pts',(3.69617676356291,-23.1742023971062,-7.94003255594855));
#86424=CARTESIAN_POINT('Ctrl Pts',(3.69507088830591,-23.1742356128,-7.9433833416931));
#86425=CARTESIAN_POINT('Ctrl Pts',(3.69394702409,-23.1742356128,-7.94679080481));
#86426=CARTESIAN_POINT('Origin',(-2.84607155346,-22.8742356128,5.53854202767));
#86427=CARTESIAN_POINT('',(6.72883656293,-23.1742356128,-5.99173026574));
#86428=CARTESIAN_POINT('Origin',(-2.84607155346,-23.1742356128,5.53854202767));
#86429=CARTESIAN_POINT('',(6.53717906469,-22.8742356128,-5.76093294477));
#86430=CARTESIAN_POINT('Origin',(6.72883656293,-22.8742356128,-5.99173026574));
#86431=CARTESIAN_POINT('Origin',(-2.84607155346,-22.8742356128,5.53854202767));
#86432=CARTESIAN_POINT('Origin',(3.1295913978,-23.1742356128,-2.83309600707));
#86433=CARTESIAN_POINT('',(3.32093311398,-19.4742356128,-2.75383967318));
#86434=CARTESIAN_POINT('',(0.11480502971,-19.4742356128,-4.08186140839));
#86435=CARTESIAN_POINT('',(-0.0382683432365,-19.4742356128,-4.14526647551));
#86436=CARTESIAN_POINT('',(0.11480502971,-23.0742356128,-4.08186140839));
#86437=CARTESIAN_POINT('',(0.11480502971,-21.2742356128,-4.08186140839));
#86438=CARTESIAN_POINT('',(3.32093311398,-23.0742356128,-2.75383967318));
#86439=CARTESIAN_POINT('',(-0.0382683432365,-23.0742356128,-4.14526647551));
#86440=CARTESIAN_POINT('',(3.32093311398,-21.2742356128,-2.75383967318));
#86441=CARTESIAN_POINT('Origin',(-2.84607155346,-20.0742356128,5.53854202767));
#86442=CARTESIAN_POINT('',(0.647446102181,-19.6742356128,-10.2675153591));
#86443=CARTESIAN_POINT('',(10.575526102,-19.6742356128,-3.51114482323));
#86444=CARTESIAN_POINT('Origin',(-2.84607155346,-19.6742356128,5.53854202767));
#86445=CARTESIAN_POINT('',(10.5755260956339,-22.0742355256,-3.51114483719302));
#86446=CARTESIAN_POINT('',(10.575526102,-21.2742356128,-3.51114482323));
#86447=CARTESIAN_POINT('',(10.9558455155,-22.6742356128,-2.9197793747));
#86448=CARTESIAN_POINT('Ctrl Pts',(10.5755260924509,-22.0742355256,-3.51114484417453));
#86449=CARTESIAN_POINT('Ctrl Pts',(10.5755260822369,-22.1031469614448,-3.51114486448172));
#86450=CARTESIAN_POINT('Ctrl Pts',(10.5767677418046,-22.1320579213261,-3.50930400549703));
#86451=CARTESIAN_POINT('Ctrl Pts',(10.5792325785806,-22.1606355884888,-3.50564573524642));
#86452=CARTESIAN_POINT('Ctrl Pts',(10.5800163561132,-22.1697228163623,-3.50448246550852));
#86453=CARTESIAN_POINT('Ctrl Pts',(10.5809235534889,-22.1787763809613,-3.50313572368826));
#86454=CARTESIAN_POINT('Ctrl Pts',(10.5819528553846,-22.1877857466703,-3.50160709265196));
#86455=CARTESIAN_POINT('Ctrl Pts',(10.5851501398811,-22.2157712244254,-3.49685875950131));
#86456=CARTESIAN_POINT('Ctrl Pts',(10.5895274155016,-22.2433280808744,-3.49035326238203));
#86457=CARTESIAN_POINT('Ctrl Pts',(10.5950216821739,-22.2701519594831,-3.48216748914416));
#86458=CARTESIAN_POINT('Ctrl Pts',(10.6005159488462,-22.2969758380917,-3.47398171590629));
#86459=CARTESIAN_POINT('Ctrl Pts',(10.6071270982676,-22.3230660301722,-3.46411560723739));
#86460=CARTESIAN_POINT('Ctrl Pts',(10.6147618810049,-22.3481448348233,-3.45268519075675));
#86461=CARTESIAN_POINT('Ctrl Pts',(10.622080654927,-22.3721856108078,-3.44172788693612));
#86462=CARTESIAN_POINT('Ctrl Pts',(10.6303374421656,-22.3952935640886,-3.42933684581244));
#86463=CARTESIAN_POINT('Ctrl Pts',(10.6394305448136,-22.4172536196383,-3.41564103111456));
#86464=CARTESIAN_POINT('Ctrl Pts',(10.6482304239307,-22.4385055335037,-3.40238686271701));
#86465=CARTESIAN_POINT('Ctrl Pts',(10.6578134256327,-22.458682025422,-3.38791074678196));
#86466=CARTESIAN_POINT('Ctrl Pts',(10.6680658047926,-22.4776185689884,-3.37236187144577));
#86467=CARTESIAN_POINT('Ctrl Pts',(10.669564024975,-22.4803858400105,-3.37008965360445));
#86468=CARTESIAN_POINT('Ctrl Pts',(10.6710765029369,-22.4831266918783,-3.36779458436634));
#86469=CARTESIAN_POINT('Ctrl Pts',(10.6726028459052,-22.4858406750051,-3.36547718891772));
#86470=CARTESIAN_POINT('Ctrl Pts',(10.6822657120498,-22.5030221710496,-3.35080638262524));
#86471=CARTESIAN_POINT('Ctrl Pts',(10.6924829158915,-22.5191257906813,-3.33524243824077));
#86472=CARTESIAN_POINT('Ctrl Pts',(10.7031594665192,-22.5340498367433,-3.31891032579951));
#86473=CARTESIAN_POINT('Ctrl Pts',(10.7138348392274,-22.5489722362692,-3.30258001524305));
#86474=CARTESIAN_POINT('Ctrl Pts',(10.7249691157714,-22.5627148211697,-3.28548218570652));
#86475=CARTESIAN_POINT('Ctrl Pts',(10.7364505099692,-22.5752141494242,-3.26777236884616));
#86476=CARTESIAN_POINT('Ctrl Pts',(10.7411978244337,-22.5803823581624,-3.2604497329104));
#86477=CARTESIAN_POINT('Ctrl Pts',(10.7460043143161,-22.5853385080984,-3.2530227890494));
#86478=CARTESIAN_POINT('Ctrl Pts',(10.7508614475812,-22.5900803309822,-3.24550376429458));
#86479=CARTESIAN_POINT('Ctrl Pts',(10.7627069683827,-22.6016446341505,-3.22716645311171));
#86480=CARTESIAN_POINT('Ctrl Pts',(10.7748560071437,-22.6119277933076,-3.20827751126037));
#86481=CARTESIAN_POINT('Ctrl Pts',(10.7871852725812,-22.620935663889,-3.18901744575809));
#86482=CARTESIAN_POINT('Ctrl Pts',(10.7903745404317,-22.6232657712415,-3.18403535594778));
#86483=CARTESIAN_POINT('Ctrl Pts',(10.7935758339048,-22.6255107998843,-3.17902851552711));
#86484=CARTESIAN_POINT('Ctrl Pts',(10.7967869569923,-22.6276714019374,-3.17400020894282));
#86485=CARTESIAN_POINT('Ctrl Pts',(10.8086005850894,-22.6356201938167,-3.15550121580945));
#86486=CARTESIAN_POINT('Ctrl Pts',(10.8205463051744,-22.6424216610541,-3.1367127417122));
#86487=CARTESIAN_POINT('Ctrl Pts',(10.8325097037303,-22.6481359064699,-3.11780970742614));
#86488=CARTESIAN_POINT('Ctrl Pts',(10.836369413317,-22.6499794735557,-3.11171108734659));
#86489=CARTESIAN_POINT('Ctrl Pts',(10.8402309498401,-22.65171026809,-3.10560060707827));
#86490=CARTESIAN_POINT('Ctrl Pts',(10.8440904541677,-22.6533314735688,-3.09948429558307));
#86491=CARTESIAN_POINT('Ctrl Pts',(10.8558666365666,-22.658278122103,-3.08082210643566));
#86492=CARTESIAN_POINT('Ctrl Pts',(10.8676229787536,-22.6621918852187,-3.06210658929104));
#86493=CARTESIAN_POINT('Ctrl Pts',(10.8792423341283,-22.6652063814963,-3.04352515477538));
#86494=CARTESIAN_POINT('Ctrl Pts',(10.8901782818038,-22.6680435762027,-3.02603661181894));
#86495=CARTESIAN_POINT('Ctrl Pts',(10.9009927099858,-22.6700845210861,-3.00866714751033));
#86496=CARTESIAN_POINT('Ctrl Pts',(10.9115939386224,-22.6714920197301,-2.99156911371205));
#86497=CARTESIAN_POINT('Ctrl Pts',(10.9122564291068,-22.6715799769368,-2.99050062579605));
#86498=CARTESIAN_POINT('Ctrl Pts',(10.9129180895068,-22.671665477032,-2.98943319573186));
#86499=CARTESIAN_POINT('Ctrl Pts',(10.9135788984978,-22.6717485664354,-2.98836685977345));
#86500=CARTESIAN_POINT('Ctrl Pts',(10.9246016135353,-22.6731345506286,-2.97057969651869));
#86501=CARTESIAN_POINT('Ctrl Pts',(10.9353804297876,-22.6738503295624,-2.95310776326211));
#86502=CARTESIAN_POINT('Ctrl Pts',(10.9458478020495,-22.6741130911883,-2.93607201666154));
#86503=CARTESIAN_POINT('Ctrl Pts',(10.9492132620403,-22.6741975740669,-2.93059469893907));
#86504=CARTESIAN_POINT('Ctrl Pts',(10.9525465530167,-22.6742356128,-2.92516247667493));
#86505=CARTESIAN_POINT('Ctrl Pts',(10.9558455155,-22.6742356128,-2.9197793747));
#86506=CARTESIAN_POINT('',(11.2053401891,-22.6742356128,-2.49849372966));
#86507=CARTESIAN_POINT('Origin',(-2.84607155346,-22.6742356128,5.53854202767));
#86508=CARTESIAN_POINT('',(11.5410915433775,-22.0742358826999,-1.880733914433));
#86509=CARTESIAN_POINT('Ctrl Pts',(11.2053401891,-22.6742356128,-2.49849372966));
#86510=CARTESIAN_POINT('Ctrl Pts',(11.2150383685076,-22.6742356128,-2.48153808629711));
#86511=CARTESIAN_POINT('Ctrl Pts',(11.2249897894519,-22.6738663548581,-2.46406918052205));
#86512=CARTESIAN_POINT('Ctrl Pts',(11.2351241182894,-22.6729000605474,-2.44619729884691));
#86513=CARTESIAN_POINT('Ctrl Pts',(11.2369260237553,-22.6727282513405,-2.44301963984323));
#86514=CARTESIAN_POINT('Ctrl Pts',(11.2387336971335,-22.6725376931046,-2.43982928294016));
#86515=CARTESIAN_POINT('Ctrl Pts',(11.2405467261739,-22.6723272624817,-2.43662689819009));
#86516=CARTESIAN_POINT('Ctrl Pts',(11.2503196279632,-22.6711929630497,-2.41936485166077));
#86517=CARTESIAN_POINT('Ctrl Pts',(11.2602458476986,-22.6694750423375,-2.40175690044939));
#86518=CARTESIAN_POINT('Ctrl Pts',(11.2702378606974,-22.6669990989714,-2.38395208224529));
#86519=CARTESIAN_POINT('Ctrl Pts',(11.2725244303702,-22.6664325047313,-2.37987763224816));
#86520=CARTESIAN_POINT('Ctrl Pts',(11.2748144198167,-22.665826417789,-2.37579294242994));
#86521=CARTESIAN_POINT('Ctrl Pts',(11.2771067403129,-22.6651791086157,-2.37169991214447));
#86522=CARTESIAN_POINT('Ctrl Pts',(11.2875627511759,-22.6622265233383,-2.35303028492714));
#86523=CARTESIAN_POINT('Ctrl Pts',(11.2980683420681,-22.658419074168,-2.33418470244293));
#86524=CARTESIAN_POINT('Ctrl Pts',(11.3085232390998,-22.6536382160094,-2.31534181654695));
#86525=CARTESIAN_POINT('Ctrl Pts',(11.311982469164,-22.6520563651097,-2.30910723793846));
#86526=CARTESIAN_POINT('Ctrl Pts',(11.3154361566497,-22.6503683749809,-2.30287299222311));
#86527=CARTESIAN_POINT('Ctrl Pts',(11.3188807244952,-22.6485711953677,-2.29664559899274));
#86528=CARTESIAN_POINT('Ctrl Pts',(11.3296723127873,-22.6429407583018,-2.27713561489883));
#86529=CARTESIAN_POINT('Ctrl Pts',(11.3403771745526,-22.6362330411102,-2.25768738349784));
#86530=CARTESIAN_POINT('Ctrl Pts',(11.350894153497,-22.6283844511168,-2.23848952894692));
#86531=CARTESIAN_POINT('Ctrl Pts',(11.3538790481232,-22.6261568899304,-2.23304085654893));
#86532=CARTESIAN_POINT('Ctrl Pts',(11.356848858058,-22.6238377439721,-2.22761230160938));
#86533=CARTESIAN_POINT('Ctrl Pts',(11.3598014066801,-22.6214262928633,-2.22220802156407));
#86534=CARTESIAN_POINT('Ctrl Pts',(11.3700755207974,-22.6130350597113,-2.20340250910257));
#86535=CARTESIAN_POINT('Ctrl Pts',(11.380144070066,-22.6035189145293,-2.18488415807147));
#86536=CARTESIAN_POINT('Ctrl Pts',(11.3899200358009,-22.5928768230476,-2.16682324106742));
#86537=CARTESIAN_POINT('Ctrl Pts',(11.3995284381226,-22.582417140672,-2.1490718943892));
#86538=CARTESIAN_POINT('Ctrl Pts',(11.4088538998602,-22.5708701456172,-2.13176302103624));
#86539=CARTESIAN_POINT('Ctrl Pts',(11.4178296800987,-22.5582763477247,-2.11503479986363));
#86540=CARTESIAN_POINT('Ctrl Pts',(11.41987788432,-22.5554025396189,-2.11121754806936));
#86541=CARTESIAN_POINT('Ctrl Pts',(11.4219079567884,-22.5524743831754,-2.10743041339639));
#86542=CARTESIAN_POINT('Ctrl Pts',(11.4239192477556,-22.5494926390321,-2.1036748141767));
#86543=CARTESIAN_POINT('Ctrl Pts',(11.43417381845,-22.5342902110344,-2.08452688464914));
#86544=CARTESIAN_POINT('Ctrl Pts',(11.4439376612349,-22.5176830774906,-2.06620306707214));
#86545=CARTESIAN_POINT('Ctrl Pts',(11.4531160015901,-22.4997822076498,-2.04890684167093));
#86546=CARTESIAN_POINT('Ctrl Pts',(11.4604919004757,-22.4853967086597,-2.03500724711187));
#86547=CARTESIAN_POINT('Ctrl Pts',(11.4674900183935,-22.4701767234614,-2.02177078277232));
#86548=CARTESIAN_POINT('Ctrl Pts',(11.4740689030204,-22.4541987893081,-2.00928995557508));
#86549=CARTESIAN_POINT('Ctrl Pts',(11.4825434750249,-22.4336168576976,-1.99321281260074));
#86550=CARTESIAN_POINT('Ctrl Pts',(11.490322094781,-22.4117772815337,-1.97839019854048));
#86551=CARTESIAN_POINT('Ctrl Pts',(11.497328194312,-22.388875007061,-1.96499799149759));
#86552=CARTESIAN_POINT('Ctrl Pts',(11.5044353732041,-22.3656423137493,-1.95141257056642));
#86553=CARTESIAN_POINT('Ctrl Pts',(11.5107475618039,-22.3413165292408,-1.93929939008369));
#86554=CARTESIAN_POINT('Ctrl Pts',(11.516202430633,-22.3161381940112,-1.92880681486341));
#86555=CARTESIAN_POINT('Ctrl Pts',(11.5217404470366,-22.2905760699918,-1.91815430322522));
#86556=CARTESIAN_POINT('Ctrl Pts',(11.5263947864914,-22.2641357626773,-1.90917247603084));
#86557=CARTESIAN_POINT('Ctrl Pts',(11.5301185510954,-22.2370988916848,-1.90197624996427));
#86558=CARTESIAN_POINT('Ctrl Pts',(11.5312011327901,-22.2292386683008,-1.89988414602147));
#86559=CARTESIAN_POINT('Ctrl Pts',(11.5322051805355,-22.2213281837172,-1.89794268745646));
#86560=CARTESIAN_POINT('Ctrl Pts',(11.5331298302645,-22.2133747150666,-1.8961540158936));
#86561=CARTESIAN_POINT('Ctrl Pts',(11.5363534362541,-22.18564654041,-1.88991817092117));
#86562=CARTESIAN_POINT('Ctrl Pts',(11.538610065403,-22.1573952246849,-1.88554404014394));
#86563=CARTESIAN_POINT('Ctrl Pts',(11.5398768288808,-22.1289373239018,-1.88308865866385));
#86564=CARTESIAN_POINT('Ctrl Pts',(11.5406859896255,-22.1107594899229,-1.88152025355765));
#86565=CARTESIAN_POINT('Ctrl Pts',(11.5410916389492,-22.0924976615588,-1.88073379444023));
#86566=CARTESIAN_POINT('Ctrl Pts',(11.5410916355629,-22.0742358827,-1.88073379476507));
#86567=CARTESIAN_POINT('',(11.5410914269,-19.6742356128,-1.88073402204));
#86568=CARTESIAN_POINT('',(11.5410914269,-21.2742356128,-1.88073402204));
#86569=CARTESIAN_POINT('',(12.9732844032,-19.6742356128,8.9713386779));
#86570=CARTESIAN_POINT('Origin',(-2.84607155346,-19.6742356128,5.53854202767));
#86571=CARTESIAN_POINT('',(12.9732844032,-22.9031898545,8.97133867789999));
#86572=CARTESIAN_POINT('',(12.9732844032,-21.2742356128,8.9713386779));
#86573=CARTESIAN_POINT('',(13.018207968,-22.8742356128,8.75735407375));
#86574=CARTESIAN_POINT('Origin',(12.9922058324069,-23.4864244001328,8.73196264121582));
#86575=CARTESIAN_POINT('',(3.81744045688,-22.8742356128,-9.21387212773));
#86576=CARTESIAN_POINT('Origin',(-2.84607155346,-22.8742356128,5.53854202767));
#86577=CARTESIAN_POINT('Ctrl Pts',(3.81744045688,-22.8742356128,-9.21387212773));
#86578=CARTESIAN_POINT('Ctrl Pts',(3.78438300100211,-22.8742356128,-9.22880383666651));
#86579=CARTESIAN_POINT('Ctrl Pts',(3.75125472648156,-22.876873984767,-9.24363320588492));
#86580=CARTESIAN_POINT('Ctrl Pts',(3.71838012225711,-22.8821739340745,-9.25821762563378));
#86581=CARTESIAN_POINT('Ctrl Pts',(3.6865095776919,-22.8873120117665,-9.27235660648325));
#86582=CARTESIAN_POINT('Ctrl Pts',(3.65487745148123,-22.8949539427161,-9.28626544525872));
#86583=CARTESIAN_POINT('Ctrl Pts',(3.62382288627738,-22.9051278862397,-9.29980564138486));
#86584=CARTESIAN_POINT('Ctrl Pts',(3.59982416043969,-22.9129902304622,-9.31026939936978));
#86585=CARTESIAN_POINT('Ctrl Pts',(3.57617118781195,-22.9223651478789,-9.32051284720793));
#86586=CARTESIAN_POINT('Ctrl Pts',(3.55303923210181,-22.9332555735994,-9.33046796299208));
#86587=CARTESIAN_POINT('Ctrl Pts',(3.52731510523081,-22.9453663824053,-9.34153865086025));
#86588=CARTESIAN_POINT('Ctrl Pts',(3.50223264779224,-22.9593502627365,-9.35225383201401));
#86589=CARTESIAN_POINT('Ctrl Pts',(3.47806004814019,-22.9751863932197,-9.36251314034884));
#86590=CARTESIAN_POINT('Ctrl Pts',(3.45499124406393,-22.990299397063,-9.37230397697133));
#86591=CARTESIAN_POINT('Ctrl Pts',(3.43275123888764,-23.0070999540256,-9.38167960517042));
#86592=CARTESIAN_POINT('Ctrl Pts',(3.41159767393858,-23.0255307665745,-9.39054653772574));
#86593=CARTESIAN_POINT('Ctrl Pts',(3.39154598669303,-23.0430015281129,-9.39895159658247));
#86594=CARTESIAN_POINT('Ctrl Pts',(3.37247065010445,-23.061937444689,-9.40689954920998));
#86595=CARTESIAN_POINT('Ctrl Pts',(3.35461163146646,-23.0822474209105,-9.41430534116002));
#86596=CARTESIAN_POINT('Ctrl Pts',(3.34903427425971,-23.0885902102061,-9.41661816405032));
#86597=CARTESIAN_POINT('Ctrl Pts',(3.34357569434173,-23.0950666709068,-9.41887806947029));
#86598=CARTESIAN_POINT('Ctrl Pts',(3.33824360900109,-23.1016730489955,-9.42108235584647));
#86599=CARTESIAN_POINT('Ctrl Pts',(3.32258626090874,-23.1210722811451,-9.42755511029096));
#86600=CARTESIAN_POINT('Ctrl Pts',(3.30801838438582,-23.1415942623807,-9.43354874753964));
#86601=CARTESIAN_POINT('Ctrl Pts',(3.29472253386083,-23.1631172221777,-9.43900011480726));
#86602=CARTESIAN_POINT('Ctrl Pts',(3.28136620602029,-23.1847380810018,-9.44447627808608));
#86603=CARTESIAN_POINT('Ctrl Pts',(3.26929464819255,-23.2073686497991,-9.44940485150287));
#86604=CARTESIAN_POINT('Ctrl Pts',(3.25868404771759,-23.2308337864388,-9.45372543317535));
#86605=CARTESIAN_POINT('Ctrl Pts',(3.24835603008727,-23.253673996612,-9.45793094857403));
#86606=CARTESIAN_POINT('Ctrl Pts',(3.23941312735556,-23.2773043321175,-9.46156012110628));
#86607=CARTESIAN_POINT('Ctrl Pts',(3.23199421260798,-23.3015220020268,-9.46456562543563));
#86608=CARTESIAN_POINT('Ctrl Pts',(3.22751779279442,-23.3161344434833,-9.46637908462574));
#86609=CARTESIAN_POINT('Ctrl Pts',(3.22359568701309,-23.3309599547749,-9.46796566933521));
#86610=CARTESIAN_POINT('Ctrl Pts',(3.22025193761968,-23.3459477027596,-9.46931721244178));
#86611=CARTESIAN_POINT('Ctrl Pts',(3.21506416160153,-23.3692009644169,-9.47141411089046));
#86612=CARTESIAN_POINT('Ctrl Pts',(3.21127189271638,-23.3928404899255,-9.47294403759531));
#86613=CARTESIAN_POINT('Ctrl Pts',(3.20893196554164,-23.4166584893515,-9.47388782994456));
#86614=CARTESIAN_POINT('Ctrl Pts',(3.20705389182888,-23.4357753059324,-9.47464533710999));
#86615=CARTESIAN_POINT('Ctrl Pts',(3.20611087685479,-23.4550065968702,-9.47502544136242));
#86616=CARTESIAN_POINT('Ctrl Pts',(3.20611087388,-23.4742356128,-9.47502544833));
#86617=CARTESIAN_POINT('',(0.647446102181,-22.5742356128,-10.2675153591));
#86618=CARTESIAN_POINT('Origin',(0.306146745892,-23.1742356128,5.46150961618));
#86619=CARTESIAN_POINT('',(0.11480502971,-19.4742356128,5.54076595007));
#86620=CARTESIAN_POINT('',(3.32093311398,-19.4742356128,4.21274421486));
#86621=CARTESIAN_POINT('',(-0.0382683432365,-19.4742356128,5.60417101718));
#86622=CARTESIAN_POINT('',(3.32093311415531,-23.073803734,4.21274421517325));
#86623=CARTESIAN_POINT('',(3.32093311398,-21.2742356128,4.21274421486));
#86624=CARTESIAN_POINT('',(3.28628881313932,-23.0742356036667,4.22709435412836));
#86625=CARTESIAN_POINT('Origin',(3.00255805893453,-22.7188049298779,4.34461947511254));
#86626=CARTESIAN_POINT('',(0.11480502971,-23.0742356128,5.54076595007));
#86627=CARTESIAN_POINT('',(-0.0382683432365,-23.0742356128,5.60417101718));
#86628=CARTESIAN_POINT('',(0.11480502971,-21.2742356128,5.54076595007));
#86629=CARTESIAN_POINT('Origin',(3.20612808427,-21.2742356128,3.93558035511));
#86630=CARTESIAN_POINT('',(3.48329194402,-19.4742356128,4.05038538482));
#86631=CARTESIAN_POINT('Origin',(3.20612808427,-19.4742356128,3.93558035511));
#86632=CARTESIAN_POINT('',(3.48329194400887,-23.0738037252489,4.05038538484686));
#86633=CARTESIAN_POINT('',(3.48329194402,-21.2742356128,4.05038538482));
#86634=CARTESIAN_POINT('Ctrl Pts',(3.48329194397624,-23.0738037279964,4.05038538492565));
#86635=CARTESIAN_POINT('Ctrl Pts',(3.48098634454964,-23.0736167153402,4.05595159432511));
#86636=CARTESIAN_POINT('Ctrl Pts',(3.4784307715636,-23.0733915443397,4.06163651831605));
#86637=CARTESIAN_POINT('Ctrl Pts',(3.47568621500459,-23.0731489780744,4.06724958582579));
#86638=CARTESIAN_POINT('Ctrl Pts',(3.47295007607425,-23.0729071557663,4.07284543790675));
#86639=CARTESIAN_POINT('Ctrl Pts',(3.47002625698439,-23.0726490502738,4.07836908794044));
#86640=CARTESIAN_POINT('Ctrl Pts',(3.46702586138249,-23.0723930177292,4.08364288587821));
#86641=CARTESIAN_POINT('Ctrl Pts',(3.46391091293507,-23.0721272100547,4.08911803345138));
#86642=CARTESIAN_POINT('Ctrl Pts',(3.46071410686951,-23.0718642230652,4.0943231709983));
#86643=CARTESIAN_POINT('Ctrl Pts',(3.45760867737687,-23.0716094471801,4.09908381872732));
#86644=CARTESIAN_POINT('Ctrl Pts',(3.45706037627568,-23.071564463419,4.09992436860887));
#86645=CARTESIAN_POINT('Ctrl Pts',(3.4565150238358,-23.0715196889556,4.10075113425691));
#86646=CARTESIAN_POINT('Ctrl Pts',(3.45597369050821,-23.0714750936175,4.10156324898665));
#86647=CARTESIAN_POINT('Ctrl Pts',(3.45121228376426,-23.0710828463037,4.10870636830695));
#86648=CARTESIAN_POINT('Ctrl Pts',(3.44576580670688,-23.0707659119886,4.11621427685738));
#86649=CARTESIAN_POINT('Ctrl Pts',(3.43950871638769,-23.0705320441909,4.12394678367705));
#86650=CARTESIAN_POINT('Ctrl Pts',(3.43696673293655,-23.0704370338839,4.12708816463349));
#86651=CARTESIAN_POINT('Ctrl Pts',(3.43413272839561,-23.0703508111332,4.13045538474554));
#86652=CARTESIAN_POINT('Ctrl Pts',(3.4311823830913,-23.0702865717675,4.13379961336395));
#86653=CARTESIAN_POINT('Ctrl Pts',(3.42822610199249,-23.0702222031588,4.13715057022999));
#86654=CARTESIAN_POINT('Ctrl Pts',(3.42515323237904,-23.070180117365,4.14047778426316));
#86655=CARTESIAN_POINT('Ctrl Pts',(3.42218199664131,-23.0701613237193,4.1435627393036));
#86656=CARTESIAN_POINT('Ctrl Pts',(3.42127115978427,-23.0701555624985,4.14450843698671));
#86657=CARTESIAN_POINT('Ctrl Pts',(3.42037014466647,-23.0701518952376,4.14543162551489));
#86658=CARTESIAN_POINT('Ctrl Pts',(3.41948589011018,-23.0701501102534,4.14632668871697));
#86659=CARTESIAN_POINT('Ctrl Pts',(3.41902952637369,-23.0701491890231,4.14678863079506));
#86660=CARTESIAN_POINT('Ctrl Pts',(3.41857813528195,-23.0701487673843,4.14724258288722));
#86661=CARTESIAN_POINT('Ctrl Pts',(3.4181311520111,-23.0701488062869,4.14768934682833));
#86662=CARTESIAN_POINT('Ctrl Pts',(3.40995185158464,-23.0701495181617,4.15586463376247));
#86663=CARTESIAN_POINT('Ctrl Pts',(3.40130199341124,-23.0703088319828,4.16357700165279));
#86664=CARTESIAN_POINT('Ctrl Pts',(3.392239298764,-23.0706029962599,4.17076819388485));
#86665=CARTESIAN_POINT('Ctrl Pts',(3.38355096748122,-23.0708850091479,4.17766233109926));
#86666=CARTESIAN_POINT('Ctrl Pts',(3.37448324687743,-23.0712911996594,4.18407710913278));
#86667=CARTESIAN_POINT('Ctrl Pts',(3.3650882824239,-23.0717548501856,4.18996630671111));
#86668=CARTESIAN_POINT('Ctrl Pts',(3.35653925662874,-23.072176752826,4.19532523087298));
#86669=CARTESIAN_POINT('Ctrl Pts',(3.34771933557013,-23.0726463371389,4.20024856543282));
#86670=CARTESIAN_POINT('Ctrl Pts',(3.33866815976237,-23.0730726361156,4.20471093107887));
#86671=CARTESIAN_POINT('Ctrl Pts',(3.33284862738816,-23.0733467287583,4.20758004796427));
#86672=CARTESIAN_POINT('Ctrl Pts',(3.32693351063594,-23.073602143823,4.21025877484239));
#86673=CARTESIAN_POINT('Ctrl Pts',(3.32093311468,-23.073803734,4.21274421611));
#86674=CARTESIAN_POINT('Origin',(3.56254827791,-23.1742356128,3.85904366864));
#86675=CARTESIAN_POINT('',(4.81131367923,-19.4742356128,0.844257300549));
#86676=CARTESIAN_POINT('',(4.02322090503,-19.4742356128,2.74688156443));
#86677=CARTESIAN_POINT('',(4.81131367968088,-23.0738037377,0.844257300670363));
#86678=CARTESIAN_POINT('',(4.81131367923,-21.2742356128,0.844257300549));
#86679=CARTESIAN_POINT('',(4.7969635399687,-23.0742356036667,0.878901601387461));
#86680=CARTESIAN_POINT('Origin',(4.67943816259639,-22.718804315054,1.16263295713764));
#86681=CARTESIAN_POINT('',(3.49764206635,-23.0742356128,4.01574112487));
#86682=CARTESIAN_POINT('',(3.72150316839,-23.0742356128,3.47529261624));
#86683=CARTESIAN_POINT('Origin',(3.6188764873545,-22.7074964989808,3.72305533773425));
#86684=CARTESIAN_POINT('Origin',(4.53414981948,-21.2742356128,0.729452270839));
#86685=CARTESIAN_POINT('',(4.81131367923,-19.4742356128,0.614647241129));
#86686=CARTESIAN_POINT('Origin',(4.53414981948,-19.4742356128,0.729452270839));
#86687=CARTESIAN_POINT('',(4.81131367923,-23.073803728,0.614647241129));
#86688=CARTESIAN_POINT('',(4.81131367923,-21.2742356128,0.614647241129));
#86689=CARTESIAN_POINT('Ctrl Pts',(4.81131367923,-23.073803728,0.614647241129));
#86690=CARTESIAN_POINT('Ctrl Pts',(4.81361941635584,-23.0736167041411,0.620213782969603));
#86691=CARTESIAN_POINT('Ctrl Pts',(4.81583231216333,-23.0733915202761,0.626041017783809));
#86692=CARTESIAN_POINT('Ctrl Pts',(4.81786074302077,-23.0731489400806,0.631951065709471));
#86693=CARTESIAN_POINT('Ctrl Pts',(4.81988294684359,-23.0729071045767,0.637842970510925));
#86694=CARTESIAN_POINT('Ctrl Pts',(4.82172136423803,-23.07264898495,0.643816521943502));
#86695=CARTESIAN_POINT('Ctrl Pts',(4.82332894451412,-23.072392936172,0.649667543460664));
#86696=CARTESIAN_POINT('Ctrl Pts',(4.82499787516201,-23.072127115759,0.655741858551897));
#86697=CARTESIAN_POINT('Ctrl Pts',(4.8264179869893,-23.0718641136417,0.66168312794498));
#86698=CARTESIAN_POINT('Ctrl Pts',(4.82758840454674,-23.0716093169037,0.667245496676535));
#86699=CARTESIAN_POINT('Ctrl Pts',(4.82779483941714,-23.0715643765905,0.668226571217771));
#86700=CARTESIAN_POINT('Ctrl Pts',(4.82799362825734,-23.0715196449537,0.669195839033689));
#86701=CARTESIAN_POINT('Ctrl Pts',(4.82818491470393,-23.0714750919041,0.670151934751179));
#86702=CARTESIAN_POINT('Ctrl Pts',(4.82986909518099,-23.0710828248214,0.678569874288066));
#86703=CARTESIAN_POINT('Ctrl Pts',(4.83132678694503,-23.0707658746989,0.687730166613046));
#86704=CARTESIAN_POINT('Ctrl Pts',(4.83237008382055,-23.070531995008,0.697622452530011));
#86705=CARTESIAN_POINT('Ctrl Pts',(4.83279391590162,-23.0704369830144,0.701641124707754));
#86706=CARTESIAN_POINT('Ctrl Pts',(4.83317095257545,-23.0703507579002,0.706025977439678));
#86707=CARTESIAN_POINT('Ctrl Pts',(4.83344946883151,-23.0702865157832,0.710476836880151));
#86708=CARTESIAN_POINT('Ctrl Pts',(4.83372854583356,-23.0702221443254,0.714936657383202));
#86709=CARTESIAN_POINT('Ctrl Pts',(4.83390839562994,-23.0701800553783,0.719462128784709));
#86710=CARTESIAN_POINT('Ctrl Pts',(4.83398881030789,-23.0701612585932,0.72374442753318));
#86711=CARTESIAN_POINT('Ctrl Pts',(4.83401346873702,-23.0701554947302,0.725057555470943));
#86712=CARTESIAN_POINT('Ctrl Pts',(4.83402915073398,-23.070151826053,0.726347808314679));
#86713=CARTESIAN_POINT('Ctrl Pts',(4.83403679243025,-23.0701500406831,0.727606300447712));
#86714=CARTESIAN_POINT('Ctrl Pts',(4.83404073492145,-23.0701491195781,0.728255579612234));
#86715=CARTESIAN_POINT('Ctrl Pts',(4.8340425442249,-23.0701486979849,0.728895692950971));
#86716=CARTESIAN_POINT('Ctrl Pts',(4.83404238791158,-23.0701487368575,0.729527607238744));
#86717=CARTESIAN_POINT('Ctrl Pts',(4.83403952722203,-23.0701494482644,0.741092268194386));
#86718=CARTESIAN_POINT('Ctrl Pts',(4.83337656821033,-23.0703087716981,0.752662286883749));
#86719=CARTESIAN_POINT('Ctrl Pts',(4.83205314158895,-23.070602953119,0.764155702040393));
#86720=CARTESIAN_POINT('Ctrl Pts',(4.83078440495958,-23.070884977629,0.775174157140385));
#86721=CARTESIAN_POINT('Ctrl Pts',(4.82890844194233,-23.0712911827742,0.786121930299115));
#86722=CARTESIAN_POINT('Ctrl Pts',(4.82642944014751,-23.0717548494332,0.796929483802132));
#86723=CARTESIAN_POINT('Ctrl Pts',(4.82417372918903,-23.0721767523,0.806763569812917));
#86724=CARTESIAN_POINT('Ctrl Pts',(4.82141849079573,-23.0726463352063,0.816481229255217));
#86725=CARTESIAN_POINT('Ctrl Pts',(4.81817380824922,-23.0730726323263,0.826036466393276));
#86726=CARTESIAN_POINT('Ctrl Pts',(4.81608756260042,-23.0733467301768,0.832180232884085));
#86727=CARTESIAN_POINT('Ctrl Pts',(4.81379910625625,-23.0736021493999,0.838256961933748));
#86728=CARTESIAN_POINT('Ctrl Pts',(4.81131368103,-23.0738037377,0.844257301033));
#86729=CARTESIAN_POINT('Origin',(4.73205734534,-23.1742356128,0.423305524947));
#86730=CARTESIAN_POINT('',(3.48329194402,-19.4742356128,-2.59148084314));
#86731=CARTESIAN_POINT('',(5.72621658766,-19.4742356128,2.8234182509));
#86732=CARTESIAN_POINT('',(3.48329194402,-23.0742356128,-2.59148084314));
#86733=CARTESIAN_POINT('',(3.48329194402,-21.2742356128,-2.59148084314));
#86734=CARTESIAN_POINT('',(4.79748445122,-23.0742356128,0.581260531297));
#86735=CARTESIAN_POINT('',(6.0279343243,-23.0742356128,3.55182930271));
#86736=CARTESIAN_POINT('',(4.80666892690046,-23.074039392286,0.603433817058651));
#86737=CARTESIAN_POINT('Ctrl Pts',(4.79748445122,-23.0742356128,0.581260531297));
#86738=CARTESIAN_POINT('Ctrl Pts',(4.79932022595,-23.0742356128,0.585692483551));
#86739=CARTESIAN_POINT('Ctrl Pts',(4.80115669118,-23.0742141429,0.590126102828));
#86740=CARTESIAN_POINT('Ctrl Pts',(4.80299369795,-23.0741730643,0.594561029481));
#86741=CARTESIAN_POINT('Ctrl Pts',(4.80483113724,-23.0741142107,0.598997000343));
#86742=CARTESIAN_POINT('Ctrl Pts',(4.80666892681,-23.0740393771,0.60343381684));
#86743=CARTESIAN_POINT('Origin',(4.6587912950397,-22.5974864729216,0.246425719139891));
#86744=CARTESIAN_POINT('Origin',(3.20612808427,-21.2742356128,-2.47667581343));
#86745=CARTESIAN_POINT('Origin',(3.20612808427,-19.4742356128,-2.47667581343));
#86746=CARTESIAN_POINT('Origin',(3.20612808427,-23.0742356128,-2.47667581343));
#86747=CARTESIAN_POINT('Origin',(9.38771846805,-25.4742356128,12.7721409138));
#86748=CARTESIAN_POINT('',(9.57074430825,-25.4742356128,13.0098414435));
#86749=CARTESIAN_POINT('Origin',(9.38771846805,-25.4742356128,12.7721409138));
#86750=CARTESIAN_POINT('Origin',(9.38771846805,-25.4742356128,12.7721409138));
#86751=CARTESIAN_POINT('Origin',(-2.72521192632E-16,-25.4742356128,0.580061096523));
#86752=CARTESIAN_POINT('',(12.4158608431,-25.4742356128,10.1688558911));
#86753=CARTESIAN_POINT('Origin',(12.1784264826,-25.4742356128,9.98548488886));
#86754=CARTESIAN_POINT('Origin',(-2.72521192632E-16,-25.4742356128,0.580061096523));
#86755=CARTESIAN_POINT('Origin',(9.38771846805,-22.5741587422,12.7721409138));
#86756=CARTESIAN_POINT('',(9.18405109086,-23.4742356128,12.9924125631));
#86757=CARTESIAN_POINT('',(9.18405109086,-24.4742356128,12.9924125631));
#86758=CARTESIAN_POINT('',(9.57074430825,-23.4742356128,13.0098414435));
#86759=CARTESIAN_POINT('',(9.57074430825,-21.2742356128,13.0098414435));
#86760=CARTESIAN_POINT('Origin',(9.38760641356428,-23.4742356128,12.7746270588514));
#86761=CARTESIAN_POINT('Origin',(3.88971125292,-23.1742356128,8.09716475273));
#86762=CARTESIAN_POINT('',(8.78908955148,-23.4742356128,12.6272235745));
#86763=CARTESIAN_POINT('',(6.87439641858,-23.4742356128,10.8568617063));
#86764=CARTESIAN_POINT('',(8.34854625295,-22.8742356128,12.2198888201));
#86765=CARTESIAN_POINT('Origin',(8.78908955139227,-22.8742356128972,12.627223574425));
#86766=CARTESIAN_POINT('',(8.34854625295,-21.0742356128,12.2198888201));
#86767=CARTESIAN_POINT('',(8.34854625295,-21.9742356128,12.2198888201));
#86768=CARTESIAN_POINT('',(5.19285862192,-21.0742356128,9.30207971851));
#86769=CARTESIAN_POINT('',(6.71750298683,-21.0742356128,10.7117950404));
#86770=CARTESIAN_POINT('',(5.19285862192,-22.8742356128,9.30207971851));
#86771=CARTESIAN_POINT('',(5.19285862192,-21.9742356128,9.30207971851));
#86772=CARTESIAN_POINT('',(6.46706166421,-22.8742356128,10.4802322066));
#86773=CARTESIAN_POINT('Origin',(4.98919124473,-21.9742356128,9.52235136777));
#86774=CARTESIAN_POINT('',(4.80552303981,-21.0742356128,9.28514683472));
#86775=CARTESIAN_POINT('Origin',(4.98919124473,-21.0742356128,9.52235136777));
#86776=CARTESIAN_POINT('',(4.80552303981,-22.8742356128,9.28514683472));
#86777=CARTESIAN_POINT('',(4.80552303981,-21.2742356128,9.28514683472));
#86778=CARTESIAN_POINT('Origin',(4.98919124473,-22.8742356128,9.52235136777));
#86779=CARTESIAN_POINT('Origin',(0.00234331738835,-21.2742356128,3.08191746407));
#86780=CARTESIAN_POINT('',(1.01141425905,-22.8742356128,10.8621723381));
#86781=CARTESIAN_POINT('Origin',(0.00234331738803,-22.8742356128,3.08191746407));
#86782=CARTESIAN_POINT('',(1.01141425905,-21.0742356128,10.8621723381));
#86783=CARTESIAN_POINT('Origin',(0.00234331738803,-21.0742356128,3.08191746407));
#86784=CARTESIAN_POINT('',(1.01141425905,-21.9742356128,10.8621723381));
#86785=CARTESIAN_POINT('Origin',(1.05,-21.9742356128,11.1596805575));
#86786=CARTESIAN_POINT('',(0.75,-21.0742356128,11.1596805575));
#86787=CARTESIAN_POINT('Origin',(1.05,-21.0742356128,11.1596805575));
#86788=CARTESIAN_POINT('',(0.75,-22.8742356128,11.1596805575));
#86789=CARTESIAN_POINT('',(0.75,-21.9742356128,11.1596805575));
#86790=CARTESIAN_POINT('Origin',(1.05,-22.8742356128,11.1596805575));
#86791=CARTESIAN_POINT('Origin',(0.75,-23.1742356128,-8.70195642562));
#86792=CARTESIAN_POINT('',(0.75,-22.8742356128,14.92922515));
#86793=CARTESIAN_POINT('',(0.75,-22.8742356128,2.93538176615));
#86794=CARTESIAN_POINT('',(0.75,-21.0742356128,14.92922515));
#86795=CARTESIAN_POINT('',(0.75,-21.0742356128,12.1167294155));
#86796=CARTESIAN_POINT('',(0.75,-21.9742356128,14.92922515));
#86797=CARTESIAN_POINT('Origin',(8.14487887576,-21.9742356128,12.4401604693));
#86798=CARTESIAN_POINT('',(8.31471092647,-21.0742356128,12.6874600337));
#86799=CARTESIAN_POINT('',(8.31471092647,-22.8742356128,12.6874600337));
#86800=CARTESIAN_POINT('',(8.31471092647,-22.5742356128,12.6874600337));
#86801=CARTESIAN_POINT('Origin',(8.14487887576,-21.0742356128,12.4401604693));
#86802=CARTESIAN_POINT('Ctrl Pts',(8.31471092647,-22.8742356128,12.6874600337));
#86803=CARTESIAN_POINT('Ctrl Pts',(8.40342053421,-22.8742356128,12.6265390425));
#86804=CARTESIAN_POINT('Ctrl Pts',(8.4651120838,-22.8742356128,12.5258960706));
#86805=CARTESIAN_POINT('Ctrl Pts',(8.47411942559,-22.8742356128,12.4014233916));
#86806=CARTESIAN_POINT('Ctrl Pts',(8.4275605919,-22.8742356128,12.2929469882));
#86807=CARTESIAN_POINT('Ctrl Pts',(8.34854625295,-22.8742356128,12.2198888201));
#86808=CARTESIAN_POINT('Origin',(1.05,-21.9742356128,14.92922515));
#86809=CARTESIAN_POINT('',(1.07189396011,-21.0742356128,15.2284251743));
#86810=CARTESIAN_POINT('Origin',(1.05,-21.0742356128,14.92922515));
#86811=CARTESIAN_POINT('',(1.07189396011,-22.8742356128,15.2284251743));
#86812=CARTESIAN_POINT('',(1.07189396011,-22.5742356128,15.2284251743));
#86813=CARTESIAN_POINT('Origin',(1.05,-22.8742356128,14.92922515));
#86814=CARTESIAN_POINT('Origin',(2.4183046301E-16,-21.2742356128,0.580061096523));
#86815=CARTESIAN_POINT('Origin',(2.04268023839E-15,-21.0742356128,0.580061096523));
#86816=CARTESIAN_POINT('Origin',(-2.61864828395E-15,-22.8742356128,0.580061096523));
#86817=CARTESIAN_POINT('Origin',(0.45,-22.8742356128,2.93538176615));
#86818=CARTESIAN_POINT('',(0.75,-22.8742356128,-6.23438845923));
#86819=CARTESIAN_POINT('',(0.75,-22.8742356128,-4.99584562937));
#86820=CARTESIAN_POINT('',(0.75,-22.8742356128,-5.6151170443));
#86821=CARTESIAN_POINT('',(0.45,-23.1742356128,-4.99584562937));
#86822=CARTESIAN_POINT('Origin',(0.45,-22.8742356128,-4.99584562937));
#86823=CARTESIAN_POINT('',(0.45,-23.1742356128,-5.6151170443));
#86824=CARTESIAN_POINT('Origin',(0.45,-22.8742356128,-6.23438845923));
#86825=CARTESIAN_POINT('Origin',(8.13895521212E-16,-22.8742356128,0.729452270839));
#86826=CARTESIAN_POINT('',(0.935307608221,-23.1742356128,5.53218022249));
#86827=CARTESIAN_POINT('',(1.12365184404,-23.1742356128,5.49163692002));
#86828=CARTESIAN_POINT('Origin',(3.42702565972E-16,-23.1742356128,0.729452270839));
#86829=CARTESIAN_POINT('',(1.19254592572,-22.8742356128,5.78361912069));
#86830=CARTESIAN_POINT('Origin',(1.12365184404,-22.8742356128,5.49163692002));
#86831=CARTESIAN_POINT('',(0.992653804111,-22.8742356128,5.82664824081));
#86832=CARTESIAN_POINT('Origin',(3.67394039744E-17,-22.8742356128,0.729452270839));
#86833=CARTESIAN_POINT('Origin',(0.935307608221,-22.8742356128,5.53218022249));
#86834=CARTESIAN_POINT('Origin',(1.05,-22.8742356128,6.12111625914));
#86835=CARTESIAN_POINT('',(0.45,-23.1742356128,6.12111625914));
#86836=CARTESIAN_POINT('Origin',(1.05,-23.1742356128,6.12111625914));
#86837=CARTESIAN_POINT('',(0.75,-22.8742356128,6.12111625914));
#86838=CARTESIAN_POINT('Origin',(1.05,-22.8742356128,6.12111625914));
#86839=CARTESIAN_POINT('Origin',(0.45,-22.8742356128,6.12111625914));
#86840=CARTESIAN_POINT('Origin',(0.45,-22.8742356128,2.93538176615));
#86841=CARTESIAN_POINT('',(0.45,-23.1742356128,9.0358656718));
#86842=CARTESIAN_POINT('',(0.45,-23.1742356128,7.57849096547));
#86843=CARTESIAN_POINT('',(0.75,-22.8742356128,9.0358656718));
#86844=CARTESIAN_POINT('',(0.75,-22.8742356128,7.57849096547));
#86845=CARTESIAN_POINT('Origin',(0.45,-22.8742356128,9.0358656718));
#86846=CARTESIAN_POINT('Origin',(1.05,-22.8742356128,9.0358656718));
#86847=CARTESIAN_POINT('',(1.15397857793,-23.1742356128,9.62678737163));
#86848=CARTESIAN_POINT('Origin',(1.05,-23.1742356128,9.0358656718));
#86849=CARTESIAN_POINT('',(1.10198928897,-22.8742356128,9.33132652171));
#86850=CARTESIAN_POINT('Origin',(1.05,-22.8742356128,9.0358656718));
#86851=CARTESIAN_POINT('Origin',(1.15397857793,-22.8742356128,9.62678737163));
#86852=CARTESIAN_POINT('Origin',(0.00234331738835,-22.8742356128,3.08191746407));
#86853=CARTESIAN_POINT('',(3.7572334818,-23.1742356128,8.56483509371));
#86854=CARTESIAN_POINT('Origin',(0.00234331738835,-23.1742356128,3.08191746407));
#86855=CARTESIAN_POINT('',(3.58772315463,-22.8742356128,8.31731489457));
#86856=CARTESIAN_POINT('Origin',(0.00234331738835,-22.8742356128,3.08191746407));
#86857=CARTESIAN_POINT('Origin',(3.7572334818,-22.8742356128,8.56483509371));
#86858=CARTESIAN_POINT('Origin',(1.2614400074,-22.8742356128,6.07560132137));
#86859=CARTESIAN_POINT('',(1.66877476178,-23.1742356128,5.63505802284));
#86860=CARTESIAN_POINT('Origin',(1.2614400074,-23.1742356128,6.07560132137));
#86861=CARTESIAN_POINT('',(1.46510738459,-22.8742356128,5.8553296721));
#86862=CARTESIAN_POINT('Origin',(1.66877476178,-22.8742356128,5.63505802284));
#86863=CARTESIAN_POINT('Origin',(1.2614400074,-22.8742356128,6.07560132137));
#86864=CARTESIAN_POINT('Origin',(3.41821282746,-22.8742356128,8.06979469543));
#86865=CARTESIAN_POINT('',(3.82554758184,-23.1742356128,7.6292513969));
#86866=CARTESIAN_POINT('Origin',(3.41821282746,-23.1742356128,8.06979469543));
#86867=CARTESIAN_POINT('',(3.62188020465,-22.8742356128,7.84952304616));
#86868=CARTESIAN_POINT('Origin',(3.41821282746,-22.8742356128,8.06979469543));
#86869=CARTESIAN_POINT('Origin',(3.82554758184,-22.8742356128,7.6292513969));
#86870=CARTESIAN_POINT('Origin',(6.6707290414,-22.8742356128,10.2599605573));
#86871=CARTESIAN_POINT('',(2.74716117181,-23.1742356128,6.63215470987));
#86872=CARTESIAN_POINT('',(2.54349379462,-22.8742356128,6.85242635913));
#86873=CARTESIAN_POINT('Origin',(0.00234331738835,-22.8742356128,3.08191746407));
#86874=CARTESIAN_POINT('',(6.21380646358,-22.8742356128,1.78497474518));
#86875=CARTESIAN_POINT('',(5.76218263052,-22.8742356128,0.419477620705));
#86876=CARTESIAN_POINT('Origin',(0.00234331738835,-22.8742356128,3.08191746407));
#86877=CARTESIAN_POINT('',(6.03449750111,-23.1742356128,0.293602240855));
#86878=CARTESIAN_POINT('Origin',(6.03449750111,-22.8742356128,0.293602240855));
#86879=CARTESIAN_POINT('',(6.50747329887,-23.1742356128,1.72365761992));
#86880=CARTESIAN_POINT('Origin',(0.00234331738835,-23.1742356128,3.08191746407));
#86881=CARTESIAN_POINT('Origin',(6.50747329887,-22.8742356128,1.72365761992));
#86882=CARTESIAN_POINT('Ctrl Pts',(4.90348290416,-23.1739412926,0.565017054665));
#86883=CARTESIAN_POINT('Ctrl Pts',(4.87372566569,-23.1752779987,0.577365446817));
#86884=CARTESIAN_POINT('Ctrl Pts',(4.8433931743,-23.1636304197,0.589733130986));
#86885=CARTESIAN_POINT('Ctrl Pts',(4.81906109907,-23.1385222588,0.599388343724));
#86886=CARTESIAN_POINT('Ctrl Pts',(4.80686116456,-23.1062808154,0.603897954914));
#86887=CARTESIAN_POINT('Ctrl Pts',(4.80666892681,-23.0740393771,0.60343381684));
#86888=CARTESIAN_POINT('Ctrl Pts',(4.90080268812,-23.1740535365,0.560642186752));
#86889=CARTESIAN_POINT('Ctrl Pts',(4.87118078695,-23.1751250633,0.572926200655));
#86890=CARTESIAN_POINT('Ctrl Pts',(4.84109884961,-23.1633367321,0.585221262381));
#86891=CARTESIAN_POINT('Ctrl Pts',(4.81703621353,-23.138278721,0.59483800517));
#86892=CARTESIAN_POINT('Ctrl Pts',(4.80498960977,-23.1061964638,0.5993796148));
#86893=CARTESIAN_POINT('Ctrl Pts',(4.80483113724,-23.0741142107,0.598997000343));
#86894=CARTESIAN_POINT('Ctrl Pts',(4.89810075797,-23.174141808,0.556252600105));
#86895=CARTESIAN_POINT('Ctrl Pts',(4.86861969578,-23.1749465698,0.568471513776));
#86896=CARTESIAN_POINT('Ctrl Pts',(4.83879402141,-23.1630185285,0.580695452156));
#86897=CARTESIAN_POINT('Ctrl Pts',(4.81500555152,-23.1380131826,0.59027755579));
#86898=CARTESIAN_POINT('Ctrl Pts',(4.80311602073,-23.1060931221,0.594856360919));
#86899=CARTESIAN_POINT('Ctrl Pts',(4.80299369795,-23.0741730643,0.594561029481));
#86900=CARTESIAN_POINT('Ctrl Pts',(4.89537785067,-23.1742034158,0.551847890098));
#86901=CARTESIAN_POINT('Ctrl Pts',(4.86604324142,-23.1747403351,0.564001283399));
#86902=CARTESIAN_POINT('Ctrl Pts',(4.83647936267,-23.162674027,0.576155883108));
#86903=CARTESIAN_POINT('Ctrl Pts',(4.81296943337,-23.1377239686,0.585707321132));
#86904=CARTESIAN_POINT('Ctrl Pts',(4.80124051889,-23.1059690552,0.590328488331));
#86905=CARTESIAN_POINT('Ctrl Pts',(4.80115669118,-23.0742141429,0.590126102828));
#86906=CARTESIAN_POINT('Ctrl Pts',(4.89263477146,-23.1742356128,0.547427786194));
#86907=CARTESIAN_POINT('Ctrl Pts',(4.86345231855,-23.1745041136,0.559515553974));
#86908=CARTESIAN_POINT('Ctrl Pts',(4.83415555361,-23.1623013592,0.571602872333));
#86909=CARTESIAN_POINT('Ctrl Pts',(4.81092823343,-23.1374093317,0.581127733296));
#86910=CARTESIAN_POINT('Ctrl Pts',(4.79936326115,-23.1058224723,0.585796379724));
#86911=CARTESIAN_POINT('Ctrl Pts',(4.79932022595,-23.0742356128,0.585692483551));
#86912=CARTESIAN_POINT('Ctrl Pts',(4.88987240447,-23.1742356128,0.542992188061));
#86913=CARTESIAN_POINT('Ctrl Pts',(4.86084787295,-23.1742356128,0.555014542658));
#86914=CARTESIAN_POINT('Ctrl Pts',(4.83182334143,-23.1618986073,0.567036897256));
#86915=CARTESIAN_POINT('Ctrl Pts',(4.80888235809,-23.1370674659,0.576539363687));
#86916=CARTESIAN_POINT('Ctrl Pts',(4.79748445122,-23.1056515394,0.581260531297));
#86917=CARTESIAN_POINT('Ctrl Pts',(4.79748445122,-23.0742356128,0.581260531297));
#86918=CARTESIAN_POINT('',(4.88987240447,-23.1742356128,0.542992188061));
#86919=CARTESIAN_POINT('Origin',(4.8892191319917,-23.074942709897,0.543262782382199));
#86920=CARTESIAN_POINT('',(4.90348290262634,-23.1739412930696,0.565017052852735));
#86921=CARTESIAN_POINT('Ctrl Pts',(4.88987240447,-23.1742356128,0.542992188061));
#86922=CARTESIAN_POINT('Ctrl Pts',(4.89447634935402,-23.1742356128,0.550384851456529));
#86923=CARTESIAN_POINT('Ctrl Pts',(4.89901587678319,-23.1741283657784,0.557725607105687));
#86924=CARTESIAN_POINT('Ctrl Pts',(4.90348290292941,-23.1739412926515,0.565017052656334));
#86925=CARTESIAN_POINT('Origin',(4.89839481331612,-23.0747913371752,0.565452395094602));
#86926=CARTESIAN_POINT('Origin',(5.48986775992,-22.8742356128,0.545353000555));
#86927=CARTESIAN_POINT('Origin',(5.48986775992,-23.1742356128,0.545353000555));
#86928=CARTESIAN_POINT('',(5.1900363009,-22.8742356128,0.55540766038));
#86929=CARTESIAN_POINT('Origin',(5.48986775992,-22.8742356128,0.545353000555));
#86930=CARTESIAN_POINT('Origin',(4.89020484189,-22.8742356128,0.565462320206));
#86931=CARTESIAN_POINT('Ctrl Pts',(4.88935150261,-23.1742356021,0.91716994496));
#86932=CARTESIAN_POINT('Ctrl Pts',(4.86032696478,-23.1742356,0.905147589619));
#86933=CARTESIAN_POINT('Ctrl Pts',(4.83130242791,-23.1618985927,0.893125234378));
#86934=CARTESIAN_POINT('Ctrl Pts',(4.80836144191,-23.1370674502,0.883622767727));
#86935=CARTESIAN_POINT('Ctrl Pts',(4.79696353608,-23.1056515239,0.878901600531));
#86936=CARTESIAN_POINT('Ctrl Pts',(4.79696353997,-23.0742355991,0.878901601388));
#86937=CARTESIAN_POINT('Ctrl Pts',(4.89352277618,-23.1742356053,0.910289082657));
#86938=CARTESIAN_POINT('Ctrl Pts',(4.86427270861,-23.1746190551,0.898173309533));
#86939=CARTESIAN_POINT('Ctrl Pts',(4.83486220494,-23.1624737743,0.886051376935));
#86940=CARTESIAN_POINT('Ctrl Pts',(4.81151797125,-23.1375556797,0.876503237567));
#86941=CARTESIAN_POINT('Ctrl Pts',(4.79988864887,-23.1058956405,0.871839755064));
#86942=CARTESIAN_POINT('Ctrl Pts',(4.7998343674,-23.0742356024,0.871970810865));
#86943=CARTESIAN_POINT('Ctrl Pts',(4.89770025261,-23.1741720972,0.903404272608));
#86944=CARTESIAN_POINT('Ctrl Pts',(4.86823093749,-23.1749477738,0.8911929985));
#86945=CARTESIAN_POINT('Ctrl Pts',(4.8384337256,-23.1630030812,0.878969713281));
#86946=CARTESIAN_POINT('Ctrl Pts',(4.81468031581,-23.138001656,0.869376268272));
#86947=CARTESIAN_POINT('Ctrl Pts',(4.80281540183,-23.1060974603,0.864773950955));
#86948=CARTESIAN_POINT('Ctrl Pts',(4.80270499263,-23.0741932655,0.865040508505));
#86949=CARTESIAN_POINT('Ctrl Pts',(4.90188362001,-23.1740438599,0.896515941201));
#86950=CARTESIAN_POINT('Ctrl Pts',(4.87220170104,-23.1752205531,0.884206882396));
#86951=CARTESIAN_POINT('Ctrl Pts',(4.84201719325,-23.1634855096,0.871880308931));
#86952=CARTESIAN_POINT('Ctrl Pts',(4.81784851738,-23.1384045129,0.862241927592));
#86953=CARTESIAN_POINT('Ctrl Pts',(4.80574369007,-23.1062561443,0.85770444106));
#86954=CARTESIAN_POINT('Ctrl Pts',(4.80557522399,-23.074107776,0.858111157027));
#86955=CARTESIAN_POINT('Ctrl Pts',(4.90607254573,-23.1738495698,0.889624547672));
#86956=CARTESIAN_POINT('Ctrl Pts',(4.87618505232,-23.1754360753,0.877215197865));
#86957=CARTESIAN_POINT('Ctrl Pts',(4.84561282186,-23.1639199594,0.864783222044));
#86958=CARTESIAN_POINT('Ctrl Pts',(4.82102262893,-23.1387632939,0.855100274339));
#86959=CARTESIAN_POINT('Ctrl Pts',(4.80867340462,-23.1063707724,0.850631487337));
#86960=CARTESIAN_POINT('Ctrl Pts',(4.80844485738,-23.0739782508,0.851183249168));
#86961=CARTESIAN_POINT('Ctrl Pts',(4.91026668047,-23.1735877856,0.88273057755));
#86962=CARTESIAN_POINT('Ctrl Pts',(4.88018105717,-23.1755928932,0.870218178851));
#86963=CARTESIAN_POINT('Ctrl Pts',(4.84922086665,-23.1643052014,0.857678479765));
#86964=CARTESIAN_POINT('Ctrl Pts',(4.82420271933,-23.1390769393,0.847951335568));
#86965=CARTESIAN_POINT('Ctrl Pts',(4.81160443804,-23.1064403336,0.843555346692));
#86966=CARTESIAN_POINT('Ctrl Pts',(4.81131367923,-23.073803728,0.844257300549));
#86967=CARTESIAN_POINT('',(4.91026667615,-23.1735877859,0.882730584254));
#86968=CARTESIAN_POINT('Origin',(4.90303610744803,-23.074577514893,0.882230480615193));
#86969=CARTESIAN_POINT('',(4.88935150281824,-23.17423560745,0.917169942276108));
#86970=CARTESIAN_POINT('Origin',(4.78463428057749,-22.695072482409,1.13494583768666));
#86971=CARTESIAN_POINT('Origin',(4.88869822348194,-23.0749427242252,0.916899342539095));
#86972=CARTESIAN_POINT('Ctrl Pts',(4.91032402632243,-23.1735838337648,0.882801288663071));
#86973=CARTESIAN_POINT('Ctrl Pts',(4.88022665094269,-23.1756159833063,0.870279796156956));
#86974=CARTESIAN_POINT('Ctrl Pts',(4.84924391018748,-23.1643432866006,0.857726457153785));
#86975=CARTESIAN_POINT('Ctrl Pts',(4.82420253417771,-23.1391098958492,0.847986322123972));
#86976=CARTESIAN_POINT('Ctrl Pts',(4.81159274228477,-23.1064572908804,0.8435837999636));
#86977=CARTESIAN_POINT('Ctrl Pts',(4.8113020121647,-23.0738046836214,0.844285468079136));
#86978=CARTESIAN_POINT('Ctrl Pts',(4.94434678643153,-23.1714537954251,0.826899603928996));
#86979=CARTESIAN_POINT('Ctrl Pts',(4.91067754612114,-23.1770054612896,0.818105977984605));
#86980=CARTESIAN_POINT('Ctrl Pts',(4.87457563392111,-23.1676522550584,0.809243170339568));
#86981=CARTESIAN_POINT('Ctrl Pts',(4.84456167258553,-23.1418126359453,0.802686041110078));
#86982=CARTESIAN_POINT('Ctrl Pts',(4.82932405322906,-23.1071018168935,0.800487598287962));
#86983=CARTESIAN_POINT('Ctrl Pts',(4.82875103516455,-23.072390977125,0.802171963194603));
#86984=CARTESIAN_POINT('Ctrl Pts',(4.96420701657059,-23.1658533501376,0.763668324381971));
#86985=CARTESIAN_POINT('Ctrl Pts',(4.92841400152884,-23.1744320422292,0.760047974352074));
#86986=CARTESIAN_POINT('Ctrl Pts',(4.88880843425898,-23.167036746932,0.75637324615978));
#86987=CARTESIAN_POINT('Ctrl Pts',(4.85536678488683,-23.1410190286572,0.753869397878117));
#86988=CARTESIAN_POINT('Ctrl Pts',(4.83885676622638,-23.104840908069,0.753537697803965));
#86989=CARTESIAN_POINT('Ctrl Pts',(4.83896173895554,-23.0686627522125,0.754909330181028));
#86990=CARTESIAN_POINT('Ctrl Pts',(4.96420960733232,-23.1658532166256,0.695240215931854));
#86991=CARTESIAN_POINT('Ctrl Pts',(4.92841570207977,-23.1744322004681,0.698860297638863));
#86992=CARTESIAN_POINT('Ctrl Pts',(4.88880908546722,-23.1670368247264,0.702534748596797));
#86993=CARTESIAN_POINT('Ctrl Pts',(4.85536672756385,-23.1410185335977,0.705038288754641));
#86994=CARTESIAN_POINT('Ctrl Pts',(4.83885679345067,-23.1048397903563,0.705369584679646));
#86995=CARTESIAN_POINT('Ctrl Pts',(4.83896246818167,-23.0686613287168,0.703997574618044));
#86996=CARTESIAN_POINT('Ctrl Pts',(4.94434696413387,-23.1714537954603,0.632005245990061));
#86997=CARTESIAN_POINT('Ctrl Pts',(4.91067766676893,-23.1770054791343,0.640798851452071));
#86998=CARTESIAN_POINT('Ctrl Pts',(4.87457568728806,-23.167652266686,0.649661638070962));
#86999=CARTESIAN_POINT('Ctrl Pts',(4.8445616776457,-23.1418126091363,0.65621874298175));
#87000=CARTESIAN_POINT('Ctrl Pts',(4.82932406284209,-23.1071017495619,0.658417158281277));
#87001=CARTESIAN_POINT('Ctrl Pts',(4.82875108823279,-23.0723908897367,0.656732768578983));
#87002=CARTESIAN_POINT('Ctrl Pts',(4.91032403084861,-23.1735838343689,0.576103259411724));
#87003=CARTESIAN_POINT('Ctrl Pts',(4.88022665064079,-23.1756159843951,0.58862475168427));
#87004=CARTESIAN_POINT('Ctrl Pts',(4.84924390460287,-23.1643432860911,0.601178090382025));
#87005=CARTESIAN_POINT('Ctrl Pts',(4.82420252556862,-23.1391098913619,0.610918224408618));
#87006=CARTESIAN_POINT('Ctrl Pts',(4.81159273532899,-23.1064572826193,0.615320744486395));
#87007=CARTESIAN_POINT('Ctrl Pts',(4.81130201028653,-23.073804673977,0.614619073855797));
#87008=CARTESIAN_POINT('',(4.91026667801796,-23.1735877850581,0.576173964176449));
#87009=CARTESIAN_POINT('Origin',(4.90303610342538,-23.0745775186776,0.576674063713962));
#87010=CARTESIAN_POINT('Ctrl Pts',(4.91026667829262,-23.1735877856817,0.576173964033033));
#87011=CARTESIAN_POINT('Ctrl Pts',(4.91879478395542,-23.1730554892432,0.590191754493607));
#87012=CARTESIAN_POINT('Ctrl Pts',(4.92622882474333,-23.1722658877838,0.604789479073382));
#87013=CARTESIAN_POINT('Ctrl Pts',(4.93243370799892,-23.1714622149877,0.619819256633221));
#87014=CARTESIAN_POINT('Ctrl Pts',(4.93811287037115,-23.1707266349428,0.633575606860094));
#87015=CARTESIAN_POINT('Ctrl Pts',(4.94276367114871,-23.169980088222,0.647693656938457));
#87016=CARTESIAN_POINT('Ctrl Pts',(4.94629890408633,-23.1693713285753,0.662053029204814));
#87017=CARTESIAN_POINT('Ctrl Pts',(4.94857426938964,-23.1689795154748,0.671295084257086));
#87018=CARTESIAN_POINT('Ctrl Pts',(4.95038777030555,-23.1686439942748,0.680636981774246));
#87019=CARTESIAN_POINT('Ctrl Pts',(4.95171673385527,-23.1683928076863,0.690045471846521));
#87020=CARTESIAN_POINT('Ctrl Pts',(4.95361415108075,-23.168034178016,0.703478369334758));
#87021=CARTESIAN_POINT('Ctrl Pts',(4.95454008117551,-23.1678467304298,0.717033448149962));
#87022=CARTESIAN_POINT('Ctrl Pts',(4.95448640970839,-23.1678573287494,0.730585086546251));
#87023=CARTESIAN_POINT('Ctrl Pts',(4.95447403946633,-23.1678597714585,0.733708478850725));
#87024=CARTESIAN_POINT('Ctrl Pts',(4.95440960372007,-23.1678725183262,0.736831685519014));
#87025=CARTESIAN_POINT('Ctrl Pts',(4.95429295109091,-23.1678955066979,0.739953164503366));
#87026=CARTESIAN_POINT('Ctrl Pts',(4.95376672469149,-23.1679992085021,0.754034327171142));
#87027=CARTESIAN_POINT('Ctrl Pts',(4.95214771891704,-23.1683223664373,0.768061308831125));
#87028=CARTESIAN_POINT('Ctrl Pts',(4.94950130935781,-23.1688045279757,0.781917200280443));
#87029=CARTESIAN_POINT('Ctrl Pts',(4.94672033804524,-23.1693112059394,0.796477621019677));
#87030=CARTESIAN_POINT('Ctrl Pts',(4.94280411815531,-23.1699929254357,0.810849003605565));
#87031=CARTESIAN_POINT('Ctrl Pts',(4.93782602638737,-23.1707197504248,0.82489992093009));
#87032=CARTESIAN_POINT('Ctrl Pts',(4.93251851625825,-23.1714946720558,0.839880638341444));
#87033=CARTESIAN_POINT('Ctrl Pts',(4.92600261331167,-23.1723201180346,0.854496854361639));
#87034=CARTESIAN_POINT('Ctrl Pts',(4.91838074795892,-23.1729821955269,0.86859655447077));
#87035=CARTESIAN_POINT('Ctrl Pts',(4.91580097596841,-23.1732062888284,0.873368878532235));
#87036=CARTESIAN_POINT('Ctrl Pts',(4.91309470690581,-23.1734112694024,0.878082103809534));
#87037=CARTESIAN_POINT('Ctrl Pts',(4.91026667614405,-23.1735877858095,0.882730584253814));
#87038=CARTESIAN_POINT('Ctrl Pts',(4.91026667737,-23.1735877838,0.576173964303));
#87039=CARTESIAN_POINT('Ctrl Pts',(4.88018105555,-23.1755928914,0.588686362769));
#87040=CARTESIAN_POINT('Ctrl Pts',(4.84922086633,-23.1643052,0.60122606158));
#87041=CARTESIAN_POINT('Ctrl Pts',(4.8242027202,-23.1390769384,0.610953205678));
#87042=CARTESIAN_POINT('Ctrl Pts',(4.81160443883,-23.1064403334,0.615349194696));
#87043=CARTESIAN_POINT('Ctrl Pts',(4.81131367923,-23.073803728,0.614647241116));
#87044=CARTESIAN_POINT('Ctrl Pts',(4.90856932846,-23.173693728,0.573384000981));
#87045=CARTESIAN_POINT('Ctrl Pts',(4.87856388841,-23.175529429,0.585854696056));
#87046=CARTESIAN_POINT('Ctrl Pts',(4.84776070495,-23.1641492947,0.59835079987));
#87047=CARTESIAN_POINT('Ctrl Pts',(4.82291574931,-23.138950008,0.608060057838));
#87048=CARTESIAN_POINT('Ctrl Pts',(4.81041826051,-23.1064121826,0.612485507872));
#87049=CARTESIAN_POINT('Ctrl Pts',(4.81015267804,-23.073874357,0.611844336315));
#87050=CARTESIAN_POINT('Ctrl Pts',(4.90687289735,-23.1737878802,0.570594502155));
#87051=CARTESIAN_POINT('Ctrl Pts',(4.87694893964,-23.1754557109,0.583023975772));
#87052=CARTESIAN_POINT('Ctrl Pts',(4.8463027189,-23.1639847944,0.595476889953));
#87053=CARTESIAN_POINT('Ctrl Pts',(4.82162983017,-23.138815193,0.605168197316));
#87054=CARTESIAN_POINT('Ctrl Pts',(4.80923231893,-23.1063761589,0.609622392402));
#87055=CARTESIAN_POINT('Ctrl Pts',(4.80899154105,-23.0739371247,0.609041103626));
#87056=CARTESIAN_POINT('Ctrl Pts',(4.90517741318,-23.173870363,0.567805508191));
#87057=CARTESIAN_POINT('Ctrl Pts',(4.87533620313,-23.1753718603,0.580194220924));
#87058=CARTESIAN_POINT('Ctrl Pts',(4.84484688747,-23.1638118024,0.59260433356));
#87059=CARTESIAN_POINT('Ctrl Pts',(4.82034495602,-23.1386725836,0.602277625735));
#87060=CARTESIAN_POINT('Ctrl Pts',(4.80804662282,-23.1063323483,0.606759869239));
#87061=CARTESIAN_POINT('Ctrl Pts',(4.80783028602,-23.0739921129,0.606237585981));
#87062=CARTESIAN_POINT('Ctrl Pts',(4.90348289858,-23.1739412934,0.56501704892));
#87063=CARTESIAN_POINT('Ctrl Pts',(4.87372566819,-23.1752779933,0.577365441412));
#87064=CARTESIAN_POINT('Ctrl Pts',(4.84339318703,-23.163630415,0.589733124619));
#87065=CARTESIAN_POINT('Ctrl Pts',(4.81906111697,-23.138522264,0.599388336927));
#87066=CARTESIAN_POINT('Ctrl Pts',(4.80686117717,-23.106280832,0.603897950258));
#87067=CARTESIAN_POINT('Ctrl Pts',(4.80666892643,-23.0740393999,0.603433815923));
#87068=CARTESIAN_POINT('Origin',(4.75289906745657,-22.5762659927124,0.262522382627455));
#87069=CARTESIAN_POINT('Origin',(3.67394039744E-17,-22.8742356128,0.729452270839));
#87070=CARTESIAN_POINT('',(5.08448267152,-22.8742356128,1.78529520144));
#87071=CARTESIAN_POINT('Origin',(3.67394039744E-17,-22.8742356128,0.729452270839));
#87072=CARTESIAN_POINT('',(4.79074910795,-23.1742356128,1.72429853244));
#87073=CARTESIAN_POINT('Origin',(4.79074910795,-22.8742356128,1.72429853244));
#87074=CARTESIAN_POINT('Origin',(3.42702565972E-16,-23.1742356128,0.729452270839));
#87075=CARTESIAN_POINT('Origin',(5.92013962829,-22.8742356128,1.84629187045));
#87076=CARTESIAN_POINT('',(5.92013962829,-22.8742356128,2.14629187045));
#87077=CARTESIAN_POINT('Origin',(5.92013962829,-22.8742356128,1.84629187045));
#87078=CARTESIAN_POINT('',(5.92013962829,-23.1742356128,2.44629187045));
#87079=CARTESIAN_POINT('Origin',(5.92013962829,-23.1742356128,1.84629187045));
#87080=CARTESIAN_POINT('Origin',(5.92013962829,-22.8742356128,2.44629187045));
#87081=CARTESIAN_POINT('Origin',(5.3782162351,-22.8742356128,1.84629187045));
#87082=CARTESIAN_POINT('',(5.3782162351,-22.8742356128,2.14629187045));
#87083=CARTESIAN_POINT('Origin',(5.3782162351,-22.8742356128,1.84629187045));
#87084=CARTESIAN_POINT('',(5.3782162351,-23.1742356128,2.44629187045));
#87085=CARTESIAN_POINT('Origin',(5.3782162351,-22.8742356128,2.44629187045));
#87086=CARTESIAN_POINT('Origin',(5.3782162351,-23.1742356128,1.84629187045));
#87087=CARTESIAN_POINT('Origin',(-6.6707290414,-22.8742356128,2.44629187045));
#87088=CARTESIAN_POINT('',(5.6491779317,-22.8742356128,2.14629187045));
#87089=CARTESIAN_POINT('',(5.6491779317,-23.1742356128,2.44629187045));
#87090=CARTESIAN_POINT('Ctrl Pts',(3.32455716278,-23.1742356021,4.31948231426));
#87091=CARTESIAN_POINT('Ctrl Pts',(3.31253480425,-23.1742356,4.29045777775));
#87092=CARTESIAN_POINT('Ctrl Pts',(3.30051244632,-23.1618985927,4.26143324199));
#87093=CARTESIAN_POINT('Ctrl Pts',(3.29100997816,-23.1370674502,4.23849225662));
#87094=CARTESIAN_POINT('Ctrl Pts',(3.286288811,-23.1056515239,4.22709435078));
#87095=CARTESIAN_POINT('Ctrl Pts',(3.28628881314,-23.0742355991,4.22709435413));
#87096=CARTESIAN_POINT('Ctrl Pts',(3.33237220301,-23.1742356053,4.31756634569));
#87097=CARTESIAN_POINT('Ctrl Pts',(3.32025642721,-23.1746190551,4.28831627923));
#87098=CARTESIAN_POINT('Ctrl Pts',(3.30803156137,-23.1624737743,4.2589484119));
#87099=CARTESIAN_POINT('Ctrl Pts',(3.29827624952,-23.1375556797,4.23568999186));
#87100=CARTESIAN_POINT('Ctrl Pts',(3.29335065691,-23.1058956405,4.22416923905));
#87101=CARTESIAN_POINT('Ctrl Pts',(3.29321960366,-23.0742356024,4.2242235267));
#87102=CARTESIAN_POINT('Ctrl Pts',(3.34019442079,-23.1741720972,4.31565197173));
#87103=CARTESIAN_POINT('Ctrl Pts',(3.32799114296,-23.1749477738,4.28617934444));
#87104=CARTESIAN_POINT('Ctrl Pts',(3.31556450024,-23.1630030812,4.25646636599));
#87105=CARTESIAN_POINT('Ctrl Pts',(3.30555189312,-23.138001656,4.23288657883));
#87106=CARTESIAN_POINT('Ctrl Pts',(3.30041646177,-23.1060974603,4.22124248791));
#87107=CARTESIAN_POINT('Ctrl Pts',(3.30014990602,-23.0741932655,4.22135290147));
#87108=CARTESIAN_POINT('Ctrl Pts',(3.3480232941,-23.1740438599,4.31373927334));
#87109=CARTESIAN_POINT('Ctrl Pts',(3.33573882686,-23.1752205531,4.28404716821));
#87110=CARTESIAN_POINT('Ctrl Pts',(3.3231113604,-23.1634855096,4.25398729437));
#87111=CARTESIAN_POINT('Ctrl Pts',(3.3128368906,-23.1384045129,4.23008209497));
#87112=CARTESIAN_POINT('Ctrl Pts',(3.30748597263,-23.1062561443,4.218314202));
#87113=CARTESIAN_POINT('Ctrl Pts',(3.3070792575,-23.074107776,4.21848267011));
#87114=CARTESIAN_POINT('Ctrl Pts',(3.35585826297,-23.1738495698,4.31182834003));
#87115=CARTESIAN_POINT('Ctrl Pts',(3.34349934911,-23.1754360753,4.28191995536));
#87116=CARTESIAN_POINT('Ctrl Pts',(3.33067225204,-23.1639199594,4.25151138948));
#87117=CARTESIAN_POINT('Ctrl Pts',(3.32013123785,-23.1387632939,4.22727661933));
#87118=CARTESIAN_POINT('Ctrl Pts',(3.31455892719,-23.1063707724,4.21538448948));
#87119=CARTESIAN_POINT('Ctrl Pts',(3.31400716536,-23.0739782508,4.21561303671));
#87120=CARTESIAN_POINT('Ctrl Pts',(3.36369873711,-23.1735877856,4.30991926812));
#87121=CARTESIAN_POINT('Ctrl Pts',(3.35127259083,-23.1755928932,4.2797979179));
#87122=CARTESIAN_POINT('Ctrl Pts',(3.33824733642,-23.1643052014,4.24903885097));
#87123=CARTESIAN_POINT('Ctrl Pts',(3.32743496442,-23.1390769393,4.22447021973));
#87124=CARTESIAN_POINT('Ctrl Pts',(3.32163506784,-23.1064403336,4.21245345605));
#87125=CARTESIAN_POINT('Ctrl Pts',(3.32093311398,-23.073803728,4.21274421486));
#87126=CARTESIAN_POINT('',(3.36369873258,-23.1735877857,4.30991926955));
#87127=CARTESIAN_POINT('Origin',(3.35893957337299,-23.074577514808,4.30445285837843));
#87128=CARTESIAN_POINT('',(3.32455716483031,-23.17423560745,4.3194823125052));
#87129=CARTESIAN_POINT('Origin',(3.09652469257192,-22.6950826646314,4.39942546521357));
#87130=CARTESIAN_POINT('Origin',(3.32428656951706,-23.0749427241466,4.31882903140108));
#87131=CARTESIAN_POINT('Ctrl Pts',(3.36368929336556,-23.1735838355436,4.3100097843108));
#87132=CARTESIAN_POINT('Ctrl Pts',(3.35126126667731,-23.1756159753277,4.27987369799882));
#87133=CARTESIAN_POINT('Ctrl Pts',(3.33822971249265,-23.1643432723425,4.24908904885602));
#87134=CARTESIAN_POINT('Ctrl Pts',(3.32741010276691,-23.1391098819976,4.22449481546317));
#87135=CARTESIAN_POINT('Ctrl Pts',(3.32160668783934,-23.1064572814787,4.21246529856621));
#87136=CARTESIAN_POINT('Ctrl Pts',(3.3209049569083,-23.0738046795702,4.21275587774604));
#87137=CARTESIAN_POINT('Ctrl Pts',(3.42727587068037,-23.1714537891356,4.29453895824509));
#87138=CARTESIAN_POINT('Ctrl Pts',(3.40968612110659,-23.1770054655411,4.26451318049342));
#87139=CARTESIAN_POINT('Ctrl Pts',(3.39042512741839,-23.1676522631102,4.23271832267249));
#87140=CARTESIAN_POINT('Ctrl Pts',(3.3738386086957,-23.1418126390217,4.20685865723294));
#87141=CARTESIAN_POINT('Ctrl Pts',(3.36461849949685,-23.1071018108388,4.19452950363387));
#87142=CARTESIAN_POINT('Ctrl Pts',(3.36302228471092,-23.0723909633791,4.1953153506082));
#87143=CARTESIAN_POINT('Ctrl Pts',(3.48602780500958,-23.1658533405815,4.26387171240888));
#87144=CARTESIAN_POINT('Ctrl Pts',(3.46327855666835,-23.1744319191555,4.23600234342951));
#87145=CARTESIAN_POINT('Ctrl Pts',(3.43787192065916,-23.1670366207478,4.20539868415393));
#87146=CARTESIAN_POINT('Ctrl Pts',(3.41599585681065,-23.1410190434613,4.1799814558232));
#87147=CARTESIAN_POINT('Ctrl Pts',(3.40455618145493,-23.1048410962315,4.16807249384115));
#87148=CARTESIAN_POINT('Ctrl Pts',(3.40366050713365,-23.068663043311,4.16911644023449));
#87149=CARTESIAN_POINT('Ctrl Pts',(3.53441735913858,-23.1658531413152,4.21548783590638));
#87150=CARTESIAN_POINT('Ctrl Pts',(3.50654749801918,-23.1744321561296,4.19273743139755));
#87151=CARTESIAN_POINT('Ctrl Pts',(3.47594318930563,-23.1670368001775,4.16732946763638));
#87152=CARTESIAN_POINT('Ctrl Pts',(3.45052561848652,-23.1410185073567,4.14545234848626));
#87153=CARTESIAN_POINT('Ctrl Pts',(3.43861708176451,-23.1048397492347,4.13401229478962));
#87154=CARTESIAN_POINT('Ctrl Pts',(3.43966196606321,-23.0686612727428,4.1331168715304));
#87155=CARTESIAN_POINT('Ctrl Pts',(3.56508656734137,-23.1714537839891,4.15672855586756));
#87156=CARTESIAN_POINT('Ctrl Pts',(3.53506076659917,-23.1770054815344,4.13913874792724));
#87157=CARTESIAN_POINT('Ctrl Pts',(3.50326587807461,-23.1676522759815,4.11987768748972));
#87158=CARTESIAN_POINT('Ctrl Pts',(3.47740619605725,-23.1418126154361,4.10329111307365));
#87159=CARTESIAN_POINT('Ctrl Pts',(3.46507706381281,-23.1071017471307,4.09407098400021));
#87160=CARTESIAN_POINT('Ctrl Pts',(3.46586295657012,-23.0723908784742,4.09247478015265));
#87161=CARTESIAN_POINT('Ctrl Pts',(3.58055751223848,-23.1735838358499,4.09314156852285));
#87162=CARTESIAN_POINT('Ctrl Pts',(3.55042142397976,-23.1756159758171,4.08071353967926));
#87163=CARTESIAN_POINT('Ctrl Pts',(3.51963677274451,-23.1643432719327,4.06768198311457));
#87164=CARTESIAN_POINT('Ctrl Pts',(3.495042538531,-23.13910987911,4.05686237170097));
#87165=CARTESIAN_POINT('Ctrl Pts',(3.48301302329125,-23.1064572763175,4.05105895662086));
#87166=CARTESIAN_POINT('Ctrl Pts',(3.48330360576356,-23.0738046736254,4.05035722683515));
#87167=CARTESIAN_POINT('',(3.58046699021159,-23.1735877810644,4.09315100260664));
#87168=CARTESIAN_POINT('Origin',(3.5750005834412,-23.0745775165868,4.08839183728771));
#87169=CARTESIAN_POINT('Ctrl Pts',(3.58046699304039,-23.1735877859444,4.09315100345836));
#87170=CARTESIAN_POINT('Ctrl Pts',(3.57658526578705,-23.1730554985274,4.10909309137931));
#87171=CARTESIAN_POINT('Ctrl Pts',(3.57151986290398,-23.1722659160818,4.1246716419425));
#87172=CARTESIAN_POINT('Ctrl Pts',(3.5652798453657,-23.1714622614676,4.13968656724023));
#87173=CARTESIAN_POINT('Ctrl Pts',(3.55956845646456,-23.170726689169,4.15342948978343));
#87174=CARTESIAN_POINT('Ctrl Pts',(3.55287415413697,-23.1699801491101,4.16670101052127));
#87175=CARTESIAN_POINT('Ctrl Pts',(3.5452204080535,-23.1693713921876,4.17935434371679));
#87176=CARTESIAN_POINT('Ctrl Pts',(3.54029406542148,-23.1689795650814,4.18749867644987));
#87177=CARTESIAN_POINT('Ctrl Pts',(3.53497051338374,-23.1686440328199,4.19538699940324));
#87178=CARTESIAN_POINT('Ctrl Pts',(3.52925723559328,-23.1683928406018,4.20297976398894));
#87179=CARTESIAN_POINT('Ctrl Pts',(3.52110035296887,-23.1680342118927,4.2138200017284));
#87180=CARTESIAN_POINT('Ctrl Pts',(3.51217014253913,-23.1678467659713,4.22405966720967));
#87181=CARTESIAN_POINT('Ctrl Pts',(3.50254971355978,-23.1678573637056,4.2336041965472));
#87182=CARTESIAN_POINT('Ctrl Pts',(3.50033236766523,-23.1678598063038,4.23580404886016));
#87183=CARTESIAN_POINT('Ctrl Pts',(3.49807833812036,-23.1678725531436,4.2379669522243));
#87184=CARTESIAN_POINT('Ctrl Pts',(3.4957886085378,-23.1678955415342,4.24009170920016));
#87185=CARTESIAN_POINT('Ctrl Pts',(3.48545965182566,-23.1679992420294,4.24967647545144));
#87186=CARTESIAN_POINT('Ctrl Pts',(3.47439638442631,-23.1683223884004,4.25845019369705));
#87187=CARTESIAN_POINT('Ctrl Pts',(3.46272764401182,-23.1688045362578,4.26637644567551));
#87188=CARTESIAN_POINT('Ctrl Pts',(3.45046583703957,-23.1693111893969,4.27470555133053));
#87189=CARTESIAN_POINT('Ctrl Pts',(3.43753502135603,-23.1699928747773,4.28209828027822));
#87190=CARTESIAN_POINT('Ctrl Pts',(3.42407993887611,-23.170719673524,4.28851360926196));
#87191=CARTESIAN_POINT('Ctrl Pts',(3.40973489722923,-23.1714945449011,4.29535326718213));
#87192=CARTESIAN_POINT('Ctrl Pts',(3.39479315367958,-23.1723199471667,4.30108085339101));
#87193=CARTESIAN_POINT('Ctrl Pts',(3.37943451815742,-23.1729820221765,4.30566133260555));
#87194=CARTESIAN_POINT('Ctrl Pts',(3.374234505679,-23.1732061826046,4.30721215715884));
#87195=CARTESIAN_POINT('Ctrl Pts',(3.36898679610344,-23.1734112234077,4.30863168405366));
#87196=CARTESIAN_POINT('Ctrl Pts',(3.36369873257884,-23.1735877856743,4.30991926954876));
#87197=CARTESIAN_POINT('Ctrl Pts',(3.58046698701,-23.1735877712,4.09315099924));
#87198=CARTESIAN_POINT('Ctrl Pts',(3.55034564212,-23.1755928789,4.0807248569));
#87199=CARTESIAN_POINT('Ctrl Pts',(3.51958658051,-23.1643051888,4.06769960633));
#87200=CARTESIAN_POINT('Ctrl Pts',(3.49501795255,-23.13907693,4.05688723684));
#87201=CARTESIAN_POINT('Ctrl Pts',(3.48300118847,-23.1064403276,4.05108734042));
#87202=CARTESIAN_POINT('Ctrl Pts',(3.48329194402,-23.073803724,4.05038538482));
#87203=CARTESIAN_POINT('Ctrl Pts',(3.58237609938,-23.1738495633,4.08531036606));
#87204=CARTESIAN_POINT('Ctrl Pts',(3.55246772359,-23.1754360605,4.07295145689));
#87205=CARTESIAN_POINT('Ctrl Pts',(3.52205916937,-23.1639199413,4.06012436711));
#87206=CARTESIAN_POINT('Ctrl Pts',(3.49782440883,-23.1387632801,4.0495833606));
#87207=CARTESIAN_POINT('Ctrl Pts',(3.48593228125,-23.1063707663,4.04401105478));
#87208=CARTESIAN_POINT('Ctrl Pts',(3.48616082452,-23.0739782513,4.04345929461));
#87209=CARTESIAN_POINT('Ctrl Pts',(3.58428706187,-23.1740438603,4.0774752762));
#87210=CARTESIAN_POINT('Ctrl Pts',(3.55459496917,-23.1752205389,4.06519081505));
#87211=CARTESIAN_POINT('Ctrl Pts',(3.52453511246,-23.1634854888,4.05256335909));
#87212=CARTESIAN_POINT('Ctrl Pts',(3.50062992774,-23.1384044972,4.0422889011));
#87213=CARTESIAN_POINT('Ctrl Pts',(3.48886203891,-23.1062561396,4.03693799135));
#87214=CARTESIAN_POINT('Ctrl Pts',(3.48903050209,-23.0741077812,4.0365312801));
#87215=CARTESIAN_POINT('Ctrl Pts',(3.58619975923,-23.1741721033,4.06964640553));
#87216=CARTESIAN_POINT('Ctrl Pts',(3.55672714472,-23.1749477659,4.05744313429));
#87217=CARTESIAN_POINT('Ctrl Pts',(3.52701418337,-23.1630030668,4.04501650225));
#87218=CARTESIAN_POINT('Ctrl Pts',(3.50343441064,-23.1380016463,4.03500390673));
#87219=CARTESIAN_POINT('Ctrl Pts',(3.49179032375,-23.1060974606,4.02986848333));
#87220=CARTESIAN_POINT('Ctrl Pts',(3.49190073237,-23.0741932746,4.02960193123));
#87221=CARTESIAN_POINT('Ctrl Pts',(3.58811409552,-23.1742356128,4.0618243387));
#87222=CARTESIAN_POINT('Ctrl Pts',(3.5588640379,-23.1746190563,4.04970856814));
#87223=CARTESIAN_POINT('Ctrl Pts',(3.52949618126,-23.162473773,4.03748370929));
#87224=CARTESIAN_POINT('Ctrl Pts',(3.50623776954,-23.1375556813,4.02772840414));
#87225=CARTESIAN_POINT('Ctrl Pts',(3.49471701837,-23.1058956471,4.02280281538));
#87226=CARTESIAN_POINT('Ctrl Pts',(3.49477130203,-23.0742356128,4.02267176303));
#87227=CARTESIAN_POINT('Ctrl Pts',(3.59003001961,-23.1742356128,4.0540094681));
#87228=CARTESIAN_POINT('Ctrl Pts',(3.56100548808,-23.1742356128,4.0419871135));
#87229=CARTESIAN_POINT('Ctrl Pts',(3.53198095656,-23.1618986073,4.02996475891));
#87230=CARTESIAN_POINT('Ctrl Pts',(3.50903997323,-23.1370674659,4.02046229248));
#87231=CARTESIAN_POINT('Ctrl Pts',(3.49764206635,-23.1056515394,4.01574112487));
#87232=CARTESIAN_POINT('Ctrl Pts',(3.49764206635,-23.0742356128,4.01574112487));
#87233=CARTESIAN_POINT('',(3.59003001961,-23.1742356128,4.0540094681));
#87234=CARTESIAN_POINT('Origin',(3.58937674712371,-23.0749427098877,4.05373887377641));
#87235=CARTESIAN_POINT('Origin',(3.67125418556151,-22.686923854516,3.82239309382983));
#87236=CARTESIAN_POINT('Origin',(-8.51439015726E-16,-22.8742356128,0.729452270839));
#87237=CARTESIAN_POINT('',(3.96612236541,-23.1742356128,3.59491374888));
#87238=CARTESIAN_POINT('Origin',(3.42702565972E-16,-23.1742356128,0.729452270839));
#87239=CARTESIAN_POINT('',(4.2092958712,-22.8742356128,3.77060280966));
#87240=CARTESIAN_POINT('Origin',(3.96612236541,-22.8742356128,3.59491374888));
#87241=CARTESIAN_POINT('',(3.13117783752,-22.8742356128,4.87221628548));
#87242=CARTESIAN_POINT('Origin',(3.67394039744E-17,-22.8742356128,0.729452270839));
#87243=CARTESIAN_POINT('',(2.95028784657,-23.1742356128,4.63288636429));
#87244=CARTESIAN_POINT('Origin',(2.95028784657,-22.8742356128,4.63288636429));
#87245=CARTESIAN_POINT('Origin',(3.42702565972E-16,-23.1742356128,0.729452270839));
#87246=CARTESIAN_POINT('Origin',(3.31206782846,-22.8742356128,5.11154620667));
#87247=CARTESIAN_POINT('',(2.90473307408,-23.1742356128,5.55208950519));
#87248=CARTESIAN_POINT('Origin',(3.31206782846,-23.1742356128,5.11154620667));
#87249=CARTESIAN_POINT('',(3.10840045127,-22.8742356128,5.33181785593));
#87250=CARTESIAN_POINT('Origin',(3.31206782846,-22.8742356128,5.11154620667));
#87251=CARTESIAN_POINT('Origin',(2.90473307408,-22.8742356128,5.55208950519));
#87252=CARTESIAN_POINT('Origin',(6.6707290414,-22.8742356128,9.03420135995));
#87253=CARTESIAN_POINT('',(4.51260368036,-23.1742356128,7.03875740065));
#87254=CARTESIAN_POINT('',(3.70866837722,-23.1742356128,6.29542345292));
#87255=CARTESIAN_POINT('',(4.71627105755,-22.8742356128,6.81848575139));
#87256=CARTESIAN_POINT('',(3.91233575441,-22.8742356128,6.07515180366));
#87257=CARTESIAN_POINT('Origin',(4.51260368036,-22.8742356128,7.03875740065));
#87258=CARTESIAN_POINT('Origin',(4.91993843473,-22.8742356128,6.59821410213));
#87259=CARTESIAN_POINT('',(5.40800342362,-23.1742356128,6.94720201972));
#87260=CARTESIAN_POINT('Origin',(4.91993843473,-23.1742356128,6.59821410213));
#87261=CARTESIAN_POINT('',(5.16397092918,-22.8742356128,6.77270806092));
#87262=CARTESIAN_POINT('Origin',(4.91993843473,-22.8742356128,6.59821410213));
#87263=CARTESIAN_POINT('Origin',(5.40800342362,-22.8742356128,6.94720201972));
#87264=CARTESIAN_POINT('Origin',(0.00234331738835,-22.8742356128,3.08191746407));
#87265=CARTESIAN_POINT('',(6.57948381998,-23.1742356128,4.03207991826));
#87266=CARTESIAN_POINT('Origin',(0.00234331738835,-23.1742356128,3.08191746407));
#87267=CARTESIAN_POINT('',(6.28256615006,-22.8742356128,3.98918589435));
#87268=CARTESIAN_POINT('Origin',(0.00234331738835,-22.8742356128,3.08191746407));
#87269=CARTESIAN_POINT('Origin',(6.57948381998,-22.8742356128,4.03207991826));
#87270=CARTESIAN_POINT('Origin',(4.452469377,-22.8742356128,3.94629187045));
#87271=CARTESIAN_POINT('',(4.452469377,-23.1742356128,3.34629187045));
#87272=CARTESIAN_POINT('Origin',(4.452469377,-23.1742356128,3.94629187045));
#87273=CARTESIAN_POINT('',(4.452469377,-22.8742356128,3.64629187045));
#87274=CARTESIAN_POINT('Origin',(4.452469377,-22.8742356128,3.34629187045));
#87275=CARTESIAN_POINT('Origin',(4.452469377,-22.8742356128,3.94629187045));
#87276=CARTESIAN_POINT('Origin',(5.98564848014,-22.8742356128,3.94629187045));
#87277=CARTESIAN_POINT('',(5.98564848014,-23.1742356128,3.34629187045));
#87278=CARTESIAN_POINT('Origin',(5.98564848014,-23.1742356128,3.94629187045));
#87279=CARTESIAN_POINT('',(5.98564848014,-22.8742356128,3.64629187045));
#87280=CARTESIAN_POINT('Origin',(5.98564848014,-22.8742356128,3.94629187045));
#87281=CARTESIAN_POINT('Origin',(5.98564848014,-22.8742356128,3.34629187045));
#87282=CARTESIAN_POINT('Origin',(-6.6707290414,-22.8742356128,3.34629187045));
#87283=CARTESIAN_POINT('',(5.21905892857,-23.1742356128,3.34629187045));
#87284=CARTESIAN_POINT('',(5.21905892857,-22.8742356128,3.64629187045));
#87285=CARTESIAN_POINT('Origin',(4.1372329486,-21.0742356128,5.87450964899));
#87286=CARTESIAN_POINT('',(3.31206782846,-20.7742356128,5.11154620667));
#87287=CARTESIAN_POINT('',(4.91993843473,-20.7742356128,6.59821410213));
#87288=CARTESIAN_POINT('',(4.1160031316,-20.7742356128,5.8548801544));
#87289=CARTESIAN_POINT('',(4.71627105755,-21.0742356128,6.81848575139));
#87290=CARTESIAN_POINT('Origin',(4.91993843473344,-21.0742356128,6.59821410212948));
#87291=CARTESIAN_POINT('',(3.10840045127,-21.0742356128,5.33181785593));
#87292=CARTESIAN_POINT('',(3.91233575441,-21.0742356128,6.07515180366));
#87293=CARTESIAN_POINT('Ctrl Pts',(3.31206782846,-20.7742356128,5.11154620667));
#87294=CARTESIAN_POINT('Ctrl Pts',(3.30444954029279,-20.7742356127999,5.1197855865974));
#87295=CARTESIAN_POINT('Ctrl Pts',(3.2973316880372,-20.7748629748481,5.12745413063611));
#87296=CARTESIAN_POINT('Ctrl Pts',(3.29076617355475,-20.7758767399775,5.13452932895326));
#87297=CARTESIAN_POINT('Ctrl Pts',(3.28578446329595,-20.7766459537473,5.13989777161435));
#87298=CARTESIAN_POINT('Ctrl Pts',(3.28111988686524,-20.7776380915859,5.14492554135016));
#87299=CARTESIAN_POINT('Ctrl Pts',(3.27678437271589,-20.7787599076263,5.14961442549687));
#87300=CARTESIAN_POINT('Ctrl Pts',(3.27175967701396,-20.7800600496722,5.15504866356119));
#87301=CARTESIAN_POINT('Ctrl Pts',(3.26717209828427,-20.781533969113,5.16002543626601));
#87302=CARTESIAN_POINT('Ctrl Pts',(3.26300921844094,-20.7830586640124,5.16454845869607));
#87303=CARTESIAN_POINT('Ctrl Pts',(3.26120731138153,-20.7837186298548,5.16650625386511));
#87304=CARTESIAN_POINT('Ctrl Pts',(3.25974366013668,-20.784288939405,5.16809834768708));
#87305=CARTESIAN_POINT('Ctrl Pts',(3.25827854408097,-20.7848814548452,5.16969158096989));
#87306=CARTESIAN_POINT('Ctrl Pts',(3.25686452541498,-20.7854533057161,5.17122924864638));
#87307=CARTESIAN_POINT('Ctrl Pts',(3.25544907274139,-20.7860461299659,5.17276805295182));
#87308=CARTESIAN_POINT('Ctrl Pts',(3.25373460238829,-20.7868025675846,5.17462932065643));
#87309=CARTESIAN_POINT('Ctrl Pts',(3.25312148822844,-20.7870730783078,5.17529493122409));
#87310=CARTESIAN_POINT('Ctrl Pts',(3.25247021809243,-20.7873649214208,5.17600168928286));
#87311=CARTESIAN_POINT('Ctrl Pts',(3.25176754480936,-20.7876862654106,5.17676389831576));
#87312=CARTESIAN_POINT('Ctrl Pts',(3.24593338674452,-20.7903543213548,5.18309237000166));
#87313=CARTESIAN_POINT('Ctrl Pts',(3.24018276622,-20.793407990483,5.18930426249853));
#87314=CARTESIAN_POINT('Ctrl Pts',(3.23463241100123,-20.7967643371934,5.19529253398549));
#87315=CARTESIAN_POINT('Ctrl Pts',(3.22898905056823,-20.800176924943,5.20138114868485));
#87316=CARTESIAN_POINT('Ctrl Pts',(3.22355313365751,-20.8039018958713,5.20723814141231));
#87317=CARTESIAN_POINT('Ctrl Pts',(3.21842848080822,-20.8078052624877,5.21277141141798));
#87318=CARTESIAN_POINT('Ctrl Pts',(3.21304718125325,-20.8119041128203,5.21858179200272));
#87319=CARTESIAN_POINT('Ctrl Pts',(3.20800942685562,-20.8161989110882,5.22403486325186));
#87320=CARTESIAN_POINT('Ctrl Pts',(3.20340861986728,-20.8204929579054,5.22905297895093));
#87321=CARTESIAN_POINT('Ctrl Pts',(3.20280377184362,-20.8210574775076,5.22971268873028));
#87322=CARTESIAN_POINT('Ctrl Pts',(3.20220643643071,-20.8216219388458,5.23036492352408));
#87323=CARTESIAN_POINT('Ctrl Pts',(3.20161679072966,-20.822185857569,5.23100954489473));
#87324=CARTESIAN_POINT('Ctrl Pts',(3.19343867455265,-20.83000715233,5.23995014846391));
#87325=CARTESIAN_POINT('Ctrl Pts',(3.18586912350675,-20.8384449654876,5.24814241044823));
#87326=CARTESIAN_POINT('Ctrl Pts',(3.1789329133062,-20.8472632641887,5.25562483465526));
#87327=CARTESIAN_POINT('Ctrl Pts',(3.1743793788751,-20.8530523659601,5.260536951686));
#87328=CARTESIAN_POINT('Ctrl Pts',(3.17009808891465,-20.8590060228511,5.26514391381523));
#87329=CARTESIAN_POINT('Ctrl Pts',(3.16608953990945,-20.8650648258508,5.26946365924601));
#87330=CARTESIAN_POINT('Ctrl Pts',(3.16283874769359,-20.8699783019249,5.27296682081462));
#87331=CARTESIAN_POINT('Ctrl Pts',(3.15985829370293,-20.8748159171735,5.2761818264669));
#87332=CARTESIAN_POINT('Ctrl Pts',(3.15704171944077,-20.8796807375898,5.27922240091002));
#87333=CARTESIAN_POINT('Ctrl Pts',(3.15406822274213,-20.8848165962964,5.28243237772125));
#87334=CARTESIAN_POINT('Ctrl Pts',(3.15127701135179,-20.8899831652855,5.285448338928));
#87335=CARTESIAN_POINT('Ctrl Pts',(3.14857270050314,-20.8953444206099,5.28837178313741));
#87336=CARTESIAN_POINT('Ctrl Pts',(3.14600766127337,-20.9004295720579,5.29114467039145));
#87337=CARTESIAN_POINT('Ctrl Pts',(3.1435207243353,-20.9056904954052,5.29383440885434));
#87338=CARTESIAN_POINT('Ctrl Pts',(3.14105900613626,-20.9112961454075,5.29649677480764));
#87339=CARTESIAN_POINT('Ctrl Pts',(3.14092534444609,-20.9116005103238,5.29664133088773));
#87340=CARTESIAN_POINT('Ctrl Pts',(3.14079176474627,-20.9119058977849,5.29678579800486));
#87341=CARTESIAN_POINT('Ctrl Pts',(3.14065826128172,-20.9122123369602,5.29693018215617));
#87342=CARTESIAN_POINT('Ctrl Pts',(3.13742614659444,-20.9196312197803,5.30042571792873));
#87343=CARTESIAN_POINT('Ctrl Pts',(3.13478487531432,-20.9266420183846,5.30348849201042));
#87344=CARTESIAN_POINT('Ctrl Pts',(3.13253832728671,-20.9331835477761,5.30615752340709));
#87345=CARTESIAN_POINT('Ctrl Pts',(3.13015585898119,-20.9401208516989,5.30898803610073));
#87346=CARTESIAN_POINT('Ctrl Pts',(3.12821700234919,-20.9465310459643,5.31137606597068));
#87347=CARTESIAN_POINT('Ctrl Pts',(3.12651001133026,-20.952389618554,5.31334417593453));
#87348=CARTESIAN_POINT('Ctrl Pts',(3.12602179849174,-20.9540652163293,5.31390707084219));
#87349=CARTESIAN_POINT('Ctrl Pts',(3.12555269902518,-20.9556959443761,5.31443545748816));
#87350=CARTESIAN_POINT('Ctrl Pts',(3.12509810909517,-20.9572817858397,5.31492948511653));
#87351=CARTESIAN_POINT('Ctrl Pts',(3.12366652371443,-20.9622758855889,5.31648526689644));
#87352=CARTESIAN_POINT('Ctrl Pts',(3.12229520001995,-20.9671617422919,5.31782333881145));
#87353=CARTESIAN_POINT('Ctrl Pts',(3.12097486219589,-20.9721576961734,5.31906465725106));
#87354=CARTESIAN_POINT('Ctrl Pts',(3.11969224644078,-20.9770109155871,5.32027051120657));
#87355=CARTESIAN_POINT('Ctrl Pts',(3.11845767571797,-20.9819684491287,5.32138513596453));
#87356=CARTESIAN_POINT('Ctrl Pts',(3.11729333615592,-20.9872457021546,5.32248622269787));
#87357=CARTESIAN_POINT('Ctrl Pts',(3.11669009887985,-20.9899798149892,5.32305668906645));
#87358=CARTESIAN_POINT('Ctrl Pts',(3.11610622112494,-20.992799963711,5.32362297214742));
#87359=CARTESIAN_POINT('Ctrl Pts',(3.11554850316912,-20.99573729042,5.32419185848304));
#87360=CARTESIAN_POINT('Ctrl Pts',(3.11424881632856,-21.0025823360749,5.32551757173375));
#87361=CARTESIAN_POINT('Ctrl Pts',(3.11320374618487,-21.0090749065193,5.32659990756699));
#87362=CARTESIAN_POINT('Ctrl Pts',(3.11233787825752,-21.015348475393,5.32750975261846));
#87363=CARTESIAN_POINT('Ctrl Pts',(3.11142278559847,-21.0219786976718,5.32847132250826));
#87364=CARTESIAN_POINT('Ctrl Pts',(3.11070786593494,-21.0283649245797,5.3292402142949));
#87365=CARTESIAN_POINT('Ctrl Pts',(3.11014076856595,-21.0346836372789,5.32986044423484));
#87366=CARTESIAN_POINT('Ctrl Pts',(3.10956040449569,-21.0411501702262,5.33049518386179));
#87367=CARTESIAN_POINT('Ctrl Pts',(3.10913483212844,-21.0475465887847,5.3309742547607));
#87368=CARTESIAN_POINT('Ctrl Pts',(3.10884490269887,-21.0540718430784,5.33130485910088));
#87369=CARTESIAN_POINT('Ctrl Pts',(3.1085549732693,-21.0605970973721,5.33163546344106));
#87370=CARTESIAN_POINT('Ctrl Pts',(3.10840045126752,-21.0672518011227,5.33181785593268));
#87371=CARTESIAN_POINT('Ctrl Pts',(3.10840045126752,-21.0742356128,5.33181785593268));
#87372=CARTESIAN_POINT('Origin',(2.31985562646,-21.0742356128,7.05423263334));
#87373=CARTESIAN_POINT('',(1.2614400074,-20.7742356128,6.07560132137));
#87374=CARTESIAN_POINT('',(2.33982641743,-20.7742356128,7.0726980084));
#87375=CARTESIAN_POINT('',(1.46510738459,-21.0742356128,5.8553296721));
#87376=CARTESIAN_POINT('Ctrl Pts',(1.46510738458927,-21.0742356128,5.85532967210079));
#87377=CARTESIAN_POINT('Ctrl Pts',(1.46510738458927,-21.0568525598039,5.85532967210079));
#87378=CARTESIAN_POINT('Ctrl Pts',(1.46407993726464,-21.0394747640594,5.85643142737418));
#87379=CARTESIAN_POINT('Ctrl Pts',(1.46201327225789,-21.0222270827341,5.85865552532541));
#87380=CARTESIAN_POINT('Ctrl Pts',(1.46007045121047,-21.0060129608573,5.86074634521981));
#87381=CARTESIAN_POINT('Ctrl Pts',(1.45720859993379,-20.9899122151244,5.86382970774848));
#87382=CARTESIAN_POINT('Ctrl Pts',(1.45339155089049,-20.9740554909872,5.86795125690417));
#87383=CARTESIAN_POINT('Ctrl Pts',(1.45314823539463,-20.9730447136427,5.86821398257658));
#87384=CARTESIAN_POINT('Ctrl Pts',(1.45290103120873,-20.9720349420427,5.86848093475406));
#87385=CARTESIAN_POINT('Ctrl Pts',(1.45264992608831,-20.9710262162607,5.86875212837015));
#87386=CARTESIAN_POINT('Ctrl Pts',(1.44881627744658,-20.9556258922154,5.87289247021678));
#87387=CARTESIAN_POINT('Ctrl Pts',(1.44407550231965,-20.9404672608799,5.87802193854843));
#87388=CARTESIAN_POINT('Ctrl Pts',(1.43838489826456,-20.9257392878566,5.88418724678318));
#87389=CARTESIAN_POINT('Ctrl Pts',(1.43785540916636,-20.9243689058939,5.88476090530268));
#87390=CARTESIAN_POINT('Ctrl Pts',(1.43731769652213,-20.9230022902451,5.88534353204184));
#87391=CARTESIAN_POINT('Ctrl Pts',(1.43677172643757,-20.9216396173414,5.88593516408484));
#87392=CARTESIAN_POINT('Ctrl Pts',(1.43434334506759,-20.9155786817951,5.88856664202062));
#87393=CARTESIAN_POINT('Ctrl Pts',(1.43169370618827,-20.9094594010707,5.89143919340066));
#87394=CARTESIAN_POINT('Ctrl Pts',(1.42887798388927,-20.9034620318311,5.89449111102838));
#87395=CARTESIAN_POINT('Ctrl Pts',(1.42605752021122,-20.897454563655,5.89754816776313));
#87396=CARTESIAN_POINT('Ctrl Pts',(1.42307059144137,-20.89157000063,5.90078500266657));
#87397=CARTESIAN_POINT('Ctrl Pts',(1.42000271460379,-20.8859602994751,5.90410708155958));
#87398=CARTESIAN_POINT('Ctrl Pts',(1.41804423247998,-20.8823791585058,5.90622784209538));
#87399=CARTESIAN_POINT('Ctrl Pts',(1.41605337921587,-20.8789093883557,5.90838267412748));
#87400=CARTESIAN_POINT('Ctrl Pts',(1.41405795094043,-20.8755830313655,5.91054098330808));
#87401=CARTESIAN_POINT('Ctrl Pts',(1.4084018122684,-20.8661543104036,5.91665881584196));
#87402=CARTESIAN_POINT('Ctrl Pts',(1.40212266410665,-20.8568965367214,5.92343229913557));
#87403=CARTESIAN_POINT('Ctrl Pts',(1.39518571116258,-20.848004932525,5.93092317372076));
#87404=CARTESIAN_POINT('Ctrl Pts',(1.39201468675336,-20.8439403966731,5.93434740714826));
#87405=CARTESIAN_POINT('Ctrl Pts',(1.38870645133448,-20.8399529582422,5.93792128289567));
#87406=CARTESIAN_POINT('Ctrl Pts',(1.38525918280401,-20.8360642290584,5.94164907444906));
#87407=CARTESIAN_POINT('Ctrl Pts',(1.37976491537811,-20.8298663602549,5.94759044035116));
#87408=CARTESIAN_POINT('Ctrl Pts',(1.37391644984959,-20.8239192141413,5.95392220208472));
#87409=CARTESIAN_POINT('Ctrl Pts',(1.36770932510617,-20.8183217629177,5.96064509578293));
#87410=CARTESIAN_POINT('Ctrl Pts',(1.36460576273446,-20.8155230373059,5.96400654263203));
#87411=CARTESIAN_POINT('Ctrl Pts',(1.36141262995974,-20.8128119253493,5.96746550388978));
#87412=CARTESIAN_POINT('Ctrl Pts',(1.35813001664382,-20.8102018162985,5.97102026930888));
#87413=CARTESIAN_POINT('Ctrl Pts',(1.35668689185399,-20.8090543424072,5.97258303945712));
#87414=CARTESIAN_POINT('Ctrl Pts',(1.35499698359374,-20.8077487870536,5.97441253609893));
#87415=CARTESIAN_POINT('Ctrl Pts',(1.3533601637152,-20.806528824505,5.97618421836793));
#87416=CARTESIAN_POINT('Ctrl Pts',(1.35154453585483,-20.8051755919222,5.97814944113282));
#87417=CARTESIAN_POINT('Ctrl Pts',(1.34979443131247,-20.8039277560863,5.98004330913371));
#87418=CARTESIAN_POINT('Ctrl Pts',(1.34854061399836,-20.8030538894474,5.98139963746283));
#87419=CARTESIAN_POINT('Ctrl Pts',(1.34835363857244,-20.8029235741413,5.98160189983724));
#87420=CARTESIAN_POINT('Ctrl Pts',(1.34817772561819,-20.8028014882097,5.98179218024529));
#87421=CARTESIAN_POINT('Ctrl Pts',(1.34801432321358,-20.8026884535921,5.98196891154972));
#87422=CARTESIAN_POINT('Ctrl Pts',(1.34352037500665,-20.7995797373015,5.9868294356682));
#87423=CARTESIAN_POINT('Ctrl Pts',(1.338386211841,-20.7963192960567,5.99238226897694));
#87424=CARTESIAN_POINT('Ctrl Pts',(1.33256949718929,-20.7931259090584,5.99867323712446));
#87425=CARTESIAN_POINT('Ctrl Pts',(1.32726165318095,-20.7902118929754,6.00441384493968));
#87426=CARTESIAN_POINT('Ctrl Pts',(1.32138489117724,-20.7873543342918,6.01076970044963));
#87427=CARTESIAN_POINT('Ctrl Pts',(1.31492003594937,-20.7847629028735,6.0177615707223));
#87428=CARTESIAN_POINT('Ctrl Pts',(1.30867724066184,-20.7822604839831,6.02451327872669));
#87429=CARTESIAN_POINT('Ctrl Pts',(1.3018854602463,-20.780006593215,6.03185870664777));
#87430=CARTESIAN_POINT('Ctrl Pts',(1.29454848205839,-20.7782260704221,6.03979378406956));
#87431=CARTESIAN_POINT('Ctrl Pts',(1.28757944370676,-20.7765348385128,6.04733092776269));
#87432=CARTESIAN_POINT('Ctrl Pts',(1.28011810284529,-20.7752712828586,6.05540051297026));
#87433=CARTESIAN_POINT('Ctrl Pts',(1.27219412867516,-20.7746541176134,6.06397047369944));
#87434=CARTESIAN_POINT('Ctrl Pts',(1.26869756731923,-20.7743817850565,6.06775208540894));
#87435=CARTESIAN_POINT('Ctrl Pts',(1.26511131777583,-20.7742356127999,6.0716307022037));
#87436=CARTESIAN_POINT('Ctrl Pts',(1.2614400074,-20.7742356128,6.07560132137));
#87437=CARTESIAN_POINT('',(2.54349379462,-21.0742356128,6.85242635913));
#87438=CARTESIAN_POINT('Origin',(0.00234331738835,-21.0742356128,3.08191746407));
#87439=CARTESIAN_POINT('',(5.48986775992,-20.7742356128,0.545353000555));
#87440=CARTESIAN_POINT('',(5.92013962829,-20.7742356128,1.84629187045));
#87441=CARTESIAN_POINT('Origin',(0.00234331738835,-20.7742356128,3.08191746407));
#87442=CARTESIAN_POINT('',(5.76218263052,-21.0742356128,0.419477620705));
#87443=CARTESIAN_POINT('Ctrl Pts',(5.76218263051847,-21.0742356128,0.419477620705708));
#87444=CARTESIAN_POINT('Ctrl Pts',(5.76218263051847,-21.0711343099908,0.419477620705708));
#87445=CARTESIAN_POINT('Ctrl Pts',(5.76212789615905,-21.0683778932532,0.419463148787726));
#87446=CARTESIAN_POINT('Ctrl Pts',(5.76202961598976,-21.0655246169381,0.419448073937373));
#87447=CARTESIAN_POINT('Ctrl Pts',(5.7619393761782,-21.0629047688154,0.419434232369283));
#87448=CARTESIAN_POINT('Ctrl Pts',(5.76181222718317,-21.0602030737192,0.419419973460183));
#87449=CARTESIAN_POINT('Ctrl Pts',(5.76162093210155,-21.0570790738875,0.419432631131333));
#87450=CARTESIAN_POINT('Ctrl Pts',(5.76147715112112,-21.0547310168705,0.419442144874982));
#87451=CARTESIAN_POINT('Ctrl Pts',(5.76129676935522,-21.052144336212,0.419467032354691));
#87452=CARTESIAN_POINT('Ctrl Pts',(5.76105046867993,-21.0491764894497,0.419527108581872));
#87453=CARTESIAN_POINT('Ctrl Pts',(5.76058502600462,-21.0435680495402,0.419640636650235));
#87454=CARTESIAN_POINT('Ctrl Pts',(5.76005667105559,-21.0380145982917,0.419983502847117));
#87455=CARTESIAN_POINT('Ctrl Pts',(5.75940097602592,-21.0324707850792,0.420422476369964));
#87456=CARTESIAN_POINT('Ctrl Pts',(5.75907312851108,-21.0296988784729,0.420641963131388));
#87457=CARTESIAN_POINT('Ctrl Pts',(5.7587133084088,-21.0269297742481,0.420885538444297));
#87458=CARTESIAN_POINT('Ctrl Pts',(5.75831217072801,-21.0241602367083,0.421135173302448));
#87459=CARTESIAN_POINT('Ctrl Pts',(5.75810699640252,-21.0227436707164,0.421262856803883));
#87460=CARTESIAN_POINT('Ctrl Pts',(5.75796930454998,-21.0218220855038,0.421353628373918));
#87461=CARTESIAN_POINT('Ctrl Pts',(5.75778181250985,-21.0206347166969,0.421461893833452));
#87462=CARTESIAN_POINT('Ctrl Pts',(5.75761225171338,-21.0195609047075,0.421559805070305));
#87463=CARTESIAN_POINT('Ctrl Pts',(5.75740301623091,-21.0182694210857,0.421671535862888));
#87464=CARTESIAN_POINT('Ctrl Pts',(5.75703739192913,-21.0162038360199,0.421851176134806));
#87465=CARTESIAN_POINT('Ctrl Pts',(5.75701687667445,-21.0160879356175,0.421861255787364));
#87466=CARTESIAN_POINT('Ctrl Pts',(5.75699585603951,-21.0159696010428,0.421871555257977));
#87467=CARTESIAN_POINT('Ctrl Pts',(5.75697430408466,-21.0158487352453,0.421882086561721));
#87468=CARTESIAN_POINT('Ctrl Pts',(5.75585610863276,-21.0095777688301,0.422428489708489));
#87469=CARTESIAN_POINT('Ctrl Pts',(5.75441381085562,-21.0027231086594,0.423037486106193));
#87470=CARTESIAN_POINT('Ctrl Pts',(5.75254933409048,-20.9952668038011,0.423852701949254));
#87471=CARTESIAN_POINT('Ctrl Pts',(5.75164469012145,-20.9916490053134,0.424248244607481));
#87472=CARTESIAN_POINT('Ctrl Pts',(5.75064012302674,-20.9878899914571,0.424692579687064));
#87473=CARTESIAN_POINT('Ctrl Pts',(5.74952131287696,-20.9839906759573,0.425203525154008));
#87474=CARTESIAN_POINT('Ctrl Pts',(5.74780897051388,-20.9780227616345,0.42598552875707));
#87475=CARTESIAN_POINT('Ctrl Pts',(5.74582812460024,-20.9717317114928,0.42691700148707));
#87476=CARTESIAN_POINT('Ctrl Pts',(5.74350992019445,-20.9651556634559,0.428019179652195));
#87477=CARTESIAN_POINT('Ctrl Pts',(5.74235081799156,-20.9618676394374,0.428570268734759));
#87478=CARTESIAN_POINT('Ctrl Pts',(5.7411071187696,-20.9585087257985,0.429163558530631));
#87479=CARTESIAN_POINT('Ctrl Pts',(5.73976875796006,-20.9550856710468,0.429798754464527));
#87480=CARTESIAN_POINT('Ctrl Pts',(5.73909957755529,-20.9533741436709,0.430116352431476));
#87481=CARTESIAN_POINT('Ctrl Pts',(5.7384067253257,-20.9516465841452,0.430444429904209));
#87482=CARTESIAN_POINT('Ctrl Pts',(5.73768884898717,-20.9499039715201,0.430782712005881));
#87483=CARTESIAN_POINT('Ctrl Pts',(5.73723620114925,-20.9488051891885,0.430996011502904));
#87484=CARTESIAN_POINT('Ctrl Pts',(5.7369582236608,-20.9481396816218,0.431127352220856));
#87485=CARTESIAN_POINT('Ctrl Pts',(5.73650730043681,-20.9470757776858,0.431338468887568));
#87486=CARTESIAN_POINT('Ctrl Pts',(5.73624308247185,-20.9464523843498,0.43146217246521));
#87487=CARTESIAN_POINT('Ctrl Pts',(5.73591920109332,-20.9456923382671,0.431613397647289));
#87488=CARTESIAN_POINT('Ctrl Pts',(5.73545877283664,-20.9446319683954,0.431827894353049));
#87489=CARTESIAN_POINT('Ctrl Pts',(5.73241146794468,-20.9376140014255,0.433247522386909));
#87490=CARTESIAN_POINT('Ctrl Pts',(5.72880348035714,-20.9300323022399,0.434890170001915));
#87491=CARTESIAN_POINT('Ctrl Pts',(5.72450075487575,-20.9219992593249,0.43685668003197));
#87492=CARTESIAN_POINT('Ctrl Pts',(5.72176499618178,-20.9168916903924,0.438107026338003));
#87493=CARTESIAN_POINT('Ctrl Pts',(5.71874800465858,-20.9116025113626,0.439488469477967));
#87494=CARTESIAN_POINT('Ctrl Pts',(5.71541312463863,-20.9061714559532,0.441027877214491));
#87495=CARTESIAN_POINT('Ctrl Pts',(5.71112318117637,-20.8991850215064,0.443008150002585));
#87496=CARTESIAN_POINT('Ctrl Pts',(5.70630577576505,-20.8919640396089,0.445245856444974));
#87497=CARTESIAN_POINT('Ctrl Pts',(5.70087617302816,-20.8846214612248,0.44777265102263));
#87498=CARTESIAN_POINT('Ctrl Pts',(5.69816137165972,-20.8809501720327,0.449036048311459));
#87499=CARTESIAN_POINT('Ctrl Pts',(5.6952934808518,-20.8772489447893,0.450371431448299));
#87500=CARTESIAN_POINT('Ctrl Pts',(5.69226197710357,-20.8735347161601,0.451780936519775));
#87501=CARTESIAN_POINT('Ctrl Pts',(5.69074622522945,-20.8716776018455,0.452485689055514));
#87502=CARTESIAN_POINT('Ctrl Pts',(5.68940323754624,-20.8700725536964,0.453110116987698));
#87503=CARTESIAN_POINT('Ctrl Pts',(5.68791548452027,-20.8683345079178,0.453800644920927));
#87504=CARTESIAN_POINT('Ctrl Pts',(5.686539273402,-20.8667267693463,0.45443940162489));
#87505=CARTESIAN_POINT('Ctrl Pts',(5.68503937868389,-20.8650047885142,0.455134631163884));
#87506=CARTESIAN_POINT('Ctrl Pts',(5.68313710135166,-20.8628930892138,0.456014882216015));
#87507=CARTESIAN_POINT('Ctrl Pts',(5.68298292177862,-20.8627219359908,0.456086226561599));
#87508=CARTESIAN_POINT('Ctrl Pts',(5.68282608050964,-20.8625482437002,0.456158794840108));
#87509=CARTESIAN_POINT('Ctrl Pts',(5.68266641862616,-20.8623718778984,0.45623266036311));
#87510=CARTESIAN_POINT('Ctrl Pts',(5.67682336636476,-20.8559175221388,0.458935873564779));
#87511=CARTESIAN_POINT('Ctrl Pts',(5.67024533328323,-20.8492424579849,0.46196525160643));
#87512=CARTESIAN_POINT('Ctrl Pts',(5.66283907998627,-20.8425348446108,0.465380025587699));
#87513=CARTESIAN_POINT('Ctrl Pts',(5.65944809206181,-20.8394637322627,0.466943495924311));
#87514=CARTESIAN_POINT('Ctrl Pts',(5.65588362700338,-20.836386463225,0.468587688276975));
#87515=CARTESIAN_POINT('Ctrl Pts',(5.65213788215834,-20.8333245964127,0.47031774081465));
#87516=CARTESIAN_POINT('Ctrl Pts',(5.64617447097158,-20.8284499529021,0.47307207008257));
#87517=CARTESIAN_POINT('Ctrl Pts',(5.63975073557742,-20.8236137372718,0.476043246403684));
#87518=CARTESIAN_POINT('Ctrl Pts',(5.63283950439035,-20.818915369188,0.479242079185539));
#87519=CARTESIAN_POINT('Ctrl Pts',(5.62938388879682,-20.8165661851461,0.480841495576468));
#87520=CARTESIAN_POINT('Ctrl Pts',(5.62580651502869,-20.8142516964488,0.482497682560015));
#87521=CARTESIAN_POINT('Ctrl Pts',(5.622104846316,-20.8119857073957,0.484211032033263));
#87522=CARTESIAN_POINT('Ctrl Pts',(5.62014404904501,-20.8107853986982,0.485118604058787));
#87523=CARTESIAN_POINT('Ctrl Pts',(5.61787341347036,-20.8094357628297,0.486169352333183));
#87524=CARTESIAN_POINT('Ctrl Pts',(5.61572711915748,-20.8082031531422,0.48716234631413));
#87525=CARTESIAN_POINT('Ctrl Pts',(5.6138215562877,-20.8071087947219,0.488043964668452));
#87526=CARTESIAN_POINT('Ctrl Pts',(5.61201474620417,-20.8061054212397,0.48887971586325));
#87527=CARTESIAN_POINT('Ctrl Pts',(5.61062513049926,-20.805347934196,0.489522239721216));
#87528=CARTESIAN_POINT('Ctrl Pts',(5.60528025572931,-20.8024344140232,0.491993577333035));
#87529=CARTESIAN_POINT('Ctrl Pts',(5.59914555171968,-20.7993271570843,0.494830284396293));
#87530=CARTESIAN_POINT('Ctrl Pts',(5.5921663409056,-20.7962101943979,0.49805747101858));
#87531=CARTESIAN_POINT('Ctrl Pts',(5.58552594074091,-20.7932445468357,0.501127991618825));
#87532=CARTESIAN_POINT('Ctrl Pts',(5.57812019278002,-20.7902703605307,0.504552390383305));
#87533=CARTESIAN_POINT('Ctrl Pts',(5.56991509591193,-20.7874902135388,0.508346244034247));
#87534=CARTESIAN_POINT('Ctrl Pts',(5.56198690494279,-20.7848038910458,0.512012062578159));
#87535=CARTESIAN_POINT('Ctrl Pts',(5.55331157924344,-20.7822990373231,0.516023202866985));
#87536=CARTESIAN_POINT('Ctrl Pts',(5.54388302057105,-20.7801968080192,0.520382359688187));
#87537=CARTESIAN_POINT('Ctrl Pts',(5.53496122955905,-20.7782075696679,0.524507219860206));
#87538=CARTESIAN_POINT('Ctrl Pts',(5.52536442562282,-20.7765793991742,0.528943956612456));
#87539=CARTESIAN_POINT('Ctrl Pts',(5.51511959478089,-20.7755282547698,0.533679993439904));
#87540=CARTESIAN_POINT('Ctrl Pts',(5.50708945068104,-20.7747043425776,0.537392212682312));
#87541=CARTESIAN_POINT('Ctrl Pts',(5.49866164782896,-20.7742356127999,0.541288095915715));
#87542=CARTESIAN_POINT('Ctrl Pts',(5.48986775992,-20.7742356128,0.545353000555));
#87543=CARTESIAN_POINT('',(6.21380646358,-21.0742356128,1.78497474518));
#87544=CARTESIAN_POINT('Origin',(0.00234331738835,-21.0742356128,3.08191746407));
#87545=CARTESIAN_POINT('Origin',(5.92013962829301,-21.0742356128,1.84629187044622));
#87546=CARTESIAN_POINT('Origin',(5.48986775992,-21.0742356128,0.545353000555));
#87547=CARTESIAN_POINT('',(5.1900363009,-21.0742356128,0.55540766038));
#87548=CARTESIAN_POINT('Origin',(5.48986775992,-21.0742356128,0.545353000555));
#87549=CARTESIAN_POINT('Origin',(5.48986775992,-21.0742356128,0.545353000555));
#87550=CARTESIAN_POINT('Origin',(-9.64069499267E-16,-21.0742356128,0.729452270839));
#87551=CARTESIAN_POINT('',(5.08448267152,-21.0742356128,1.78529520144));
#87552=CARTESIAN_POINT('Origin',(2.57175827821E-16,-21.0742356128,0.729452270839));
#87553=CARTESIAN_POINT('',(5.3782162351,-20.7742356128,1.84629187045));
#87554=CARTESIAN_POINT('Origin',(4.75197961991E-16,-20.7742356128,0.729452270839));
#87555=CARTESIAN_POINT('Ctrl Pts',(5.08448267152151,-21.0742356128,1.78529520144031));
#87556=CARTESIAN_POINT('Ctrl Pts',(5.08448267152151,-21.0645012808632,1.78529520144031));
#87557=CARTESIAN_POINT('Ctrl Pts',(5.08493635413104,-21.0548222582473,1.78541942341338));
#87558=CARTESIAN_POINT('Ctrl Pts',(5.08585408050998,-21.0451000686285,1.78566598382418));
#87559=CARTESIAN_POINT('Ctrl Pts',(5.0861237656047,-21.0422430845769,1.78573843860947));
#87560=CARTESIAN_POINT('Ctrl Pts',(5.08643385657685,-21.0393824001939,1.78582152773478));
#87561=CARTESIAN_POINT('Ctrl Pts',(5.08678544912873,-21.0365156373058,1.7859153777379));
#87562=CARTESIAN_POINT('Ctrl Pts',(5.087358954137,-21.0318394777425,1.78606846245636));
#87563=CARTESIAN_POINT('Ctrl Pts',(5.08800922997164,-21.0273865922814,1.78624165419594));
#87564=CARTESIAN_POINT('Ctrl Pts',(5.0887681237863,-21.0228804144151,1.78643788818155));
#87565=CARTESIAN_POINT('Ctrl Pts',(5.08949382756653,-21.01857131313,1.78662553992205));
#87566=CARTESIAN_POINT('Ctrl Pts',(5.09031904028443,-21.0142131582222,1.78683430063852));
#87567=CARTESIAN_POINT('Ctrl Pts',(5.09131507023229,-21.0095725885318,1.78707576275223));
#87568=CARTESIAN_POINT('Ctrl Pts',(5.09208897432893,-21.0059669179375,1.78726337610601));
#87569=CARTESIAN_POINT('Ctrl Pts',(5.09296663835046,-21.0021907778178,1.78747086375398));
#87570=CARTESIAN_POINT('Ctrl Pts',(5.09400200555433,-20.9981410352675,1.7877079192303));
#87571=CARTESIAN_POINT('Ctrl Pts',(5.09735848797456,-20.9850124663638,1.78847641231749));
#87572=CARTESIAN_POINT('Ctrl Pts',(5.10160218254057,-20.9721584640941,1.78927961768519));
#87573=CARTESIAN_POINT('Ctrl Pts',(5.106717486722,-20.9595797111132,1.79023334935614));
#87574=CARTESIAN_POINT('Ctrl Pts',(5.10733456447915,-20.9580622903691,1.79034840147808));
#87575=CARTESIAN_POINT('Ctrl Pts',(5.10796438229745,-20.9565488997241,1.79046565666436));
#87576=CARTESIAN_POINT('Ctrl Pts',(5.10860695783828,-20.9550395633781,1.79058532849954));
#87577=CARTESIAN_POINT('Ctrl Pts',(5.1115915804258,-20.9480290267735,1.79114117795172));
#87578=CARTESIAN_POINT('Ctrl Pts',(5.11485094784533,-20.9411066703631,1.79174864351049));
#87579=CARTESIAN_POINT('Ctrl Pts',(5.11838596254678,-20.9342820340361,1.79242876609553));
#87580=CARTESIAN_POINT('Ctrl Pts',(5.11997031565205,-20.9312233101919,1.79273358924921));
#87581=CARTESIAN_POINT('Ctrl Pts',(5.12147401393412,-20.9284382834278,1.79302477068904));
#87582=CARTESIAN_POINT('Ctrl Pts',(5.12307240443405,-20.9255823146597,1.7933407263901));
#87583=CARTESIAN_POINT('Ctrl Pts',(5.12458936757298,-20.922871838498,1.79364058625043));
#87584=CARTESIAN_POINT('Ctrl Pts',(5.12619170434029,-20.9200972224439,1.79396277721054));
#87585=CARTESIAN_POINT('Ctrl Pts',(5.12806711119576,-20.9169866084276,1.79434799265438));
#87586=CARTESIAN_POINT('Ctrl Pts',(5.128624655078,-20.9160618470566,1.7944625142119));
#87587=CARTESIAN_POINT('Ctrl Pts',(5.12920660615708,-20.9151075694506,1.79458266270214));
#87588=CARTESIAN_POINT('Ctrl Pts',(5.12981865714652,-20.9141171584819,1.79470966561171));
#87589=CARTESIAN_POINT('Ctrl Pts',(5.13571048973975,-20.9045830906885,1.79593224329713));
#87590=CARTESIAN_POINT('Ctrl Pts',(5.14237609352167,-20.8949759521074,1.79734044684605));
#87591=CARTESIAN_POINT('Ctrl Pts',(5.14994010475542,-20.8854315566452,1.79893114249031));
#87592=CARTESIAN_POINT('Ctrl Pts',(5.15480356908058,-20.8792947562887,1.79995391880291));
#87593=CARTESIAN_POINT('Ctrl Pts',(5.16003847376736,-20.8731848198683,1.80105213969165));
#87594=CARTESIAN_POINT('Ctrl Pts',(5.16567611424345,-20.8671492374168,1.80222448041741));
#87595=CARTESIAN_POINT('Ctrl Pts',(5.1728789674508,-20.8594379591608,1.80372230529511));
#87596=CARTESIAN_POINT('Ctrl Pts',(5.18073771166217,-20.8518495686742,1.80534366782332));
#87597=CARTESIAN_POINT('Ctrl Pts',(5.18929178411293,-20.8445144710433,1.80710321495179));
#87598=CARTESIAN_POINT('Ctrl Pts',(5.19356882033831,-20.8408469222279,1.80798298851602));
#87599=CARTESIAN_POINT('Ctrl Pts',(5.19801929010056,-20.8372431454817,1.80889750837796));
#87600=CARTESIAN_POINT('Ctrl Pts',(5.2026453324478,-20.8337219160368,1.80984986035332));
#87601=CARTESIAN_POINT('Ctrl Pts',(5.20482458890421,-20.8320631197211,1.81029849852723));
#87602=CARTESIAN_POINT('Ctrl Pts',(5.20729377052198,-20.8302368573979,1.81080756543739));
#87603=CARTESIAN_POINT('Ctrl Pts',(5.20970255987384,-20.8285141256464,1.81130484348002));
#87604=CARTESIAN_POINT('Ctrl Pts',(5.21226982625804,-20.8266780533841,1.81183483801917));
#87605=CARTESIAN_POINT('Ctrl Pts',(5.21476811176166,-20.8249595464615,1.81235136263844));
#87606=CARTESIAN_POINT('Ctrl Pts',(5.21673873283519,-20.8236350991637,1.81275981371049));
#87607=CARTESIAN_POINT('Ctrl Pts',(5.21684407011857,-20.8235643023564,1.81278164699285));
#87608=CARTESIAN_POINT('Ctrl Pts',(5.2169478937756,-20.8234946216469,1.81280317024565));
#87609=CARTESIAN_POINT('Ctrl Pts',(5.21705013203445,-20.823426096337,1.81282436866361));
#87610=CARTESIAN_POINT('Ctrl Pts',(5.22311200407881,-20.8193631196666,1.81408125721617));
#87611=CARTESIAN_POINT('Ctrl Pts',(5.2299956639905,-20.815073378029,1.81550954592068));
#87612=CARTESIAN_POINT('Ctrl Pts',(5.23778079317007,-20.8107451705707,1.81712556253911));
#87613=CARTESIAN_POINT('Ctrl Pts',(5.2456193267744,-20.8063872724772,1.81875266470743));
#87614=CARTESIAN_POINT('Ctrl Pts',(5.25437302208229,-20.8019900893308,1.82057034556678));
#87615=CARTESIAN_POINT('Ctrl Pts',(5.26410524797891,-20.7977994050181,1.82259154001717));
#87616=CARTESIAN_POINT('Ctrl Pts',(5.27286540995792,-20.7940272902139,1.82441085565623));
#87617=CARTESIAN_POINT('Ctrl Pts',(5.28241898978949,-20.7904232329663,1.82639518524843));
#87618=CARTESIAN_POINT('Ctrl Pts',(5.29278538050293,-20.7872047120146,1.82854839034495));
#87619=CARTESIAN_POINT('Ctrl Pts',(5.30279387491744,-20.7840973094615,1.83062725672936));
#87620=CARTESIAN_POINT('Ctrl Pts',(5.31356076205147,-20.7813497253196,1.83286369230111));
#87621=CARTESIAN_POINT('Ctrl Pts',(5.32506738039261,-20.7791875533763,1.83525366970004));
#87622=CARTESIAN_POINT('Ctrl Pts',(5.33601843901391,-20.7771297748877,1.83752825479734));
#87623=CARTESIAN_POINT('Ctrl Pts',(5.34763998791755,-20.7756028672462,1.83994200986043));
#87624=CARTESIAN_POINT('Ctrl Pts',(5.35987426374726,-20.7748210789055,1.84248280497264));
#87625=CARTESIAN_POINT('Ctrl Pts',(5.36584662389524,-20.7744394362488,1.84372313531042));
#87626=CARTESIAN_POINT('Ctrl Pts',(5.37196431144922,-20.7742356127999,1.84499359689556));
#87627=CARTESIAN_POINT('Ctrl Pts',(5.3782162351,-20.7742356128,1.84629187045));
#87628=CARTESIAN_POINT('Origin',(5.92013962829,-21.0742356128,1.84629187045));
#87629=CARTESIAN_POINT('',(5.92013962829,-21.0742356128,2.14629187045));
#87630=CARTESIAN_POINT('Origin',(5.92013962829,-21.0742356128,1.84629187045));
#87631=CARTESIAN_POINT('Origin',(5.92013962829,-21.0742356128,1.84629187045));
#87632=CARTESIAN_POINT('Origin',(5.3782162351,-21.0742356128,1.84629187045));
#87633=CARTESIAN_POINT('',(5.3782162351,-21.0742356128,2.14629187045));
#87634=CARTESIAN_POINT('Origin',(5.3782162351,-21.0742356128,1.84629187045));
#87635=CARTESIAN_POINT('Origin',(5.3782162351,-21.0742356128,1.84629187045));
#87636=CARTESIAN_POINT('Origin',(3.31206782846,-21.0742356128,5.11154620667));
#87637=CARTESIAN_POINT('',(3.13117783752,-21.0742356128,4.87221628548));
#87638=CARTESIAN_POINT('Origin',(3.31206782846,-21.0742356128,5.11154620667));
#87639=CARTESIAN_POINT('Origin',(3.31206782846,-21.0742356128,5.11154620667));
#87640=CARTESIAN_POINT('Origin',(-5.60029074364,-21.0742356128,1.84629187045));
#87641=CARTESIAN_POINT('',(5.6491779317,-21.0742356128,2.14629187045));
#87642=CARTESIAN_POINT('',(5.6491779317,-20.7742356128,1.84629187045));
#87643=CARTESIAN_POINT('Origin',(-9.64069499267E-16,-21.0742356128,0.729452270839));
#87644=CARTESIAN_POINT('',(4.452469377,-20.7742356128,3.94629187045));
#87645=CARTESIAN_POINT('Origin',(4.75197961991E-16,-20.7742356128,0.729452270839));
#87646=CARTESIAN_POINT('',(4.2092958712,-21.0742356128,3.77060280966));
#87647=CARTESIAN_POINT('Origin',(2.57175827821E-16,-21.0742356128,0.729452270839));
#87648=CARTESIAN_POINT('Origin',(4.45246937699693,-21.0742356128,3.94629187044695));
#87649=CARTESIAN_POINT('Origin',(1.05,-22.8742356128,-4.99584562937));
#87650=CARTESIAN_POINT('',(1.01141425905,-22.8742356128,-4.69833741));
#87651=CARTESIAN_POINT('Origin',(1.05,-22.8742356128,-4.99584562937));
#87652=CARTESIAN_POINT('',(0.972828518105,-23.1742356128,-4.40082919062));
#87653=CARTESIAN_POINT('Origin',(0.972828518105,-22.8742356128,-4.40082919062));
#87654=CARTESIAN_POINT('Origin',(1.05,-23.1742356128,-4.99584562937));
#87655=CARTESIAN_POINT('Origin',(0.00234331738835,-22.8742356128,3.08191746407));
#87656=CARTESIAN_POINT('',(4.40684492179,-22.8742356128,-3.41045927235));
#87657=CARTESIAN_POINT('Origin',(0.00234331738835,-22.8742356128,3.08191746407));
#87658=CARTESIAN_POINT('',(4.23842172091,-23.1742356128,-3.16219806837));
#87659=CARTESIAN_POINT('Origin',(4.23842172091,-22.8742356128,-3.16219806837));
#87660=CARTESIAN_POINT('Origin',(0.00234331738835,-23.1742356128,3.08191746407));
#87661=CARTESIAN_POINT('Origin',(6.34552156645,-22.8742356128,-5.5301356238));
#87662=CARTESIAN_POINT('',(6.56346233154,-22.8742356128,-5.32397592135));
#87663=CARTESIAN_POINT('Origin',(6.34552156645,-22.8742356128,-5.5301356238));
#87664=CARTESIAN_POINT('',(6.78140309663,-23.1742356128,-5.11781621891));
#87665=CARTESIAN_POINT('Origin',(6.34552156645,-23.1742356128,-5.5301356238));
#87666=CARTESIAN_POINT('Origin',(6.78140309663,-22.8742356128,-5.11781621891));
#87667=CARTESIAN_POINT('Origin',(4.57526812267,-22.8742356128,-3.65872047634));
#87668=CARTESIAN_POINT('',(4.79320888776,-22.8742356128,-3.4525607739));
#87669=CARTESIAN_POINT('Origin',(4.57526812267,-22.8742356128,-3.65872047634));
#87670=CARTESIAN_POINT('',(5.01114965285,-23.1742356128,-3.24640107146));
#87671=CARTESIAN_POINT('Origin',(5.01114965285,-22.8742356128,-3.24640107146));
#87672=CARTESIAN_POINT('Origin',(4.57526812267,-23.1742356128,-3.65872047634));
#87673=CARTESIAN_POINT('Origin',(1.2614400074,-21.0742356128,6.07560132137));
#87674=CARTESIAN_POINT('',(1.19254592572,-21.0742356128,5.78361912069));
#87675=CARTESIAN_POINT('Origin',(1.2614400074,-21.0742356128,6.07560132137));
#87676=CARTESIAN_POINT('Origin',(1.2614400074,-21.0742356128,6.07560132137));
#87677=CARTESIAN_POINT('Origin',(-2.84607155346,-21.3642356128,5.53854202767));
#87678=CARTESIAN_POINT('',(0.24693418390444,-21.0742356128,-6.59919549800697));
#87679=CARTESIAN_POINT('',(0.530881034116209,-21.0742356128,-6.5232798892238));
#87680=CARTESIAN_POINT('Origin',(-2.84607155346,-21.0742356128,5.53854202767));
#87681=CARTESIAN_POINT('',(0.530881036642,-22.1242356128,-6.52327988851));
#87682=CARTESIAN_POINT('',(0.246934184763,-21.9742356128,-6.59919549778));
#87683=CARTESIAN_POINT('Origin',(0.45,-22.8742356128,-6.23438845923));
#87684=CARTESIAN_POINT('Origin',(0.45,-22.8742356128,-6.23438845923));
#87685=CARTESIAN_POINT('Origin',(-2.84607155346,-21.0742356128,5.53854202767));
#87686=CARTESIAN_POINT('',(-2.57204347673E-14,-20.7742356128,-6.9673210071));
#87687=CARTESIAN_POINT('',(1.05,-20.7742356128,-6.68100624476));
#87688=CARTESIAN_POINT('Origin',(-2.84607155346,-20.7742356128,5.53854202767));
#87689=CARTESIAN_POINT('Ctrl Pts',(1.05,-20.7742356128,-6.68100624476));
#87690=CARTESIAN_POINT('Ctrl Pts',(1.006378088465,-20.774235612803,-6.66794906990942));
#87691=CARTESIAN_POINT('Ctrl Pts',(0.971270142094555,-20.7774178420795,
-6.65723073068667));
#87692=CARTESIAN_POINT('Ctrl Pts',(0.931206866676575,-20.7823657860325,
-6.64516796906486));
#87693=CARTESIAN_POINT('Ctrl Pts',(0.919947591790132,-20.7840670881655,
-6.6417964225193));
#87694=CARTESIAN_POINT('Ctrl Pts',(0.906163283936589,-20.7863320840288,
-6.63767504469205));
#87695=CARTESIAN_POINT('Ctrl Pts',(0.900047303757202,-20.7873950394116,
-6.6358478896007));
#87696=CARTESIAN_POINT('Ctrl Pts',(0.894263030875596,-20.7884563412427,
-6.63411460040872));
#87697=CARTESIAN_POINT('Ctrl Pts',(0.892072910743004,-20.7888681600112,
-6.63345609672299));
#87698=CARTESIAN_POINT('Ctrl Pts',(0.890676953005833,-20.7891326580897,
-6.63303572875016));
#87699=CARTESIAN_POINT('Ctrl Pts',(0.891342463725141,-20.7890036879005,
-6.63323730344035));
#87700=CARTESIAN_POINT('Ctrl Pts',(0.857932066361018,-20.795432472259,-6.62313857302724));
#87701=CARTESIAN_POINT('Ctrl Pts',(0.829362919845069,-20.802875391614,-6.61444203033488));
#87702=CARTESIAN_POINT('Ctrl Pts',(0.790768248157906,-20.8150830094904,
-6.60272732837196));
#87703=CARTESIAN_POINT('Ctrl Pts',(0.772534435649399,-20.8214503084994,
-6.59719758887313));
#87704=CARTESIAN_POINT('Ctrl Pts',(0.753100910252478,-20.8291425208755,
-6.59130218188709));
#87705=CARTESIAN_POINT('Ctrl Pts',(0.745163626503657,-20.8324766906795,
-6.58889074338885));
#87706=CARTESIAN_POINT('Ctrl Pts',(0.739958766209563,-20.8347057549421,
-6.58730823813184));
#87707=CARTESIAN_POINT('Ctrl Pts',(0.738546223118208,-20.8353131034927,
-6.58687880685544));
#87708=CARTESIAN_POINT('Ctrl Pts',(0.70558389892941,-20.8499843029599,-6.57683802928427));
#87709=CARTESIAN_POINT('Ctrl Pts',(0.679666465671247,-20.8643807451744,
-6.56888477745874));
#87710=CARTESIAN_POINT('Ctrl Pts',(0.645800235846747,-20.8870802526004,
-6.55852605327747));
#87711=CARTESIAN_POINT('Ctrl Pts',(0.630118691860855,-20.8987080773537,
-6.5537351047842));
#87712=CARTESIAN_POINT('Ctrl Pts',(0.613992298402707,-20.9125803270019,
-6.54880951587271));
#87713=CARTESIAN_POINT('Ctrl Pts',(0.607543073274637,-20.9185736067731,
-6.5468369254342));
#87714=CARTESIAN_POINT('Ctrl Pts',(0.603345978244923,-20.9225778908473,
-6.5455521436202));
#87715=CARTESIAN_POINT('Ctrl Pts',(0.602161475406804,-20.9237156571488,
-6.54518957594162));
#87716=CARTESIAN_POINT('Ctrl Pts',(0.553555750815527,-20.9726539431238,
-6.53027978485194));
#87717=CARTESIAN_POINT('Ctrl Pts',(0.530881010941542,-21.02423748137,-6.52327989573953));
#87718=CARTESIAN_POINT('Ctrl Pts',(0.530881033271,-21.0742356128,-6.52327988945));
#87719=CARTESIAN_POINT('Ctrl Pts',(-2.57204347673E-14,-20.7742356128,-6.9673210071));
#87720=CARTESIAN_POINT('Ctrl Pts',(0.0620789114664,-20.7727817153,-6.86712083978));
#87721=CARTESIAN_POINT('Ctrl Pts',(0.126706651057,-20.809097628,-6.7683471563));
#87722=CARTESIAN_POINT('Ctrl Pts',(0.185538258403,-20.8478771982,-6.68330934255));
#87723=CARTESIAN_POINT('Ctrl Pts',(0.248193078621,-20.9544277624,-6.59756027965));
#87724=CARTESIAN_POINT('Ctrl Pts',(0.246934184763,-21.0742356128,-6.59919549778));
#87725=CARTESIAN_POINT('Origin',(2.45,-20.1742356128,10.7304528845));
#87726=CARTESIAN_POINT('',(2.45,-20.6742356128,10.4304528845));
#87727=CARTESIAN_POINT('',(2.45,-19.6742356128,10.4304528845));
#87728=CARTESIAN_POINT('',(2.45,-20.1742356128,10.4304528845));
#87729=CARTESIAN_POINT('',(2.75,-20.6742356128,10.7304528845));
#87730=CARTESIAN_POINT('Origin',(2.45,-20.6742356128,10.7304528845));
#87731=CARTESIAN_POINT('',(2.75,-19.6742356128,10.7304528845));
#87732=CARTESIAN_POINT('',(2.75,-20.1742356128,10.7304528845));
#87733=CARTESIAN_POINT('Origin',(2.45,-19.6742356128,10.7304528845));
#87734=CARTESIAN_POINT('Origin',(-9.64069499267E-16,-21.0742356128,0.729452270839));
#87735=CARTESIAN_POINT('',(1.05,-20.7742356128,6.12111625914));
#87736=CARTESIAN_POINT('Origin',(4.75197961991E-16,-20.7742356128,0.729452270839));
#87737=CARTESIAN_POINT('',(0.992653804111,-21.0742356128,5.82664824081));
#87738=CARTESIAN_POINT('Ctrl Pts',(0.992653804110976,-21.0742356128,5.82664824080987));
#87739=CARTESIAN_POINT('Ctrl Pts',(0.992653804110976,-21.0613737826999,
5.82664824080987));
#87740=CARTESIAN_POINT('Ctrl Pts',(0.992825465996969,-21.0486394859167,
5.82745302551633));
#87741=CARTESIAN_POINT('Ctrl Pts',(0.993151712284542,-21.0360081665505,
5.82904274860581));
#87742=CARTESIAN_POINT('Ctrl Pts',(0.993476339962666,-21.023439515094,5.8306245845839));
#87743=CARTESIAN_POINT('Ctrl Pts',(0.993954068039893,-21.0109715861115,
5.83298378539892));
#87744=CARTESIAN_POINT('Ctrl Pts',(0.994577669380009,-20.9985866770784,
5.83615027998842));
#87745=CARTESIAN_POINT('Ctrl Pts',(0.994884640200276,-20.9924901448225,
5.83770900249105));
#87746=CARTESIAN_POINT('Ctrl Pts',(0.995227101477724,-20.9864139435517,
5.8394640863575));
#87747=CARTESIAN_POINT('Ctrl Pts',(0.995604989294859,-20.9803579410823,
5.84142326476368));
#87748=CARTESIAN_POINT('Ctrl Pts',(0.996177838868538,-20.9711774957876,
5.84439323220866));
#87749=CARTESIAN_POINT('Ctrl Pts',(0.996830573889298,-20.962155591815,5.84779097546331));
#87750=CARTESIAN_POINT('Ctrl Pts',(0.997575235448733,-20.9532078147706,
5.85166511578626));
#87751=CARTESIAN_POINT('Ctrl Pts',(0.998306361330434,-20.9444226810437,
5.85546883604489));
#87752=CARTESIAN_POINT('Ctrl Pts',(0.999126166345993,-20.9357082365423,
5.85973212489889));
#87753=CARTESIAN_POINT('Ctrl Pts',(1.00005409684399,-20.9270106806024,5.86454224149691));
#87754=CARTESIAN_POINT('Ctrl Pts',(1.00094215928179,-20.918686810714,5.86914569389055));
#87755=CARTESIAN_POINT('Ctrl Pts',(1.00192934138979,-20.9103777939368,5.87425043911198));
#87756=CARTESIAN_POINT('Ctrl Pts',(1.00303902096319,-20.9020702878808,5.87996533679234));
#87757=CARTESIAN_POINT('Ctrl Pts',(1.00354099141114,-20.8983123359133,5.88255050625687));
#87758=CARTESIAN_POINT('Ctrl Pts',(1.00406810880741,-20.8945552183043,5.88526094126346));
#87759=CARTESIAN_POINT('Ctrl Pts',(1.00462291545805,-20.8908006844483,5.88810864711666));
#87760=CARTESIAN_POINT('Ctrl Pts',(1.00604541019738,-20.8811742593637,5.89541001344061));
#87761=CARTESIAN_POINT('Ctrl Pts',(1.00761700622559,-20.8716304920317,5.90356829143893));
#87762=CARTESIAN_POINT('Ctrl Pts',(1.00937693368903,-20.8623392678651,5.91267032767187));
#87763=CARTESIAN_POINT('Ctrl Pts',(1.01031913859313,-20.8573650645773,5.91754324621774));
#87764=CARTESIAN_POINT('Ctrl Pts',(1.01131528205079,-20.8524640313087,5.92268642406207));
#87765=CARTESIAN_POINT('Ctrl Pts',(1.01237095229975,-20.8476679491939,5.92811068835221));
#87766=CARTESIAN_POINT('Ctrl Pts',(1.01388472108653,-20.8407906507086,5.93588876297518));
#87767=CARTESIAN_POINT('Ctrl Pts',(1.01551908576205,-20.8341296333023,5.94424489985484));
#87768=CARTESIAN_POINT('Ctrl Pts',(1.0172728984018,-20.8277975927477,5.95319592166203));
#87769=CARTESIAN_POINT('Ctrl Pts',(1.01814980472168,-20.8246315724705,5.95767143256562));
#87770=CARTESIAN_POINT('Ctrl Pts',(1.01905633611331,-20.8215480876829,5.96229539287826));
#87771=CARTESIAN_POINT('Ctrl Pts',(1.01999076354253,-20.8185628017482,5.96706802156685));
#87772=CARTESIAN_POINT('Ctrl Pts',(1.02040789087176,-20.8172301735418,5.96919851752195));
#87773=CARTESIAN_POINT('Ctrl Pts',(1.0208895573644,-20.8157326799941,5.97166143704105));
#87774=CARTESIAN_POINT('Ctrl Pts',(1.0213573719682,-20.8143264991543,5.97405554883608));
#87775=CARTESIAN_POINT('Ctrl Pts',(1.02186869752868,-20.8127895308763,5.97667233451461));
#87776=CARTESIAN_POINT('Ctrl Pts',(1.02236341457022,-20.8113617135062,5.97920661000325));
#87777=CARTESIAN_POINT('Ctrl Pts',(1.02273276025893,-20.8103182140549,5.98110160177315));
#87778=CARTESIAN_POINT('Ctrl Pts',(1.02278248133912,-20.8101777388267,5.98135670435221));
#87779=CARTESIAN_POINT('Ctrl Pts',(1.02282992379982,-20.8100441598503,5.98160018774461));
#87780=CARTESIAN_POINT('Ctrl Pts',(1.0228748175706,-20.8099180973871,5.98183066934277));
#87781=CARTESIAN_POINT('Ctrl Pts',(1.02409474741574,-20.8064925138705,5.98809370707443));
#87782=CARTESIAN_POINT('Ctrl Pts',(1.02547918299804,-20.8028985711144,5.99520200039718));
#87783=CARTESIAN_POINT('Ctrl Pts',(1.02704067673227,-20.7993296264459,6.00321982941105));
#87784=CARTESIAN_POINT('Ctrl Pts',(1.02851792533699,-20.7959532321535,6.01080508349438));
#87785=CARTESIAN_POINT('Ctrl Pts',(1.03015381253913,-20.7925995024583,6.01920525300589));
#87786=CARTESIAN_POINT('Ctrl Pts',(1.03195568051599,-20.7894746092439,6.02845788990672));
#87787=CARTESIAN_POINT('Ctrl Pts',(1.0336950692818,-20.7864580707288,6.03738969450398));
#87788=CARTESIAN_POINT('Ctrl Pts',(1.03558929375091,-20.7836550977369,6.04711672596956));
#87789=CARTESIAN_POINT('Ctrl Pts',(1.03763939303912,-20.7812876463859,6.05764418362696));
#87790=CARTESIAN_POINT('Ctrl Pts',(1.03957796100886,-20.7790489912215,6.06759891720247));
#87791=CARTESIAN_POINT('Ctrl Pts',(1.04165601533973,-20.7772003243519,6.07826992132226));
#87792=CARTESIAN_POINT('Ctrl Pts',(1.04386745197186,-20.7759559810919,6.08962573416775));
#87793=CARTESIAN_POINT('Ctrl Pts',(1.04581189579586,-20.7748618708056,6.0996105285919));
#87794=CARTESIAN_POINT('Ctrl Pts',(1.04785943431315,-20.7742356127999,6.11012462968347));
#87795=CARTESIAN_POINT('Ctrl Pts',(1.05,-20.7742356128,6.12111625914));
#87796=CARTESIAN_POINT('Origin',(2.57175827821E-16,-21.0742356128,0.729452270839));
#87797=CARTESIAN_POINT('Origin',(9.79717439318E-17,-22.3742356128,0.729452270839));
#87798=CARTESIAN_POINT('',(10.7000575594,-22.3742356128,-2.76302312605));
#87799=CARTESIAN_POINT('',(10.9449284019,-22.3742356128,-2.34954507713));
#87800=CARTESIAN_POINT('Origin',(-2.84607155346,-22.3742356128,5.53854202767));
#87801=CARTESIAN_POINT('Origin',(11.0821857629,-22.3742356128,-2.71007990903));
#87802=CARTESIAN_POINT('Origin',(-2.84607155346,-19.6742356128,5.53854202767));
#87803=CARTESIAN_POINT('',(11.2744572343,-19.3742356128,-1.7432341771));
#87804=CARTESIAN_POINT('',(12.6801076867,-19.3742356128,8.90771939699));
#87805=CARTESIAN_POINT('Origin',(-2.84607155346,-19.3742356128,5.53854202767));
#87806=CARTESIAN_POINT('Origin',(12.6801076867,-19.6742356128,8.90771939699));
#87807=CARTESIAN_POINT('Origin',(11.2744572343,-19.6742356128,-1.7432341771));
#87808=CARTESIAN_POINT('Origin',(1.77004158042E-15,-19.6742356128,0.580061096523));
#87809=CARTESIAN_POINT('',(12.1784262599,-19.3742356128,9.98548517727));
#87810=CARTESIAN_POINT('',(3.05,-19.3742356128,15.662287998));
#87811=CARTESIAN_POINT('Origin',(-2.6471818243E-16,-19.3742356128,0.580061096523));
#87812=CARTESIAN_POINT('',(3.109463736,-19.6742356128,15.9563357222));
#87813=CARTESIAN_POINT('Origin',(3.05,-19.6742356128,15.662287998));
#87814=CARTESIAN_POINT('',(12.4158607189067,-19.6742356128,10.1688560519572));
#87815=CARTESIAN_POINT('Origin',(4.37773950874E-16,-19.6742356128,0.580061096523));
#87816=CARTESIAN_POINT('Origin',(12.1784262599,-19.6742356128,9.98548517727));
#87817=CARTESIAN_POINT('Origin',(-2.84607155346,-19.6742356128,5.53854202767));
#87818=CARTESIAN_POINT('',(-1.59504721506E-14,-19.3742356128,-10.0919881826));
#87819=CARTESIAN_POINT('Ctrl Pts',(0.647446102181,-19.6742356128,-10.2675153591));
#87820=CARTESIAN_POINT('Ctrl Pts',(0.647446102180998,-19.6661145052506,
-10.2675153591));
#87821=CARTESIAN_POINT('Ctrl Pts',(0.646514029910601,-19.6579171021141,
-10.2673712859773));
#87822=CARTESIAN_POINT('Ctrl Pts',(0.64468675786068,-19.649672691115,-10.2670767778534));
#87823=CARTESIAN_POINT('Ctrl Pts',(0.642484067022575,-19.6397344399529,
-10.2667217621094));
#87824=CARTESIAN_POINT('Ctrl Pts',(0.638978968301581,-19.629725348657,-10.266147977288));
#87825=CARTESIAN_POINT('Ctrl Pts',(0.634153962808074,-19.6196963097844,
-10.2653265413293));
#87826=CARTESIAN_POINT('Ctrl Pts',(0.63040461389043,-19.611903082172,-10.2646882311704));
#87827=CARTESIAN_POINT('Ctrl Pts',(0.62585543611501,-19.6040982920229,-10.263899832074));
#87828=CARTESIAN_POINT('Ctrl Pts',(0.620491482566137,-19.5963142733431,
-10.2629448315708));
#87829=CARTESIAN_POINT('Ctrl Pts',(0.614628484782217,-19.5878060556909,
-10.2619009810261));
#87830=CARTESIAN_POINT('Ctrl Pts',(0.6078099922246,-19.5793188188891,-10.260651735256));
#87831=CARTESIAN_POINT('Ctrl Pts',(0.600023817872344,-19.5709021743201,
-10.2591844483976));
#87832=CARTESIAN_POINT('Ctrl Pts',(0.595862391014903,-19.5664037840742,
-10.2584002369654));
#87833=CARTESIAN_POINT('Ctrl Pts',(0.591425464005122,-19.5619252987295,
-10.25755382013));
#87834=CARTESIAN_POINT('Ctrl Pts',(0.586716534392515,-19.5574710301045,
-10.2566435084696));
#87835=CARTESIAN_POINT('Ctrl Pts',(0.579956784063687,-19.5510768500509,
-10.2553367402543));
#87836=CARTESIAN_POINT('Ctrl Pts',(0.572632437983098,-19.5447350403784,
-10.2539002805891));
#87837=CARTESIAN_POINT('Ctrl Pts',(0.56474609288734,-19.5384613170291,-10.2523376323413));
#87838=CARTESIAN_POINT('Ctrl Pts',(0.560802920339461,-19.5353244553545,
-10.2515563082174));
#87839=CARTESIAN_POINT('Ctrl Pts',(0.556719258945826,-19.5322045354405,
-10.2507434914554));
#87840=CARTESIAN_POINT('Ctrl Pts',(0.552495335544852,-19.5291037878776,
-10.2498990306019));
#87841=CARTESIAN_POINT('Ctrl Pts',(0.550383373844366,-19.5275534140961,
-10.2494768001751));
#87842=CARTESIAN_POINT('Ctrl Pts',(0.548235277312453,-19.5260077421965,
-10.2490468190963));
#87843=CARTESIAN_POINT('Ctrl Pts',(0.546049957467887,-19.5244670276599,
-10.2486090864764));
#87844=CARTESIAN_POINT('Ctrl Pts',(0.544524237517349,-19.5233913503798,
-10.2483034756556));
#87845=CARTESIAN_POINT('Ctrl Pts',(0.542513261054432,-19.521993581982,-10.247899197113));
#87846=CARTESIAN_POINT('Ctrl Pts',(0.540999194023679,-19.5209556339349,
-10.2475938147385));
#87847=CARTESIAN_POINT('Ctrl Pts',(0.540344631924859,-19.5205069077963,
-10.2474617917013));
#87848=CARTESIAN_POINT('Ctrl Pts',(0.53978335417908,-19.5201246497013,-10.2473484155898));
#87849=CARTESIAN_POINT('Ctrl Pts',(0.539396023575437,-19.5198615198152,
-10.2472701690991));
#87850=CARTESIAN_POINT('Ctrl Pts',(0.5365359708291,-19.5179185663116,-10.2466923962906));
#87851=CARTESIAN_POINT('Ctrl Pts',(0.533598144968601,-19.5159691901031,
-10.2460961657641));
#87852=CARTESIAN_POINT('Ctrl Pts',(0.530579239314274,-19.514015815137,-10.2454801288448));
#87853=CARTESIAN_POINT('Ctrl Pts',(0.520942696132119,-19.5077805152082,
-10.2435136989345));
#87854=CARTESIAN_POINT('Ctrl Pts',(0.510477444889386,-19.5015000483366,
-10.241345014764));
#87855=CARTESIAN_POINT('Ctrl Pts',(0.499188517402588,-19.4951987036651,
-10.238944290718));
#87856=CARTESIAN_POINT('Ctrl Pts',(0.488625147959329,-19.4893023568392,
-10.2366978651776));
#87857=CARTESIAN_POINT('Ctrl Pts',(0.477341422036914,-19.4833898482769,
-10.2342485041625));
#87858=CARTESIAN_POINT('Ctrl Pts',(0.465340425103763,-19.4775255046665,
-10.2315715082685));
#87859=CARTESIAN_POINT('Ctrl Pts',(0.45701593025548,-19.473457701096,-10.2297146093248));
#87860=CARTESIAN_POINT('Ctrl Pts',(0.448344875980685,-19.4694104929294,
-10.2277440364128));
#87861=CARTESIAN_POINT('Ctrl Pts',(0.439325215689106,-19.4654018145338,
-10.225653455845));
#87862=CARTESIAN_POINT('Ctrl Pts',(0.432718427317387,-19.462465507738,-10.224122131722));
#87863=CARTESIAN_POINT('Ctrl Pts',(0.425924517260663,-19.4595485265549,
-10.2225263148284));
#87864=CARTESIAN_POINT('Ctrl Pts',(0.418945134426883,-19.4566588813194,
-10.220863546663));
#87865=CARTESIAN_POINT('Ctrl Pts',(0.410691277831415,-19.453241570942,-10.2188971478689));
#87866=CARTESIAN_POINT('Ctrl Pts',(0.402176808635664,-19.4498619528698,
-10.2168368040588));
#87867=CARTESIAN_POINT('Ctrl Pts',(0.393402134457967,-19.4465329233363,
-10.2146787128479));
#87868=CARTESIAN_POINT('Ctrl Pts',(0.389014797369119,-19.4448684085696,
-10.2135996672424));
#87869=CARTESIAN_POINT('Ctrl Pts',(0.384562409197909,-19.4432165396316,
-10.2124961856045));
#87870=CARTESIAN_POINT('Ctrl Pts',(0.380045035728103,-19.4415789656171,
-10.2113678424595));
#87871=CARTESIAN_POINT('Ctrl Pts',(0.3777863489932,-19.4407601786098,-10.210803670887));
#87872=CARTESIAN_POINT('Ctrl Pts',(0.375511415934218,-19.4399449653191,
-10.2102332839411));
#87873=CARTESIAN_POINT('Ctrl Pts',(0.373220246465779,-19.4391335362231,
-10.2096566337111));
#87874=CARTESIAN_POINT('Ctrl Pts',(0.37126483257825,-19.4384410166409,-10.2091644877204));
#87875=CARTESIAN_POINT('Ctrl Pts',(0.368456147018735,-19.4374586741451,
-10.2084548315196));
#87876=CARTESIAN_POINT('Ctrl Pts',(0.366948540082698,-19.4369360561463,
-10.2080727559659));
#87877=CARTESIAN_POINT('Ctrl Pts',(0.366689675478217,-19.4368463196916,
-10.2080071514408));
#87878=CARTESIAN_POINT('Ctrl Pts',(0.366469198567963,-19.4367700102461,
-10.2079512492117));
#87879=CARTESIAN_POINT('Ctrl Pts',(0.366298039268187,-19.4367108132956,
-10.2079078469347));
#87880=CARTESIAN_POINT('Ctrl Pts',(0.356260121683919,-19.4332391111383,
-10.2053624492886));
#87881=CARTESIAN_POINT('Ctrl Pts',(0.344523522384,-19.4293734552193,-10.2023698293493));
#87882=CARTESIAN_POINT('Ctrl Pts',(0.331093866419504,-19.4252612897843,
-10.1988398420676));
#87883=CARTESIAN_POINT('Ctrl Pts',(0.319521466675984,-19.421717816865,-10.1957980348895));
#87884=CARTESIAN_POINT('Ctrl Pts',(0.306692181674625,-19.4179917981974,
-10.1923571037522));
#87885=CARTESIAN_POINT('Ctrl Pts',(0.292589265961312,-19.4141990783959,
-10.1884495017355));
#87886=CARTESIAN_POINT('Ctrl Pts',(0.27735466068823,-19.4101020115012,-10.1842283338935));
#87887=CARTESIAN_POINT('Ctrl Pts',(0.260641154924078,-19.4059290029001,
-10.1794643813728));
#87888=CARTESIAN_POINT('Ctrl Pts',(0.24244820239673,-19.4018711064667,-10.1740860690497));
#87889=CARTESIAN_POINT('Ctrl Pts',(0.233353953358138,-19.3998426550274,
-10.1713975713141));
#87890=CARTESIAN_POINT('Ctrl Pts',(0.223581355390598,-19.3977783193054,
-10.1684623406569));
#87891=CARTESIAN_POINT('Ctrl Pts',(0.213592020167185,-19.3958100852677,
-10.1654109992299));
#87892=CARTESIAN_POINT('Ctrl Pts',(0.212217188156573,-19.3955391972557,
-10.1649910431692));
#87893=CARTESIAN_POINT('Ctrl Pts',(0.210838283811837,-19.3952700611272,
-10.1645689166307));
#87894=CARTESIAN_POINT('Ctrl Pts',(0.209456541976758,-19.3950029537208,
-10.1641449888382));
#87895=CARTESIAN_POINT('Ctrl Pts',(0.20079382531649,-19.3933283458306,-10.1614872084504));
#87896=CARTESIAN_POINT('Ctrl Pts',(0.192018974991822,-19.3917356758629,
-10.1587578386406));
#87897=CARTESIAN_POINT('Ctrl Pts',(0.183437645601415,-19.3902770692547,
-10.1560558665988));
#87898=CARTESIAN_POINT('Ctrl Pts',(0.162049521978107,-19.3866416350422,
-10.1493214657353));
#87899=CARTESIAN_POINT('Ctrl Pts',(0.141963744437887,-19.3838261803671,
-10.1427586050297));
#87900=CARTESIAN_POINT('Ctrl Pts',(0.123218156746419,-19.3816330503464,
-10.1364476902696));
#87901=CARTESIAN_POINT('Ctrl Pts',(0.10191282119446,-19.3791404439919,-10.1292750073525));
#87902=CARTESIAN_POINT('Ctrl Pts',(0.0823386209659976,-19.377452038616,
-10.1224257079578));
#87903=CARTESIAN_POINT('Ctrl Pts',(0.0645043297250956,-19.3763190342603,
-10.116009220907));
#87904=CARTESIAN_POINT('Ctrl Pts',(0.0455284429160304,-19.3751135048609,
-10.1091820063939));
#87905=CARTESIAN_POINT('Ctrl Pts',(0.0285209561981343,-19.3745367951057,
-10.1028465719473));
#87906=CARTESIAN_POINT('Ctrl Pts',(0.0134553406264266,-19.3743288400826,
-10.0971275629238));
#87907=CARTESIAN_POINT('Ctrl Pts',(0.00878408254826948,-19.3742643613644,
-10.0953543219319));
#87908=CARTESIAN_POINT('Ctrl Pts',(0.00429934326341183,-19.3742356128,-10.0936401659177));
#87909=CARTESIAN_POINT('Ctrl Pts',(1.13381424745833E-15,-19.3742356128,
-10.0919881826));
#87910=CARTESIAN_POINT('',(10.3267865236,-19.3742356128,-3.3434289261));
#87911=CARTESIAN_POINT('Origin',(-2.84607155346,-19.3742356128,5.53854202767));
#87912=CARTESIAN_POINT('Origin',(10.3267865236652,-19.6742356128,-3.34342892613464));
#87913=CARTESIAN_POINT('Origin',(11.0821857629,-19.6742356128,-2.71007990903));
#87914=CARTESIAN_POINT('',(11.2159436339,-19.6742356128,-2.03747244546));
#87915=CARTESIAN_POINT('Ctrl Pts',(11.2159436339004,-19.6742356128,-2.03747244545784));
#87916=CARTESIAN_POINT('Ctrl Pts',(11.2159436338995,-19.6693613928602,-2.03747244545767));
#87917=CARTESIAN_POINT('Ctrl Pts',(11.2159655230008,-19.6640117573582,-2.03735938679454));
#87918=CARTESIAN_POINT('Ctrl Pts',(11.2160281016569,-19.6580667153257,-2.0370446657002));
#87919=CARTESIAN_POINT('Ctrl Pts',(11.2160872352179,-19.6524489611568,-2.03674727070616));
#87920=CARTESIAN_POINT('Ctrl Pts',(11.2161826332475,-19.6462990285337,-2.03627014239475));
#87921=CARTESIAN_POINT('Ctrl Pts',(11.2163384018002,-19.6395287243193,-2.03549712925787));
#87922=CARTESIAN_POINT('Ctrl Pts',(11.2164821525656,-19.6332807596527,-2.03478375529222));
#87923=CARTESIAN_POINT('Ctrl Pts',(11.2166773185298,-19.6265039597716,-2.03381837797931));
#87924=CARTESIAN_POINT('Ctrl Pts',(11.2169504658595,-19.619147424528,-2.03247155937132));
#87925=CARTESIAN_POINT('Ctrl Pts',(11.2171665294076,-19.6133282971438,-2.03140620607881));
#87926=CARTESIAN_POINT('Ctrl Pts',(11.2174315183419,-19.6071465569882,-2.03010151757666));
#87927=CARTESIAN_POINT('Ctrl Pts',(11.2177623828648,-19.6005900787551,-2.02847447984685));
#87928=CARTESIAN_POINT('Ctrl Pts',(11.218258591935,-19.5907570995657,-2.02603435458925));
#87929=CARTESIAN_POINT('Ctrl Pts',(11.2188255021808,-19.5818481179776,-2.02330895032003));
#87930=CARTESIAN_POINT('Ctrl Pts',(11.2194011752077,-19.5738403257838,-2.0205239658219));
#87931=CARTESIAN_POINT('Ctrl Pts',(11.2198012071017,-19.5682757567871,-2.01858869602226));
#87932=CARTESIAN_POINT('Ctrl Pts',(11.2202056395416,-19.5631455115216,-2.01662372036666));
#87933=CARTESIAN_POINT('Ctrl Pts',(11.2205960026702,-19.5584353020539,-2.01469186385905));
#87934=CARTESIAN_POINT('Ctrl Pts',(11.2210720637434,-19.5526910418769,-2.01233589933555));
#87935=CARTESIAN_POINT('Ctrl Pts',(11.2215309766499,-19.5475701479139,-2.01003015077224));
#87936=CARTESIAN_POINT('Ctrl Pts',(11.2219592146484,-19.5430379937272,-2.00786819701386));
#87937=CARTESIAN_POINT('Ctrl Pts',(11.2221733336476,-19.5407719166338,-2.00678722013467));
#87938=CARTESIAN_POINT('Ctrl Pts',(11.2223799594567,-19.5386529605451,-2.00574183086384));
#87939=CARTESIAN_POINT('Ctrl Pts',(11.222578261594,-19.5366766942524,-2.0047416089727));
#87940=CARTESIAN_POINT('Ctrl Pts',(11.2226959635169,-19.5355036844903,-2.00414792883612));
#87941=CARTESIAN_POINT('Ctrl Pts',(11.2227632467704,-19.5348401327041,-2.00380636847078));
#87942=CARTESIAN_POINT('Ctrl Pts',(11.2228640658506,-19.5338660918148,-2.00330063603375));
#87943=CARTESIAN_POINT('Ctrl Pts',(11.22293310499,-19.5331990856817,-2.00295431932273));
#87944=CARTESIAN_POINT('Ctrl Pts',(11.2230179020481,-19.5323865415852,-2.0025308549887));
#87945=CARTESIAN_POINT('Ctrl Pts',(11.2231477904519,-19.5311716776,-2.00188466056667));
#87946=CARTESIAN_POINT('Ctrl Pts',(11.2243488190571,-19.5199382929807,-1.99590954683396));
#87947=CARTESIAN_POINT('Ctrl Pts',(11.2256255742843,-19.5095883708649,-1.98949289875886));
#87948=CARTESIAN_POINT('Ctrl Pts',(11.2269421893286,-19.5000727519268,-1.9828372680661));
#87949=CARTESIAN_POINT('Ctrl Pts',(11.2283389310385,-19.4899780306761,-1.97577658845831));
#87950=CARTESIAN_POINT('Ctrl Pts',(11.2297804517346,-19.4808214431763,-1.96844723872592));
#87951=CARTESIAN_POINT('Ctrl Pts',(11.2312343309138,-19.4725140943552,-1.96104193633524));
#87952=CARTESIAN_POINT('Ctrl Pts',(11.2327789135453,-19.4636884732944,-1.95317463785666));
#87953=CARTESIAN_POINT('Ctrl Pts',(11.2343374115243,-19.4558204434581,-1.94522171060417));
#87954=CARTESIAN_POINT('Ctrl Pts',(11.2358832957294,-19.448784286417,-1.93735720972956));
#87955=CARTESIAN_POINT('Ctrl Pts',(11.237350034937,-19.4421083611644,-1.92989534955764));
#87956=CARTESIAN_POINT('Ctrl Pts',(11.238805608868,-19.4361805746817,-1.92251221094851));
#87957=CARTESIAN_POINT('Ctrl Pts',(11.2402365654223,-19.4308894383749,-1.91531434798852));
#87958=CARTESIAN_POINT('Ctrl Pts',(11.2424783121132,-19.4226003066944,-1.90403812480444));
#87959=CARTESIAN_POINT('Ctrl Pts',(11.2447614681787,-19.4153947337217,-1.8925549054251));
#87960=CARTESIAN_POINT('Ctrl Pts',(11.2470547932876,-19.4091625001044,-1.88102151742434));
#87961=CARTESIAN_POINT('Ctrl Pts',(11.2495134495914,-19.4024809701238,-1.86865666038664));
#87962=CARTESIAN_POINT('Ctrl Pts',(11.2519838185799,-19.3969172471324,-1.85623401887946));
#87963=CARTESIAN_POINT('Ctrl Pts',(11.2544393837905,-19.392334226818,-1.84388652056322));
#87964=CARTESIAN_POINT('Ctrl Pts',(11.2569925855012,-19.3875689795923,-1.83104806948533));
#87965=CARTESIAN_POINT('Ctrl Pts',(11.2595299095001,-19.3838631500315,-1.81829021968229));
#87966=CARTESIAN_POINT('Ctrl Pts',(11.2620327668194,-19.3810753841191,-1.80570587411781));
#87967=CARTESIAN_POINT('Ctrl Pts',(11.2646923382581,-19.3781130647965,-1.79233357127776));
#87968=CARTESIAN_POINT('Ctrl Pts',(11.2673131246881,-19.3761865920875,-1.77915651243343));
#87969=CARTESIAN_POINT('Ctrl Pts',(11.2698832252856,-19.3751535179302,-1.76623371991554));
#87970=CARTESIAN_POINT('Ctrl Pts',(11.2714264017639,-19.3745332248019,-1.75847443241259));
#87971=CARTESIAN_POINT('Ctrl Pts',(11.2729514923844,-19.3742356128001,-1.75080586802915));
#87972=CARTESIAN_POINT('Ctrl Pts',(11.2744572343,-19.3742356128,-1.7432341771));
#87973=CARTESIAN_POINT('',(10.5566756949,-19.6742356128,-3.15068305993));
#87974=CARTESIAN_POINT('Origin',(11.0821857629,-19.6742356128,-2.71007990903));
#87975=CARTESIAN_POINT('Origin',(10.3267865236,-19.6742356128,-3.3434289261));
#87976=CARTESIAN_POINT('Origin',(11.0821857629,-19.3742356128,-2.71007990903));
#87977=CARTESIAN_POINT('Origin',(12.5441720511,-22.5760378048,9.34841724773));
#87978=CARTESIAN_POINT('',(12.8222448231109,-23.4742356815,9.46100293550673));
#87979=CARTESIAN_POINT('Origin',(12.5441720511,-23.4742356478461,9.34841724773));
#87980=CARTESIAN_POINT('',(12.8222448081,-25.4742356128,9.46100295649));
#87981=CARTESIAN_POINT('',(12.8222448081,-21.2742356128,9.46100295649));
#87982=CARTESIAN_POINT('Origin',(12.5441720511,-25.4742356128,9.34841724773));
#87983=CARTESIAN_POINT('Origin',(12.5441720511,-25.4742356128,9.34841724773));
#87984=CARTESIAN_POINT('Origin',(12.5441720511,-25.4742356128,9.34841724773));
#87985=CARTESIAN_POINT('Origin',(10.0415172382,-25.4742356128,8.33514586886));
#87986=CARTESIAN_POINT('Origin',(10.0415172382,-25.4742356128,8.33514586886));
#87987=CARTESIAN_POINT('Origin',(10.0415172382,-19.6742356128,8.33514586886));
#87988=CARTESIAN_POINT('Origin',(10.0415172382,-19.3742356128,8.33514586886));
#87989=CARTESIAN_POINT('Origin',(10.0415172382,-19.6742356128,8.33514586886));
#87990=CARTESIAN_POINT('Origin',(10.0415172382,-21.2742356128,8.33514586886));
#87991=CARTESIAN_POINT('',(12.4158608431,-21.2742356128,10.1688558911));
#87992=CARTESIAN_POINT('Ctrl Pts',(12.822244843051,-23.4742356815,9.46100291845212));
#87993=CARTESIAN_POINT('Ctrl Pts',(12.8222448374688,-23.4526557884998,9.46100292804296));
#87994=CARTESIAN_POINT('Ctrl Pts',(12.8227658011016,-23.4310761714824,9.459718249267));
#87995=CARTESIAN_POINT('Ctrl Pts',(12.8237956782946,-23.4096767931088,9.45716500907838));
#87996=CARTESIAN_POINT('Ctrl Pts',(12.8249218353694,-23.3862768561876,9.45437307473734));
#87997=CARTESIAN_POINT('Ctrl Pts',(12.8266564446377,-23.3630965146334,9.45006425351064));
#87998=CARTESIAN_POINT('Ctrl Pts',(12.8289489787169,-23.3403539792507,9.4443040829754));
#87999=CARTESIAN_POINT('Ctrl Pts',(12.8312709606729,-23.3173193132581,9.43846992235491));
#88000=CARTESIAN_POINT('Ctrl Pts',(12.8341646949754,-23.2947342337854,9.43114748157285));
#88001=CARTESIAN_POINT('Ctrl Pts',(12.8375494613154,-23.2727938554516,9.42244323588751));
#88002=CARTESIAN_POINT('Ctrl Pts',(12.8410023873676,-23.250411659361,9.41356371107774));
#88003=CARTESIAN_POINT('Ctrl Pts',(12.8449656668396,-23.2287009550523,9.40324680779877));
#88004=CARTESIAN_POINT('Ctrl Pts',(12.8493339497345,-23.2078282931751,9.39163588847771));
#88005=CARTESIAN_POINT('Ctrl Pts',(12.8533668576591,-23.1885581301571,9.38091639762304));
#88006=CARTESIAN_POINT('Ctrl Pts',(12.8577443119826,-23.1700021065795,9.36909474059184));
#88007=CARTESIAN_POINT('Ctrl Pts',(12.8623765483007,-23.1522553698924,9.35629852758267));
#88008=CARTESIAN_POINT('Ctrl Pts',(12.8676258737502,-23.1321444795705,9.34179765111725));
#88009=CARTESIAN_POINT('Ctrl Pts',(12.8732011777363,-23.1130741318264,9.3260463447321));
#88010=CARTESIAN_POINT('Ctrl Pts',(12.8789692176796,-23.0951288263937,9.30924271806145));
#88011=CARTESIAN_POINT('Ctrl Pts',(12.8847323055415,-23.0771989276877,9.29245351794285));
#88012=CARTESIAN_POINT('Ctrl Pts',(12.8906877245128,-23.0603914552665,9.27461404125843));
#88013=CARTESIAN_POINT('Ctrl Pts',(12.8967175034202,-23.0447417766193,9.25591265355548));
#88014=CARTESIAN_POINT('Ctrl Pts',(12.9032960762988,-23.0276677589662,9.23550917876373));
#88015=CARTESIAN_POINT('Ctrl Pts',(12.909961941791,-23.0119710592708,9.21408281923307));
#88016=CARTESIAN_POINT('Ctrl Pts',(12.9165837263722,-22.997646095339,9.1918614547601));
#88017=CARTESIAN_POINT('Ctrl Pts',(12.9229613039847,-22.9838494264575,9.17045959928658));
#88018=CARTESIAN_POINT('Ctrl Pts',(12.9292980187867,-22.9713240464602,9.14832050002835));
#88019=CARTESIAN_POINT('Ctrl Pts',(12.9354980002173,-22.9600302011921,9.12562740036042));
#88020=CARTESIAN_POINT('Ctrl Pts',(12.9422358704374,-22.9477565412539,9.10096552642308));
#88021=CARTESIAN_POINT('Ctrl Pts',(12.9488130289529,-22.9369364542937,9.07564536621217));
#88022=CARTESIAN_POINT('Ctrl Pts',(12.9551362385969,-22.9274915788356,9.04986970620133));
#88023=CARTESIAN_POINT('Ctrl Pts',(12.9614594482409,-22.9180467033774,9.02409404619048));
#88024=CARTESIAN_POINT('Ctrl Pts',(12.9675285501681,-22.9099757205391,8.99786337398523));
#88025=CARTESIAN_POINT('Ctrl Pts',(12.9732844031999,-22.9031898545,8.97133867789998));
#88026=CARTESIAN_POINT('Ctrl Pts',(10.5755264816041,-22.073347939028,-3.51114426672837));
#88027=CARTESIAN_POINT('Ctrl Pts',(10.6189732998864,-22.0734675796473,-3.44670824878185));
#88028=CARTESIAN_POINT('Ctrl Pts',(10.6415548738579,-22.073587220165,-3.36820356962979));
#88029=CARTESIAN_POINT('Ctrl Pts',(10.6370073188241,-22.0736899806765,-3.28463114868135));
#88030=CARTESIAN_POINT('Ctrl Pts',(10.6060354193007,-22.0737598091151,-3.20904188084407));
#88031=CARTESIAN_POINT('Ctrl Pts',(10.5558506553124,-22.0737923598628,-3.14970279055262));
#88032=CARTESIAN_POINT('Ctrl Pts',(10.5754458724638,-22.1652998410927,-3.51126386273525));
#88033=CARTESIAN_POINT('Ctrl Pts',(10.618903371002,-22.1530274460811,-3.44681323084733));
#88034=CARTESIAN_POINT('Ctrl Pts',(10.641496283718,-22.1407550510704,-3.36829411184493));
#88035=CARTESIAN_POINT('Ctrl Pts',(10.6369593909186,-22.1302141599519,-3.28470925230792));
#88036=CARTESIAN_POINT('Ctrl Pts',(10.6059957968922,-22.1230513527872,-3.20911112586287));
#88037=CARTESIAN_POINT('Ctrl Pts',(10.5558161001343,-22.1197123858053,-3.14976720010066));
#88038=CARTESIAN_POINT('Ctrl Pts',(10.5857997847365,-22.2572834900482,-3.49590425496629));
#88039=CARTESIAN_POINT('Ctrl Pts',(10.6278856426866,-22.2326147094154,-3.4333298375838));
#88040=CARTESIAN_POINT('Ctrl Pts',(10.6490223141032,-22.2079459286819,-3.35666455173243));
#88041=CARTESIAN_POINT('Ctrl Pts',(10.6431159920152,-22.1867575798953,-3.2746766456359));
#88042=CARTESIAN_POINT('Ctrl Pts',(10.6110854924619,-22.1723594349106,-3.20021597700034));
#88043=CARTESIAN_POINT('Ctrl Pts',(10.5602546815746,-22.1656479230153,-3.14149308533282));
#88044=CARTESIAN_POINT('Ctrl Pts',(10.6065715306299,-22.3443167259089,-3.46513076367994));
#88045=CARTESIAN_POINT('Ctrl Pts',(10.6459119686815,-22.3078279887505,-3.40630062234996));
#88046=CARTESIAN_POINT('Ctrl Pts',(10.6641106942264,-22.2713392514914,-3.3333218087324));
#88047=CARTESIAN_POINT('Ctrl Pts',(10.6554225922274,-22.2400430269978,-3.2544822528469));
#88048=CARTESIAN_POINT('Ctrl Pts',(10.6212346959669,-22.2188693850443,-3.18223722148648));
#88049=CARTESIAN_POINT('Ctrl Pts',(10.5691144274879,-22.209114211317,-3.12470547607949));
#88050=CARTESIAN_POINT('Ctrl Pts',(10.6748166371955,-22.5209266907492,-3.36289055825833));
#88051=CARTESIAN_POINT('Ctrl Pts',(10.7052316290396,-22.4602477908528,-3.31650182759889));
#88052=CARTESIAN_POINT('Ctrl Pts',(10.7138733888551,-22.3995688908556,-3.25576778202096));
#88053=CARTESIAN_POINT('Ctrl Pts',(10.6960859309467,-22.3476657503612,-3.18746418308737));
#88054=CARTESIAN_POINT('Ctrl Pts',(10.6546593558206,-22.3128693591781,-3.12274837994517));
#88055=CARTESIAN_POINT('Ctrl Pts',(10.5979621503895,-22.2973226488988,-3.06936176748442));
#88056=CARTESIAN_POINT('Ctrl Pts',(10.7770676343791,-22.6313508349927,-3.20587132888339));
#88057=CARTESIAN_POINT('Ctrl Pts',(10.7947683037157,-22.5535956183832,-3.17804091297403));
#88058=CARTESIAN_POINT('Ctrl Pts',(10.7887694347283,-22.4758404017738,-3.13498582812424));
#88059=CARTESIAN_POINT('Ctrl Pts',(10.7560189786525,-22.4102922092715,-3.08108257829107));
#88060=CARTESIAN_POINT('Ctrl Pts',(10.7022156734909,-22.3684261450212,-3.02593957847265));
#88061=CARTESIAN_POINT('Ctrl Pts',(10.6376381360204,-22.3525284903903,-2.97725090948219));
#88062=CARTESIAN_POINT('Ctrl Pts',(10.8411323863464,-22.6664009565298,-3.10546741472568));
#88063=CARTESIAN_POINT('Ctrl Pts',(10.8511507365709,-22.582155535137,-3.08929951273552));
#88064=CARTESIAN_POINT('Ctrl Pts',(10.8360597596591,-22.4979101137442,-3.05723132474782));
#88065=CARTESIAN_POINT('Ctrl Pts',(10.7937463726032,-22.4275879287889,-3.01219357566858));
#88066=CARTESIAN_POINT('Ctrl Pts',(10.7317180936056,-22.3842297203853,-2.96288258512268));
#88067=CARTESIAN_POINT('Ctrl Pts',(10.6616004183053,-22.3700818046728,-2.91694755475329));
#88068=CARTESIAN_POINT('Ctrl Pts',(10.9026335403798,-22.6742830962032,-3.00661736786854));
#88069=CARTESIAN_POINT('Ctrl Pts',(10.9059308011903,-22.5846434461728,-3.00123595319039));
#88070=CARTESIAN_POINT('Ctrl Pts',(10.8808935813686,-22.4950037961424,-2.97821475154161));
#88071=CARTESIAN_POINT('Ctrl Pts',(10.8265348140848,-22.4221227996667,-2.93850991788712));
#88072=CARTESIAN_POINT('Ctrl Pts',(10.754120168993,-22.3814334073002,-2.89056167992165));
#88073=CARTESIAN_POINT('Ctrl Pts',(10.6779444379831,-22.3741354186777,-2.84322868920662));
#88074=CARTESIAN_POINT('Ctrl Pts',(10.9562463120162,-22.6742354344034,-2.91912533867425));
#88075=CARTESIAN_POINT('Ctrl Pts',(10.9562214113882,-22.5796388423537,-2.91916597451867));
#88076=CARTESIAN_POINT('Ctrl Pts',(10.9244049920089,-22.4850422503039,-2.89972567303062));
#88077=CARTESIAN_POINT('Ctrl Pts',(10.8603955187549,-22.4104207249433,-2.86054658143736));
#88078=CARTESIAN_POINT('Ctrl Pts',(10.7795412374011,-22.3736906146549,-2.81102307954316));
#88079=CARTESIAN_POINT('Ctrl Pts',(10.6988848574274,-22.3742405364324,-2.76159881818277));
#88080=CARTESIAN_POINT('',(10.5566756928877,-22.0742356130312,-3.15068306070111));
#88081=CARTESIAN_POINT('Ctrl Pts',(10.5566756909963,-22.0742356130312,-3.15068305522312));
#88082=CARTESIAN_POINT('Ctrl Pts',(10.5566756934735,-22.0899525193036,-3.15068305815888));
#88083=CARTESIAN_POINT('Ctrl Pts',(10.5573623074021,-22.1056755510411,-3.14957422284101));
#88084=CARTESIAN_POINT('Ctrl Pts',(10.5586671517577,-22.1211849491845,-3.14730288034606));
#88085=CARTESIAN_POINT('Ctrl Pts',(10.559949323621,-22.136424861771,-3.14507100385689));
#88086=CARTESIAN_POINT('Ctrl Pts',(10.5618278097496,-22.1514578348887,-3.14171667117984));
#88087=CARTESIAN_POINT('Ctrl Pts',(10.5642316242454,-22.1660850328081,-3.13723770193223));
#88088=CARTESIAN_POINT('Ctrl Pts',(10.5666187611341,-22.1806107475803,-3.13278980766549));
#88089=CARTESIAN_POINT('Ctrl Pts',(10.5695234657495,-22.1947357268319,-3.12723298635599));
#88090=CARTESIAN_POINT('Ctrl Pts',(10.5728784346858,-22.208284065637,-3.12061247077665));
#88091=CARTESIAN_POINT('Ctrl Pts',(10.5762351667071,-22.2218395242907,-3.11398847602029));
#88092=CARTESIAN_POINT('Ctrl Pts',(10.5800422752663,-22.234817250828,-3.10629997477472));
#88093=CARTESIAN_POINT('Ctrl Pts',(10.5842410421963,-22.2470679396434,-3.09763643012156));
#88094=CARTESIAN_POINT('Ctrl Pts',(10.5882460917805,-22.2587534218252,-3.08937259302623));
#88095=CARTESIAN_POINT('Ctrl Pts',(10.5926074196856,-22.2697773332744,-3.08022227091879));
#88096=CARTESIAN_POINT('Ctrl Pts',(10.5972849163347,-22.2800381439071,-3.0702956139941));
#88097=CARTESIAN_POINT('Ctrl Pts',(10.6012330710361,-22.2886990304408,-3.06191677801711));
#88098=CARTESIAN_POINT('Ctrl Pts',(10.6054661382905,-22.296879480602,-3.05296180738476));
#88099=CARTESIAN_POINT('Ctrl Pts',(10.6098478833313,-22.3044716723759,-3.04340827272847));
#88100=CARTESIAN_POINT('Ctrl Pts',(10.6140927795382,-22.3118267479824,-3.03415311008243));
#88101=CARTESIAN_POINT('Ctrl Pts',(10.6184766453214,-22.3186295557672,-3.02433701732395));
#88102=CARTESIAN_POINT('Ctrl Pts',(10.6228936503569,-22.3248195086567,-3.0139710852086));
#88103=CARTESIAN_POINT('Ctrl Pts',(10.6272969718839,-22.3309902855951,-3.0036372658752));
#88104=CARTESIAN_POINT('Ctrl Pts',(10.6317327207341,-22.3365518968271,-2.99275788444388));
#88105=CARTESIAN_POINT('Ctrl Pts',(10.6361223115085,-22.3414844523268,-2.98136320543062));
#88106=CARTESIAN_POINT('Ctrl Pts',(10.6404844891338,-22.3463862038436,-2.97003968658923));
#88107=CARTESIAN_POINT('Ctrl Pts',(10.6448007098638,-22.3506668911406,-2.95820823841755));
#88108=CARTESIAN_POINT('Ctrl Pts',(10.6490263221702,-22.3543462073631,-2.9459038456027));
#88109=CARTESIAN_POINT('Ctrl Pts',(10.6531973013616,-22.3579779535552,-2.93375853678779));
#88110=CARTESIAN_POINT('Ctrl Pts',(10.6572797194545,-22.3610241695016,-2.92115327288598));
#88111=CARTESIAN_POINT('Ctrl Pts',(10.6612670512316,-22.3635379124603,-2.90811347414347));
#88112=CARTESIAN_POINT('Ctrl Pts',(10.6651259957032,-22.3659707159077,-2.89549354129583));
#88113=CARTESIAN_POINT('Ctrl Pts',(10.6688956905757,-22.3679053423702,-2.88246710423552));
#88114=CARTESIAN_POINT('Ctrl Pts',(10.6726076695519,-22.3694148940626,-2.86903976949775));
#88115=CARTESIAN_POINT('Ctrl Pts',(10.6762290310023,-22.3708875942965,-2.85594022536955));
#88116=CARTESIAN_POINT('Ctrl Pts',(10.6797951054022,-22.3719562403948,-2.84245930266272));
#88117=CARTESIAN_POINT('Ctrl Pts',(10.6833753682069,-22.3727050906066,-2.82858037372522));
#88118=CARTESIAN_POINT('Ctrl Pts',(10.6867948611643,-22.3734203140874,-2.81532467090519));
#88119=CARTESIAN_POINT('Ctrl Pts',(10.6902269714035,-22.3738442904274,-2.80170567475361));
#88120=CARTESIAN_POINT('Ctrl Pts',(10.6937740147699,-22.3740583609835,-2.78768927445374));
#88121=CARTESIAN_POINT('Ctrl Pts',(10.6958203922006,-22.3741818636051,-2.77960286493741));
#88122=CARTESIAN_POINT('Ctrl Pts',(10.6979058195049,-22.3742356128001,-2.77138381588323));
#88123=CARTESIAN_POINT('Ctrl Pts',(10.7000575594,-22.3742356128,-2.76302312605));
#88124=CARTESIAN_POINT('Origin',(10.7018662383156,-22.6721143297048,-2.76413150880985));
#88125=CARTESIAN_POINT('Origin',(10.3289417811658,-22.0742353985912,-3.34331623669745));
#88126=CARTESIAN_POINT('Origin',(-2.84607155346,-22.6742356128,5.53854202767));
#88127=CARTESIAN_POINT('Origin',(10.9449284019752,-22.6742356128,-2.34954507716718));
#88128=CARTESIAN_POINT('Ctrl Pts',(11.2053401891,-22.6742356128,-2.49849372966));
#88129=CARTESIAN_POINT('Ctrl Pts',(11.2053401891,-22.5799878332,-2.49849372966));
#88130=CARTESIAN_POINT('Ctrl Pts',(11.1732131726,-22.4857400536,-2.48011792621));
#88131=CARTESIAN_POINT('Ctrl Pts',(11.1085499535,-22.4112466293,-2.44313227564));
#88132=CARTESIAN_POINT('Ctrl Pts',(11.0267391777,-22.3742356128,-2.39633867638));
#88133=CARTESIAN_POINT('Ctrl Pts',(10.9449284019,-22.3742356128,-2.34954507713));
#88134=CARTESIAN_POINT('Ctrl Pts',(11.2476948874,-22.6742356128,-2.42444362923));
#88135=CARTESIAN_POINT('Ctrl Pts',(11.2450653313,-22.5840941242,-2.429040968));
#88136=CARTESIAN_POINT('Ctrl Pts',(11.2130113811,-22.4939526355,-2.41703302845));
#88137=CARTESIAN_POINT('Ctrl Pts',(11.1517699452,-22.4209218727,-2.38727936284));
#88138=CARTESIAN_POINT('Ctrl Pts',(11.0744430753,-22.3806857596,-2.34601859644));
#88139=CARTESIAN_POINT('Ctrl Pts',(10.9959501219,-22.3742356128,-2.30169489009));
#88140=CARTESIAN_POINT('Ctrl Pts',(11.2941946283,-22.6686213022,-2.34203463014));
#88141=CARTESIAN_POINT('Ctrl Pts',(11.2868586676,-22.5829413188,-2.35499473105));
#88142=CARTESIAN_POINT('Ctrl Pts',(11.2526857413,-22.4972613355,-2.35302785728));
#88143=CARTESIAN_POINT('Ctrl Pts',(11.1928402247,-22.426280398,-2.33351209766));
#88144=CARTESIAN_POINT('Ctrl Pts',(11.1189291588,-22.3836825181,-2.2998966476));
#88145=CARTESIAN_POINT('Ctrl Pts',(11.043868081,-22.3714284849,-2.25918468729));
#88146=CARTESIAN_POINT('Ctrl Pts',(11.3417981924,-22.6467118109,-2.25595171063));
#88147=CARTESIAN_POINT('Ctrl Pts',(11.3291442479,-22.5660000486,-2.27877967267));
#88148=CARTESIAN_POINT('Ctrl Pts',(11.2910933501,-22.4852882864,-2.28766776945));
#88149=CARTESIAN_POINT('Ctrl Pts',(11.229550879,-22.4176465288,-2.27867532762));
#88150=CARTESIAN_POINT('Ctrl Pts',(11.1557537306,-22.375311083,-2.25331234023));
#88151=CARTESIAN_POINT('Ctrl Pts',(11.0817600114,-22.3604736068,-2.21745676256));
#88152=CARTESIAN_POINT('Ctrl Pts',(11.4353537652,-22.5603047021,-2.08352845036));
#88153=CARTESIAN_POINT('Ctrl Pts',(11.4121163918,-22.4942390833,-2.12677174602));
#88154=CARTESIAN_POINT('Ctrl Pts',(11.3657157526,-22.4281734646,-2.15766880717));
#88155=CARTESIAN_POINT('Ctrl Pts',(11.2994862528,-22.3717132431,-2.16962607727));
#88156=CARTESIAN_POINT('Ctrl Pts',(11.2242843437,-22.3339703351,-2.16051799049));
#88157=CARTESIAN_POINT('Ctrl Pts',(11.1508960681,-22.3172702763,-2.13427099913));
#88158=CARTESIAN_POINT('Ctrl Pts',(11.5032693058,-22.4004263802,-1.95414386857));
#88159=CARTESIAN_POINT('Ctrl Pts',(11.4721201637,-22.3564749274,-2.01366537708));
#88160=CARTESIAN_POINT('Ctrl Pts',(11.418463566,-22.3125234745,-2.06143417372));
#88161=CARTESIAN_POINT('Ctrl Pts',(11.3465841747,-22.2747985542,-2.0888955933));
#88162=CARTESIAN_POINT('Ctrl Pts',(11.2678343078,-22.2492105131,-2.09172776553));
#88163=CARTESIAN_POINT('Ctrl Pts',(11.1928782665,-22.237330862,-2.07277075552));
#88164=CARTESIAN_POINT('Ctrl Pts',(11.5284593408,-22.2976444921,-1.90521795022));
#88165=CARTESIAN_POINT('Ctrl Pts',(11.4944206426,-22.2676340437,-1.97094002685));
#88166=CARTESIAN_POINT('Ctrl Pts',(11.4380739731,-22.2376235953,-2.02511044406));
#88167=CARTESIAN_POINT('Ctrl Pts',(11.3640715597,-22.2118199507,-2.05839415541));
#88168=CARTESIAN_POINT('Ctrl Pts',(11.283947635,-22.1942244807,-2.0655995494));
#88169=CARTESIAN_POINT('Ctrl Pts',(11.208324537,-22.1859402315,-2.04918926595));
#88170=CARTESIAN_POINT('Ctrl Pts',(11.5410916547,-22.1859264501,-1.88073379583));
#88171=CARTESIAN_POINT('Ctrl Pts',(11.5055896574,-22.1709238273,-1.9495777849));
#88172=CARTESIAN_POINT('Ctrl Pts',(11.4478685938,-22.1559212045,-2.00696368603));
#88173=CARTESIAN_POINT('Ctrl Pts',(11.3727622471,-22.1430213573,-2.04316893107));
#88174=CARTESIAN_POINT('Ctrl Pts',(11.2919149591,-22.1342242685,-2.05258032919));
#88175=CARTESIAN_POINT('Ctrl Pts',(11.2159437174,-22.1300808784,-2.0374723572));
#88176=CARTESIAN_POINT('Ctrl Pts',(11.5410916367,-22.0742358827,-1.88073379256));
#88177=CARTESIAN_POINT('Ctrl Pts',(11.5055896399,-22.0742358104,-1.94957779219));
#88178=CARTESIAN_POINT('Ctrl Pts',(11.4478685736,-22.0742357381,-2.00696370221));
#88179=CARTESIAN_POINT('Ctrl Pts',(11.3727622216,-22.074235676,-2.04316895153));
#88180=CARTESIAN_POINT('Ctrl Pts',(11.2919149284,-22.0742356336,-2.05258034776));
#88181=CARTESIAN_POINT('Ctrl Pts',(11.2159436836,-22.0742356136,-2.03747236903));
#88182=CARTESIAN_POINT('',(11.2159436600663,-22.0742356133472,-2.03747240750538));
#88183=CARTESIAN_POINT('Ctrl Pts',(10.9449284019,-22.3742356128,-2.34954507713));
#88184=CARTESIAN_POINT('Ctrl Pts',(10.9555579269,-22.3742356128,-2.33957628816333));
#88185=CARTESIAN_POINT('Ctrl Pts',(10.9660214617852,-22.3740877440668,-2.32988311338671));
#88186=CARTESIAN_POINT('Ctrl Pts',(10.9762103266067,-22.3736977371534,-2.3203917889783));
#88187=CARTESIAN_POINT('Ctrl Pts',(10.9866077289775,-22.3732997478899,-2.31070620372078));
#88188=CARTESIAN_POINT('Ctrl Pts',(10.99671966122,-22.3726496161805,-2.30123099399582));
#88189=CARTESIAN_POINT('Ctrl Pts',(11.006479915341,-22.3716678922283,-2.29191758434368));
#88190=CARTESIAN_POINT('Ctrl Pts',(11.0167560942109,-22.3706342745777,-2.28211187003672));
#88191=CARTESIAN_POINT('Ctrl Pts',(11.0266429407752,-22.3692329814202,-2.27248559795379));
#88192=CARTESIAN_POINT('Ctrl Pts',(11.0361092934492,-22.3673949047112,-2.26301295646525));
#88193=CARTESIAN_POINT('Ctrl Pts',(11.0462075675716,-22.3654341281477,-2.2529079737218));
#88194=CARTESIAN_POINT('Ctrl Pts',(11.0558281166974,-22.3629761417554,-2.24297794072533));
#88195=CARTESIAN_POINT('Ctrl Pts',(11.0649742091976,-22.3599654715829,-2.23322425948526));
#88196=CARTESIAN_POINT('Ctrl Pts',(11.0752293070643,-22.3565897439415,-2.22228789997717));
#88197=CARTESIAN_POINT('Ctrl Pts',(11.0848893155074,-22.3525186606634,-2.21157331885061));
#88198=CARTESIAN_POINT('Ctrl Pts',(11.0939918679988,-22.3477145948015,-2.20112134524111));
#88199=CARTESIAN_POINT('Ctrl Pts',(11.1031456188729,-22.3428835079033,-2.19061058327036));
#88200=CARTESIAN_POINT('Ctrl Pts',(11.1117380324015,-22.3373113929668,-2.18036628908064));
#88201=CARTESIAN_POINT('Ctrl Pts',(11.1198079816964,-22.3309999394505,-2.17045843415635));
#88202=CARTESIAN_POINT('Ctrl Pts',(11.1271861983587,-22.3252294854122,-2.16139985180119));
#88203=CARTESIAN_POINT('Ctrl Pts',(11.1341290619681,-22.3188416151799,-2.1526233573693));
#88204=CARTESIAN_POINT('Ctrl Pts',(11.1406408102254,-22.3118641259116,-2.14419334888398));
#88205=CARTESIAN_POINT('Ctrl Pts',(11.1491541793956,-22.3027418534165,-2.13317207295198));
#88206=CARTESIAN_POINT('Ctrl Pts',(11.1569273589696,-22.2926111216346,-2.12274422351284));
#88207=CARTESIAN_POINT('Ctrl Pts',(11.1639866875261,-22.2815665889067,-2.11305404282817));
#88208=CARTESIAN_POINT('Ctrl Pts',(11.1713496846492,-22.2700469575351,-2.10294702316865));
#88209=CARTESIAN_POINT('Ctrl Pts',(11.177935601256,-22.2575335578597,-2.09364320727755));
#88210=CARTESIAN_POINT('Ctrl Pts',(11.1837492551854,-22.2441835831467,-2.08529357693297));
#88211=CARTESIAN_POINT('Ctrl Pts',(11.1898122988749,-22.2302609312447,-2.0765857704167));
#88212=CARTESIAN_POINT('Ctrl Pts',(11.1950346999939,-22.2154289170774,-2.06891671406967));
#88213=CARTESIAN_POINT('Ctrl Pts',(11.1994045937774,-22.1999120981238,-2.06243120336764));
#88214=CARTESIAN_POINT('Ctrl Pts',(11.203749759914,-22.1844830832312,-2.05598239182281));
#88215=CARTESIAN_POINT('Ctrl Pts',(11.2072511776712,-22.1683779027648,-2.05070452963748));
#88216=CARTESIAN_POINT('Ctrl Pts',(11.2098925170254,-22.151850614658,-2.04670170035793));
#88217=CARTESIAN_POINT('Ctrl Pts',(11.2124164316883,-22.1360580718618,-2.04287682284054));
#88218=CARTESIAN_POINT('Ctrl Pts',(11.2141543672614,-22.1198809963637,-2.04021647547921));
#88219=CARTESIAN_POINT('Ctrl Pts',(11.215098859081,-22.1035583375612,-2.03876892570883));
#88220=CARTESIAN_POINT('Ctrl Pts',(11.2156624545062,-22.0938183105583,-2.03790514646659));
#88221=CARTESIAN_POINT('Ctrl Pts',(11.2159437036462,-22.0840267162861,-2.0374723697639));
#88222=CARTESIAN_POINT('Ctrl Pts',(11.2159436836,-22.0742356136,-2.03747236903));
#88223=CARTESIAN_POINT('Origin',(11.275394600458,-22.0742358814361,-1.74517805615967));
#88224=CARTESIAN_POINT('Origin',(11.2744572343,-19.6742356128,-1.7432341771));
#88225=CARTESIAN_POINT('Origin',(11.2744572343,-19.6742356128,-1.7432341771));
#88226=CARTESIAN_POINT('Origin',(11.2744572343,-21.2742356128,-1.7432341771));
#88227=CARTESIAN_POINT('',(11.2159436339,-20.8742356128,-2.03747244546));
#88228=CARTESIAN_POINT('Origin',(10.3267865236,-21.2742356128,-3.3434289261));
#88229=CARTESIAN_POINT('',(10.5566756949,-20.8742356128,-3.15068305993));
#88230=CARTESIAN_POINT('Origin',(10.3267865236,-19.6742356128,-3.3434289261));
#88231=CARTESIAN_POINT('Origin',(3.05,-19.6742356128,15.662287998));
#88232=CARTESIAN_POINT('',(2.75,-19.6742356128,15.662287998));
#88233=CARTESIAN_POINT('Origin',(3.05,-19.6742356128,15.662287998));
#88234=CARTESIAN_POINT('Origin',(3.05,-19.6742356128,15.662287998));
#88235=CARTESIAN_POINT('',(2.97246042119851,-19.3848539651149,15.6779684221767));
#88236=CARTESIAN_POINT('Origin',(3.05,-19.6742356128,15.662287998));
#88237=CARTESIAN_POINT('Origin',(3.05,-19.6742356128,2.96634320571));
#88238=CARTESIAN_POINT('',(3.05,-19.3742356128,10.7304528845));
#88239=CARTESIAN_POINT('',(3.05,-19.3742356128,13.1963704412));
#88240=CARTESIAN_POINT('Origin',(3.05,-19.6742356128,10.7304528845));
#88241=CARTESIAN_POINT('',(2.75,-19.6742356128,13.1963704412));
#88242=CARTESIAN_POINT('Origin',(3.05,-22.4223864096,15.662287998));
#88243=CARTESIAN_POINT('',(2.75,-20.6742356128027,15.662287996875));
#88244=CARTESIAN_POINT('',(2.75,-20.1742356128,15.662287998));
#88245=CARTESIAN_POINT('',(3.10946375819699,-20.6742355012686,15.9563357201073));
#88246=CARTESIAN_POINT('Origin',(3.05000000000001,-20.6742355569137,15.662287998));
#88247=CARTESIAN_POINT('',(3.109463736,-21.2742356128,15.9563357222));
#88248=CARTESIAN_POINT('Origin',(2.75,-19.3742356128,10.4304528845));
#88249=CARTESIAN_POINT('',(2.75,-20.6742356128,13.3490218086));
#88250=CARTESIAN_POINT('Ctrl Pts',(3.1094637805,-20.6742355012,15.9563357204));
#88251=CARTESIAN_POINT('Ctrl Pts',(3.00535146138,-20.6742355416,15.9773898081));
#88252=CARTESIAN_POINT('Ctrl Pts',(2.89192096986,-20.6742355819,15.9523656045));
#88253=CARTESIAN_POINT('Ctrl Pts',(2.7970110589,-20.6742356114,15.8747276156));
#88254=CARTESIAN_POINT('Ctrl Pts',(2.75000002192,-20.6742356209,15.7685078059));
#88255=CARTESIAN_POINT('Ctrl Pts',(2.75000002182,-20.6742356129,15.6622879962));
#88256=CARTESIAN_POINT('Ctrl Pts',(3.10946380353,-20.7613039297,15.9563357159));
#88257=CARTESIAN_POINT('Ctrl Pts',(3.00535147528,-20.7455779654,15.9773898056));
#88258=CARTESIAN_POINT('Ctrl Pts',(2.89192097435,-20.7298520012,15.9523656029));
#88259=CARTESIAN_POINT('Ctrl Pts',(2.79701105681,-20.7183575883,15.8747276131));
#88260=CARTESIAN_POINT('Ctrl Pts',(2.75000001886,-20.7146527462,15.7685078017));
#88261=CARTESIAN_POINT('Ctrl Pts',(2.75000002231,-20.7177698279,15.6622879905));
#88262=CARTESIAN_POINT('Ctrl Pts',(3.09336559174,-20.8484128662,15.9595900965));
#88263=CARTESIAN_POINT('Ctrl Pts',(2.99245619263,-20.8169453132,15.9798833716));
#88264=CARTESIAN_POINT('Ctrl Pts',(2.88234381849,-20.7854777603,15.9544199132));
#88265=CARTESIAN_POINT('Ctrl Pts',(2.78979771265,-20.7624813454,15.8769278231));
#88266=CARTESIAN_POINT('Ctrl Pts',(2.74323291398,-20.755077053,15.7712039881));
#88267=CARTESIAN_POINT('Ctrl Pts',(2.74210499444,-20.7613240613,15.6654801511));
#88268=CARTESIAN_POINT('Ctrl Pts',(3.0611129676,-20.9309303248,15.9661188953));
#88269=CARTESIAN_POINT('Ctrl Pts',(2.96663575098,-20.8849847431,15.9848817048));
#88270=CARTESIAN_POINT('Ctrl Pts',(2.86318716199,-20.8390391614,15.9585340485));
#88271=CARTESIAN_POINT('Ctrl Pts',(2.77538294467,-20.80528071,15.8813354034));
#88272=CARTESIAN_POINT('Ctrl Pts',(2.72969914456,-20.7940068531,15.7766097304));
#88273=CARTESIAN_POINT('Ctrl Pts',(2.72628672053,-20.8025832991,15.6718840609));
#88274=CARTESIAN_POINT('Ctrl Pts',(2.95857415151,-21.0968055424,15.9864129862));
#88275=CARTESIAN_POINT('Ctrl Pts',(2.883615269,-21.0232686806,16.0006863819));
#88276=CARTESIAN_POINT('Ctrl Pts',(2.80037813885,-20.9497318188,15.9717891925));
#88277=CARTESIAN_POINT('Ctrl Pts',(2.72731697454,-20.8948262684,15.8954574233));
#88278=CARTESIAN_POINT('Ctrl Pts',(2.68525006547,-20.8745215131,15.7936237677));
#88279=CARTESIAN_POINT('Ctrl Pts',(2.67599823713,-20.8855201685,15.6917901077));
#88280=CARTESIAN_POINT('Ctrl Pts',(2.802073414,-21.210145586,16.0157241263));
#88281=CARTESIAN_POINT('Ctrl Pts',(2.75443180074,-21.1206683319,16.0242286253));
#88282=CARTESIAN_POINT('Ctrl Pts',(2.69943877243,-21.0311910779,15.9921593039));
#88283=CARTESIAN_POINT('Ctrl Pts',(2.64793358485,-20.9628100879,15.9169517332));
#88284=CARTESIAN_POINT('Ctrl Pts',(2.61350648776,-20.9339674316,15.8187461919));
#88285=CARTESIAN_POINT('Ctrl Pts',(2.59924369788,-20.942191106,15.7205406559));
#88286=CARTESIAN_POINT('Ctrl Pts',(2.70443397686,-21.2527626391,16.0332525536));
#88287=CARTESIAN_POINT('Ctrl Pts',(2.67281955818,-21.1584143796,16.038616685));
#88288=CARTESIAN_POINT('Ctrl Pts',(2.63437509944,-21.0640661201,16.0048673446));
#88289=CARTESIAN_POINT('Ctrl Pts',(2.59591773658,-20.9910117695,15.9302754357));
#88290=CARTESIAN_POINT('Ctrl Pts',(2.56711899741,-20.9580670061,15.8340046748));
#88291=CARTESIAN_POINT('Ctrl Pts',(2.55135784288,-20.9634991119,15.7377339138));
#88292=CARTESIAN_POINT('Ctrl Pts',(2.60121936463,-21.2742356128,16.0507826341));
#88293=CARTESIAN_POINT('Ctrl Pts',(2.58568379068,-21.1783721495,16.0532881684));
#88294=CARTESIAN_POINT('Ctrl Pts',(2.56380921231,-21.0825086862,16.0180414277));
#88295=CARTESIAN_POINT('Ctrl Pts',(2.53876678585,-21.0074397583,15.9440093758));
#88296=CARTESIAN_POINT('Ctrl Pts',(2.51662240651,-20.9716977028,15.8494690665));
#88297=CARTESIAN_POINT('Ctrl Pts',(2.50073751227,-20.9742356128,15.7549287572));
#88298=CARTESIAN_POINT('Ctrl Pts',(2.49776595187,-21.2742356128,16.0674673138));
#88299=CARTESIAN_POINT('Ctrl Pts',(2.49776595187,-21.1799878332,16.0674673138));
#88300=CARTESIAN_POINT('Ctrl Pts',(2.49187306376,-21.0857400536,16.0309284411));
#88301=CARTESIAN_POINT('Ctrl Pts',(2.4800122327,-21.0112466293,15.9573853181));
#88302=CARTESIAN_POINT('Ctrl Pts',(2.46500611635,-20.9742356128,15.864339843));
#88303=CARTESIAN_POINT('Ctrl Pts',(2.45,-20.9742356128,15.7712943679));
#88304=CARTESIAN_POINT('',(2.45,-20.9742356128,15.7712943679));
#88305=CARTESIAN_POINT('Ctrl Pts',(2.75,-20.6742356128,15.6622879962));
#88306=CARTESIAN_POINT('Ctrl Pts',(2.75000002231,-20.7177698279,15.6622879905));
#88307=CARTESIAN_POINT('Ctrl Pts',(2.74210499444,-20.7613240613,15.6654801511));
#88308=CARTESIAN_POINT('Ctrl Pts',(2.72628672053,-20.8025832991,15.6718840609));
#88309=CARTESIAN_POINT('Ctrl Pts',(2.67599823713,-20.8855201685,15.6917901077));
#88310=CARTESIAN_POINT('Ctrl Pts',(2.59924369788,-20.942191106,15.7205406559));
#88311=CARTESIAN_POINT('Ctrl Pts',(2.55135784288,-20.9634991119,15.7377339138));
#88312=CARTESIAN_POINT('Ctrl Pts',(2.50073751227,-20.9742356128,15.7549287572));
#88313=CARTESIAN_POINT('Ctrl Pts',(2.45,-20.9742356128,15.7712943679));
#88314=CARTESIAN_POINT('',(2.49776595187,-21.2742356128,16.0674673138));
#88315=CARTESIAN_POINT('Origin',(2.45033775172211,-21.2721143211372,15.7733885986677));
#88316=CARTESIAN_POINT('Ctrl Pts',(3.10946378033133,-20.6742355013784,15.9563357204341));
#88317=CARTESIAN_POINT('Ctrl Pts',(3.10932768110122,-20.7015979331535,15.9563632431162));
#88318=CARTESIAN_POINT('Ctrl Pts',(3.10730450936222,-20.7288604793434,15.956772561971));
#88319=CARTESIAN_POINT('Ctrl Pts',(3.10345054269395,-20.7557624287955,15.9575502978747));
#88320=CARTESIAN_POINT('Ctrl Pts',(3.09926382748793,-20.7849870720104,15.958395182902));
#88321=CARTESIAN_POINT('Ctrl Pts',(3.09291696055621,-20.8137858925351,15.9596747192825));
#88322=CARTESIAN_POINT('Ctrl Pts',(3.08453096290127,-20.8418628784539,15.9613564337185));
#88323=CARTESIAN_POINT('Ctrl Pts',(3.07580203981782,-20.8710880059325,15.9631069178664));
#88324=CARTESIAN_POINT('Ctrl Pts',(3.06486464518896,-20.8995309366648,15.9652928813008));
#88325=CARTESIAN_POINT('Ctrl Pts',(3.05189543077425,-20.9269002090981,15.9678650667302));
#88326=CARTESIAN_POINT('Ctrl Pts',(3.03848325063018,-20.9552042836972,15.9705251055915));
#88327=CARTESIAN_POINT('Ctrl Pts',(3.02289902586137,-20.9823598229141,15.9735978967696));
#88328=CARTESIAN_POINT('Ctrl Pts',(3.00536632094155,-21.0080918248321,15.9770201456985));
#88329=CARTESIAN_POINT('Ctrl Pts',(2.99098985450783,-21.0291915503758,15.9798263211904));
#88330=CARTESIAN_POINT('Ctrl Pts',(2.97530407509012,-21.0493349218278,15.982867211148));
#88331=CARTESIAN_POINT('Ctrl Pts',(2.95843887653005,-21.0683954688054,15.9861059378342));
#88332=CARTESIAN_POINT('Ctrl Pts',(2.947268491013,-21.081019907062,15.988251054925));
#88333=CARTESIAN_POINT('Ctrl Pts',(2.93558083779082,-21.0931699793608,15.9904829195074));
#88334=CARTESIAN_POINT('Ctrl Pts',(2.92341504117381,-21.1048131353117,15.9927905019296));
#88335=CARTESIAN_POINT('Ctrl Pts',(2.90102154963683,-21.1262446060538,15.9970380517671));
#88336=CARTESIAN_POINT('Ctrl Pts',(2.87712998286052,-21.1457721989991,16.00151876457));
#88337=CARTESIAN_POINT('Ctrl Pts',(2.85200450801134,-21.1633257927321,16.0061638407846));
#88338=CARTESIAN_POINT('Ctrl Pts',(2.82373910759164,-21.1830730555658,16.0113894112455));
#88339=CARTESIAN_POINT('Ctrl Pts',(2.7939115527548,-21.2003241299158,16.0168230390457));
#88340=CARTESIAN_POINT('Ctrl Pts',(2.76283377953572,-21.2149836940284,16.0223832732222));
#88341=CARTESIAN_POINT('Ctrl Pts',(2.75087357606706,-21.2206253906942,16.0245231154694));
#88342=CARTESIAN_POINT('Ctrl Pts',(2.73872764677138,-21.2258831354447,16.0266818619891));
#88343=CARTESIAN_POINT('Ctrl Pts',(2.72641206839653,-21.2307506374264,16.0288553736645));
#88344=CARTESIAN_POINT('Ctrl Pts',(2.70470559779606,-21.2393297138976,16.032686234534));
#88345=CARTESIAN_POINT('Ctrl Pts',(2.68268567272168,-21.2466165494237,16.0365252973163));
#88346=CARTESIAN_POINT('Ctrl Pts',(2.66036444590225,-21.2526520015251,16.0403664154533));
#88347=CARTESIAN_POINT('Ctrl Pts',(2.63807259783438,-21.2586795098854,16.0442024779876));
#88348=CARTESIAN_POINT('Ctrl Pts',(2.61547922403521,-21.263459231883,16.0480407832021));
#88349=CARTESIAN_POINT('Ctrl Pts',(2.59257948477896,-21.2669830827316,16.0518780878269));
#88350=CARTESIAN_POINT('Ctrl Pts',(2.57021450818643,-21.2704246433914,16.0556257823816));
#88351=CARTESIAN_POINT('Ctrl Pts',(2.54755637811659,-21.2726683931181,16.0593726685482));
#88352=CARTESIAN_POINT('Ctrl Pts',(2.52459873201666,-21.2736576793356,16.0631159841377));
#88353=CARTESIAN_POINT('Ctrl Pts',(2.51569942332494,-21.2740411665362,16.0645670440946));
#88354=CARTESIAN_POINT('Ctrl Pts',(2.50675516073449,-21.2742356128,16.066017559107));
#88355=CARTESIAN_POINT('Ctrl Pts',(2.49776595187,-21.2742356128,16.0674673138));
#88356=CARTESIAN_POINT('Origin',(2.45,-20.6742356128,13.3490218086));
#88357=CARTESIAN_POINT('',(2.73249401778459,-20.7752152053705,10.7304528485382));
#88358=CARTESIAN_POINT('Origin',(2.45,-20.6742356128,10.7304528845));
#88359=CARTESIAN_POINT('',(2.73284184833111,-20.7742356128,10.7560440517756));
#88360=CARTESIAN_POINT('Origin',(2.6183724284568,-21.0942392385765,10.8006651610913));
#88361=CARTESIAN_POINT('',(2.7328425359048,-20.7742356128,14.7056612864094));
#88362=CARTESIAN_POINT('',(2.73284210357,-20.7742356128,12.7308526862));
#88363=CARTESIAN_POINT('',(2.45000000025794,-20.9742356128,15.0444077730863));
#88364=CARTESIAN_POINT('Ctrl Pts',(2.45000000065989,-20.9742356128,15.0444077754594));
#88365=CARTESIAN_POINT('Ctrl Pts',(2.45060618541105,-20.9742356127987,15.044305098672));
#88366=CARTESIAN_POINT('Ctrl Pts',(2.45121325755483,-20.9742337755027,15.0442015735626));
#88367=CARTESIAN_POINT('Ctrl Pts',(2.45286377483275,-20.9742237555269,15.0439181984608));
#88368=CARTESIAN_POINT('Ctrl Pts',(2.45390823845169,-20.9742119797694,15.0437368106927));
#88369=CARTESIAN_POINT('Ctrl Pts',(2.45715653062603,-20.9741583263579,15.0431662137099));
#88370=CARTESIAN_POINT('Ctrl Pts',(2.45936133985891,-20.9740976540959,15.0427696908689));
#88371=CARTESIAN_POINT('Ctrl Pts',(2.47380236930478,-20.97354037289,15.0401113790515));
#88372=CARTESIAN_POINT('Ctrl Pts',(2.4859522398806,-20.9723204874474,15.037590560837));
#88373=CARTESIAN_POINT('Ctrl Pts',(2.49792722488249,-20.9703825039116,15.0347954601431));
#88374=CARTESIAN_POINT('Ctrl Pts',(2.51978994719543,-20.9668443286334,15.0296924466282));
#88375=CARTESIAN_POINT('Ctrl Pts',(2.54102226288492,-20.9609132340753,15.0237041443004));
#88376=CARTESIAN_POINT('Ctrl Pts',(2.58663934051023,-20.9427190138178,15.0074386652922));
#88377=CARTESIAN_POINT('Ctrl Pts',(2.60989476914103,-20.9293629068578,14.9966041376225));
#88378=CARTESIAN_POINT('Ctrl Pts',(2.65288015563397,-20.8970213813152,14.9679758450514));
#88379=CARTESIAN_POINT('Ctrl Pts',(2.67115973053595,-20.8782900142092,14.9501370800874));
#88380=CARTESIAN_POINT('Ctrl Pts',(2.70119454675138,-20.8401597687455,14.9048926284374));
#88381=CARTESIAN_POINT('Ctrl Pts',(2.71168115894417,-20.8218448720293,14.8780286003523));
#88382=CARTESIAN_POINT('Ctrl Pts',(2.7267534339897,-20.791371833055,14.814608554777));
#88383=CARTESIAN_POINT('Ctrl Pts',(2.73059155074725,-20.7804840144795,14.7785359194907));
#88384=CARTESIAN_POINT('Ctrl Pts',(2.73261231507094,-20.7748951009433,14.7291853931118));
#88385=CARTESIAN_POINT('Ctrl Pts',(2.73284271201381,-20.7742356141034,14.7173522523963));
#88386=CARTESIAN_POINT('Ctrl Pts',(2.73284271247462,-20.7742356128,14.7056612864095));
#88387=CARTESIAN_POINT('',(2.45,-20.9742356128,15.4078510693));
#88388=CARTESIAN_POINT('Origin',(6.51383560964,-21.0742356128,10.9320666897));
#88389=CARTESIAN_POINT('',(4.98919124473,-20.7742356128,9.52235136777));
#88390=CARTESIAN_POINT('Origin',(4.98919124473,-21.0742356128,9.52235136777));
#88391=CARTESIAN_POINT('',(8.14487887576,-20.7742356128,12.4401604693));
#88392=CARTESIAN_POINT('Origin',(8.14487887576,-21.0742356128,12.4401604693));
#88393=CARTESIAN_POINT('',(6.56703506025,-20.7742356128,10.9812559186));
#88394=CARTESIAN_POINT('Origin',(4.98919124473,-21.0742356128,9.52235136777));
#88395=CARTESIAN_POINT('Origin',(4.98919124473,-21.0742356128,9.52235136777));
#88396=CARTESIAN_POINT('Origin',(0.00234331738803,-21.0742356128,3.08191746407));
#88397=CARTESIAN_POINT('',(1.01362103240136,-20.9742355987892,10.879187255885));
#88398=CARTESIAN_POINT('Origin',(1.05,-21.0742356128,11.1596805575));
#88399=CARTESIAN_POINT('Origin',(0.00234331738835,-20.7742356128,3.08191746407));
#88400=CARTESIAN_POINT('',(2.45,-20.9304376384,10.5743743079));
#88401=CARTESIAN_POINT('Ctrl Pts',(2.73249449536286,-20.7752151161147,10.7304528285094));
#88402=CARTESIAN_POINT('Ctrl Pts',(2.73245710700268,-20.7753197109045,10.7290952012981));
#88403=CARTESIAN_POINT('Ctrl Pts',(2.73240712664869,-20.7754319433538,10.727752397751));
#88404=CARTESIAN_POINT('Ctrl Pts',(2.73152298709635,-20.7771409318656,10.7087546905869));
#88405=CARTESIAN_POINT('Ctrl Pts',(2.72772545244807,-20.7809744979902,10.6881339522637));
#88406=CARTESIAN_POINT('Ctrl Pts',(2.71679996433014,-20.790736326335,10.6559122059645));
#88407=CARTESIAN_POINT('Ctrl Pts',(2.70771619875055,-20.7984214920223,10.6384138803735));
#88408=CARTESIAN_POINT('Ctrl Pts',(2.68765731828286,-20.8146185581327,10.6112737349406));
#88409=CARTESIAN_POINT('Ctrl Pts',(2.67249689114105,-20.8263682945712,10.5972506978324));
#88410=CARTESIAN_POINT('Ctrl Pts',(2.6394257692643,-20.8502432000307,10.5761069546454));
#88411=CARTESIAN_POINT('Ctrl Pts',(2.61427989630388,-20.866832947014,10.5673521750875));
#88412=CARTESIAN_POINT('Ctrl Pts',(2.57563645957671,-20.8884881384831,10.5611700175102));
#88413=CARTESIAN_POINT('Ctrl Pts',(2.55565602930822,-20.8983536598197,10.5602963146483));
#88414=CARTESIAN_POINT('Ctrl Pts',(2.51151087548647,-20.9166072793448,10.562148593287));
#88415=CARTESIAN_POINT('Ctrl Pts',(2.48028974593005,-20.925972433295,10.5670447011082));
#88416=CARTESIAN_POINT('Ctrl Pts',(2.45000000001651,-20.9304376384374,10.5743743079454));
#88417=CARTESIAN_POINT('',(1.82443157197449,-20.9742356128,10.7304528194434));
#88418=CARTESIAN_POINT('Ctrl Pts',(2.4500000000165,-20.9304376384374,10.5743743079454));
#88419=CARTESIAN_POINT('Ctrl Pts',(2.35301070638687,-20.9447354504351,10.5978440786011));
#88420=CARTESIAN_POINT('Ctrl Pts',(2.24920782247063,-20.9566073584057,10.6246065671936));
#88421=CARTESIAN_POINT('Ctrl Pts',(2.07922400989342,-20.9679537533597,10.6677900651879));
#88422=CARTESIAN_POINT('Ctrl Pts',(2.0255308573803,-20.9704953103501,10.6813308519351));
#88423=CARTESIAN_POINT('Ctrl Pts',(1.94060113457634,-20.9730149159474,10.7023545221609));
#88424=CARTESIAN_POINT('Ctrl Pts',(1.90970835320785,-20.9736270659681,10.7099231588312));
#88425=CARTESIAN_POINT('Ctrl Pts',(1.86062551950229,-20.9741422809688,10.7217960060706));
#88426=CARTESIAN_POINT('Ctrl Pts',(1.84256776105564,-20.9742356100387,10.7261321551956));
#88427=CARTESIAN_POINT('Ctrl Pts',(1.8244315417982,-20.9742356127999,10.7304526927731));
#88428=CARTESIAN_POINT('Origin',(0.00234331738803,-20.9742356128,3.08191746407));
#88429=CARTESIAN_POINT('Origin',(1.05,-21.0742356128,11.1596805575));
#88430=CARTESIAN_POINT('',(0.767157426230295,-20.9742355987887,11.1596805575));
#88431=CARTESIAN_POINT('Origin',(1.05,-20.9742356128,11.1596805575));
#88432=CARTESIAN_POINT('Origin',(1.05,-21.0742356128,11.1596805575));
#88433=CARTESIAN_POINT('Origin',(1.05,-21.0742356128,12.1167294155));
#88434=CARTESIAN_POINT('',(0.767157287525,-20.9742356128,14.92922515));
#88435=CARTESIAN_POINT('',(0.767157387839,-20.9742356128,13.0444528538));
#88436=CARTESIAN_POINT('Origin',(1.05,-21.0742356128,14.92922515));
#88437=CARTESIAN_POINT('Origin',(8.14487887576,-21.0742356128,12.4401604693));
#88438=CARTESIAN_POINT('Origin',(8.14487887576,-21.0742356128,12.4401604693));
#88439=CARTESIAN_POINT('Origin',(1.05,-21.0742356128,14.92922515));
#88440=CARTESIAN_POINT('',(1.07064182343228,-20.9742356126354,15.2113136364792));
#88441=CARTESIAN_POINT('Origin',(1.05,-20.9742356128,14.92922515));
#88442=CARTESIAN_POINT('Origin',(1.05,-21.0742356128,14.92922515));
#88443=CARTESIAN_POINT('Origin',(2.04268023839E-15,-21.0742356128,0.580061096523));
#88444=CARTESIAN_POINT('Origin',(1.14862552646E-15,-20.7742356128,0.580061096523));
#88445=CARTESIAN_POINT('Origin',(2.05492670639E-15,-20.9742356128,0.580061096523));
#88446=CARTESIAN_POINT('Origin',(2.93915231795E-16,-20.7742356128,0.729452270839));
#88447=CARTESIAN_POINT('Origin',(2.45,-20.6742356128,10.7304528845));
#88448=CARTESIAN_POINT('Origin',(2.45,-20.6742356128,10.7304528845));
#88449=CARTESIAN_POINT('Origin',(0.75,-23.1742356128,-8.70195642562));
#88450=CARTESIAN_POINT('',(0.74999999938425,-21.0742356128,-6.2343884565225));
#88451=CARTESIAN_POINT('',(0.75,-22.1242356128,-6.23438845923));
#88452=CARTESIAN_POINT('',(0.75,-21.0742356128,-4.99584562937));
#88453=CARTESIAN_POINT('',(0.75,-21.0742356128,-6.03615517446));
#88454=CARTESIAN_POINT('',(0.75,-22.1242356128,-4.99584562937));
#88455=CARTESIAN_POINT('Origin',(2.32682891838E-16,-21.2742356128,0.729452270839));
#88456=CARTESIAN_POINT('',(1.19254592572,-22.1242356128,5.7836191207));
#88457=CARTESIAN_POINT('',(0.992653804111,-22.1242356128,5.82664824081));
#88458=CARTESIAN_POINT('Origin',(1.05,-22.1242356128,6.12111625914));
#88459=CARTESIAN_POINT('',(0.75,-21.0742356128,6.12111625914));
#88460=CARTESIAN_POINT('Origin',(1.05,-21.0742356128,6.12111625914));
#88461=CARTESIAN_POINT('',(0.75,-21.9742356128,6.12111625914));
#88462=CARTESIAN_POINT('Origin',(0.75,-23.1742356128,-8.70195642562));
#88463=CARTESIAN_POINT('',(0.75,-21.0742356128,9.0358656718));
#88464=CARTESIAN_POINT('',(0.75,-21.0742356128,7.56406439184));
#88465=CARTESIAN_POINT('',(0.75,-22.1242356128,9.0358656718));
#88466=CARTESIAN_POINT('Origin',(1.05,-22.1242356128,9.0358656718));
#88467=CARTESIAN_POINT('',(1.10198928897,-21.0742356128,9.33132652171));
#88468=CARTESIAN_POINT('Origin',(1.05,-21.0742356128,9.0358656718));
#88469=CARTESIAN_POINT('',(1.10198928897,-21.2742356128,9.33132652171));
#88470=CARTESIAN_POINT('Origin',(0.00234331738835,-21.2742356128,3.08191746407));
#88471=CARTESIAN_POINT('Origin',(0.00234331738835,-21.0742356128,3.08191746407));
#88472=CARTESIAN_POINT('',(3.58772315463,-22.1242356128,8.31731489457));
#88473=CARTESIAN_POINT('Origin',(1.2614400074,-22.1242356128,6.07560132137));
#88474=CARTESIAN_POINT('',(1.46510738459,-21.9742356128,5.8553296721));
#88475=CARTESIAN_POINT('Origin',(3.41821282746,-22.1242356128,8.06979469543));
#88476=CARTESIAN_POINT('',(3.62188020465,-21.9742356128,7.84952304616));
#88477=CARTESIAN_POINT('Origin',(3.88971125292,-23.1742356128,8.09716475273));
#88478=CARTESIAN_POINT('Origin',(0.00234331738835,-21.2742356128,3.08191746407));
#88479=CARTESIAN_POINT('',(6.21380646358,-22.1242356128,1.78497474518));
#88480=CARTESIAN_POINT('',(5.76218263052,-22.1242356128,0.419477620705));
#88481=CARTESIAN_POINT('Origin',(5.48986775992,-22.1242356128,0.545353000555));
#88482=CARTESIAN_POINT('',(5.1900363009,-21.9742356128,0.55540766038));
#88483=CARTESIAN_POINT('Origin',(2.32682891838E-16,-21.2742356128,0.729452270839));
#88484=CARTESIAN_POINT('',(5.08448267152,-22.1242356128,1.78529520144));
#88485=CARTESIAN_POINT('Origin',(5.92013962829,-22.1242356128,1.84629187045));
#88486=CARTESIAN_POINT('',(5.92013962829,-21.9742356128,2.14629187045));
#88487=CARTESIAN_POINT('Origin',(5.3782162351,-22.1242356128,1.84629187045));
#88488=CARTESIAN_POINT('',(5.3782162351,-21.9742356128,2.14629187045));
#88489=CARTESIAN_POINT('Origin',(-11.4443506127,-23.1742356128,2.14629187045));
#88490=CARTESIAN_POINT('Origin',(2.32682891838E-16,-21.2742356128,0.729452270839));
#88491=CARTESIAN_POINT('',(4.2092958712,-22.1242356128,3.77060280966));
#88492=CARTESIAN_POINT('',(3.13117783752,-22.1242356128,4.87221628548));
#88493=CARTESIAN_POINT('Origin',(3.31206782846,-22.1242356128,5.11154620667));
#88494=CARTESIAN_POINT('',(3.10840045127,-21.9742356128,5.33181785593));
#88495=CARTESIAN_POINT('Origin',(9.80058174751,-23.1742356128,11.519536597));
#88496=CARTESIAN_POINT('',(4.71627105755,-22.1242356128,6.81848575139));
#88497=CARTESIAN_POINT('Origin',(4.91993843473,-22.1242356128,6.59821410213));
#88498=CARTESIAN_POINT('',(5.16397092918,-21.0742356128,6.77270806092));
#88499=CARTESIAN_POINT('Origin',(4.91993843473,-21.0742356128,6.59821410213));
#88500=CARTESIAN_POINT('',(5.16397092918,-21.2742356128,6.77270806092));
#88501=CARTESIAN_POINT('Origin',(0.00234331738835,-21.2742356128,3.08191746407));
#88502=CARTESIAN_POINT('',(6.28256615006,-21.0742356128,3.98918589435));
#88503=CARTESIAN_POINT('Origin',(0.00234331738835,-21.0742356128,3.08191746407));
#88504=CARTESIAN_POINT('',(6.28256615006,-22.1242356128,3.98918589435));
#88505=CARTESIAN_POINT('Origin',(4.452469377,-22.1242356128,3.94629187045));
#88506=CARTESIAN_POINT('',(4.452469377,-21.0742356128,3.64629187045));
#88507=CARTESIAN_POINT('',(4.452469377,-21.9742356128,3.64629187045));
#88508=CARTESIAN_POINT('Origin',(4.452469377,-21.0742356128,3.94629187045));
#88509=CARTESIAN_POINT('Origin',(5.98564848014,-22.1242356128,3.94629187045));
#88510=CARTESIAN_POINT('',(5.98564848014,-21.0742356128,3.64629187045));
#88511=CARTESIAN_POINT('Origin',(5.98564848014,-21.0742356128,3.94629187045));
#88512=CARTESIAN_POINT('',(5.98564848014,-21.9742356128,3.64629187045));
#88513=CARTESIAN_POINT('Origin',(-11.7190551593,-23.1742356128,3.64629187045));
#88514=CARTESIAN_POINT('',(-4.57919858809,-21.0742356128,3.64629187045));
#88515=CARTESIAN_POINT('Origin',(4.91993843473,-21.0742356128,6.59821410213));
#88516=CARTESIAN_POINT('Origin',(4.91993843473,-21.0742356128,6.59821410213));
#88517=CARTESIAN_POINT('Origin',(0.00234331738835,-21.0742356128,3.08191746407));
#88518=CARTESIAN_POINT('',(5.98564848014,-20.7742356128,3.94629187045));
#88519=CARTESIAN_POINT('Origin',(0.00234331738835,-20.7742356128,3.08191746407));
#88520=CARTESIAN_POINT('Ctrl Pts',(5.98564848014,-20.7742356128,3.94629187045));
#88521=CARTESIAN_POINT('Ctrl Pts',(6.00325376366273,-20.7742356128,3.94883520662962));
#88522=CARTESIAN_POINT('Ctrl Pts',(6.02086151892848,-20.7758219937196,3.95137159218802));
#88523=CARTESIAN_POINT('Ctrl Pts',(6.03819046933219,-20.7789698139932,3.95387127852019));
#88524=CARTESIAN_POINT('Ctrl Pts',(6.05551616145726,-20.7821170423974,3.95637049484844));
#88525=CARTESIAN_POINT('Ctrl Pts',(6.07256227259131,-20.7868248395128,3.95883357428083));
#88526=CARTESIAN_POINT('Ctrl Pts',(6.0890604606157,-20.7930184980419,3.96122159453396));
#88527=CARTESIAN_POINT('Ctrl Pts',(6.10203541218976,-20.7978894826229,3.96309964605673));
#88528=CARTESIAN_POINT('Ctrl Pts',(6.11467162344997,-20.8036783444377,3.96493111746659));
#88529=CARTESIAN_POINT('Ctrl Pts',(6.12684913512964,-20.8103298005963,3.96669033401031));
#88530=CARTESIAN_POINT('Ctrl Pts',(6.14176502552207,-20.8184769815329,3.96884514870751));
#88531=CARTESIAN_POINT('Ctrl Pts',(6.15599039473335,-20.8279195594011,3.97089881512368));
#88532=CARTESIAN_POINT('Ctrl Pts',(6.16931229547304,-20.8385161827716,3.97282398767375));
#88533=CARTESIAN_POINT('Ctrl Pts',(6.17525926176098,-20.8432465709633,3.9736833947867));
#88534=CARTESIAN_POINT('Ctrl Pts',(6.18102680506576,-20.8482065514678,3.97451707692433));
#88535=CARTESIAN_POINT('Ctrl Pts',(6.18659908662289,-20.8533824917211,3.97532207306466));
#88536=CARTESIAN_POINT('Ctrl Pts',(6.19562650893926,-20.8617678179239,3.97662621393537));
#88537=CARTESIAN_POINT('Ctrl Pts',(6.2041391134579,-20.87071888487,3.97785598197763));
#88538=CARTESIAN_POINT('Ctrl Pts',(6.21207169969898,-20.880167130521,3.97900195804526));
#88539=CARTESIAN_POINT('Ctrl Pts',(6.21603799281952,-20.8848912533465,3.97957494607907));
#88540=CARTESIAN_POINT('Ctrl Pts',(6.21985942235242,-20.8897395549112,3.98012700648607));
#88541=CARTESIAN_POINT('Ctrl Pts',(6.22352864890558,-20.8947027251433,3.98065707898559));
#88542=CARTESIAN_POINT('Ctrl Pts',(6.22536326218216,-20.8971843102593,3.98092211523535));
#88543=CARTESIAN_POINT('Ctrl Pts',(6.22715983319936,-20.8996946046435,3.98118165573411));
#88544=CARTESIAN_POINT('Ctrl Pts',(6.22891750090729,-20.9022324050138,3.98143557609082));
#88545=CARTESIAN_POINT('Ctrl Pts',(6.22992901378548,-20.9036928731929,3.98158170366073));
#88546=CARTESIAN_POINT('Ctrl Pts',(6.23113763302248,-20.905473872797,3.98176162924324));
#88547=CARTESIAN_POINT('Ctrl Pts',(6.23217750243642,-20.9070389005777,3.98191069395136));
#88548=CARTESIAN_POINT('Ctrl Pts',(6.2329445748111,-20.9081933624361,3.98202065335406));
#88549=CARTESIAN_POINT('Ctrl Pts',(6.23362112590207,-20.909229675745,3.98211508230871));
#88550=CARTESIAN_POINT('Ctrl Pts',(6.23407297039883,-20.9099270947014,3.98218035773892));
#88551=CARTESIAN_POINT('Ctrl Pts',(6.24140060621849,-20.9212372515438,3.98323894002544));
#88552=CARTESIAN_POINT('Ctrl Pts',(6.24797445346109,-20.9330497413319,3.98416457610613));
#88553=CARTESIAN_POINT('Ctrl Pts',(6.25373323382676,-20.9452535591513,3.9849466848626));
#88554=CARTESIAN_POINT('Ctrl Pts',(6.2546664150874,-20.9472311261662,3.98507342163479));
#88555=CARTESIAN_POINT('Ctrl Pts',(6.25557826501334,-20.9492190377732,3.98519644133876));
#88556=CARTESIAN_POINT('Ctrl Pts',(6.25646859717888,-20.9512169122126,3.98531575432681));
#88557=CARTESIAN_POINT('Ctrl Pts',(6.25966093983393,-20.9583804181927,3.98574355864053));
#88558=CARTESIAN_POINT('Ctrl Pts',(6.26257588740962,-20.965670468392,3.98612291044023));
#88559=CARTESIAN_POINT('Ctrl Pts',(6.26520446752445,-20.9730645987735,3.98645249592255));
#88560=CARTESIAN_POINT('Ctrl Pts',(6.26632784754956,-20.9762246387991,3.98659335133924));
#88561=CARTESIAN_POINT('Ctrl Pts',(6.26746961610877,-20.9796167701875,3.98674544026523));
#88562=CARTESIAN_POINT('Ctrl Pts',(6.26853189014378,-20.9829670042927,3.98687533316301));
#88563=CARTESIAN_POINT('Ctrl Pts',(6.26964178137131,-20.9864674150351,3.98701104860272));
#88564=CARTESIAN_POINT('Ctrl Pts',(6.2706648700053,-20.9899217568917,3.98712247524996));
#88565=CARTESIAN_POINT('Ctrl Pts',(6.27152961786085,-20.9930121729073,3.98721531003455));
#88566=CARTESIAN_POINT('Ctrl Pts',(6.27177382310526,-20.9938849079983,3.98724152662603));
#88567=CARTESIAN_POINT('Ctrl Pts',(6.27200562645505,-20.9947286067318,3.98726650908391));
#88568=CARTESIAN_POINT('Ctrl Pts',(6.27222388875607,-20.9955360948653,3.98729090767503));
#88569=CARTESIAN_POINT('Ctrl Pts',(6.2754008551609,-21.0072896714587,3.98764604689953));
#88570=CARTESIAN_POINT('Ctrl Pts',(6.27785776815197,-21.0192458614175,3.98798398659007));
#88571=CARTESIAN_POINT('Ctrl Pts',(6.27957628318323,-21.0313012257436,3.98828097625466));
#88572=CARTESIAN_POINT('Ctrl Pts',(6.28145475340164,-21.0444786739747,3.98860560899279));
#88573=CARTESIAN_POINT('Ctrl Pts',(6.28245216396942,-21.0577747139993,3.98888156993282));
#88574=CARTESIAN_POINT('Ctrl Pts',(6.28255779916532,-21.0710863072773,3.98912804850833));
#88575=CARTESIAN_POINT('Ctrl Pts',(6.28256612893013,-21.0721359805447,3.98914748434642));
#88576=CARTESIAN_POINT('Ctrl Pts',(6.28256891438073,-21.0731857638459,3.98916675941873));
#88577=CARTESIAN_POINT('Ctrl Pts',(6.28256615006486,-21.0742356128,3.9891858943507));
#88578=CARTESIAN_POINT('Origin',(4.452469377,-21.0742356128,3.94629187045));
#88579=CARTESIAN_POINT('Origin',(4.452469377,-21.0742356128,3.94629187045));
#88580=CARTESIAN_POINT('Origin',(5.98564848014,-21.0742356128,3.94629187045));
#88581=CARTESIAN_POINT('Origin',(5.98564848014,-21.0742356128,3.94629187045));
#88582=CARTESIAN_POINT('Origin',(-4.57919858809,-21.0742356128,3.94629187045));
#88583=CARTESIAN_POINT('',(5.21905892857,-20.7742356128,3.94629187045));
#88584=CARTESIAN_POINT('Origin',(2.93915231795E-16,-20.7742356128,0.729452270839));
#88585=CARTESIAN_POINT('',(1.05,-20.7742356128,9.0358656718));
#88586=CARTESIAN_POINT('',(1.05,-20.7742356128,7.56406439184));
#88587=CARTESIAN_POINT('Origin',(0.00234331738835,-20.7742356128,3.08191746407));
#88588=CARTESIAN_POINT('Origin',(10.3267865236,-19.6742356128,-3.3434289261));
#88589=CARTESIAN_POINT('Origin',(1.05,-21.0742356128,-4.99584562937));
#88590=CARTESIAN_POINT('',(1.01141425905,-21.0742356128,-4.69833741));
#88591=CARTESIAN_POINT('Origin',(1.05,-21.0742356128,-4.99584562937));
#88592=CARTESIAN_POINT('',(1.05,-20.7742356128,-4.99584562937));
#88593=CARTESIAN_POINT('Origin',(1.05,-21.0742356128,-4.99584562937));
#88594=CARTESIAN_POINT('Origin',(1.05,-21.0742356128,-4.99584562937));
#88595=CARTESIAN_POINT('Origin',(2.93915231795E-16,-20.7742356128,0.729452270839));
#88596=CARTESIAN_POINT('Origin',(2.93915231795E-16,-20.7742356128,0.729452270839));
#88597=CARTESIAN_POINT('Origin',(1.05,-22.1242356128,-4.99584562937));
#88598=CARTESIAN_POINT('',(1.01141425905,-21.2742356128,-4.69833741));
#88599=CARTESIAN_POINT('Origin',(11.0821857629,-20.8742356128,-2.71007990903));
#88600=CARTESIAN_POINT('Origin',(11.0821857629,-22.0742356128,-2.71007990903));
#88601=CARTESIAN_POINT('Origin',(1.05,-21.0742356128,6.12111625914));
#88602=CARTESIAN_POINT('Origin',(1.05,-21.0742356128,6.12111625914));
#88603=CARTESIAN_POINT('Origin',(0.00234331738835,-21.0742356128,3.08191746407));
#88604=CARTESIAN_POINT('Ctrl Pts',(1.05,-20.7742356128,9.0358656718));
#88605=CARTESIAN_POINT('Ctrl Pts',(1.05194346679646,-20.7742356127999,9.04691060744439));
#88606=CARTESIAN_POINT('Ctrl Pts',(1.05373571268161,-20.7748621802049,9.05721123155974));
#88607=CARTESIAN_POINT('Ctrl Pts',(1.05539004573013,-20.7758744125586,9.0667127620523));
#88608=CARTESIAN_POINT('Ctrl Pts',(1.05664195232833,-20.7766404133126,9.07390298818438));
#88609=CARTESIAN_POINT('Ctrl Pts',(1.05781511495567,-20.7776277333487,9.08063685240658));
#88610=CARTESIAN_POINT('Ctrl Pts',(1.05891817857726,-20.7787438986221,9.08690601609574));
#88611=CARTESIAN_POINT('Ctrl Pts',(1.06019853257273,-20.780039460038,9.09418279380878));
#88612=CARTESIAN_POINT('Ctrl Pts',(1.06137963728991,-20.7815082048312,9.10083598740895));
#88613=CARTESIAN_POINT('Ctrl Pts',(1.0624569555597,-20.783027573221,9.1068776662104));
#88614=CARTESIAN_POINT('Ctrl Pts',(1.06292348574346,-20.7836855321863,9.10949400123461));
#88615=CARTESIAN_POINT('Ctrl Pts',(1.0633037229392,-20.7842538831696,9.1116194090953));
#88616=CARTESIAN_POINT('Ctrl Pts',(1.06368406010907,-20.7848444845195,9.11374713142444));
#88617=CARTESIAN_POINT('Ctrl Pts',(1.0640510629429,-20.7854143798288,9.11580025740389));
#88618=CARTESIAN_POINT('Ctrl Pts',(1.06441817676359,-20.7860052807807,9.1178556394656));
#88619=CARTESIAN_POINT('Ctrl Pts',(1.06486103473096,-20.7867597488703,9.12034512089835));
#88620=CARTESIAN_POINT('Ctrl Pts',(1.06501903860616,-20.7870289297153,9.12123332375928));
#88621=CARTESIAN_POINT('Ctrl Pts',(1.06518666287036,-20.7873193387291,9.12217666319411));
#88622=CARTESIAN_POINT('Ctrl Pts',(1.06536725084921,-20.7876390838914,9.12319423081729));
#88623=CARTESIAN_POINT('Ctrl Pts',(1.06687631132471,-20.7903109936706,9.13169740523177));
#88624=CARTESIAN_POINT('Ctrl Pts',(1.06834277231229,-20.7933703249366,9.14006063447592));
#88625=CARTESIAN_POINT('Ctrl Pts',(1.06975205420403,-20.7967336412273,9.14812658276299));
#88626=CARTESIAN_POINT('Ctrl Pts',(1.07118502872607,-20.800153501074,9.15632813453146));
#88627=CARTESIAN_POINT('Ctrl Pts',(1.07255878230226,-20.8038871259129,9.16422173025703));
#88628=CARTESIAN_POINT('Ctrl Pts',(1.07386305000202,-20.8078000652983,9.17166940850749));
#88629=CARTESIAN_POINT('Ctrl Pts',(1.075232223093,-20.8119077276394,9.17948771195293));
#88630=CARTESIAN_POINT('Ctrl Pts',(1.07652474432684,-20.8162122271943,9.18681414579865));
#88631=CARTESIAN_POINT('Ctrl Pts',(1.07773580012668,-20.8205166591577,9.19352802619739));
#88632=CARTESIAN_POINT('Ctrl Pts',(1.07787931959557,-20.8210267676014,9.19432367289601));
#88633=CARTESIAN_POINT('Ctrl Pts',(1.07802170331068,-20.8215368384517,9.19511076325773));
#88634=CARTESIAN_POINT('Ctrl Pts',(1.0781629498924,-20.8220465170099,9.19588913334329));
#88635=CARTESIAN_POINT('Ctrl Pts',(1.08032804869949,-20.8298591268785,9.20782038239202));
#88636=CARTESIAN_POINT('Ctrl Pts',(1.08226652975325,-20.8382896507038,9.21881468989689));
#88637=CARTESIAN_POINT('Ctrl Pts',(1.08402351013971,-20.8471020783112,9.22887541721332));
#88638=CARTESIAN_POINT('Ctrl Pts',(1.08517584511253,-20.852881806193,9.23547385623297));
#88639=CARTESIAN_POINT('Ctrl Pts',(1.08625031498372,-20.8588263848537,9.24167173694038));
#88640=CARTESIAN_POINT('Ctrl Pts',(1.08726153943815,-20.86487656414,9.24747939313306));
#88641=CARTESIAN_POINT('Ctrl Pts',(1.08808125864387,-20.8697809630964,9.25218719791422));
#88642=CARTESIAN_POINT('Ctrl Pts',(1.08883536059498,-20.8746095350316,9.25650566075248));
#88643=CARTESIAN_POINT('Ctrl Pts',(1.08954994669871,-20.879465449889,9.26058857987151));
#88644=CARTESIAN_POINT('Ctrl Pts',(1.0903054586788,-20.8845994733886,9.26490533651148));
#88645=CARTESIAN_POINT('Ctrl Pts',(1.0910168938194,-20.8897644415258,9.26895933782676));
#88646=CARTESIAN_POINT('Ctrl Pts',(1.09170742387484,-20.8951252431836,9.27288880630623));
#88647=CARTESIAN_POINT('Ctrl Pts',(1.09236126852373,-20.9002012445105,9.27660951609725));
#88648=CARTESIAN_POINT('Ctrl Pts',(1.09299638824525,-20.9054534538637,9.28021867678994));
#88649=CARTESIAN_POINT('Ctrl Pts',(1.09362516937514,-20.9110509216446,9.2837922762023));
#88650=CARTESIAN_POINT('Ctrl Pts',(1.09366044853728,-20.9113649800093,9.28399278093614));
#88651=CARTESIAN_POINT('Ctrl Pts',(1.09369570566157,-20.9116801319542,9.28419316189014));
#88652=CARTESIAN_POINT('Ctrl Pts',(1.0937309421707,-20.9119964096905,9.28439342814165));
#88653=CARTESIAN_POINT('Ctrl Pts',(1.09455787442067,-20.9194188322443,9.28909328706713));
#88654=CARTESIAN_POINT('Ctrl Pts',(1.09539733055772,-20.9264344691809,9.29306015364301));
#88655=CARTESIAN_POINT('Ctrl Pts',(1.09616241712905,-20.9329817607834,9.29647355247341));
#88656=CARTESIAN_POINT('Ctrl Pts',(1.09697381650712,-20.9399253780594,9.30009357377806));
#88657=CARTESIAN_POINT('Ctrl Pts',(1.0977016092117,-20.9463428927236,9.30309156448054));
#88658=CARTESIAN_POINT('Ctrl Pts',(1.09823552189471,-20.9522094034754,9.30564980905609));
#88659=CARTESIAN_POINT('Ctrl Pts',(1.09838767546572,-20.9538812322006,9.30637885344867));
#88660=CARTESIAN_POINT('Ctrl Pts',(1.09852404269639,-20.9555085643539,9.30707197485802));
#88661=CARTESIAN_POINT('Ctrl Pts',(1.09864197616628,-20.9570913748885,9.30773289237069));
#88662=CARTESIAN_POINT('Ctrl Pts',(1.09901475411098,-20.9620945080828,9.30982199796739));
#88663=CARTESIAN_POINT('Ctrl Pts',(1.0992510098558,-20.9669907190302,9.3117310437097));
#88664=CARTESIAN_POINT('Ctrl Pts',(1.09944107532713,-20.9719977802765,9.31354051571788));
#88665=CARTESIAN_POINT('Ctrl Pts',(1.09962572085938,-20.9768620593187,9.3152983885167));
#88666=CARTESIAN_POINT('Ctrl Pts',(1.09976679713354,-20.981831375378,9.31696238538762));
#88667=CARTESIAN_POINT('Ctrl Pts',(1.09993952702919,-20.9871206659853,9.31856173716953));
#88668=CARTESIAN_POINT('Ctrl Pts',(1.10002874388929,-20.9898526418156,9.31938781967031));
#88669=CARTESIAN_POINT('Ctrl Pts',(1.10012627944569,-20.9926701971939,9.32019592075339));
#88670=CARTESIAN_POINT('Ctrl Pts',(1.10024158038163,-20.9956041247815,9.32098473025938));
#88671=CARTESIAN_POINT('Ctrl Pts',(1.1005109347092,-21.002458068213,9.32282746685415));
#88672=CARTESIAN_POINT('Ctrl Pts',(1.10074051696748,-21.0089603913746,9.32431951715542));
#88673=CARTESIAN_POINT('Ctrl Pts',(1.10094115953662,-21.015244260674,9.32556382456884));
#88674=CARTESIAN_POINT('Ctrl Pts',(1.10115318185268,-21.0218845291291,9.32687870476));
#88675=CARTESIAN_POINT('Ctrl Pts',(1.10133288275599,-21.0282814763706,9.32791692087774));
#88676=CARTESIAN_POINT('Ctrl Pts',(1.10148363819399,-21.0346111901984,9.32874677840441));
#88677=CARTESIAN_POINT('Ctrl Pts',(1.10163793722913,-21.041089687753,9.32959614223087));
#88678=CARTESIAN_POINT('Ctrl Pts',(1.10176192015105,-21.0474983506607,9.33022727982751));
#88679=CARTESIAN_POINT('Ctrl Pts',(1.10184974337085,-21.0540357911593,9.33065978940719));
#88680=CARTESIAN_POINT('Ctrl Pts',(1.10193756659064,-21.060573231658,9.33109229898687));
#88681=CARTESIAN_POINT('Ctrl Pts',(1.10198928897115,-21.0672400649741,9.33132652171654));
#88682=CARTESIAN_POINT('Ctrl Pts',(1.10198928897115,-21.0742356128,9.33132652171654));
#88683=CARTESIAN_POINT('Origin',(0.45,-22.1242356128,-6.23438845923));
#88684=CARTESIAN_POINT('Origin',(0.451735403140307,-21.0742356268872,-6.23570473075995));
#88685=CARTESIAN_POINT('Ctrl Pts',(0.530469794195843,-21.0743245297157,
-6.52339509610176));
#88686=CARTESIAN_POINT('Ctrl Pts',(0.605567644237528,-21.0743045727586,
-6.50248549027524));
#88687=CARTESIAN_POINT('Ctrl Pts',(0.673874294281432,-21.0742929409078,
-6.45718387642163));
#88688=CARTESIAN_POINT('Ctrl Pts',(0.724680377815537,-21.0742929154351,
-6.3902979847186));
#88689=CARTESIAN_POINT('Ctrl Pts',(0.750000527627887,-21.0743044999368,
-6.31234350391071));
#88690=CARTESIAN_POINT('Ctrl Pts',(0.750000364792457,-21.0743244203334,
-6.23438902308944));
#88691=CARTESIAN_POINT('Ctrl Pts',(0.529382289785393,-20.9333453475782,
-6.52305698967578));
#88692=CARTESIAN_POINT('Ctrl Pts',(0.604379979183787,-20.964969743794,-6.50191658027744));
#88693=CARTESIAN_POINT('Ctrl Pts',(0.672544464007601,-20.9834025266085,
-6.45625456200327));
#88694=CARTESIAN_POINT('Ctrl Pts',(0.723444072664958,-20.9834428927103,
-6.38924960266457));
#88695=CARTESIAN_POINT('Ctrl Pts',(0.749147469416239,-20.9650851420997,
-6.3113527732948));
#88696=CARTESIAN_POINT('Ctrl Pts',(0.749396133634582,-20.9335186780883,
-6.23345594923032));
#88697=CARTESIAN_POINT('Ctrl Pts',(0.682790624388214,-20.8340546276202,
-6.57041298136646));
#88698=CARTESIAN_POINT('Ctrl Pts',(0.708912783176195,-20.8612993243623,
-6.52470345794668));
#88699=CARTESIAN_POINT('Ctrl Pts',(0.735010274608166,-20.8749839393705,
-6.48004084831971));
#88700=CARTESIAN_POINT('Ctrl Pts',(0.764785838670641,-20.8750139028965,
-6.43996377974995));
#88701=CARTESIAN_POINT('Ctrl Pts',(0.79985759450253,-20.8613891112934,-6.4024626941325));
#88702=CARTESIAN_POINT('Ctrl Pts',(0.83594438370652,-20.8342039270154,-6.36496160653959));
#88703=CARTESIAN_POINT('Ctrl Pts',(0.784751637977717,-20.8055921195135,
-6.60126308111576));
#88704=CARTESIAN_POINT('Ctrl Pts',(0.81115374258346,-20.8073594222485,-6.57634919799807));
#88705=CARTESIAN_POINT('Ctrl Pts',(0.836973064211128,-20.8079610962015,
-6.54907865572581));
#88706=CARTESIAN_POINT('Ctrl Pts',(0.859860043401567,-20.8079624129721,
-6.51825025363853));
#88707=CARTESIAN_POINT('Ctrl Pts',(0.87856407045771,-20.8073639920301,-6.48547428652468));
#88708=CARTESIAN_POINT('Ctrl Pts',(0.894834790258138,-20.8056018007968,
-6.45269832121122));
#88709=CARTESIAN_POINT('Ctrl Pts',(0.922269592128314,-20.7721965716525,
-6.64281131501362));
#88710=CARTESIAN_POINT('Ctrl Pts',(0.931687523370322,-20.7721714559979,
-6.62728238450244));
#88711=CARTESIAN_POINT('Ctrl Pts',(0.941236644076639,-20.7721534139295,
-6.61231329467342));
#88712=CARTESIAN_POINT('Ctrl Pts',(0.951507076621634,-20.77215320473,-6.59822048475924));
#88713=CARTESIAN_POINT('Ctrl Pts',(0.962806769208053,-20.7721710748754,
-6.58460782258426));
#88714=CARTESIAN_POINT('Ctrl Pts',(0.9746824612806,-20.7721964339549,-6.57098901863393));
#88715=CARTESIAN_POINT('Ctrl Pts',(1.05,-20.7742356128,-6.68100624476));
#88716=CARTESIAN_POINT('Ctrl Pts',(1.05,-20.7742356128,-6.68100624476));
#88717=CARTESIAN_POINT('Ctrl Pts',(1.05,-20.7742356128,-6.68100624476));
#88718=CARTESIAN_POINT('Ctrl Pts',(1.05,-20.7742356128,-6.68100624476));
#88719=CARTESIAN_POINT('Ctrl Pts',(1.05,-20.7742356128,-6.68100624476));
#88720=CARTESIAN_POINT('Ctrl Pts',(1.05,-20.7742356128,-6.68100624476));
#88721=CARTESIAN_POINT('Ctrl Pts',(1.05,-20.7742356128,-6.68100624476));
#88722=CARTESIAN_POINT('Ctrl Pts',(1.04185133965169,-20.7740151821963,-6.66912323008901));
#88723=CARTESIAN_POINT('Ctrl Pts',(1.03364154604321,-20.7742886139255,-6.65712795842614));
#88724=CARTESIAN_POINT('Ctrl Pts',(1.0254283835494,-20.7749660951999,-6.64510629905131));
#88725=CARTESIAN_POINT('Ctrl Pts',(1.01686694079147,-20.7756723051592,-6.63257485958806));
#88726=CARTESIAN_POINT('Ctrl Pts',(1.00830156833828,-20.7768176645118,-6.62001433313557));
#88727=CARTESIAN_POINT('Ctrl Pts',(0.999773202279283,-20.7783415832968,
-6.60748637620009));
#88728=CARTESIAN_POINT('Ctrl Pts',(0.990516308375853,-20.7799956814457,
-6.59388823003983));
#88729=CARTESIAN_POINT('Ctrl Pts',(0.981302730655643,-20.7820956741035,
-6.58032799535186));
#88730=CARTESIAN_POINT('Ctrl Pts',(0.972160688749562,-20.7846119703408,
-6.56685002089311));
#88731=CARTESIAN_POINT('Ctrl Pts',(0.966662483256319,-20.7861253208523,
-6.55874409948429));
#88732=CARTESIAN_POINT('Ctrl Pts',(0.961189710615404,-20.7877901735135,
-6.55066730455419));
#88733=CARTESIAN_POINT('Ctrl Pts',(0.955745648342861,-20.7896074561403,
-6.54262532894721));
#88734=CARTESIAN_POINT('Ctrl Pts',(0.945091671144306,-20.7931638606596,
-6.52688726048678));
#88735=CARTESIAN_POINT('Ctrl Pts',(0.934548826309054,-20.7973004363901,
-6.51128114796628));
#88736=CARTESIAN_POINT('Ctrl Pts',(0.924133552938165,-20.8020720545725,
-6.49583202115931));
#88737=CARTESIAN_POINT('Ctrl Pts',(0.913983176009837,-20.806722313993,-6.48077581910679));
#88738=CARTESIAN_POINT('Ctrl Pts',(0.903952604551205,-20.8119771913179,
-6.46586663394951));
#88739=CARTESIAN_POINT('Ctrl Pts',(0.894062671861464,-20.8179299419942,
-6.45113668546664));
#88740=CARTESIAN_POINT('Ctrl Pts',(0.884728957361107,-20.8235479049317,
-6.43723516175994));
#88741=CARTESIAN_POINT('Ctrl Pts',(0.875519620967452,-20.8297886520844,
-6.42349192647127));
#88742=CARTESIAN_POINT('Ctrl Pts',(0.866472894903575,-20.8367498259702,
-6.40996619617227));
#88743=CARTESIAN_POINT('Ctrl Pts',(0.858512683717075,-20.8428749605046,
-6.39806491068275));
#88744=CARTESIAN_POINT('Ctrl Pts',(0.850678234212531,-20.8495585348559,
-6.38633181316587));
#88745=CARTESIAN_POINT('Ctrl Pts',(0.843017929021964,-20.8568702967361,
-6.37484167223405));
#88746=CARTESIAN_POINT('Ctrl Pts',(0.835728552685902,-20.8638280069967,
-6.36390790924122));
#88747=CARTESIAN_POINT('Ctrl Pts',(0.828596625165056,-20.871354920686,-6.35319378039933));
#88748=CARTESIAN_POINT('Ctrl Pts',(0.821688263209047,-20.8795073540466,
-6.34280129650637));
#88749=CARTESIAN_POINT('Ctrl Pts',(0.815188118199059,-20.887178057951,-6.33302290725166));
#88750=CARTESIAN_POINT('Ctrl Pts',(0.808885816695372,-20.8954027709262,
-6.32352915177084));
#88751=CARTESIAN_POINT('Ctrl Pts',(0.802860701131854,-20.9042208042776,
-6.31444228904566));
#88752=CARTESIAN_POINT('Ctrl Pts',(0.797952094672979,-20.9114047752748,
-6.30703930522012));
#88753=CARTESIAN_POINT('Ctrl Pts',(0.793227830308663,-20.9189824725644,
-6.29990695086639));
#88754=CARTESIAN_POINT('Ctrl Pts',(0.788744524978859,-20.9269695397081,
-6.2931323825073));
#88755=CARTESIAN_POINT('Ctrl Pts',(0.783537340438766,-20.9362462071424,
-6.28526398519098));
#88756=CARTESIAN_POINT('Ctrl Pts',(0.778654465486172,-20.9460755460276,
-6.27787710052425));
#88757=CARTESIAN_POINT('Ctrl Pts',(0.774208582045746,-20.9564706602872,
-6.27114504890079));
#88758=CARTESIAN_POINT('Ctrl Pts',(0.769935816653026,-20.9664609996781,
-6.26467513632118));
#88759=CARTESIAN_POINT('Ctrl Pts',(0.766066640928027,-20.9769740075416,
-6.25881000506791));
#88760=CARTESIAN_POINT('Ctrl Pts',(0.762726389024589,-20.9880079998434,
-6.25374228386215));
#88761=CARTESIAN_POINT('Ctrl Pts',(0.75945227095981,-20.9988235294999,-6.24877489875866));
#88762=CARTESIAN_POINT('Ctrl Pts',(0.756686247671062,-21.0101397324872,
-6.2445735214744));
#88763=CARTESIAN_POINT('Ctrl Pts',(0.754572184142313,-21.0219403794457,
-6.24135910637881));
#88764=CARTESIAN_POINT('Ctrl Pts',(0.752512978193132,-21.0334348128394,
-6.23822810175291));
#88765=CARTESIAN_POINT('Ctrl Pts',(0.751072291099966,-21.0453889517463,
-6.23603343627861));
#88766=CARTESIAN_POINT('Ctrl Pts',(0.75040877541252,-21.0577724001193,-6.2350186214298));
#88767=CARTESIAN_POINT('Ctrl Pts',(0.750119049159553,-21.0631796725678,
-6.23457549927133));
#88768=CARTESIAN_POINT('Ctrl Pts',(0.749977843125384,-21.0686685916167,
-6.234357854582));
#88769=CARTESIAN_POINT('Ctrl Pts',(0.749999997537,-21.0742356128,-6.23438845562));
#88770=CARTESIAN_POINT('Origin',(1.05,-21.0742356128,7.56406439184));
#88771=CARTESIAN_POINT('Ctrl Pts',(1.05,-20.7742356128,9.0358656718));
#88772=CARTESIAN_POINT('Ctrl Pts',(1.03202389557851,-20.7742356128,9.0358656718));
#88773=CARTESIAN_POINT('Ctrl Pts',(1.01404810351911,-20.7758556512248,9.03586567179998));
#88774=CARTESIAN_POINT('Ctrl Pts',(0.996361658047574,-20.7790696793446,
9.03586567179994));
#88775=CARTESIAN_POINT('Ctrl Pts',(0.978670794646673,-20.7822845103023,
9.0358656717999));
#88776=CARTESIAN_POINT('Ctrl Pts',(0.961270037985875,-20.7870940177168,
9.03586567179984));
#88777=CARTESIAN_POINT('Ctrl Pts',(0.94443931537033,-20.7934208306739,9.03586567179976));
#88778=CARTESIAN_POINT('Ctrl Pts',(0.931321632902273,-20.7983518799997,
9.03586567179969));
#88779=CARTESIAN_POINT('Ctrl Pts',(0.918550114703901,-20.8042035471181,
9.03586567179962));
#88780=CARTESIAN_POINT('Ctrl Pts',(0.906249801614279,-20.810918540691,9.03586567179953));
#88781=CARTESIAN_POINT('Ctrl Pts',(0.890471751000551,-20.8195321026135,
9.03586567179942));
#88782=CARTESIAN_POINT('Ctrl Pts',(0.875470244037574,-20.829567460778,9.03586567179929));
#88783=CARTESIAN_POINT('Ctrl Pts',(0.861486491178611,-20.8408632558426,
9.03586567179914));
#88784=CARTESIAN_POINT('Ctrl Pts',(0.856033990875819,-20.8452676762175,
9.03586567179908));
#88785=CARTESIAN_POINT('Ctrl Pts',(0.850735912921936,-20.8498632609397,
9.03586567179902));
#88786=CARTESIAN_POINT('Ctrl Pts',(0.845605262111768,-20.8546387295717,
9.03586567179895));
#88787=CARTESIAN_POINT('Ctrl Pts',(0.836460775867545,-20.8631501658067,
9.03586567179884));
#88788=CARTESIAN_POINT('Ctrl Pts',(0.827848666191205,-20.872233507004,9.03586567179871));
#88789=CARTESIAN_POINT('Ctrl Pts',(0.819835992199914,-20.8818180213137,
9.03586567179857));
#88790=CARTESIAN_POINT('Ctrl Pts',(0.815829655204269,-20.8866102784685,
9.03586567179851));
#88791=CARTESIAN_POINT('Ctrl Pts',(0.811973029026346,-20.8915277101616,
9.03586567179843));
#88792=CARTESIAN_POINT('Ctrl Pts',(0.808273644182413,-20.89656071614,9.03586567179836));
#88793=CARTESIAN_POINT('Ctrl Pts',(0.806423951760447,-20.8990772191291,
9.03586567179832));
#88794=CARTESIAN_POINT('Ctrl Pts',(0.804613560752439,-20.901622607585,9.03586567179828));
#88795=CARTESIAN_POINT('Ctrl Pts',(0.802843353271149,-20.9041956410941,
9.03586567179824));
#88796=CARTESIAN_POINT('Ctrl Pts',(0.801780698696832,-20.90574023169,9.03586567179822));
#88797=CARTESIAN_POINT('Ctrl Pts',(0.800495085070646,-20.90764888492,9.0358656717982));
#88798=CARTESIAN_POINT('Ctrl Pts',(0.799417570014984,-20.9092857847225,
9.03586567179817));
#88799=CARTESIAN_POINT('Ctrl Pts',(0.798700122475243,-20.9103756903622,
9.03586567179815));
#88800=CARTESIAN_POINT('Ctrl Pts',(0.798073491215928,-20.9113441289506,
9.03586567179814));
#88801=CARTESIAN_POINT('Ctrl Pts',(0.797654124306547,-20.9119964097062,
9.03586567179813));
#88802=CARTESIAN_POINT('Ctrl Pts',(0.78926050248039,-20.9250517983519,9.03586567179794));
#88803=CARTESIAN_POINT('Ctrl Pts',(0.78188214283678,-20.9387597450956,9.03589999168628));
#88804=CARTESIAN_POINT('Ctrl Pts',(0.775607596296699,-20.9529557348733,
9.03596863146315));
#88805=CARTESIAN_POINT('Ctrl Pts',(0.772470323026658,-20.9600537297621,
9.03600295135159));
#88806=CARTESIAN_POINT('Ctrl Pts',(0.76960860666254,-20.9672735141048,9.03604585121217));
#88807=CARTESIAN_POINT('Ctrl Pts',(0.767031056629434,-20.9745933673027,
9.03609733104487));
#88808=CARTESIAN_POINT('Ctrl Pts',(0.765851262758171,-20.9779438038919,
9.03612089434737));
#88809=CARTESIAN_POINT('Ctrl Pts',(0.764648990061719,-20.98156092275,9.03614854597792));
#88810=CARTESIAN_POINT('Ctrl Pts',(0.763545455771623,-20.9851076481037,
9.03617714035478));
#88811=CARTESIAN_POINT('Ctrl Pts',(0.762387498750328,-20.9888292864458,
9.03620714491354));
#88812=CARTESIAN_POINT('Ctrl Pts',(0.761338259871668,-20.99247304056,9.03623818749787));
#88813=CARTESIAN_POINT('Ctrl Pts',(0.76048046437477,-20.9956325690208,9.03626663380754));
#88814=CARTESIAN_POINT('Ctrl Pts',(0.760369753607963,-20.9960403513185,
9.0362703052103));
#88815=CARTESIAN_POINT('Ctrl Pts',(0.760262162949232,-20.9964400516044,
9.03627393336538));
#88816=CARTESIAN_POINT('Ctrl Pts',(0.760157814465616,-20.9968307842384,
9.0362775104594));
#88817=CARTESIAN_POINT('Ctrl Pts',(0.755519525522536,-21.0141988455,9.03643651224889));
#88818=CARTESIAN_POINT('Ctrl Pts',(0.752446613553971,-21.0319846306718,
9.03642084523756));
#88819=CARTESIAN_POINT('Ctrl Pts',(0.750988491653542,-21.0499021404548,
9.03623050942544));
#88820=CARTESIAN_POINT('Ctrl Pts',(0.750329859351278,-21.05799546291,9.03614453491666));
#88821=CARTESIAN_POINT('Ctrl Pts',(0.749999999999998,-21.0661155349141,
9.03602292237484));
#88822=CARTESIAN_POINT('Ctrl Pts',(0.749999999999998,-21.0742356128,9.0358656718));
#88823=CARTESIAN_POINT('Origin',(1.05,-21.0742356128,-6.03615517446));
#88824=CARTESIAN_POINT('',(1.05,-20.7742356128,-5.83842593707));
#88825=CARTESIAN_POINT('Origin',(1.05,-21.0742356128,9.0358656718));
#88826=CARTESIAN_POINT('Origin',(11.0821857629,-22.0742356128,-2.71007990903));
#88827=CARTESIAN_POINT('Origin',(2.45,-19.6742356128,10.7304528845));
#88828=CARTESIAN_POINT('',(2.45,-19.3742356128,10.1304528845));
#88829=CARTESIAN_POINT('Origin',(2.45,-19.3742356128,10.7304528845));
#88830=CARTESIAN_POINT('Origin',(2.45,-19.6742356128,10.1304528845));
#88831=CARTESIAN_POINT('Origin',(4.57526812267,-21.0742356128,-3.65872047634));
#88832=CARTESIAN_POINT('',(4.79320888776,-21.0742356128,-3.4525607739));
#88833=CARTESIAN_POINT('',(4.40684492179,-21.0742356128,-3.41045927235));
#88834=CARTESIAN_POINT('Origin',(4.57526812267,-21.0742356128,-3.65872047634));
#88835=CARTESIAN_POINT('',(4.57526812267,-20.7742356128,-3.65872047634));
#88836=CARTESIAN_POINT('Origin',(4.57526812267,-21.0742356128,-3.65872047634));
#88837=CARTESIAN_POINT('Origin',(4.57526812267,-21.0742356128,-3.65872047634));
#88838=CARTESIAN_POINT('Origin',(4.57526812267,-22.1242356128,-3.65872047634));
#88839=CARTESIAN_POINT('',(4.40684492179,-21.2742356128,-3.41045927235));
#88840=CARTESIAN_POINT('',(4.79320888776,-21.9742356128,-3.4525607739));
#88841=CARTESIAN_POINT('Origin',(0.00234331738835,-21.2742356128,3.08191746407));
#88842=CARTESIAN_POINT('Origin',(0.00234331738835,-21.0742356128,3.08191746407));
#88843=CARTESIAN_POINT('Origin',(0.00234331738835,-21.0742356128,3.08191746407));
#88844=CARTESIAN_POINT('Origin',(0.00234331738835,-20.7742356128,3.08191746407));
#88845=CARTESIAN_POINT('Origin',(3.69394702409,-21.0742356128,-6.14889144395));
#88846=CARTESIAN_POINT('',(3.69394702409,-20.7742356128,-7.0794205347));
#88847=CARTESIAN_POINT('Origin',(3.69394702409,-21.0742356128,-7.0794205347));
#88848=CARTESIAN_POINT('',(3.69394702409,-20.7742356128,-7.27665075431));
#88849=CARTESIAN_POINT('Origin',(3.69394702409,-21.0742356128,-7.27665075431));
#88850=CARTESIAN_POINT('',(3.69394702409,-20.7742356128,-7.17803564451));
#88851=CARTESIAN_POINT('Origin',(3.09394702409,-21.0742356128,-7.0794205347));
#88852=CARTESIAN_POINT('',(2.83839294143,-20.7742356128,-6.53656501909));
#88853=CARTESIAN_POINT('Origin',(2.83839294143,-21.0742356128,-6.53656501909));
#88854=CARTESIAN_POINT('Origin',(3.09394702409,-20.7742356128,-7.0794205347));
#88855=CARTESIAN_POINT('Origin',(-2.84607155346,-21.0742356128,5.53854202767));
#88856=CARTESIAN_POINT('',(2.48410064475,-20.7742356128,-6.69708673107));
#88857=CARTESIAN_POINT('Origin',(2.48410064475,-21.0742356128,-6.69708673107));
#88858=CARTESIAN_POINT('Origin',(-2.84607155346,-20.7742356128,5.53854202767));
#88859=CARTESIAN_POINT('Origin',(2.72372695744,-21.0742356128,-7.24715875387));
#88860=CARTESIAN_POINT('',(2.12372695744,-20.7742356128,-7.24715875387));
#88861=CARTESIAN_POINT('Origin',(2.12372695744,-21.0742356128,-7.24715875387));
#88862=CARTESIAN_POINT('Origin',(2.72372695744,-20.7742356128,-7.24715875387));
#88863=CARTESIAN_POINT('Origin',(2.12372695744,-21.0742356128,-6.11170048962));
#88864=CARTESIAN_POINT('',(2.12372695744,-20.7742356128,-7.96338790087));
#88865=CARTESIAN_POINT('Origin',(2.12372695744,-21.0742356128,-7.96338790087));
#88866=CARTESIAN_POINT('',(2.12372695744,-20.7742356128,-7.60527332737));
#88867=CARTESIAN_POINT('Origin',(3.69394702409,-21.0742356128,-7.27665075431));
#88868=CARTESIAN_POINT('',(3.83031550589,-21.0742356128,-7.54386534443));
#88869=CARTESIAN_POINT('Origin',(3.69394702409,-21.0742356128,-7.27665075431));
#88870=CARTESIAN_POINT('Origin',(3.69394702409,-21.0742356128,-7.27665075431));
#88871=CARTESIAN_POINT('',(3.69394702409,-20.7869530199367,-7.36307246360657));
#88872=CARTESIAN_POINT('Origin',(3.69394702409,-21.0742356128,-7.27665075431));
#88873=CARTESIAN_POINT('Origin',(-2.84607155346,-21.0742356128,5.53854202767));
#88874=CARTESIAN_POINT('',(6.53717906469,-21.0742356128,-5.76093294477));
#88875=CARTESIAN_POINT('Origin',(-2.84607155346,-21.0742356128,5.53854202767));
#88876=CARTESIAN_POINT('',(6.34552156645,-20.7742356128,-5.5301356238));
#88877=CARTESIAN_POINT('Ctrl Pts',(6.34552156645,-20.7742356128,-5.5301356238));
#88878=CARTESIAN_POINT('Ctrl Pts',(6.35174034324132,-20.7742356127986,-5.53762438388832));
#88879=CARTESIAN_POINT('Ctrl Pts',(6.35742859914234,-20.7747062490391,-5.54448824766959));
#88880=CARTESIAN_POINT('Ctrl Pts',(6.36256699872495,-20.7754276309491,-5.55070852110689));
#88881=CARTESIAN_POINT('Ctrl Pts',(6.3678994278893,-20.7761762527474,-5.55716367644349));
#88882=CARTESIAN_POINT('Ctrl Pts',(6.37264035260703,-20.7771944005427,-5.56292651713689));
#88883=CARTESIAN_POINT('Ctrl Pts',(6.37678906820952,-20.7782819825865,-5.5680013143877));
#88884=CARTESIAN_POINT('Ctrl Pts',(6.37894431376028,-20.7788469782588,-5.57063765663039));
#88885=CARTESIAN_POINT('Ctrl Pts',(6.38094000743543,-20.7794315014735,-5.57308863873272));
#88886=CARTESIAN_POINT('Ctrl Pts',(6.38277728175031,-20.7800126526577,-5.57535633957807));
#88887=CARTESIAN_POINT('Ctrl Pts',(6.38638444340125,-20.7811536397426,-5.57980856723886));
#88888=CARTESIAN_POINT('Ctrl Pts',(6.38939025144264,-20.7822789779567,-5.5835505570955));
#88889=CARTESIAN_POINT('Ctrl Pts',(6.39182761328184,-20.7832571893903,-5.58659360401943));
#88890=CARTESIAN_POINT('Ctrl Pts',(6.39235720901811,-20.7834697374807,-5.58725480444124));
#88891=CARTESIAN_POINT('Ctrl Pts',(6.39285996977376,-20.7836755352566,-5.58788300900781));
#88892=CARTESIAN_POINT('Ctrl Pts',(6.39333622863194,-20.7838735566742,-5.5884783276713));
#88893=CARTESIAN_POINT('Ctrl Pts',(6.39467030265331,-20.7844282450004,-5.5901459064465));
#88894=CARTESIAN_POINT('Ctrl Pts',(6.39579652923337,-20.7849214295115,-5.59155550086856));
#88895=CARTESIAN_POINT('Ctrl Pts',(6.3967213044829,-20.7853351743983,-5.59270930512864));
#88896=CARTESIAN_POINT('Ctrl Pts',(6.39718369210766,-20.7855420468417,-5.59328620725868));
#88897=CARTESIAN_POINT('Ctrl Pts',(6.39732902439631,-20.785609782216,-5.59347304518995));
#88898=CARTESIAN_POINT('Ctrl Pts',(6.39755820869149,-20.7857142794367,-5.59375953787831));
#88899=CARTESIAN_POINT('Ctrl Pts',(6.39778739298666,-20.7858187766574,-5.59404603056667));
#88900=CARTESIAN_POINT('Ctrl Pts',(6.39810064993959,-20.7859589015239,-5.59443244375046));
#88901=CARTESIAN_POINT('Ctrl Pts',(6.39889593392354,-20.7863267818361,-5.59540494006124));
#88902=CARTESIAN_POINT('Ctrl Pts',(6.40404794656149,-20.7887099858944,-5.60170497047125));
#88903=CARTESIAN_POINT('Ctrl Pts',(6.40977643932818,-20.7916764543232,-5.60846234457286));
#88904=CARTESIAN_POINT('Ctrl Pts',(6.41591040714488,-20.7954242675397,-5.61563336197756));
#88905=CARTESIAN_POINT('Ctrl Pts',(6.41735133745903,-20.7963046663023,-5.61731790559932));
#88906=CARTESIAN_POINT('Ctrl Pts',(6.41881449983512,-20.7972282257994,-5.61902510707537));
#88907=CARTESIAN_POINT('Ctrl Pts',(6.42029740193474,-20.7981975666476,-5.6207540767046));
#88908=CARTESIAN_POINT('Ctrl Pts',(6.42419517278191,-20.8007454546706,-5.62529862986033));
#88909=CARTESIAN_POINT('Ctrl Pts',(6.42822810099414,-20.8036096225989,-5.6299947451574));
#88910=CARTESIAN_POINT('Ctrl Pts',(6.43233592097233,-20.8068348561763,-5.63482617722769));
#88911=CARTESIAN_POINT('Ctrl Pts',(6.43408287762893,-20.808206470146,-5.63688086863602));
#88912=CARTESIAN_POINT('Ctrl Pts',(6.4360229497544,-20.8097917703793,-5.63917812802395));
#88913=CARTESIAN_POINT('Ctrl Pts',(6.43791817945649,-20.8114135266398,-5.64143439912276));
#88914=CARTESIAN_POINT('Ctrl Pts',(6.43989708759085,-20.813106886897,-5.6437902894013));
#88915=CARTESIAN_POINT('Ctrl Pts',(6.44182686918908,-20.8148399819277,-5.64610120824757));
#88916=CARTESIAN_POINT('Ctrl Pts',(6.44345562697637,-20.8163576317262,-5.64806724246914));
#88917=CARTESIAN_POINT('Ctrl Pts',(6.4439349217766,-20.8168042307618,-5.64864578765667));
#88918=CARTESIAN_POINT('Ctrl Pts',(6.44438827496193,-20.8172318574099,-5.64919461873951));
#88919=CARTESIAN_POINT('Ctrl Pts',(6.4448095419601,-20.8176333489548,-5.64970642349391));
#88920=CARTESIAN_POINT('Ctrl Pts',(6.45271403902305,-20.8251667867785,-5.65930973729628));
#88921=CARTESIAN_POINT('Ctrl Pts',(6.46005563597925,-20.8333640871257,-5.66815201559128));
#88922=CARTESIAN_POINT('Ctrl Pts',(6.46680425788755,-20.8419892536935,-5.67625933714307));
#88923=CARTESIAN_POINT('Ctrl Pts',(6.47106538871199,-20.8474352489837,-5.68137836118048));
#88924=CARTESIAN_POINT('Ctrl Pts',(6.47509076231836,-20.8530523456082,-5.68620517151398));
#88925=CARTESIAN_POINT('Ctrl Pts',(6.47887829642981,-20.8587871989418,-5.69075306944489));
#88926=CARTESIAN_POINT('Ctrl Pts',(6.4837713419325,-20.8661959502525,-5.69662841495012));
#88927=CARTESIAN_POINT('Ctrl Pts',(6.48827128604217,-20.8738016698329,-5.70203664313868));
#88928=CARTESIAN_POINT('Ctrl Pts',(6.49240130722295,-20.8815114106274,-5.70700767832463));
#88929=CARTESIAN_POINT('Ctrl Pts',(6.4941955719898,-20.8848608647012,-5.70916731695564));
#88930=CARTESIAN_POINT('Ctrl Pts',(6.49601100333805,-20.8884066452834,-5.71135394124107));
#88931=CARTESIAN_POINT('Ctrl Pts',(6.49772743922749,-20.8919183912156,-5.71342174719814));
#88932=CARTESIAN_POINT('Ctrl Pts',(6.4995360642771,-20.8956187517709,-5.71560061427653));
#88933=CARTESIAN_POINT('Ctrl Pts',(6.50123465242143,-20.8992809205782,-5.71764741014477));
#88934=CARTESIAN_POINT('Ctrl Pts',(6.5027136656765,-20.9026002822876,-5.71942893398982));
#88935=CARTESIAN_POINT('Ctrl Pts',(6.5030618778577,-20.9033817777726,-5.71984836789402));
#88936=CARTESIAN_POINT('Ctrl Pts',(6.50339804632306,-20.9041441473342,-5.72025325107986));
#88937=CARTESIAN_POINT('Ctrl Pts',(6.50372095659477,-20.9048832171215,-5.72064210415656));
#88938=CARTESIAN_POINT('Ctrl Pts',(6.50817483638558,-20.9150771572898,-5.72600552864804));
#88939=CARTESIAN_POINT('Ctrl Pts',(6.51208297248286,-20.9253660622679,-5.73071176481533));
#88940=CARTESIAN_POINT('Ctrl Pts',(6.51551887458798,-20.9356960421862,-5.7348493327296));
#88941=CARTESIAN_POINT('Ctrl Pts',(6.51908984608229,-20.9464321058739,-5.73914955334871));
#88942=CARTESIAN_POINT('Ctrl Pts',(6.52215114646008,-20.9572133335537,-5.74283602360956));
#88943=CARTESIAN_POINT('Ctrl Pts',(6.5247662065358,-20.9680266144033,-5.74598512619714));
#88944=CARTESIAN_POINT('Ctrl Pts',(6.52749312419639,-20.9793024266844,-5.74926892970927));
#88945=CARTESIAN_POINT('Ctrl Pts',(6.52973519744188,-20.9906139949508,-5.75196887803585));
#88946=CARTESIAN_POINT('Ctrl Pts',(6.53153761692296,-21.0019836757955,-5.75413938848151));
#88947=CARTESIAN_POINT('Ctrl Pts',(6.53341564424095,-21.0138302916622,-5.75640094743252));
#88948=CARTESIAN_POINT('Ctrl Pts',(6.53481674186588,-21.0257411027344,-5.75808818025164));
#88949=CARTESIAN_POINT('Ctrl Pts',(6.53575756861761,-21.0377652510857,-5.75922114543387));
#88950=CARTESIAN_POINT('Ctrl Pts',(6.53669839536933,-21.049789399437,-5.76035411061609));
#88951=CARTESIAN_POINT('Ctrl Pts',(6.53717906472003,-21.0619281910693,-5.76093294480616));
#88952=CARTESIAN_POINT('Ctrl Pts',(6.53717906472003,-21.0742356128,-5.76093294480616));
#88953=CARTESIAN_POINT('Origin',(-2.84607155346,-20.7742356128,5.53854202767));
#88954=CARTESIAN_POINT('Origin',(2.12372695744,-21.0742356128,-7.96338790087));
#88955=CARTESIAN_POINT('Origin',(2.12372695744,-21.0742356128,-7.96338790086));
#88956=CARTESIAN_POINT('Origin',(-2.84607155346,-21.0742356128,5.53854202767));
#88957=CARTESIAN_POINT('',(0.207931718075,-21.0742356128,-8.82796731988));
#88958=CARTESIAN_POINT('Origin',(-2.84607155346,-21.0742356128,5.53854202767));
#88959=CARTESIAN_POINT('',(2.93466272541E-14,-20.7742356128,-8.56468050289));
#88960=CARTESIAN_POINT('Origin',(-2.84607155346,-20.7742356128,5.53854202767));
#88961=CARTESIAN_POINT('Ctrl Pts',(0.207931718075,-21.0742356128,-8.82796731988));
#88962=CARTESIAN_POINT('Ctrl Pts',(0.208944325295,-20.9488183216,-8.82888814763));
#88963=CARTESIAN_POINT('Ctrl Pts',(0.15281970676,-20.8273615349,-8.76362621195));
#88964=CARTESIAN_POINT('Ctrl Pts',(0.0739219411508,-20.7751437694,-8.66437291113));
#88965=CARTESIAN_POINT('Ctrl Pts',(2.93466272541E-14,-20.7742356128,-8.56468050289));
#88966=CARTESIAN_POINT('Origin',(3.69394702409,-23.1223803511,-7.27665075431));
#88967=CARTESIAN_POINT('',(3.83031550589,-22.5742356128,-7.54386534443));
#88968=CARTESIAN_POINT('Origin',(-2.84607155346,-21.2742356128,5.53854202767));
#88969=CARTESIAN_POINT('',(6.53717906469,-22.1242356128,-5.76093294477));
#88970=CARTESIAN_POINT('Origin',(-2.84607155346,-22.6642356128,5.53854202767));
#88971=CARTESIAN_POINT('',(0.207931718075,-23.2742356128,-8.82796731988));
#88972=CARTESIAN_POINT('Origin',(6.34552156645,-22.1242356128,-5.5301356238));
#88973=CARTESIAN_POINT('',(6.56346233154,-21.0742356128,-5.32397592135));
#88974=CARTESIAN_POINT('',(6.56346233154,-21.9742356128,-5.32397592135));
#88975=CARTESIAN_POINT('Origin',(6.34552156645,-21.0742356128,-5.5301356238));
#88976=CARTESIAN_POINT('Origin',(6.34552156645,-21.0742356128,-5.5301356238));
#88977=CARTESIAN_POINT('Origin',(6.34552156645,-21.0742356128,-5.5301356238));
#88978=CARTESIAN_POINT('Origin',(5.6152263525,-21.0742356128,-4.75810745444));
#88979=CARTESIAN_POINT('',(5.67833560965,-21.0742356128,-4.38826834763));
#88980=CARTESIAN_POINT('',(5.46039484456,-20.7742356128,-4.59442805007));
#88981=CARTESIAN_POINT('Origin',(6.78099426296,-23.1742356128,-5.55393878512));
#88982=CARTESIAN_POINT('',(6.4527882763,-22.8742356128,-5.20697736155));
#88983=CARTESIAN_POINT('Origin',(6.6707290414,-22.8742356128,-5.00081765911));
#88984=CARTESIAN_POINT('',(5.89627637474,-23.1742356128,-4.18210864518));
#88985=CARTESIAN_POINT('Ctrl Pts',(8.01224741424,-22.8742356128,11.9089404858));
#88986=CARTESIAN_POINT('Ctrl Pts',(8.01224741424,-22.8742356128,11.9089404858));
#88987=CARTESIAN_POINT('Ctrl Pts',(8.01224741424,-22.8742356128,11.9089404858));
#88988=CARTESIAN_POINT('Ctrl Pts',(8.01224741424,-22.8742356128,11.9089404858));
#88989=CARTESIAN_POINT('Ctrl Pts',(8.01224741424,-22.8742356128,11.9089404858));
#88990=CARTESIAN_POINT('Ctrl Pts',(8.01224741423999,-22.8742356128,11.9089404858));
#88991=CARTESIAN_POINT('Ctrl Pts',(7.9829584197,-22.9540055384,11.8818593216));
#88992=CARTESIAN_POINT('Ctrl Pts',(7.9770990599352,-22.9460253560251,11.8764416455582));
#88993=CARTESIAN_POINT('Ctrl Pts',(7.97123968718953,-22.9380451737504,11.8710239575141));
#88994=CARTESIAN_POINT('Ctrl Pts',(7.96538034046018,-22.9300650091037,11.8656062935251));
#88995=CARTESIAN_POINT('Ctrl Pts',(7.95952098070146,-22.9220848089627,11.860188617489));
#88996=CARTESIAN_POINT('Ctrl Pts',(7.95366162093663,-22.914104626726,11.8547709414472));
#88997=CARTESIAN_POINT('Ctrl Pts',(7.95813278234,-23.0338190575,11.8499462819));
#88998=CARTESIAN_POINT('Ctrl Pts',(7.94825905166378,-23.0178496871499,11.8371162897713));
#88999=CARTESIAN_POINT('Ctrl Pts',(7.93746144800327,-23.0018803166997,11.8252680214644));
#89000=CARTESIAN_POINT('Ctrl Pts',(7.92573318729569,-22.9859083057293,11.8144258374139));
#89001=CARTESIAN_POINT('Ctrl Pts',(7.91307644092752,-22.969936608137,11.8045917287975));
#89002=CARTESIAN_POINT('Ctrl Pts',(7.8995045515438,-22.9539767898742,11.7957473669925));
#89003=CARTESIAN_POINT('Ctrl Pts',(7.93828028322,-23.1128615217,11.8131880532));
#89004=CARTESIAN_POINT('Ctrl Pts',(7.92683935647196,-23.0883986064311,11.7920888374253));
#89005=CARTESIAN_POINT('Ctrl Pts',(7.91212856723288,-23.0639356911622,11.7732848241785));
#89006=CARTESIAN_POINT('Ctrl Pts',(7.89438791009002,-23.0397784455373,11.7568870252871));
#89007=CARTESIAN_POINT('Ctrl Pts',(7.87382726489228,-23.0162127276929,11.7430895590338));
#89008=CARTESIAN_POINT('Ctrl Pts',(7.85061574634478,-22.9934900789388,11.7321598018371));
#89009=CARTESIAN_POINT('Ctrl Pts',(7.91959338184,-23.2114810387,11.7607695014));
#89010=CARTESIAN_POINT('Ctrl Pts',(7.91104290590454,-23.1749426359854,11.7286346798805));
#89011=CARTESIAN_POINT('Ctrl Pts',(7.89351740441245,-23.1384042333708,11.699893196182));
#89012=CARTESIAN_POINT('Ctrl Pts',(7.86768957667201,-23.103241423932,11.6760256725457));
#89013=CARTESIAN_POINT('Ctrl Pts',(7.83459760655358,-23.0708679220605,11.6579915758093));
#89014=CARTESIAN_POINT('Ctrl Pts',(7.79567993551832,-23.0427829224516,11.6462613688059));
#89015=CARTESIAN_POINT('Ctrl Pts',(7.9155846643,-23.3039994083,11.6969647216));
#89016=CARTESIAN_POINT('Ctrl Pts',(7.91452273992938,-23.2518430212389,11.6602665109009));
#89017=CARTESIAN_POINT('Ctrl Pts',(7.89658289688478,-23.1996866341778,11.6241420094615));
#89018=CARTESIAN_POINT('Ctrl Pts',(7.86183588918055,-23.1523923703251,11.5920351112702));
#89019=CARTESIAN_POINT('Ctrl Pts',(7.81377648892191,-23.1147174093106,11.5671753477237));
#89020=CARTESIAN_POINT('Ctrl Pts',(7.75766059577219,-23.0890492050938,11.5510403468213));
#89021=CARTESIAN_POINT('Ctrl Pts',(7.91547477954,-23.3227166577,11.6832984902));
#89022=CARTESIAN_POINT('Ctrl Pts',(7.91611368027112,-23.2671793589699,11.6460281227172));
#89023=CARTESIAN_POINT('Ctrl Pts',(7.89817677511925,-23.2116420601397,11.6085483823846));
#89024=CARTESIAN_POINT('Ctrl Pts',(7.8615589396166,-23.1618034258408,11.5747131302309));
#89025=CARTESIAN_POINT('Ctrl Pts',(7.81033796782714,-23.1232141110753,11.5482906652978));
#89026=CARTESIAN_POINT('Ctrl Pts',(7.75066973611005,-23.098410069918,11.5310175530077));
#89027=CARTESIAN_POINT('Ctrl Pts',(7.91677660432,-23.3563766548,11.6571003353));
#89028=CARTESIAN_POINT('Ctrl Pts',(7.9207682851848,-23.2942792858749,11.619652082997));
#89029=CARTESIAN_POINT('Ctrl Pts',(7.90297924229356,-23.2321819169498,11.5801041049053));
#89030=CARTESIAN_POINT('Ctrl Pts',(7.8628578513892,-23.1775788143209,11.5430317511911));
#89031=CARTESIAN_POINT('Ctrl Pts',(7.80571697781476,-23.1377014621359,11.5133446867667));
#89032=CARTESIAN_POINT('Ctrl Pts',(7.7395970182243,-23.1152461674912,11.493386398801));
#89033=CARTESIAN_POINT('Ctrl Pts',(7.92150726931,-23.3879026248,11.6287650914));
#89034=CARTESIAN_POINT('Ctrl Pts',(7.92877476677365,-23.318688693446,11.5932981429158));
#89035=CARTESIAN_POINT('Ctrl Pts',(7.91116012626247,-23.249474761992,11.5528780102254));
#89036=CARTESIAN_POINT('Ctrl Pts',(7.86749085858668,-23.1900474596595,11.5125263244749));
#89037=CARTESIAN_POINT('Ctrl Pts',(7.8046060841006,-23.1497152870341,11.4785634108322));
#89038=CARTESIAN_POINT('Ctrl Pts',(7.73273866216467,-23.1310192862307,11.4543385166681));
#89039=CARTESIAN_POINT('Ctrl Pts',(7.92449811306,-23.4017307742,11.6153459759));
#89040=CARTESIAN_POINT('Ctrl Pts',(7.933160012689,-23.329167474491,11.5813212138622));
#89041=CARTESIAN_POINT('Ctrl Pts',(7.91558915602351,-23.2566041748821,11.5408186562867));
#89042=CARTESIAN_POINT('Ctrl Pts',(7.87030342328902,-23.194978958134,11.4989724871098));
#89043=CARTESIAN_POINT('Ctrl Pts',(7.80489676739664,-23.1546275335721,11.4628007513679));
#89044=CARTESIAN_POINT('Ctrl Pts',(7.73064661099946,-23.1379387567491,11.4362192511351));
#89045=CARTESIAN_POINT('Ctrl Pts',(7.93181038161,-23.4257772831,11.589727728));
#89046=CARTESIAN_POINT('Ctrl Pts',(7.94259898634281,-23.3469242604025,11.5595784538612));
#89047=CARTESIAN_POINT('Ctrl Pts',(7.9249159224873,-23.2680712378051,11.5196955912591));
#89048=CARTESIAN_POINT('Ctrl Pts',(7.87670243326465,-23.202465097965,11.4751415902794));
#89049=CARTESIAN_POINT('Ctrl Pts',(7.80703642869538,-23.1624609825163,11.4343063448108));
#89050=CARTESIAN_POINT('Ctrl Pts',(7.72912102101426,-23.149972994791,11.4024242587647));
#89051=CARTESIAN_POINT('Ctrl Pts',(7.9432480685,-23.4460266432,11.5624437668));
#89052=CARTESIAN_POINT('Ctrl Pts',(7.95449392576775,-23.3611564773106,11.5385890032017));
#89053=CARTESIAN_POINT('Ctrl Pts',(7.93588514160407,-23.2762863115213,11.5010092226736));
#89054=CARTESIAN_POINT('Ctrl Pts',(7.8850335890661,-23.2070923242712,11.4540126467371));
#89055=CARTESIAN_POINT('Ctrl Pts',(7.81252461794977,-23.1679811870594,11.4073832166432));
#89056=CARTESIAN_POINT('Ctrl Pts',(7.73312092819091,-23.1601101382277,11.3682475271265));
#89057=CARTESIAN_POINT('Ctrl Pts',(7.94999449773,-23.4537301075,11.5494738265));
#89058=CARTESIAN_POINT('Ctrl Pts',(7.96070890734367,-23.3664431521595,11.529053261775));
#89059=CARTESIAN_POINT('Ctrl Pts',(7.94044985180303,-23.2791561968191,11.4939666534735));
#89060=CARTESIAN_POINT('Ctrl Pts',(7.88853929471968,-23.2085200743833,11.4459866136166));
#89061=CARTESIAN_POINT('Ctrl Pts',(7.81626122848945,-23.1698936980673,11.3955452574941));
#89062=CARTESIAN_POINT('Ctrl Pts',(7.73703971994881,-23.1639670049992,11.3526526368584));
#89063=CARTESIAN_POINT('Ctrl Pts',(7.96050853719668,-23.4651190523151,11.5297147907699));
#89064=CARTESIAN_POINT('Ctrl Pts',(7.97009076391529,-23.3740252890692,11.515240726516));
#89065=CARTESIAN_POINT('Ctrl Pts',(7.94977536603235,-23.2829315258232,11.4813952869434));
#89066=CARTESIAN_POINT('Ctrl Pts',(7.89632703655667,-23.2102050064346,11.4319920118367));
#89067=CARTESIAN_POINT('Ctrl Pts',(7.82189905423964,-23.1723857998439,11.3782644258795));
#89068=CARTESIAN_POINT('Ctrl Pts',(7.74337446791057,-23.1696699763263,11.3290106935214));
#89069=CARTESIAN_POINT('Ctrl Pts',(7.97509183792815,-23.4709933117087,11.5096161616792));
#89070=CARTESIAN_POINT('Ctrl Pts',(7.98108947414199,-23.3778496890314,11.5016366199269));
#89071=CARTESIAN_POINT('Ctrl Pts',(7.95748972962179,-23.2847060664544,11.4721514013342));
#89072=CARTESIAN_POINT('Ctrl Pts',(7.9031883490932,-23.21081514454,11.4219514862163));
#89073=CARTESIAN_POINT('Ctrl Pts',(7.83094794647299,-23.1735479550381,11.3628364646954));
#89074=CARTESIAN_POINT('Ctrl Pts',(7.75581025806313,-23.1726118741218,11.3069002853781));
#89075=CARTESIAN_POINT('Ctrl Pts',(7.97861893248622,-23.473260396731,11.5041318446739));
#89076=CARTESIAN_POINT('Ctrl Pts',(7.9838658852677,-23.3793118654716,11.4980034647542));
#89077=CARTESIAN_POINT('Ctrl Pts',(7.96094626176686,-23.2853633341106,11.4680133231507));
#89078=CARTESIAN_POINT('Ctrl Pts',(7.90635986062969,-23.2110860736012,11.4175510811059));
#89079=CARTESIAN_POINT('Ctrl Pts',(7.83296289653072,-23.1739766319726,11.3585003064285));
#89080=CARTESIAN_POINT('Ctrl Pts',(7.75850686040753,-23.1737472812249,11.3006412853113));
#89081=CARTESIAN_POINT('Ctrl Pts',(7.98975597461567,-23.4742457267098,11.4913611376641));
#89082=CARTESIAN_POINT('Ctrl Pts',(7.99160755459269,-23.3799440577819,11.4893633092269));
#89083=CARTESIAN_POINT('Ctrl Pts',(7.96482946649136,-23.285642388855,11.4637948888249));
#89084=CARTESIAN_POINT('Ctrl Pts',(7.91005112742093,-23.2110984877512,11.4131466533274));
#89085=CARTESIAN_POINT('Ctrl Pts',(7.84038338301816,-23.1741586517633,11.349542256543));
#89086=CARTESIAN_POINT('Ctrl Pts',(7.76929114060095,-23.1742407835368,11.2875250338872));
#89087=CARTESIAN_POINT('Ctrl Pts',(7.99571961591542,-23.4742355477988,11.4849187987967));
#89088=CARTESIAN_POINT('Ctrl Pts',(7.99569557118151,-23.3799375266448,11.4849447735798));
#89089=CARTESIAN_POINT('Ctrl Pts',(7.96848591980764,-23.2856395054908,11.459797141352));
#89090=CARTESIAN_POINT('Ctrl Pts',(7.91373170704263,-23.2111278317668,11.4091703379498));
#89091=CARTESIAN_POINT('Ctrl Pts',(7.8444766974065,-23.1741567081313,11.3451248634117));
#89092=CARTESIAN_POINT('Ctrl Pts',(7.77526352266813,-23.1742356855177,11.2810807525728));
#89093=CARTESIAN_POINT('',(7.77537149291,-23.1742356128,11.2813340821));
#89094=CARTESIAN_POINT('Origin',(7.77692918256182,-23.4721143225786,11.2827740387544));
#89095=CARTESIAN_POINT('Ctrl Pts',(7.77537149291,-23.1742356128,11.2813340821));
#89096=CARTESIAN_POINT('Ctrl Pts',(7.76374104627574,-23.1742356128017,11.293912717408));
#89097=CARTESIAN_POINT('Ctrl Pts',(7.75422556697312,-23.1727644436418,11.3086587661566));
#89098=CARTESIAN_POINT('Ctrl Pts',(7.74700423060917,-23.1697651572032,11.325378445193));
#89099=CARTESIAN_POINT('Ctrl Pts',(7.7425104458973,-23.1678987232268,11.3357829789599));
#89100=CARTESIAN_POINT('Ctrl Pts',(7.73890541557416,-23.1654413846783,11.3469514170409));
#89101=CARTESIAN_POINT('Ctrl Pts',(7.73623506584673,-23.1623888293302,11.3588340890296));
#89102=CARTESIAN_POINT('Ctrl Pts',(7.73275431717079,-23.1584098830982,11.3743229197122));
#89103=CARTESIAN_POINT('Ctrl Pts',(7.73086161191565,-23.153418739856,11.3910253167369));
#89104=CARTESIAN_POINT('Ctrl Pts',(7.73066226175709,-23.147426234148,11.4088273827439));
#89105=CARTESIAN_POINT('Ctrl Pts',(7.73056258667781,-23.144429981294,11.4177284157475));
#89106=CARTESIAN_POINT('Ctrl Pts',(7.73088630262042,-23.1411837592989,11.4269043094893));
#89107=CARTESIAN_POINT('Ctrl Pts',(7.73164678524262,-23.1376912299659,11.4363405978422));
#89108=CARTESIAN_POINT('Ctrl Pts',(7.73202702655371,-23.1359449652994,11.4410587420186));
#89109=CARTESIAN_POINT('Ctrl Pts',(7.73251645269071,-23.1341371416057,11.4458419922498));
#89110=CARTESIAN_POINT('Ctrl Pts',(7.73311675196239,-23.1322683759517,11.4506885225852));
#89111=CARTESIAN_POINT('Ctrl Pts',(7.73344741043022,-23.1312390174017,11.4533581015279));
#89112=CARTESIAN_POINT('Ctrl Pts',(7.7339045178077,-23.1299666679476,11.4566347081119));
#89113=CARTESIAN_POINT('Ctrl Pts',(7.73433695096052,-23.1288177725429,11.4595445510173));
#89114=CARTESIAN_POINT('Ctrl Pts',(7.73468958557988,-23.1278808871744,11.4619174295504));
#89115=CARTESIAN_POINT('Ctrl Pts',(7.73502509891724,-23.127027931523,11.4640471871358));
#89116=CARTESIAN_POINT('Ctrl Pts',(7.73525192860467,-23.1264799476953,11.4654161591939));
#89117=CARTESIAN_POINT('Ctrl Pts',(7.73848253767501,-23.1186753188378,11.4849136667643));
#89118=CARTESIAN_POINT('Ctrl Pts',(7.74349539285463,-23.1097913251982,11.5057237030058));
#89119=CARTESIAN_POINT('Ctrl Pts',(7.75044578480054,-23.0997931642341,11.5276783169699));
#89120=CARTESIAN_POINT('Ctrl Pts',(7.75218693764301,-23.0972885103214,11.5331781993948));
#89121=CARTESIAN_POINT('Ctrl Pts',(7.75404978036979,-23.0947141448011,11.5387498051114));
#89122=CARTESIAN_POINT('Ctrl Pts',(7.75603694220467,-23.0920699629726,11.5443902905449));
#89123=CARTESIAN_POINT('Ctrl Pts',(7.76099673254253,-23.0854703054841,11.5584684721317));
#89124=CARTESIAN_POINT('Ctrl Pts',(7.76673081976914,-23.0784351413131,11.5729759213888));
#89125=CARTESIAN_POINT('Ctrl Pts',(7.7732818622679,-23.0709684340554,11.5878665021477));
#89126=CARTESIAN_POINT('Ctrl Pts',(7.77655738351728,-23.0672350804265,11.5953117925271));
#89127=CARTESIAN_POINT('Ctrl Pts',(7.7800371228966,-23.0633938664975,11.6028528881567));
#89128=CARTESIAN_POINT('Ctrl Pts',(7.78372668136522,-23.0594462135951,11.6104837314509));
#89129=CARTESIAN_POINT('Ctrl Pts',(7.78557146059952,-23.0574723871439,11.614299153098));
#89130=CARTESIAN_POINT('Ctrl Pts',(7.78746869256675,-23.0554719535869,11.6181370138669));
#89131=CARTESIAN_POINT('Ctrl Pts',(7.78941907716873,-23.053445127409,11.6219965567953));
#89132=CARTESIAN_POINT('Ctrl Pts',(7.79039426946972,-23.0524317143201,11.6239263282596));
#89133=CARTESIAN_POINT('Ctrl Pts',(7.79138274980825,-23.0514117032099,11.6258615203947));
#89134=CARTESIAN_POINT('Ctrl Pts',(7.79238460634559,-23.0503851245528,11.627802037852));
#89135=CARTESIAN_POINT('Ctrl Pts',(7.79327498135915,-23.0494727783717,11.6295266243501));
#89136=CARTESIAN_POINT('Ctrl Pts',(7.79457377940076,-23.0481531572387,11.6320118167801));
#89137=CARTESIAN_POINT('Ctrl Pts',(7.79522040103178,-23.0474982175083,11.6332407477843));
#89138=CARTESIAN_POINT('Ctrl Pts',(7.79530136283287,-23.0474162142198,11.6333946190171));
#89139=CARTESIAN_POINT('Ctrl Pts',(7.79537206171456,-23.0473446716066,11.6335288379675));
#89140=CARTESIAN_POINT('Ctrl Pts',(7.7954303926167,-23.0472857178485,11.6336394709482));
#89141=CARTESIAN_POINT('Ctrl Pts',(7.80208355969398,-23.0405615084088,11.6462581632275));
#89142=CARTESIAN_POINT('Ctrl Pts',(7.80998678809139,-23.0329991199816,11.6602784378245));
#89143=CARTESIAN_POINT('Ctrl Pts',(7.81927494322304,-23.02451481789,11.6755544342307));
#89144=CARTESIAN_POINT('Ctrl Pts',(7.82866197294038,-23.0159401984164,11.6909930471946));
#89145=CARTESIAN_POINT('Ctrl Pts',(7.83946339968006,-23.0064225736304,11.7077144456189));
#89146=CARTESIAN_POINT('Ctrl Pts',(7.85185402085194,-22.9958996979574,11.7255295814866));
#89147=CARTESIAN_POINT('Ctrl Pts',(7.86292576688609,-22.9864968919653,11.7414484492459));
#89148=CARTESIAN_POINT('Ctrl Pts',(7.87526695740995,-22.9762909665692,11.7582400059061));
#89149=CARTESIAN_POINT('Ctrl Pts',(7.88902654132087,-22.9652683672498,11.7757431592995));
#89150=CARTESIAN_POINT('Ctrl Pts',(7.90232388219312,-22.9546160639972,11.7926583072079));
#89151=CARTESIAN_POINT('Ctrl Pts',(7.91694624226786,-22.943200344013,11.8102376925225));
#89152=CARTESIAN_POINT('Ctrl Pts',(7.93304631206559,-22.9310481852965,11.8283161764112));
#89153=CARTESIAN_POINT('Ctrl Pts',(7.94839546150332,-22.9194628131537,11.8455514650963));
#89154=CARTESIAN_POINT('Ctrl Pts',(7.9650881246001,-22.9072076806557,11.8632399135403));
#89155=CARTESIAN_POINT('Ctrl Pts',(7.98326798754674,-22.8943501383266,11.8812261213315));
#89156=CARTESIAN_POINT('Ctrl Pts',(7.99253469834919,-22.8877963415932,11.8903941214712));
#89157=CARTESIAN_POINT('Ctrl Pts',(8.00218796093379,-22.8810867861946,11.8996393229713));
#89158=CARTESIAN_POINT('Ctrl Pts',(8.01224741425247,-22.8742356128,11.9089404857865));
#89159=CARTESIAN_POINT('Origin',(6.6707290414,-22.8742356128,10.2599605573));
#89160=CARTESIAN_POINT('',(5.39652599911,-23.1742356128,9.08180806924));
#89161=CARTESIAN_POINT('Origin',(5.39652599911,-22.8742356128,9.08180806924));
#89162=CARTESIAN_POINT('',(6.58594874601,-23.1742356128,10.1815710757));
#89163=CARTESIAN_POINT('Origin',(4.98919124473,-22.8742356128,9.52235136777));
#89164=CARTESIAN_POINT('',(4.62185483489,-23.1742356128,9.04794230167));
#89165=CARTESIAN_POINT('Origin',(4.62185483489,-22.8742356128,9.04794230167));
#89166=CARTESIAN_POINT('Origin',(4.98919124473,-23.1742356128,9.52235136777));
#89167=CARTESIAN_POINT('Origin',(0.00234331738803,-22.8742356128,3.08191746407));
#89168=CARTESIAN_POINT('',(0.972828518105,-23.1742356128,10.5646641188));
#89169=CARTESIAN_POINT('Origin',(0.972828518105,-22.8742356128,10.5646641188));
#89170=CARTESIAN_POINT('Origin',(0.00234331738835,-23.1742356128,3.08191746407));
#89171=CARTESIAN_POINT('Origin',(1.05,-22.8742356128,11.1596805575));
#89172=CARTESIAN_POINT('',(0.45,-23.1742356128,11.1596805575));
#89173=CARTESIAN_POINT('Origin',(0.45,-22.8742356128,11.1596805575));
#89174=CARTESIAN_POINT('Origin',(1.05,-23.1742356128,11.1596805575));
#89175=CARTESIAN_POINT('Origin',(0.45,-22.8742356128,2.93538176615));
#89176=CARTESIAN_POINT('',(0.45,-23.1742356128,14.92922515));
#89177=CARTESIAN_POINT('Origin',(0.45,-22.8742356128,14.92922515));
#89178=CARTESIAN_POINT('',(0.45,-23.1742356128,13.0444528538));
#89179=CARTESIAN_POINT('Ctrl Pts',(8.78908955148,-23.4742356128,12.6272235745));
#89180=CARTESIAN_POINT('Ctrl Pts',(8.78908955148,-23.3799878332,12.6272235745));
#89181=CARTESIAN_POINT('Ctrl Pts',(8.76403540825,-23.2856521198,12.6543202923));
#89182=CARTESIAN_POINT('Ctrl Pts',(8.71344985896,-23.2111401141,12.7090299003));
#89183=CARTESIAN_POINT('Ctrl Pts',(8.64940616788,-23.1742356128,12.7782948442));
#89184=CARTESIAN_POINT('Ctrl Pts',(8.58542217429,-23.1742356128,12.8474952237));
#89185=CARTESIAN_POINT('Ctrl Pts',(8.71988917196,-23.4742356128,12.5632395809));
#89186=CARTESIAN_POINT('Ctrl Pts',(8.72947215345,-23.3790967554,12.5721001887));
#89187=CARTESIAN_POINT('Ctrl Pts',(8.71152123069,-23.285897088,12.6066774531));
#89188=CARTESIAN_POINT('Ctrl Pts',(8.66821560358,-23.2117943285,12.6661101146));
#89189=CARTESIAN_POINT('Ctrl Pts',(8.60980196734,-23.1742356128,12.7407571089));
#89190=CARTESIAN_POINT('Ctrl Pts',(8.55126681507,-23.1742356128,12.8159145257));
#89191=CARTESIAN_POINT('Ctrl Pts',(8.65068769611,-23.4557342571,12.4992545736));
#89192=CARTESIAN_POINT('Ctrl Pts',(8.67114447119,-23.3616092561,12.5181692988));
#89193=CARTESIAN_POINT('Ctrl Pts',(8.6616791149,-23.2705882254,12.5620766304));
#89194=CARTESIAN_POINT('Ctrl Pts',(8.62409294795,-23.1983198307,12.6285650769));
#89195=CARTESIAN_POINT('Ctrl Pts',(8.568611422,-23.16211697,12.707808508));
#89196=CARTESIAN_POINT('Ctrl Pts',(8.51298776904,-23.1652660131,12.7860692819));
#89197=CARTESIAN_POINT('Ctrl Pts',(8.58504814405,-23.4187037356,12.4385629891));
#89198=CARTESIAN_POINT('Ctrl Pts',(8.61720687318,-23.3287980114,12.4682975647));
#89199=CARTESIAN_POINT('Ctrl Pts',(8.61787660959,-23.2418003868,12.5228744536));
#89200=CARTESIAN_POINT('Ctrl Pts',(8.58556282332,-23.1726965799,12.5981338043));
#89201=CARTESIAN_POINT('Ctrl Pts',(8.53069999004,-23.1387145708,12.6814672949));
#89202=CARTESIAN_POINT('Ctrl Pts',(8.47363957019,-23.1456118409,12.7605886079));
#89203=CARTESIAN_POINT('Ctrl Pts',(8.46797276655,-23.3115821157,12.3303128573));
#89204=CARTESIAN_POINT('Ctrl Pts',(8.52237213304,-23.2378310806,12.3806115513));
#89205=CARTESIAN_POINT('Ctrl Pts',(8.54446981637,-23.1647358306,12.4578324878));
#89206=CARTESIAN_POINT('Ctrl Pts',(8.52245288296,-23.1060736658,12.5529815994));
#89207=CARTESIAN_POINT('Ctrl Pts',(8.46636077569,-23.0779179681,12.6438102103));
#89208=CARTESIAN_POINT('Ctrl Pts',(8.40034769996,-23.089880852,12.7198837328));
#89209=CARTESIAN_POINT('Ctrl Pts',(8.38931991359,-23.1521307593,12.2575889261));
#89210=CARTESIAN_POINT('Ctrl Pts',(8.45970633708,-23.1061611813,12.3226695586));
#89211=CARTESIAN_POINT('Ctrl Pts',(8.4993062219,-23.0588540528,12.4194802488));
#89212=CARTESIAN_POINT('Ctrl Pts',(8.48540796624,-23.0202466991,12.5332516118));
#89213=CARTESIAN_POINT('Ctrl Pts',(8.42613724507,-23.0015045278,12.6297956016));
#89214=CARTESIAN_POINT('Ctrl Pts',(8.34720486119,-23.0113292253,12.6980018322));
#89215=CARTESIAN_POINT('Ctrl Pts',(8.36213066678,-23.0627326652,12.2324492288));
#89216=CARTESIAN_POINT('Ctrl Pts',(8.43792182062,-23.0327194928,12.3025271783));
#89217=CARTESIAN_POINT('Ctrl Pts',(8.48363550117,-23.0005841899,12.4073998633));
#89218=CARTESIAN_POINT('Ctrl Pts',(8.47259449573,-22.9739829087,12.5290848856));
#89219=CARTESIAN_POINT('Ctrl Pts',(8.41152527253,-22.9610560938,12.6277894396));
#89220=CARTESIAN_POINT('Ctrl Pts',(8.32640121972,-22.9690248134,12.6908033837));
#89221=CARTESIAN_POINT('Ctrl Pts',(8.34854625295,-22.9684833924,12.2198888201));
#89222=CARTESIAN_POINT('Ctrl Pts',(8.42693586094,-22.9542535279,12.29236935));
#89223=CARTESIAN_POINT('Ctrl Pts',(8.47477476029,-22.9392158893,12.4011922791));
#89224=CARTESIAN_POINT('Ctrl Pts',(8.46499990031,-22.9265127562,12.5267357874));
#89225=CARTESIAN_POINT('Ctrl Pts',(8.40290084109,-22.9193127846,12.6268959398));
#89226=CARTESIAN_POINT('Ctrl Pts',(8.31471092647,-22.9207536636,12.6874600337));
#89227=CARTESIAN_POINT('Ctrl Pts',(8.34854625295,-22.8742356128,12.2198888201));
#89228=CARTESIAN_POINT('Ctrl Pts',(8.4275605919,-22.8742356128,12.2929469882));
#89229=CARTESIAN_POINT('Ctrl Pts',(8.47411942559,-22.8742356128,12.4014233916));
#89230=CARTESIAN_POINT('Ctrl Pts',(8.4651120838,-22.8742356128,12.5258960706));
#89231=CARTESIAN_POINT('Ctrl Pts',(8.40342053421,-22.8742356128,12.6265390425));
#89232=CARTESIAN_POINT('Ctrl Pts',(8.31471092647,-22.8742356128,12.6874600337));
#89233=CARTESIAN_POINT('',(8.58542217429,-23.1742356128,12.8474952237));
#89234=CARTESIAN_POINT('Origin',(8.58542217429,-23.4742356128,12.8474952237));
#89235=CARTESIAN_POINT('Ctrl Pts',(8.31471092647,-22.8742356128,12.6874600337));
#89236=CARTESIAN_POINT('Ctrl Pts',(8.31471092647,-22.8777933584003,12.6874600337));
#89237=CARTESIAN_POINT('Ctrl Pts',(8.31479323139441,-22.8809325043544,12.6874789206066));
#89238=CARTESIAN_POINT('Ctrl Pts',(8.31492315770647,-22.8839115627938,12.6875091517772));
#89239=CARTESIAN_POINT('Ctrl Pts',(8.31506107853501,-22.8870739261499,12.6875412431067));
#89240=CARTESIAN_POINT('Ctrl Pts',(8.31525325722673,-22.8900565885356,12.6875861793263));
#89241=CARTESIAN_POINT('Ctrl Pts',(8.31551250222541,-22.8931767624084,12.6876505482859));
#89242=CARTESIAN_POINT('Ctrl Pts',(8.31567428634882,-22.8951239343789,12.6876907183018));
#89243=CARTESIAN_POINT('Ctrl Pts',(8.31586311600635,-22.89712476739,12.6877387266233));
#89244=CARTESIAN_POINT('Ctrl Pts',(8.31609186404498,-22.899256284786,12.6877992720059));
#89245=CARTESIAN_POINT('Ctrl Pts',(8.31703246295758,-22.9080209629744,12.6880482311724));
#89246=CARTESIAN_POINT('Ctrl Pts',(8.3184720943893,-22.9172029832652,12.6884570892979));
#89247=CARTESIAN_POINT('Ctrl Pts',(8.32049148999543,-22.9267496321353,12.6890982804029));
#89248=CARTESIAN_POINT('Ctrl Pts',(8.32297113453986,-22.9384720978654,12.6898856080671));
#89249=CARTESIAN_POINT('Ctrl Pts',(8.32631087462861,-22.9507561859589,12.6910381665959));
#89250=CARTESIAN_POINT('Ctrl Pts',(8.33074250887902,-22.963423387773,12.6926430971044));
#89251=CARTESIAN_POINT('Ctrl Pts',(8.33352902430523,-22.9713882493269,12.6936522425724));
#89252=CARTESIAN_POINT('Ctrl Pts',(8.3367465938535,-22.9795039863439,12.6948406517394));
#89253=CARTESIAN_POINT('Ctrl Pts',(8.34044372268016,-22.9877227211584,12.6962343599784));
#89254=CARTESIAN_POINT('Ctrl Pts',(8.34224120057069,-22.9917185229845,12.6969119559896));
#89255=CARTESIAN_POINT('Ctrl Pts',(8.34390869384712,-22.995219463642,12.6975515515556));
#89256=CARTESIAN_POINT('Ctrl Pts',(8.34552920341066,-22.9984967024445,12.6981802531784));
#89257=CARTESIAN_POINT('Ctrl Pts',(8.34726210727647,-23.0020012419535,12.6988525599004));
#89258=CARTESIAN_POINT('Ctrl Pts',(8.34894196075464,-23.0052499587694,12.6995125290509));
#89259=CARTESIAN_POINT('Ctrl Pts',(8.35071808844439,-23.0085506780283,12.7002171923411));
#89260=CARTESIAN_POINT('Ctrl Pts',(8.35170576082534,-23.0103861481176,12.7006090428109));
#89261=CARTESIAN_POINT('Ctrl Pts',(8.35272393885807,-23.0122373070308,12.7010150983056));
#89262=CARTESIAN_POINT('Ctrl Pts',(8.3538036353473,-23.0141539170075,12.701448202217));
#89263=CARTESIAN_POINT('Ctrl Pts',(8.35864062942183,-23.022740247697,12.7033884892088));
#89264=CARTESIAN_POINT('Ctrl Pts',(8.36383403677917,-23.031093409479,12.7055393286181));
#89265=CARTESIAN_POINT('Ctrl Pts',(8.36933050847485,-23.0391865217467,12.7079039186945));
#89266=CARTESIAN_POINT('Ctrl Pts',(8.37670817730011,-23.0500495454068,12.7110778024979));
#89267=CARTESIAN_POINT('Ctrl Pts',(8.38462952763295,-23.0604448682787,12.7146360574884));
#89268=CARTESIAN_POINT('Ctrl Pts',(8.39305270598872,-23.0703067991067,12.7185390012323));
#89269=CARTESIAN_POINT('Ctrl Pts',(8.39710320140982,-23.0750491545425,12.720415829087));
#89270=CARTESIAN_POINT('Ctrl Pts',(8.40127001039262,-23.0796676000566,12.7223723738313));
#89271=CARTESIAN_POINT('Ctrl Pts',(8.40555038878184,-23.0841506907025,12.724404563646));
#89272=CARTESIAN_POINT('Ctrl Pts',(8.405631874623,-23.0842360355901,12.7244432505754));
#89273=CARTESIAN_POINT('Ctrl Pts',(8.40571340166903,-23.0843213313238,12.7244819649315));
#89274=CARTESIAN_POINT('Ctrl Pts',(8.40579496984911,-23.084406577819,12.7245207066686));
#89275=CARTESIAN_POINT('Ctrl Pts',(8.40850861987399,-23.0872425998286,12.7258095856842));
#89276=CARTESIAN_POINT('Ctrl Pts',(8.41092778889889,-23.0896803647717,12.7269739252582));
#89277=CARTESIAN_POINT('Ctrl Pts',(8.41326672462745,-23.0919820120415,12.7281155702397));
#89278=CARTESIAN_POINT('Ctrl Pts',(8.41566938155185,-23.0943463646327,12.7292883178216));
#89279=CARTESIAN_POINT('Ctrl Pts',(8.41798793352237,-23.0965670756276,12.7304373235459));
#89280=CARTESIAN_POINT('Ctrl Pts',(8.42048300223408,-23.0988941811888,12.731700441442));
#89281=CARTESIAN_POINT('Ctrl Pts',(8.42150070885261,-23.0998433777862,12.7322156510781));
#89282=CARTESIAN_POINT('Ctrl Pts',(8.42254806424813,-23.1008098845419,12.7327501444207));
#89283=CARTESIAN_POINT('Ctrl Pts',(8.42364392096638,-23.101808858012,12.73331460736));
#89284=CARTESIAN_POINT('Ctrl Pts',(8.43004185632291,-23.1076411603363,12.7366101088038));
#89285=CARTESIAN_POINT('Ctrl Pts',(8.43685251341664,-23.1134783932573,12.7403437273528));
#89286=CARTESIAN_POINT('Ctrl Pts',(8.44411972875044,-23.1191908462093,12.7445439750782));
#89287=CARTESIAN_POINT('Ctrl Pts',(8.45142329300889,-23.1249318715254,12.748765231468));
#89288=CARTESIAN_POINT('Ctrl Pts',(8.45918899558952,-23.1305448328952,12.753452576356));
#89289=CARTESIAN_POINT('Ctrl Pts',(8.46745203663362,-23.1358786540093,12.7586265124918));
#89290=CARTESIAN_POINT('Ctrl Pts',(8.4756328294368,-23.141159383604,12.7637489485632));
#89291=CARTESIAN_POINT('Ctrl Pts',(8.4843014823735,-23.1461660797944,12.7693486066843));
#89292=CARTESIAN_POINT('Ctrl Pts',(8.49345089413583,-23.1507232195509,12.7754411948738));
#89293=CARTESIAN_POINT('Ctrl Pts',(8.49676613901879,-23.1523744769925,12.7776488145922));
#89294=CARTESIAN_POINT('Ctrl Pts',(8.49966497227245,-23.1537362767192,12.7796135340646));
#89295=CARTESIAN_POINT('Ctrl Pts',(8.50237503110583,-23.154959764541,12.7814721598892));
#89296=CARTESIAN_POINT('Ctrl Pts',(8.5052438883696,-23.1562549437753,12.7834396936312));
#89297=CARTESIAN_POINT('Ctrl Pts',(8.50790164006921,-23.1573947053208,12.7852887419358));
#89298=CARTESIAN_POINT('Ctrl Pts',(8.51062282062748,-23.1585068781719,12.7872069045525));
#89299=CARTESIAN_POINT('Ctrl Pts',(8.51207455775593,-23.1591002171975,12.7882302353568));
#89300=CARTESIAN_POINT('Ctrl Pts',(8.51354438219107,-23.1596849239924,12.7892736043561));
#89301=CARTESIAN_POINT('Ctrl Pts',(8.51507388564811,-23.1602748447744,12.79036794282));
#89302=CARTESIAN_POINT('Ctrl Pts',(8.51588296434197,-23.1605869018238,12.7909468273795));
#89303=CARTESIAN_POINT('Ctrl Pts',(8.51671436748897,-23.1609023851636,12.7915440936407));
#89304=CARTESIAN_POINT('Ctrl Pts',(8.51754234275166,-23.1612111635393,12.7921414367448));
#89305=CARTESIAN_POINT('Ctrl Pts',(8.52886755029603,-23.1654346945393,12.8003120125255));
#89306=CARTESIAN_POINT('Ctrl Pts',(8.54029588627425,-23.1686990756866,12.8090252630494));
#89307=CARTESIAN_POINT('Ctrl Pts',(8.55166402911457,-23.1708993416419,12.8182595233406));
#89308=CARTESIAN_POINT('Ctrl Pts',(8.56115568234122,-23.1727364193202,12.8259695246768));
#89309=CARTESIAN_POINT('Ctrl Pts',(8.57060899114612,-23.1738324293023,12.8340455882575));
#89310=CARTESIAN_POINT('Ctrl Pts',(8.57991872237668,-23.1741433117178,12.8424633105735));
#89311=CARTESIAN_POINT('Ctrl Pts',(8.58175924620776,-23.1742047728364,12.8441274852035));
#89312=CARTESIAN_POINT('Ctrl Pts',(8.58359405486515,-23.1742356128,12.8458049095361));
#89313=CARTESIAN_POINT('Ctrl Pts',(8.58542217429,-23.1742356128,12.8474952237));
#89314=CARTESIAN_POINT('Origin',(8.14487887576,-22.8742356128,12.4401604693));
#89315=CARTESIAN_POINT('',(8.48454297717,-23.1742356128,12.9347595981));
#89316=CARTESIAN_POINT('Origin',(8.14487887576,-23.1742356128,12.4401604693));
#89317=CARTESIAN_POINT('Origin',(8.48454297717,-22.8742356128,12.9347595981));
#89318=CARTESIAN_POINT('Origin',(1.05,-22.8742356128,14.92922515));
#89319=CARTESIAN_POINT('',(1.09378792023,-23.1742356128,15.5276251985));
#89320=CARTESIAN_POINT('Origin',(1.09378792023,-22.8742356128,15.5276251985));
#89321=CARTESIAN_POINT('Origin',(1.05,-23.1742356128,14.92922515));
#89322=CARTESIAN_POINT('Origin',(-2.61864828395E-15,-22.8742356128,0.580061096523));
#89323=CARTESIAN_POINT('Origin',(3.98755858312E-16,-23.1742356128,0.580061096523));
#89324=CARTESIAN_POINT('Origin',(8.21591479143,-23.4742356128,11.6886688365));
#89325=CARTESIAN_POINT('',(7.85913400544,-23.1742356128,11.2062712093));
#89326=CARTESIAN_POINT('Origin',(7.85913400544,-23.4742356128,11.2062712093));
#89327=CARTESIAN_POINT('Origin',(8.21591479143,-23.1742356128,11.6886688365));
#89328=CARTESIAN_POINT('Origin',(2.30650470794E-14,-23.4742356128,0.580061096523));
#89329=CARTESIAN_POINT('',(8.48602987721,-23.1742356128,10.7126632105));
#89330=CARTESIAN_POINT('Origin',(8.48602987717703,-23.4742356128,10.7126632104571));
#89331=CARTESIAN_POINT('Origin',(-8.67605652836E-16,-23.1742356128,0.580061096523));
#89332=CARTESIAN_POINT('Ctrl Pts',(12.9732843937,-22.9031898545,8.97133867634));
#89333=CARTESIAN_POINT('Ctrl Pts',(12.9781011914,-22.9849535816,8.94914145692));
#89334=CARTESIAN_POINT('Ctrl Pts',(12.9535953066,-23.0667173088,8.92058122207));
#89335=CARTESIAN_POINT('Ctrl Pts',(12.8986935104,-23.1346740075,8.88934991896));
#89336=CARTESIAN_POINT('Ctrl Pts',(12.8237786321,-23.1759719524,8.86135389883));
#89337=CARTESIAN_POINT('Ctrl Pts',(12.7426122303,-23.1887127298,8.84011906693));
#89338=CARTESIAN_POINT('Ctrl Pts',(12.9823757633,-22.8915014019,8.92944287783));
#89339=CARTESIAN_POINT('Ctrl Pts',(12.9862583246,-22.9763016188,8.91126726307));
#89340=CARTESIAN_POINT('Ctrl Pts',(12.9595430587,-23.0611018356,8.88653324147));
#89341=CARTESIAN_POINT('Ctrl Pts',(12.9012478152,-23.1309752745,8.85841244838));
#89342=CARTESIAN_POINT('Ctrl Pts',(12.822883741,-23.172105454,8.83249977476));
#89343=CARTESIAN_POINT('Ctrl Pts',(12.7392305459,-23.1828685028,8.81230742555));
#89344=CARTESIAN_POINT('Ctrl Pts',(12.9914751666,-22.882822481,8.8868408148));
#89345=CARTESIAN_POINT('Ctrl Pts',(12.9944056315,-22.9704026765,8.87289342313));
#89346=CARTESIAN_POINT('Ctrl Pts',(12.9654027633,-23.0579828719,8.85218917069));
#89347=CARTESIAN_POINT('Ctrl Pts',(12.9035898329,-23.1294730391,8.82727742946));
#89348=CARTESIAN_POINT('Ctrl Pts',(12.8217308477,-23.1700741969,8.8033687928));
#89349=CARTESIAN_POINT('Ctrl Pts',(12.7356821525,-23.1785290452,8.78399143876));
#89350=CARTESIAN_POINT('Ctrl Pts',(13.000513389,-22.8770866751,8.84380834125));
#89351=CARTESIAN_POINT('Ctrl Pts',(13.0024779758,-22.9671810863,8.834295766));
#89352=CARTESIAN_POINT('Ctrl Pts',(12.9711165232,-23.0572754975,8.81782605389));
#89353=CARTESIAN_POINT('Ctrl Pts',(12.9056733165,-23.1300795876,8.79620887499));
#89354=CARTESIAN_POINT('Ctrl Pts',(12.820300204,-23.1698045819,8.77418794581));
#89355=CARTESIAN_POINT('Ctrl Pts',(12.731982211,-23.1756611501,8.75535198255));
#89356=CARTESIAN_POINT('Ctrl Pts',(13.0094376369,-22.8742356128,8.80057964365));
#89357=CARTESIAN_POINT('Ctrl Pts',(13.0104250706,-22.9665621944,8.79571296462));
#89358=CARTESIAN_POINT('Ctrl Pts',(12.97663939,-23.0588887759,8.78368803172));
#89359=CARTESIAN_POINT('Ctrl Pts',(12.9074626588,-23.1326978759,8.76544020738));
#89360=CARTESIAN_POINT('Ctrl Pts',(12.8185800084,-23.171217802,8.7451543519));
#89361=CARTESIAN_POINT('Ctrl Pts',(12.728148167,-23.1742356128,8.7265439874));
#89362=CARTESIAN_POINT('Ctrl Pts',(13.018207968,-22.8742356128,8.75735407375));
#89363=CARTESIAN_POINT('Ctrl Pts',(13.018207968,-22.9684833924,8.75735407375));
#89364=CARTESIAN_POINT('Ctrl Pts',(12.9819360276,-23.0627311721,8.74999461196));
#89365=CARTESIAN_POINT('Ctrl Pts',(12.9089301686,-23.1372245963,8.73518195451));
#89366=CARTESIAN_POINT('Ctrl Pts',(12.8165644307,-23.1742356128,8.71644123897));
#89367=CARTESIAN_POINT('Ctrl Pts',(12.7241986928,-23.1742356128,8.69770052342));
#89368=CARTESIAN_POINT('',(12.7426122114145,-23.1887126377471,8.8401190872892));
#89369=CARTESIAN_POINT('',(12.7241986928,-23.1742356128,8.69770052342));
#89370=CARTESIAN_POINT('Origin',(12.6973454005032,-23.4896761342038,8.67085289361702));
#89371=CARTESIAN_POINT('Origin',(12.7262776236387,-22.8763569039497,8.69812233191237));
#89372=CARTESIAN_POINT('Origin',(12.6820770505264,-22.9047706797711,8.90769738430112));
#89373=CARTESIAN_POINT('Ctrl Pts',(12.8222448424,-23.4742356815,9.46100292006));
#89374=CARTESIAN_POINT('Ctrl Pts',(12.8494736832,-23.4742356636,9.39375104048));
#89375=CARTESIAN_POINT('Ctrl Pts',(12.8563714436,-23.4742356458,9.31826754191));
#89376=CARTESIAN_POINT('Ctrl Pts',(12.8394938336,-23.4742356301,9.24276446755));
#89377=CARTESIAN_POINT('Ctrl Pts',(12.8011121316,-23.4742356188,9.17740252767));
#89378=CARTESIAN_POINT('Ctrl Pts',(12.7478394439,-23.4742356125,9.1281455822));
#89379=CARTESIAN_POINT('Ctrl Pts',(12.8222448265,-23.4046541603,9.4610029458));
#89380=CARTESIAN_POINT('Ctrl Pts',(12.8494736715,-23.4136498524,9.39375106135));
#89381=CARTESIAN_POINT('Ctrl Pts',(12.8563714358,-23.4226455445,9.31826755752));
#89382=CARTESIAN_POINT('Ctrl Pts',(12.8394938286,-23.4305372305,9.24276447831));
#89383=CARTESIAN_POINT('Ctrl Pts',(12.801112128,-23.4362628909,9.17740253498));
#89384=CARTESIAN_POINT('Ctrl Pts',(12.7478394405,-23.4394448584,9.12814558784));
#89385=CARTESIAN_POINT('Ctrl Pts',(12.8267376752,-23.3350444003,9.44989804488));
#89386=CARTESIAN_POINT('Ctrl Pts',(12.8532287465,-23.3530402345,9.38369795688));
#89387=CARTESIAN_POINT('Ctrl Pts',(12.8592761475,-23.3710360687,9.30931517965));
#89388=CARTESIAN_POINT('Ctrl Pts',(12.8415116196,-23.3868230014,9.23486539817));
#89389=CARTESIAN_POINT('Ctrl Pts',(12.8023354301,-23.3982761819,9.17041054742));
#89390=CARTESIAN_POINT('Ctrl Pts',(12.7484601992,-23.4046400789,9.12185309334));
#89391=CARTESIAN_POINT('Ctrl Pts',(12.8357660159,-23.2683909506,9.42765504858));
#89392=CARTESIAN_POINT('Ctrl Pts',(12.8607726482,-23.2950473443,9.36356310571));
#89393=CARTESIAN_POINT('Ctrl Pts',(12.8651123819,-23.3217037379,9.29138732719));
#89394=CARTESIAN_POINT('Ctrl Pts',(12.8455698325,-23.3450683354,9.21904951484));
#89395=CARTESIAN_POINT('Ctrl Pts',(12.8048034097,-23.3619761005,9.15641249749));
#89396=CARTESIAN_POINT('Ctrl Pts',(12.7497239393,-23.3713130963,9.10925542748));
#89397=CARTESIAN_POINT('Ctrl Pts',(12.8654176334,-23.1205674467,9.35093873948));
#89398=CARTESIAN_POINT('Ctrl Pts',(12.8856609251,-23.1667016048,9.29404448239));
#89399=CARTESIAN_POINT('Ctrl Pts',(12.88434645,-23.2128357629,9.22937157743));
#89400=CARTESIAN_POINT('Ctrl Pts',(12.8587400955,-23.2531200257,9.16420855068));
#89401=CARTESIAN_POINT('Ctrl Pts',(12.8124201304,-23.2819402616,9.10778516284));
#89402=CARTESIAN_POINT('Ctrl Pts',(12.7530521925,-23.2974017916,9.06547349059));
#89403=CARTESIAN_POINT('Ctrl Pts',(12.9068680488,-23.010101918,9.22909905079));
#89404=CARTESIAN_POINT('Ctrl Pts',(12.9207907755,-23.0719215919,9.18344085273));
#89405=CARTESIAN_POINT('Ctrl Pts',(12.9112658476,-23.1337412658,9.13042485238));
#89406=CARTESIAN_POINT('Ctrl Pts',(12.8761980932,-23.187134812,9.07635129743));
#89407=CARTESIAN_POINT('Ctrl Pts',(12.8208608743,-23.2240649689,9.02951363011));
#89408=CARTESIAN_POINT('Ctrl Pts',(12.7544308643,-23.2421683956,8.99467312589));
#89409=CARTESIAN_POINT('Ctrl Pts',(12.9314667335,-22.9612266295,9.14763068363));
#89410=CARTESIAN_POINT('Ctrl Pts',(12.9418297489,-23.0307478118,9.10939417332));
#89411=CARTESIAN_POINT('Ctrl Pts',(12.9272163182,-23.1002689941,9.06405821655));
#89412=CARTESIAN_POINT('Ctrl Pts',(12.8858996435,-23.1597742276,9.01725069446));
#89413=CARTESIAN_POINT('Ctrl Pts',(12.8244369644,-23.1997556874,8.97665312932));
#89414=CARTESIAN_POINT('Ctrl Pts',(12.7531935733,-23.2177311451,8.94663366293));
#89415=CARTESIAN_POINT('Ctrl Pts',(12.9538489501,-22.9261034781,9.0609030715));
#89416=CARTESIAN_POINT('Ctrl Pts',(12.9611499959,-23.0022194475,9.03052977793));
#89417=CARTESIAN_POINT('Ctrl Pts',(12.941507993,-23.078335417,8.99337186849));
#89418=CARTESIAN_POINT('Ctrl Pts',(12.8935474744,-23.1426522193,8.95421942683));
#89419=CARTESIAN_POINT('Ctrl Pts',(12.8254935651,-23.1840524297,8.91999612505));
#89420=CARTESIAN_POINT('Ctrl Pts',(12.7492414901,-23.2001695455,8.89463935599));
#89421=CARTESIAN_POINT('Ctrl Pts',(12.9732844032,-22.9031895891,8.9713386779));
#89422=CARTESIAN_POINT('Ctrl Pts',(12.9781011912,-22.9849533577,8.94914147504));
#89423=CARTESIAN_POINT('Ctrl Pts',(12.9535952945,-23.0667171263,8.92058125628));
#89424=CARTESIAN_POINT('Ctrl Pts',(12.8986934857,-23.1346738584,8.88934996626));
#89425=CARTESIAN_POINT('Ctrl Pts',(12.8237785974,-23.1759718213,8.86135395422));
#89426=CARTESIAN_POINT('Ctrl Pts',(12.7426121901,-23.188712601,8.84011912524));
#89427=CARTESIAN_POINT('Ctrl Pts',(12.7478394286,-23.4742356128,9.12814559875));
#89428=CARTESIAN_POINT('Ctrl Pts',(12.7478394405,-23.4394448584,9.12814558784));
#89429=CARTESIAN_POINT('Ctrl Pts',(12.7484601992,-23.4046400789,9.12185309334));
#89430=CARTESIAN_POINT('Ctrl Pts',(12.7497239393,-23.3713130963,9.10925542748));
#89431=CARTESIAN_POINT('Ctrl Pts',(12.7530521925,-23.2974017916,9.06547349059));
#89432=CARTESIAN_POINT('Ctrl Pts',(12.7544308643,-23.2421683956,8.99467312589));
#89433=CARTESIAN_POINT('Ctrl Pts',(12.7531935733,-23.2177311451,8.94663366293));
#89434=CARTESIAN_POINT('Ctrl Pts',(12.7492414901,-23.2001695455,8.89463935599));
#89435=CARTESIAN_POINT('Ctrl Pts',(12.7426122014,-23.188712592,8.84011909812));
#89436=CARTESIAN_POINT('Origin',(6.6707290414,-23.4742356128,3.1005467775));
#89437=CARTESIAN_POINT('',(11.9421544921,-23.1742356128,7.97460750747));
#89438=CARTESIAN_POINT('Origin',(11.9421544921158,-23.4742356128,7.97460750744535));
#89439=CARTESIAN_POINT('',(12.3331765925,-23.1742356128,8.33615401544));
#89440=CARTESIAN_POINT('Ctrl Pts',(3.81744045688,-22.8742356128,-9.21387212773));
#89441=CARTESIAN_POINT('Ctrl Pts',(3.81744045688,-22.9684833924,-9.21387212773));
#89442=CARTESIAN_POINT('Ctrl Pts',(3.80220506528,-23.0627311721,-9.18014234586));
#89443=CARTESIAN_POINT('Ctrl Pts',(3.77154023633,-23.1372245963,-9.11225318231));
#89444=CARTESIAN_POINT('Ctrl Pts',(3.73274363021,-23.1742356128,-9.02636099807));
#89445=CARTESIAN_POINT('Ctrl Pts',(3.69394702409,-23.1742356128,-8.94046881382));
#89446=CARTESIAN_POINT('Ctrl Pts',(3.71160470889,-22.8742356128,-9.26167703413));
#89447=CARTESIAN_POINT('Ctrl Pts',(3.72515638761,-22.9642074605,-9.25555588183));
#89448=CARTESIAN_POINT('Ctrl Pts',(3.7250970863,-23.0541793081,-9.21865622161));
#89449=CARTESIAN_POINT('Ctrl Pts',(3.70844285493,-23.1271496569,-9.15193510136));
#89450=CARTESIAN_POINT('Ctrl Pts',(3.67843010495,-23.1675189946,-9.06966143177));
#89451=CARTESIAN_POINT('Ctrl Pts',(3.64200986566,-23.1742356128,-8.98738776219));
#89452=CARTESIAN_POINT('Ctrl Pts',(3.60518947181,-22.8967702026,-9.30860522068));
#89453=CARTESIAN_POINT('Ctrl Pts',(3.63104913481,-22.9796757788,-9.29721692608));
#89454=CARTESIAN_POINT('Ctrl Pts',(3.64474315,-23.0625813551,-9.25775017492));
#89455=CARTESIAN_POINT('Ctrl Pts',(3.64141126432,-23.131420749,-9.19204052568));
#89456=CARTESIAN_POINT('Ctrl Pts',(3.62129881914,-23.1730680404,-9.11274337915));
#89457=CARTESIAN_POINT('Ctrl Pts',(3.58978817426,-23.1855028319,-9.03344623294));
#89458=CARTESIAN_POINT('Ctrl Pts',(3.50276689342,-22.9419634255,-9.35255588844));
#89459=CARTESIAN_POINT('Ctrl Pts',(3.53957219131,-23.0156863099,-9.33675316789));
#89460=CARTESIAN_POINT('Ctrl Pts',(3.56543990858,-23.0894091943,-9.29523917398));
#89461=CARTESIAN_POINT('Ctrl Pts',(3.57431565494,-23.1517903264,-9.2303724476));
#89462=CARTESIAN_POINT('Ctrl Pts',(3.56438630978,-23.1921341626,-9.15347743429));
#89463=CARTESIAN_POINT('Ctrl Pts',(3.53952573637,-23.2081001313,-9.07658241785));
#89464=CARTESIAN_POINT('Ctrl Pts',(3.34853990601,-23.0590627588,-9.41717252271));
#89465=CARTESIAN_POINT('Ctrl Pts',(3.40101481294,-23.1138397009,-9.39536923091));
#89466=CARTESIAN_POINT('Ctrl Pts',(3.44422712818,-23.1686166429,-9.35116723508));
#89467=CARTESIAN_POINT('Ctrl Pts',(3.47088045966,-23.2161685094,-9.28743732801));
#89468=CARTESIAN_POINT('Ctrl Pts',(3.47682492232,-23.2495777226,-9.21371939274));
#89469=CARTESIAN_POINT('Ctrl Pts',(3.4638420321,-23.2666487717,-9.14000145959));
#89470=CARTESIAN_POINT('Ctrl Pts',(3.24903060406,-23.2324009559,-9.45772855228));
#89471=CARTESIAN_POINT('Ctrl Pts',(3.31106586193,-23.2635682408,-9.43250094395));
#89472=CARTESIAN_POINT('Ctrl Pts',(3.36479660614,-23.2947355258,-9.38683384758));
#89473=CARTESIAN_POINT('Ctrl Pts',(3.40250113652,-23.322122922,-9.32374506153));
#89474=CARTESIAN_POINT('Ctrl Pts',(3.41904507547,-23.3420909713,-9.25177549042));
#89475=CARTESIAN_POINT('Ctrl Pts',(3.41500902577,-23.3533185645,-9.17980591789));
#89476=CARTESIAN_POINT('Ctrl Pts',(3.22037852073,-23.3101536719,-9.46927274181));
#89477=CARTESIAN_POINT('Ctrl Pts',(3.28511942878,-23.331162522,-9.44310189027));
#89478=CARTESIAN_POINT('Ctrl Pts',(3.34181908965,-23.3521713721,-9.39703707137));
#89479=CARTESIAN_POINT('Ctrl Pts',(3.38266593906,-23.3706950509,-9.33412380265));
#89480=CARTESIAN_POINT('Ctrl Pts',(3.40228901679,-23.384336583,-9.2626299648));
#89481=CARTESIAN_POINT('Ctrl Pts',(3.40094883361,-23.3921942807,-9.19113612813));
#89482=CARTESIAN_POINT('Ctrl Pts',(3.2061108834,-23.3922234913,-9.47502541989));
#89483=CARTESIAN_POINT('Ctrl Pts',(3.27219964976,-23.4027249383,-9.44838409371));
#89484=CARTESIAN_POINT('Ctrl Pts',(3.33037855145,-23.4132263854,-9.4021208728));
#89485=CARTESIAN_POINT('Ctrl Pts',(3.37279084839,-23.422485337,-9.33929519246));
#89486=CARTESIAN_POINT('Ctrl Pts',(3.393947035,-23.4293033961,-9.26803870195));
#89487=CARTESIAN_POINT('Ctrl Pts',(3.39394702816,-23.4332296702,-9.19678221123));
#89488=CARTESIAN_POINT('Ctrl Pts',(3.20611087388,-23.4742356128,-9.47502544833));
#89489=CARTESIAN_POINT('Ctrl Pts',(3.27219964627,-23.4742356465,-9.44838411889));
#89490=CARTESIAN_POINT('Ctrl Pts',(3.33037855462,-23.4742356801,-9.40212089616));
#89491=CARTESIAN_POINT('Ctrl Pts',(3.37279085872,-23.4742357098,-9.33929521563));
#89492=CARTESIAN_POINT('Ctrl Pts',(3.39394705252,-23.4742357316,-9.26803872592));
#89493=CARTESIAN_POINT('Ctrl Pts',(3.39394705213,-23.4742357442,-9.19678223621));
#89494=CARTESIAN_POINT('',(3.69394702409,-23.1742356128,-8.94046881382));
#89495=CARTESIAN_POINT('Ctrl Pts',(3.69394702409,-23.1742356128,-8.94046881382));
#89496=CARTESIAN_POINT('Ctrl Pts',(3.64200986566,-23.1742356128,-8.98738776219));
#89497=CARTESIAN_POINT('Ctrl Pts',(3.58978817426,-23.1855028319,-9.03344623294));
#89498=CARTESIAN_POINT('Ctrl Pts',(3.53952573637,-23.2081001313,-9.07658241785));
#89499=CARTESIAN_POINT('Ctrl Pts',(3.4638420321,-23.2666487717,-9.14000145959));
#89500=CARTESIAN_POINT('Ctrl Pts',(3.41500902577,-23.3533185645,-9.17980591789));
#89501=CARTESIAN_POINT('Ctrl Pts',(3.40094883361,-23.3921942807,-9.19113612813));
#89502=CARTESIAN_POINT('Ctrl Pts',(3.39394702816,-23.4332296702,-9.19678221123));
#89503=CARTESIAN_POINT('Ctrl Pts',(3.39394702409,-23.4742356128,-9.19678210318));
#89504=CARTESIAN_POINT('Origin',(3.69482032662239,-22.876356953309,-8.94240205678344));
#89505=CARTESIAN_POINT('Origin',(3.69394702409,-23.4742356128,3.39628270998));
#89506=CARTESIAN_POINT('',(3.69394702409,-23.1742356128,-8.44362980932));
#89507=CARTESIAN_POINT('Ctrl Pts',(9.06991786197,-22.8742351711,13.3798726472));
#89508=CARTESIAN_POINT('Ctrl Pts',(9.06991791346,-22.9684830268,13.3798726085));
#89509=CARTESIAN_POINT('Ctrl Pts',(9.04851963512,-23.0627308825,13.3496744364));
#89510=CARTESIAN_POINT('Ctrl Pts',(9.00545047601,-23.1372243637,13.2888935201));
#89511=CARTESIAN_POINT('Ctrl Pts',(8.95096009845,-23.1742354012,13.2119945921));
#89512=CARTESIAN_POINT('Ctrl Pts',(8.89646970336,-23.1742353894,13.1350956831));
#89513=CARTESIAN_POINT('Ctrl Pts',(9.22406041417,-22.8742363569,13.2706476151));
#89514=CARTESIAN_POINT('Ctrl Pts',(9.20132424908,-22.9647386701,13.2867584141));
#89515=CARTESIAN_POINT('Ctrl Pts',(9.15852680885,-23.0552409834,13.275328887));
#89516=CARTESIAN_POINT('Ctrl Pts',(9.10021479707,-23.128400233,13.232683254));
#89517=CARTESIAN_POINT('Ctrl Pts',(9.0393710411,-23.168352818,13.1677082076));
#89518=CARTESIAN_POINT('Ctrl Pts',(8.986120014,-23.1742360128,13.0945214235));
#89519=CARTESIAN_POINT('Ctrl Pts',(9.3768173424,-22.9427255764,13.1589191215));
#89520=CARTESIAN_POINT('Ctrl Pts',(9.33383370545,-23.019699187,13.1904054535));
#89521=CARTESIAN_POINT('Ctrl Pts',(9.27188264132,-23.0966727976,13.1965141601));
#89522=CARTESIAN_POINT('Ctrl Pts',(9.19881019143,-23.1602830893,13.1710975036));
#89523=CARTESIAN_POINT('Ctrl Pts',(9.1296041316,-23.1981089887,13.1188723071));
#89524=CARTESIAN_POINT('Ctrl Pts',(9.07411181992,-23.2084805514,13.051815332));
#89525=CARTESIAN_POINT('Ctrl Pts',(9.5056235281,-23.0835945845,13.0599834668));
#89526=CARTESIAN_POINT('Ctrl Pts',(9.44694848687,-23.1391655975,13.1046059873));
#89527=CARTESIAN_POINT('Ctrl Pts',(9.36995382261,-23.1947366105,13.1251829804));
#89528=CARTESIAN_POINT('Ctrl Pts',(9.2844923694,-23.2410848235,13.113878162));
#89529=CARTESIAN_POINT('Ctrl Pts',(9.20688851793,-23.2696054116,13.0728111063));
#89530=CARTESIAN_POINT('Ctrl Pts',(9.14715364651,-23.2789180606,13.0124182766));
#89531=CARTESIAN_POINT('Ctrl Pts',(9.57074430825,-23.2789184576,13.0098414435));
#89532=CARTESIAN_POINT('Ctrl Pts',(9.50407307406,-23.3067030636,13.0611772932));
#89533=CARTESIAN_POINT('Ctrl Pts',(9.41940322383,-23.3344876695,13.0891378612));
#89534=CARTESIAN_POINT('Ctrl Pts',(9.32764499777,-23.3576610293,13.0850021715));
#89535=CARTESIAN_POINT('Ctrl Pts',(9.2458338001,-23.3719208617,13.049538037));
#89536=CARTESIAN_POINT('Ctrl Pts',(9.18405109086,-23.3765770352,12.9924125631));
#89537=CARTESIAN_POINT('Ctrl Pts',(9.57074430825,-23.4742356128,13.0098414435));
#89538=CARTESIAN_POINT('Ctrl Pts',(9.50407307406,-23.4742356128,13.0611772932));
#89539=CARTESIAN_POINT('Ctrl Pts',(9.41940322382,-23.4742356128,13.0891378611));
#89540=CARTESIAN_POINT('Ctrl Pts',(9.32764499778,-23.4742356128,13.0850021715));
#89541=CARTESIAN_POINT('Ctrl Pts',(9.2458338001,-23.4742356128,13.049538037));
#89542=CARTESIAN_POINT('Ctrl Pts',(9.18405109086,-23.4742356128,12.9924125631));
#89543=CARTESIAN_POINT('',(8.89646971542626,-23.1742355011026,13.1350957106811));
#89544=CARTESIAN_POINT('Ctrl Pts',(8.89646970862946,-23.1742353894,13.1350956905365));
#89545=CARTESIAN_POINT('Ctrl Pts',(8.91341513014285,-23.1742355071256,13.1274264703531));
#89546=CARTESIAN_POINT('Ctrl Pts',(8.93029127126005,-23.1757068619148,13.1196632450321));
#89547=CARTESIAN_POINT('Ctrl Pts',(8.94689277562026,-23.1786594058135,13.11190151293));
#89548=CARTESIAN_POINT('Ctrl Pts',(8.96413730237382,-23.1817263099414,13.1038391473766));
#89549=CARTESIAN_POINT('Ctrl Pts',(8.98108480439148,-23.1863918522805,13.0957789597802));
#89550=CARTESIAN_POINT('Ctrl Pts',(8.99748754661613,-23.1926227295045,13.0878568815035));
#89551=CARTESIAN_POINT('Ctrl Pts',(9.01388437542077,-23.1988513604093,13.0799376592479));
#89552=CARTESIAN_POINT('Ctrl Pts',(9.02973598052021,-23.2066444162773,13.0721572366115));
#89553=CARTESIAN_POINT('Ctrl Pts',(9.04478970250645,-23.2159201010348,13.0646691125016));
#89554=CARTESIAN_POINT('Ctrl Pts',(9.05953393120249,-23.2250050846357,13.0573349386354));
#89555=CARTESIAN_POINT('Ctrl Pts',(9.07351197595636,-23.2355123975707,13.0502819205507));
#89556=CARTESIAN_POINT('Ctrl Pts',(9.08649348099754,-23.2473169973954,13.0436598229282));
#89557=CARTESIAN_POINT('Ctrl Pts',(9.09906099757469,-23.258745141013,13.0372489082166));
#89558=CARTESIAN_POINT('Ctrl Pts',(9.11069392323561,-23.2713890780425,13.0312424769986));
#89559=CARTESIAN_POINT('Ctrl Pts',(9.12119976253034,-23.28509010912,13.0257718268833));
#89560=CARTESIAN_POINT('Ctrl Pts',(9.13117359321529,-23.2980973292328,13.0205782067968));
#89561=CARTESIAN_POINT('Ctrl Pts',(9.14013124265935,-23.3120570858951,13.0158678825228));
#89562=CARTESIAN_POINT('Ctrl Pts',(9.14792971774513,-23.3267943578383,13.0117419122437));
#89563=CARTESIAN_POINT('Ctrl Pts',(9.1554919724439,-23.3410852291655,13.0077409200259));
#89564=CARTESIAN_POINT('Ctrl Pts',(9.16196389354133,-23.3561071559953,13.004289751406));
#89565=CARTESIAN_POINT('Ctrl Pts',(9.16724094845525,-23.3716644543252,13.0014643636574));
#89566=CARTESIAN_POINT('Ctrl Pts',(9.17238371002682,-23.3868258421284,12.9987108779015));
#89567=CARTESIAN_POINT('Ctrl Pts',(9.17639137749551,-23.4024956538032,12.9965520057846));
#89568=CARTESIAN_POINT('Ctrl Pts',(9.17919641784377,-23.4184587554085,12.9950379956692));
#89569=CARTESIAN_POINT('Ctrl Pts',(9.18191243967219,-23.4339152647724,12.9935720329694));
#89570=CARTESIAN_POINT('Ctrl Pts',(9.18350078228183,-23.449646661283,12.9927108436825));
#89571=CARTESIAN_POINT('Ctrl Pts',(9.1839310101514,-23.4654263360779,12.9924776563453));
#89572=CARTESIAN_POINT('Ctrl Pts',(9.18401104207622,-23.4683617055323,12.9924342783293));
#89573=CARTESIAN_POINT('Ctrl Pts',(9.18405109089593,-23.4712986577741,12.9924125631332));
#89574=CARTESIAN_POINT('Ctrl Pts',(9.18405109086,-23.4742356128,12.9924125631));
#89575=CARTESIAN_POINT('',(9.069917864047,-22.8742353916481,13.3798726501317));
#89576=CARTESIAN_POINT('Ctrl Pts',(9.06991786197,-22.8742351711,13.3798726472));
#89577=CARTESIAN_POINT('Ctrl Pts',(9.08998575407497,-22.8742353255134,13.3656525883774));
#89578=CARTESIAN_POINT('Ctrl Pts',(9.10955660519836,-22.8756242289139,13.3517136535672));
#89579=CARTESIAN_POINT('Ctrl Pts',(9.12864703192581,-22.8782518413693,13.3380519691444));
#89580=CARTESIAN_POINT('Ctrl Pts',(9.14793774246996,-22.8809070209535,13.3242469555893));
#89581=CARTESIAN_POINT('Ctrl Pts',(9.16673844715609,-22.88482699622,13.310724778741));
#89582=CARTESIAN_POINT('Ctrl Pts',(9.18507464936658,-22.889909819839,13.2974764327235));
#89583=CARTESIAN_POINT('Ctrl Pts',(9.20358499520628,-22.8950409163415,13.2841022637558));
#89584=CARTESIAN_POINT('Ctrl Pts',(9.22162263549148,-22.9013571522458,13.271006726178));
#89585=CARTESIAN_POINT('Ctrl Pts',(9.23921303209337,-22.9088067632157,13.2581807473248));
#89586=CARTESIAN_POINT('Ctrl Pts',(9.25678868288205,-22.9162501292683,13.245365520332));
#89587=CARTESIAN_POINT('Ctrl Pts',(9.27391854665928,-22.9248252575798,13.232818884081));
#89588=CARTESIAN_POINT('Ctrl Pts',(9.29061694379971,-22.934530243736,13.2205390954791));
#89589=CARTESIAN_POINT('Ctrl Pts',(9.30710079952112,-22.9441105399902,13.2084170779046));
#89590=CARTESIAN_POINT('Ctrl Pts',(9.32316487751703,-22.9547923032227,13.1965545677702));
#89591=CARTESIAN_POINT('Ctrl Pts',(9.33880195550392,-22.9666165308916,13.1849647453894));
#89592=CARTESIAN_POINT('Ctrl Pts',(9.35387417400676,-22.9780136309893,13.1737935831378));
#89593=CARTESIAN_POINT('Ctrl Pts',(9.36855017700297,-22.9904727776667,13.1628753549093));
#89594=CARTESIAN_POINT('Ctrl Pts',(9.382795583024,-23.004062622776,13.1522424354472));
#89595=CARTESIAN_POINT('Ctrl Pts',(9.39534907250807,-23.0160384118421,13.1428723801146));
#89596=CARTESIAN_POINT('Ctrl Pts',(9.4075680781392,-23.0288929873676,13.1337239314646));
#89597=CARTESIAN_POINT('Ctrl Pts',(9.41940527139236,-23.0426889421547,13.1248372557628));
#89598=CARTESIAN_POINT('Ctrl Pts',(9.43131771533443,-23.0565725997511,13.1158940862238));
#89599=CARTESIAN_POINT('Ctrl Pts',(9.44248897416376,-23.0710261714051,13.1074823780018));
#89600=CARTESIAN_POINT('Ctrl Pts',(9.4529877344115,-23.0860428865014,13.0995587831363));
#89601=CARTESIAN_POINT('Ctrl Pts',(9.46345139189945,-23.1010093929892,13.0916616809272));
#89602=CARTESIAN_POINT('Ctrl Pts',(9.47324759923271,-23.1165359483353,13.0842489546468));
#89603=CARTESIAN_POINT('Ctrl Pts',(9.48241933488591,-23.13265844651,13.0772947232701));
#89604=CARTESIAN_POINT('Ctrl Pts',(9.4916372236028,-23.1488620746599,13.0703054975265));
#89605=CARTESIAN_POINT('Ctrl Pts',(9.50022492714466,-23.165668329315,13.0637789008759));
#89606=CARTESIAN_POINT('Ctrl Pts',(9.50819213354862,-23.183146856145,13.0577131974299));
#89607=CARTESIAN_POINT('Ctrl Pts',(9.51615933995259,-23.200625382975,13.0516474939839));
#89608=CARTESIAN_POINT('Ctrl Pts',(9.52350662524997,-23.2187770242996,13.0460422080318));
#89609=CARTESIAN_POINT('Ctrl Pts',(9.53020114144296,-23.237693246794,13.0409273075514));
#89610=CARTESIAN_POINT('Ctrl Pts',(9.53760959696005,-23.2586267973092,13.0352669264887));
#89611=CARTESIAN_POINT('Ctrl Pts',(9.54395926915395,-23.2798231161351,13.0304053695222));
#89612=CARTESIAN_POINT('Ctrl Pts',(9.54930506873862,-23.3012669711949,13.0263077604947));
#89613=CARTESIAN_POINT('Ctrl Pts',(9.55465924086306,-23.3227444114139,13.0222037338315));
#89614=CARTESIAN_POINT('Ctrl Pts',(9.55900668819699,-23.344471439241,13.0188657804003));
#89615=CARTESIAN_POINT('Ctrl Pts',(9.56236311517375,-23.3664524350163,13.0162868858771));
#89616=CARTESIAN_POINT('Ctrl Pts',(9.5656336340413,-23.3878708248423,13.0137739984365));
#89617=CARTESIAN_POINT('Ctrl Pts',(9.56796318463351,-23.409531684921,13.0119818130114));
#89618=CARTESIAN_POINT('Ctrl Pts',(9.56932722686825,-23.4314384942518,13.0109321578799));
#89619=CARTESIAN_POINT('Ctrl Pts',(9.57020916152404,-23.4456025529991,13.0102534932363));
#89620=CARTESIAN_POINT('Ctrl Pts',(9.57068667570032,-23.4598693913192,13.0098858196983));
#89621=CARTESIAN_POINT('Ctrl Pts',(9.57074430825,-23.4742356128,13.0098414435));
#89622=CARTESIAN_POINT('Origin',(8.89769590716719,-22.8763565140159,13.1368267800033));
#89623=CARTESIAN_POINT('Origin',(6.6707290414,-23.4742356128,11.0771333555));
#89624=CARTESIAN_POINT('',(8.74094594938,-23.1742356128,12.9912954789));
#89625=CARTESIAN_POINT('Origin',(-2.84607155346,-22.8742356128,5.53854202767));
#89626=CARTESIAN_POINT('Origin',(-2.84607155346,-23.1742356128,5.53854202767));
#89627=CARTESIAN_POINT('Origin',(10.1862176145,-22.8742356128,9.72278707155));
#89628=CARTESIAN_POINT('',(11.1383462684,-22.8742356128,10.0284846777));
#89629=CARTESIAN_POINT('Ctrl Pts',(11.138346268408,-22.8742356128,10.0284846777026));
#89630=CARTESIAN_POINT('Ctrl Pts',(11.1304025349713,-22.8879754443996,10.0532263049571));
#89631=CARTESIAN_POINT('Ctrl Pts',(11.1227115500163,-22.9011602400043,10.0769601464436));
#89632=CARTESIAN_POINT('Ctrl Pts',(11.1149362788915,-22.9142785484054,10.1007522253721));
#89633=CARTESIAN_POINT('Ctrl Pts',(11.1089402979403,-22.9243948679554,10.1190997337428));
#89634=CARTESIAN_POINT('Ctrl Pts',(11.1028949842124,-22.9344737618983,10.1374798306995));
#89635=CARTESIAN_POINT('Ctrl Pts',(11.0966317645807,-22.9447233863069,10.1563922783035));
#89636=CARTESIAN_POINT('Ctrl Pts',(11.0947731720942,-22.9477649329931,10.1620044929607));
#89637=CARTESIAN_POINT('Ctrl Pts',(11.0928952369663,-22.9508212969781,10.1676637551768));
#89638=CARTESIAN_POINT('Ctrl Pts',(11.090993057621,-22.9538972342935,10.1733836478105));
#89639=CARTESIAN_POINT('',(10.9304145503,-22.8742356128,10.3907473403));
#89640=CARTESIAN_POINT('Ctrl Pts',(10.9304145503437,-22.8742356128,10.3907473403392));
#89641=CARTESIAN_POINT('Ctrl Pts',(10.9481405479233,-22.8882672659973,10.3709982119854));
#89642=CARTESIAN_POINT('Ctrl Pts',(10.9645717766644,-22.9013026990597,10.3525880372788));
#89643=CARTESIAN_POINT('Ctrl Pts',(10.9810103536057,-22.9142753573368,10.3340804995609));
#89644=CARTESIAN_POINT('Ctrl Pts',(10.992000443497,-22.9229482905903,10.3217071959644));
#89645=CARTESIAN_POINT('Ctrl Pts',(11.002992272732,-22.9315950772944,10.3092917362859));
#89646=CARTESIAN_POINT('Ctrl Pts',(11.0143770648586,-22.9404798718002,10.2963873039649));
#89647=CARTESIAN_POINT('Ctrl Pts',(11.0200212309283,-22.944884629931,10.2899897555297));
#89648=CARTESIAN_POINT('Ctrl Pts',(11.0257621179678,-22.9493475068719,10.2834716325873));
#89649=CARTESIAN_POINT('Ctrl Pts',(11.031648508022,-22.9538972342928,10.2767748704144));
#89650=CARTESIAN_POINT('Origin',(10.1862176145,-22.8742356128,9.72278707155));
#89651=CARTESIAN_POINT('Ctrl Pts',(11.9005548436,-23.1693861532,7.89557218486));
#89652=CARTESIAN_POINT('Ctrl Pts',(11.8339499555,-23.1595472711,7.96980237474));
#89653=CARTESIAN_POINT('Ctrl Pts',(11.7599452826,-23.1908783468,8.04284981847));
#89654=CARTESIAN_POINT('Ctrl Pts',(11.6942870876,-23.2663663442,8.09701806802));
#89655=CARTESIAN_POINT('Ctrl Pts',(11.6548578916,-23.3654515188,8.11755397837));
#89656=CARTESIAN_POINT('Ctrl Pts',(11.6438378503,-23.4645366935,8.10736463748));
#89657=CARTESIAN_POINT('Ctrl Pts',(11.8668157199,-23.1614761236,7.83132058431));
#89658=CARTESIAN_POINT('Ctrl Pts',(11.8129234492,-23.1460753827,7.92069454621));
#89659=CARTESIAN_POINT('Ctrl Pts',(11.7451516804,-23.1734640687,8.00787961054));
#89660=CARTESIAN_POINT('Ctrl Pts',(11.6772007057,-23.2482114783,8.07033400293));
#89661=CARTESIAN_POINT('Ctrl Pts',(11.6288782137,-23.3484640563,8.08997448939));
#89662=CARTESIAN_POINT('Ctrl Pts',(11.6054955414,-23.4487166343,8.07191260584));
#89663=CARTESIAN_POINT('Ctrl Pts',(11.8201190291,-23.1436931675,7.77911937176));
#89664=CARTESIAN_POINT('Ctrl Pts',(11.7896480761,-23.1271929291,7.88233980762));
#89665=CARTESIAN_POINT('Ctrl Pts',(11.7361184989,-23.1516755686,7.98200912796));
#89666=CARTESIAN_POINT('Ctrl Pts',(11.6667987778,-23.2222222498,8.05091722103));
#89667=CARTESIAN_POINT('Ctrl Pts',(11.6024958012,-23.3176864267,8.06826984747));
#89668=CARTESIAN_POINT('Ctrl Pts',(11.5554237252,-23.4131506081,8.04186749464));
#89669=CARTESIAN_POINT('Ctrl Pts',(11.7752729456,-23.1083028984,7.76843597189));
#89670=CARTESIAN_POINT('Ctrl Pts',(11.7595402729,-23.1052304081,7.86585583205));
#89671=CARTESIAN_POINT('Ctrl Pts',(11.7167014673,-23.1327309513,7.95914759566));
#89672=CARTESIAN_POINT('Ctrl Pts',(11.6496136328,-23.1915820263,8.02617572742));
#89673=CARTESIAN_POINT('Ctrl Pts',(11.5756983226,-23.2669761984,8.04953640203));
#89674=CARTESIAN_POINT('Ctrl Pts',(11.5102889752,-23.3423703627,8.03319245204));
#89675=CARTESIAN_POINT('Ctrl Pts',(11.717675025,-23.0445100599,7.76252036052));
#89676=CARTESIAN_POINT('Ctrl Pts',(11.7084114695,-23.0501289834,7.8515782493));
#89677=CARTESIAN_POINT('Ctrl Pts',(11.6708968566,-23.0738598269,7.93631728547));
#89678=CARTESIAN_POINT('Ctrl Pts',(11.6066799831,-23.1148476696,8.0001560579));
#89679=CARTESIAN_POINT('Ctrl Pts',(11.5292674801,-23.1648160129,8.02969505599));
#89680=CARTESIAN_POINT('Ctrl Pts',(11.4529027709,-23.2147843626,8.02583184946));
#89681=CARTESIAN_POINT('Ctrl Pts',(11.6840057838,-22.9724912879,7.77196745159));
#89682=CARTESIAN_POINT('Ctrl Pts',(11.6739934323,-22.9791841994,7.85280062059));
#89683=CARTESIAN_POINT('Ctrl Pts',(11.6374046012,-22.9945001244,7.92955173236));
#89684=CARTESIAN_POINT('Ctrl Pts',(11.575491188,-23.017355905,7.98966707089));
#89685=CARTESIAN_POINT('Ctrl Pts',(11.4989860406,-23.044051495,8.02274251311));
#89686=CARTESIAN_POINT('Ctrl Pts',(11.4203500465,-23.0707470797,8.02802946276));
#89687=CARTESIAN_POINT('Ctrl Pts',(11.674734675,-22.9402340389,7.77528500471));
#89688=CARTESIAN_POINT('Ctrl Pts',(11.6632751245,-22.9448939304,7.85395206414));
#89689=CARTESIAN_POINT('Ctrl Pts',(11.6261291027,-22.9551888401,7.92866239052));
#89690=CARTESIAN_POINT('Ctrl Pts',(11.5648099781,-22.9704904338,7.98774399745));
#89691=CARTESIAN_POINT('Ctrl Pts',(11.4893943947,-22.9883613924,8.02148806052));
#89692=CARTESIAN_POINT('Ctrl Pts',(11.4114432261,-23.0062323557,8.02896986926));
#89693=CARTESIAN_POINT('Ctrl Pts',(11.6698654776,-22.907226316,7.77708988832));
#89694=CARTESIAN_POINT('Ctrl Pts',(11.6579204713,-22.9095613324,7.85454768026));
#89695=CARTESIAN_POINT('Ctrl Pts',(11.6206811584,-22.914710848,7.92810475864));
#89696=CARTESIAN_POINT('Ctrl Pts',(11.5596933648,-22.9223583919,7.98661599137));
#89697=CARTESIAN_POINT('Ctrl Pts',(11.4846565636,-22.931287768,8.02077577683));
#89698=CARTESIAN_POINT('Ctrl Pts',(11.4067703651,-22.9402171391,8.02950137053));
#89699=CARTESIAN_POINT('Ctrl Pts',(11.6698655273,-22.8742356121,7.77708987718));
#89700=CARTESIAN_POINT('Ctrl Pts',(11.6579205194,-22.8742356226,7.85454767439));
#89701=CARTESIAN_POINT('Ctrl Pts',(11.6206812044,-22.8742356357,7.92810475784));
#89702=CARTESIAN_POINT('Ctrl Pts',(11.5596934089,-22.87423565,7.98661599254));
#89703=CARTESIAN_POINT('Ctrl Pts',(11.4846566078,-22.8742356631,8.02077577467));
#89704=CARTESIAN_POINT('Ctrl Pts',(11.4067704135,-22.8742356736,8.02950136067));
#89705=CARTESIAN_POINT('',(11.669865562592,-22.8742356128,7.77708987370031));
#89706=CARTESIAN_POINT('Origin',(11.3748952831028,-22.8742356444552,7.73295572116956));
#89707=CARTESIAN_POINT('',(11.9005548348247,-23.1693861585283,7.89557218624769));
#89708=CARTESIAN_POINT('Ctrl Pts',(11.6698655614,-22.8742356128,7.77708988131));
#89709=CARTESIAN_POINT('Ctrl Pts',(11.6698654776,-22.907226316,7.77708988832));
#89710=CARTESIAN_POINT('Ctrl Pts',(11.674734675,-22.9402340389,7.77528500471));
#89711=CARTESIAN_POINT('Ctrl Pts',(11.6840057838,-22.9724912879,7.77196745159));
#89712=CARTESIAN_POINT('Ctrl Pts',(11.717675025,-23.0445100599,7.76252036052));
#89713=CARTESIAN_POINT('Ctrl Pts',(11.7752729456,-23.1083028984,7.76843597189));
#89714=CARTESIAN_POINT('Ctrl Pts',(11.8201190291,-23.1436931675,7.77911937176));
#89715=CARTESIAN_POINT('Ctrl Pts',(11.8668157199,-23.1614761236,7.83132058431));
#89716=CARTESIAN_POINT('Ctrl Pts',(11.900554836,-23.1693861518,7.89557218629));
#89717=CARTESIAN_POINT('Ctrl Pts',(11.6438378503,-23.4645366935,8.10736463748));
#89718=CARTESIAN_POINT('Ctrl Pts',(11.6457407548972,-23.4474269895683,8.10912409945425));
#89719=CARTESIAN_POINT('Ctrl Pts',(11.6486630325428,-23.4303180321677,8.10978091601121));
#89720=CARTESIAN_POINT('Ctrl Pts',(11.65256298317,-23.4134680180269,8.10932257821117));
#89721=CARTESIAN_POINT('Ctrl Pts',(11.6565377789634,-23.3962946300209,8.10885544430778));
#89722=CARTESIAN_POINT('Ctrl Pts',(11.6615279369715,-23.37939060852,8.10723006852047));
#89723=CARTESIAN_POINT('Ctrl Pts',(11.6674552116862,-23.3630165572466,8.10447292972245));
#89724=CARTESIAN_POINT('Ctrl Pts',(11.6735237627704,-23.3462522310777,8.10165007462501));
#89725=CARTESIAN_POINT('Ctrl Pts',(11.6805744213503,-23.3300439067293,8.09764098964142));
#89726=CARTESIAN_POINT('Ctrl Pts',(11.6884909237533,-23.3146514397464,8.09251343822578));
#89727=CARTESIAN_POINT('Ctrl Pts',(11.6964815336893,-23.2991148816364,8.0873378870539));
#89728=CARTESIAN_POINT('Ctrl Pts',(11.7053539547591,-23.2844099860543,8.08102307394607));
#89729=CARTESIAN_POINT('Ctrl Pts',(11.7149602963441,-23.2707770127254,8.073675339938));
#89730=CARTESIAN_POINT('Ctrl Pts',(11.7245993021421,-23.2570976835241,8.06630262160608));
#89731=CARTESIAN_POINT('Ctrl Pts',(11.7349768686908,-23.2444980259262,8.05789023480772));
#89732=CARTESIAN_POINT('Ctrl Pts',(11.745920364852,-23.2331869359498,8.04857827595082));
#89733=CARTESIAN_POINT('Ctrl Pts',(11.756829296706,-23.2219115713012,8.03929572829864));
#89734=CARTESIAN_POINT('Ctrl Pts',(11.7683002094792,-23.2119170519958,8.02911960219298));
#89735=CARTESIAN_POINT('Ctrl Pts',(11.7801446348235,-23.2033704216458,8.01821646048037));
#89736=CARTESIAN_POINT('Ctrl Pts',(11.7918096503827,-23.1949532487468,8.00747847074887));
#89737=CARTESIAN_POINT('Ctrl Pts',(11.8038365705567,-23.1879407235758,7.99603566767177));
#89738=CARTESIAN_POINT('Ctrl Pts',(11.8160340495087,-23.1824486649995,7.98406915540296));
#89739=CARTESIAN_POINT('Ctrl Pts',(11.8280723255704,-23.1770282893999,7.97225883142101));
#89740=CARTESIAN_POINT('Ctrl Pts',(11.840276398251,-23.1730892198954,7.95993868610934));
#89741=CARTESIAN_POINT('Ctrl Pts',(11.8524564888357,-23.1706957080467,7.94729963439744));
#89742=CARTESIAN_POINT('Ctrl Pts',(11.8643709607006,-23.1683543929817,7.93493621025267));
#89743=CARTESIAN_POINT('Ctrl Pts',(11.8762621855935,-23.1674921212114,7.92226792528629));
#89744=CARTESIAN_POINT('Ctrl Pts',(11.8879515998144,-23.1681206308898,7.90948528184542));
#89745=CARTESIAN_POINT('Ctrl Pts',(11.892181889249,-23.1683480826509,7.90485936300358));
#89746=CARTESIAN_POINT('Ctrl Pts',(11.8963857612096,-23.1687702957837,7.90021856034556));
#89747=CARTESIAN_POINT('Ctrl Pts',(11.9005548359276,-23.1693861518639,7.89557218635399));
#89748=CARTESIAN_POINT('Ctrl Pts',(11.9421544921,-23.1742356128,7.97460750747));
#89749=CARTESIAN_POINT('Ctrl Pts',(11.8781704985,-23.1742356128,8.04380788698));
#89750=CARTESIAN_POINT('Ctrl Pts',(11.8141865049,-23.2112466293,8.11300826649));
#89751=CARTESIAN_POINT('Ctrl Pts',(11.7636135705,-23.2857400536,8.16770423124));
#89752=CARTESIAN_POINT('Ctrl Pts',(11.7384871149,-23.3799878332,8.19487915673));
#89753=CARTESIAN_POINT('Ctrl Pts',(11.7384871149,-23.4742356128,8.19487915673));
#89754=CARTESIAN_POINT('Ctrl Pts',(11.9338050766,-23.1742356128,7.95878179633));
#89755=CARTESIAN_POINT('Ctrl Pts',(11.8690129979,-23.1723658919,8.02885614127));
#89756=CARTESIAN_POINT('Ctrl Pts',(11.8029049395,-23.2084420454,8.09871370492));
#89757=CARTESIAN_POINT('Ctrl Pts',(11.7493954495,-23.283359451,8.15328464759));
#89758=CARTESIAN_POINT('Ctrl Pts',(11.7215525483,-23.3787975319,8.17922113275));
#89759=CARTESIAN_POINT('Ctrl Pts',(11.7194707712,-23.4742356128,8.17729628178));
#89760=CARTESIAN_POINT('Ctrl Pts',(11.925456866,-23.1737486504,7.94293960289));
#89761=CARTESIAN_POINT('Ctrl Pts',(11.8599896787,-23.169946111,8.01395123592));
#89762=CARTESIAN_POINT('Ctrl Pts',(11.7918088017,-23.204981018,8.08451905773));
#89763=CARTESIAN_POINT('Ctrl Pts',(11.7353200262,-23.2802129884,8.13897414048));
#89764=CARTESIAN_POINT('Ctrl Pts',(11.704689803,-23.37673734,8.16362951651));
#89765=CARTESIAN_POINT('Ctrl Pts',(11.7004667677,-23.4732616915,8.15972481694));
#89766=CARTESIAN_POINT('Ctrl Pts',(11.9171250584,-23.1727778426,7.92710974195));
#89767=CARTESIAN_POINT('Ctrl Pts',(11.8511250917,-23.166992891,7.99912450114));
#89768=CARTESIAN_POINT('Ctrl Pts',(11.7809316294,-23.2008856654,8.07045852272));
#89769=CARTESIAN_POINT('Ctrl Pts',(11.721423774,-23.276320039,8.12480753543));
#89770=CARTESIAN_POINT('Ctrl Pts',(11.6879347422,-23.3738200593,8.14813746342));
#89771=CARTESIAN_POINT('Ctrl Pts',(11.6815098074,-23.471320079,8.14219684908));
#89772=CARTESIAN_POINT('Ctrl Pts',(11.9088198181,-23.171323915,7.91131175397));
#89773=CARTESIAN_POINT('Ctrl Pts',(11.8424378979,-23.1635210449,7.98439851249));
#89774=CARTESIAN_POINT('Ctrl Pts',(11.7703001202,-23.1961765665,8.0565580465));
#89775=CARTESIAN_POINT('Ctrl Pts',(11.7077347865,-23.2716977713,8.11081129139));
#89776=CARTESIAN_POINT('Ctrl Pts',(11.6713131361,-23.3700549965,8.13276881012));
#89777=CARTESIAN_POINT('Ctrl Pts',(11.6626231066,-23.4684122213,8.12473384452));
#89778=CARTESIAN_POINT('Ctrl Pts',(11.9005548343,-23.1693861722,7.89557218484));
#89779=CARTESIAN_POINT('Ctrl Pts',(11.8339499495,-23.1595472906,7.96980237485));
#89780=CARTESIAN_POINT('Ctrl Pts',(11.7599452801,-23.1908783692,8.04284981853));
#89781=CARTESIAN_POINT('Ctrl Pts',(11.6942870876,-23.2663663719,8.09701806797));
#89782=CARTESIAN_POINT('Ctrl Pts',(11.6548578924,-23.3654515527,8.11755397832));
#89783=CARTESIAN_POINT('Ctrl Pts',(11.6438378503,-23.4645367334,8.10736463748));
#89784=CARTESIAN_POINT('Origin',(11.9551818975745,-22.3491879643317,7.96775954099132));
#89785=CARTESIAN_POINT('Origin',(-2.84607155346,-22.8742356128,5.53854202767));
#89786=CARTESIAN_POINT('',(11.7512376696,-22.8742356128,3.91309124051));
#89787=CARTESIAN_POINT('Origin',(-2.84607155346,-22.8742356128,5.53854202767));
#89788=CARTESIAN_POINT('',(12.0493948734,-23.1742356128,3.87989061057));
#89789=CARTESIAN_POINT('Origin',(12.0493948734,-22.8742356128,3.87989061057));
#89790=CARTESIAN_POINT('Origin',(-2.84607155346,-23.1742356128,5.53854202767));
#89791=CARTESIAN_POINT('Origin',(11.4530804658,-22.8742356128,3.94629187045));
#89792=CARTESIAN_POINT('',(11.4530804658,-22.8742356128,3.64629187045));
#89793=CARTESIAN_POINT('Origin',(11.4530804658,-22.8742356128,3.94629187045));
#89794=CARTESIAN_POINT('',(11.4530804658,-23.1742356128,3.34629187045));
#89795=CARTESIAN_POINT('Origin',(11.4530804658,-22.8742356128,3.34629187045));
#89796=CARTESIAN_POINT('Origin',(11.4530804658,-23.1742356128,3.94629187045));
#89797=CARTESIAN_POINT('Origin',(-6.6707290414,-22.8742356128,3.34629187045));
#89798=CARTESIAN_POINT('',(8.10176909975,-22.8742356128,3.64629187045));
#89799=CARTESIAN_POINT('',(9.77742478279,-22.8742356128,3.64629187045));
#89800=CARTESIAN_POINT('',(8.10176909975,-23.1742356128,3.34629187045));
#89801=CARTESIAN_POINT('Origin',(8.10176909975,-22.8742356128,3.34629187045));
#89802=CARTESIAN_POINT('',(9.77742478279,-23.1742356128,3.34629187045));
#89803=CARTESIAN_POINT('Origin',(8.10176909975,-22.8742356128,3.94629187045));
#89804=CARTESIAN_POINT('',(7.80346303227,-22.8742356128,3.91445651114));
#89805=CARTESIAN_POINT('Origin',(8.10176909975,-22.8742356128,3.94629187045));
#89806=CARTESIAN_POINT('',(7.50515696478,-23.1742356128,3.88262115182));
#89807=CARTESIAN_POINT('Origin',(7.50515696478,-22.8742356128,3.88262115182));
#89808=CARTESIAN_POINT('Origin',(8.10176909975,-23.1742356128,3.94629187045));
#89809=CARTESIAN_POINT('Origin',(0.00234331738835,-22.8742356128,3.08191746407));
#89810=CARTESIAN_POINT('',(6.23264645859,-22.8742356128,7.84992678029));
#89811=CARTESIAN_POINT('Origin',(0.00234331738835,-22.8742356128,3.08191746407));
#89812=CARTESIAN_POINT('',(5.99440665492,-23.1742356128,7.66760345225));
#89813=CARTESIAN_POINT('Origin',(5.99440665492,-22.8742356128,7.66760345225));
#89814=CARTESIAN_POINT('Origin',(0.00234331738835,-23.1742356128,3.08191746407));
#89815=CARTESIAN_POINT('Origin',(6.47088626226,-22.8742356128,8.03225010833));
#89816=CARTESIAN_POINT('',(6.26721888507,-22.8742356128,8.25252175759));
#89817=CARTESIAN_POINT('Origin',(6.47088626226,-22.8742356128,8.03225010833));
#89818=CARTESIAN_POINT('',(6.06355150788,-23.1742356128,8.47279340685));
#89819=CARTESIAN_POINT('Origin',(6.06355150788,-22.8742356128,8.47279340685));
#89820=CARTESIAN_POINT('Origin',(6.47088626226,-23.1742356128,8.03225010833));
#89821=CARTESIAN_POINT('Ctrl Pts',(8.73611662316,-23.4697910609,10.8942571942));
#89822=CARTESIAN_POINT('Ctrl Pts',(8.72752432309,-23.3771104598,10.9015348722));
#89823=CARTESIAN_POINT('Ctrl Pts',(8.69545860941,-23.2844298587,10.881098933));
#89824=CARTESIAN_POINT('Ctrl Pts',(8.6413960311,-23.2107990757,10.8311116668));
#89825=CARTESIAN_POINT('Ctrl Pts',(8.57793853593,-23.1733813929,10.7632250691));
#89826=CARTESIAN_POINT('Ctrl Pts',(8.51747666777,-23.1720133445,10.6920986219));
#89827=CARTESIAN_POINT('Ctrl Pts',(8.72470175689,-23.4715681133,10.9039255852));
#89828=CARTESIAN_POINT('Ctrl Pts',(8.7177987489,-23.3784476295,10.9097561006));
#89829=CARTESIAN_POINT('Ctrl Pts',(8.68736831632,-23.2853271458,10.8877470417));
#89830=CARTESIAN_POINT('Ctrl Pts',(8.63454393537,-23.211417996,10.8363489167));
#89831=CARTESIAN_POINT('Ctrl Pts',(8.57168882428,-23.1740163051,10.7675887259));
#89832=CARTESIAN_POINT('Ctrl Pts',(8.51124350946,-23.1729018671,10.696222277));
#89833=CARTESIAN_POINT('Ctrl Pts',(8.71323427675,-23.4729019084,10.9136114204));
#89834=CARTESIAN_POINT('Ctrl Pts',(8.70803661002,-23.3794040149,10.9179891886));
#89835=CARTESIAN_POINT('Ctrl Pts',(8.67925545718,-23.2859061213,10.8943982297));
#89836=CARTESIAN_POINT('Ctrl Pts',(8.62767478659,-23.2117711836,10.8415808992));
#89837=CARTESIAN_POINT('Ctrl Pts',(8.5654164258,-23.1744185718,10.771945772));
#89838=CARTESIAN_POINT('Ctrl Pts',(8.50497501432,-23.1735687617,10.7003455662));
#89839=CARTESIAN_POINT('Ctrl Pts',(8.70172748022,-23.4737911951,10.9233030613));
#89840=CARTESIAN_POINT('Ctrl Pts',(8.69824977302,-23.3799791247,10.9262239001));
#89841=CARTESIAN_POINT('Ctrl Pts',(8.67113050266,-23.2861670544,10.9010437414));
#89842=CARTESIAN_POINT('Ctrl Pts',(8.62079773014,-23.2118592846,10.8468003207));
#89843=CARTESIAN_POINT('Ctrl Pts',(8.55912932234,-23.1745884938,10.7762902146));
#89844=CARTESIAN_POINT('Ctrl Pts',(8.49867834935,-23.1740134037,10.7044634205));
#89845=CARTESIAN_POINT('Ctrl Pts',(8.69019480669,-23.4742356128,10.9329890024));
#89846=CARTESIAN_POINT('Ctrl Pts',(8.68845018412,-23.3801733377,10.9344501196));
#89847=CARTESIAN_POINT('Ctrl Pts',(8.66300395829,-23.2861110626,10.9076749542));
#89848=CARTESIAN_POINT('Ctrl Pts',(8.61392194556,-23.2116837148,10.8520000359));
#89849=CARTESIAN_POINT('Ctrl Pts',(8.55283556198,-23.1745270026,10.7806162216));
#89850=CARTESIAN_POINT('Ctrl Pts',(8.49236081888,-23.1742356128,10.7085709021));
#89851=CARTESIAN_POINT('Ctrl Pts',(8.67864985337,-23.4742356128,10.942657873));
#89852=CARTESIAN_POINT('Ctrl Pts',(8.67864985337,-23.3799878332,10.942657873));
#89853=CARTESIAN_POINT('Ctrl Pts',(8.65488631632,-23.2857400536,10.9142834188));
#89854=CARTESIAN_POINT('Ctrl Pts',(8.60705657762,-23.2112466293,10.8571731189));
#89855=CARTESIAN_POINT('Ctrl Pts',(8.54654322741,-23.1742356128,10.7849181647));
#89856=CARTESIAN_POINT('Ctrl Pts',(8.48602987721,-23.1742356128,10.7126632105));
#89857=CARTESIAN_POINT('',(8.51747674095254,-23.1720132750395,10.6920985878956));
#89858=CARTESIAN_POINT('Origin',(8.54339070302529,-23.4677320541598,10.6671045573098));
#89859=CARTESIAN_POINT('Origin',(8.46564327939413,-22.8727019153709,10.6937226627841));
#89860=CARTESIAN_POINT('Ctrl Pts',(8.73611663424,-23.4697908757,10.8942572059));
#89861=CARTESIAN_POINT('Ctrl Pts',(8.72752435034,-23.3771103023,10.9015348641));
#89862=CARTESIAN_POINT('Ctrl Pts',(8.69545865342,-23.2844297289,10.881098906));
#89863=CARTESIAN_POINT('Ctrl Pts',(8.64139608915,-23.2107989673,10.8311116257));
#89864=CARTESIAN_POINT('Ctrl Pts',(8.57793860163,-23.1733812942,10.7632250217));
#89865=CARTESIAN_POINT('Ctrl Pts',(8.51747673428,-23.1720132443,10.6920985753));
#89866=CARTESIAN_POINT('Ctrl Pts',(8.85271909481,-23.4283765706,10.7986501186));
#89867=CARTESIAN_POINT('Ctrl Pts',(8.80174479507,-23.3522217493,10.8290472717));
#89868=CARTESIAN_POINT('Ctrl Pts',(8.74702097884,-23.2760669279,10.8249995844));
#89869=CARTESIAN_POINT('Ctrl Pts',(8.69926483364,-23.2110252232,10.7808433397));
#89870=CARTESIAN_POINT('Ctrl Pts',(8.66655321101,-23.1680969408,10.704046549));
#89871=CARTESIAN_POINT('Ctrl Pts',(8.64928312709,-23.1513060056,10.6105493344));
#89872=CARTESIAN_POINT('Ctrl Pts',(8.95374236957,-23.2551805764,10.8169485727));
#89873=CARTESIAN_POINT('Ctrl Pts',(8.90906105284,-23.2232432649,10.7961844516));
#89874=CARTESIAN_POINT('Ctrl Pts',(8.87369407635,-23.1913059533,10.770178964));
#89875=CARTESIAN_POINT('Ctrl Pts',(8.84720879161,-23.1552341963,10.7456901634));
#89876=CARTESIAN_POINT('Ctrl Pts',(8.82709666423,-23.1116114836,10.7203986113));
#89877=CARTESIAN_POINT('Ctrl Pts',(8.81389010608,-23.0647081339,10.6876384968));
#89878=CARTESIAN_POINT('Ctrl Pts',(9.01791018836,-23.1549008445,10.8214049608));
#89879=CARTESIAN_POINT('Ctrl Pts',(8.99622746462,-23.1216722312,10.8155316644));
#89880=CARTESIAN_POINT('Ctrl Pts',(8.97425273896,-23.0884436179,10.8039507789));
#89881=CARTESIAN_POINT('Ctrl Pts',(8.95224692858,-23.0584727018,10.783603786));
#89882=CARTESIAN_POINT('Ctrl Pts',(8.93220449355,-23.0344758471,10.7563348016));
#89883=CARTESIAN_POINT('Ctrl Pts',(8.91487253124,-23.0145682268,10.7261343735));
#89884=CARTESIAN_POINT('Ctrl Pts',(9.08532173979,-23.0061361581,10.858062108));
#89885=CARTESIAN_POINT('Ctrl Pts',(9.07401122054583,-22.994360504385,10.847601774363));
#89886=CARTESIAN_POINT('Ctrl Pts',(9.06350105813443,-22.9825848532249,10.8378821902984));
#89887=CARTESIAN_POINT('Ctrl Pts',(9.05419277619886,-22.9699073952249,10.8292755748936));
#89888=CARTESIAN_POINT('Ctrl Pts',(9.04554579428692,-22.955591884285,10.8212820971294));
#89889=CARTESIAN_POINT('Ctrl Pts',(9.03689844897,-22.9401858313,10.8132890077));
#89890=CARTESIAN_POINT('Ctrl Pts',(9.1336794452,-22.8742356128,10.9029059811));
#89891=CARTESIAN_POINT('Ctrl Pts',(9.1336794452,-22.8742356128,10.9029059811));
#89892=CARTESIAN_POINT('Ctrl Pts',(9.1336794452,-22.8742356128,10.9029059811));
#89893=CARTESIAN_POINT('Ctrl Pts',(9.1336794452,-22.8742356128,10.9029059811));
#89894=CARTESIAN_POINT('Ctrl Pts',(9.1336794452,-22.8742356128,10.9029059811));
#89895=CARTESIAN_POINT('Ctrl Pts',(9.1336794452,-22.8742356128,10.9029059811));
#89896=CARTESIAN_POINT('Ctrl Pts',(9.1336794452,-22.8742356128,10.9029059811));
#89897=CARTESIAN_POINT('Ctrl Pts',(9.12513493716062,-22.8800589421312,10.894993962939));
#89898=CARTESIAN_POINT('Ctrl Pts',(9.1165963718414,-22.8858083341009,10.8873291251196));
#89899=CARTESIAN_POINT('Ctrl Pts',(9.10813461288467,-22.891442518539,10.8799452426598));
#89900=CARTESIAN_POINT('Ctrl Pts',(9.0987334575265,-22.897702191438,10.8717416260707));
#89901=CARTESIAN_POINT('Ctrl Pts',(9.08942655406422,-22.9038201324466,10.8638840973876));
#89902=CARTESIAN_POINT('Ctrl Pts',(9.08026451623907,-22.9097707148096,10.8563787344658));
#89903=CARTESIAN_POINT('Ctrl Pts',(9.06975354042648,-22.9165974086611,10.8477683478202));
#89904=CARTESIAN_POINT('Ctrl Pts',(9.05943264238283,-22.9232043535186,10.8396206480343));
#89905=CARTESIAN_POINT('Ctrl Pts',(9.04932970007876,-22.9295830542483,10.8319075912454));
#89906=CARTESIAN_POINT('Ctrl Pts',(9.03694696588163,-22.9374011485502,10.8224540351238));
#89907=CARTESIAN_POINT('Ctrl Pts',(9.02489106059946,-22.9448769807609,10.813652296514));
#89908=CARTESIAN_POINT('Ctrl Pts',(9.01315523782939,-22.9520273019305,10.8054156098417));
#89909=CARTESIAN_POINT('Ctrl Pts',(9.00003909933142,-22.9600186123484,10.7962101604006));
#89910=CARTESIAN_POINT('Ctrl Pts',(8.98732119582686,-22.9676044421161,10.7877087692407));
#89911=CARTESIAN_POINT('Ctrl Pts',(8.97494743412375,-22.9748283264758,10.7797773122612));
#89912=CARTESIAN_POINT('Ctrl Pts',(8.95691518561776,-22.9853556730562,10.7682188220704));
#89913=CARTESIAN_POINT('Ctrl Pts',(8.93983387064254,-22.9950142631594,10.7580274751551));
#89914=CARTESIAN_POINT('Ctrl Pts',(8.92385304365272,-23.0038402727672,10.7490310140701));
#89915=CARTESIAN_POINT('Ctrl Pts',(8.91881256768606,-23.0066240642028,10.7461934609252));
#89916=CARTESIAN_POINT('Ctrl Pts',(8.91388163935561,-23.0093251472349,10.7434751434281));
#89917=CARTESIAN_POINT('Ctrl Pts',(8.90906530481319,-23.0119447843037,10.7408717490746));
#89918=CARTESIAN_POINT('Ctrl Pts',(8.89902204419398,-23.0174073819654,10.7354430215317));
#89919=CARTESIAN_POINT('Ctrl Pts',(8.88947488845928,-23.0225171138711,10.7305122434003));
#89920=CARTESIAN_POINT('Ctrl Pts',(8.88045886577374,-23.0272916226541,10.7260415210383));
#89921=CARTESIAN_POINT('Ctrl Pts',(8.87595085443097,-23.0296788770456,10.7238061598573));
#89922=CARTESIAN_POINT('Ctrl Pts',(8.87157553457791,-23.0319822448368,10.7216857056986));
#89923=CARTESIAN_POINT('Ctrl Pts',(8.86734037703127,-23.0342103559124,10.7196849617963));
#89924=CARTESIAN_POINT('Ctrl Pts',(8.86522279825795,-23.0353244114502,10.7186845898452));
#89925=CARTESIAN_POINT('Ctrl Pts',(8.86313980497631,-23.0364188696591,10.7177131043847));
#89926=CARTESIAN_POINT('Ctrl Pts',(8.86109074211417,-23.0374921538938,10.7167673462285));
#89927=CARTESIAN_POINT('Ctrl Pts',(8.8600662106831,-23.0380287960111,10.7162944671504));
#89928=CARTESIAN_POINT('Ctrl Pts',(8.85905016031001,-23.038560143269,10.7158280141272));
#89929=CARTESIAN_POINT('Ctrl Pts',(8.85804263220622,-23.0390862143151,10.7153678876521));
#89930=CARTESIAN_POINT('Ctrl Pts',(8.85753886815433,-23.0393492498382,10.7151378244146));
#89931=CARTESIAN_POINT('Ctrl Pts',(8.85737477662451,-23.0394348372563,10.7150631549235));
#89932=CARTESIAN_POINT('Ctrl Pts',(8.8570442017229,-23.039607264533,10.7149127131171));
#89933=CARTESIAN_POINT('Ctrl Pts',(8.8567136268213,-23.0397796918097,10.7147622713108));
#89934=CARTESIAN_POINT('Ctrl Pts',(8.85621672904443,-23.0400390597548,10.7145355866259));
#89935=CARTESIAN_POINT('Ctrl Pts',(8.85504565480858,-23.0406486176515,10.7140063890137));
#89936=CARTESIAN_POINT('Ctrl Pts',(8.8375081072783,-23.0497771171593,10.706081333545));
#89937=CARTESIAN_POINT('Ctrl Pts',(8.82035364600279,-23.0584559152379,10.6990667696001));
#89938=CARTESIAN_POINT('Ctrl Pts',(8.80361240503948,-23.0666866946299,10.6929251497074));
#89939=CARTESIAN_POINT('Ctrl Pts',(8.7814795534295,-23.0775682427372,10.6848055866458));
#89940=CARTESIAN_POINT('Ctrl Pts',(8.76006900585031,-23.0876660498215,10.6782137157404));
#89941=CARTESIAN_POINT('Ctrl Pts',(8.73951183134782,-23.0969407417162,10.6731237801854));
#89942=CARTESIAN_POINT('Ctrl Pts',(8.71985880705542,-23.1058075120541,10.6682577113053));
#89943=CARTESIAN_POINT('Ctrl Pts',(8.70098941074461,-23.113919168474,10.6647686786032));
#89944=CARTESIAN_POINT('Ctrl Pts',(8.68302914806466,-23.1212408406627,10.6626236735639));
#89945=CARTESIAN_POINT('Ctrl Pts',(8.66738338370802,-23.1276189855596,10.6607550904597));
#89946=CARTESIAN_POINT('Ctrl Pts',(8.6524284691694,-23.1333971706594,10.6599068060774));
#89947=CARTESIAN_POINT('Ctrl Pts',(8.63822807834273,-23.1385709426346,10.6600230757282));
#89948=CARTESIAN_POINT('Ctrl Pts',(8.62419824174967,-23.1436825748613,10.6601379489188));
#89949=CARTESIAN_POINT('Ctrl Pts',(8.6109053274306,-23.1482040959269,10.6611942792068));
#89950=CARTESIAN_POINT('Ctrl Pts',(8.59838126145788,-23.1521547389558,10.6631008777657));
#89951=CARTESIAN_POINT('Ctrl Pts',(8.58543739956392,-23.1562378041415,10.6650713838686));
#89952=CARTESIAN_POINT('Ctrl Pts',(8.57331497071912,-23.1597111696374,10.6679496544977));
#89953=CARTESIAN_POINT('Ctrl Pts',(8.56201267336647,-23.162621878775,10.6715985087102));
#89954=CARTESIAN_POINT('Ctrl Pts',(8.54945169004857,-23.1658567404831,10.6756537193866));
#89955=CARTESIAN_POINT('Ctrl Pts',(8.53790390195525,-23.1683968954813,10.6806597285344));
#89956=CARTESIAN_POINT('Ctrl Pts',(8.52731880357864,-23.1703362662535,10.6863944651257));
#89957=CARTESIAN_POINT('Ctrl Pts',(8.52394129456544,-23.1709550835786,10.6882243134499));
#89958=CARTESIAN_POINT('Ctrl Pts',(8.52066145345847,-23.1715129157972,10.6901281926098));
#89959=CARTESIAN_POINT('Ctrl Pts',(8.51747674491568,-23.1720132445407,10.6920985878117));
#89960=CARTESIAN_POINT('Origin',(6.6707290414,-22.8742356128,9.03420135995));
#89961=CARTESIAN_POINT('',(7.27479069254,-23.1742356128,9.59272830866));
#89962=CARTESIAN_POINT('',(7.70044916513,-22.8742356128,9.57771386935));
#89963=CARTESIAN_POINT('Origin',(7.16045579301E-17,-22.6642356128,0.580061096523));
#89964=CARTESIAN_POINT('',(10.0062431967,-21.0742356128,11.3317411468));
#89965=CARTESIAN_POINT('',(10.0062431967,-23.2742356128,11.3317411468));
#89966=CARTESIAN_POINT('',(10.9304145503,-21.0742356128,10.3907473403));
#89967=CARTESIAN_POINT('Origin',(-1.51003344041E-15,-21.0742356128,0.580061096523));
#89968=CARTESIAN_POINT('',(10.9304145503,-21.9742356128,10.3907473403));
#89969=CARTESIAN_POINT('Origin',(10.1862176145,-21.9742356128,9.72278707155));
#89970=CARTESIAN_POINT('',(11.1383462684,-21.0742356128,10.0284846777));
#89971=CARTESIAN_POINT('Origin',(10.1862176145,-21.0742356128,9.72278707155));
#89972=CARTESIAN_POINT('',(11.1383462684,-22.6642356128,10.0284846777));
#89973=CARTESIAN_POINT('Origin',(-2.84607155346,-22.6642356128,5.53854202767));
#89974=CARTESIAN_POINT('Origin',(-2.84607155346,-21.0742356128,5.53854202767));
#89975=CARTESIAN_POINT('Origin',(11.3733704264,-23.1237854196,7.73136642019));
#89976=CARTESIAN_POINT('',(11.669865565,-21.0742356128,7.77708985809));
#89977=CARTESIAN_POINT('Origin',(11.3733704264,-21.0742356128,7.73136642019));
#89978=CARTESIAN_POINT('',(11.669865565,-22.5742356128,7.77708985809));
#89979=CARTESIAN_POINT('Origin',(-2.84607155346,-21.2742356128,5.53854202767));
#89980=CARTESIAN_POINT('',(11.7512376696,-21.0742356128,3.91309124051));
#89981=CARTESIAN_POINT('Origin',(-2.84607155346,-21.0742356128,5.53854202767));
#89982=CARTESIAN_POINT('',(11.7512376696,-22.1242356128,3.91309124051));
#89983=CARTESIAN_POINT('Origin',(11.4530804658,-22.1242356128,3.94629187045));
#89984=CARTESIAN_POINT('',(11.4530804658,-21.0742356128,3.64629187045));
#89985=CARTESIAN_POINT('Origin',(11.4530804658,-21.0742356128,3.94629187045));
#89986=CARTESIAN_POINT('',(11.4530804658,-21.9742356128,3.64629187045));
#89987=CARTESIAN_POINT('Origin',(-11.7190551593,-23.1742356128,3.64629187045));
#89988=CARTESIAN_POINT('',(8.10176909975,-21.0742356128,3.64629187045));
#89989=CARTESIAN_POINT('',(-8.95225019493,-21.0742356128,3.64629187045));
#89990=CARTESIAN_POINT('',(8.10176909975,-22.1242356128,3.64629187045));
#89991=CARTESIAN_POINT('Origin',(8.10176909975,-22.1242356128,3.94629187045));
#89992=CARTESIAN_POINT('',(7.80346303227,-21.0742356128,3.91445651114));
#89993=CARTESIAN_POINT('Origin',(8.10176909975,-21.0742356128,3.94629187045));
#89994=CARTESIAN_POINT('',(7.80346303227,-21.2742356128,3.91445651114));
#89995=CARTESIAN_POINT('Origin',(0.00234331738835,-21.2742356128,3.08191746407));
#89996=CARTESIAN_POINT('',(6.23264645859,-21.0742356128,7.84992678029));
#89997=CARTESIAN_POINT('Origin',(0.00234331738835,-21.0742356128,3.08191746407));
#89998=CARTESIAN_POINT('',(6.23264645859,-22.1242356128,7.84992678029));
#89999=CARTESIAN_POINT('Origin',(6.47088626226,-22.1242356128,8.03225010833));
#90000=CARTESIAN_POINT('',(6.26721888507,-21.0742356128,8.25252175759));
#90001=CARTESIAN_POINT('Origin',(6.47088626226,-21.0742356128,8.03225010833));
#90002=CARTESIAN_POINT('',(6.26721888507,-21.9742356128,8.25252175759));
#90003=CARTESIAN_POINT('Origin',(9.80058174751,-23.1742356128,11.519536597));
#90004=CARTESIAN_POINT('',(9.59819339216,-21.0742356128,11.3324044552));
#90005=CARTESIAN_POINT('',(8.22276378328,-21.0742356128,10.0606559488));
#90006=CARTESIAN_POINT('',(9.59819339216,-23.2742356128,11.3324044552));
#90007=CARTESIAN_POINT('Origin',(9.80186076935,-23.2742356128,11.1121328059));
#90008=CARTESIAN_POINT('Origin',(9.80186076935,-21.0742356128,11.1121328059));
#90009=CARTESIAN_POINT('Origin',(9.80186076935,-21.0742356128,11.1121328059));
#90010=CARTESIAN_POINT('',(9.80186076935,-20.7742356128,11.1121328059));
#90011=CARTESIAN_POINT('Origin',(9.80186076935,-21.0742356128,11.1121328059));
#90012=CARTESIAN_POINT('Origin',(9.80186076935,-21.0742356128,11.1121328059));
#90013=CARTESIAN_POINT('Origin',(-1.51003344041E-15,-21.0742356128,0.580061096523));
#90014=CARTESIAN_POINT('',(10.7071554695,-20.7742356128,10.1903592597));
#90015=CARTESIAN_POINT('Origin',(1.14862552646E-15,-20.7742356128,0.580061096523));
#90016=CARTESIAN_POINT('Origin',(10.7071554695,-21.0742356128,10.1903592597));
#90017=CARTESIAN_POINT('Origin',(10.1862176145,-21.0742356128,9.72278707155));
#90018=CARTESIAN_POINT('',(10.8527076722,-20.7742356128,9.93677539585));
#90019=CARTESIAN_POINT('Origin',(10.1862176145,-20.7742356128,9.72278707155));
#90020=CARTESIAN_POINT('Origin',(10.8527076722,-21.0742356128,9.93677539585));
#90021=CARTESIAN_POINT('Origin',(10.8795671881,-21.0742356128,9.85222376962));
#90022=CARTESIAN_POINT('',(10.8795671881,-20.7742356128,9.85222376962));
#90023=CARTESIAN_POINT('Origin',(10.8795671881,-21.0742356128,9.85222376962));
#90024=CARTESIAN_POINT('Origin',(10.8795671881,-21.0742356128,9.85222376962));
#90025=CARTESIAN_POINT('Origin',(-2.84607155346,-21.0742356128,5.53854202767));
#90026=CARTESIAN_POINT('Origin',(-2.84607155346,-20.7742356128,5.53854202767));
#90027=CARTESIAN_POINT('Origin',(11.3733704264,-21.0742356128,7.73136642019));
#90028=CARTESIAN_POINT('',(11.3733704264,-20.7742356128,7.73136642019));
#90029=CARTESIAN_POINT('Origin',(11.3733704264,-21.0742356128,7.73136642019));
#90030=CARTESIAN_POINT('Origin',(11.3733704264,-21.0742356128,7.73136642019));
#90031=CARTESIAN_POINT('Origin',(-2.84607155346,-21.0742356128,5.53854202767));
#90032=CARTESIAN_POINT('',(11.4530804658,-20.7742356128,3.94629187045));
#90033=CARTESIAN_POINT('Origin',(-2.84607155346,-20.7742356128,5.53854202767));
#90034=CARTESIAN_POINT('Ctrl Pts',(11.7512376696703,-21.0742356128,3.91309124050216));
#90035=CARTESIAN_POINT('Ctrl Pts',(11.7512376696703,-21.061953784972,3.91309124050216));
#90036=CARTESIAN_POINT('Ctrl Pts',(11.7504944812795,-21.0498158353317,3.91319258196987));
#90037=CARTESIAN_POINT('Ctrl Pts',(11.7490326898121,-21.0377819506246,3.91337662775074));
#90038=CARTESIAN_POINT('Ctrl Pts',(11.7475741872629,-21.0257751412316,3.91356025944277));
#90039=CARTESIAN_POINT('Ctrl Pts',(11.7454001436074,-21.0138707693975,3.91382623933377));
#90040=CARTESIAN_POINT('Ctrl Pts',(11.7424843663441,-21.0020342015883,3.91416170558472));
#90041=CARTESIAN_POINT('Ctrl Pts',(11.7408977618661,-20.9955933970294,3.91434424773657));
#90042=CARTESIAN_POINT('Ctrl Pts',(11.7390906675882,-20.989172855015,3.91454746142827));
#90043=CARTESIAN_POINT('Ctrl Pts',(11.7370528663661,-20.9827694783049,3.91476994898516));
#90044=CARTESIAN_POINT('Ctrl Pts',(11.7331534939108,-20.9705164918538,3.91519568327249));
#90045=CARTESIAN_POINT('Ctrl Pts',(11.7284135628784,-20.9583285255006,3.9157030054636));
#90046=CARTESIAN_POINT('Ctrl Pts',(11.7227474029947,-20.9462470252009,3.91631409645459));
#90047=CARTESIAN_POINT('Ctrl Pts',(11.7214850798771,-20.9435554744087,3.91645023703317));
#90048=CARTESIAN_POINT('Ctrl Pts',(11.7201766628825,-20.9408693694333,3.91659154143874));
#90049=CARTESIAN_POINT('Ctrl Pts',(11.7188210035705,-20.9381894695388,3.91673827700573));
#90050=CARTESIAN_POINT('Ctrl Pts',(11.7151006159899,-20.930834917996,3.9171409690215));
#90051=CARTESIAN_POINT('Ctrl Pts',(11.711024953989,-20.9235274344412,3.91758468300204));
#90052=CARTESIAN_POINT('Ctrl Pts',(11.7065715477149,-20.9162925106405,3.91807400392752));
#90053=CARTESIAN_POINT('Ctrl Pts',(11.7046069350836,-20.9131008362658,3.91828986702461));
#90054=CARTESIAN_POINT('Ctrl Pts',(11.7024319865283,-20.9097091974042,3.91852987197131));
#90055=CARTESIAN_POINT('Ctrl Pts',(11.7002182775194,-20.9064091635286,3.91877487588534));
#90056=CARTESIAN_POINT('Ctrl Pts',(11.6979303480295,-20.9029984872422,3.91902809420708));
#90057=CARTESIAN_POINT('Ctrl Pts',(11.6956012072243,-20.8996859843533,3.91928663093016));
#90058=CARTESIAN_POINT('Ctrl Pts',(11.6934678401137,-20.8967605599251,3.91952405550537));
#90059=CARTESIAN_POINT('Ctrl Pts',(11.6929863050353,-20.8961002448419,3.91957764602941));
#90060=CARTESIAN_POINT('Ctrl Pts',(11.6925149133686,-20.8954595177209,3.91963014209845));
#90061=CARTESIAN_POINT('Ctrl Pts',(11.692056655695,-20.894841483953,3.91968121022605));
#90062=CARTESIAN_POINT('Ctrl Pts',(11.6868870171147,-20.8878693994812,3.92025731353614));
#90063=CARTESIAN_POINT('Ctrl Pts',(11.681028978478,-20.8806146987769,3.92079056445445));
#90064=CARTESIAN_POINT('Ctrl Pts',(11.6743536993568,-20.8731965252264,3.92136149180633));
#90065=CARTESIAN_POINT('Ctrl Pts',(11.6679298789804,-20.8660577953628,3.92191091224103));
#90066=CARTESIAN_POINT('Ctrl Pts',(11.6607485156396,-20.8587673526175,3.92249531322976));
#90067=CARTESIAN_POINT('Ctrl Pts',(11.6526950743861,-20.8514781481433,3.92318622219881));
#90068=CARTESIAN_POINT('Ctrl Pts',(11.6450908858519,-20.8445955642465,3.92383858954033));
#90069=CARTESIAN_POINT('Ctrl Pts',(11.6367084813275,-20.8377140858643,3.92458600237492));
#90070=CARTESIAN_POINT('Ctrl Pts',(11.6274618609907,-20.8310069727909,3.92548719456923));
#90071=CARTESIAN_POINT('Ctrl Pts',(11.6216163226962,-20.8267668629034,3.92605691121063));
#90072=CARTESIAN_POINT('Ctrl Pts',(11.6154256196503,-20.8225973359018,3.92668805493909));
#90073=CARTESIAN_POINT('Ctrl Pts',(11.6088725503865,-20.8185520694094,3.92739486347025));
#90074=CARTESIAN_POINT('Ctrl Pts',(11.5990462859797,-20.8124862311662,3.92845471607254));
#90075=CARTESIAN_POINT('Ctrl Pts',(11.5884024743053,-20.8066968351051,3.92972025328186));
#90076=CARTESIAN_POINT('Ctrl Pts',(11.5769335115456,-20.8014122888872,3.93113673006546));
#90077=CARTESIAN_POINT('Ctrl Pts',(11.5658173333816,-20.7962902949891,3.9325096361095));
#90078=CARTESIAN_POINT('Ctrl Pts',(11.5539255155658,-20.7916431888797,3.93402438121635));
#90079=CARTESIAN_POINT('Ctrl Pts',(11.5412952243341,-20.7876957303457,3.93562656642631));
#90080=CARTESIAN_POINT('Ctrl Pts',(11.5289826087367,-20.7838475578353,3.93718845365792));
#90081=CARTESIAN_POINT('Ctrl Pts',(11.515967870747,-20.7806649881655,3.93883346656174));
#90082=CARTESIAN_POINT('Ctrl Pts',(11.5023338717146,-20.7783628051133,3.94050629235595));
#90083=CARTESIAN_POINT('Ctrl Pts',(11.4891284616509,-20.7761329918961,3.9421265323549));
#90084=CARTESIAN_POINT('Ctrl Pts',(11.4753420359553,-20.7747298298989,3.94377286916209));
#90085=CARTESIAN_POINT('Ctrl Pts',(11.4610987246952,-20.7743441416219,3.94539013989711));
#90086=CARTESIAN_POINT('Ctrl Pts',(11.4584413983245,-20.7742721850655,3.94569186862397));
#90087=CARTESIAN_POINT('Ctrl Pts',(11.4557683109257,-20.7742356127993,3.94599257145532));
#90088=CARTESIAN_POINT('Ctrl Pts',(11.4530804658,-20.7742356128,3.94629187045));
#90089=CARTESIAN_POINT('Origin',(11.4530804658,-21.0742356128,3.94629187045));
#90090=CARTESIAN_POINT('Origin',(11.4530804658,-21.0742356128,3.94629187045));
#90091=CARTESIAN_POINT('Origin',(-8.95225019493,-21.0742356128,3.94629187045));
#90092=CARTESIAN_POINT('',(8.10176909975,-20.7742356128,3.94629187045));
#90093=CARTESIAN_POINT('',(9.77742478279,-20.7742356128,3.94629187045));
#90094=CARTESIAN_POINT('Ctrl Pts',(8.10176909975,-21.0742356128,3.64629187045));
#90095=CARTESIAN_POINT('Ctrl Pts',(8.10176909975,-21.0619847846212,3.64629187045));
#90096=CARTESIAN_POINT('Ctrl Pts',(8.10178777058952,-21.0498787025718,3.64703790633803));
#90097=CARTESIAN_POINT('Ctrl Pts',(8.10180917103989,-21.0378767553172,3.64850329867038));
#90098=CARTESIAN_POINT('Ctrl Pts',(8.1018305261806,-21.0259002189328,3.64996558843165));
#90099=CARTESIAN_POINT('Ctrl Pts',(8.10185459938597,-21.0140262212391,3.65214435902398));
#90100=CARTESIAN_POINT('Ctrl Pts',(8.1018655504668,-21.0022192441784,3.65506405129366));
#90101=CARTESIAN_POINT('Ctrl Pts',(8.10187153783563,-20.9957639245915,3.65666035715581));
#90102=CARTESIAN_POINT('Ctrl Pts',(8.10187360271116,-20.9893288232958,3.6584790192082));
#90103=CARTESIAN_POINT('Ctrl Pts',(8.10186915629961,-20.9829106437654,3.66053016897335));
#90104=CARTESIAN_POINT('Ctrl Pts',(8.10186068552984,-20.9706834982078,3.66443777339922));
#90105=CARTESIAN_POINT('Ctrl Pts',(8.101840116808,-20.9585199787489,3.6691862056774));
#90106=CARTESIAN_POINT('Ctrl Pts',(8.10182011974497,-20.9464605656251,3.6748631738841));
#90107=CARTESIAN_POINT('Ctrl Pts',(8.10181564929347,-20.9437646186569,3.67613229080285));
#90108=CARTESIAN_POINT('Ctrl Pts',(8.10181120741178,-20.9410740368944,3.67744793841355));
#90109=CARTESIAN_POINT('Ctrl Pts',(8.1018069356528,-20.9383895761731,3.67881130230953));
#90110=CARTESIAN_POINT('Ctrl Pts',(8.1017952456339,-20.9310433291839,3.68254225945719));
#90111=CARTESIAN_POINT('Ctrl Pts',(8.10178500679284,-20.9237432623569,3.68663004481532));
#90112=CARTESIAN_POINT('Ctrl Pts',(8.10177833444282,-20.9165146982158,3.69109760503107));
#90113=CARTESIAN_POINT('Ctrl Pts',(8.10177538111668,-20.9133151797057,3.69307504361027));
#90114=CARTESIAN_POINT('Ctrl Pts',(8.10177315721422,-20.9099165309174,3.69526371375841));
#90115=CARTESIAN_POINT('Ctrl Pts',(8.10177162915918,-20.9066099782108,3.69749145520004));
#90116=CARTESIAN_POINT('Ctrl Pts',(8.10177005043771,-20.9031937886207,3.69979306288564));
#90117=CARTESIAN_POINT('Ctrl Pts',(8.10176921447374,-20.8998762238456,3.70213617883799));
#90118=CARTESIAN_POINT('Ctrl Pts',(8.1017690842391,-20.8969455452457,3.70428312691668));
#90119=CARTESIAN_POINT('Ctrl Pts',(8.10176905573697,-20.8963041598008,3.70475299121658));
#90120=CARTESIAN_POINT('Ctrl Pts',(8.10176906103665,-20.8956811799168,3.70521329960476));
#90121=CARTESIAN_POINT('Ctrl Pts',(8.10176909975,-20.8950794308293,3.70566131864562));
#90122=CARTESIAN_POINT('Ctrl Pts',(8.10176954837301,-20.8881061653975,3.71085310996751));
#90123=CARTESIAN_POINT('Ctrl Pts',(8.10165103493539,-20.8808495135392,3.71672358548636));
#90124=CARTESIAN_POINT('Ctrl Pts',(8.10147915722924,-20.8734282573273,3.72340982543949));
#90125=CARTESIAN_POINT('Ctrl Pts',(8.10131375448263,-20.8662865739282,3.72984418203802));
#90126=CARTESIAN_POINT('Ctrl Pts',(8.10109893240106,-20.8589921286811,3.73703471542109));
#90127=CARTESIAN_POINT('Ctrl Pts',(8.10089315097308,-20.851697542693,3.74510338332156));
#90128=CARTESIAN_POINT('Ctrl Pts',(8.10069886081103,-20.8448103016647,3.75272147990688));
#90129=CARTESIAN_POINT('Ctrl Pts',(8.10051262979633,-20.8379229353717,3.76112310089669));
#90130=CARTESIAN_POINT('Ctrl Pts',(8.10038366104728,-20.8312084104219,3.77040048662393));
#90131=CARTESIAN_POINT('Ctrl Pts',(8.10030161028707,-20.8269365858078,3.77630281999828));
#90132=CARTESIAN_POINT('Ctrl Pts',(8.10024273692979,-20.822735620552,3.78255940771729));
#90133=CARTESIAN_POINT('Ctrl Pts',(8.10021971127824,-20.8186601819094,3.78918935893252));
#90134=CARTESIAN_POINT('Ctrl Pts',(8.10018536535161,-20.8125811045673,3.79907884316888));
#90135=CARTESIAN_POINT('Ctrl Pts',(8.10026502916778,-20.8067783917534,3.80980573572973));
#90136=CARTESIAN_POINT('Ctrl Pts',(8.10040384447576,-20.8014812562884,3.82137165189451));
#90137=CARTESIAN_POINT('Ctrl Pts',(8.10053823548761,-20.7963529501573,3.83256894129223));
#90138=CARTESIAN_POINT('Ctrl Pts',(8.10072806754702,-20.7916991304606,3.844553088688));
#90139=CARTESIAN_POINT('Ctrl Pts',(8.10092356229844,-20.7877445949121,3.85728121564088));
#90140=CARTESIAN_POINT('Ctrl Pts',(8.10111414163741,-20.7838894900292,3.86968931357396));
#90141=CARTESIAN_POINT('Ctrl Pts',(8.10131010248906,-20.7806996541778,3.88280478000332));
#90142=CARTESIAN_POINT('Ctrl Pts',(8.10146532767923,-20.7783899206235,3.89653921805234));
#90143=CARTESIAN_POINT('Ctrl Pts',(8.10161566583163,-20.7761529056471,3.90984124743561));
#90144=CARTESIAN_POINT('Ctrl Pts',(8.1017277929501,-20.7747421928388,3.9237239632078));
#90145=CARTESIAN_POINT('Ctrl Pts',(8.10175981195886,-20.7743486289048,3.93805798374527));
#90146=CARTESIAN_POINT('Ctrl Pts',(8.10176590746594,-20.7742737055441,3.94078677289168));
#90147=CARTESIAN_POINT('Ctrl Pts',(8.10176909975,-20.7742356128,3.94353176975334));
#90148=CARTESIAN_POINT('Ctrl Pts',(8.10176909975,-20.7742356128,3.94629187045));
#90149=CARTESIAN_POINT('Origin',(8.10176909975,-21.0742356128,3.94629187045));
#90150=CARTESIAN_POINT('Origin',(8.10176909975,-21.0742356128,3.94629187045));
#90151=CARTESIAN_POINT('Origin',(0.00234331738835,-21.0742356128,3.08191746407));
#90152=CARTESIAN_POINT('',(6.47088626226,-20.7742356128,8.03225010833));
#90153=CARTESIAN_POINT('Origin',(0.00234331738835,-20.7742356128,3.08191746407));
#90154=CARTESIAN_POINT('Ctrl Pts',(6.23264645858874,-21.0742356128,7.84992678028904));
#90155=CARTESIAN_POINT('Ctrl Pts',(6.23264645858874,-21.0620738653159,7.84992678028904));
#90156=CARTESIAN_POINT('Ctrl Pts',(6.23324197790072,-21.0500593540845,7.85035827840671));
#90157=CARTESIAN_POINT('Ctrl Pts',(6.23440148065616,-21.0381491830447,7.85121773708456));
#90158=CARTESIAN_POINT('Ctrl Pts',(6.23555896176804,-21.0262597779071,7.85207569725876));
#90159=CARTESIAN_POINT('Ctrl Pts',(6.23727859457928,-21.0144732053028,7.85336022155103));
#90160=CARTESIAN_POINT('Ctrl Pts',(6.23956950843529,-21.0027514162633,7.85509881860574));
#90161=CARTESIAN_POINT('Ctrl Pts',(6.24083883124489,-20.99625674421,7.85606212016877));
#90162=CARTESIAN_POINT('Ctrl Pts',(6.242284241646,-20.9897821389332,7.85716536211542));
#90163=CARTESIAN_POINT('Ctrl Pts',(6.24391239277648,-20.9833237084844,7.85841714394168));
#90164=CARTESIAN_POINT('Ctrl Pts',(6.24697603836402,-20.9711710639439,7.86077258613424));
#90165=CARTESIAN_POINT('Ctrl Pts',(6.25069157623758,-20.9590780258119,7.86364274042942));
#90166=CARTESIAN_POINT('Ctrl Pts',(6.25513679500523,-20.9470823057364,7.86707079100242));
#90167=CARTESIAN_POINT('Ctrl Pts',(6.25614018231608,-20.9443745979863,7.86784458024109));
#90168=CARTESIAN_POINT('Ctrl Pts',(6.25718085020712,-20.9416720126045,7.8686468730048));
#90169=CARTESIAN_POINT('Ctrl Pts',(6.25825986455158,-20.9389752940825,7.8694782961947));
#90170=CARTESIAN_POINT('Ctrl Pts',(6.26118950301342,-20.9316534170906,7.87173569839489));
#90171=CARTESIAN_POINT('Ctrl Pts',(6.26440152010394,-20.9243751453831,7.8742073792891));
#90172=CARTESIAN_POINT('Ctrl Pts',(6.26791574646482,-20.9171653086749,7.87690568653838));
#90173=CARTESIAN_POINT('Ctrl Pts',(6.26948675885108,-20.913942197353,7.87811194751171));
#90174=CARTESIAN_POINT('Ctrl Pts',(6.27122487389521,-20.9105224459337,7.87944512175967));
#90175=CARTESIAN_POINT('Ctrl Pts',(6.27299449129919,-20.9071962313223,7.88080146346944));
#90176=CARTESIAN_POINT('Ctrl Pts',(6.27482085484793,-20.9037633553189,7.88220129885351));
#90177=CARTESIAN_POINT('Ctrl Pts',(6.27668060789435,-20.9004304235927,7.88362568450306));
#90178=CARTESIAN_POINT('Ctrl Pts',(6.27838681422104,-20.8974837625284,7.88493158970018));
#90179=CARTESIAN_POINT('Ctrl Pts',(6.2787254732354,-20.8968988899277,7.88519079432273));
#90180=CARTESIAN_POINT('Ctrl Pts',(6.27905797805986,-20.8963291325229,7.88544525088481));
#90181=CARTESIAN_POINT('Ctrl Pts',(6.27938272573509,-20.8957765857997,7.88569373289182));
#90182=CARTESIAN_POINT('Ctrl Pts',(6.28348298362732,-20.8888001415159,7.888831061926));
#90183=CARTESIAN_POINT('Ctrl Pts',(6.28804763236961,-20.8815380508843,7.89247468318607));
#90184=CARTESIAN_POINT('Ctrl Pts',(6.29322559803938,-20.8741080370697,7.89665611919858));
#90185=CARTESIAN_POINT('Ctrl Pts',(6.29820836303392,-20.8669581223917,7.90067992204296));
#90186=CARTESIAN_POINT('Ctrl Pts',(6.30375962933618,-20.8596523763411,7.90520220172809));
#90187=CARTESIAN_POINT('Ctrl Pts',(6.31001241524958,-20.8523424382694,7.91025080344716));
#90188=CARTESIAN_POINT('Ctrl Pts',(6.31591479917088,-20.8454421442984,7.91501648486092));
#90189=CARTESIAN_POINT('Ctrl Pts',(6.32244284542141,-20.8385381115029,7.92025160452025));
#90190=CARTESIAN_POINT('Ctrl Pts',(6.32970078569121,-20.8318024119911,7.92597298656875));
#90191=CARTESIAN_POINT('Ctrl Pts',(6.33440503712393,-20.827436652161,7.92968131409671));
#90192=CARTESIAN_POINT('Ctrl Pts',(6.33941576294771,-20.8231425171236,7.933593787265));
#90193=CARTESIAN_POINT('Ctrl Pts',(6.34475758866928,-20.8189776690091,7.93771186558751));
#90194=CARTESIAN_POINT('Ctrl Pts',(6.35260440530219,-20.8128597607952,7.94376107182541));
#90195=CARTESIAN_POINT('Ctrl Pts',(6.36119100892562,-20.8070179672896,7.95023172960266));
#90196=CARTESIAN_POINT('Ctrl Pts',(6.37048584081494,-20.8016838718932,7.95716832362973));
#90197=CARTESIAN_POINT('Ctrl Pts',(6.37945335292896,-20.7965376179691,7.96386064380384));
#90198=CARTESIAN_POINT('Ctrl Pts',(6.38908045099127,-20.7918645698442,7.97098691526333));
#90199=CARTESIAN_POINT('Ctrl Pts',(6.39930314779427,-20.7878895669207,7.97856062207488));
#90200=CARTESIAN_POINT('Ctrl Pts',(6.4092689470059,-20.7840144562953,7.98594400072988));
#90201=CARTESIAN_POINT('Ctrl Pts',(6.41980105771033,-20.7808034552105,7.9937527988218));
#90202=CARTESIAN_POINT('Ctrl Pts',(6.43080104167877,-20.7784714692945,8.00197063081155));
#90203=CARTESIAN_POINT('Ctrl Pts',(6.44145351983779,-20.7762131542725,8.00992884929957));
#90204=CARTESIAN_POINT('Ctrl Pts',(6.45254484058177,-20.7747799372274,8.01827070709806));
#90205=CARTESIAN_POINT('Ctrl Pts',(6.46394607649882,-20.7743626945913,8.02695229170245));
#90206=CARTESIAN_POINT('Ctrl Pts',(6.46624740026132,-20.77427847474,8.02870465759433));
#90207=CARTESIAN_POINT('Ctrl Pts',(6.46856121725986,-20.7742356128,8.03047076694482));
#90208=CARTESIAN_POINT('Ctrl Pts',(6.47088626226,-20.7742356128,8.03225010833));
#90209=CARTESIAN_POINT('Origin',(6.47088626226,-21.0742356128,8.03225010833));
#90210=CARTESIAN_POINT('Origin',(6.47088626226,-21.0742356128,8.03225010833));
#90211=CARTESIAN_POINT('Origin',(8.42643116047,-21.0742356128,9.84038429957));
#90212=CARTESIAN_POINT('',(8.1363735158,-20.7742356128,9.57219145714));
#90213=CARTESIAN_POINT('Origin',(9.00617217252,-21.0742356128,8.1200469301));
#90214=CARTESIAN_POINT('',(10.5002881066,-20.7742356128,9.5015350813));
#90215=CARTESIAN_POINT('',(10.6899276473,-20.7742356128,9.67687942546));
#90216=CARTESIAN_POINT('Origin',(10.5002881066,-21.0742356128,9.5015350813));
#90217=CARTESIAN_POINT('Origin',(10.9076228609,-21.0742356128,9.06099178277));
#90218=CARTESIAN_POINT('',(10.4339531167,-20.7742356128,8.69270253038));
#90219=CARTESIAN_POINT('Origin',(10.9076228609,-20.7742356128,9.06099178277));
#90220=CARTESIAN_POINT('Origin',(10.4339531167,-21.0742356128,8.69270253038));
#90221=CARTESIAN_POINT('Origin',(-5.06274711921E-15,-21.0742356128,0.580061096523));
#90222=CARTESIAN_POINT('',(10.9433745451,-20.7742356128,7.99119341506));
#90223=CARTESIAN_POINT('Origin',(-1.97939039323E-16,-20.7742356128,0.580061096523));
#90224=CARTESIAN_POINT('Origin',(10.9433745451,-21.0742356128,7.99119341506));
#90225=CARTESIAN_POINT('Origin',(11.4401704731,-21.0742356128,8.32763628675));
#90226=CARTESIAN_POINT('Origin',(11.4401704731,-20.7742356128,8.32763628675));
#90227=CARTESIAN_POINT('Origin',(2.93915231795E-16,-20.7742356128,0.729452270839));
#90228=CARTESIAN_POINT('Origin',(-8.21591479143,-23.2742356128,11.6886688365));
#90229=CARTESIAN_POINT('',(-8.01224741424,-22.8742356128,11.9089404858));
#90230=CARTESIAN_POINT('',(-8.01224741424,-25.4742356128,11.9089404858));
#90231=CARTESIAN_POINT('',(-8.01224741424,-24.1742356128,11.9089404858));
#90232=CARTESIAN_POINT('',(-8.03752439844,-25.4742356128,11.4474700229));
#90233=CARTESIAN_POINT('Origin',(-8.21591479143,-25.4742356128,11.6886688365));
#90234=CARTESIAN_POINT('',(-8.03752439844,-23.4742356128,11.4474700229));
#90235=CARTESIAN_POINT('',(-8.03752439844,-22.6642356128,11.4474700229));
#90236=CARTESIAN_POINT('',(-7.99564314217,-23.4742356128,11.4850014593));
#90237=CARTESIAN_POINT('Origin',(-8.21591479143,-23.4742356128,11.6886688365));
#90238=CARTESIAN_POINT('Ctrl Pts',(-7.99564314217397,-23.4742356128,11.4850014593037));
#90239=CARTESIAN_POINT('Ctrl Pts',(-7.98401306350167,-23.4742356128,11.4975796966502));
#90240=CARTESIAN_POINT('Ctrl Pts',(-7.9733574518956,-23.4712114944548,11.5112709020565));
#90241=CARTESIAN_POINT('Ctrl Pts',(-7.9638973064836,-23.4651632577643,11.5259199892497));
#90242=CARTESIAN_POINT('Ctrl Pts',(-7.95801133283008,-23.4614001272563,
11.53503445182));
#90243=CARTESIAN_POINT('Ctrl Pts',(-7.95258786652577,-23.456466312469,11.544518764159));
#90244=CARTESIAN_POINT('Ctrl Pts',(-7.94767597957468,-23.4503618134027,
11.5543262155101));
#90245=CARTESIAN_POINT('Ctrl Pts',(-7.94127275672447,-23.4424038802702,
11.5671113828436));
#90246=CARTESIAN_POINT('Ctrl Pts',(-7.9357395366415,-23.4324564638547,11.5804463404673));
#90247=CARTESIAN_POINT('Ctrl Pts',(-7.93117367235329,-23.420519564156,11.5942098765918));
#90248=CARTESIAN_POINT('Ctrl Pts',(-7.92889074020919,-23.4145511143067,
11.601091644654));
#90249=CARTESIAN_POINT('Ctrl Pts',(-7.92684942663567,-23.4080852936365,
11.6080802486667));
#90250=CARTESIAN_POINT('Ctrl Pts',(-7.92506041898695,-23.4011221021457,
11.6151587417459));
#90251=CARTESIAN_POINT('Ctrl Pts',(-7.92416591516259,-23.3976405064002,
11.6186979882854));
#90252=CARTESIAN_POINT('Ctrl Pts',(-7.92333446790805,-23.3940345679496,
11.6222597024052));
#90253=CARTESIAN_POINT('Ctrl Pts',(-7.92256731255003,-23.3903042867937,
11.6258416398829));
#90254=CARTESIAN_POINT('Ctrl Pts',(-7.92214484180027,-23.3882500292561,
11.6278142048869));
#90255=CARTESIAN_POINT('Ctrl Pts',(-7.92165638884266,-23.385690596397,11.6302162286501));
#90256=CARTESIAN_POINT('Ctrl Pts',(-7.92124875102252,-23.3833982859291,
11.6323489942543));
#90257=CARTESIAN_POINT('Ctrl Pts',(-7.92091616827586,-23.3815280401522,
11.6340890708803));
#90258=CARTESIAN_POINT('Ctrl Pts',(-7.9206353184784,-23.3798356062595,11.635649439268));
#90259=CARTESIAN_POINT('Ctrl Pts',(-7.92045987171943,-23.3787404152106,
11.6366458567813));
#90260=CARTESIAN_POINT('Ctrl Pts',(-7.9179685496474,-23.3631888390565,11.6507948610625));
#90261=CARTESIAN_POINT('Ctrl Pts',(-7.91642902368058,-23.3454430882469,
11.665497956093));
#90262=CARTESIAN_POINT('Ctrl Pts',(-7.91602298477787,-23.325503162782,11.6806125158188));
#90263=CARTESIAN_POINT('Ctrl Pts',(-7.91591988682191,-23.3204401859498,
11.6844502766898));
#90264=CARTESIAN_POINT('Ctrl Pts',(-7.91588981140854,-23.3152357483491,
11.688314310615));
#90265=CARTESIAN_POINT('Ctrl Pts',(-7.91593559468154,-23.3098898499798,
11.6922017557107));
#90266=CARTESIAN_POINT('Ctrl Pts',(-7.91604864227584,-23.2966898118354,
11.7018005957939));
#90267=CARTESIAN_POINT('Ctrl Pts',(-7.91662445381236,-23.2826273017215,
11.7115427457266));
#90268=CARTESIAN_POINT('Ctrl Pts',(-7.91770341386166,-23.2677023196379,
11.7213792979579));
#90269=CARTESIAN_POINT('Ctrl Pts',(-7.91824289388631,-23.2602398285961,
11.7262975740736));
#90270=CARTESIAN_POINT('Ctrl Pts',(-7.91890812230629,-23.2525617195619,
11.731239455762));
#90271=CARTESIAN_POINT('Ctrl Pts',(-7.91970373737013,-23.2446679925353,
11.7361978955349));
#90272=CARTESIAN_POINT('Ctrl Pts',(-7.92010154490205,-23.240721129022,11.7386771154213));
#90273=CARTESIAN_POINT('Ctrl Pts',(-7.92053194513749,-23.2367203610106,
11.7411604752441));
#90274=CARTESIAN_POINT('Ctrl Pts',(-7.92099549064719,-23.2326656885011,
11.7436470687904));
#90275=CARTESIAN_POINT('Ctrl Pts',(-7.92122726340204,-23.2306383522464,
11.7448903655636));
#90276=CARTESIAN_POINT('Ctrl Pts',(-7.92146732225737,-23.2285975398671,
11.7461344708073));
#90277=CARTESIAN_POINT('Ctrl Pts',(-7.92171573426593,-23.2265432513633,
11.7473792679732));
#90278=CARTESIAN_POINT('Ctrl Pts',(-7.92193628450917,-23.2247193708197,
11.7484844493182));
#90279=CARTESIAN_POINT('Ctrl Pts',(-7.92226510694275,-23.2220783175044,
11.7500732961721));
#90280=CARTESIAN_POINT('Ctrl Pts',(-7.9224315764798,-23.2207683548869,11.7508588882968));
#90281=CARTESIAN_POINT('Ctrl Pts',(-7.92245260631457,-23.22060286937,11.7509581309143));
#90282=CARTESIAN_POINT('Ctrl Pts',(-7.92247097527054,-23.2204586265584,
11.7510445692356));
#90283=CARTESIAN_POINT('Ctrl Pts',(-7.92248609565397,-23.2203399574783,
11.7511156178036));
#90284=CARTESIAN_POINT('Ctrl Pts',(-7.92419557411386,-23.2069234831436,
11.7591482181149));
#90285=CARTESIAN_POINT('Ctrl Pts',(-7.92639661216216,-23.1916362840756,
11.7678836193289));
#90286=CARTESIAN_POINT('Ctrl Pts',(-7.92928545952422,-23.1744783602743,
11.7772330848807));
#90287=CARTESIAN_POINT('Ctrl Pts',(-7.93206140751313,-23.1579909872495,
11.7862171629034));
#90288=CARTESIAN_POINT('Ctrl Pts',(-7.93547326947577,-23.139776252284,11.7957687872142));
#90289=CARTESIAN_POINT('Ctrl Pts',(-7.93971042418088,-23.119834155378,11.8057634457376));
#90290=CARTESIAN_POINT('Ctrl Pts',(-7.94370007518413,-23.1010569304558,
11.8151742891409));
#90291=CARTESIAN_POINT('Ctrl Pts',(-7.94842224736297,-23.080748249551,11.8249780647689));
#90292=CARTESIAN_POINT('Ctrl Pts',(-7.95403716199756,-23.0589081126635,
11.835024933752));
#90293=CARTESIAN_POINT('Ctrl Pts',(-7.95946291660408,-23.0378037449151,
11.844733335253));
#90294=CARTESIAN_POINT('Ctrl Pts',(-7.96572310798611,-23.0152693690631,
11.8546688582846));
#90295=CARTESIAN_POINT('Ctrl Pts',(-7.9729525225692,-22.9913049851077,11.8646499034078));
#90296=CARTESIAN_POINT('Ctrl Pts',(-7.97983963799616,-22.9684752695698,
11.8741583648545));
#90297=CARTESIAN_POINT('Ctrl Pts',(-7.98760710476378,-22.9443477564508,
11.883707961496));
#90298=CARTESIAN_POINT('Ctrl Pts',(-7.99635127818823,-22.9189224457506,
11.893099420447));
#90299=CARTESIAN_POINT('Ctrl Pts',(-8.00132945383483,-22.9044474740876,
11.8984461044578));
#90300=CARTESIAN_POINT('Ctrl Pts',(-8.00662377160518,-22.8895518631041,
11.9037407582921));
#90301=CARTESIAN_POINT('Ctrl Pts',(-8.01224741425901,-22.8742356128,11.9089404857794));
#90302=CARTESIAN_POINT('Origin',(7.16045579301E-17,-22.6642356128,0.580061096523));
#90303=CARTESIAN_POINT('',(-8.73611663980898,-23.4697909663899,10.8942572011661));
#90304=CARTESIAN_POINT('',(-8.67864985337,-23.4742356128,10.942657873));
#90305=CARTESIAN_POINT('Origin',(-8.65818093366798,-22.8777633816448,10.9233631052074));
#90306=CARTESIAN_POINT('Origin',(-2.3120230745E-14,-23.4742356128,0.580061096523));
#90307=CARTESIAN_POINT('',(-8.73611663424,-25.4742356128,10.8942572059));
#90308=CARTESIAN_POINT('Origin',(1.5714690362E-14,-25.4742356128,0.580061096523));
#90309=CARTESIAN_POINT('',(-8.73611663424,-23.2742356128,10.8942572059));
#90310=CARTESIAN_POINT('Origin',(-8.93001206801,-23.2742356128,11.1231776304));
#90311=CARTESIAN_POINT('',(-9.1336794452,-25.4742356128,10.9029059811));
#90312=CARTESIAN_POINT('Origin',(-8.93001206801,-25.4742356128,11.1231776304));
#90313=CARTESIAN_POINT('',(-9.1336794452,-22.8742356128,10.9029059811));
#90314=CARTESIAN_POINT('',(-9.1336794452,-24.1742356128,10.9029059811));
#90315=CARTESIAN_POINT('Ctrl Pts',(-9.1336794452,-22.8742356128,10.9029059811));
#90316=CARTESIAN_POINT('Ctrl Pts',(-9.12940941048534,-22.8858810056524,
10.8989462223991));
#90317=CARTESIAN_POINT('Ctrl Pts',(-9.1250732717887,-22.8973540636349,10.8951670399834));
#90318=CARTESIAN_POINT('Ctrl Pts',(-9.12071717713756,-22.9085797926161,
10.8915793258319));
#90319=CARTESIAN_POINT('Ctrl Pts',(-9.11587741156969,-22.9210519496623,
10.8875932564721));
#90320=CARTESIAN_POINT('Ctrl Pts',(-9.11101276238942,-22.9332196957832,
10.8838431045504));
#90321=CARTESIAN_POINT('Ctrl Pts',(-9.10616236875762,-22.945041707572,10.8803242976032));
#90322=CARTESIAN_POINT('Ctrl Pts',(-9.10059797910354,-22.9586039635624,
10.8762875091572));
#90323=CARTESIAN_POINT('Ctrl Pts',(-9.09505210507099,-22.9717121890023,
10.8725546903098));
#90324=CARTESIAN_POINT('Ctrl Pts',(-9.08955784168385,-22.9843649123,10.8691025663662));
#90325=CARTESIAN_POINT('Ctrl Pts',(-9.08282324320706,-22.9998739996959,
10.8648711222191));
#90326=CARTESIAN_POINT('Ctrl Pts',(-9.07616602179342,-23.0146999042907,
10.8610606879207));
#90327=CARTESIAN_POINT('Ctrl Pts',(-9.06961407777495,-23.0289064212666,
10.8576164151034));
#90328=CARTESIAN_POINT('Ctrl Pts',(-9.06227588436141,-23.0448177552169,
10.8537588210777));
#90329=CARTESIAN_POINT('Ctrl Pts',(-9.05506908330778,-23.0599544556301,
10.850359635989));
#90330=CARTESIAN_POINT('Ctrl Pts',(-9.04800375660265,-23.0744480608874,
10.8473434006867));
#90331=CARTESIAN_POINT('Ctrl Pts',(-9.03773489471981,-23.0955133048292,
10.842959554756));
#90332=CARTESIAN_POINT('Ctrl Pts',(-9.0278615445671,-23.1149522563626,10.8394273586293));
#90333=CARTESIAN_POINT('Ctrl Pts',(-9.01851166005801,-23.1327720803782,
10.8365549291929));
#90334=CARTESIAN_POINT('Ctrl Pts',(-9.01554963574945,-23.1384173642164,
10.8356449494165));
#90335=CARTESIAN_POINT('Ctrl Pts',(-9.01263990783723,-23.1438998494754,
10.8348012685031));
#90336=CARTESIAN_POINT('Ctrl Pts',(-9.00978606355942,-23.1492187492881,
10.8340181186981));
#90337=CARTESIAN_POINT('Ctrl Pts',(-9.00385493895204,-23.1602729815769,
10.8323905039343));
#90338=CARTESIAN_POINT('Ctrl Pts',(-8.99816412150493,-23.1706234478825,
10.8310236012099));
#90339=CARTESIAN_POINT('Ctrl Pts',(-8.99273569023084,-23.1802701547496,
10.8298674484874));
#90340=CARTESIAN_POINT('Ctrl Pts',(-8.9900214745938,-23.1850935081831,10.8292893721262));
#90341=CARTESIAN_POINT('Ctrl Pts',(-8.98737294268441,-23.1897410872773,
10.8287640185669));
#90342=CARTESIAN_POINT('Ctrl Pts',(-8.98478347236165,-23.1942025419636,
10.8282841697181));
#90343=CARTESIAN_POINT('Ctrl Pts',(-8.98348873720026,-23.1964332693068,
10.8280442452937));
#90344=CARTESIAN_POINT('Ctrl Pts',(-8.98221073044467,-23.198619790564,10.8278160958339));
#90345=CARTESIAN_POINT('Ctrl Pts',(-8.98095114953504,-23.2007638642198,
10.8275992663868));
#90346=CARTESIAN_POINT('Ctrl Pts',(-8.98032135908022,-23.2018359010476,
10.8274908516632));
#90347=CARTESIAN_POINT('Ctrl Pts',(-8.97969617700721,-23.2028973291489,
10.8273852661301));
#90348=CARTESIAN_POINT('Ctrl Pts',(-8.97907565827039,-23.2039481859462,
10.8272824227911));
#90349=CARTESIAN_POINT('Ctrl Pts',(-8.97876539890198,-23.2044736143448,
10.8272310011215));
#90350=CARTESIAN_POINT('Ctrl Pts',(-8.97866475208692,-23.2046437660682,
10.8272145374228));
#90351=CARTESIAN_POINT('Ctrl Pts',(-8.9784612739697,-23.2049877805326,10.82718123946));
#90352=CARTESIAN_POINT('Ctrl Pts',(-8.9783587400747,-23.2051611315713,10.8271644604084));
#90353=CARTESIAN_POINT('Ctrl Pts',(-8.97823005958759,-23.2053786520945,
10.8271434289838));
#90354=CARTESIAN_POINT('Ctrl Pts',(-8.97803512506575,-23.20570783814,10.8271118119532));
#90355=CARTESIAN_POINT('Ctrl Pts',(-8.97793803853632,-23.2058717882213,
10.8270960651899));
#90356=CARTESIAN_POINT('Ctrl Pts',(-8.97782451443108,-23.206063436029,10.827077696863));
#90357=CARTESIAN_POINT('Ctrl Pts',(-8.97768956490296,-23.2062911099582,
10.8270559676401));
#90358=CARTESIAN_POINT('Ctrl Pts',(-8.97757894031321,-23.2064777451793,
10.8270381551556));
#90359=CARTESIAN_POINT('Ctrl Pts',(-8.97745391794019,-23.2066885894156,
10.8270180844363));
#90360=CARTESIAN_POINT('Ctrl Pts',(-8.97731173154554,-23.206928224683,10.8269953726106));
#90361=CARTESIAN_POINT('Ctrl Pts',(-8.97723087601023,-23.2070644953711,
10.8269824573325));
#90362=CARTESIAN_POINT('Ctrl Pts',(-8.97714435523225,-23.2072102659226,
10.8269686725624));
#90363=CARTESIAN_POINT('Ctrl Pts',(-8.97705970789074,-23.2073528287402,
10.8269552241012));
#90364=CARTESIAN_POINT('Ctrl Pts',(-8.96621708389224,-23.22561394598,10.8252325875136));
#90365=CARTESIAN_POINT('Ctrl Pts',(-8.95542760073463,-23.2429744055504,
10.8241158085228));
#90366=CARTESIAN_POINT('Ctrl Pts',(-8.94472278985177,-23.2594373001478,
10.8235685069978));
#90367=CARTESIAN_POINT('Ctrl Pts',(-8.93052828447575,-23.2812669848033,
10.8228427889515));
#90368=CARTESIAN_POINT('Ctrl Pts',(-8.91648221334131,-23.3015171376975,
10.8231198537275));
#90369=CARTESIAN_POINT('Ctrl Pts',(-8.9026880892877,-23.3201078063195,10.824346632956));
#90370=CARTESIAN_POINT('Ctrl Pts',(-8.8895824540684,-23.3377705821867,10.8255121814896));
#90371=CARTESIAN_POINT('Ctrl Pts',(-8.87670585544422,-23.3539298048985,
10.8275373802581));
#90372=CARTESIAN_POINT('Ctrl Pts',(-8.86415748997195,-23.3685165511626,
10.8303657063101));
#90373=CARTESIAN_POINT('Ctrl Pts',(-8.8532047363803,-23.3812484912618,10.8328343910478));
#90374=CARTESIAN_POINT('Ctrl Pts',(-8.84250263762646,-23.3927815156541,
10.8359149806679));
#90375=CARTESIAN_POINT('Ctrl Pts',(-8.8321114600471,-23.4031070884454,10.8395485817495));
#90376=CARTESIAN_POINT('Ctrl Pts',(-8.82183938576005,-23.413314309904,10.8431405346302));
#90377=CARTESIAN_POINT('Ctrl Pts',(-8.81187146444347,-23.4223413440303,
10.8472727389923));
#90378=CARTESIAN_POINT('Ctrl Pts',(-8.80225367273463,-23.430227052521,10.8518668482273));
#90379=CARTESIAN_POINT('Ctrl Pts',(-8.79231137006379,-23.4383788302848,
10.8566159658938));
#90380=CARTESIAN_POINT('Ctrl Pts',(-8.78274346738949,-23.4453111491342,
10.8618582840456));
#90381=CARTESIAN_POINT('Ctrl Pts',(-8.77358312485918,-23.4511185790067,
10.8674882887901));
#90382=CARTESIAN_POINT('Ctrl Pts',(-8.76340116713159,-23.4575736875654,
10.8737461847284));
#90383=CARTESIAN_POINT('Ctrl Pts',(-8.75372315170681,-23.4626395111084,
10.8804822534289));
#90384=CARTESIAN_POINT('Ctrl Pts',(-8.74456740587474,-23.4665045713782,
10.8875378283139));
#90385=CARTESIAN_POINT('Ctrl Pts',(-8.74169943618646,-23.4677152729311,
10.8897479349808));
#90386=CARTESIAN_POINT('Ctrl Pts',(-8.73888250639547,-23.4688085064365,
10.8919893551245));
#90387=CARTESIAN_POINT('Ctrl Pts',(-8.73611663424,-23.4697908757,10.8942572059));
#90388=CARTESIAN_POINT('Origin',(-10.806321674,-23.2742356128,10.0787147334));
#90389=CARTESIAN_POINT('',(-11.031648508,-22.9538972343,10.2767748704));
#90390=CARTESIAN_POINT('',(-11.0909930576,-22.9538972343,10.1733836478));
#90391=CARTESIAN_POINT('Ctrl Pts',(-11.0316485080236,-22.9538972342712,
10.2767748704012));
#90392=CARTESIAN_POINT('Ctrl Pts',(-11.0364414874478,-22.9576018392429,
10.2713220473568));
#90393=CARTESIAN_POINT('Ctrl Pts',(-11.0412887837959,-22.9605581903059,
10.2654028401508));
#90394=CARTESIAN_POINT('Ctrl Pts',(-11.050182860397,-22.9647393225438,10.2535848889028));
#90395=CARTESIAN_POINT('Ctrl Pts',(-11.0542446140175,-22.9661256456956,
10.247786383537));
#90396=CARTESIAN_POINT('Ctrl Pts',(-11.0610297049498,-22.9675767047451,
10.2373096114452));
#90397=CARTESIAN_POINT('Ctrl Pts',(-11.0638318077743,-22.9678862078995,
10.2327193905693));
#90398=CARTESIAN_POINT('Ctrl Pts',(-11.0665081104589,-22.9678862078995,
10.2280566842471));
#90399=CARTESIAN_POINT('Ctrl Pts',(-11.0692420535233,-22.9678862078995,
10.2232935557399));
#90400=CARTESIAN_POINT('Ctrl Pts',(-11.071844430281,-22.9675632436939,10.2184552280518));
#90401=CARTESIAN_POINT('Ctrl Pts',(-11.077589003477,-22.9660452016239,10.2070412179224));
#90402=CARTESIAN_POINT('Ctrl Pts',(-11.0806076488283,-22.9645897469489,
10.2004413153353));
#90403=CARTESIAN_POINT('Ctrl Pts',(-11.0862338558044,-22.9603378044189,
10.1869112738819));
#90404=CARTESIAN_POINT('Ctrl Pts',(-11.0887879815709,-22.9574629735521,
10.1800143570539));
#90405=CARTESIAN_POINT('Ctrl Pts',(-11.0909930576014,-22.9538972342539,
10.1733836478253));
#90406=CARTESIAN_POINT('',(-11.031648508,-25.4742356128,10.2767748704));
#90407=CARTESIAN_POINT('',(-11.031648508,-22.6642356128,10.2767748704));
#90408=CARTESIAN_POINT('',(-11.0909930576,-25.4742356128,10.1733836478));
#90409=CARTESIAN_POINT('Origin',(-10.806321674,-25.4742356128,10.0787147334));
#90410=CARTESIAN_POINT('',(-11.0909930576,-22.6642356128,10.1733836478));
#90411=CARTESIAN_POINT('Origin',(-10.8795671881,-23.2742356128,9.85222376962));
#90412=CARTESIAN_POINT('',(-11.1657658425,-21.0742356128,9.94217003248));
#90413=CARTESIAN_POINT('',(-11.0832345653,-21.0742356128,9.63195212036));
#90414=CARTESIAN_POINT('Ctrl Pts',(-11.1657658425273,-21.0742356128,9.94217003248857));
#90415=CARTESIAN_POINT('Ctrl Pts',(-11.1701441004766,-21.0742356127987,
9.92823891969006));
#90416=CARTESIAN_POINT('Ctrl Pts',(-11.1733712020923,-21.0741948386066,
9.91441315929395));
#90417=CARTESIAN_POINT('Ctrl Pts',(-11.1755965166384,-21.0741446195935,
9.90087185946038));
#90418=CARTESIAN_POINT('Ctrl Pts',(-11.1779157725236,-21.0740922805919,
9.88675891556742));
#90419=CARTESIAN_POINT('Ctrl Pts',(-11.1791476929329,-21.0740296825142,
9.87295501972334));
#90420=CARTESIAN_POINT('Ctrl Pts',(-11.1794763079321,-21.0739922922776,
9.85960752486672));
#90421=CARTESIAN_POINT('Ctrl Pts',(-11.179675594885,-21.0739696171522,9.85151300214193));
#90422=CARTESIAN_POINT('Ctrl Pts',(-11.1795428889997,-21.0739562128569,
9.84358524958266));
#90423=CARTESIAN_POINT('Ctrl Pts',(-11.1791199073328,-21.0739599897817,
9.83584792154246));
#90424=CARTESIAN_POINT('Ctrl Pts',(-11.1786092657732,-21.0739645494469,
9.82650708820039));
#90425=CARTESIAN_POINT('Ctrl Pts',(-11.1776611953628,-21.0739888517107,
9.81726250742656));
#90426=CARTESIAN_POINT('Ctrl Pts',(-11.1763323365263,-21.0740212860748,
9.80828692085334));
#90427=CARTESIAN_POINT('Ctrl Pts',(-11.1749746890983,-21.0740544231017,
9.7991168858652));
#90428=CARTESIAN_POINT('Ctrl Pts',(-11.1732200234797,-21.0740960483956,
9.79022835166622));
#90429=CARTESIAN_POINT('Ctrl Pts',(-11.1711809999612,-21.0741337803976,
9.78178667192448));
#90430=CARTESIAN_POINT('Ctrl Pts',(-11.1690077288837,-21.0741739966422,
9.77278919923085));
#90431=CARTESIAN_POINT('Ctrl Pts',(-11.1665121299432,-21.0742097900565,
9.76430006175474));
#90432=CARTESIAN_POINT('Ctrl Pts',(-11.1638809828609,-21.0742261689598,
9.75648628423073));
#90433=CARTESIAN_POINT('Ctrl Pts',(-11.1629285294711,-21.0742320979867,
9.75365776166727));
#90434=CARTESIAN_POINT('Ctrl Pts',(-11.1619587083146,-21.0742354829752,
9.75091738912241));
#90435=CARTESIAN_POINT('Ctrl Pts',(-11.1609814983982,-21.0742356128,9.74827192519493));
#90436=CARTESIAN_POINT('Ctrl Pts',(-11.1566371977885,-21.0742361899513,
9.73651120688754));
#90437=CARTESIAN_POINT('Ctrl Pts',(-11.1516844235512,-21.074236478527,9.72535793251623));
#90438=CARTESIAN_POINT('Ctrl Pts',(-11.146209343146,-21.074236586743,9.71473936631389));
#90439=CARTESIAN_POINT('Ctrl Pts',(-11.1406978489627,-21.0742366956787,
9.70405017793173));
#90440=CARTESIAN_POINT('Ctrl Pts',(-11.1346564614678,-21.0742366218476,
9.69390176377249));
#90441=CARTESIAN_POINT('Ctrl Pts',(-11.1281164027013,-21.074236475639,9.68422588891586));
#90442=CARTESIAN_POINT('Ctrl Pts',(-11.1214821824725,-21.0742363273254,
9.67441070422159));
#90443=CARTESIAN_POINT('Ctrl Pts',(-11.1143342358999,-21.0742361045353,
9.6650807888115));
#90444=CARTESIAN_POINT('Ctrl Pts',(-11.1066561229926,-21.0742359224949,
9.65618648834588));
#90445=CARTESIAN_POINT('Ctrl Pts',(-11.099345990661,-21.0742357491789,9.64771845535586));
#90446=CARTESIAN_POINT('Ctrl Pts',(-11.0915543979062,-21.0742356128004,
9.63964479662113));
#90447=CARTESIAN_POINT('Ctrl Pts',(-11.0832345652963,-21.0742356128,9.63195212036397));
#90448=CARTESIAN_POINT('',(-11.1657658425,-25.4742356128,9.94217003248));
#90449=CARTESIAN_POINT('',(-11.1657658425,-22.6642356128,9.94217003248));
#90450=CARTESIAN_POINT('',(-11.0832345653,-25.4742356128,9.63195212036));
#90451=CARTESIAN_POINT('Origin',(-10.8795671881,-25.4742356128,9.85222376962));
#90452=CARTESIAN_POINT('',(-11.0832345653,-23.2742356128,9.63195212036));
#90453=CARTESIAN_POINT('Origin',(-11.221722051,-23.1742356128,9.76000029674));
#90454=CARTESIAN_POINT('',(-10.7039554837,-21.0742356128,9.28126343203));
#90455=CARTESIAN_POINT('',(-9.20983954971,-21.0742356128,7.89977528084));
#90456=CARTESIAN_POINT('',(-10.7039554837,-25.4742356128,9.28126343203));
#90457=CARTESIAN_POINT('',(-11.080905232,-25.4742356128,9.62979837427));
#90458=CARTESIAN_POINT('',(-10.7039554837,-23.2742356128,9.28126343203));
#90459=CARTESIAN_POINT('Origin',(-10.9076228609,-23.2742356128,9.06099178277));
#90460=CARTESIAN_POINT('',(-10.6707879888,-25.4742356128,8.87684715658));
#90461=CARTESIAN_POINT('Origin',(-10.9076228609,-25.4742356128,9.06099178277));
#90462=CARTESIAN_POINT('',(-10.6707879888,-21.0742356128,8.87684715658));
#90463=CARTESIAN_POINT('',(-10.6707879888,-22.6642356128,8.87684715658));
#90464=CARTESIAN_POINT('Origin',(-10.9076228609,-21.0742356128,9.06099178277));
#90465=CARTESIAN_POINT('Origin',(7.16045579301E-17,-22.6642356128,0.580061096523));
#90466=CARTESIAN_POINT('',(-11.1917725091,-21.0742356128,8.1594148509));
#90467=CARTESIAN_POINT('Origin',(5.59539391719E-15,-21.0742356128,0.580061096523));
#90468=CARTESIAN_POINT('',(-11.1917725091,-25.4742356128,8.1594148509));
#90469=CARTESIAN_POINT('Origin',(-2.15888032654E-14,-25.4742356128,0.580061096523));
#90470=CARTESIAN_POINT('',(-11.1917725091,-23.2742356128,8.1594148509));
#90471=CARTESIAN_POINT('Origin',(-11.4401704731,-23.2742356128,8.32763628675));
#90472=CARTESIAN_POINT('',(-11.6438378503,-25.4742356128,8.10736463748));
#90473=CARTESIAN_POINT('Origin',(-11.4401704731,-25.4742356128,8.32763628675));
#90474=CARTESIAN_POINT('',(-11.6438378497605,-23.4645367153794,8.10736463698115));
#90475=CARTESIAN_POINT('',(-11.6438378503,-24.4693861731,8.10736463748));
#90476=CARTESIAN_POINT('',(-11.4067704324827,-22.8742356736,8.0295013564461));
#90477=CARTESIAN_POINT('Ctrl Pts',(-11.4067704237,-22.8742356736,8.02950135638));
#90478=CARTESIAN_POINT('Ctrl Pts',(-11.4067703651,-22.9402171391,8.02950137053));
#90479=CARTESIAN_POINT('Ctrl Pts',(-11.4114432261,-23.0062323557,8.02896986926));
#90480=CARTESIAN_POINT('Ctrl Pts',(-11.4203500465,-23.0707470797,8.02802946276));
#90481=CARTESIAN_POINT('Ctrl Pts',(-11.4529027709,-23.2147843626,8.02583184946));
#90482=CARTESIAN_POINT('Ctrl Pts',(-11.5102889752,-23.3423703627,8.03319245204));
#90483=CARTESIAN_POINT('Ctrl Pts',(-11.5554237252,-23.4131506081,8.04186749464));
#90484=CARTESIAN_POINT('Ctrl Pts',(-11.6054955414,-23.4487166343,8.07191260584));
#90485=CARTESIAN_POINT('Ctrl Pts',(-11.6438378503,-23.4645367334,8.10736463748));
#90486=CARTESIAN_POINT('',(-11.4067704497,-21.0742356128,8.02950135347));
#90487=CARTESIAN_POINT('',(-11.4067704497,-23.1237854196,8.02950135347));
#90488=CARTESIAN_POINT('Origin',(-11.4401704731,-21.0742356128,8.32763628675));
#90489=CARTESIAN_POINT('Origin',(-12.8942551175,-23.1742356128,9.2635243433));
#90490=CARTESIAN_POINT('',(-11.7384871149,-23.4742356128,8.19487915673));
#90491=CARTESIAN_POINT('',(-12.7478394324279,-23.4742356126688,9.12814559461005));
#90492=CARTESIAN_POINT('',(-6.46706166421,-23.4742356128,3.32081842676));
#90493=CARTESIAN_POINT('Origin',(-11.7384707086266,-22.6130235696614,8.19486399662491));
#90494=CARTESIAN_POINT('',(-12.7478394283,-25.4742356128,9.12814559847));
#90495=CARTESIAN_POINT('',(-12.1510854644,-25.4742356128,8.57637547707));
#90496=CARTESIAN_POINT('',(-12.7478394283,-22.5760378048,9.12814559847));
#90497=CARTESIAN_POINT('Origin',(-8.92072771219,-25.4742356128,12.3403523349));
#90498=CARTESIAN_POINT('',(-8.21591479143,-25.7742356128,11.6886688365));
#90499=CARTESIAN_POINT('',(-9.38771846805,-25.7742356128,12.7721409138));
#90500=CARTESIAN_POINT('',(-8.80181662974,-25.7742356128,12.2304048752));
#90501=CARTESIAN_POINT('Origin',(-8.21591479143,-25.4742356128,11.6886688365));
#90502=CARTESIAN_POINT('',(-9.18405109086,-25.4742356128,12.9924125631));
#90503=CARTESIAN_POINT('',(-8.59814925255,-25.4742356128,12.4506765244));
#90504=CARTESIAN_POINT('Origin',(-9.38771846803591,-25.4742356128,12.772140913833));
#90505=CARTESIAN_POINT('Origin',(-8.21591479143,-25.4742356128,11.6886688365));
#90506=CARTESIAN_POINT('Origin',(-8.21591479143,-25.4742356128,11.6886688365));
#90507=CARTESIAN_POINT('Origin',(1.5714690362E-14,-25.4742356128,0.580061096523));
#90508=CARTESIAN_POINT('',(-8.93001206801,-25.7742356128,11.1231776304));
#90509=CARTESIAN_POINT('Origin',(-8.93001206801,-25.4742356128,11.1231776304));
#90510=CARTESIAN_POINT('Origin',(-3.09260596606E-16,-25.7742356128,0.580061096523));
#90511=CARTESIAN_POINT('Origin',(-8.93001206801,-25.4742356128,11.1231776304));
#90512=CARTESIAN_POINT('Origin',(-8.93001206801,-25.4742356128,11.1231776304));
#90513=CARTESIAN_POINT('Origin',(-9.58357319026,-25.4742356128,11.7274727362));
#90514=CARTESIAN_POINT('',(-9.39452601497,-25.7742356128,11.5526761045));
#90515=CARTESIAN_POINT('',(-9.59819339216,-25.4742356128,11.3324044552));
#90516=CARTESIAN_POINT('Origin',(-9.39452601497,-25.4742356128,11.5526761045));
#90517=CARTESIAN_POINT('',(-9.36593641868,-25.4742356128,11.1176552182));
#90518=CARTESIAN_POINT('',(-9.16226904149,-25.7742356128,11.3379268674));
#90519=CARTESIAN_POINT('Origin',(-9.80186076935,-25.4742356128,11.1121328059));
#90520=CARTESIAN_POINT('',(-10.2106256241,-25.7742356128,11.5513494877));
#90521=CARTESIAN_POINT('',(-10.0062431967,-25.4742356128,11.3317411468));
#90522=CARTESIAN_POINT('Origin',(-10.2106256241,-25.4742356128,11.5513494877));
#90523=CARTESIAN_POINT('Origin',(-9.80186076935,-25.4742356128,11.1121328059));
#90524=CARTESIAN_POINT('Origin',(-9.80186076935,-25.7742356128,11.1121328059));
#90525=CARTESIAN_POINT('Origin',(-3.82523487143E-15,-25.4742356128,0.580061096523));
#90526=CARTESIAN_POINT('',(-11.256975342,-25.7742356128,10.4748350074));
#90527=CARTESIAN_POINT('Origin',(-11.256975342,-25.4742356128,10.4748350074));
#90528=CARTESIAN_POINT('Origin',(-2.72521192632E-16,-25.4742356128,0.580061096523));
#90529=CARTESIAN_POINT('Origin',(-1.47808545802E-15,-25.7742356128,0.580061096523));
#90530=CARTESIAN_POINT('Origin',(-10.806321674,-25.4742356128,10.0787147334));
#90531=CARTESIAN_POINT('',(-11.3756644412,-25.7742356128,10.2680525622));
#90532=CARTESIAN_POINT('Origin',(-11.3756644412,-25.4742356128,10.2680525622));
#90533=CARTESIAN_POINT('Origin',(-10.806321674,-25.7742356128,10.0787147334));
#90534=CARTESIAN_POINT('Origin',(2.84607155346,-25.4742356128,5.53854202767));
#90535=CARTESIAN_POINT('',(-11.4519644969,-25.7742356128,10.0321162953));
#90536=CARTESIAN_POINT('Origin',(-11.4519644969,-25.4742356128,10.0321162953));
#90537=CARTESIAN_POINT('Origin',(2.84607155346,-25.4742356128,5.53854202767));
#90538=CARTESIAN_POINT('Origin',(2.84607155346,-25.7742356128,5.53854202767));
#90539=CARTESIAN_POINT('Origin',(-10.8795671881,-25.4742356128,9.85222376962));
#90540=CARTESIAN_POINT('',(-11.2869019425,-25.7742356128,9.4116804711));
#90541=CARTESIAN_POINT('Origin',(-11.2869019425,-25.4742356128,9.4116804711));
#90542=CARTESIAN_POINT('Origin',(-10.8795671881,-25.7742356128,9.85222376962));
#90543=CARTESIAN_POINT('Origin',(-11.2845726092,-25.4742356128,9.409526725));
#90544=CARTESIAN_POINT('',(-10.9076228609,-25.7742356128,9.06099178277));
#90545=CARTESIAN_POINT('Origin',(-10.9076228609,-25.4742356128,9.06099178277));
#90546=CARTESIAN_POINT('',(-11.0972624017,-25.7742356128,9.23633612693));
#90547=CARTESIAN_POINT('Origin',(-10.9076228609,-25.4742356128,9.06099178277));
#90548=CARTESIAN_POINT('Origin',(-10.9076228609,-25.4742356128,9.06099178277));
#90549=CARTESIAN_POINT('Origin',(-2.15888032654E-14,-25.4742356128,0.580061096523));
#90550=CARTESIAN_POINT('',(-11.4401704731,-25.7742356128,8.32763628675));
#90551=CARTESIAN_POINT('Origin',(-11.4401704731,-25.4742356128,8.32763628675));
#90552=CARTESIAN_POINT('Origin',(-3.09260596606E-16,-25.7742356128,0.580061096523));
#90553=CARTESIAN_POINT('Origin',(-11.4401704731,-25.4742356128,8.32763628675));
#90554=CARTESIAN_POINT('Origin',(-11.4401704731,-25.4742356128,8.32763628675));
#90555=CARTESIAN_POINT('Origin',(-11.9474180872,-25.4742356128,8.79664712633));
#90556=CARTESIAN_POINT('',(-12.5441720511,-25.7742356128,9.34841724773));
#90557=CARTESIAN_POINT('',(-11.9921712621,-25.7742356128,8.83802676724));
#90558=CARTESIAN_POINT('Origin',(-12.5441720511046,-25.4742356128,9.34841724773267));
#90559=CARTESIAN_POINT('Origin',(-3.18408167778E-16,-25.7742356128,0.729452270839));
#90560=CARTESIAN_POINT('',(-12.1784264826,-25.7742356128,9.98548488886));
#90561=CARTESIAN_POINT('Origin',(-3.09260596606E-16,-25.7742356128,0.580061096523));
#90562=CARTESIAN_POINT('Origin',(-10.0415172382,-25.7742356128,8.33514586886));
#90563=CARTESIAN_POINT('Origin',(-3.39394702409,-23.1742356128,-9.39793292047));
#90564=CARTESIAN_POINT('',(-3.39394702409,-21.0742356128,-7.0794205347));
#90565=CARTESIAN_POINT('',(-3.39394702409,-21.0742356128,-7.27665075431));
#90566=CARTESIAN_POINT('',(-3.39394702409,-21.0742356128,-6.14889144395));
#90567=CARTESIAN_POINT('',(-3.39394702409,-22.8742356071,-7.27665075406));
#90568=CARTESIAN_POINT('',(-3.39394702409,-23.1223803511,-7.27665075431));
#90569=CARTESIAN_POINT('',(-3.39394702409,-23.4742356128,-7.94679080481));
#90570=CARTESIAN_POINT('Ctrl Pts',(-3.39394702409,-22.8742356071,-7.27665075406));
#90571=CARTESIAN_POINT('Ctrl Pts',(-3.39394702409,-22.8963796807801,-7.27665075202916));
#90572=CARTESIAN_POINT('Ctrl Pts',(-3.39394702409,-22.9185266226574,-7.27803164667852));
#90573=CARTESIAN_POINT('Ctrl Pts',(-3.39394702409019,-22.9404763729725,
-7.28076880448012));
#90574=CARTESIAN_POINT('Ctrl Pts',(-3.39394702409038,-22.9635612306701,
-7.28364751141022));
#90575=CARTESIAN_POINT('Ctrl Pts',(-3.39394702409077,-22.9864277437381,
-7.28802596271889));
#90576=CARTESIAN_POINT('Ctrl Pts',(-3.39394702409072,-23.0088766193784,
-7.29382800372885));
#90577=CARTESIAN_POINT('Ctrl Pts',(-3.3939470240907,-23.0181604618048,-7.29622746619418));
#90578=CARTESIAN_POINT('Ctrl Pts',(-3.39394702409061,-23.0273732778489,
-7.29886989897477));
#90579=CARTESIAN_POINT('Ctrl Pts',(-3.39394702409046,-23.0365026587174,
-7.30174800896343));
#90580=CARTESIAN_POINT('Ctrl Pts',(-3.39394702409007,-23.0599555275722,
-7.30914171255472));
#90581=CARTESIAN_POINT('Ctrl Pts',(-3.39394702409004,-23.0828466467018,
-7.31809082810804));
#90582=CARTESIAN_POINT('Ctrl Pts',(-3.39394702409001,-23.1049940708735,
-7.32844271008414));
#90583=CARTESIAN_POINT('Ctrl Pts',(-3.39394702408999,-23.1281264931002,
-7.33925498797506));
#90584=CARTESIAN_POINT('Ctrl Pts',(-3.39394702409,-23.1504472805791,-7.35159636510977));
#90585=CARTESIAN_POINT('Ctrl Pts',(-3.39394702409,-23.1717995438951,-7.36526779521605));
#90586=CARTESIAN_POINT('Ctrl Pts',(-3.39394702409,-23.1802621945299,-7.37068626233385));
#90587=CARTESIAN_POINT('Ctrl Pts',(-3.39394702409,-23.1885732730389,-7.37631349194848));
#90588=CARTESIAN_POINT('Ctrl Pts',(-3.39394702409,-23.1967252289902,-7.38213675751289));
#90589=CARTESIAN_POINT('Ctrl Pts',(-3.39394702409,-23.216964154042,-7.39659422465562));
#90590=CARTESIAN_POINT('Ctrl Pts',(-3.39394702409,-23.2362264780343,-7.41226456121671));
#90591=CARTESIAN_POINT('Ctrl Pts',(-3.39394702409,-23.2544248664386,-7.42895825046336));
#90592=CARTESIAN_POINT('Ctrl Pts',(-3.39394702409,-23.2663051018241,-7.43985619116538));
#90593=CARTESIAN_POINT('Ctrl Pts',(-3.39394702409,-23.2777329032204,-7.45119035077379));
#90594=CARTESIAN_POINT('Ctrl Pts',(-3.39394702409,-23.2886950564466,-7.46291290030111));
#90595=CARTESIAN_POINT('Ctrl Pts',(-3.39394702409,-23.3092436284265,-7.48488683624042));
#90596=CARTESIAN_POINT('Ctrl Pts',(-3.39394702407267,-23.3281539933134,
-7.5082252168758));
#90597=CARTESIAN_POINT('Ctrl Pts',(-3.39394702415533,-23.3453669419493,
-7.53263177580096));
#90598=CARTESIAN_POINT('Ctrl Pts',(-3.39394702418428,-23.351396654865,-7.54118141750917));
#90599=CARTESIAN_POINT('Ctrl Pts',(-3.39394702422707,-23.3572183823464,
-7.54986251226728));
#90600=CARTESIAN_POINT('Ctrl Pts',(-3.39394702429189,-23.3628304875723,
-7.55866347490331));
#90601=CARTESIAN_POINT('Ctrl Pts',(-3.39394702449706,-23.3805929863697,
-7.58651881295321));
#90602=CARTESIAN_POINT('Ctrl Pts',(-3.39394702467124,-23.3962633147006,
-7.61557726389403));
#90603=CARTESIAN_POINT('Ctrl Pts',(-3.39394702467555,-23.4098082144408,
-7.64551044052));
#90604=CARTESIAN_POINT('Ctrl Pts',(-3.39394702468063,-23.4257384366872,
-7.68071499465771));
#90605=CARTESIAN_POINT('Ctrl Pts',(-3.39394702450576,-23.4387297283905,
-7.71712955274666));
#90606=CARTESIAN_POINT('Ctrl Pts',(-3.3939470243646,-23.448763496914,-7.75428420736052));
#90607=CARTESIAN_POINT('Ctrl Pts',(-3.39394702420207,-23.4603148681498,
-7.79705848579653));
#90608=CARTESIAN_POINT('Ctrl Pts',(-3.39394702411207,-23.4679503272946,
-7.84081579026664));
#90609=CARTESIAN_POINT('Ctrl Pts',(-3.39394702409605,-23.4716451363039,
-7.88490127919122));
#90610=CARTESIAN_POINT('Ctrl Pts',(-3.39394702408857,-23.4733699118574,
-7.90548084727437));
#90611=CARTESIAN_POINT('Ctrl Pts',(-3.39394702409,-23.4742356128,-7.92613251437262));
#90612=CARTESIAN_POINT('Ctrl Pts',(-3.39394702409,-23.4742356128,-7.94679080481));
#90613=CARTESIAN_POINT('',(-3.39394703109999,-23.4742356128,-9.19678217153944));
#90614=CARTESIAN_POINT('',(-3.39394702409,-23.4742356128,3.39628270998));
#90615=CARTESIAN_POINT('',(-3.39394702409,-25.4742356128,-9.19678210318));
#90616=CARTESIAN_POINT('',(-3.39394702409,-23.2742356128,-9.19678210318));
#90617=CARTESIAN_POINT('',(-3.39394702409,-25.4742356128,-7.0794205347));
#90618=CARTESIAN_POINT('',(-3.39394702409,-25.4742356128,-8.58812386759));
#90619=CARTESIAN_POINT('',(-3.39394702409,-23.2742356128,-7.0794205347));
#90620=CARTESIAN_POINT('Origin',(-3.09394702409,-23.2742356128,-7.0794205347));
#90621=CARTESIAN_POINT('',(-2.96616998276,-25.4742356128,-6.8079927769));
#90622=CARTESIAN_POINT('Origin',(-3.09394702409,-25.4742356128,-7.0794205347));
#90623=CARTESIAN_POINT('',(-2.96616998276,-21.0742356128,-6.8079927769));
#90624=CARTESIAN_POINT('',(-2.96616998276,-22.6642356128,-6.8079927769));
#90625=CARTESIAN_POINT('Origin',(-3.09394702409,-21.0742356128,-7.0794205347));
#90626=CARTESIAN_POINT('Origin',(2.84607155346,-22.6642356128,5.53854202767));
#90627=CARTESIAN_POINT('',(-2.60391380109,-21.0742356128,-6.97212274247));
#90628=CARTESIAN_POINT('Origin',(2.84607155346,-21.0742356128,5.53854202767));
#90629=CARTESIAN_POINT('',(-2.60391380109,-25.4742356128,-6.97212274247));
#90630=CARTESIAN_POINT('Origin',(2.84607155346,-25.4742356128,5.53854202767));
#90631=CARTESIAN_POINT('',(-2.60391380109,-23.2742356128,-6.97212274247));
#90632=CARTESIAN_POINT('Origin',(-2.72372695744,-23.2742356128,-7.24715875387));
#90633=CARTESIAN_POINT('',(-2.42372695744,-25.4742356128,-7.24715875387));
#90634=CARTESIAN_POINT('Origin',(-2.72372695744,-25.4742356128,-7.24715875387));
#90635=CARTESIAN_POINT('',(-2.42372695744,-21.0742356128,-7.24715875387));
#90636=CARTESIAN_POINT('',(-2.42372695744,-23.2742356128,-7.24715875387));
#90637=CARTESIAN_POINT('Origin',(-2.72372695744,-21.0742356128,-7.24715875387));
#90638=CARTESIAN_POINT('Origin',(-2.42372695744,-23.1742356128,-8.1710440518));
#90639=CARTESIAN_POINT('',(-2.42372695744,-25.4742356128,-7.96338790087));
#90640=CARTESIAN_POINT('',(-2.42372695744,-25.4742356128,-8.58812386759));
#90641=CARTESIAN_POINT('',(-2.42372695744,-21.0742356128,-7.96338790087));
#90642=CARTESIAN_POINT('',(-2.42372695744,-23.2742356128,-7.96338790087));
#90643=CARTESIAN_POINT('',(-2.42372695744,-21.0742356128,-6.11170048962));
#90644=CARTESIAN_POINT('Origin',(-2.12372695744,-23.2742356128,-7.96338790087));
#90645=CARTESIAN_POINT('',(-2.22735416732,-21.0742356128,-8.24492191546));
#90646=CARTESIAN_POINT('Origin',(-2.12372695744,-21.0742356128,-7.96338790087));
#90647=CARTESIAN_POINT('',(-2.22735416732,-25.4742356128,-8.24492191546));
#90648=CARTESIAN_POINT('Origin',(-2.12372695744,-25.4742356128,-7.96338790087));
#90649=CARTESIAN_POINT('',(-2.22735416732,-22.6642356128,-8.24492191546));
#90650=CARTESIAN_POINT('Origin',(-3.09394702409,-23.2742356128,-9.19678210318));
#90651=CARTESIAN_POINT('',(-3.20611083607784,-23.4742356128,-9.47502535777846));
#90652=CARTESIAN_POINT('',(-3.20611081633,-25.4742356128,-9.47502531282));
#90653=CARTESIAN_POINT('',(-3.20611081633,-20.0742356128,-9.47502531282));
#90654=CARTESIAN_POINT('Origin',(-3.09394702409,-25.4742356128,-9.19678210318));
#90655=CARTESIAN_POINT('Origin',(-3.09394702409079,-23.474235151356,-9.19678210318053));
#90656=CARTESIAN_POINT('Origin',(-3.09394702409,-25.4742356128,-8.58812386759));
#90657=CARTESIAN_POINT('',(-3.09394702409,-25.7742356128,-7.0794205347));
#90658=CARTESIAN_POINT('Origin',(-3.09394702409,-25.4742356128,-7.0794205347));
#90659=CARTESIAN_POINT('',(-3.09394702409,-25.7742356128,-9.19678210318));
#90660=CARTESIAN_POINT('Origin',(-3.09394702409,-25.4742356128,-9.19678210318));
#90661=CARTESIAN_POINT('',(-3.09394702409,-25.7742356128,-8.13810131894));
#90662=CARTESIAN_POINT('Origin',(-3.09394702409,-25.4742356128,-7.0794205347));
#90663=CARTESIAN_POINT('Origin',(-3.09394702409,-25.4742356128,-7.0794205347));
#90664=CARTESIAN_POINT('Origin',(2.84607155346,-25.4742356128,5.53854202767));
#90665=CARTESIAN_POINT('',(-2.72372695744,-25.7742356128,-7.24715875387));
#90666=CARTESIAN_POINT('Origin',(-2.72372695744,-25.4742356128,-7.24715875387));
#90667=CARTESIAN_POINT('Origin',(2.84607155346,-25.7742356128,5.53854202767));
#90668=CARTESIAN_POINT('Origin',(-2.72372695744,-25.4742356128,-7.24715875387));
#90669=CARTESIAN_POINT('Origin',(-2.72372695744,-25.4742356128,-7.24715875387));
#90670=CARTESIAN_POINT('Origin',(-2.72372695744,-25.4742356128,-8.58812386759));
#90671=CARTESIAN_POINT('',(-2.72372695744,-25.7742356128,-7.96338790087));
#90672=CARTESIAN_POINT('Origin',(-2.72372695744,-25.4742356128,-7.96338790087));
#90673=CARTESIAN_POINT('',(-2.72372695744,-25.7742356128,-7.60527332737));
#90674=CARTESIAN_POINT('Origin',(-2.12372695744,-25.4742356128,-7.96338790087));
#90675=CARTESIAN_POINT('',(-2.3309813772,-25.7742356128,-8.52645593005));
#90676=CARTESIAN_POINT('Origin',(-2.3309813772,-25.4742356128,-8.52645593005));
#90677=CARTESIAN_POINT('Origin',(-2.12372695744,-25.7742356128,-7.96338790087));
#90678=CARTESIAN_POINT('Ctrl Pts',(2.72048009119833E-16,-25.7742356128,
-9.1762777575));
#90679=CARTESIAN_POINT('Ctrl Pts',(2.72048009119833E-16,-25.7742356128,
-9.1762777575));
#90680=CARTESIAN_POINT('Ctrl Pts',(2.72048009119833E-16,-25.7742356128,
-9.1762777575));
#90681=CARTESIAN_POINT('Ctrl Pts',(2.72048009119833E-16,-25.7742356128,
-9.1762777575));
#90682=CARTESIAN_POINT('Ctrl Pts',(2.72048009119833E-16,-25.7742356128,
-9.1762777575));
#90683=CARTESIAN_POINT('Ctrl Pts',(2.72048009119833E-16,-25.7742356128,
-9.1762777575));
#90684=CARTESIAN_POINT('Ctrl Pts',(-0.0543179010659,-25.7751862689,-9.07845703679));
#90685=CARTESIAN_POINT('Ctrl Pts',(-0.0326006378767,-25.7751848901861,-9.0785989038544));
#90686=CARTESIAN_POINT('Ctrl Pts',(-0.0108684102149,-25.7751842248025,-9.07866737056662));
#90687=CARTESIAN_POINT('Ctrl Pts',(0.0108684102491,-25.7751842248025,-9.07866737056662));
#90688=CARTESIAN_POINT('Ctrl Pts',(0.0326006378991,-25.775184890186,-9.0785989038644));
#90689=CARTESIAN_POINT('Ctrl Pts',(0.0543179010637,-25.7751862689,-9.07845703679));
#90690=CARTESIAN_POINT('Ctrl Pts',(-0.109343357829,-25.7400248661,-8.98386898437));
#90691=CARTESIAN_POINT('Ctrl Pts',(-0.0655774722522,-25.7385135131,-8.98345841906));
#90692=CARTESIAN_POINT('Ctrl Pts',(-0.0218550902065,-25.7377882247,-8.98326842912));
#90693=CARTESIAN_POINT('Ctrl Pts',(0.0218550900655,-25.7377882247,-8.98326842912));
#90694=CARTESIAN_POINT('Ctrl Pts',(0.0655774721579,-25.7385135131,-8.98345841906));
#90695=CARTESIAN_POINT('Ctrl Pts',(0.109343357832,-25.7400248661,-8.98386898437));
#90696=CARTESIAN_POINT('Ctrl Pts',(-0.163251797833,-25.6940006666,-8.89703057892));
#90697=CARTESIAN_POINT('Ctrl Pts',(-0.098232070722,-25.681892459,-8.90144092994));
#90698=CARTESIAN_POINT('Ctrl Pts',(-0.0327886103307,-25.6757886735,-8.90359473304));
#90699=CARTESIAN_POINT('Ctrl Pts',(0.0327886095603,-25.6757886735,-8.90359473304));
#90700=CARTESIAN_POINT('Ctrl Pts',(0.0982320702102,-25.681892459,-8.90144092994));
#90701=CARTESIAN_POINT('Ctrl Pts',(0.16325179783,-25.6940006666,-8.89703057892));
#90702=CARTESIAN_POINT('Ctrl Pts',(-0.208904902042,-25.586489454,-8.82655958228));
#90703=CARTESIAN_POINT('Ctrl Pts',(-0.126605010039,-25.5795174219,-8.84455225061));
#90704=CARTESIAN_POINT('Ctrl Pts',(-0.0424177258938,-25.5759707943,-8.85368477148));
#90705=CARTESIAN_POINT('Ctrl Pts',(0.0424177261375,-25.5759707943,-8.85368477148));
#90706=CARTESIAN_POINT('Ctrl Pts',(0.126605010201,-25.5795174219,-8.84455225061));
#90707=CARTESIAN_POINT('Ctrl Pts',(0.208904902043,-25.586489454,-8.82655958228));
#90708=CARTESIAN_POINT('Ctrl Pts',(-0.20793136194,-25.4742356094,-8.82796730262));
#90709=CARTESIAN_POINT('Ctrl Pts',(-0.125978740127,-25.4742355994,-8.84538857459));
#90710=CARTESIAN_POINT('Ctrl Pts',(-0.042201592792,-25.4742355944,-8.85422697274));
#90711=CARTESIAN_POINT('Ctrl Pts',(0.042201592792,-25.4742355944,-8.85422697274));
#90712=CARTESIAN_POINT('Ctrl Pts',(0.125978740127,-25.4742355994,-8.84538857459));
#90713=CARTESIAN_POINT('Ctrl Pts',(0.20793136194,-25.4742356094,-8.82796730262));
#90714=CARTESIAN_POINT('',(-0.207931539813729,-25.4742356124822,-8.8279673345371));
#90715=CARTESIAN_POINT('Origin',(1.53982046821E-14,-25.4742356128,-7.84982397628));
#90716=CARTESIAN_POINT('Ctrl Pts',(-4.87606379654255E-15,-25.7742356128,
-9.17627775749999));
#90717=CARTESIAN_POINT('Ctrl Pts',(-0.00568547427394062,-25.7743351183165,
-9.16603882742094));
#90718=CARTESIAN_POINT('Ctrl Pts',(-0.011368426530604,-25.7739612468302,
-9.15579871367803));
#90719=CARTESIAN_POINT('Ctrl Pts',(-0.0170703292688694,-25.7731573020962,
-9.14559137800037));
#90720=CARTESIAN_POINT('Ctrl Pts',(-0.0226364418683845,-25.7723725032108,
-9.13562712881359));
#90721=CARTESIAN_POINT('Ctrl Pts',(-0.0282205239040065,-25.7711779079194,
-9.12569413414896));
#90722=CARTESIAN_POINT('Ctrl Pts',(-0.0337959481892083,-25.7696026140516,
-9.11582586073));
#90723=CARTESIAN_POINT('Ctrl Pts',(-0.0394393811271053,-25.7680081048545,
-9.10583721477161));
#90724=CARTESIAN_POINT('Ctrl Pts',(-0.0450930084467941,-25.7660239966216,
-9.09591552325664));
#90725=CARTESIAN_POINT('Ctrl Pts',(-0.0507631920877221,-25.7636711985576,
-9.08609020857896));
#90726=CARTESIAN_POINT('Ctrl Pts',(-0.0534551785308526,-25.7625541799753,
-9.08142552475446));
#90727=CARTESIAN_POINT('Ctrl Pts',(-0.056005605584535,-25.7614179275892,
-9.07703139117622));
#90728=CARTESIAN_POINT('Ctrl Pts',(-0.0586150679449305,-25.7601797386401,
-9.0725547076834));
#90729=CARTESIAN_POINT('Ctrl Pts',(-0.0611360075911444,-25.7589835536869,
-9.06822989002293));
#90730=CARTESIAN_POINT('Ctrl Pts',(-0.0637121682055152,-25.7576922631742,
-9.06382781887072));
#90731=CARTESIAN_POINT('Ctrl Pts',(-0.0665212281533235,-25.7561855928279,
-9.05904218763215));
#90732=CARTESIAN_POINT('Ctrl Pts',(-0.0669290135226217,-25.7559668726386,
-9.05834746753425));
#90733=CARTESIAN_POINT('Ctrl Pts',(-0.0673416988396855,-25.7557435281346,
-9.05764469015058));
#90734=CARTESIAN_POINT('Ctrl Pts',(-0.0677598182107501,-25.7555150997744,
-9.05693294696415));
#90735=CARTESIAN_POINT('Ctrl Pts',(-0.075841245909943,-25.7511000274162,
-9.04317634657783));
#90736=CARTESIAN_POINT('Ctrl Pts',(-0.083598223070189,-25.7460632812599,
-9.03005200253529));
#90737=CARTESIAN_POINT('Ctrl Pts',(-0.0909902917209981,-25.7405256146399,
-9.01760109199645));
#90738=CARTESIAN_POINT('Ctrl Pts',(-0.0950863809707422,-25.7374570856824,
-9.01070179990153));
#90739=CARTESIAN_POINT('Ctrl Pts',(-0.0990713564419826,-25.7342344321942,
-9.00400917533817));
#90740=CARTESIAN_POINT('Ctrl Pts',(-0.102944990399136,-25.7308778204123,
-8.99752866965076));
#90741=CARTESIAN_POINT('Ctrl Pts',(-0.108377113069743,-25.7261707347252,
-8.98844084611067));
#90742=CARTESIAN_POINT('Ctrl Pts',(-0.113590978844581,-25.7211999701095,
-8.97976991046837));
#90743=CARTESIAN_POINT('Ctrl Pts',(-0.118573216099615,-25.7160195091,-8.97152442357315));
#90744=CARTESIAN_POINT('Ctrl Pts',(-0.121064334727132,-25.7134292785952,
-8.96740168012554));
#90745=CARTESIAN_POINT('Ctrl Pts',(-0.123497555221235,-25.7107867120833,
-8.96338529594356));
#90746=CARTESIAN_POINT('Ctrl Pts',(-0.125871825980486,-25.7080985186622,
-8.9594754157065));
#90747=CARTESIAN_POINT('Ctrl Pts',(-0.127058961360111,-25.7067544219517,
-8.95752047558797));
#90748=CARTESIAN_POINT('Ctrl Pts',(-0.128010959055845,-25.7056534598856,
-8.95595469215668));
#90749=CARTESIAN_POINT('Ctrl Pts',(-0.1290598601512,-25.7044204435857,-8.95423111088934));
#90750=CARTESIAN_POINT('Ctrl Pts',(-0.130001663376611,-25.7033133242079,
-8.95268351559744));
#90751=CARTESIAN_POINT('Ctrl Pts',(-0.131021744978592,-25.7020999937992,
-8.95100844782097));
#90752=CARTESIAN_POINT('Ctrl Pts',(-0.132351089285718,-25.700475004152,
-8.94882886846802));
#90753=CARTESIAN_POINT('Ctrl Pts',(-0.132502256684463,-25.7002902172186,
-8.94858101594451));
#90754=CARTESIAN_POINT('Ctrl Pts',(-0.132657409241681,-25.7001000597447,
-8.94832666705564));
#90755=CARTESIAN_POINT('Ctrl Pts',(-0.132816874301156,-25.6999040417534,
-8.94806529151949));
#90756=CARTESIAN_POINT('Ctrl Pts',(-0.142818422392116,-25.687609916797,
-8.93167198251981));
#90757=CARTESIAN_POINT('Ctrl Pts',(-0.151863061499928,-25.6742515575359,
-8.91697497315247));
#90758=CARTESIAN_POINT('Ctrl Pts',(-0.159899286686074,-25.6601365363902,
-8.90397985664614));
#90759=CARTESIAN_POINT('Ctrl Pts',(-0.168778192586148,-25.6445414103669,
-8.88962206876096));
#90760=CARTESIAN_POINT('Ctrl Pts',(-0.176426109948507,-25.6280246493504,
-8.87734215821455));
#90761=CARTESIAN_POINT('Ctrl Pts',(-0.182828262798463,-25.6110143627422,
-8.86711124483626));
#90762=CARTESIAN_POINT('Ctrl Pts',(-0.189130157638363,-25.5942704580099,
-8.85704054803518));
#90763=CARTESIAN_POINT('Ctrl Pts',(-0.194226910336029,-25.5770510543607,
-8.8489534320159));
#90764=CARTESIAN_POINT('Ctrl Pts',(-0.198138215714044,-25.5597363439882,
-8.84280068827599));
#90765=CARTESIAN_POINT('Ctrl Pts',(-0.201688146798981,-25.5440213786154,
-8.83721641035621));
#90766=CARTESIAN_POINT('Ctrl Pts',(-0.204263213458548,-25.5282278823503,
-8.83322384006026));
#90767=CARTESIAN_POINT('Ctrl Pts',(-0.205880845811087,-25.5126006491252,
-8.83079326747201));
#90768=CARTESIAN_POINT('Ctrl Pts',(-0.207220444982422,-25.4996593719272,
-8.82878045348497));
#90769=CARTESIAN_POINT('Ctrl Pts',(-0.207903911128972,-25.4868311126593,
-8.82783840536747));
#90770=CARTESIAN_POINT('Ctrl Pts',(-0.207931361961233,-25.4742356118482,
-8.8279673025893));
#90771=CARTESIAN_POINT('Origin',(2.84607155346,-25.4742356128,5.53854202767));
#90772=CARTESIAN_POINT('Origin',(2.84607155346,-25.4742356128,5.53854202767));
#90773=CARTESIAN_POINT('Origin',(2.84607155346,-25.7742356128,5.53854202767));
#90774=CARTESIAN_POINT('Origin',(-3.09394702409,-25.4742356128,-9.19678210318));
#90775=CARTESIAN_POINT('Origin',(-3.09394702409,-25.4742356128,-9.19678210318));
#90776=CARTESIAN_POINT('Ctrl Pts',(-0.647446102181,-25.4742356128,-10.2675153591));
#90777=CARTESIAN_POINT('Ctrl Pts',(-0.392565377877,-25.4742356128,-10.3238501103));
#90778=CARTESIAN_POINT('Ctrl Pts',(-0.131557494527,-25.4742356128,-10.3524631675));
#90779=CARTESIAN_POINT('Ctrl Pts',(0.131557494527,-25.4742356128,-10.3524631675));
#90780=CARTESIAN_POINT('Ctrl Pts',(0.392565377877,-25.4742356128,-10.3238501103));
#90781=CARTESIAN_POINT('Ctrl Pts',(0.647446102181,-25.4742356128,-10.2675153591));
#90782=CARTESIAN_POINT('Ctrl Pts',(-0.647446102181,-25.5155830458,-10.2675153591));
#90783=CARTESIAN_POINT('Ctrl Pts',(-0.392565377877,-25.5235347589,-10.3238501103));
#90784=CARTESIAN_POINT('Ctrl Pts',(-0.131557494811,-25.5275737357,-10.3524631688));
#90785=CARTESIAN_POINT('Ctrl Pts',(0.131557494823,-25.5275737357,-10.3524631688));
#90786=CARTESIAN_POINT('Ctrl Pts',(0.392565377877,-25.5235347589,-10.3238501103));
#90787=CARTESIAN_POINT('Ctrl Pts',(0.647446102181,-25.5155830458,-10.2675153591));
#90788=CARTESIAN_POINT('Ctrl Pts',(-0.627595169723,-25.5568342995,-10.2641149764));
#90789=CARTESIAN_POINT('Ctrl Pts',(-0.380265102139,-25.5727314135,-10.3153699887));
#90790=CARTESIAN_POINT('Ctrl Pts',(-0.127389297365,-25.5808054122,-10.3413729865));
#90791=CARTESIAN_POINT('Ctrl Pts',(0.127389292297,-25.5808054122,-10.3413729864));
#90792=CARTESIAN_POINT('Ctrl Pts',(0.380265098792,-25.5727314135,-10.3153699887));
#90793=CARTESIAN_POINT('Ctrl Pts',(0.627595169723,-25.5568342995,-10.2641149764));
#90794=CARTESIAN_POINT('Ctrl Pts',(-0.597178385154,-25.585971161,-10.2587039368));
#90795=CARTESIAN_POINT('Ctrl Pts',(-0.361468937707,-25.6047622193,-10.3027765927));
#90796=CARTESIAN_POINT('Ctrl Pts',(-0.121028943718,-25.614285036,-10.3250995669));
#90797=CARTESIAN_POINT('Ctrl Pts',(0.121028934599,-25.614285036,-10.3250995669));
#90798=CARTESIAN_POINT('Ctrl Pts',(0.361468931643,-25.6047622194,-10.3027765927));
#90799=CARTESIAN_POINT('Ctrl Pts',(0.597178385154,-25.585971161,-10.2587039368));
#90800=CARTESIAN_POINT('Ctrl Pts',(-0.530488628937,-25.640279625,-10.2458929885));
#90801=CARTESIAN_POINT('Ctrl Pts',(-0.320457713344,-25.662289159,-10.27663424));
#90802=CARTESIAN_POINT('Ctrl Pts',(-0.107186299105,-25.6734095169,-10.2921548338));
#90803=CARTESIAN_POINT('Ctrl Pts',(0.107186308951,-25.6734095169,-10.2921548338));
#90804=CARTESIAN_POINT('Ctrl Pts',(0.320457719891,-25.662289159,-10.27663424));
#90805=CARTESIAN_POINT('Ctrl Pts',(0.530488628937,-25.640279625,-10.2458929885));
#90806=CARTESIAN_POINT('Ctrl Pts',(-0.4531778394,-25.6783993125,-10.2291640789));
#90807=CARTESIAN_POINT('Ctrl Pts',(-0.273239866064,-25.6975272473,-10.2484964575));
#90808=CARTESIAN_POINT('Ctrl Pts',(-0.0913048492628,-25.70716081,-10.258228475));
#90809=CARTESIAN_POINT('Ctrl Pts',(0.091304838632,-25.70716081,-10.258228475));
#90810=CARTESIAN_POINT('Ctrl Pts',(0.273239858995,-25.6975272473,-10.2484964575));
#90811=CARTESIAN_POINT('Ctrl Pts',(0.4531778394,-25.6783993125,-10.2291640789));
#90812=CARTESIAN_POINT('Ctrl Pts',(-0.413292394149,-25.6957964187,-10.2198588554));
#90813=CARTESIAN_POINT('Ctrl Pts',(-0.248982805037,-25.7129087236,-10.2346106919));
#90814=CARTESIAN_POINT('Ctrl Pts',(-0.0831639035802,-25.7215163706,-10.2420292941));
#90815=CARTESIAN_POINT('Ctrl Pts',(0.0831639040251,-25.7215163706,-10.2420292941));
#90816=CARTESIAN_POINT('Ctrl Pts',(0.24898280533,-25.7129087236,-10.2346106919));
#90817=CARTESIAN_POINT('Ctrl Pts',(0.41329239415,-25.6957964187,-10.2198588554));
#90818=CARTESIAN_POINT('Ctrl Pts',(-0.307070337712,-25.7341644835,-10.1935337935));
#90819=CARTESIAN_POINT('Ctrl Pts',(-0.184562591785,-25.7449724555,-10.1984969504));
#90820=CARTESIAN_POINT('Ctrl Pts',(-0.0615742676879,-25.7503882214,-10.2009791749));
#90821=CARTESIAN_POINT('Ctrl Pts',(0.0615742669891,-25.7503882214,-10.2009791749));
#90822=CARTESIAN_POINT('Ctrl Pts',(0.184562591324,-25.7449724555,-10.1984969504));
#90823=CARTESIAN_POINT('Ctrl Pts',(0.30707033771,-25.7341644835,-10.1935337935));
#90824=CARTESIAN_POINT('Ctrl Pts',(-0.198295724974,-25.7583712199,-10.1618347919));
#90825=CARTESIAN_POINT('Ctrl Pts',(-0.119029769688,-25.7627099942,-10.1626983779));
#90826=CARTESIAN_POINT('Ctrl Pts',(-0.0396853151447,-25.7648787482,-10.1631301076));
#90827=CARTESIAN_POINT('Ctrl Pts',(0.0396853162421,-25.7648787482,-10.1631301076));
#90828=CARTESIAN_POINT('Ctrl Pts',(0.119029770412,-25.7627099942,-10.1626983779));
#90829=CARTESIAN_POINT('Ctrl Pts',(0.198295724976,-25.7583712199,-10.1618347919));
#90830=CARTESIAN_POINT('Ctrl Pts',(-0.131798268447,-25.7686774631,-10.1406643293));
#90831=CARTESIAN_POINT('Ctrl Pts',(-0.0790791152422,-25.7701121563,-10.1406657135));
#90832=CARTESIAN_POINT('Ctrl Pts',(-0.0263597373143,-25.770829644,-10.1406665006));
#90833=CARTESIAN_POINT('Ctrl Pts',(0.0263597378916,-25.770829644,-10.1406665006));
#90834=CARTESIAN_POINT('Ctrl Pts',(0.0790791156243,-25.7701121563,-10.1406657135));
#90835=CARTESIAN_POINT('Ctrl Pts',(0.131798268439,-25.7686774631,-10.1406643293));
#90836=CARTESIAN_POINT('Ctrl Pts',(-0.065481115176,-25.7742356128,-10.1171486981));
#90837=CARTESIAN_POINT('Ctrl Pts',(-0.0392886691043,-25.7742356128,-10.1171486981));
#90838=CARTESIAN_POINT('Ctrl Pts',(-0.0130962204949,-25.7742356128,-10.1171486842));
#90839=CARTESIAN_POINT('Ctrl Pts',(0.0130962205017,-25.7742356128,-10.1171486842));
#90840=CARTESIAN_POINT('Ctrl Pts',(0.039288669111,-25.7742356128,-10.1171486981));
#90841=CARTESIAN_POINT('Ctrl Pts',(0.0654811151827,-25.7742356128,-10.1171486981));
#90842=CARTESIAN_POINT('Ctrl Pts',(3.42781358853E-16,-25.7742356128,-10.0919881826));
#90843=CARTESIAN_POINT('Ctrl Pts',(3.42781358853E-16,-25.7742356128,-10.0919881826));
#90844=CARTESIAN_POINT('Ctrl Pts',(3.42781358853E-16,-25.7742356128,-10.0919881826));
#90845=CARTESIAN_POINT('Ctrl Pts',(3.42781358853E-16,-25.7742356128,-10.0919881826));
#90846=CARTESIAN_POINT('Ctrl Pts',(3.42781358853E-16,-25.7742356128,-10.0919881826));
#90847=CARTESIAN_POINT('Ctrl Pts',(3.42781358853E-16,-25.7742356128,-10.0919881826));
#90848=CARTESIAN_POINT('',(-0.647446102181,-25.4742356128,-10.2675153591));
#90849=CARTESIAN_POINT('Ctrl Pts',(-3.24740234702858E-14,-25.7742356128,
-10.0919881826));
#90850=CARTESIAN_POINT('Ctrl Pts',(-0.0235196339982131,-25.7742356128,-10.1010256276367));
#90851=CARTESIAN_POINT('Ctrl Pts',(-0.0471678069020204,-25.7733772305021,
-10.1098045487055));
#90852=CARTESIAN_POINT('Ctrl Pts',(-0.0708866431001756,-25.7717289970315,
-10.1182789368445));
#90853=CARTESIAN_POINT('Ctrl Pts',(-0.0966290502736267,-25.7699401446291,
-10.1274763168592));
#90854=CARTESIAN_POINT('Ctrl Pts',(-0.122455512086546,-25.767221846971,
-10.1363160322598));
#90855=CARTESIAN_POINT('Ctrl Pts',(-0.148303169698643,-25.7636236570487,
-10.1447855092778));
#90856=CARTESIAN_POINT('Ctrl Pts',(-0.174041159353539,-25.7600407337376,
-10.1532190515022));
#90857=CARTESIAN_POINT('Ctrl Pts',(-0.199801235626655,-25.7555858123977,
-10.1612873432931));
#90858=CARTESIAN_POINT('Ctrl Pts',(-0.225517053246078,-25.7502618225559,
-10.1689985160843));
#90859=CARTESIAN_POINT('Ctrl Pts',(-0.249359974970968,-25.7453255815644,
-10.1761480802937));
#90860=CARTESIAN_POINT('Ctrl Pts',(-0.273165470049946,-25.7396420837996,
-10.1829919915144));
#90861=CARTESIAN_POINT('Ctrl Pts',(-0.296865340757198,-25.7331730781103,
-10.1895318604185));
#90862=CARTESIAN_POINT('Ctrl Pts',(-0.308029880813459,-25.7301256575553,
-10.1926126632315));
#90863=CARTESIAN_POINT('Ctrl Pts',(-0.319170697082919,-25.7269033259966,
-10.195625803403));
#90864=CARTESIAN_POINT('Ctrl Pts',(-0.330278797444865,-25.7234987590446,
-10.1985698394716));
#90865=CARTESIAN_POINT('Ctrl Pts',(-0.34261025619996,-25.7197192399929,
-10.2018381084078));
#90866=CARTESIAN_POINT('Ctrl Pts',(-0.354897638044309,-25.7157145097747,
-10.2050204892709));
#90867=CARTESIAN_POINT('Ctrl Pts',(-0.367105872537722,-25.7114687570995,
-10.2081139321681));
#90868=CARTESIAN_POINT('Ctrl Pts',(-0.385126196057862,-25.7052016890124,
-10.2126800995225));
#90869=CARTESIAN_POINT('Ctrl Pts',(-0.40297610449847,-25.6984122503821,
-10.2170528265071));
#90870=CARTESIAN_POINT('Ctrl Pts',(-0.420636994599819,-25.6910428686672,
-10.2212375928647));
#90871=CARTESIAN_POINT('Ctrl Pts',(-0.433545439506098,-25.6856565457064,
-10.2242962623691));
#90872=CARTESIAN_POINT('Ctrl Pts',(-0.446356355529867,-25.6799606038231,
-10.2272550722783));
#90873=CARTESIAN_POINT('Ctrl Pts',(-0.459049014260705,-25.6739129474909,
-10.2301142135947));
#90874=CARTESIAN_POINT('Ctrl Pts',(-0.470368158089606,-25.6685197282054,
-10.2326639577005));
#90875=CARTESIAN_POINT('Ctrl Pts',(-0.481594267898779,-25.662846955066,
-10.235134598567));
#90876=CARTESIAN_POINT('Ctrl Pts',(-0.492677079222134,-25.6568444879693,
-10.2375207710333));
#90877=CARTESIAN_POINT('Ctrl Pts',(-0.502760483560487,-25.6513833011821,
-10.2396917672812));
#90878=CARTESIAN_POINT('Ctrl Pts',(-0.512725655776792,-25.6456492313659,
-10.2417929043888));
#90879=CARTESIAN_POINT('Ctrl Pts',(-0.52249481072194,-25.6395855696877,
-10.2438139229356));
#90880=CARTESIAN_POINT('Ctrl Pts',(-0.525208289062237,-25.6379013283465,
-10.2443752806049));
#90881=CARTESIAN_POINT('Ctrl Pts',(-0.527906371542221,-25.6361915361913,
-10.2449304144876));
#90882=CARTESIAN_POINT('Ctrl Pts',(-0.530586719226974,-25.6344546812032,
-10.2454789998168));
#90883=CARTESIAN_POINT('Ctrl Pts',(-0.537810197396088,-25.6297738951391,
-10.246957425236));
#90884=CARTESIAN_POINT('Ctrl Pts',(-0.544908504816467,-25.6248998886178,
-10.2483888192076));
#90885=CARTESIAN_POINT('Ctrl Pts',(-0.551874314062618,-25.6198254103934,
-10.2497728843233));
#90886=CARTESIAN_POINT('Ctrl Pts',(-0.559323254554293,-25.6143989789504,
-10.2512529447611));
#90887=CARTESIAN_POINT('Ctrl Pts',(-0.566620766544608,-25.6087420717409,
-10.2526789006053));
#90888=CARTESIAN_POINT('Ctrl Pts',(-0.573704306571406,-25.602809065489,
-10.2540425086271));
#90889=CARTESIAN_POINT('Ctrl Pts',(-0.581145473669519,-25.5965765192272,
-10.2554749612015));
#90890=CARTESIAN_POINT('Ctrl Pts',(-0.588350320822431,-25.5900372592432,
-10.2568385890757));
#90891=CARTESIAN_POINT('Ctrl Pts',(-0.595190181936405,-25.583125162139,
-10.258115490506));
#90892=CARTESIAN_POINT('Ctrl Pts',(-0.601870189660219,-25.5763746066417,
-10.2593625496604));
#90893=CARTESIAN_POINT('Ctrl Pts',(-0.608201257607,-25.5692663939245,-10.2605267740838));
#90894=CARTESIAN_POINT('Ctrl Pts',(-0.614019955468735,-25.561757524453,
-10.261584913393));
#90895=CARTESIAN_POINT('Ctrl Pts',(-0.619257719139411,-25.5549983345689,
-10.2625374089107));
#90896=CARTESIAN_POINT('Ctrl Pts',(-0.624079449617989,-25.5479136958671,
-10.2634038182789));
#90897=CARTESIAN_POINT('Ctrl Pts',(-0.628342381682246,-25.5405057357972,
-10.2641635474767));
#90898=CARTESIAN_POINT('Ctrl Pts',(-0.632390115918174,-25.5334717382713,
-10.2648849246504));
#90899=CARTESIAN_POINT('Ctrl Pts',(-0.6359336164384,-25.5261456012722,-10.265510058591));
#90900=CARTESIAN_POINT('Ctrl Pts',(-0.638836694515535,-25.518571015401,
-10.266019087808));
#90901=CARTESIAN_POINT('Ctrl Pts',(-0.641550569217845,-25.5114900907996,
-10.2664949418767));
#90902=CARTESIAN_POINT('Ctrl Pts',(-0.643704468813425,-25.5041918114808,
-10.2668692865141));
#90903=CARTESIAN_POINT('Ctrl Pts',(-0.645179709623052,-25.4967551141897,
-10.2671246377927));
#90904=CARTESIAN_POINT('Ctrl Pts',(-0.646649962504335,-25.4893435610736,
-10.2673791257046));
#90905=CARTESIAN_POINT('Ctrl Pts',(-0.647445936812433,-25.481793895823,
-10.2675153956504));
#90906=CARTESIAN_POINT('Ctrl Pts',(-0.647446102181,-25.4742356128,-10.2675153591));
#90907=CARTESIAN_POINT('Origin',(4.4311807394E-15,-25.4742356128,-7.33821278943));
#90908=CARTESIAN_POINT('Origin',(2.84607155346,-25.4742356128,5.53854202767));
#90909=CARTESIAN_POINT('Origin',(2.84607155346,-25.7742356128,5.53854202767));
#90910=CARTESIAN_POINT('Origin',(2.84607155346,-25.4742356128,5.53854202767));
#90911=CARTESIAN_POINT('Origin',(-3.18408167778E-16,-25.7742356128,0.729452270839));
#90912=CARTESIAN_POINT('Origin',(-7.06664156103,-21.0742356128,-3.23658091327));
#90913=CARTESIAN_POINT('',(-5.92940140951,-21.0742356128,-2.47090756951));
#90914=CARTESIAN_POINT('',(-6.1473421746,-20.7742356128,-2.26474786707));
#90915=CARTESIAN_POINT('Origin',(-6.14734217459869,-21.0742356128,-2.26474786707128));
#90916=CARTESIAN_POINT('',(-7.85893479751,-20.7742356128,-4.07415000213));
#90917=CARTESIAN_POINT('',(-7.00313848605,-20.7742356128,-3.1694489346));
#90918=CARTESIAN_POINT('',(-7.64099403241,-21.0742356128,-4.28030970457));
#90919=CARTESIAN_POINT('Ctrl Pts',(-7.85893479751,-20.7742356128,-4.07415000213));
#90920=CARTESIAN_POINT('Ctrl Pts',(-7.84849506278719,-20.7742356127997,
-4.08402540383888));
#90921=CARTESIAN_POINT('Ctrl Pts',(-7.83801774285179,-20.7752699441924,
-4.093860924025));
#90922=CARTESIAN_POINT('Ctrl Pts',(-7.82761030038593,-20.7773279598862,
-4.1035549090369));
#90923=CARTESIAN_POINT('Ctrl Pts',(-7.82358114562669,-20.778124703539,-4.10730785467891));
#90924=CARTESIAN_POINT('Ctrl Pts',(-7.81941960537616,-20.7791069904586,
-4.11117060042872));
#90925=CARTESIAN_POINT('Ctrl Pts',(-7.81529955037287,-20.780248032667,-4.11498346292577));
#90926=CARTESIAN_POINT('Ctrl Pts',(-7.81108729772222,-20.7814146088567,
-4.11888164878662));
#90927=CARTESIAN_POINT('Ctrl Pts',(-7.80691879648666,-20.7827471087771,
-4.12272732617575));
#90928=CARTESIAN_POINT('Ctrl Pts',(-7.80297123741338,-20.784162024816,-4.12635799991167));
#90929=CARTESIAN_POINT('Ctrl Pts',(-7.80080645801016,-20.7849379425518,
-4.12834900437225));
#90930=CARTESIAN_POINT('Ctrl Pts',(-7.79870792837904,-20.7857376710547,
-4.13027553448078));
#90931=CARTESIAN_POINT('Ctrl Pts',(-7.79670329286778,-20.7865412504096,
-4.13211228414853));
#90932=CARTESIAN_POINT('Ctrl Pts',(-7.78746760851805,-20.7902434722002,
-4.1405744909016));
#90933=CARTESIAN_POINT('Ctrl Pts',(-7.77851371633938,-20.7947647208706,
-4.14898219734389));
#90934=CARTESIAN_POINT('Ctrl Pts',(-7.76991752227422,-20.8000665345526,
-4.15726360072429));
#90935=CARTESIAN_POINT('Ctrl Pts',(-7.76561942524165,-20.8027174413937,
-4.16140430241449));
#90936=CARTESIAN_POINT('Ctrl Pts',(-7.7614106975515,-20.8055632750576,-4.16551348054201));
#90937=CARTESIAN_POINT('Ctrl Pts',(-7.7573004438439,-20.8085979712109,-4.16958252262954));
#90938=CARTESIAN_POINT('Ctrl Pts',(-7.7552453169901,-20.8101153192876,-4.1716170436733));
#90939=CARTESIAN_POINT('Ctrl Pts',(-7.7532148037416,-20.8116798704867,-4.17364153533306));
#90940=CARTESIAN_POINT('Ctrl Pts',(-7.7512100143084,-20.8132907906684,-4.17565494741259));
#90941=CARTESIAN_POINT('Ctrl Pts',(-7.7502076195918,-20.8140962507592,-4.17666165345236));
#90942=CARTESIAN_POINT('Ctrl Pts',(-7.7492116555409,-20.8149133022977,-4.17766558986963));
#90943=CARTESIAN_POINT('Ctrl Pts',(-7.7482222589582,-20.8157418364263,-4.17866662725692));
#90944=CARTESIAN_POINT('Ctrl Pts',(-7.74760225646034,-20.8162610349341,
-4.1792939244312));
#90945=CARTESIAN_POINT('Ctrl Pts',(-7.74662787134155,-20.8170898064891,
-4.18028384051793));
#90946=CARTESIAN_POINT('Ctrl Pts',(-7.74597119137793,-20.8176568705062,
-4.18095156732887));
#90947=CARTESIAN_POINT('Ctrl Pts',(-7.74557994506031,-20.8179947241348,
-4.18134939529746));
#90948=CARTESIAN_POINT('Ctrl Pts',(-7.74530086020065,-20.8182382659002,
-4.18163343684703));
#90949=CARTESIAN_POINT('Ctrl Pts',(-7.74527390710255,-20.8182617746731,
-4.181660914165));
#90950=CARTESIAN_POINT('Ctrl Pts',(-7.74515661698443,-20.8183640763354,
-4.18178048549805));
#90951=CARTESIAN_POINT('Ctrl Pts',(-7.74445013879524,-20.8189489345674,
-4.18243767221834));
#90952=CARTESIAN_POINT('Ctrl Pts',(-7.74316657846176,-20.8200431347351,
-4.18362102280022));
#90953=CARTESIAN_POINT('Ctrl Pts',(-7.74287007718748,-20.8202958939826,
-4.18389437571265));
#90954=CARTESIAN_POINT('Ctrl Pts',(-7.74254286865722,-20.8205760166097,
-4.18419572351062));
#90955=CARTESIAN_POINT('Ctrl Pts',(-7.74218526120033,-20.8208841621755,
-4.18452477453189));
#90956=CARTESIAN_POINT('Ctrl Pts',(-7.74123241232193,-20.8217052193183,
-4.18540153448337));
#90957=CARTESIAN_POINT('Ctrl Pts',(-7.74006349915141,-20.8227248080896,
-4.18647520710011));
#90958=CARTESIAN_POINT('Ctrl Pts',(-7.738686614958,-20.823959517673,-4.18773813660473));
#90959=CARTESIAN_POINT('Ctrl Pts',(-7.73783905626572,-20.8247195589639,
-4.18851554902947));
#90960=CARTESIAN_POINT('Ctrl Pts',(-7.7366212791383,-20.8258278773245,-4.18963152051371));
#90961=CARTESIAN_POINT('Ctrl Pts',(-7.73557557589417,-20.8267999372688,
-4.19058935247806));
#90962=CARTESIAN_POINT('Ctrl Pts',(-7.734922503253,-20.8274070174885,-4.19118754690298));
#90963=CARTESIAN_POINT('Ctrl Pts',(-7.73433596497018,-20.8279597364692,
-4.19172461049083));
#90964=CARTESIAN_POINT('Ctrl Pts',(-7.73394368876629,-20.8283313289077,
-4.19208368551059));
#90965=CARTESIAN_POINT('Ctrl Pts',(-7.73141359108293,-20.8307280207245,
-4.19439964265158));
#90966=CARTESIAN_POINT('Ctrl Pts',(-7.72923493859774,-20.8328997589094,
-4.19640894337873));
#90967=CARTESIAN_POINT('Ctrl Pts',(-7.72719909536861,-20.8350073074348,
-4.19830970528371));
#90968=CARTESIAN_POINT('Ctrl Pts',(-7.72595070836115,-20.8362996644096,
-4.1994752598964));
#90969=CARTESIAN_POINT('Ctrl Pts',(-7.72475647671546,-20.8375688873218,
-4.20059957015176));
#90970=CARTESIAN_POINT('Ctrl Pts',(-7.72357219194332,-20.8388597509998,
-4.20172462996783));
#90971=CARTESIAN_POINT('Ctrl Pts',(-7.72045660051683,-20.8422557279664,
-4.20468441362771));
#90972=CARTESIAN_POINT('Ctrl Pts',(-7.71733482311445,-20.8458756638456,
-4.20768719738774));
#90973=CARTESIAN_POINT('Ctrl Pts',(-7.71434994951472,-20.8495600603431,
-4.21059110535395));
#90974=CARTESIAN_POINT('Ctrl Pts',(-7.71136507591499,-20.8532444568406,
-4.21349501332017));
#90975=CARTESIAN_POINT('Ctrl Pts',(-7.70851723702915,-20.8569927769074,
-4.21629992165792));
#90976=CARTESIAN_POINT('Ctrl Pts',(-7.70592253659978,-20.8606057200984,
-4.21888948174501));
#90977=CARTESIAN_POINT('Ctrl Pts',(-7.70351882668188,-20.8639527220423,
-4.22128842969056));
#90978=CARTESIAN_POINT('Ctrl Pts',(-7.70102646930738,-20.867518906612,-4.22367269782641));
#90979=CARTESIAN_POINT('Ctrl Pts',(-7.69859503733839,-20.8711137133317,
-4.22591514901058));
#90980=CARTESIAN_POINT('Ctrl Pts',(-7.69610053773627,-20.8748017638493,
-4.22821576595484));
#90981=CARTESIAN_POINT('Ctrl Pts',(-7.69367034678098,-20.8785195625902,
-4.23036694169355));
#90982=CARTESIAN_POINT('Ctrl Pts',(-7.6914354950889,-20.8820242700916,-4.23226022490153));
#90983=CARTESIAN_POINT('Ctrl Pts',(-7.69114582996405,-20.8824785246354,
-4.23250561841858));
#90984=CARTESIAN_POINT('Ctrl Pts',(-7.6908594050254,-20.8829291561293,-4.23274671865086));
#90985=CARTESIAN_POINT('Ctrl Pts',(-7.69057646979513,-20.8833755998666,
-4.23298332330633));
#90986=CARTESIAN_POINT('Ctrl Pts',(-7.68827966874672,-20.8869997241689,
-4.23490402374441));
#90987=CARTESIAN_POINT('Ctrl Pts',(-7.68612525160318,-20.8906940503882,
-4.23685135783739));
#90988=CARTESIAN_POINT('Ctrl Pts',(-7.68411554461339,-20.8944545039745,
-4.23882312508471));
#90989=CARTESIAN_POINT('Ctrl Pts',(-7.6831106911185,-20.8963347307677,-4.23980900870837));
#90990=CARTESIAN_POINT('Ctrl Pts',(-7.68214201293391,-20.8982314871563,
-4.2408010027283));
#90991=CARTESIAN_POINT('Ctrl Pts',(-7.68120978772197,-20.9001442498646,
-4.24179884449155));
#90992=CARTESIAN_POINT('Ctrl Pts',(-7.68072489377046,-20.9011391672474,
-4.24231786868159));
#90993=CARTESIAN_POINT('Ctrl Pts',(-7.68003169248704,-20.9026139354804,
-4.24309349704736));
#90994=CARTESIAN_POINT('Ctrl Pts',(-7.67947389717516,-20.9038295405041,
-4.24372468740508));
#90995=CARTESIAN_POINT('Ctrl Pts',(-7.67895931191554,-20.9049509777292,
-4.24430698210563));
#90996=CARTESIAN_POINT('Ctrl Pts',(-7.67855809536675,-20.9058500061099,
-4.2447681200575));
#90997=CARTESIAN_POINT('Ctrl Pts',(-7.67852273949611,-20.9059300251565,
-4.2448096590329));
#90998=CARTESIAN_POINT('Ctrl Pts',(-7.67842273446044,-20.9061563611928,
-4.24492715314753));
#90999=CARTESIAN_POINT('Ctrl Pts',(-7.67792313080382,-20.9071520128035,
-4.24538789360321));
#91000=CARTESIAN_POINT('Ctrl Pts',(-7.67704431333244,-20.9089356457351,
-4.24617259752016));
#91001=CARTESIAN_POINT('Ctrl Pts',(-7.67662816010833,-20.9097802632117,
-4.24654418442602));
#91002=CARTESIAN_POINT('Ctrl Pts',(-7.6761274306967,-20.9108019927213,-4.24698798304712));
#91003=CARTESIAN_POINT('Ctrl Pts',(-7.67554682098165,-20.9120049371452,
-4.24749955134125));
#91004=CARTESIAN_POINT('Ctrl Pts',(-7.6746434607252,-20.9138765768287,-4.2482954912875));
#91005=CARTESIAN_POINT('Ctrl Pts',(-7.67354621288957,-20.9161866189024,
-4.24925597389064));
#91006=CARTESIAN_POINT('Ctrl Pts',(-7.6722810160251,-20.9189561339372,-4.25035646274137));
#91007=CARTESIAN_POINT('Ctrl Pts',(-7.67164475994857,-20.9203488980353,
-4.25090988864534));
#91008=CARTESIAN_POINT('Ctrl Pts',(-7.67077313411016,-20.9222878700344,
-4.25166542252786));
#91009=CARTESIAN_POINT('Ctrl Pts',(-7.66996638151831,-20.9241313941136,
-4.25236283993768));
#91010=CARTESIAN_POINT('Ctrl Pts',(-7.66916890448114,-20.9259537224649,
-4.25305223886278));
#91011=CARTESIAN_POINT('Ctrl Pts',(-7.66843406290105,-20.927681993207,-4.25368556383537));
#91012=CARTESIAN_POINT('Ctrl Pts',(-7.66801806851435,-20.9286697585403,
-4.25404343038915));
#91013=CARTESIAN_POINT('Ctrl Pts',(-7.66521378196361,-20.9353284470419,
-4.25645586766188));
#91014=CARTESIAN_POINT('Ctrl Pts',(-7.66287302397626,-20.9415795983916,
-4.25855395966484));
#91015=CARTESIAN_POINT('Ctrl Pts',(-7.66088643169644,-20.9474577204314,
-4.26044222711536));
#91016=CARTESIAN_POINT('Ctrl Pts',(-7.66050174766622,-20.9485959608743,
-4.26080787151073));
#91017=CARTESIAN_POINT('Ctrl Pts',(-7.66013042505954,-20.9497203243416,
-4.26116557117456));
#91018=CARTESIAN_POINT('Ctrl Pts',(-7.65977178445987,-20.9508312089874,
-4.2615159765629));
#91019=CARTESIAN_POINT('Ctrl Pts',(-7.65756104553905,-20.9576789443666,
-4.26367595184394));
#91020=CARTESIAN_POINT('Ctrl Pts',(-7.65556299823219,-20.9646428172267,
-4.26568628175605));
#91021=CARTESIAN_POINT('Ctrl Pts',(-7.65378344616355,-20.9717031898789,
-4.2675414763972));
#91022=CARTESIAN_POINT('Ctrl Pts',(-7.65289367012923,-20.975233376205,-4.26846907371778));
#91023=CARTESIAN_POINT('Ctrl Pts',(-7.65205850085302,-20.9787876792683,
-4.26935790335033));
#91024=CARTESIAN_POINT('Ctrl Pts',(-7.65127856258358,-20.9823635907031,
-4.27020737479072));
#91025=CARTESIAN_POINT('Ctrl Pts',(-7.65088859344886,-20.9841515464204,
-4.27063211051092));
#91026=CARTESIAN_POINT('Ctrl Pts',(-7.65051243100888,-20.9859449036594,
-4.27104700768289));
#91027=CARTESIAN_POINT('Ctrl Pts',(-7.65015014678754,-20.9877433462015,
-4.27145199864907));
#91028=CARTESIAN_POINT('Ctrl Pts',(-7.64994370704688,-20.9887681493536,
-4.27168277389431));
#91029=CARTESIAN_POINT('Ctrl Pts',(-7.64962911607452,-20.9903748845687,
-4.27203903130631));
#91030=CARTESIAN_POINT('Ctrl Pts',(-7.64940168679224,-20.9915725880104,
-4.2722981831617));
#91031=CARTESIAN_POINT('Ctrl Pts',(-7.64922999698933,-20.9924767524425,
-4.27249382081456));
#91032=CARTESIAN_POINT('Ctrl Pts',(-7.64910620270052,-20.9931470874676,
-4.2726357998818));
#91033=CARTESIAN_POINT('Ctrl Pts',(-7.64910499597593,-20.9931536117467,
-4.27263718936608));
#91034=CARTESIAN_POINT('Ctrl Pts',(-7.64910091505347,-20.9931756756687,
-4.27264188834849));
#91035=CARTESIAN_POINT('Ctrl Pts',(-7.64890512371104,-20.9940939717512,
-4.27281659316766));
#91036=CARTESIAN_POINT('Ctrl Pts',(-7.64853633164759,-20.9959155521025,
-4.27314360550097));
#91037=CARTESIAN_POINT('Ctrl Pts',(-7.64839811038513,-20.9965982705251,
-4.27326616794748));
#91038=CARTESIAN_POINT('Ctrl Pts',(-7.6482359556156,-20.9974080097675,-4.27340977700282));
#91039=CARTESIAN_POINT('Ctrl Pts',(-7.64805218413761,-20.9983455875219,
-4.27357224110587));
#91040=CARTESIAN_POINT('Ctrl Pts',(-7.64771513545709,-21.000065165274,-4.27387021069376));
#91041=CARTESIAN_POINT('Ctrl Pts',(-7.64730487789276,-21.002214682967,-4.27423207276858));
#91042=CARTESIAN_POINT('Ctrl Pts',(-7.64684216014807,-21.0048007089235,
-4.27463820022418));
#91043=CARTESIAN_POINT('Ctrl Pts',(-7.64659282098928,-21.0061942097002,
-4.27485704525293));
#91044=CARTESIAN_POINT('Ctrl Pts',(-7.64623883424678,-21.0082340176968,
-4.27516695562776));
#91045=CARTESIAN_POINT('Ctrl Pts',(-7.64593356616682,-21.010082740552,-4.27543315195173));
#91046=CARTESIAN_POINT('Ctrl Pts',(-7.645672324926,-21.0116648340767,-4.275660956503));
#91047=CARTESIAN_POINT('Ctrl Pts',(-7.64544537182912,-21.0131064775254,
-4.27585806285514));
#91048=CARTESIAN_POINT('Ctrl Pts',(-7.64532585637403,-21.0138760210362,
-4.27596172879676));
#91049=CARTESIAN_POINT('Ctrl Pts',(-7.64459396626892,-21.0185885603524,
-4.27659655947077));
#91050=CARTESIAN_POINT('Ctrl Pts',(-7.64394117298286,-21.0234810301987,
-4.27719038206959));
#91051=CARTESIAN_POINT('Ctrl Pts',(-7.64340440880833,-21.0282841408939,
-4.27770630625303));
#91052=CARTESIAN_POINT('Ctrl Pts',(-7.6431808694144,-21.0302844317194,-4.27792116667917));
#91053=CARTESIAN_POINT('Ctrl Pts',(-7.64297700046929,-21.0322691066079,
-4.27812294541838));
#91054=CARTESIAN_POINT('Ctrl Pts',(-7.64279355523369,-21.0342183284971,
-4.27831078875905));
#91055=CARTESIAN_POINT('Ctrl Pts',(-7.64154568509503,-21.0474777395748,
-4.27958857662201));
#91056=CARTESIAN_POINT('Ctrl Pts',(-7.6409439068007,-21.060856640496,-4.28025671451936));
#91057=CARTESIAN_POINT('Ctrl Pts',(-7.64099403240862,-21.0742356128,-4.28030970457131));
#91058=CARTESIAN_POINT('',(-6.78519772096,-21.0742356128,-3.37560863704));
#91059=CARTESIAN_POINT('Origin',(-0.00234331738835,-21.0742356128,3.08191746407));
#91060=CARTESIAN_POINT('',(-5.92101866809,-21.0742356128,-2.06782739988));
#91061=CARTESIAN_POINT('Ctrl Pts',(-5.92101866809097,-21.0742356128,-2.06782739988085));
#91062=CARTESIAN_POINT('Ctrl Pts',(-5.92101866809097,-21.0620465312503,
-2.06782739988085));
#91063=CARTESIAN_POINT('Ctrl Pts',(-5.92158831198356,-21.0500039224024,
-2.06829775848026));
#91064=CARTESIAN_POINT('Ctrl Pts',(-5.92269655478147,-21.0380655899987,
-2.0692329656236));
#91065=CARTESIAN_POINT('Ctrl Pts',(-5.92380273941395,-21.0261494287864,
-2.07016643595348));
#91066=CARTESIAN_POINT('Ctrl Pts',(-5.92544565218085,-21.0143360094162,
-2.07156313341593));
#91067=CARTESIAN_POINT('Ctrl Pts',(-5.92763287787142,-21.0025880579166,
-2.07345107416981));
#91068=CARTESIAN_POINT('Ctrl Pts',(-5.9288398742164,-20.9961050806079,-2.07449291342733));
#91069=CARTESIAN_POINT('Ctrl Pts',(-5.93021329816248,-20.9896422204813,
-2.07568493338501));
#91070=CARTESIAN_POINT('Ctrl Pts',(-5.93175919989028,-20.9831957718637,
-2.07703601509382));
#91071=CARTESIAN_POINT('Ctrl Pts',(-5.93467897629011,-20.9710202317257,
-2.07958783091541));
#91072=CARTESIAN_POINT('Ctrl Pts',(-5.93821952912064,-20.9589055336624,
-2.08269623846277));
#91073=CARTESIAN_POINT('Ctrl Pts',(-5.94245564556774,-20.9468902378141,
-2.08640923248926));
#91074=CARTESIAN_POINT('Ctrl Pts',(-5.94340905434637,-20.9441859947455,
-2.08724490382741));
#91075=CARTESIAN_POINT('Ctrl Pts',(-5.94439779365108,-20.9414869503422,
-2.08811128428384));
#91076=CARTESIAN_POINT('Ctrl Pts',(-5.9454228766398,-20.9387938528172,-2.08900905987206));
#91077=CARTESIAN_POINT('Ctrl Pts',(-5.9482127051728,-20.9314644166643,-2.09145241321985));
#91078=CARTESIAN_POINT('Ctrl Pts',(-5.95127145415772,-20.9241793796424,
-2.09412782900737));
#91079=CARTESIAN_POINT('Ctrl Pts',(-5.95461804302441,-20.9169637237184,
-2.0970488446907));
#91080=CARTESIAN_POINT('Ctrl Pts',(-5.95610946992881,-20.9137480244477,
-2.09835061241654));
#91081=CARTESIAN_POINT('Ctrl Pts',(-5.9577600186495,-20.9103349058525,-2.09978982587361));
#91082=CARTESIAN_POINT('Ctrl Pts',(-5.95944053176509,-20.9070148772698,
-2.10125414170714));
#91083=CARTESIAN_POINT('Ctrl Pts',(-5.9611755033533,-20.9035872603059,-2.10276590995446));
#91084=CARTESIAN_POINT('Ctrl Pts',(-5.96294225821851,-20.9002591792144,
-2.10430429923713));
#91085=CARTESIAN_POINT('Ctrl Pts',(-5.96456266631968,-20.897317568035,-2.10571435869351));
#91086=CARTESIAN_POINT('Ctrl Pts',(-5.96489459080275,-20.8967150082419,
-2.10600319534881));
#91087=CARTESIAN_POINT('Ctrl Pts',(-5.9652202685808,-20.8961285551481,-2.10628655506147));
#91088=CARTESIAN_POINT('Ctrl Pts',(-5.96553802050222,-20.895560516182,-2.10656297715136));
#91089=CARTESIAN_POINT('Ctrl Pts',(-5.96943999050983,-20.8885850398452,
-2.10995741989574));
#91090=CARTESIAN_POINT('Ctrl Pts',(-5.97377445859389,-20.8813246189463,
-2.11388641840716));
#91091=CARTESIAN_POINT('Ctrl Pts',(-5.97868787468633,-20.8738973043163,
-2.11839084933764));
#91092=CARTESIAN_POINT('Ctrl Pts',(-5.98341610951698,-20.8667499170259,
-2.12272551320837));
#91093=CARTESIAN_POINT('Ctrl Pts',(-5.98868100137614,-20.8594476500422,
-2.1275935338901));
#91094=CARTESIAN_POINT('Ctrl Pts',(-5.99461331171819,-20.8521424468673,
-2.13303105290131));
#91095=CARTESIAN_POINT('Ctrl Pts',(-6.00021350704609,-20.8452462188665,
-2.13816415734227));
#91096=CARTESIAN_POINT('Ctrl Pts',(-6.00640901896054,-20.8383473719427,
-2.14380526705499));
#91097=CARTESIAN_POINT('Ctrl Pts',(-6.01330255816048,-20.8316182518332,
-2.14997766062494));
#91098=CARTESIAN_POINT('Ctrl Pts',(-6.01774519911283,-20.8272815731396,
-2.15395554885515));
#91099=CARTESIAN_POINT('Ctrl Pts',(-6.02247760495861,-20.8230162934579,
-2.15815395116255));
#91100=CARTESIAN_POINT('Ctrl Pts',(-6.02752376872349,-20.8188791385191,
-2.16257579879535));
#91101=CARTESIAN_POINT('Ctrl Pts',(-6.03497120631767,-20.8127732718332,
-2.16910183239843));
#91102=CARTESIAN_POINT('Ctrl Pts',(-6.04312863302932,-20.806943602497,-2.17609415913291));
#91103=CARTESIAN_POINT('Ctrl Pts',(-6.05196187418653,-20.8016209760895,
-2.18359488576368));
#91104=CARTESIAN_POINT('Ctrl Pts',(-6.06049325274665,-20.7964802423534,
-2.19083928645694));
#91105=CARTESIAN_POINT('Ctrl Pts',(-6.06965539423694,-20.7918131204054,
-2.19855821334899));
#91106=CARTESIAN_POINT('Ctrl Pts',(-6.07938360613618,-20.7878444413393,
-2.20676096030881));
#91107=CARTESIAN_POINT('Ctrl Pts',(-6.08886726552373,-20.7839755288535,
-2.2147575026349));
#91108=CARTESIAN_POINT('Ctrl Pts',(-6.09888915179127,-20.7807710925393,
-2.22321405218668));
#91109=CARTESIAN_POINT('Ctrl Pts',(-6.10935206214159,-20.7784460175651,
-2.23210793494573));
#91110=CARTESIAN_POINT('Ctrl Pts',(-6.11948454120585,-20.7761943712536,
-2.24072093819615));
#91111=CARTESIAN_POINT('Ctrl Pts',(-6.13003068944631,-20.7747681652049,
-2.24974413303381));
#91112=CARTESIAN_POINT('Ctrl Pts',(-6.14086459511848,-20.7743582551055,
-2.25912546437508));
#91113=CARTESIAN_POINT('Ctrl Pts',(-6.14301298428552,-20.7742769689615,
-2.26098580461026));
#91114=CARTESIAN_POINT('Ctrl Pts',(-6.14517256622352,-20.7742356128001,
-2.26286012548388));
#91115=CARTESIAN_POINT('Ctrl Pts',(-6.1473421746,-20.7742356128,-2.26474786707));
#91116=CARTESIAN_POINT('',(-7.75696851341,-21.0742356128,1.89180060423));
#91117=CARTESIAN_POINT('Origin',(-0.00234331738835,-21.0742356128,3.08191746407));
#91118=CARTESIAN_POINT('',(-8.05349668264,-20.7742356128,1.84629187045));
#91119=CARTESIAN_POINT('Origin',(-8.05349668264169,-21.0742356128,1.84629187044922));
#91120=CARTESIAN_POINT('Origin',(-0.00234331738835,-20.7742356128,3.08191746407));
#91121=CARTESIAN_POINT('Origin',(-8.59172680003,-21.0742356128,1.84629187045));
#91122=CARTESIAN_POINT('',(-8.05349668264,-21.0742356128,2.14629187045));
#91123=CARTESIAN_POINT('Ctrl Pts',(-8.05349668264,-21.0742356128,2.14629187045));
#91124=CARTESIAN_POINT('Ctrl Pts',(-8.05349668264,-21.0616661505988,2.14629187045));
#91125=CARTESIAN_POINT('Ctrl Pts',(-8.05351323889987,-21.0492324805558,
2.1455062899062));
#91126=CARTESIAN_POINT('Ctrl Pts',(-8.05353196047696,-21.0369022763782,
2.14395984318408));
#91127=CARTESIAN_POINT('Ctrl Pts',(-8.05355061584828,-21.0246156759339,
2.14241886521572));
#91128=CARTESIAN_POINT('Ctrl Pts',(-8.05357142124933,-21.0124306137542,
2.14012220955366));
#91129=CARTESIAN_POINT('Ctrl Pts',(-8.05358013787175,-21.0003207612194,
2.13704364553627));
#91130=CARTESIAN_POINT('Ctrl Pts',(-8.05358466303609,-20.9940340288004,
2.1354454338193));
#91131=CARTESIAN_POINT('Ctrl Pts',(-8.05358593017351,-20.9877677679401,
2.13363567327742));
#91132=CARTESIAN_POINT('Ctrl Pts',(-8.05358194708828,-20.9815205327896,
2.13160558189524));
#91133=CARTESIAN_POINT('Ctrl Pts',(-8.05357646511694,-20.9729223828324,
2.12881154105794));
#91134=CARTESIAN_POINT('Ctrl Pts',(-8.0535671003131,-20.9644930322314,2.12564711986058));
#91135=CARTESIAN_POINT('Ctrl Pts',(-8.05355653390898,-20.9561289564286,
2.12206499771362));
#91136=CARTESIAN_POINT('Ctrl Pts',(-8.05354614300608,-20.94790380257,2.1185423723222));
#91137=CARTESIAN_POINT('Ctrl Pts',(-8.05353459008704,-20.9397410562187,
2.11461550731705));
#91138=CARTESIAN_POINT('Ctrl Pts',(-8.05352442499017,-20.9315661832454,
2.11019608388846));
#91139=CARTESIAN_POINT('Ctrl Pts',(-8.05351471672478,-20.9237586987363,
2.1059752745779));
#91140=CARTESIAN_POINT('Ctrl Pts',(-8.05350627434382,-20.9159395752215,
2.10130478889639));
#91141=CARTESIAN_POINT('Ctrl Pts',(-8.05350131912569,-20.908074923903,2.09607302559444));
#91142=CARTESIAN_POINT('Ctrl Pts',(-8.05349811070886,-20.9029827001034,
2.09268555061026));
#91143=CARTESIAN_POINT('Ctrl Pts',(-8.05349636422765,-20.8978720151952,
2.08906207723948));
#91144=CARTESIAN_POINT('Ctrl Pts',(-8.05349668264,-20.8927430724885,2.08516517957281));
#91145=CARTESIAN_POINT('Ctrl Pts',(-8.05349728076221,-20.8831086015271,
2.07784504566683));
#91146=CARTESIAN_POINT('Ctrl Pts',(-8.05347983282803,-20.8735442883448,
2.06966063490902));
#91147=CARTESIAN_POINT('Ctrl Pts',(-8.05346690182125,-20.8642170348392,
2.06051651168285));
#91148=CARTESIAN_POINT('Ctrl Pts',(-8.05345984899157,-20.8591297642566,
2.05552912401669));
#91149=CARTESIAN_POINT('Ctrl Pts',(-8.05345413987088,-20.8541138227069,
2.05025646025968));
#91150=CARTESIAN_POINT('Ctrl Pts',(-8.05345343537466,-20.8492024318137,
2.04468558873566));
#91151=CARTESIAN_POINT('Ctrl Pts',(-8.05345243729745,-20.8422443428754,
2.03679319727835));
#91152=CARTESIAN_POINT('Ctrl Pts',(-8.05345966742439,-20.8354966553014,
2.02830258366614));
#91153=CARTESIAN_POINT('Ctrl Pts',(-8.05347058591999,-20.8290738365618,
2.0191956109293));
#91154=CARTESIAN_POINT('Ctrl Pts',(-8.05347604516779,-20.825862427192,2.01464212456088));
#91155=CARTESIAN_POINT('Ctrl Pts',(-8.05348223770851,-20.8227325395361,
2.00993486590606));
#91156=CARTESIAN_POINT('Ctrl Pts',(-8.05348734675697,-20.8197001322682,
2.0050737622086));
#91157=CARTESIAN_POINT('Ctrl Pts',(-8.05348963342434,-20.8183429114868,
2.00289806799087));
#91158=CARTESIAN_POINT('Ctrl Pts',(-8.05349171593753,-20.81682014971,2.00038693537785));
#91159=CARTESIAN_POINT('Ctrl Pts',(-8.05349333125322,-20.8153894858194,
1.99794503575545));
#91160=CARTESIAN_POINT('Ctrl Pts',(-8.0534950936214,-20.8138285794693,1.99528083443472));
#91161=CARTESIAN_POINT('Ctrl Pts',(-8.05349629985619,-20.8123773614345,
1.99269936191406));
#91162=CARTESIAN_POINT('Ctrl Pts',(-8.05349660833629,-20.8113116696654,
1.99075986042202));
#91163=CARTESIAN_POINT('Ctrl Pts',(-8.05349664883622,-20.8111717564355,
1.9905052258963));
#91164=CARTESIAN_POINT('Ctrl Pts',(-8.05349667386182,-20.8110384236002,
1.99026169002046));
#91165=CARTESIAN_POINT('Ctrl Pts',(-8.05349668264,-20.8109122481073,1.99003054167983));
#91166=CARTESIAN_POINT('Ctrl Pts',(-8.05349692473061,-20.8074324937806,
1.98365577412581));
#91167=CARTESIAN_POINT('Ctrl Pts',(-8.05349705981208,-20.8037803081111,
1.97642146393256));
#91168=CARTESIAN_POINT('Ctrl Pts',(-8.05349712335962,-20.8001488318908,
1.96826086868649));
#91169=CARTESIAN_POINT('Ctrl Pts',(-8.05349718345239,-20.7967147809143,
1.96054392428884));
#91170=CARTESIAN_POINT('Ctrl Pts',(-8.05349717957771,-20.7932995376926,
1.95199778390212));
#91171=CARTESIAN_POINT('Ctrl Pts',(-8.0534971417338,-20.7901088517368,1.94258301047705));
#91172=CARTESIAN_POINT('Ctrl Pts',(-8.05349710520334,-20.7870289057441,
1.93349499802954));
#91173=CARTESIAN_POINT('Ctrl Pts',(-8.0534970370207,-20.784158518396,1.92359673510507));
#91174=CARTESIAN_POINT('Ctrl Pts',(-8.05349696416779,-20.781719287374,1.91288165464604));
#91175=CARTESIAN_POINT('Ctrl Pts',(-8.0534968953135,-20.7794139366638,1.9027546850711));
#91176=CARTESIAN_POINT('Ctrl Pts',(-8.05349682228755,-20.7774942735949,
1.89189752857833));
#91177=CARTESIAN_POINT('Ctrl Pts',(-8.05349676786842,-20.7761741033937,
1.88034090289527));
#91178=CARTESIAN_POINT('Ctrl Pts',(-8.05349671718391,-20.7749445324848,
1.86957737351649));
#91179=CARTESIAN_POINT('Ctrl Pts',(-8.05349668264,-20.7742356128,1.85820684501475));
#91180=CARTESIAN_POINT('Ctrl Pts',(-8.05349668264,-20.7742356128,1.84629187045));
#91181=CARTESIAN_POINT('',(-11.0596214465,-21.0742356128,2.14629187045));
#91182=CARTESIAN_POINT('',(-9.55655906459,-21.0742356128,2.14629187045));
#91183=CARTESIAN_POINT('',(-11.0596214465,-20.7742356128,1.84629187045));
#91184=CARTESIAN_POINT('Ctrl Pts',(-11.0596214465,-20.7742356128,1.84629187045));
#91185=CARTESIAN_POINT('Ctrl Pts',(-11.0596214465,-20.7742356128,1.85761625667422));
#91186=CARTESIAN_POINT('Ctrl Pts',(-11.059642963506,-20.7748745883609,1.86818502268977));
#91187=CARTESIAN_POINT('Ctrl Pts',(-11.0596632830869,-20.7759101728573,
1.87794517806547));
#91188=CARTESIAN_POINT('Ctrl Pts',(-11.0596805287041,-20.7767890932354,
1.88622880869402));
#91189=CARTESIAN_POINT('Ctrl Pts',(-11.0596969117872,-20.777953966298,1.89393130523717));
#91190=CARTESIAN_POINT('Ctrl Pts',(-11.0596985458026,-20.7792742044041,
1.90104374308561));
#91191=CARTESIAN_POINT('Ctrl Pts',(-11.0597003254466,-20.7807121061485,
1.90879006304244));
#91192=CARTESIAN_POINT('Ctrl Pts',(-11.059690915806,-20.7823340171186,1.91583863354018));
#91193=CARTESIAN_POINT('Ctrl Pts',(-11.0596791895441,-20.7839989800967,
1.92220430050639));
#91194=CARTESIAN_POINT('Ctrl Pts',(-11.0596733264131,-20.7848314615858,
1.92538713398949));
#91195=CARTESIAN_POINT('Ctrl Pts',(-11.0596670744678,-20.785675165982,1.92839953863267));
#91196=CARTESIAN_POINT('Ctrl Pts',(-11.0596624003455,-20.7865152326722,
1.93124469770798));
#91197=CARTESIAN_POINT('Ctrl Pts',(-11.0596597538015,-20.7869908884821,
1.93285566081342));
#91198=CARTESIAN_POINT('Ctrl Pts',(-11.0596574856804,-20.7873370464992,
1.93399191036223));
#91199=CARTESIAN_POINT('Ctrl Pts',(-11.0596562333712,-20.7877657305251,
1.93537052417471));
#91200=CARTESIAN_POINT('Ctrl Pts',(-11.0596552739482,-20.788094155239,1.9364267119953));
#91201=CARTESIAN_POINT('Ctrl Pts',(-11.0596549107504,-20.7884712476927,
1.93762513492828));
#91202=CARTESIAN_POINT('Ctrl Pts',(-11.0596554303936,-20.7890114782493,
1.93928215526398));
#91203=CARTESIAN_POINT('Ctrl Pts',(-11.059658976655,-20.7926982362845,1.95059035129758));
#91204=CARTESIAN_POINT('Ctrl Pts',(-11.0596541534426,-20.7968715153589,
1.9611181067061));
#91205=CARTESIAN_POINT('Ctrl Pts',(-11.0596471209352,-20.8013436976379,
1.97091130167637));
#91206=CARTESIAN_POINT('Ctrl Pts',(-11.0596396610574,-20.8060876576077,
1.98129963605465));
#91207=CARTESIAN_POINT('Ctrl Pts',(-11.0596297152047,-20.8111677980098,
1.99086227742229));
#91208=CARTESIAN_POINT('Ctrl Pts',(-11.059624636264,-20.8164139319331,1.99968020401865));
#91209=CARTESIAN_POINT('Ctrl Pts',(-11.0596215642414,-20.819587082183,2.0050137708685));
#91210=CARTESIAN_POINT('Ctrl Pts',(-11.0596202727764,-20.822822013273,2.01007530969174));
#91211=CARTESIAN_POINT('Ctrl Pts',(-11.0596223889592,-20.8260898529763,
2.01488511432867));
#91212=CARTESIAN_POINT('Ctrl Pts',(-11.0596274412372,-20.8338916523628,
2.02636827576629));
#91213=CARTESIAN_POINT('Ctrl Pts',(-11.059647255111,-20.8421947911733,2.03687551725596));
#91214=CARTESIAN_POINT('Ctrl Pts',(-11.0596612382408,-20.8507666748555,
2.04644589557552));
#91215=CARTESIAN_POINT('Ctrl Pts',(-11.0596719237107,-20.8573170399532,
2.05375927900922));
#91216=CARTESIAN_POINT('Ctrl Pts',(-11.0596792042956,-20.8640250667126,
2.06052666622852));
#91217=CARTESIAN_POINT('Ctrl Pts',(-11.0596738908863,-20.8708019000932,
2.0667793406934));
#91218=CARTESIAN_POINT('Ctrl Pts',(-11.0596677575872,-20.8786244381344,
2.07399683906081));
#91219=CARTESIAN_POINT('Ctrl Pts',(-11.0596503856799,-20.8865395212126,
2.08053044995971));
#91220=CARTESIAN_POINT('Ctrl Pts',(-11.0596353586119,-20.8944454799549,
2.08644912753701));
#91221=CARTESIAN_POINT('Ctrl Pts',(-11.0596291584308,-20.8977074852617,
2.08889117894348));
#91222=CARTESIAN_POINT('Ctrl Pts',(-11.0596238733896,-20.9011756458164,
2.09137844049239));
#91223=CARTESIAN_POINT('Ctrl Pts',(-11.0596207646266,-20.9045941052338,
2.09372218167052));
#91224=CARTESIAN_POINT('Ctrl Pts',(-11.0596174417513,-20.9082480068714,
2.09622734516174));
#91225=CARTESIAN_POINT('Ctrl Pts',(-11.0596166052546,-20.9118447609928,
2.09856830978726));
#91226=CARTESIAN_POINT('Ctrl Pts',(-11.0596197952121,-20.9150376476084,
2.10056732714775));
#91227=CARTESIAN_POINT('Ctrl Pts',(-11.0596208540094,-20.9160974171127,
2.10123083258726));
#91228=CARTESIAN_POINT('Ctrl Pts',(-11.0596223563935,-20.9171124635461,
2.10185707248893));
#91229=CARTESIAN_POINT('Ctrl Pts',(-11.0596243586796,-20.9180695616067,
2.10244058595469));
#91230=CARTESIAN_POINT('Ctrl Pts',(-11.0596517158804,-20.9311463762198,
2.11041312056716));
#91231=CARTESIAN_POINT('Ctrl Pts',(-11.0598122508444,-20.9446114029323,
2.11725326253638));
#91232=CARTESIAN_POINT('Ctrl Pts',(-11.0599398380114,-20.9583708107472,
2.12301438063896));
#91233=CARTESIAN_POINT('Ctrl Pts',(-11.059985476179,-20.9632925765907,2.12507514333156));
#91234=CARTESIAN_POINT('Ctrl Pts',(-11.0600259384965,-20.9684653521836,
2.12708203867674));
#91235=CARTESIAN_POINT('Ctrl Pts',(-11.0600554539948,-20.9736656141531,
2.12893241137108));
#91236=CARTESIAN_POINT('Ctrl Pts',(-11.060085860925,-20.9790229352646,2.13083866931689));
#91237=CARTESIAN_POINT('Ctrl Pts',(-11.0601046498154,-20.9844089944274,
2.13257846615161));
#91238=CARTESIAN_POINT('Ctrl Pts',(-11.0601055108586,-20.9895605965473,
2.13409413177296));
#91239=CARTESIAN_POINT('Ctrl Pts',(-11.0601061505986,-20.9933881462091,
2.13522024464062));
#91240=CARTESIAN_POINT('Ctrl Pts',(-11.0600968937575,-20.9970858075619,
2.13622396439941));
#91241=CARTESIAN_POINT('Ctrl Pts',(-11.0600751524104,-21.0005418908902,
2.13709977156528));
#91242=CARTESIAN_POINT('Ctrl Pts',(-11.0600142322725,-21.0102259768093,
2.13955381883132));
#91243=CARTESIAN_POINT('Ctrl Pts',(-11.0599332901061,-21.0197415078409,
2.14145488072622));
#91244=CARTESIAN_POINT('Ctrl Pts',(-11.0598566502278,-21.0291627743857,
2.14288660950867));
#91245=CARTESIAN_POINT('Ctrl Pts',(-11.059778127918,-21.0388154464452,2.14435350446906));
#91246=CARTESIAN_POINT('Ctrl Pts',(-11.0597041218377,-21.0483700448158,
2.14532786081222));
#91247=CARTESIAN_POINT('Ctrl Pts',(-11.0596607930529,-21.057924127132,2.14584810129039));
#91248=CARTESIAN_POINT('Ctrl Pts',(-11.0596361636607,-21.0633549565775,
2.14614382171796));
#91249=CARTESIAN_POINT('Ctrl Pts',(-11.0596214465,-21.0687858631891,2.14629187045));
#91250=CARTESIAN_POINT('Ctrl Pts',(-11.0596214465,-21.0742356128,2.14629187045));
#91251=CARTESIAN_POINT('',(-9.55655906459,-20.7742356128,1.84629187045));
#91252=CARTESIAN_POINT('Origin',(2.84607155346,-21.0742356128,5.53854202767));
#91253=CARTESIAN_POINT('',(-8.08214906615,-21.0742356128,-4.27458799822));
#91254=CARTESIAN_POINT('Ctrl Pts',(-7.85893479751,-20.7742356128,-4.07415000213));
#91255=CARTESIAN_POINT('Ctrl Pts',(-7.86867005783962,-20.774235612798,-4.08289189880141));
#91256=CARTESIAN_POINT('Ctrl Pts',(-7.87794459209518,-20.7750912521639,
-4.0912908295309));
#91257=CARTESIAN_POINT('Ctrl Pts',(-7.88671096678694,-20.7765812278629,
-4.09925710494256));
#91258=CARTESIAN_POINT('Ctrl Pts',(-7.89592146767705,-20.7781466894116,
-4.10762697154646));
#91259=CARTESIAN_POINT('Ctrl Pts',(-7.90457129324857,-20.7804115075564,
-4.11551947771955));
#91260=CARTESIAN_POINT('Ctrl Pts',(-7.91264842931803,-20.7831317256994,
-4.12286860916846));
#91261=CARTESIAN_POINT('Ctrl Pts',(-7.91818651298307,-20.7849968416928,
-4.12790753688732));
#91262=CARTESIAN_POINT('Ctrl Pts',(-7.92345628776262,-20.7870763568834,
-4.13269182999611));
#91263=CARTESIAN_POINT('Ctrl Pts',(-7.92846334501722,-20.7892977054482,
-4.1372085828105));
#91264=CARTESIAN_POINT('Ctrl Pts',(-7.93615415887783,-20.7927096852726,
-4.14414629160502));
#91265=CARTESIAN_POINT('Ctrl Pts',(-7.94321492459647,-20.7964557545231,
-4.15047134353813));
#91266=CARTESIAN_POINT('Ctrl Pts',(-7.94965916493774,-20.8003139394615,
-4.15622441062207));
#91267=CARTESIAN_POINT('Ctrl Pts',(-7.9512841305117,-20.8012868109515,-4.15767509145658));
#91268=CARTESIAN_POINT('Ctrl Pts',(-7.95287000622591,-20.8022670254849,
-4.15908950458363));
#91269=CARTESIAN_POINT('Ctrl Pts',(-7.95441720769774,-20.8032514563752,
-4.16046848329981));
#91270=CARTESIAN_POINT('Ctrl Pts',(-7.95825873131789,-20.8056956852532,
-4.16389232913134));
#91271=CARTESIAN_POINT('Ctrl Pts',(-7.96186133808005,-20.8081655857621,
-4.16709855052187));
#91272=CARTESIAN_POINT('Ctrl Pts',(-7.96523109252315,-20.8106188105178,
-4.17010529982328));
#91273=CARTESIAN_POINT('Ctrl Pts',(-7.9669159697447,-20.8118454228956,-4.17160867447399));
#91274=CARTESIAN_POINT('Ctrl Pts',(-7.96827678400785,-20.8128676208252,
-4.17282213945004));
#91275=CARTESIAN_POINT('Ctrl Pts',(-7.96971581084777,-20.813975090629,-4.1741107736294));
#91276=CARTESIAN_POINT('Ctrl Pts',(-7.97102627021838,-20.8149836153776,
-4.17528427692258));
#91277=CARTESIAN_POINT('Ctrl Pts',(-7.97240169868035,-20.8160629485353,
-4.17652021395837));
#91278=CARTESIAN_POINT('Ctrl Pts',(-7.97412962130567,-20.8174693670533,
-4.1780796833385));
#91279=CARTESIAN_POINT('Ctrl Pts',(-7.97429914555349,-20.8176073489502,
-4.1782326808569));
#91280=CARTESIAN_POINT('Ctrl Pts',(-7.97447204595328,-20.8177485150464,
-4.17838877747379));
#91281=CARTESIAN_POINT('Ctrl Pts',(-7.97464858184815,-20.8178931330592,
-4.17854820882513));
#91282=CARTESIAN_POINT('Ctrl Pts',(-7.98332468641013,-20.8250005884708,
-4.18638368656571));
#91283=CARTESIAN_POINT('Ctrl Pts',(-7.99131018115002,-20.8326239943172,
-4.19356432373331));
#91284=CARTESIAN_POINT('Ctrl Pts',(-7.99863186617331,-20.8405310579859,
-4.20011451649722));
#91285=CARTESIAN_POINT('Ctrl Pts',(-8.00464991219655,-20.8470302549488,
-4.20549843582576));
#91286=CARTESIAN_POINT('Ctrl Pts',(-8.01022032314814,-20.8537217587971,
-4.21045717841229));
#91287=CARTESIAN_POINT('Ctrl Pts',(-8.01537097958385,-20.8604961122412,
-4.21501600509421));
#91288=CARTESIAN_POINT('Ctrl Pts',(-8.0192422021813,-20.8655877021119,-4.21844240968732));
#91289=CARTESIAN_POINT('Ctrl Pts',(-8.02297330630799,-20.8708622671668,
-4.22173188947109));
#91290=CARTESIAN_POINT('Ctrl Pts',(-8.02646659080307,-20.8761580355519,
-4.22480987956169));
#91291=CARTESIAN_POINT('Ctrl Pts',(-8.03018669861847,-20.8817976647851,
-4.22808772738883));
#91292=CARTESIAN_POINT('Ctrl Pts',(-8.03363674440835,-20.8874607571514,
-4.23112541073459));
#91293=CARTESIAN_POINT('Ctrl Pts',(-8.03673703076693,-20.8929161654381,
-4.23386733271056));
#91294=CARTESIAN_POINT('Ctrl Pts',(-8.03931139776239,-20.8974461415163,
-4.23614412672976));
#91295=CARTESIAN_POINT('Ctrl Pts',(-8.04164554775715,-20.9018319174455,
-4.23821784132976));
#91296=CARTESIAN_POINT('Ctrl Pts',(-8.04371227855687,-20.9059300251781,
-4.24007321236907));
#91297=CARTESIAN_POINT('Ctrl Pts',(-8.04883156724945,-20.9160810310949,
-4.24466896329285));
#91298=CARTESIAN_POINT('Ctrl Pts',(-8.05332097862139,-20.9263165631395,
-4.24869954377612));
#91299=CARTESIAN_POINT('Ctrl Pts',(-8.05726683881383,-20.9365856343797,
-4.25224235137789));
#91300=CARTESIAN_POINT('Ctrl Pts',(-8.06136720484735,-20.9472568059001,
-4.25592388271582));
#91301=CARTESIAN_POINT('Ctrl Pts',(-8.06488109853223,-20.9579649933757,
-4.25907912474788));
#91302=CARTESIAN_POINT('Ctrl Pts',(-8.0678827527923,-20.968700015227,-4.26177459981986));
#91303=CARTESIAN_POINT('Ctrl Pts',(-8.07101172145835,-20.979890360314,-4.26458440278501));
#91304=CARTESIAN_POINT('Ctrl Pts',(-8.07358451687653,-20.9911107636718,
-4.26689500558006));
#91305=CARTESIAN_POINT('Ctrl Pts',(-8.0756538546644,-21.0023865074548,-4.26875358985655));
#91306=CARTESIAN_POINT('Ctrl Pts',(-8.07781579187343,-21.0141668220013,
-4.27069534268541));
#91307=CARTESIAN_POINT('Ctrl Pts',(-8.07942866747217,-21.026008635305,-4.27214413248312));
#91308=CARTESIAN_POINT('Ctrl Pts',(-8.08051195256235,-21.0379645200357,
-4.27311726631233));
#91309=CARTESIAN_POINT('Ctrl Pts',(-8.08159523765254,-21.0499204047663,
-4.27409040014153));
#91310=CARTESIAN_POINT('Ctrl Pts',(-8.08214906618287,-21.0619916709181,
-4.27458799824952));
#91311=CARTESIAN_POINT('Ctrl Pts',(-8.08214906618287,-21.0742356128,-4.27458799824952));
#91312=CARTESIAN_POINT('Origin',(2.84607155346,-20.7742356128,5.53854202767));
#91313=CARTESIAN_POINT('',(-11.3495744826,-21.0742356128,1.76930332028));
#91314=CARTESIAN_POINT('Origin',(-11.059621446593,-21.0742356128,1.8462918704235));
#91315=CARTESIAN_POINT('Origin',(2.84607155346,-21.0742356128,5.53854202767));
#91316=CARTESIAN_POINT('Origin',(-7.85893479751,-21.0742356128,-4.07415000213));
#91317=CARTESIAN_POINT('Origin',(-7.85893479751,-21.0742356128,-4.07415000213));
#91318=CARTESIAN_POINT('Origin',(-7.86219292935,-23.1742356128,-4.51414908377));
#91319=CARTESIAN_POINT('',(-5.92940140951,-22.8742356128,-2.47090756951));
#91320=CARTESIAN_POINT('',(-5.92940140951,-22.1242356128,-2.47090756951));
#91321=CARTESIAN_POINT('',(-7.64099403241,-22.8742356128,-4.28030970457));
#91322=CARTESIAN_POINT('',(-7.64099403241,-22.1242356128,-4.28030970457));
#91323=CARTESIAN_POINT('',(-6.88866980649,-22.8742356128,-3.48499366825));
#91324=CARTESIAN_POINT('Origin',(-6.1473421746,-21.0742356128,-2.26474786707));
#91325=CARTESIAN_POINT('Origin',(-6.1473421746,-21.0742356128,-2.26474786707));
#91326=CARTESIAN_POINT('Origin',(-0.00234331738835,-21.2742356128,3.08191746407));
#91327=CARTESIAN_POINT('',(-7.75696851341,-22.8742356128,1.89180060423));
#91328=CARTESIAN_POINT('',(-7.75696851341,-22.1242356128,1.89180060423));
#91329=CARTESIAN_POINT('',(-5.92101866809,-22.8742356128,-2.06782739988));
#91330=CARTESIAN_POINT('',(-5.92101866809,-22.1242356128,-2.06782739988));
#91331=CARTESIAN_POINT('Origin',(-0.00234331738837,-22.8742356128,3.08191746407));
#91332=CARTESIAN_POINT('Origin',(-8.05349668264,-21.0742356128,1.84629187045));
#91333=CARTESIAN_POINT('Origin',(-8.05349668264,-21.0742356128,1.84629187045));
#91334=CARTESIAN_POINT('Origin',(-11.4443506127,-23.1742356128,2.14629187045));
#91335=CARTESIAN_POINT('',(-8.05349668264,-22.8742356128,2.14629187045));
#91336=CARTESIAN_POINT('',(-11.0596214465,-22.8742356128,2.14629187045));
#91337=CARTESIAN_POINT('',(-6.6707290414,-22.8742356128,2.14629187045));
#91338=CARTESIAN_POINT('',(-11.0596214465,-22.1242356128,2.14629187045));
#91339=CARTESIAN_POINT('',(-8.05349668264,-22.1242356128,2.14629187045));
#91340=CARTESIAN_POINT('Origin',(-11.0596214465,-21.0742356128,1.84629187045));
#91341=CARTESIAN_POINT('Origin',(-11.0596214465,-21.0742356128,1.84629187045));
#91342=CARTESIAN_POINT('Origin',(2.84607155346,-21.2742356128,5.53854202767));
#91343=CARTESIAN_POINT('',(-11.3495744826,-22.8742356128,1.76930332028));
#91344=CARTESIAN_POINT('',(-8.08214906615,-22.8742356128,-4.27458799822));
#91345=CARTESIAN_POINT('Origin',(2.84607155346,-22.8742356128,5.53854202767));
#91346=CARTESIAN_POINT('',(-8.08214906615,-22.1242356128,-4.27458799822));
#91347=CARTESIAN_POINT('',(-11.3495744826,-22.1242356128,1.76930332028));
#91348=CARTESIAN_POINT('Origin',(-7.85893479751,-22.1242356128,-4.07415000213));
#91349=CARTESIAN_POINT('Origin',(-7.85893479751,-22.8742356128,-4.07415000213));
#91350=CARTESIAN_POINT('Origin',(-6.6707290414,-22.8742356128,-3.69115337069));
#91351=CARTESIAN_POINT('',(-7.42305326732,-23.1742356128,-4.48646940701));
#91352=CARTESIAN_POINT('Origin',(-7.42305326732,-22.8742356128,-4.48646940701));
#91353=CARTESIAN_POINT('',(-5.71146064442,-23.1742356128,-2.67706727196));
#91354=CARTESIAN_POINT('',(-6.56725695587,-23.1742356128,-3.58176833949));
#91355=CARTESIAN_POINT('Origin',(-5.71146064442,-22.8742356128,-2.67706727196));
#91356=CARTESIAN_POINT('Origin',(-6.1473421746,-22.1242356128,-2.26474786707));
#91357=CARTESIAN_POINT('Origin',(-6.1473421746,-22.8742356128,-2.26474786707));
#91358=CARTESIAN_POINT('Origin',(-0.00234331738837,-22.8742356128,3.08191746407));
#91359=CARTESIAN_POINT('',(-5.69469516158,-23.1742356128,-1.87090693268));
#91360=CARTESIAN_POINT('Origin',(-5.69469516158,-22.8742356128,-1.87090693268));
#91361=CARTESIAN_POINT('',(-7.46044034417,-23.1742356128,1.93730933801));
#91362=CARTESIAN_POINT('Origin',(-0.00234331738835,-23.1742356128,3.08191746407));
#91363=CARTESIAN_POINT('Origin',(-7.46044034417,-22.8742356128,1.93730933801));
#91364=CARTESIAN_POINT('Origin',(-8.05349668264,-22.1242356128,1.84629187045));
#91365=CARTESIAN_POINT('Origin',(-8.05349668264,-22.8742356128,1.84629187045));
#91366=CARTESIAN_POINT('Origin',(-6.6707290414,-22.8742356128,2.44629187045));
#91367=CARTESIAN_POINT('',(-8.05349668264,-23.1742356128,2.44629187045));
#91368=CARTESIAN_POINT('Origin',(-8.05349668264,-22.8742356128,2.44629187045));
#91369=CARTESIAN_POINT('',(-11.0596214465,-23.1742356128,2.44629187045));
#91370=CARTESIAN_POINT('',(-9.55655906459,-23.1742356128,2.44629187045));
#91371=CARTESIAN_POINT('Origin',(-11.0596214465,-22.8742356128,2.44629187045));
#91372=CARTESIAN_POINT('Origin',(-11.0596214465,-22.1242356128,1.84629187045));
#91373=CARTESIAN_POINT('Origin',(-11.0596214465,-22.8742356128,1.84629187045));
#91374=CARTESIAN_POINT('Origin',(2.84607155346,-22.8742356128,5.53854202767));
#91375=CARTESIAN_POINT('',(-11.6395275187,-23.1742356128,1.69231477012));
#91376=CARTESIAN_POINT('Origin',(-11.6395275187,-22.8742356128,1.69231477012));
#91377=CARTESIAN_POINT('',(-8.30536333479,-23.1742356128,-4.4750259943));
#91378=CARTESIAN_POINT('Origin',(2.84607155346,-23.1742356128,5.53854202767));
#91379=CARTESIAN_POINT('Origin',(-8.30536333479,-22.8742356128,-4.4750259943));
#91380=CARTESIAN_POINT('Origin',(-7.85893479751,-22.8742356128,-4.07415000213));
#91381=CARTESIAN_POINT('Origin',(-7.85893479751,-23.1742356128,-4.07415000213));
#91382=CARTESIAN_POINT('Origin',(-3.41821282746,-21.0742356128,8.06979469543));
#91383=CARTESIAN_POINT('',(-3.62188020465,-21.0742356128,7.84952304616));
#91384=CARTESIAN_POINT('',(-3.41821282746,-20.7742356128,8.06979469543));
#91385=CARTESIAN_POINT('Origin',(-3.41821282746,-21.0742356128,8.06979469543));
#91386=CARTESIAN_POINT('',(-3.58772315463,-21.0742356128,8.31731489457));
#91387=CARTESIAN_POINT('Origin',(-3.41821282746,-21.0742356128,8.06979469543));
#91388=CARTESIAN_POINT('Origin',(-3.41821282746,-21.0742356128,8.06979469543));
#91389=CARTESIAN_POINT('Origin',(-6.1473421746,-22.8742356128,-2.26474786707));
#91390=CARTESIAN_POINT('Origin',(-6.1473421746,-23.1742356128,-2.26474786707));
#91391=CARTESIAN_POINT('Origin',(-8.05349668264,-22.8742356128,1.84629187045));
#91392=CARTESIAN_POINT('Origin',(-8.05349668264,-23.1742356128,1.84629187045));
#91393=CARTESIAN_POINT('Origin',(-11.0596214465,-22.8742356128,1.84629187045));
#91394=CARTESIAN_POINT('Origin',(-11.0596214465,-23.1742356128,1.84629187045));
#91395=CARTESIAN_POINT('Ctrl Pts',(2.55692631419833E-13,-23.1742356128,
-6.35119542306));
#91396=CARTESIAN_POINT('Ctrl Pts',(2.55692631419833E-13,-23.1742356128,
-6.35119542306));
#91397=CARTESIAN_POINT('Ctrl Pts',(2.55692631419833E-13,-23.1742356128,
-6.35119542306));
#91398=CARTESIAN_POINT('Ctrl Pts',(2.55692631419833E-13,-23.1742356128,
-6.35119542306));
#91399=CARTESIAN_POINT('Ctrl Pts',(2.55692631419833E-13,-23.1742356128,
-6.35119542306));
#91400=CARTESIAN_POINT('Ctrl Pts',(2.55692631419833E-13,-23.1742356128,
-6.35119542306));
#91401=CARTESIAN_POINT('Ctrl Pts',(0.0693760469986,-23.1744148412,-6.42641803012));
#91402=CARTESIAN_POINT('Ctrl Pts',(0.0416634461355,-23.1744158772939,-6.42685288131863));
#91403=CARTESIAN_POINT('Ctrl Pts',(0.0138942651446,-23.1744164026919,-6.42707339217563));
#91404=CARTESIAN_POINT('Ctrl Pts',(-0.0138942622373,-23.1744164026919,-6.42707339217563));
#91405=CARTESIAN_POINT('Ctrl Pts',(-0.0416634441983,-23.1744158772939,-6.42685288131863));
#91406=CARTESIAN_POINT('Ctrl Pts',(-0.0693760469997,-23.1744148412,-6.42641803012));
#91407=CARTESIAN_POINT('Ctrl Pts',(0.139040717811,-23.1404071843,-6.49840377124));
#91408=CARTESIAN_POINT('Ctrl Pts',(0.0832786080695,-23.1440517726,-6.49672753331));
#91409=CARTESIAN_POINT('Ctrl Pts',(0.0277352763853,-23.1458041293,-6.49588968315));
#91410=CARTESIAN_POINT('Ctrl Pts',(-0.0277352847943,-23.1458041293,-6.49588968315));
#91411=CARTESIAN_POINT('Ctrl Pts',(-0.0832786136747,-23.1440517726,-6.49672753331));
#91412=CARTESIAN_POINT('Ctrl Pts',(-0.13904071781,-23.1404071843,-6.49840377124));
#91413=CARTESIAN_POINT('Ctrl Pts',(0.206909891011,-23.0789305063,-6.56242231995));
#91414=CARTESIAN_POINT('Ctrl Pts',(0.124968889226,-23.0969576242,-6.57247555688));
#91415=CARTESIAN_POINT('Ctrl Pts',(0.0417906073157,-23.1061050685,-6.57744690499));
#91416=CARTESIAN_POINT('Ctrl Pts',(-0.0417906059394,-23.1061050685,-6.57744690499));
#91417=CARTESIAN_POINT('Ctrl Pts',(-0.124968888301,-23.0969576242,-6.57247555688));
#91418=CARTESIAN_POINT('Ctrl Pts',(-0.206909891012,-23.0789305063,-6.56242231995));
#91419=CARTESIAN_POINT('Ctrl Pts',(0.247420066333,-22.976056074,-6.59957097409));
#91420=CARTESIAN_POINT('Ctrl Pts',(0.150569899025,-22.9846635857,-6.62490497029));
#91421=CARTESIAN_POINT('Ctrl Pts',(0.0505568500284,-22.9890723968,-6.63785003768));
#91422=CARTESIAN_POINT('Ctrl Pts',(-0.050556853062,-22.9890723968,-6.63785003768));
#91423=CARTESIAN_POINT('Ctrl Pts',(-0.150569901037,-22.9846635857,-6.62490497029));
#91424=CARTESIAN_POINT('Ctrl Pts',(-0.247420066332,-22.976056074,-6.59957097409));
#91425=CARTESIAN_POINT('Ctrl Pts',(0.246934114499,-22.8742356112,-6.59919568243));
#91426=CARTESIAN_POINT('Ctrl Pts',(0.150218834034,-22.8742356274,-6.62384117741));
#91427=CARTESIAN_POINT('Ctrl Pts',(0.0504288433358,-22.8742356357,-6.63642072129));
#91428=CARTESIAN_POINT('Ctrl Pts',(-0.0504288433346,-22.8742356357,-6.63642072129));
#91429=CARTESIAN_POINT('Ctrl Pts',(-0.150218834033,-22.8742356274,-6.62384117741));
#91430=CARTESIAN_POINT('Ctrl Pts',(-0.246934114499,-22.8742356112,-6.59919568243));
#91431=CARTESIAN_POINT('',(-0.246934184021341,-22.8742356128,-6.5991954979861));
#91432=CARTESIAN_POINT('Origin',(-1.7193597103E-13,-22.8742356128,-5.63016324424));
#91433=CARTESIAN_POINT('Ctrl Pts',(-0.246934184771513,-22.8742356128,-6.5991954978134));
#91434=CARTESIAN_POINT('Ctrl Pts',(-0.246934148859527,-22.8894270636949,
-6.5991955069647));
#91435=CARTESIAN_POINT('Ctrl Pts',(-0.245832550213217,-22.9049462154072,
-6.59828338132465));
#91436=CARTESIAN_POINT('Ctrl Pts',(-0.243597179910913,-22.9205953175446,
-6.59632674366846));
#91437=CARTESIAN_POINT('Ctrl Pts',(-0.241426171250814,-22.9357938447094,
-6.59442644227684));
#91438=CARTESIAN_POINT('Ctrl Pts',(-0.238185574552008,-22.9511146303327,
-6.59154030865736));
#91439=CARTESIAN_POINT('Ctrl Pts',(-0.233855755675857,-22.9663366921647,
-6.58757377565012));
#91440=CARTESIAN_POINT('Ctrl Pts',(-0.231751034635713,-22.9737361226557,
-6.58564564754233));
#91441=CARTESIAN_POINT('Ctrl Pts',(-0.229389104734593,-22.9811116449574,
-6.58346269236169));
#91442=CARTESIAN_POINT('Ctrl Pts',(-0.226768764028958,-22.9884347304813,
-6.58101708621562));
#91443=CARTESIAN_POINT('Ctrl Pts',(-0.221564610785134,-23.0029788159899,
-6.57615996624994));
#91444=CARTESIAN_POINT('Ctrl Pts',(-0.215340314283273,-23.0173176761779,
-6.57026416175073));
#91445=CARTESIAN_POINT('Ctrl Pts',(-0.208096029442936,-23.0312064758602,
-6.5632974320514));
#91446=CARTESIAN_POINT('Ctrl Pts',(-0.205901552518285,-23.0354137442222,
-6.56118703359214));
#91447=CARTESIAN_POINT('Ctrl Pts',(-0.203613572566933,-23.0395795323824,
-6.55897865797242));
#91448=CARTESIAN_POINT('Ctrl Pts',(-0.201232350872621,-23.0436965948026,
-6.55667221971715));
#91449=CARTESIAN_POINT('Ctrl Pts',(-0.19611136189576,-23.0525506344417,
-6.551712057919));
#91450=CARTESIAN_POINT('Ctrl Pts',(-0.190558945505526,-23.0611795166653,
-6.54629773499068));
#91451=CARTESIAN_POINT('Ctrl Pts',(-0.184579755856799,-23.0695085808111,
-6.54043512283862));
#91452=CARTESIAN_POINT('Ctrl Pts',(-0.181590161032435,-23.073673112884,
-6.53750381676259));
#91453=CARTESIAN_POINT('Ctrl Pts',(-0.178493887542788,-23.0777627441734,
-6.53446049681495));
#91454=CARTESIAN_POINT('Ctrl Pts',(-0.175291824842479,-23.0817677673643,
-6.53130691713594));
#91455=CARTESIAN_POINT('Ctrl Pts',(-0.173690793492324,-23.0837702789598,
-6.52973012729644));
#91456=CARTESIAN_POINT('Ctrl Pts',(-0.172063316107631,-23.0857516428652,
-6.52812577757538));
#91457=CARTESIAN_POINT('Ctrl Pts',(-0.170409517042958,-23.0877106510946,
-6.5264941352391));
#91458=CARTESIAN_POINT('Ctrl Pts',(-0.169513596563035,-23.0887719139955,
-6.52561021782966));
#91459=CARTESIAN_POINT('Ctrl Pts',(-0.16832213036844,-23.0901574536878,
-6.52443867090292));
#91460=CARTESIAN_POINT('Ctrl Pts',(-0.167302169472591,-23.0913259294168,
-6.52343072184713));
#91461=CARTESIAN_POINT('Ctrl Pts',(-0.166439362407042,-23.0923143684041,
-6.52257807585787));
#91462=CARTESIAN_POINT('Ctrl Pts',(-0.165699629296992,-23.0931490318436,
-6.52184402288916));
#91463=CARTESIAN_POINT('Ctrl Pts',(-0.165369287155041,-23.0935194071582,
-6.52151762661803));
#91464=CARTESIAN_POINT('Ctrl Pts',(-0.161836338647704,-23.0974805030916,
-6.51802687847412));
#91465=CARTESIAN_POINT('Ctrl Pts',(-0.157587882532729,-23.1019181705425,
-6.51393902538029));
#91466=CARTESIAN_POINT('Ctrl Pts',(-0.152602238932102,-23.1066909261856,
-6.50915125144019));
#91467=CARTESIAN_POINT('Ctrl Pts',(-0.147737241770845,-23.1113481870159,
-6.50447933573719));
#91468=CARTESIAN_POINT('Ctrl Pts',(-0.142170055788602,-23.1163247933947,
-6.49914001872231));
#91469=CARTESIAN_POINT('Ctrl Pts',(-0.135881001461339,-23.1214407035688,
-6.49303298020319));
#91470=CARTESIAN_POINT('Ctrl Pts',(-0.129869686747692,-23.1263306829684,
-6.48719564304621));
#91471=CARTESIAN_POINT('Ctrl Pts',(-0.123198620014974,-23.1313478806465,
-6.48065594156337));
#91472=CARTESIAN_POINT('Ctrl Pts',(-0.115854507961916,-23.1362887742648,
-6.47333550793134));
#91473=CARTESIAN_POINT('Ctrl Pts',(-0.1130506684961,-23.1381751115679,-6.47054070842717));
#91474=CARTESIAN_POINT('Ctrl Pts',(-0.110148788302281,-23.1400498356338,
-6.46763228559098));
#91475=CARTESIAN_POINT('Ctrl Pts',(-0.107148401110344,-23.1418997756208,
-6.46460672780985));
#91476=CARTESIAN_POINT('Ctrl Pts',(-0.0998500822266901,-23.1463996788256,
-6.45724718249954));
#91477=CARTESIAN_POINT('Ctrl Pts',(-0.0919682950176149,-23.1507554091233,
-6.44919239150519));
#91478=CARTESIAN_POINT('Ctrl Pts',(-0.0835018169479741,-23.1547520216881,
-6.44041063626865));
#91479=CARTESIAN_POINT('Ctrl Pts',(-0.0753232474895919,-23.1586127265988,
-6.43192751086777));
#91480=CARTESIAN_POINT('Ctrl Pts',(-0.0665989231761761,-23.1621379113261,
-6.42276530222363));
#91481=CARTESIAN_POINT('Ctrl Pts',(-0.0573371151123641,-23.1651037243234,
-6.41292977338023));
#91482=CARTESIAN_POINT('Ctrl Pts',(-0.0485532283374504,-23.1679164975296,
-6.40360177056086));
#91483=CARTESIAN_POINT('Ctrl Pts',(-0.0392858230691978,-23.1702255396838,
-6.39366771310547));
#91484=CARTESIAN_POINT('Ctrl Pts',(-0.0295520826905258,-23.1718197203897,
-6.38317190916846));
#91485=CARTESIAN_POINT('Ctrl Pts',(-0.0201296495668507,-23.1733629155545,
-6.37301178502005));
#91486=CARTESIAN_POINT('Ctrl Pts',(-0.0102701699337132,-23.1742356128018,
-6.36232486459476));
#91487=CARTESIAN_POINT('Ctrl Pts',(2.3805464551794E-13,-23.1742356128,-6.35119542306));
#91488=CARTESIAN_POINT('Origin',(2.84607155346,-22.8742356128,5.53854202767));
#91489=CARTESIAN_POINT('',(-0.45,-23.1742356128,-6.23438845923));
#91490=CARTESIAN_POINT('Origin',(2.84607155346,-23.1742356128,5.53854202767));
#91491=CARTESIAN_POINT('',(-0.530881036642,-22.8742356128,-6.52327988851));
#91492=CARTESIAN_POINT('Origin',(-0.45,-22.8742356128,-6.23438845923));
#91493=CARTESIAN_POINT('Origin',(2.84607155346,-22.8742356128,5.53854202767));
#91494=CARTESIAN_POINT('Origin',(2.93915231795E-16,-20.7742356128,0.729452270839));
#91495=CARTESIAN_POINT('Ctrl Pts',(-3.39394702409,-22.8742356071,-7.27665075406));
#91496=CARTESIAN_POINT('Ctrl Pts',(-3.3939470242,-22.8742356096,-7.39921133184));
#91497=CARTESIAN_POINT('Ctrl Pts',(-3.45653492108,-22.8742356121,-7.52177190961));
#91498=CARTESIAN_POINT('Ctrl Pts',(-3.58353228733,-22.8742356136,-7.59954001295));
#91499=CARTESIAN_POINT('Ctrl Pts',(-3.72114892405,-22.8742356136,-7.59957667728));
#91500=CARTESIAN_POINT('Ctrl Pts',(-3.83031550589,-22.8742356125,-7.54386534431));
#91501=CARTESIAN_POINT('Ctrl Pts',(-3.39394702409,-22.9689887672,-7.27665074537));
#91502=CARTESIAN_POINT('Ctrl Pts',(-3.3939470273,-22.9472590608,-7.39921132275));
#91503=CARTESIAN_POINT('Ctrl Pts',(-3.45653492596,-22.9255293543,-7.52177190012));
#91504=CARTESIAN_POINT('Ctrl Pts',(-3.5835322914,-22.9117412055,-7.59954000419));
#91505=CARTESIAN_POINT('Ctrl Pts',(-3.72114892639,-22.9117347492,-7.59957667094));
#91506=CARTESIAN_POINT('Ctrl Pts',(-3.83031550688,-22.9216122395,-7.54386534051));
#91507=CARTESIAN_POINT('Ctrl Pts',(-3.39394702409,-23.0638368546,-7.29765903263));
#91508=CARTESIAN_POINT('Ctrl Pts',(-3.39394703709,-23.0202773024,-7.41438252872));
#91509=CARTESIAN_POINT('Ctrl Pts',(-3.45551763217,-22.9767177502,-7.53110602482));
#91510=CARTESIAN_POINT('Ctrl Pts',(-3.58040884259,-22.9491120295,-7.6059738358));
#91511=CARTESIAN_POINT('Ctrl Pts',(-3.71667793436,-22.9491723593,-7.60786209828));
#91512=CARTESIAN_POINT('Ctrl Pts',(-3.82588511173,-22.969036255,-7.55663051616));
#91513=CARTESIAN_POINT('Ctrl Pts',(-3.39394702409,-23.1509380315,-7.33965594802));
#91514=CARTESIAN_POINT('Ctrl Pts',(-3.39394697957,-23.0896047046,-7.44484208723));
#91515=CARTESIAN_POINT('Ctrl Pts',(-3.45348987378,-23.0282713776,-7.55002822643));
#91516=CARTESIAN_POINT('Ctrl Pts',(-3.57418338496,-22.9885124598,-7.61911093785));
#91517=CARTESIAN_POINT('Ctrl Pts',(-3.70775302124,-22.9865706365,-7.62456986686));
#91518=CARTESIAN_POINT('Ctrl Pts',(-3.81702777332,-23.0125868459,-7.58214937101));
#91519=CARTESIAN_POINT('Ctrl Pts',(-3.39394702409,-23.3144960216,-7.46222952989));
#91520=CARTESIAN_POINT('Ctrl Pts',(-3.39394707642,-23.2249734796,-7.53850326899));
#91521=CARTESIAN_POINT('Ctrl Pts',(-3.4480237922,-23.1354509376,-7.6147770081));
#91522=CARTESIAN_POINT('Ctrl Pts',(-3.55743149517,-23.0743105508,-7.66795137089));
#91523=CARTESIAN_POINT('Ctrl Pts',(-3.68302539363,-23.0640733183,-7.67932532721));
#91524=CARTESIAN_POINT('Ctrl Pts',(-3.79142259861,-23.0943657893,-7.65641303197));
#91525=CARTESIAN_POINT('Ctrl Pts',(-3.39394702409,-23.4183511293,-7.6347947685));
#91526=CARTESIAN_POINT('Ctrl Pts',(-3.39394696259,-23.319135779,-7.67899068739));
#91527=CARTESIAN_POINT('Ctrl Pts',(-3.44128745287,-23.2199204287,-7.72318660628));
#91528=CARTESIAN_POINT('Ctrl Pts',(-3.53685705407,-23.1477285443,-7.75602607095));
#91529=CARTESIAN_POINT('Ctrl Pts',(-3.65117651028,-23.1252941134,-7.76773938497));
#91530=CARTESIAN_POINT('Ctrl Pts',(-3.75606800489,-23.1462934039,-7.76036589659));
#91531=CARTESIAN_POINT('Ctrl Pts',(-3.39394702409,-23.4554260016,-7.73594528854));
#91532=CARTESIAN_POINT('Ctrl Pts',(-3.39394732526,-23.3552502828,-7.7641726908));
#91533=CARTESIAN_POINT('Ctrl Pts',(-3.43768548772,-23.255074564,-7.79240009306));
#91534=CARTESIAN_POINT('Ctrl Pts',(-3.52588291425,-23.1798234897,-7.81406109398));
#91535=CARTESIAN_POINT('Ctrl Pts',(-3.63360843235,-23.151042617,-7.82338875536));
#91536=CARTESIAN_POINT('Ctrl Pts',(-3.73562880641,-23.1648309328,-7.82105608415));
#91537=CARTESIAN_POINT('Ctrl Pts',(-3.39394702409,-23.4742356128,-7.84128512581));
#91538=CARTESIAN_POINT('Ctrl Pts',(-3.39394702409,-23.3758453918,-7.85470223468));
#91539=CARTESIAN_POINT('Ctrl Pts',(-3.43421150493,-23.2774551707,-7.86811934354));
#91540=CARTESIAN_POINT('Ctrl Pts',(-3.51532352314,-23.2014862199,-7.87872422454));
#91541=CARTESIAN_POINT('Ctrl Pts',(-3.61626901029,-23.167728681,-7.88399310977));
#91542=CARTESIAN_POINT('Ctrl Pts',(-3.71465923135,-23.1742356128,-7.88399310977));
#91543=CARTESIAN_POINT('Ctrl Pts',(-3.39394702409,-23.4742356128,-7.94679080481));
#91544=CARTESIAN_POINT('Ctrl Pts',(-3.39394702409,-23.3799878332,-7.94679080481));
#91545=CARTESIAN_POINT('Ctrl Pts',(-3.4309580406,-23.2857400536,-7.94679080481));
#91546=CARTESIAN_POINT('Ctrl Pts',(-3.50545146488,-23.2112466293,-7.94679080481));
#91547=CARTESIAN_POINT('Ctrl Pts',(-3.59969924449,-23.1742356128,-7.94679080481));
#91548=CARTESIAN_POINT('Ctrl Pts',(-3.69394702409,-23.1742356128,-7.94679080481));
#91549=CARTESIAN_POINT('',(-3.8303155059,-22.8742356128,-7.54386534442));
#91550=CARTESIAN_POINT('',(-3.69394702409,-23.1742356128,-7.94679080481));
#91551=CARTESIAN_POINT('Ctrl Pts',(-3.8303155059,-22.8742356128,-7.54386534442));
#91552=CARTESIAN_POINT('Ctrl Pts',(-3.83031550688,-22.9216122395,-7.54386534051));
#91553=CARTESIAN_POINT('Ctrl Pts',(-3.82588511173,-22.969036255,-7.55663051616));
#91554=CARTESIAN_POINT('Ctrl Pts',(-3.81702777332,-23.0125868459,-7.58214937101));
#91555=CARTESIAN_POINT('Ctrl Pts',(-3.79142259861,-23.0943657893,-7.65641303197));
#91556=CARTESIAN_POINT('Ctrl Pts',(-3.75606800489,-23.1462934039,-7.76036589659));
#91557=CARTESIAN_POINT('Ctrl Pts',(-3.73562880641,-23.1648309328,-7.82105608415));
#91558=CARTESIAN_POINT('Ctrl Pts',(-3.71465923135,-23.1742356128,-7.88399310977));
#91559=CARTESIAN_POINT('Ctrl Pts',(-3.69394702409,-23.1742356128,-7.94679080481));
#91560=CARTESIAN_POINT('Origin',(-3.69182573245668,-23.4721143211804,-7.94679080481));
#91561=CARTESIAN_POINT('Ctrl Pts',(-3.8303155058534,-22.8742356128,-7.54386534432868));
#91562=CARTESIAN_POINT('Ctrl Pts',(-3.81518314929505,-22.8742356128939,
-7.55158788853908));
#91563=CARTESIAN_POINT('Ctrl Pts',(-3.79939056241824,-22.8742356129764,
-7.55802229157615));
#91564=CARTESIAN_POINT('Ctrl Pts',(-3.78316997118284,-22.8742356130436,
-7.5630658635742));
#91565=CARTESIAN_POINT('Ctrl Pts',(-3.76665552522089,-22.874235613112,-7.56820080569857));
#91566=CARTESIAN_POINT('Ctrl Pts',(-3.74969782981516,-22.8742356131644,
-7.57189413383619));
#91567=CARTESIAN_POINT('Ctrl Pts',(-3.73255167002916,-22.8742356131991,
-7.57409096118322));
#91568=CARTESIAN_POINT('Ctrl Pts',(-3.71493679959741,-22.8742356132347,
-7.5763478414154));
#91569=CARTESIAN_POINT('Ctrl Pts',(-3.69712349521037,-22.8742356132514,
-7.57702531075057));
#91570=CARTESIAN_POINT('Ctrl Pts',(-3.67939142268828,-22.8742356132509,
-7.57611921848549));
#91571=CARTESIAN_POINT('Ctrl Pts',(-3.66143051624416,-22.8742356132503,
-7.57520143302174));
#91572=CARTESIAN_POINT('Ctrl Pts',(-3.64355349380092,-22.8742356132319,
-7.57265914646795));
#91573=CARTESIAN_POINT('Ctrl Pts',(-3.62604663418343,-22.8742356132015,
-7.56854219910733));
#91574=CARTESIAN_POINT('Ctrl Pts',(-3.60828649605848,-22.8742356131707,
-7.56436569027734));
#91575=CARTESIAN_POINT('Ctrl Pts',(-3.59090790575233,-22.8742356131275,
-7.55856885321304));
#91576=CARTESIAN_POINT('Ctrl Pts',(-3.57419660503199,-22.8742356130833,
-7.55125591270884));
#91577=CARTESIAN_POINT('Ctrl Pts',(-3.56154804494767,-22.8742356130498,
-7.54572084581559));
#91578=CARTESIAN_POINT('Ctrl Pts',(-3.54928154903051,-22.8742356130158,
-7.53931835010142));
#91579=CARTESIAN_POINT('Ctrl Pts',(-3.53751294855566,-22.8742356129882,
-7.53211173026943));
#91580=CARTESIAN_POINT('Ctrl Pts',(-3.52194460449692,-22.8742356129516,
-7.52257829957095));
#91581=CARTESIAN_POINT('Ctrl Pts',(-3.50723469779423,-22.8742356128951,
-7.51162760824219));
#91582=CARTESIAN_POINT('Ctrl Pts',(-3.49363196674743,-22.8742356128088,
-7.49943703911464));
#91583=CARTESIAN_POINT('Ctrl Pts',(-3.48014654190352,-22.8742356127232,
-7.48735159809485));
#91584=CARTESIAN_POINT('Ctrl Pts',(-3.46774980238245,-22.8742356126084,
-7.47404796167307));
#91585=CARTESIAN_POINT('Ctrl Pts',(-3.45665074877321,-22.8742356124454,
-7.45973758957544));
#91586=CARTESIAN_POINT('Ctrl Pts',(-3.44579169741472,-22.8742356122859,
-7.4457366602135));
#91587=CARTESIAN_POINT('Ctrl Pts',(-3.43617519122419,-22.8742356120803,
-7.4307724949923));
#91588=CARTESIAN_POINT('Ctrl Pts',(-3.42795843215071,-22.8742356118008,
-7.41507410196173));
#91589=CARTESIAN_POINT('Ctrl Pts',(-3.41986382836557,-22.8742356115254,
-7.39960909069516));
#91590=CARTESIAN_POINT('Ctrl Pts',(-3.41312801722337,-22.8742356111781,
-7.38343188314801));
#91591=CARTESIAN_POINT('Ctrl Pts',(-3.40785807822884,-22.8742356107227,
-7.36678603675321));
#91592=CARTESIAN_POINT('Ctrl Pts',(-3.40271733726589,-22.8742356102784,
-7.35054828058307));
#91593=CARTESIAN_POINT('Ctrl Pts',(-3.39897168837945,-22.8742356097309,
-7.33386493486951));
#91594=CARTESIAN_POINT('Ctrl Pts',(-3.39667506741503,-22.8742356090388,
-7.31698039369392));
#91595=CARTESIAN_POINT('Ctrl Pts',(-3.39485783558188,-22.8742356084911,
-7.30362027629198));
#91596=CARTESIAN_POINT('Ctrl Pts',(-3.3939470241021,-22.8742356078525,-7.29013459097236));
#91597=CARTESIAN_POINT('Ctrl Pts',(-3.39394702409,-22.8742356071,-7.27665075406));
#91598=CARTESIAN_POINT('Origin',(2.84607155346,-22.8742356128,5.53854202767));
#91599=CARTESIAN_POINT('',(-6.53717906469,-22.8742356128,-5.76093294477));
#91600=CARTESIAN_POINT('Origin',(2.84607155346,-22.8742356128,5.53854202767));
#91601=CARTESIAN_POINT('',(-6.72883656293,-23.1742356128,-5.99173026574));
#91602=CARTESIAN_POINT('Origin',(-6.72883656293,-22.8742356128,-5.99173026574));
#91603=CARTESIAN_POINT('Origin',(2.84607155346,-23.1742356128,5.53854202767));
#91604=CARTESIAN_POINT('Origin',(1.35123173137E-15,-21.2742356128,-3.80469754864));
#91605=CARTESIAN_POINT('',(-0.11480502971,-19.4742356128,-4.08186140839));
#91606=CARTESIAN_POINT('Origin',(1.61893433855E-15,-19.4742356128,-3.80469754864));
#91607=CARTESIAN_POINT('',(-0.11480502971,-23.0742356128,-4.08186140839));
#91608=CARTESIAN_POINT('',(-0.11480502971,-21.2742356128,-4.08186140839));
#91609=CARTESIAN_POINT('Origin',(1.12255033962E-15,-23.0742356128,-3.80469754864));
#91610=CARTESIAN_POINT('Origin',(-3.1295913978,-23.1742356128,-2.83309600707));
#91611=CARTESIAN_POINT('',(-3.32093311398,-19.4742356128,-2.75383967318));
#91612=CARTESIAN_POINT('',(-3.32093311398,-23.0742356128,-2.75383967318));
#91613=CARTESIAN_POINT('',(-3.32093311398,-21.2742356128,-2.75383967318));
#91614=CARTESIAN_POINT('',(0.0382683432365,-23.0742356128,-4.14526647551));
#91615=CARTESIAN_POINT('',(0.0382683432365,-19.4742356128,-4.14526647551));
#91616=CARTESIAN_POINT('Origin',(4.78632831116E-15,-22.5742356128,-7.33821278943));
#91617=CARTESIAN_POINT('',(-0.647446102181,-19.6742356128,-10.2675153591));
#91618=CARTESIAN_POINT('',(-0.647446102181,-20.0742356128,-10.2675153591));
#91619=CARTESIAN_POINT('Origin',(-4.16333634234434E-16,-19.6742356129479,
-7.33819410486897));
#91620=CARTESIAN_POINT('Origin',(2.84607155346,-20.0742356128,5.53854202767));
#91621=CARTESIAN_POINT('',(-3.81744045688,-22.8742356128,-9.21387212773));
#91622=CARTESIAN_POINT('Ctrl Pts',(-3.81744045688,-22.8742356128,-9.21387212773));
#91623=CARTESIAN_POINT('Ctrl Pts',(-3.78438300100211,-22.8742356128,-9.22880383666651));
#91624=CARTESIAN_POINT('Ctrl Pts',(-3.75125472648156,-22.876873984767,-9.24363320588492));
#91625=CARTESIAN_POINT('Ctrl Pts',(-3.71838012225711,-22.8821739340745,
-9.25821762563378));
#91626=CARTESIAN_POINT('Ctrl Pts',(-3.6865095776919,-22.8873120117665,-9.27235660648325));
#91627=CARTESIAN_POINT('Ctrl Pts',(-3.65487745148123,-22.8949539427161,
-9.28626544525872));
#91628=CARTESIAN_POINT('Ctrl Pts',(-3.62382288627738,-22.9051278862397,
-9.29980564138486));
#91629=CARTESIAN_POINT('Ctrl Pts',(-3.59982416043969,-22.9129902304622,
-9.31026939936978));
#91630=CARTESIAN_POINT('Ctrl Pts',(-3.57617118781195,-22.9223651478789,
-9.32051284720793));
#91631=CARTESIAN_POINT('Ctrl Pts',(-3.55303923210181,-22.9332555735994,
-9.33046796299208));
#91632=CARTESIAN_POINT('Ctrl Pts',(-3.52731510523081,-22.9453663824053,
-9.34153865086025));
#91633=CARTESIAN_POINT('Ctrl Pts',(-3.50223264779224,-22.9593502627365,
-9.35225383201401));
#91634=CARTESIAN_POINT('Ctrl Pts',(-3.47806004814019,-22.9751863932197,
-9.36251314034884));
#91635=CARTESIAN_POINT('Ctrl Pts',(-3.45499124406393,-22.990299397063,-9.37230397697133));
#91636=CARTESIAN_POINT('Ctrl Pts',(-3.43275123888764,-23.0070999540256,
-9.38167960517042));
#91637=CARTESIAN_POINT('Ctrl Pts',(-3.41159767393858,-23.0255307665745,
-9.39054653772574));
#91638=CARTESIAN_POINT('Ctrl Pts',(-3.39154598669303,-23.0430015281129,
-9.39895159658247));
#91639=CARTESIAN_POINT('Ctrl Pts',(-3.37247065010445,-23.061937444689,-9.40689954920998));
#91640=CARTESIAN_POINT('Ctrl Pts',(-3.35461163146646,-23.0822474209105,
-9.41430534116002));
#91641=CARTESIAN_POINT('Ctrl Pts',(-3.34903427425971,-23.0885902102061,
-9.41661816405032));
#91642=CARTESIAN_POINT('Ctrl Pts',(-3.34357569434173,-23.0950666709068,
-9.41887806947029));
#91643=CARTESIAN_POINT('Ctrl Pts',(-3.33824360900109,-23.1016730489955,
-9.42108235584647));
#91644=CARTESIAN_POINT('Ctrl Pts',(-3.32258626090874,-23.1210722811451,
-9.42755511029096));
#91645=CARTESIAN_POINT('Ctrl Pts',(-3.30801838438582,-23.1415942623807,
-9.43354874753964));
#91646=CARTESIAN_POINT('Ctrl Pts',(-3.29472253386083,-23.1631172221777,
-9.43900011480726));
#91647=CARTESIAN_POINT('Ctrl Pts',(-3.28136620602029,-23.1847380810018,
-9.44447627808608));
#91648=CARTESIAN_POINT('Ctrl Pts',(-3.26929464819255,-23.2073686497991,
-9.44940485150287));
#91649=CARTESIAN_POINT('Ctrl Pts',(-3.25868404771759,-23.2308337864388,
-9.45372543317535));
#91650=CARTESIAN_POINT('Ctrl Pts',(-3.24835603008727,-23.253673996612,-9.45793094857403));
#91651=CARTESIAN_POINT('Ctrl Pts',(-3.23941312735556,-23.2773043321175,
-9.46156012110628));
#91652=CARTESIAN_POINT('Ctrl Pts',(-3.23199421260798,-23.3015220020268,
-9.46456562543563));
#91653=CARTESIAN_POINT('Ctrl Pts',(-3.22751779279442,-23.3161344434833,
-9.46637908462574));
#91654=CARTESIAN_POINT('Ctrl Pts',(-3.22359568701309,-23.3309599547749,
-9.46796566933521));
#91655=CARTESIAN_POINT('Ctrl Pts',(-3.22025193761968,-23.3459477027596,
-9.46931721244178));
#91656=CARTESIAN_POINT('Ctrl Pts',(-3.21506416160153,-23.3692009644169,
-9.47141411089046));
#91657=CARTESIAN_POINT('Ctrl Pts',(-3.21127189271638,-23.3928404899255,
-9.47294403759531));
#91658=CARTESIAN_POINT('Ctrl Pts',(-3.20893196554164,-23.4166584893515,
-9.47388782994456));
#91659=CARTESIAN_POINT('Ctrl Pts',(-3.20705389182888,-23.4357753059324,
-9.47464533710999));
#91660=CARTESIAN_POINT('Ctrl Pts',(-3.20611087685479,-23.4550065968702,
-9.47502544136242));
#91661=CARTESIAN_POINT('Ctrl Pts',(-3.20611087388,-23.4742356128,-9.47502544833));
#91662=CARTESIAN_POINT('',(-13.018207968,-22.8742356128,8.75735407375));
#91663=CARTESIAN_POINT('Origin',(2.84607155346,-22.8742356128,5.53854202767));
#91664=CARTESIAN_POINT('',(-12.9732844032,-22.9031898545,8.9713386779));
#91665=CARTESIAN_POINT('Origin',(-12.9922058324069,-23.4864244001328,8.73196264121582));
#91666=CARTESIAN_POINT('',(-12.9732844032,-19.6742356128,8.9713386779));
#91667=CARTESIAN_POINT('',(-12.9732844032,-21.2742356128,8.9713386779));
#91668=CARTESIAN_POINT('',(-11.5410914269,-19.6742356128,-1.88073402204));
#91669=CARTESIAN_POINT('Origin',(2.84607155346,-19.6742356128,5.53854202767));
#91670=CARTESIAN_POINT('',(-11.5410915433775,-22.0742358826999,-1.880733914433));
#91671=CARTESIAN_POINT('',(-11.5410914269,-21.2742356128,-1.88073402204));
#91672=CARTESIAN_POINT('',(-11.2053401891,-22.6742356128,-2.49849372966));
#91673=CARTESIAN_POINT('Ctrl Pts',(-11.2053401891,-22.6742356128,-2.49849372966));
#91674=CARTESIAN_POINT('Ctrl Pts',(-11.2150383685076,-22.6742356128,-2.48153808629711));
#91675=CARTESIAN_POINT('Ctrl Pts',(-11.2249897894519,-22.6738663548581,
-2.46406918052205));
#91676=CARTESIAN_POINT('Ctrl Pts',(-11.2351241182894,-22.6729000605474,
-2.44619729884691));
#91677=CARTESIAN_POINT('Ctrl Pts',(-11.2369260237553,-22.6727282513405,
-2.44301963984323));
#91678=CARTESIAN_POINT('Ctrl Pts',(-11.2387336971335,-22.6725376931046,
-2.43982928294016));
#91679=CARTESIAN_POINT('Ctrl Pts',(-11.2405467261739,-22.6723272624817,
-2.43662689819009));
#91680=CARTESIAN_POINT('Ctrl Pts',(-11.2503196279632,-22.6711929630497,
-2.41936485166077));
#91681=CARTESIAN_POINT('Ctrl Pts',(-11.2602458476986,-22.6694750423375,
-2.40175690044939));
#91682=CARTESIAN_POINT('Ctrl Pts',(-11.2702378606974,-22.6669990989714,
-2.38395208224529));
#91683=CARTESIAN_POINT('Ctrl Pts',(-11.2725244303702,-22.6664325047313,
-2.37987763224816));
#91684=CARTESIAN_POINT('Ctrl Pts',(-11.2748144198167,-22.665826417789,-2.37579294242994));
#91685=CARTESIAN_POINT('Ctrl Pts',(-11.2771067403129,-22.6651791086157,
-2.37169991214447));
#91686=CARTESIAN_POINT('Ctrl Pts',(-11.2875627511759,-22.6622265233383,
-2.35303028492714));
#91687=CARTESIAN_POINT('Ctrl Pts',(-11.2980683420681,-22.658419074168,-2.33418470244293));
#91688=CARTESIAN_POINT('Ctrl Pts',(-11.3085232390998,-22.6536382160094,
-2.31534181654695));
#91689=CARTESIAN_POINT('Ctrl Pts',(-11.311982469164,-22.6520563651097,-2.30910723793846));
#91690=CARTESIAN_POINT('Ctrl Pts',(-11.3154361566497,-22.6503683749809,
-2.30287299222311));
#91691=CARTESIAN_POINT('Ctrl Pts',(-11.3188807244952,-22.6485711953677,
-2.29664559899274));
#91692=CARTESIAN_POINT('Ctrl Pts',(-11.3296723127873,-22.6429407583018,
-2.27713561489883));
#91693=CARTESIAN_POINT('Ctrl Pts',(-11.3403771745526,-22.6362330411102,
-2.25768738349784));
#91694=CARTESIAN_POINT('Ctrl Pts',(-11.350894153497,-22.6283844511168,-2.23848952894692));
#91695=CARTESIAN_POINT('Ctrl Pts',(-11.3538790481232,-22.6261568899304,
-2.23304085654893));
#91696=CARTESIAN_POINT('Ctrl Pts',(-11.356848858058,-22.6238377439721,-2.22761230160938));
#91697=CARTESIAN_POINT('Ctrl Pts',(-11.3598014066801,-22.6214262928633,
-2.22220802156407));
#91698=CARTESIAN_POINT('Ctrl Pts',(-11.3700755207974,-22.6130350597113,
-2.20340250910257));
#91699=CARTESIAN_POINT('Ctrl Pts',(-11.380144070066,-22.6035189145293,-2.18488415807147));
#91700=CARTESIAN_POINT('Ctrl Pts',(-11.3899200358009,-22.5928768230476,
-2.16682324106742));
#91701=CARTESIAN_POINT('Ctrl Pts',(-11.3995284381226,-22.582417140672,-2.1490718943892));
#91702=CARTESIAN_POINT('Ctrl Pts',(-11.4088538998602,-22.5708701456172,
-2.13176302103624));
#91703=CARTESIAN_POINT('Ctrl Pts',(-11.4178296800987,-22.5582763477247,
-2.11503479986363));
#91704=CARTESIAN_POINT('Ctrl Pts',(-11.41987788432,-22.5554025396189,-2.11121754806936));
#91705=CARTESIAN_POINT('Ctrl Pts',(-11.4219079567884,-22.5524743831754,
-2.10743041339639));
#91706=CARTESIAN_POINT('Ctrl Pts',(-11.4239192477556,-22.5494926390321,
-2.1036748141767));
#91707=CARTESIAN_POINT('Ctrl Pts',(-11.43417381845,-22.5342902110344,-2.08452688464914));
#91708=CARTESIAN_POINT('Ctrl Pts',(-11.4439376612349,-22.5176830774906,
-2.06620306707214));
#91709=CARTESIAN_POINT('Ctrl Pts',(-11.4531160015901,-22.4997822076498,
-2.04890684167093));
#91710=CARTESIAN_POINT('Ctrl Pts',(-11.4604919004757,-22.4853967086597,
-2.03500724711187));
#91711=CARTESIAN_POINT('Ctrl Pts',(-11.4674900183935,-22.4701767234614,
-2.02177078277232));
#91712=CARTESIAN_POINT('Ctrl Pts',(-11.4740689030204,-22.4541987893081,
-2.00928995557508));
#91713=CARTESIAN_POINT('Ctrl Pts',(-11.4825434750249,-22.4336168576976,
-1.99321281260074));
#91714=CARTESIAN_POINT('Ctrl Pts',(-11.490322094781,-22.4117772815337,-1.97839019854048));
#91715=CARTESIAN_POINT('Ctrl Pts',(-11.497328194312,-22.388875007061,-1.96499799149759));
#91716=CARTESIAN_POINT('Ctrl Pts',(-11.5044353732041,-22.3656423137493,
-1.95141257056642));
#91717=CARTESIAN_POINT('Ctrl Pts',(-11.5107475618039,-22.3413165292408,
-1.93929939008369));
#91718=CARTESIAN_POINT('Ctrl Pts',(-11.516202430633,-22.3161381940112,-1.92880681486341));
#91719=CARTESIAN_POINT('Ctrl Pts',(-11.5217404470366,-22.2905760699918,
-1.91815430322522));
#91720=CARTESIAN_POINT('Ctrl Pts',(-11.5263947864914,-22.2641357626773,
-1.90917247603084));
#91721=CARTESIAN_POINT('Ctrl Pts',(-11.5301185510954,-22.2370988916848,
-1.90197624996427));
#91722=CARTESIAN_POINT('Ctrl Pts',(-11.5312011327901,-22.2292386683008,
-1.89988414602147));
#91723=CARTESIAN_POINT('Ctrl Pts',(-11.5322051805355,-22.2213281837172,
-1.89794268745646));
#91724=CARTESIAN_POINT('Ctrl Pts',(-11.5331298302645,-22.2133747150666,
-1.8961540158936));
#91725=CARTESIAN_POINT('Ctrl Pts',(-11.5363534362541,-22.18564654041,-1.88991817092117));
#91726=CARTESIAN_POINT('Ctrl Pts',(-11.538610065403,-22.1573952246849,-1.88554404014394));
#91727=CARTESIAN_POINT('Ctrl Pts',(-11.5398768288808,-22.1289373239018,
-1.88308865866385));
#91728=CARTESIAN_POINT('Ctrl Pts',(-11.5406859896255,-22.1107594899229,
-1.88152025355765));
#91729=CARTESIAN_POINT('Ctrl Pts',(-11.5410916389492,-22.0924976615588,
-1.88073379444023));
#91730=CARTESIAN_POINT('Ctrl Pts',(-11.5410916355629,-22.0742358827,-1.88073379476507));
#91731=CARTESIAN_POINT('',(-10.9558455155,-22.6742356128,-2.9197793747));
#91732=CARTESIAN_POINT('Origin',(2.84607155346,-22.6742356128,5.53854202767));
#91733=CARTESIAN_POINT('',(-10.5755260945836,-22.0742355256,-3.51114483648484));
#91734=CARTESIAN_POINT('Ctrl Pts',(-10.5755260924509,-22.0742355256,-3.51114484417453));
#91735=CARTESIAN_POINT('Ctrl Pts',(-10.5755260822369,-22.1031469614448,
-3.51114486448172));
#91736=CARTESIAN_POINT('Ctrl Pts',(-10.5767677418046,-22.1320579213261,
-3.50930400549702));
#91737=CARTESIAN_POINT('Ctrl Pts',(-10.5792325785806,-22.1606355884888,
-3.50564573524642));
#91738=CARTESIAN_POINT('Ctrl Pts',(-10.5800163561132,-22.1697228163623,
-3.50448246550852));
#91739=CARTESIAN_POINT('Ctrl Pts',(-10.5809235534889,-22.1787763809613,
-3.50313572368826));
#91740=CARTESIAN_POINT('Ctrl Pts',(-10.5819528553846,-22.1877857466703,
-3.50160709265196));
#91741=CARTESIAN_POINT('Ctrl Pts',(-10.5851501398811,-22.2157712244254,
-3.49685875950131));
#91742=CARTESIAN_POINT('Ctrl Pts',(-10.5895274155016,-22.2433280808745,
-3.49035326238203));
#91743=CARTESIAN_POINT('Ctrl Pts',(-10.5950216821739,-22.2701519594831,
-3.48216748914416));
#91744=CARTESIAN_POINT('Ctrl Pts',(-10.6005159488462,-22.2969758380917,
-3.47398171590629));
#91745=CARTESIAN_POINT('Ctrl Pts',(-10.6071270982676,-22.3230660301722,
-3.46411560723739));
#91746=CARTESIAN_POINT('Ctrl Pts',(-10.6147618810049,-22.3481448348233,
-3.45268519075675));
#91747=CARTESIAN_POINT('Ctrl Pts',(-10.622080654927,-22.3721856108078,-3.44172788693613));
#91748=CARTESIAN_POINT('Ctrl Pts',(-10.6303374421656,-22.3952935640885,
-3.42933684581246));
#91749=CARTESIAN_POINT('Ctrl Pts',(-10.6394305448135,-22.4172536196382,
-3.41564103111459));
#91750=CARTESIAN_POINT('Ctrl Pts',(-10.6482304239307,-22.4385055335036,
-3.40238686271707));
#91751=CARTESIAN_POINT('Ctrl Pts',(-10.6578134256327,-22.4586820254219,
-3.38791074678206));
#91752=CARTESIAN_POINT('Ctrl Pts',(-10.6680658047925,-22.4776185689882,
-3.37236187144591));
#91753=CARTESIAN_POINT('Ctrl Pts',(-10.6695640249749,-22.4803858400104,
-3.37008965360454));
#91754=CARTESIAN_POINT('Ctrl Pts',(-10.6710765029368,-22.4831266918782,
-3.36779458436639));
#91755=CARTESIAN_POINT('Ctrl Pts',(-10.6726028459052,-22.4858406750051,
-3.36547718891772));
#91756=CARTESIAN_POINT('Ctrl Pts',(-10.6822657120498,-22.5030221710496,
-3.35080638262523));
#91757=CARTESIAN_POINT('Ctrl Pts',(-10.6924829158915,-22.5191257906813,
-3.33524243824076));
#91758=CARTESIAN_POINT('Ctrl Pts',(-10.7031594665192,-22.5340498367433,
-3.31891032579949));
#91759=CARTESIAN_POINT('Ctrl Pts',(-10.7138348392274,-22.5489722362692,
-3.30258001524302));
#91760=CARTESIAN_POINT('Ctrl Pts',(-10.7249691157714,-22.5627148211697,
-3.28548218570648));
#91761=CARTESIAN_POINT('Ctrl Pts',(-10.7364505099692,-22.5752141494242,
-3.26777236884611));
#91762=CARTESIAN_POINT('Ctrl Pts',(-10.7411978244337,-22.5803823581624,
-3.26044973291037));
#91763=CARTESIAN_POINT('Ctrl Pts',(-10.7460043143161,-22.5853385080984,
-3.25302278904938));
#91764=CARTESIAN_POINT('Ctrl Pts',(-10.7508614475812,-22.5900803309822,
-3.24550376429458));
#91765=CARTESIAN_POINT('Ctrl Pts',(-10.7627069683827,-22.6016446341505,
-3.22716645311171));
#91766=CARTESIAN_POINT('Ctrl Pts',(-10.7748560071437,-22.6119277933076,
-3.20827751126036));
#91767=CARTESIAN_POINT('Ctrl Pts',(-10.7871852725812,-22.620935663889,-3.18901744575809));
#91768=CARTESIAN_POINT('Ctrl Pts',(-10.7903745404317,-22.6232657712414,
-3.18403535594777));
#91769=CARTESIAN_POINT('Ctrl Pts',(-10.7935758339048,-22.6255107998843,
-3.17902851552711));
#91770=CARTESIAN_POINT('Ctrl Pts',(-10.7967869569923,-22.6276714019374,
-3.17400020894282));
#91771=CARTESIAN_POINT('Ctrl Pts',(-10.8086005850894,-22.6356201938167,
-3.15550121580946));
#91772=CARTESIAN_POINT('Ctrl Pts',(-10.8205463051744,-22.6424216610541,
-3.1367127417122));
#91773=CARTESIAN_POINT('Ctrl Pts',(-10.8325097037303,-22.6481359064699,
-3.11780970742615));
#91774=CARTESIAN_POINT('Ctrl Pts',(-10.836369413317,-22.6499794735557,-3.1117110873466));
#91775=CARTESIAN_POINT('Ctrl Pts',(-10.8402309498401,-22.65171026809,-3.10560060707827));
#91776=CARTESIAN_POINT('Ctrl Pts',(-10.8440904541677,-22.6533314735688,
-3.09948429558307));
#91777=CARTESIAN_POINT('Ctrl Pts',(-10.8558666365666,-22.658278122103,-3.08082210643566));
#91778=CARTESIAN_POINT('Ctrl Pts',(-10.8676229787536,-22.6621918852187,
-3.06210658929104));
#91779=CARTESIAN_POINT('Ctrl Pts',(-10.8792423341283,-22.6652063814963,
-3.04352515477537));
#91780=CARTESIAN_POINT('Ctrl Pts',(-10.8901782818038,-22.6680435762026,
-3.02603661181894));
#91781=CARTESIAN_POINT('Ctrl Pts',(-10.9009927099857,-22.6700845210861,
-3.00866714751034));
#91782=CARTESIAN_POINT('Ctrl Pts',(-10.9115939386224,-22.6714920197301,
-2.99156911371207));
#91783=CARTESIAN_POINT('Ctrl Pts',(-10.9122564291068,-22.6715799769367,
-2.99050062579606));
#91784=CARTESIAN_POINT('Ctrl Pts',(-10.9129180895067,-22.671665477032,-2.98943319573186));
#91785=CARTESIAN_POINT('Ctrl Pts',(-10.9135788984978,-22.6717485664354,
-2.98836685977345));
#91786=CARTESIAN_POINT('Ctrl Pts',(-10.9246016135353,-22.6731345506286,
-2.9705796965187));
#91787=CARTESIAN_POINT('Ctrl Pts',(-10.9353804297876,-22.6738503295624,
-2.95310776326213));
#91788=CARTESIAN_POINT('Ctrl Pts',(-10.9458478020495,-22.6741130911883,
-2.93607201666157));
#91789=CARTESIAN_POINT('Ctrl Pts',(-10.9492132620403,-22.6741975740668,
-2.93059469893909));
#91790=CARTESIAN_POINT('Ctrl Pts',(-10.9525465530167,-22.6742356128,-2.92516247667494));
#91791=CARTESIAN_POINT('Ctrl Pts',(-10.9558455155,-22.6742356128,-2.9197793747));
#91792=CARTESIAN_POINT('',(-10.575526102,-19.6742356128,-3.51114482323));
#91793=CARTESIAN_POINT('',(-10.575526102,-21.2742356128,-3.51114482323));
#91794=CARTESIAN_POINT('Origin',(2.84607155346,-19.6742356128,5.53854202767));
#91795=CARTESIAN_POINT('Origin',(-5.88314991338E-17,-21.2742356128,5.26360209032));
#91796=CARTESIAN_POINT('',(-0.11480502971,-19.4742356128,5.54076595007));
#91797=CARTESIAN_POINT('Origin',(3.14260590599E-16,-19.4742356128,5.26360209032));
#91798=CARTESIAN_POINT('',(-0.11480502971,-23.0742356128,5.54076595007));
#91799=CARTESIAN_POINT('Origin',(-1.5436783271E-16,-23.0742356128,5.26360209032));
#91800=CARTESIAN_POINT('',(-0.11480502971,-21.2742356128,5.54076595007));
#91801=CARTESIAN_POINT('Origin',(-0.306146745892,-23.1742356128,5.46150961618));
#91802=CARTESIAN_POINT('',(-3.28628885403,-23.0742356128,4.22709433719));
#91803=CARTESIAN_POINT('',(0.0382683432365,-23.0742356128,5.60417101718));
#91804=CARTESIAN_POINT('',(-3.32093311400686,-23.0738037252489,4.21274421484887));
#91805=CARTESIAN_POINT('Origin',(-2.99360273116386,-22.7074961024392,4.3483288972549));
#91806=CARTESIAN_POINT('',(-3.32093311398,-19.4742356128,4.21274421486));
#91807=CARTESIAN_POINT('',(-3.32093311398,-21.2742356128,4.21274421486));
#91808=CARTESIAN_POINT('',(0.0382683432365,-19.4742356128,5.60417101718));
#91809=CARTESIAN_POINT('Origin',(-3.20612808427,-21.2742356128,3.93558035511));
#91810=CARTESIAN_POINT('',(-3.48329194402,-19.4742356128,4.05038538482));
#91811=CARTESIAN_POINT('Origin',(-3.20612808427,-19.4742356128,3.93558035511));
#91812=CARTESIAN_POINT('',(-3.48329194413303,-23.0738037264187,4.05038538486682));
#91813=CARTESIAN_POINT('Ctrl Pts',(-3.32093311408565,-23.0738037279965,
4.21274421481624));
#91814=CARTESIAN_POINT('Ctrl Pts',(-3.32649953892796,-23.0736167080344,
4.21043852615111));
#91815=CARTESIAN_POINT('Ctrl Pts',(-3.33218472035755,-23.0733915385147,
4.20788283100398));
#91816=CARTESIAN_POINT('Ctrl Pts',(-3.33779803563545,-23.0731489797998,
4.2051381487545));
#91817=CARTESIAN_POINT('Ctrl Pts',(-3.3433941674316,-23.0729071636055,4.20240186852682));
#91818=CARTESIAN_POINT('Ctrl Pts',(-3.34891808664344,-23.0726490695311,
4.19947790246271));
#91819=CARTESIAN_POINT('Ctrl Pts',(-3.3541921005032,-23.0723930661155,4.19647738284274));
#91820=CARTESIAN_POINT('Ctrl Pts',(-3.35966736019967,-23.0721272941207,
4.19336236938608));
#91821=CARTESIAN_POINT('Ctrl Pts',(-3.36487256382545,-23.0718643619847,
4.1901655261768));
#91822=CARTESIAN_POINT('Ctrl Pts',(-3.36963320621352,-23.0716096917244,
4.18706010956818));
#91823=CARTESIAN_POINT('Ctrl Pts',(-3.3704732769902,-23.0715647521919,4.18651212265178));
#91824=CARTESIAN_POINT('Ctrl Pts',(-3.37129957700738,-23.0715200233368,
4.18596708260654));
#91825=CARTESIAN_POINT('Ctrl Pts',(-3.37211124092873,-23.0714754752609,
4.18542605817892));
#91826=CARTESIAN_POINT('Ctrl Pts',(-3.37925430544364,-23.0710834290309,
4.18066476192198));
#91827=CARTESIAN_POINT('Ctrl Pts',(-3.38676214200264,-23.0707665220959,
4.17521843173161));
#91828=CARTESIAN_POINT('Ctrl Pts',(-3.39449455836696,-23.0705326312762,
4.16896150743035));
#91829=CARTESIAN_POINT('Ctrl Pts',(-3.39765144005647,-23.0704371416373,
4.16640701879075));
#91830=CARTESIAN_POINT('Ctrl Pts',(-3.40103633252313,-23.07035052779,4.16355761839104));
#91831=CARTESIAN_POINT('Ctrl Pts',(-3.40439681524113,-23.0702861543674,
4.16059166666122));
#91832=CARTESIAN_POINT('Ctrl Pts',(-3.40775272380699,-23.0702218685672,
4.15762975206403));
#91833=CARTESIAN_POINT('Ctrl Pts',(-3.41108364310168,-23.070179967768,4.15455185397879));
#91834=CARTESIAN_POINT('Ctrl Pts',(-3.41417028014852,-23.0701613960827,
4.15157738913841));
#91835=CARTESIAN_POINT('Ctrl Pts',(-3.41556346404581,-23.0701530135705,
4.15023483526642));
#91836=CARTESIAN_POINT('Ctrl Pts',(-3.41690737724349,-23.0701491978883,
4.14891389157001));
#91837=CARTESIAN_POINT('Ctrl Pts',(-3.41818426505082,-23.0701491888037,
4.14763700853578));
#91838=CARTESIAN_POINT('Ctrl Pts',(-3.4263619288722,-23.0701491306227,4.13945937528304));
#91839=CARTESIAN_POINT('Ctrl Pts',(-3.43407663369041,-23.0703076690209,
4.13081108398498));
#91840=CARTESIAN_POINT('Ctrl Pts',(-3.44127024360413,-23.0706011962246,
4.12174976949149));
#91841=CARTESIAN_POINT('Ctrl Pts',(-3.44816625075039,-23.0708825800805,
4.11306332551536));
#91842=CARTESIAN_POINT('Ctrl Pts',(-3.45458303810648,-23.0712882536269,
4.10399736533341));
#91843=CARTESIAN_POINT('Ctrl Pts',(-3.4604744230075,-23.0717516366824,4.09460399601809));
#91844=CARTESIAN_POINT('Ctrl Pts',(-3.46583461881877,-23.0721732394048,
4.08605756768185));
#91845=CARTESIAN_POINT('Ctrl Pts',(-3.47075949094676,-23.0726427185181,
4.07724017642156));
#91846=CARTESIAN_POINT('Ctrl Pts',(-3.4752236042024,-23.0730692325225,4.06819151220635));
#91847=CARTESIAN_POINT('Ctrl Pts',(-3.47810595867232,-23.0733446208196,
4.06234903997189));
#91848=CARTESIAN_POINT('Ctrl Pts',(-3.48079639531383,-23.0736013142645,
4.05641016936358));
#91849=CARTESIAN_POINT('Ctrl Pts',(-3.48329194424607,-23.0738037257,4.05038538491364));
#91850=CARTESIAN_POINT('',(-3.48329194402,-21.2742356128,4.05038538482));
#91851=CARTESIAN_POINT('Origin',(-3.56254827791,-23.1742356128,3.85904366864));
#91852=CARTESIAN_POINT('',(-3.49764208328952,-23.0742356036667,4.0157410839798));
#91853=CARTESIAN_POINT('Origin',(-3.61516698256916,-22.7188054056451,3.73201086501446));
#91854=CARTESIAN_POINT('',(-4.7969635569,-23.0742356128,0.878901560502));
#91855=CARTESIAN_POINT('',(-3.72150316839,-23.0742356128,3.47529261624));
#91856=CARTESIAN_POINT('',(-4.81131367924113,-23.0738037252489,0.844257300522139));
#91857=CARTESIAN_POINT('Origin',(-4.67572895257626,-22.7074959741112,1.17158778382924));
#91858=CARTESIAN_POINT('',(-4.81131367923,-19.4742356128,0.844257300549));
#91859=CARTESIAN_POINT('',(-4.81131367923,-21.2742356128,0.844257300549));
#91860=CARTESIAN_POINT('',(-4.02322090503,-19.4742356128,2.74688156443));
#91861=CARTESIAN_POINT('Origin',(-4.53414981948,-21.2742356128,0.729452270839));
#91862=CARTESIAN_POINT('',(-4.81131367923,-19.4742356128,0.614647241129));
#91863=CARTESIAN_POINT('Origin',(-4.53414981948,-19.4742356128,0.729452270839));
#91864=CARTESIAN_POINT('',(-4.81131367935289,-23.0738037265127,0.61464724109448));
#91865=CARTESIAN_POINT('Ctrl Pts',(-4.81131367927376,-23.0738037279964,
0.844257300443346));
#91866=CARTESIAN_POINT('Ctrl Pts',(-4.81361936799537,-23.0736167080296,
0.838690875456146));
#91867=CARTESIAN_POINT('Ctrl Pts',(-4.81583224901354,-23.0733915385045,
0.832863695608802));
#91868=CARTESIAN_POINT('Ctrl Pts',(-4.81786067891667,-23.0731489797839,
0.826953698746072));
#91869=CARTESIAN_POINT('Ctrl Pts',(-4.81988289938928,-23.0729071635841,
0.821061793568343));
#91870=CARTESIAN_POINT('Ctrl Pts',(-4.82172134391612,-23.0726490695041,
0.815088236474101));
#91871=CARTESIAN_POINT('Ctrl Pts',(-4.82332894712803,-23.0723930660825,
0.809237257609517));
#91872=CARTESIAN_POINT('Ctrl Pts',(-4.82499789326136,-23.0721272940827,
0.803163017100496));
#91873=CARTESIAN_POINT('Ctrl Pts',(-4.82641801853694,-23.0718643619411,
0.797221872695268));
#91874=CARTESIAN_POINT('Ctrl Pts',(-4.82758843991301,-23.0716096916733,
0.791659728914695));
#91875=CARTESIAN_POINT('Ctrl Pts',(-4.82779497430443,-23.0715647521585,
0.790678224300857));
#91876=CARTESIAN_POINT('Ctrl Pts',(-4.8279938550574,-23.0715200233209,0.78970854082669));
#91877=CARTESIAN_POINT('Ctrl Pts',(-4.82818522600442,-23.0714754752622,
0.788752046093464));
#91878=CARTESIAN_POINT('Ctrl Pts',(-4.82986939051381,-23.0710834290264,
0.780334391751288));
#91879=CARTESIAN_POINT('Ctrl Pts',(-4.83132709564776,-23.0707665220907,
0.771174412539057));
#91880=CARTESIAN_POINT('Ctrl Pts',(-4.83237042608539,-23.0705326312721,
0.761282454889659));
#91881=CARTESIAN_POINT('Ctrl Pts',(-4.8327963823021,-23.0704371416318,0.757243906119096));
#91882=CARTESIAN_POINT('Ctrl Pts',(-4.83317503237506,-23.0703505277842,
0.752835595290697));
#91883=CARTESIAN_POINT('Ctrl Pts',(-4.83345400791012,-23.0702861543619,
0.748362130534413));
#91884=CARTESIAN_POINT('Ctrl Pts',(-4.83373260371525,-23.0702218685622,
0.743894754873028));
#91885=CARTESIAN_POINT('Ctrl Pts',(-4.83391151672308,-23.0701799677641,
0.739363036592918));
#91886=CARTESIAN_POINT('Ctrl Pts',(-4.83399083444416,-23.0701613960804,
0.735077190299951));
#91887=CARTESIAN_POINT('Ctrl Pts',(-4.83402663527135,-23.0701530135698,
0.73314273176506));
#91888=CARTESIAN_POINT('Ctrl Pts',(-4.83404287715848,-23.0701491978883,
0.731258393567419));
#91889=CARTESIAN_POINT('Ctrl Pts',(-4.83404288053355,-23.0701491888037,
0.729452605050674));
#91890=CARTESIAN_POINT('Ctrl Pts',(-4.83404290214876,-23.0701491306227,
0.717887663578479));
#91891=CARTESIAN_POINT('Ctrl Pts',(-4.8333827568176,-23.0703076690209,0.706317278061772));
#91892=CARTESIAN_POINT('Ctrl Pts',(-4.83206209024346,-23.0706011962248,
0.694823310783213));
#91893=CARTESIAN_POINT('Ctrl Pts',(-4.83079606021932,-23.0708825800807,
0.683804853925016));
#91894=CARTESIAN_POINT('Ctrl Pts',(-4.82892281214912,-23.0712882536273,
0.672856898147235));
#91895=CARTESIAN_POINT('Ctrl Pts',(-4.82644653522177,-23.071751636683,0.662048944789373));
#91896=CARTESIAN_POINT('Ctrl Pts',(-4.8241935285967,-23.0721732394055,0.652215476549306));
#91897=CARTESIAN_POINT('Ctrl Pts',(-4.82144110192226,-23.0726427185188,
0.642498228916228));
#91898=CARTESIAN_POINT('Ctrl Pts',(-4.81819933485018,-23.0730692325233,
0.632943252331222));
#91899=CARTESIAN_POINT('Ctrl Pts',(-4.81610621550821,-23.0733446208201,
0.626773868209116));
#91900=CARTESIAN_POINT('Ctrl Pts',(-4.81380922582505,-23.0736013142647,
0.620672026540791));
#91901=CARTESIAN_POINT('Ctrl Pts',(-4.81131367946162,-23.0738037257,0.614647241033059));
#91902=CARTESIAN_POINT('',(-4.81131367923,-21.2742356128,0.614647241129));
#91903=CARTESIAN_POINT('Origin',(-4.73205734534,-23.1742356128,0.423305524947));
#91904=CARTESIAN_POINT('',(-4.80666892645645,-23.0740393995008,0.603433815990868));
#91905=CARTESIAN_POINT('Ctrl Pts',(-4.81131367925832,-23.0738037283007,
0.614647241182803));
#91906=CARTESIAN_POINT('Ctrl Pts',(-4.80976568786345,-23.0738979005228,
0.610910059368051));
#91907=CARTESIAN_POINT('Ctrl Pts',(-4.80821741312739,-23.0739763495673,
0.607172193515546));
#91908=CARTESIAN_POINT('Ctrl Pts',(-4.80666892647,-23.0740393981,0.603433816023));
#91909=CARTESIAN_POINT('',(-4.79748444904916,-23.0742356281333,0.581260526068347));
#91910=CARTESIAN_POINT('Ctrl Pts',(-4.80666892644968,-23.0740394002012,
0.603433815974802));
#91911=CARTESIAN_POINT('Ctrl Pts',(-4.80360593375962,-23.0741641147023,
0.596039097464416));
#91912=CARTESIAN_POINT('Ctrl Pts',(-4.800544079459,-23.0742356283685,0.588647127288019));
#91913=CARTESIAN_POINT('Ctrl Pts',(-4.79748444904758,-23.0742356358,0.581260526069004));
#91914=CARTESIAN_POINT('',(-3.48329194402,-23.0742356128,-2.59148084314));
#91915=CARTESIAN_POINT('',(-6.0279343243,-23.0742356128,3.55182930271));
#91916=CARTESIAN_POINT('',(-3.48329194402,-19.4742356128,-2.59148084314));
#91917=CARTESIAN_POINT('',(-3.48329194402,-21.2742356128,-2.59148084314));
#91918=CARTESIAN_POINT('',(-5.72621658766,-19.4742356128,2.8234182509));
#91919=CARTESIAN_POINT('Origin',(-3.20612808427,-21.2742356128,-2.47667581343));
#91920=CARTESIAN_POINT('Origin',(-3.20612808427,-19.4742356128,-2.47667581343));
#91921=CARTESIAN_POINT('Origin',(-3.20612808427,-23.0742356128,-2.47667581343));
#91922=CARTESIAN_POINT('Origin',(-9.38771846805,-25.4742356128,12.7721409138));
#91923=CARTESIAN_POINT('',(-9.57074430825,-25.4742356128,13.0098414435));
#91924=CARTESIAN_POINT('Origin',(-9.38771846805,-25.4742356128,12.7721409138));
#91925=CARTESIAN_POINT('Origin',(-9.38771846805,-25.4742356128,12.7721409138));
#91926=CARTESIAN_POINT('Origin',(-2.72521192632E-16,-25.4742356128,0.580061096523));
#91927=CARTESIAN_POINT('',(-12.4158608431,-25.4742356128,10.1688558911));
#91928=CARTESIAN_POINT('Origin',(-2.72521192632E-16,-25.4742356128,0.580061096523));
#91929=CARTESIAN_POINT('Origin',(-12.1784264826,-25.4742356128,9.98548488886));
#91930=CARTESIAN_POINT('Origin',(2.4183046301E-16,-21.2742356128,0.580061096523));
#91931=CARTESIAN_POINT('',(-12.4158607189067,-19.6742356128,10.1688560519572));
#91932=CARTESIAN_POINT('',(-3.109463736,-19.6742356128,15.9563357222));
#91933=CARTESIAN_POINT('Origin',(-8.94493678676E-16,-19.6742356128,0.580061096523));
#91934=CARTESIAN_POINT('',(-12.4158608431,-21.2742356128,10.1688558911));
#91935=CARTESIAN_POINT('',(-9.57074430825,-23.4742356128,13.0098414435));
#91936=CARTESIAN_POINT('',(-9.57074430825,-22.5741587422,13.0098414435));
#91937=CARTESIAN_POINT('',(-9.06991786753072,-22.874235391647,13.3798726563422));
#91938=CARTESIAN_POINT('Ctrl Pts',(-9.0699178675,-22.8742351711,13.3798726563));
#91939=CARTESIAN_POINT('Ctrl Pts',(-9.22406041417,-22.8742363569,13.2706476151));
#91940=CARTESIAN_POINT('Ctrl Pts',(-9.3768173424,-22.9427255764,13.1589191215));
#91941=CARTESIAN_POINT('Ctrl Pts',(-9.5056235281,-23.0835945845,13.0599834668));
#91942=CARTESIAN_POINT('Ctrl Pts',(-9.57074430825,-23.2789184576,13.0098414435));
#91943=CARTESIAN_POINT('Ctrl Pts',(-9.57074430825,-23.4742356128,13.0098414435));
#91944=CARTESIAN_POINT('Origin',(4.58869751468E-17,-22.8742356128,0.580061096523));
#91945=CARTESIAN_POINT('',(-2.49776595187,-21.2742356128,16.0674673138));
#91946=CARTESIAN_POINT('Origin',(-1.97861558624E-15,-21.2742356128,0.580061096523));
#91947=CARTESIAN_POINT('',(-3.10946375819683,-20.6742355012,15.9563357201048));
#91948=CARTESIAN_POINT('Ctrl Pts',(-3.10946378033221,-20.6742355012,15.9563357204339));
#91949=CARTESIAN_POINT('Ctrl Pts',(-3.10946378735857,-20.7002248449885,
15.95633571906));
#91950=CARTESIAN_POINT('Ctrl Pts',(-3.10773833558802,-20.7262145171259,
15.9566848789689));
#91951=CARTESIAN_POINT('Ctrl Pts',(-3.10431023879153,-20.7519525807421,
15.9573769620387));
#91952=CARTESIAN_POINT('Ctrl Pts',(-3.10395560128583,-20.7546151901211,
15.9574485582124));
#91953=CARTESIAN_POINT('Ctrl Pts',(-3.10358278308959,-20.7572751232837,
15.9575238125558));
#91954=CARTESIAN_POINT('Ctrl Pts',(-3.10319183705832,-20.7599321129217,
15.9576027102366));
#91955=CARTESIAN_POINT('Ctrl Pts',(-3.099307134996,-20.7863337446062,15.9583866905278));
#91956=CARTESIAN_POINT('Ctrl Pts',(-3.0936290098475,-20.8124388627447,15.9595314025541));
#91957=CARTESIAN_POINT('Ctrl Pts',(-3.08623683217655,-20.8379928558938,
15.9610147519107));
#91958=CARTESIAN_POINT('Ctrl Pts',(-3.07851101700349,-20.8647001993577,
15.9625650505474));
#91959=CARTESIAN_POINT('Ctrl Pts',(-3.06891341716237,-20.8908050127768,
15.9644850853575));
#91960=CARTESIAN_POINT('Ctrl Pts',(-3.05758035100362,-20.9160480560527,
15.9667371363132));
#91961=CARTESIAN_POINT('Ctrl Pts',(-3.04602935090593,-20.9417765209943,
15.9690324940253));
#91962=CARTESIAN_POINT('Ctrl Pts',(-3.03267630960258,-20.9666092779845,
15.9716725056088));
#91963=CARTESIAN_POINT('Ctrl Pts',(-3.01770170425029,-20.9903114039395,
15.9746078088576));
#91964=CARTESIAN_POINT('Ctrl Pts',(-3.0026101605923,-21.0141986223484,15.9775660342055));
#91965=CARTESIAN_POINT('Ctrl Pts',(-2.98587257741445,-21.0369370503983,
15.9808238878688));
#91966=CARTESIAN_POINT('Ctrl Pts',(-2.9676965498713,-21.058332813913,15.9843255532809));
#91967=CARTESIAN_POINT('Ctrl Pts',(-2.96474362937427,-21.0618088203441,
15.9848944421399));
#91968=CARTESIAN_POINT('Ctrl Pts',(-2.96175277307212,-21.0652494956996,
15.9854697605075));
#91969=CARTESIAN_POINT('Ctrl Pts',(-2.95872490069565,-21.0686541357244,
15.9860512642797));
#91970=CARTESIAN_POINT('Ctrl Pts',(-2.93804665294392,-21.0919054426437,
15.9900225277859));
#91971=CARTESIAN_POINT('Ctrl Pts',(-2.91564036809565,-21.1134718480583,
15.9942823225078));
#91972=CARTESIAN_POINT('Ctrl Pts',(-2.89181128846758,-21.1331574400962,
15.9987514051654));
#91973=CARTESIAN_POINT('Ctrl Pts',(-2.87100351620025,-21.1503470807564,
16.0026538493904));
#91974=CARTESIAN_POINT('Ctrl Pts',(-2.8491109162229,-21.1661037147375,16.0067158795856));
#91975=CARTESIAN_POINT('Ctrl Pts',(-2.82633684712334,-21.1803292052124,
16.010887082969));
#91976=CARTESIAN_POINT('Ctrl Pts',(-2.79803654352825,-21.1980065775549,
16.016070448383));
#91977=CARTESIAN_POINT('Ctrl Pts',(-2.76837177274804,-21.2133225213693,
16.0214227358652));
#91978=CARTESIAN_POINT('Ctrl Pts',(-2.73773014859016,-21.2261403216352,
16.0268536353127));
#91979=CARTESIAN_POINT('Ctrl Pts',(-2.7149562079203,-21.235666964912,16.0308900721922));
#91980=CARTESIAN_POINT('Ctrl Pts',(-2.69164267896409,-21.2438149588589,
16.0349700557871));
#91981=CARTESIAN_POINT('Ctrl Pts',(-2.66794852457163,-21.2505464024847,
16.0390594036265));
#91982=CARTESIAN_POINT('Ctrl Pts',(-2.6320530991438,-21.2607441934119,16.0452545553078));
#91983=CARTESIAN_POINT('Ctrl Pts',(-2.59528016107295,-21.2676884801428,
16.051471061566));
#91984=CARTESIAN_POINT('Ctrl Pts',(-2.55817677954374,-21.2713011763122,
16.0576035767246));
#91985=CARTESIAN_POINT('Ctrl Pts',(-2.53810797210176,-21.2732552435907,
16.0609205861394));
#91986=CARTESIAN_POINT('Ctrl Pts',(-2.51794240601556,-21.2742356128,16.0642133111923));
#91987=CARTESIAN_POINT('Ctrl Pts',(-2.49776595187,-21.2742356128,16.0674673138));
#91988=CARTESIAN_POINT('',(-3.109463736,-22.4223864096,15.9563357222));
#91989=CARTESIAN_POINT('Origin',(-9.38771846805,-22.5741587422,12.7721409138));
#91990=CARTESIAN_POINT('',(-9.18405109086,-23.4742356128,12.9924125631));
#91991=CARTESIAN_POINT('Origin',(-9.38771846805,-23.4742356128,12.7721409138));
#91992=CARTESIAN_POINT('',(-9.18405109086,-24.4742356128,12.9924125631));
#91993=CARTESIAN_POINT('Origin',(-3.88971125292,-23.1742356128,8.09716475273));
#91994=CARTESIAN_POINT('',(-5.19285862192,-22.8742356128,9.30207971851));
#91995=CARTESIAN_POINT('',(-6.46706166421,-22.8742356128,10.4802322066));
#91996=CARTESIAN_POINT('',(-5.19285862192,-21.0742356128,9.30207971851));
#91997=CARTESIAN_POINT('',(-5.19285862192,-21.9742356128,9.30207971851));
#91998=CARTESIAN_POINT('',(-8.34854625295,-21.0742356128,12.2198888201));
#91999=CARTESIAN_POINT('',(-6.71750298683,-21.0742356128,10.7117950404));
#92000=CARTESIAN_POINT('',(-8.34854625295,-22.8742356128,12.2198888201));
#92001=CARTESIAN_POINT('',(-8.34854625295,-21.9742356128,12.2198888201));
#92002=CARTESIAN_POINT('',(-8.78908955148,-23.4742356128,12.6272235745));
#92003=CARTESIAN_POINT('Origin',(-8.78908955139227,-22.8742356128972,12.627223574425));
#92004=CARTESIAN_POINT('',(-6.87439641858,-23.4742356128,10.8568617063));
#92005=CARTESIAN_POINT('Origin',(-4.98919124473,-21.9742356128,9.52235136777));
#92006=CARTESIAN_POINT('',(-4.80552303981,-22.8742356128,9.28514683472));
#92007=CARTESIAN_POINT('Origin',(-4.98919124473,-22.8742356128,9.52235136777));
#92008=CARTESIAN_POINT('',(-4.80552303981,-21.0742356128,9.28514683472));
#92009=CARTESIAN_POINT('',(-4.80552303981,-21.2742356128,9.28514683472));
#92010=CARTESIAN_POINT('Origin',(-4.98919124473,-21.0742356128,9.52235136777));
#92011=CARTESIAN_POINT('Origin',(-0.00234331738835,-21.2742356128,3.08191746407));
#92012=CARTESIAN_POINT('',(-1.01141425905,-21.0742356128,10.8621723381));
#92013=CARTESIAN_POINT('',(-1.01141425905,-22.8742356128,10.8621723381));
#92014=CARTESIAN_POINT('',(-1.01141425905,-21.9742356128,10.8621723381));
#92015=CARTESIAN_POINT('Origin',(-0.00234331738803,-21.0742356128,3.08191746407));
#92016=CARTESIAN_POINT('Origin',(-0.00234331738803,-22.8742356128,3.08191746407));
#92017=CARTESIAN_POINT('Origin',(-1.05,-21.9742356128,11.1596805575));
#92018=CARTESIAN_POINT('',(-0.75,-22.8742356128,11.1596805575));
#92019=CARTESIAN_POINT('Origin',(-1.05,-22.8742356128,11.1596805575));
#92020=CARTESIAN_POINT('',(-0.75,-21.0742356128,11.1596805575));
#92021=CARTESIAN_POINT('',(-0.75,-21.9742356128,11.1596805575));
#92022=CARTESIAN_POINT('Origin',(-1.05,-21.0742356128,11.1596805575));
#92023=CARTESIAN_POINT('Origin',(-0.75,-23.1742356128,-8.70195642562));
#92024=CARTESIAN_POINT('',(-0.75,-21.0742356128,14.92922515));
#92025=CARTESIAN_POINT('',(-0.75,-22.8742356128,14.92922515));
#92026=CARTESIAN_POINT('',(-0.75,-21.9742356128,14.92922515));
#92027=CARTESIAN_POINT('',(-0.75,-21.0742356128,12.1167294155));
#92028=CARTESIAN_POINT('',(-0.75,-22.8742356128,2.93538176615));
#92029=CARTESIAN_POINT('Origin',(-8.14487887576,-21.9742356128,12.4401604693));
#92030=CARTESIAN_POINT('',(-8.31471092647,-22.8742356128,12.6874600337));
#92031=CARTESIAN_POINT('Ctrl Pts',(-8.31471092647,-22.8742356128,12.6874600337));
#92032=CARTESIAN_POINT('Ctrl Pts',(-8.32883744679105,-22.8742356128,12.6777586987252));
#92033=CARTESIAN_POINT('Ctrl Pts',(-8.34213871713093,-22.87423561284,12.6668454324847));
#92034=CARTESIAN_POINT('Ctrl Pts',(-8.35440983412802,-22.8742356129023,
12.65487775851));
#92035=CARTESIAN_POINT('Ctrl Pts',(-8.36739587231599,-22.8742356129683,
12.6422128420811));
#92036=CARTESIAN_POINT('Ctrl Pts',(-8.37922775178076,-22.8742356130598,
12.6283672875421));
#92037=CARTESIAN_POINT('Ctrl Pts',(-8.38970962078642,-22.8742356131585,
12.6135677349304));
#92038=CARTESIAN_POINT('Ctrl Pts',(-8.4000338934081,-22.8742356132558,12.5989906956869));
#92039=CARTESIAN_POINT('Ctrl Pts',(-8.40904851996284,-22.8742356133604,
12.5834888008467));
#92040=CARTESIAN_POINT('Ctrl Pts',(-8.4166128270163,-22.8742356134502,12.5673088581972));
#92041=CARTESIAN_POINT('Ctrl Pts',(-8.42435033379277,-22.8742356135419,
12.550758443862));
#92042=CARTESIAN_POINT('Ctrl Pts',(-8.43057011020167,-22.8742356136185,
12.5334991192691));
#92043=CARTESIAN_POINT('Ctrl Pts',(-8.43517222719556,-22.8742356136446,
12.5158179803121));
#92044=CARTESIAN_POINT('Ctrl Pts',(-8.43977434418945,-22.8742356136708,
12.4981368413551));
#92045=CARTESIAN_POINT('Ctrl Pts',(-8.44275875512409,-22.8742356136469,
12.4800345388221));
#92046=CARTESIAN_POINT('Ctrl Pts',(-8.44407743450015,-22.8742356135222,
12.4618116758578));
#92047=CARTESIAN_POINT('Ctrl Pts',(-8.44539020172562,-22.8742356133981,
12.4436705130489));
#92048=CARTESIAN_POINT('Ctrl Pts',(-8.44505217626979,-22.8742356132917,
12.4254099092049));
#92049=CARTESIAN_POINT('Ctrl Pts',(-8.44306743009479,-22.8742356132021,
12.4073301787109));
#92050=CARTESIAN_POINT('Ctrl Pts',(-8.44111043587038,-22.8742356131139,
12.3895032502093));
#92051=CARTESIAN_POINT('Ctrl Pts',(-8.43755252343825,-22.8742356130421,
12.3718527651297));
#92052=CARTESIAN_POINT('Ctrl Pts',(-8.43244743182453,-22.8742356129856,
12.3546611841392));
#92053=CARTESIAN_POINT('Ctrl Pts',(-8.42740525448748,-22.8742356129299,
12.337681469255));
#92054=CARTESIAN_POINT('Ctrl Pts',(-8.42085385627011,-22.8742356128891,
12.3211499566653));
#92055=CARTESIAN_POINT('Ctrl Pts',(-8.41289301572016,-22.8742356128608,
12.3053251052911));
#92056=CARTESIAN_POINT('Ctrl Pts',(-8.40484005245799,-22.8742356128322,
12.2893171290043));
#92057=CARTESIAN_POINT('Ctrl Pts',(-8.39534470099704,-22.8742356128163,
12.2740328873715));
#92058=CARTESIAN_POINT('Ctrl Pts',(-8.38456053591612,-22.8742356128083,
12.259716988749));
#92059=CARTESIAN_POINT('Ctrl Pts',(-8.37377637083519,-22.8742356128002,
12.2454010901265));
#92060=CARTESIAN_POINT('Ctrl Pts',(-8.36170335091807,-22.8742356128,12.2320541243705));
#92061=CARTESIAN_POINT('Ctrl Pts',(-8.34854625295,-22.8742356128,12.2198888201));
#92062=CARTESIAN_POINT('',(-8.31471092647,-21.0742356128,12.6874600337));
#92063=CARTESIAN_POINT('Origin',(-8.14487887576,-21.0742356128,12.4401604693));
#92064=CARTESIAN_POINT('',(-8.31471092647,-22.5742356128,12.6874600337));
#92065=CARTESIAN_POINT('Origin',(-1.05,-21.9742356128,14.92922515));
#92066=CARTESIAN_POINT('',(-1.07189396011,-22.8742356128,15.2284251743));
#92067=CARTESIAN_POINT('Origin',(-1.05,-22.8742356128,14.92922515));
#92068=CARTESIAN_POINT('',(-1.07189396011,-21.0742356128,15.2284251743));
#92069=CARTESIAN_POINT('',(-1.07189396011,-22.5742356128,15.2284251743));
#92070=CARTESIAN_POINT('Origin',(-1.05,-21.0742356128,14.92922515));
#92071=CARTESIAN_POINT('Origin',(2.4183046301E-16,-21.2742356128,0.580061096523));
#92072=CARTESIAN_POINT('Origin',(2.71042223425E-15,-22.8742356128,0.580061096523));
#92073=CARTESIAN_POINT('Origin',(-1.51003344041E-15,-21.0742356128,0.580061096523));
#92074=CARTESIAN_POINT('Origin',(-0.45,-22.8742356128,2.93538176615));
#92075=CARTESIAN_POINT('',(-0.75,-22.8742356128,-6.23438845923));
#92076=CARTESIAN_POINT('Origin',(-0.45,-22.8742356128,-6.23438845923));
#92077=CARTESIAN_POINT('',(-0.45,-23.1742356128,-4.99584562937));
#92078=CARTESIAN_POINT('',(-0.45,-23.1742356128,-5.6151170443));
#92079=CARTESIAN_POINT('',(-0.75,-22.8742356128,-4.99584562937));
#92080=CARTESIAN_POINT('Origin',(-0.45,-22.8742356128,-4.99584562937));
#92081=CARTESIAN_POINT('',(-0.75,-22.8742356128,-5.6151170443));
#92082=CARTESIAN_POINT('Origin',(-7.40416713263E-16,-22.8742356128,0.729452270839));
#92083=CARTESIAN_POINT('',(-0.935307608221,-23.1742356128,5.53218022249));
#92084=CARTESIAN_POINT('',(-0.992653804111,-22.8742356128,5.82664824081));
#92085=CARTESIAN_POINT('Origin',(-0.935307608221,-22.8742356128,5.53218022249));
#92086=CARTESIAN_POINT('',(-1.19254592572,-22.8742356128,5.78361912069));
#92087=CARTESIAN_POINT('Origin',(3.67394039744E-17,-22.8742356128,0.729452270839));
#92088=CARTESIAN_POINT('',(-1.12365184404,-23.1742356128,5.49163692002));
#92089=CARTESIAN_POINT('Origin',(-1.12365184404,-22.8742356128,5.49163692002));
#92090=CARTESIAN_POINT('Origin',(-3.42702565972E-16,-23.1742356128,0.729452270839));
#92091=CARTESIAN_POINT('Origin',(-1.05,-22.8742356128,6.12111625914));
#92092=CARTESIAN_POINT('',(-0.45,-23.1742356128,6.12111625914));
#92093=CARTESIAN_POINT('',(-0.75,-22.8742356128,6.12111625914));
#92094=CARTESIAN_POINT('Origin',(-0.45,-22.8742356128,6.12111625914));
#92095=CARTESIAN_POINT('Origin',(-1.05,-22.8742356128,6.12111625914));
#92096=CARTESIAN_POINT('Origin',(-1.05,-23.1742356128,6.12111625914));
#92097=CARTESIAN_POINT('Origin',(-0.45,-22.8742356128,2.93538176615));
#92098=CARTESIAN_POINT('',(-0.45,-23.1742356128,9.0358656718));
#92099=CARTESIAN_POINT('',(-0.75,-22.8742356128,9.0358656718));
#92100=CARTESIAN_POINT('Origin',(-0.45,-22.8742356128,9.0358656718));
#92101=CARTESIAN_POINT('',(-0.75,-22.8742356128,7.57849096547));
#92102=CARTESIAN_POINT('',(-0.45,-23.1742356128,7.57849096547));
#92103=CARTESIAN_POINT('Origin',(-1.05,-22.8742356128,9.0358656718));
#92104=CARTESIAN_POINT('',(-1.15397857793,-23.1742356128,9.62678737163));
#92105=CARTESIAN_POINT('',(-1.10198928897,-22.8742356128,9.33132652171));
#92106=CARTESIAN_POINT('Origin',(-1.15397857793,-22.8742356128,9.62678737163));
#92107=CARTESIAN_POINT('Origin',(-1.05,-22.8742356128,9.0358656718));
#92108=CARTESIAN_POINT('Origin',(-1.05,-23.1742356128,9.0358656718));
#92109=CARTESIAN_POINT('Origin',(-0.00234331738835,-22.8742356128,3.08191746407));
#92110=CARTESIAN_POINT('',(-3.7572334818,-23.1742356128,8.56483509371));
#92111=CARTESIAN_POINT('',(-3.58772315463,-22.8742356128,8.31731489457));
#92112=CARTESIAN_POINT('Origin',(-3.7572334818,-22.8742356128,8.56483509371));
#92113=CARTESIAN_POINT('Origin',(-0.00234331738835,-22.8742356128,3.08191746407));
#92114=CARTESIAN_POINT('Origin',(-0.00234331738835,-23.1742356128,3.08191746407));
#92115=CARTESIAN_POINT('Origin',(-1.2614400074,-22.8742356128,6.07560132137));
#92116=CARTESIAN_POINT('',(-1.46510738459,-22.8742356128,5.8553296721));
#92117=CARTESIAN_POINT('Origin',(-1.2614400074,-22.8742356128,6.07560132137));
#92118=CARTESIAN_POINT('',(-1.66877476178,-23.1742356128,5.63505802284));
#92119=CARTESIAN_POINT('Origin',(-1.66877476178,-22.8742356128,5.63505802284));
#92120=CARTESIAN_POINT('Origin',(-1.2614400074,-23.1742356128,6.07560132137));
#92121=CARTESIAN_POINT('Origin',(-3.41821282746,-22.8742356128,8.06979469543));
#92122=CARTESIAN_POINT('',(-3.82554758184,-23.1742356128,7.6292513969));
#92123=CARTESIAN_POINT('',(-3.62188020465,-22.8742356128,7.84952304616));
#92124=CARTESIAN_POINT('Origin',(-3.82554758184,-22.8742356128,7.6292513969));
#92125=CARTESIAN_POINT('Origin',(-3.41821282746,-22.8742356128,8.06979469543));
#92126=CARTESIAN_POINT('Origin',(-3.41821282746,-23.1742356128,8.06979469543));
#92127=CARTESIAN_POINT('Origin',(-6.6707290414,-22.8742356128,10.2599605573));
#92128=CARTESIAN_POINT('',(-2.54349379462,-22.8742356128,6.85242635913));
#92129=CARTESIAN_POINT('',(-2.74716117181,-23.1742356128,6.63215470987));
#92130=CARTESIAN_POINT('Origin',(-0.00234331738835,-22.8742356128,3.08191746407));
#92131=CARTESIAN_POINT('',(-6.21380646358,-22.8742356128,1.78497474518));
#92132=CARTESIAN_POINT('',(-6.50747329887,-23.1742356128,1.72365761992));
#92133=CARTESIAN_POINT('Origin',(-6.50747329887,-22.8742356128,1.72365761992));
#92134=CARTESIAN_POINT('',(-6.03449750111,-23.1742356128,0.293602240855));
#92135=CARTESIAN_POINT('Origin',(-0.00234331738835,-23.1742356128,3.08191746407));
#92136=CARTESIAN_POINT('',(-5.76218263052,-22.8742356128,0.419477620705));
#92137=CARTESIAN_POINT('Origin',(-6.03449750111,-22.8742356128,0.293602240855));
#92138=CARTESIAN_POINT('Origin',(-0.00234331738835,-22.8742356128,3.08191746407));
#92139=CARTESIAN_POINT('Ctrl Pts',(-4.88987240374,-23.1742356097,0.542992178472));
#92140=CARTESIAN_POINT('Ctrl Pts',(-4.86084787859,-23.1742356067,0.555014532813));
#92141=CARTESIAN_POINT('Ctrl Pts',(-4.83182335285,-23.1618986036,0.567036885942));
#92142=CARTESIAN_POINT('Ctrl Pts',(-4.80888237522,-23.137067473,0.576539351728));
#92143=CARTESIAN_POINT('Ctrl Pts',(-4.79748446133,-23.1056515569,0.581260521919));
#92144=CARTESIAN_POINT('Ctrl Pts',(-4.79748444899,-23.0742356355,0.58126052593));
#92145=CARTESIAN_POINT('Ctrl Pts',(-4.89332536714,-23.1742356121,0.548536687929));
#92146=CARTESIAN_POINT('Ctrl Pts',(-4.86410343804,-23.1745712361,0.560640808584));
#92147=CARTESIAN_POINT('Ctrl Pts',(-4.83473862243,-23.1624020478,0.572744367244));
#92148=CARTESIAN_POINT('Ctrl Pts',(-4.81143971624,-23.1374948049,0.582274826956));
#92149=CARTESIAN_POINT('Ctrl Pts',(-4.79983297467,-23.1058652194,0.58693034427));
#92150=CARTESIAN_POINT('Ctrl Pts',(-4.79977917182,-23.07423563,0.586800476896));
#92151=CARTESIAN_POINT('Ctrl Pts',(-4.89674616735,-23.1741819495,0.554055341853));
#92152=CARTESIAN_POINT('Ctrl Pts',(-4.86733644658,-23.174853061,0.566241584166));
#92153=CARTESIAN_POINT('Ctrl Pts',(-4.83763986632,-23.1628553414,0.578430209837));
#92154=CARTESIAN_POINT('Ctrl Pts',(-4.81398926394,-23.1378767526,0.587995632443));
#92155=CARTESIAN_POINT('Ctrl Pts',(-4.80217889215,-23.1060383,0.59259390235));
#92156=CARTESIAN_POINT('Ctrl Pts',(-4.80207503274,-23.0741998456,0.592343175471));
#92157=CARTESIAN_POINT('Ctrl Pts',(-4.90013262037,-23.1740815975,0.559548447604));
#92158=CARTESIAN_POINT('Ctrl Pts',(-4.87054456006,-23.1750868242,0.571816367149));
#92159=CARTESIAN_POINT('Ctrl Pts',(-4.84052526678,-23.1632633043,0.584093271995));
#92160=CARTESIAN_POINT('Ctrl Pts',(-4.816529999,-23.1382178393,0.593700396416));
#92161=CARTESIAN_POINT('Ctrl Pts',(-4.8045217228,-23.1061753876,0.59825000772));
#92162=CARTESIAN_POINT('Ctrl Pts',(-4.80437168194,-23.074132936,0.597887777111));
#92163=CARTESIAN_POINT('Ctrl Pts',(-4.9034828985,-23.1739412939,0.565017049189));
#92164=CARTESIAN_POINT('Ctrl Pts',(-4.87372566794,-23.1752779938,0.577365441326));
#92165=CARTESIAN_POINT('Ctrl Pts',(-4.84339318826,-23.1636304163,0.589733124501));
#92166=CARTESIAN_POINT('Ctrl Pts',(-4.81906111591,-23.1385222645,0.599388337029));
#92167=CARTESIAN_POINT('Ctrl Pts',(-4.80686117712,-23.1062808323,0.603897950179));
#92168=CARTESIAN_POINT('Ctrl Pts',(-4.80666892648,-23.0740394002,0.603433816048));
#92169=CARTESIAN_POINT('',(-4.90348289994913,-23.1739412934337,0.565017049040251));
#92170=CARTESIAN_POINT('Origin',(-4.8983948094157,-23.0747913407119,0.56545239354252));
#92171=CARTESIAN_POINT('',(-4.88987240399273,-23.17423561125,0.542992182694935));
#92172=CARTESIAN_POINT('Ctrl Pts',(-4.9034828985,-23.1739412939,0.565017049189));
#92173=CARTESIAN_POINT('Ctrl Pts',(-4.89901586077995,-23.1741283653771,
0.557725581051751));
#92174=CARTESIAN_POINT('Ctrl Pts',(-4.89447635549808,-23.1742356128882,
0.550384858685629));
#92175=CARTESIAN_POINT('Ctrl Pts',(-4.88987240449,-23.1742356097,0.542992182489001));
#92176=CARTESIAN_POINT('Origin',(-4.8892191322679,-23.0749427012436,0.543262776949538));
#92177=CARTESIAN_POINT('Origin',(-5.48986775992,-22.8742356128,0.545353000555));
#92178=CARTESIAN_POINT('',(-5.1900363009,-22.8742356128,0.55540766038));
#92179=CARTESIAN_POINT('Origin',(-4.89020484189,-22.8742356128,0.565462320206));
#92180=CARTESIAN_POINT('Origin',(-5.48986775992,-22.8742356128,0.545353000555));
#92181=CARTESIAN_POINT('Origin',(-5.48986775992,-23.1742356128,0.545353000555));
#92182=CARTESIAN_POINT('Ctrl Pts',(-4.91026666705,-23.1735877712,0.882730576443));
#92183=CARTESIAN_POINT('Ctrl Pts',(-4.88018105031,-23.1755928789,0.870218178727));
#92184=CARTESIAN_POINT('Ctrl Pts',(-4.84922086626,-23.1643051888,0.857678480686));
#92185=CARTESIAN_POINT('Ctrl Pts',(-4.82420272303,-23.13907693,0.847951337039));
#92186=CARTESIAN_POINT('Ctrl Pts',(-4.81160444157,-23.1064403276,0.843555347761));
#92187=CARTESIAN_POINT('Ctrl Pts',(-4.81131367923,-23.073803724,0.844257300549));
#92188=CARTESIAN_POINT('Ctrl Pts',(-4.90607244846,-23.1738495633,0.889624687643));
#92189=CARTESIAN_POINT('Ctrl Pts',(-4.87618496465,-23.1754360605,0.877215340784));
#92190=CARTESIAN_POINT('Ctrl Pts',(-4.84561274758,-23.1639199413,0.864783368054));
#92191=CARTESIAN_POINT('Ctrl Pts',(-4.82102256688,-23.1387632801,0.855100421724));
#92192=CARTESIAN_POINT('Ctrl Pts',(-4.80867334759,-23.1063707663,0.8506316329));
#92193=CARTESIAN_POINT('Ctrl Pts',(-4.80844479873,-23.0739782513,0.85118339076));
#92194=CARTESIAN_POINT('Ctrl Pts',(-4.90188345783,-23.1740438603,0.89651618735));
#92195=CARTESIAN_POINT('Ctrl Pts',(-4.87220155195,-23.1752205389,0.884207133034));
#92196=CARTESIAN_POINT('Ctrl Pts',(-4.84201706368,-23.1634854888,0.871880564251));
#92197=CARTESIAN_POINT('Ctrl Pts',(-4.81784840655,-23.1384044972,0.862242184947));
#92198=CARTESIAN_POINT('Ctrl Pts',(-4.80574358799,-23.1062561396,0.857704695525));
#92199=CARTESIAN_POINT('Ctrl Pts',(-4.80557512116,-23.0741077812,0.85811140527));
#92200=CARTESIAN_POINT('Ctrl Pts',(-4.89770009156,-23.1741721033,0.903404516156));
#92201=CARTESIAN_POINT('Ctrl Pts',(-4.86823079014,-23.1749477659,0.891193246426));
#92202=CARTESIAN_POINT('Ctrl Pts',(-4.83843359789,-23.1630030668,0.878969965755));
#92203=CARTESIAN_POINT('Ctrl Pts',(-4.81468020651,-23.1380016463,0.869376522739));
#92204=CARTESIAN_POINT('Ctrl Pts',(-4.802815301,-23.1060974606,0.864774202654));
#92205=CARTESIAN_POINT('Ctrl Pts',(-4.80270489088,-23.0741932746,0.865040754137));
#92206=CARTESIAN_POINT('Ctrl Pts',(-4.89352269524,-23.1742356128,0.91028919283));
#92207=CARTESIAN_POINT('Ctrl Pts',(-4.86427263762,-23.1746190563,0.898173422263));
#92208=CARTESIAN_POINT('Ctrl Pts',(-4.83486214645,-23.162473773,0.886051492275));
#92209=CARTESIAN_POINT('Ctrl Pts',(-4.81151792338,-23.1375556813,0.876503354045));
#92210=CARTESIAN_POINT('Ctrl Pts',(-4.79988860489,-23.1058956471,0.871839869986));
#92211=CARTESIAN_POINT('Ctrl Pts',(-4.79983432123,-23.0742356128,0.871970922337));
#92212=CARTESIAN_POINT('Ctrl Pts',(-4.88935151015,-23.1742356128,0.917169903738));
#92213=CARTESIAN_POINT('Ctrl Pts',(-4.86032697863,-23.1742356128,0.90514754914));
#92214=CARTESIAN_POINT('Ctrl Pts',(-4.83130244711,-23.1618986073,0.893125194543));
#92215=CARTESIAN_POINT('Ctrl Pts',(-4.80836146378,-23.1370674659,0.883622728112));
#92216=CARTESIAN_POINT('Ctrl Pts',(-4.7969635569,-23.1056515394,0.878901560502));
#92217=CARTESIAN_POINT('Ctrl Pts',(-4.7969635569,-23.0742356128,0.878901560502));
#92218=CARTESIAN_POINT('',(-4.88935151015,-23.1742356128,0.917169903738));
#92219=CARTESIAN_POINT('Origin',(-4.88869823765389,-23.0749427099031,0.916899309412879));
#92220=CARTESIAN_POINT('',(-4.91026667169405,-23.1735877810644,0.882730576328867));
#92221=CARTESIAN_POINT('Origin',(-4.78300704958758,-22.686919287924,1.13838380064551));
#92222=CARTESIAN_POINT('Origin',(-4.90303610019935,-23.0745775166647,0.882230481220324));
#92223=CARTESIAN_POINT('Ctrl Pts',(-4.91032411032826,-23.1735838288474,
0.882801380280842));
#92224=CARTESIAN_POINT('Ctrl Pts',(-4.88022671384046,-23.1756160163728,
0.870279875408482));
#92225=CARTESIAN_POINT('Ctrl Pts',(-4.84924393654162,-23.1643433388717,
0.857726517801697));
#92226=CARTESIAN_POINT('Ctrl Pts',(-4.82420252529952,-23.1391099370352,
0.847986365762712));
#92227=CARTESIAN_POINT('Ctrl Pts',(-4.81159271910536,-23.1064573061117,
0.843583836626828));
#92228=CARTESIAN_POINT('Ctrl Pts',(-4.81130199410985,-23.0738046752881,
0.844285506864908));
#92229=CARTESIAN_POINT('Ctrl Pts',(-4.94434742826404,-23.171453756981,0.826898793291758));
#92230=CARTESIAN_POINT('Ctrl Pts',(-4.91067807699736,-23.1770055230639,
0.818105216460323));
#92231=CARTESIAN_POINT('Ctrl Pts',(-4.87457600571307,-23.167652358011,0.809242452726758));
#92232=CARTESIAN_POINT('Ctrl Pts',(-4.8445619038014,-23.1418126887911,0.802685366669083));
#92233=CARTESIAN_POINT('Ctrl Pts',(-4.8293242397813,-23.1071017824707,0.800486968739525));
#92234=CARTESIAN_POINT('Ctrl Pts',(-4.82875126200463,-23.0723908765014,
0.802171370483634));
#92235=CARTESIAN_POINT('Ctrl Pts',(-4.96420776206773,-23.1658532222896,
0.763665118766352));
#92236=CARTESIAN_POINT('Ctrl Pts',(-4.92841514195084,-23.174432018286,0.760045081408559));
#92237=CARTESIAN_POINT('Ctrl Pts',(-4.88880992409556,-23.1670369908996,
0.756370657617406));
#92238=CARTESIAN_POINT('Ctrl Pts',(-4.85536837092642,-23.1410196792605,
0.753866960469878));
#92239=CARTESIAN_POINT('Ctrl Pts',(-4.83885806030122,-23.1048418671394,
0.753535150521697));
#92240=CARTESIAN_POINT('Ctrl Pts',(-4.83896248410945,-23.0686637734685,
0.754906483839526));
#92241=CARTESIAN_POINT('Ctrl Pts',(-4.9642104382863,-23.1658530695551,0.695241429168574));
#92242=CARTESIAN_POINT('Ctrl Pts',(-4.92841670517027,-23.1744321920304,
0.698861429442802));
#92243=CARTESIAN_POINT('Ctrl Pts',(-4.88881020696589,-23.1670369970505,
0.702535807890803));
#92244=CARTESIAN_POINT('Ctrl Pts',(-4.85536781453051,-23.141018906302,0.705039301384199));
#92245=CARTESIAN_POINT('Ctrl Pts',(-4.83885769137182,-23.1048402717239,
0.705370657456912));
#92246=CARTESIAN_POINT('Ctrl Pts',(-4.83896308256911,-23.0686617900272,
0.703998762393385));
#92247=CARTESIAN_POINT('Ctrl Pts',(-4.94434734509692,-23.1714537621886,
0.632005686936182));
#92248=CARTESIAN_POINT('Ctrl Pts',(-4.91067802717319,-23.1770055181565,
0.640799265178577));
#92249=CARTESIAN_POINT('Ctrl Pts',(-4.87457599443822,-23.167652357672,0.649662030565025));
#92250=CARTESIAN_POINT('Ctrl Pts',(-4.84456191778467,-23.1418127111943,
0.656219122931779));
#92251=CARTESIAN_POINT('Ctrl Pts',(-4.82932424873922,-23.107101829449,0.658417534179115));
#92252=CARTESIAN_POINT('Ctrl Pts',(-4.82875124236076,-23.0723909352002,
0.656733148919665));
#92253=CARTESIAN_POINT('Ctrl Pts',(-4.91032411262656,-23.1735838286412,
0.576103162589323));
#92254=CARTESIAN_POINT('Ctrl Pts',(-4.88022671491257,-23.1756160164777,
0.588624667473674));
#92255=CARTESIAN_POINT('Ctrl Pts',(-4.84924393621136,-23.1643433387761,
0.601178025081577));
#92256=CARTESIAN_POINT('Ctrl Pts',(-4.82420252410613,-23.1391099360228,
0.61091817693581));
#92257=CARTESIAN_POINT('Ctrl Pts',(-4.81159271820302,-23.1064573042801,
0.615320705592525));
#92258=CARTESIAN_POINT('Ctrl Pts',(-4.81130199435762,-23.0738046729465,
0.614619034738959));
#92259=CARTESIAN_POINT('',(-4.91026668200588,-23.1735877855957,0.576173964916216));
#92260=CARTESIAN_POINT('Ctrl Pts',(-4.91026667429727,-23.1735877859444,
0.882730577727296));
#92261=CARTESIAN_POINT('Ctrl Pts',(-4.91879411776458,-23.1730555309431,
0.868713877246766));
#92262=CARTESIAN_POINT('Ctrl Pts',(-4.92622758773466,-23.1722660176644,
0.854117529858202));
#92263=CARTESIAN_POINT('Ctrl Pts',(-4.93243211502344,-23.171462420821,0.839089304309771));
#92264=CARTESIAN_POINT('Ctrl Pts',(-4.93811142443016,-23.1707268490523,
0.825333229309873));
#92265=CARTESIAN_POINT('Ctrl Pts',(-4.9427623803931,-23.1699802976463,0.811215540434539));
#92266=CARTESIAN_POINT('Ctrl Pts',(-4.94629784193977,-23.1693715096677,
0.796856553293824));
#92267=CARTESIAN_POINT('Ctrl Pts',(-4.94857306719722,-23.1689797277838,
0.787615912494103));
#92268=CARTESIAN_POINT('Ctrl Pts',(-4.95038657496731,-23.1686442133483,
0.778275464280113));
#92269=CARTESIAN_POINT('Ctrl Pts',(-4.95171571795756,-23.1683929962434,
0.768868428703813));
#92270=CARTESIAN_POINT('Ctrl Pts',(-4.95361365836277,-23.1680342725415,
0.7554357182697));
#92271=CARTESIAN_POINT('Ctrl Pts',(-4.95454013240377,-23.1678467144829,
0.741880779640089));
#92272=CARTESIAN_POINT('Ctrl Pts',(-4.95448697348868,-23.1678572110641,
0.7283291771088));
#92273=CARTESIAN_POINT('Ctrl Pts',(-4.95447471934027,-23.1678596307272,
0.725205273086987));
#92274=CARTESIAN_POINT('Ctrl Pts',(-4.95441038067712,-23.1678723584511,
0.722081549228793));
#92275=CARTESIAN_POINT('Ctrl Pts',(-4.95429380538934,-23.1678953318367,
0.718959547665966));
#92276=CARTESIAN_POINT('Ctrl Pts',(-4.9537680339869,-23.1679989451272,0.70487886923606));
#92277=CARTESIAN_POINT('Ctrl Pts',(-4.95214944036737,-23.1683220299151,
0.690852161339055));
#92278=CARTESIAN_POINT('Ctrl Pts',(-4.94950342663415,-23.1688041380817,
0.676996407633137));
#92279=CARTESIAN_POINT('Ctrl Pts',(-4.94672280729924,-23.1693107716162,
0.662435796638999));
#92280=CARTESIAN_POINT('Ctrl Pts',(-4.94280686905793,-23.1699924763006,
0.648064082382267));
#92281=CARTESIAN_POINT('Ctrl Pts',(-4.93782902584385,-23.1707193115796,
0.6340127869156));
#92282=CARTESIAN_POINT('Ctrl Pts',(-4.93252157779082,-23.1714942738113,
0.619031093527582));
#92283=CARTESIAN_POINT('Ctrl Pts',(-4.92600560665533,-23.1723197923502,
0.604413876753238));
#92284=CARTESIAN_POINT('Ctrl Pts',(-4.91838360323196,-23.1729819475197,
0.590313280824429));
#92285=CARTESIAN_POINT('Ctrl Pts',(-4.91580296743621,-23.173206138095,0.585539141982699));
#92286=CARTESIAN_POINT('Ctrl Pts',(-4.91309574645361,-23.173411204469,0.580824151361539));
#92287=CARTESIAN_POINT('Ctrl Pts',(-4.91026668277928,-23.173587785389,0.576173965249023));
#92288=CARTESIAN_POINT('Origin',(-4.90303611057442,-23.0745775160784,0.576674065905074));
#92289=CARTESIAN_POINT('Ctrl Pts',(-4.90348290199,-23.1739412927,0.565017048926));
#92290=CARTESIAN_POINT('Ctrl Pts',(-4.87372566996,-23.1752779928,0.577365441579));
#92291=CARTESIAN_POINT('Ctrl Pts',(-4.84339318716,-23.1636304143,0.589733124946));
#92292=CARTESIAN_POINT('Ctrl Pts',(-4.81906111615,-23.1385222628,0.599388337346));
#92293=CARTESIAN_POINT('Ctrl Pts',(-4.80686117638,-23.1062808303,0.603897950601));
#92294=CARTESIAN_POINT('Ctrl Pts',(-4.80666892647,-23.0740393981,0.603433816023));
#92295=CARTESIAN_POINT('Ctrl Pts',(-4.90574226327,-23.1738467182,0.568735011834));
#92296=CARTESIAN_POINT('Ctrl Pts',(-4.87587305899,-23.175403149,0.581137165172));
#92297=CARTESIAN_POINT('Ctrl Pts',(-4.84533146364,-23.163872265,0.593561421472));
#92298=CARTESIAN_POINT('Ctrl Pts',(-4.82077291013,-23.13872269,0.603240740434));
#92299=CARTESIAN_POINT('Ctrl Pts',(-4.80844177844,-23.1063495195,0.607713860274));
#92300=CARTESIAN_POINT('Ctrl Pts',(-4.80821741307,-23.0739763492,0.607172193377));
#92301=CARTESIAN_POINT('Ctrl Pts',(-4.90800356168,-23.1737290414,0.572454037538));
#92302=CARTESIAN_POINT('Ctrl Pts',(-4.87802484771,-23.1755082749,0.584910832115));
#92303=CARTESIAN_POINT('Ctrl Pts',(-4.84727399761,-23.164097327,0.597392404899));
#92304=CARTESIAN_POINT('Ctrl Pts',(-4.82248677013,-23.1389076984,0.607095701029));
#92305=CARTESIAN_POINT('Ctrl Pts',(-4.81002287785,-23.1064027985,0.611530970941));
#92306=CARTESIAN_POINT('Ctrl Pts',(-4.80976568781,-23.0738978985,0.610910059239));
#92307=CARTESIAN_POINT('Ctrl Pts',(-4.91026668053,-23.173587786,0.576173964221));
#92308=CARTESIAN_POINT('Ctrl Pts',(-4.88018105713,-23.1755928936,0.588686362821));
#92309=CARTESIAN_POINT('Ctrl Pts',(-4.84922086635,-23.164305202,0.601226061781));
#92310=CARTESIAN_POINT('Ctrl Pts',(-4.82420271933,-23.1390769396,0.610953205986));
#92311=CARTESIAN_POINT('Ctrl Pts',(-4.81160443804,-23.1064403339,0.615349194972));
#92312=CARTESIAN_POINT('Ctrl Pts',(-4.81131367927,-23.0738037283,0.614647241211));
#92313=CARTESIAN_POINT('Ctrl Pts',(-4.91026668053,-23.173587786,0.576173964221));
#92314=CARTESIAN_POINT('Ctrl Pts',(-4.90800356173676,-23.1737290413966,
0.572454037692303));
#92315=CARTESIAN_POINT('Ctrl Pts',(-4.90574226337073,-23.1738467181957,
0.568735011999752));
#92316=CARTESIAN_POINT('Ctrl Pts',(-4.90348290200454,-23.1739412926994,
0.56501704894993));
#92317=CARTESIAN_POINT('Origin',(3.67394039744E-17,-22.8742356128,0.729452270839));
#92318=CARTESIAN_POINT('',(-4.79074910795,-23.1742356128,1.72429853244));
#92319=CARTESIAN_POINT('Origin',(-3.42702565972E-16,-23.1742356128,0.729452270839));
#92320=CARTESIAN_POINT('',(-5.08448267152,-22.8742356128,1.78529520144));
#92321=CARTESIAN_POINT('Origin',(-4.79074910795,-22.8742356128,1.72429853244));
#92322=CARTESIAN_POINT('Origin',(3.67394039744E-17,-22.8742356128,0.729452270839));
#92323=CARTESIAN_POINT('Origin',(-5.92013962829,-22.8742356128,1.84629187045));
#92324=CARTESIAN_POINT('',(-5.92013962829,-22.8742356128,2.14629187045));
#92325=CARTESIAN_POINT('',(-5.92013962829,-23.1742356128,2.44629187045));
#92326=CARTESIAN_POINT('Origin',(-5.92013962829,-22.8742356128,2.44629187045));
#92327=CARTESIAN_POINT('Origin',(-5.92013962829,-23.1742356128,1.84629187045));
#92328=CARTESIAN_POINT('Origin',(-5.92013962829,-22.8742356128,1.84629187045));
#92329=CARTESIAN_POINT('Origin',(-5.3782162351,-22.8742356128,1.84629187045));
#92330=CARTESIAN_POINT('',(-5.3782162351,-23.1742356128,2.44629187045));
#92331=CARTESIAN_POINT('Origin',(-5.3782162351,-23.1742356128,1.84629187045));
#92332=CARTESIAN_POINT('',(-5.3782162351,-22.8742356128,2.14629187045));
#92333=CARTESIAN_POINT('Origin',(-5.3782162351,-22.8742356128,2.44629187045));
#92334=CARTESIAN_POINT('Origin',(-5.3782162351,-22.8742356128,1.84629187045));
#92335=CARTESIAN_POINT('Origin',(-6.6707290414,-22.8742356128,2.44629187045));
#92336=CARTESIAN_POINT('',(-5.6491779317,-23.1742356128,2.44629187045));
#92337=CARTESIAN_POINT('',(-5.6491779317,-22.8742356128,2.14629187045));
#92338=CARTESIAN_POINT('Ctrl Pts',(-3.36369872841,-23.1735877712,4.30991925785));
#92339=CARTESIAN_POINT('Ctrl Pts',(-3.35127258606,-23.1755928789,4.27979791296));
#92340=CARTESIAN_POINT('Ctrl Pts',(-3.33824733549,-23.1643051888,4.24903885135));
#92341=CARTESIAN_POINT('Ctrl Pts',(-3.327434966,-23.13907693,4.22447022338));
#92342=CARTESIAN_POINT('Ctrl Pts',(-3.32163506958,-23.1064403276,4.21245345931));
#92343=CARTESIAN_POINT('Ctrl Pts',(-3.32093311398,-23.073803724,4.21274421486));
#92344=CARTESIAN_POINT('Ctrl Pts',(-3.35585809522,-23.1738495633,4.31182837022));
#92345=CARTESIAN_POINT('Ctrl Pts',(-3.34349918606,-23.1754360605,4.28191999443));
#92346=CARTESIAN_POINT('Ctrl Pts',(-3.33067209627,-23.1639199413,4.2515114402));
#92347=CARTESIAN_POINT('Ctrl Pts',(-3.32013108976,-23.1387632801,4.22727667967));
#92348=CARTESIAN_POINT('Ctrl Pts',(-3.31455878394,-23.1063707663,4.21538455208));
#92349=CARTESIAN_POINT('Ctrl Pts',(-3.31400702377,-23.0739782513,4.21561309536));
#92350=CARTESIAN_POINT('Ctrl Pts',(-3.34802300536,-23.1740438603,4.31373933271));
#92351=CARTESIAN_POINT('Ctrl Pts',(-3.33573854421,-23.1752205389,4.28404724001));
#92352=CARTESIAN_POINT('Ctrl Pts',(-3.32311108825,-23.1634854888,4.2539873833));
#92353=CARTESIAN_POINT('Ctrl Pts',(-3.31283663026,-23.1384044972,4.23008219858));
#92354=CARTESIAN_POINT('Ctrl Pts',(-3.30748572051,-23.1062561396,4.21831430975));
#92355=CARTESIAN_POINT('Ctrl Pts',(-3.30707900926,-23.0741077812,4.21848277293));
#92356=CARTESIAN_POINT('Ctrl Pts',(-3.34019413469,-23.1741721033,4.31565203007));
#92357=CARTESIAN_POINT('Ctrl Pts',(-3.32799086345,-23.1749477659,4.28617941556));
#92358=CARTESIAN_POINT('Ctrl Pts',(-3.31556423141,-23.1630030668,4.25646645421));
#92359=CARTESIAN_POINT('Ctrl Pts',(-3.3055516359,-23.1380016463,4.23288668148));
#92360=CARTESIAN_POINT('Ctrl Pts',(-3.30041621249,-23.1060974606,4.22124259459));
#92361=CARTESIAN_POINT('Ctrl Pts',(-3.30014966039,-23.0741932746,4.22135300321));
#92362=CARTESIAN_POINT('Ctrl Pts',(-3.33237206787,-23.1742356128,4.31756636636));
#92363=CARTESIAN_POINT('Ctrl Pts',(-3.3202562973,-23.1746190563,4.28831630874));
#92364=CARTESIAN_POINT('Ctrl Pts',(-3.30803143845,-23.162473773,4.2589484521));
#92365=CARTESIAN_POINT('Ctrl Pts',(-3.29827613331,-23.1375556813,4.23569004038));
#92366=CARTESIAN_POINT('Ctrl Pts',(-3.29335054454,-23.1058956471,4.22416928921));
#92367=CARTESIAN_POINT('Ctrl Pts',(-3.29321949219,-23.0742356128,4.22422357287));
#92368=CARTESIAN_POINT('Ctrl Pts',(-3.32455719726,-23.1742356128,4.31948229044));
#92369=CARTESIAN_POINT('Ctrl Pts',(-3.31253484266,-23.1742356128,4.29045775892));
#92370=CARTESIAN_POINT('Ctrl Pts',(-3.30051248807,-23.1618986073,4.2614332274));
#92371=CARTESIAN_POINT('Ctrl Pts',(-3.29101002164,-23.1370674659,4.23849224407));
#92372=CARTESIAN_POINT('Ctrl Pts',(-3.28628885403,-23.1056515394,4.22709433719));
#92373=CARTESIAN_POINT('Ctrl Pts',(-3.28628885403,-23.0742356128,4.22709433719));
#92374=CARTESIAN_POINT('',(-3.32455719726,-23.1742356128,4.31948229044));
#92375=CARTESIAN_POINT('Origin',(-3.32428660293348,-23.0749427099053,4.31882901794046));
#92376=CARTESIAN_POINT('',(-3.36369873177259,-23.1735877810642,4.30991926105255));
#92377=CARTESIAN_POINT('Origin',(-3.09293905505095,-22.6869204620332,4.40070704808497));
#92378=CARTESIAN_POINT('Origin',(-3.3589395662952,-23.0745775166517,4.30445285428866));
#92379=CARTESIAN_POINT('Ctrl Pts',(-3.36368928106124,-23.1735838288475,
4.31000994225207));
#92380=CARTESIAN_POINT('Ctrl Pts',(-3.35126124891729,-23.1756160163725,
4.27987382809444));
#92381=CARTESIAN_POINT('Ctrl Pts',(-3.33822968127554,-23.1643433388712,
4.2490891318676));
#92382=CARTESIAN_POINT('Ctrl Pts',(-3.32741005713184,-23.1391099370348,
4.22449485261762));
#92383=CARTESIAN_POINT('Ctrl Pts',(-3.32160663587613,-23.1064573061115,
4.21246531493779));
#92384=CARTESIAN_POINT('Ctrl Pts',(-3.32090490647545,-23.0738046752881,
4.2127558971094));
#92385=CARTESIAN_POINT('Ctrl Pts',(-3.42727649823542,-23.1714537569812,
4.29453896273396));
#92386=CARTESIAN_POINT('Ctrl Pts',(-3.40968666944009,-23.1770055230636,
4.26451313832345));
#92387=CARTESIAN_POINT('Ctrl Pts',(-3.39042557036629,-23.1676523580104,
4.23271819857054));
#92388=CARTESIAN_POINT('Ctrl Pts',(-3.37383895538399,-23.1418126887906,
4.20685846356792));
#92389=CARTESIAN_POINT('Ctrl Pts',(-3.36461880191793,-23.1071017824704,
4.19452930592906));
#92390=CARTESIAN_POINT('Ctrl Pts',(-3.36302259354816,-23.0723908765014,
4.1953152013499));
#92391=CARTESIAN_POINT('Ctrl Pts',(-3.48603283499412,-23.1658532222902,
4.26386937938429));
#92392=CARTESIAN_POINT('Ctrl Pts',(-3.46328338356492,-23.1744320182858,
4.23600042202927));
#92393=CARTESIAN_POINT('Ctrl Pts',(-3.43787647541882,-23.167036990899,4.20539709393266));
#92394=CARTESIAN_POINT('Ctrl Pts',(-3.41600010763765,-23.14101967926,4.17997996368029));
#92395=CARTESIAN_POINT('Ctrl Pts',(-3.40456018010292,-23.1048418671392,
4.1680707860097));
#92396=CARTESIAN_POINT('Ctrl Pts',(-3.40366433978954,-23.0686637734687,
4.16911430388931));
#92397=CARTESIAN_POINT('Ctrl Pts',(-3.5344175822824,-23.1658530695554,4.21548841685241));
#92398=CARTESIAN_POINT('Ctrl Pts',(-3.50654786413253,-23.1744321920302,
4.1927381521826));
#92399=CARTESIAN_POINT('Ctrl Pts',(-3.47594366275913,-23.1670369970499,
4.16733030664708));
#92400=CARTESIAN_POINT('Ctrl Pts',(-3.45052608305801,-23.1410189063015,
4.14545320139491));
#92401=CARTESIAN_POINT('Ctrl Pts',(-3.43861735888675,-23.1048402717236,
4.13401308548029));
#92402=CARTESIAN_POINT('Ctrl Pts',(-3.4396619580288,-23.0686617900272,4.13311753200938));
#92403=CARTESIAN_POINT('Ctrl Pts',(-3.56508667654552,-23.1714537621884,
4.15672866682488));
#92404=CARTESIAN_POINT('Ctrl Pts',(-3.53506087470362,-23.1770055181561,
4.13913886260155));
#92405=CARTESIAN_POINT('Ctrl Pts',(-3.50326596105016,-23.1676523576714,
4.1198777919475));
#92406=CARTESIAN_POINT('Ctrl Pts',(-3.4774062394318,-23.1418127111937,4.10329119928901));
#92407=CARTESIAN_POINT('Ctrl Pts',(-3.46507706882468,-23.1071018294486,
4.09407105167612));
#92408=CARTESIAN_POINT('Ctrl Pts',(-3.46586293236865,-23.0723909351999,
4.09247483475298));
#92409=CARTESIAN_POINT('Ctrl Pts',(-3.58055767219067,-23.1735838286411,
4.09314155437213));
#92410=CARTESIAN_POINT('Ctrl Pts',(-3.55042155715734,-23.1756160164775,
4.08071352136631));
#92411=CARTESIAN_POINT('Ctrl Pts',(-3.51963685995032,-23.1643433387759,
4.06768195273836));
#92412=CARTESIAN_POINT('Ctrl Pts',(-3.49504258020861,-23.1391099360226,
4.05686232785297));
#92413=CARTESIAN_POINT('Ctrl Pts',(-3.48301304307739,-23.1064573042799,
4.05105890645977));
#92414=CARTESIAN_POINT('Ctrl Pts',(-3.48330362649208,-23.0738046729463,
4.05035717743438));
#92415=CARTESIAN_POINT('',(-3.58046699781502,-23.1735877854623,4.09315100955954));
#92416=CARTESIAN_POINT('Ctrl Pts',(-3.36369873262431,-23.1735877859441,
4.30991926388135));
#92417=CARTESIAN_POINT('Ctrl Pts',(-3.37963984968545,-23.1730555309427,
4.3060377730225));
#92418=CARTESIAN_POINT('Ctrl Pts',(-3.39521728292792,-23.1722660176641,
4.30097285382577));
#92419=CARTESIAN_POINT('Ctrl Pts',(-3.41023110644254,-23.1714624208208,
4.29473355694982));
#92420=CARTESIAN_POINT('Ctrl Pts',(-3.42397399855252,-23.1707268490521,
4.28902242122716));
#92421=CARTESIAN_POINT('Ctrl Pts',(-3.43724543459262,-23.1699802976461,
4.28232843018724));
#92422=CARTESIAN_POINT('Ctrl Pts',(-3.44989872060649,-23.1693715096676,
4.27467504184132));
#92423=CARTESIAN_POINT('Ctrl Pts',(-3.4580416675809,-23.1689797277841,4.26974974928039));
#92424=CARTESIAN_POINT('Ctrl Pts',(-3.46592870548895,-23.1686442133489,
4.26442739865431));
#92425=CARTESIAN_POINT('Ctrl Pts',(-3.4735203301526,-23.1683929962441,4.25871546603301));
#92426=CARTESIAN_POINT('Ctrl Pts',(-3.48436073732317,-23.168034272542,4.25055915192515));
#92427=CARTESIAN_POINT('Ctrl Pts',(-3.49460064242592,-23.1678467144834,
4.24162947897747));
#92428=CARTESIAN_POINT('Ctrl Pts',(-3.50414548344453,-23.1678572110644,
4.23200945990114));
#92429=CARTESIAN_POINT('Ctrl Pts',(-3.50634575216987,-23.1678596307274,
4.22979186119314));
#92430=CARTESIAN_POINT('Ctrl Pts',(-3.50850906418678,-23.1678723584513,
4.22753756056653));
#92431=CARTESIAN_POINT('Ctrl Pts',(-3.51063422148549,-23.1678953318369,
4.22524754091519));
#92432=CARTESIAN_POINT('Ctrl Pts',(-3.52021898816255,-23.1679989451271,
4.21491922119162));
#92433=CARTESIAN_POINT('Ctrl Pts',(-3.52899284990985,-23.1683220299147,
4.20385632239788));
#92434=CARTESIAN_POINT('Ctrl Pts',(-3.53691933305998,-23.168804138081,4.19218781074263));
#92435=CARTESIAN_POINT('Ctrl Pts',(-3.54524904504247,-23.169310771615,4.17992570918867));
#92436=CARTESIAN_POINT('Ctrl Pts',(-3.55264239516412,-23.1699924762988,
4.16699438610174));
#92437=CARTESIAN_POINT('Ctrl Pts',(-3.55905829477961,-23.1707193115775,
4.15353875310712));
#92438=CARTESIAN_POINT('Ctrl Pts',(-3.56589901925505,-23.1714942738086,
4.13919216362241));
#92439=CARTESIAN_POINT('Ctrl Pts',(-3.57162746497981,-23.1723197923469,
4.12424874315674));
#92440=CARTESIAN_POINT('Ctrl Pts',(-3.57620852167135,-23.1729819475165,
4.10888854586347));
#92441=CARTESIAN_POINT('Ctrl Pts',(-3.57775956255688,-23.173206138093,4.10368793482203));
#92442=CARTESIAN_POINT('Ctrl Pts',(-3.57917927008932,-23.173411204468,4.09843963864397));
#92443=CARTESIAN_POINT('Ctrl Pts',(-3.58046699811946,-23.1735877853888,
4.0931510103795));
#92444=CARTESIAN_POINT('Origin',(-3.57500058690307,-23.0745775160831,4.08839184830127));
#92445=CARTESIAN_POINT('Ctrl Pts',(-3.59003004342,-23.1742356021,4.05400943362));
#92446=CARTESIAN_POINT('Ctrl Pts',(-3.56100550691,-23.1742356,4.04198707509));
#92447=CARTESIAN_POINT('Ctrl Pts',(-3.53198097115,-23.1618985927,4.02996471716));
#92448=CARTESIAN_POINT('Ctrl Pts',(-3.50903998578,-23.1370674502,4.020462249));
#92449=CARTESIAN_POINT('Ctrl Pts',(-3.49764207994,-23.1056515239,4.01574108184));
#92450=CARTESIAN_POINT('Ctrl Pts',(-3.49764208329,-23.0742355991,4.01574108398));
#92451=CARTESIAN_POINT('Ctrl Pts',(-3.58811407486,-23.1742356053,4.06182447384));
#92452=CARTESIAN_POINT('Ctrl Pts',(-3.55886400839,-23.1746190551,4.04970869805));
#92453=CARTESIAN_POINT('Ctrl Pts',(-3.52949614106,-23.1624737743,4.03748383221));
#92454=CARTESIAN_POINT('Ctrl Pts',(-3.50623772102,-23.1375556797,4.02772852035));
#92455=CARTESIAN_POINT('Ctrl Pts',(-3.49471696821,-23.1058956405,4.02280292775));
#92456=CARTESIAN_POINT('Ctrl Pts',(-3.49477125586,-23.0742356024,4.0226718745));
#92457=CARTESIAN_POINT('Ctrl Pts',(-3.5861997009,-23.1741720972,4.06964669163));
#92458=CARTESIAN_POINT('Ctrl Pts',(-3.5567270736,-23.1749477738,4.05744341379));
#92459=CARTESIAN_POINT('Ctrl Pts',(-3.52701409515,-23.1630030812,4.04501677108));
#92460=CARTESIAN_POINT('Ctrl Pts',(-3.50343430799,-23.138001656,4.03500416396));
#92461=CARTESIAN_POINT('Ctrl Pts',(-3.49179021707,-23.1060974603,4.02986873261));
#92462=CARTESIAN_POINT('Ctrl Pts',(-3.49190063063,-23.0741932655,4.02960217686));
#92463=CARTESIAN_POINT('Ctrl Pts',(-3.5842870025,-23.1740438599,4.07747556494));
#92464=CARTESIAN_POINT('Ctrl Pts',(-3.55459489737,-23.1752205531,4.0651910977));
#92465=CARTESIAN_POINT('Ctrl Pts',(-3.52453502353,-23.1634855096,4.05256363124));
#92466=CARTESIAN_POINT('Ctrl Pts',(-3.50062982413,-23.1384045129,4.04228916144));
#92467=CARTESIAN_POINT('Ctrl Pts',(-3.48886193116,-23.1062561443,4.03693824347));
#92468=CARTESIAN_POINT('Ctrl Pts',(-3.48903039927,-23.074107776,4.03653152834));
#92469=CARTESIAN_POINT('Ctrl Pts',(-3.58237606919,-23.1738495698,4.08531053381));
#92470=CARTESIAN_POINT('Ctrl Pts',(-3.55246768452,-23.1754360753,4.07295161995));
#92471=CARTESIAN_POINT('Ctrl Pts',(-3.52205911864,-23.1639199594,4.06012452288));
#92472=CARTESIAN_POINT('Ctrl Pts',(-3.49782434849,-23.1387632939,4.04958350869));
#92473=CARTESIAN_POINT('Ctrl Pts',(-3.48593221864,-23.1063707724,4.04401119803));
#92474=CARTESIAN_POINT('Ctrl Pts',(-3.48616076587,-23.0739782508,4.0434594362));
#92475=CARTESIAN_POINT('Ctrl Pts',(-3.58046699728,-23.1735877856,4.09315100795));
#92476=CARTESIAN_POINT('Ctrl Pts',(-3.55034564706,-23.1755928932,4.08072486167));
#92477=CARTESIAN_POINT('Ctrl Pts',(-3.51958658013,-23.1643052014,4.06769960726));
#92478=CARTESIAN_POINT('Ctrl Pts',(-3.49501794889,-23.1390769393,4.05688723526));
#92479=CARTESIAN_POINT('Ctrl Pts',(-3.48300118522,-23.1064403336,4.05108733867));
#92480=CARTESIAN_POINT('Ctrl Pts',(-3.48329194402,-23.073803728,4.05038538482));
#92481=CARTESIAN_POINT('',(-3.59003004166812,-23.17423560745,4.05400943566779));
#92482=CARTESIAN_POINT('Origin',(-3.66997333637772,-22.6950817829913,3.82597648379911));
#92483=CARTESIAN_POINT('Origin',(-3.58937676056356,-23.0749427241466,4.05373884035109));
#92484=CARTESIAN_POINT('Origin',(9.24917823675E-16,-22.8742356128,0.729452270839));
#92485=CARTESIAN_POINT('',(-2.95028784657,-23.1742356128,4.63288636429));
#92486=CARTESIAN_POINT('Origin',(-3.42702565972E-16,-23.1742356128,0.729452270839));
#92487=CARTESIAN_POINT('',(-3.13117783752,-22.8742356128,4.87221628548));
#92488=CARTESIAN_POINT('Origin',(-2.95028784657,-22.8742356128,4.63288636429));
#92489=CARTESIAN_POINT('',(-4.2092958712,-22.8742356128,3.77060280966));
#92490=CARTESIAN_POINT('Origin',(3.67394039744E-17,-22.8742356128,0.729452270839));
#92491=CARTESIAN_POINT('',(-3.96612236541,-23.1742356128,3.59491374888));
#92492=CARTESIAN_POINT('Origin',(-3.96612236541,-22.8742356128,3.59491374888));
#92493=CARTESIAN_POINT('Origin',(-3.42702565972E-16,-23.1742356128,0.729452270839));
#92494=CARTESIAN_POINT('Origin',(-3.31206782846,-22.8742356128,5.11154620667));
#92495=CARTESIAN_POINT('',(-2.90473307408,-23.1742356128,5.55208950519));
#92496=CARTESIAN_POINT('',(-3.10840045127,-22.8742356128,5.33181785593));
#92497=CARTESIAN_POINT('Origin',(-2.90473307408,-22.8742356128,5.55208950519));
#92498=CARTESIAN_POINT('Origin',(-3.31206782846,-22.8742356128,5.11154620667));
#92499=CARTESIAN_POINT('Origin',(-3.31206782846,-23.1742356128,5.11154620667));
#92500=CARTESIAN_POINT('Origin',(-6.6707290414,-22.8742356128,9.03420135995));
#92501=CARTESIAN_POINT('',(-4.51260368036,-23.1742356128,7.03875740065));
#92502=CARTESIAN_POINT('',(-4.71627105755,-22.8742356128,6.81848575139));
#92503=CARTESIAN_POINT('Origin',(-4.51260368036,-22.8742356128,7.03875740065));
#92504=CARTESIAN_POINT('',(-3.91233575441,-22.8742356128,6.07515180366));
#92505=CARTESIAN_POINT('',(-3.70866837722,-23.1742356128,6.29542345292));
#92506=CARTESIAN_POINT('Origin',(-4.91993843473,-22.8742356128,6.59821410213));
#92507=CARTESIAN_POINT('',(-5.40800342362,-23.1742356128,6.94720201972));
#92508=CARTESIAN_POINT('',(-5.16397092918,-22.8742356128,6.77270806092));
#92509=CARTESIAN_POINT('Origin',(-5.40800342362,-22.8742356128,6.94720201972));
#92510=CARTESIAN_POINT('Origin',(-4.91993843473,-22.8742356128,6.59821410213));
#92511=CARTESIAN_POINT('Origin',(-4.91993843473,-23.1742356128,6.59821410213));
#92512=CARTESIAN_POINT('Origin',(-0.00234331738835,-22.8742356128,3.08191746407));
#92513=CARTESIAN_POINT('',(-6.57948381998,-23.1742356128,4.03207991826));
#92514=CARTESIAN_POINT('',(-6.28256615006,-22.8742356128,3.98918589435));
#92515=CARTESIAN_POINT('Origin',(-6.57948381998,-22.8742356128,4.03207991826));
#92516=CARTESIAN_POINT('Origin',(-0.00234331738835,-22.8742356128,3.08191746407));
#92517=CARTESIAN_POINT('Origin',(-0.00234331738835,-23.1742356128,3.08191746407));
#92518=CARTESIAN_POINT('Origin',(-4.452469377,-22.8742356128,3.94629187045));
#92519=CARTESIAN_POINT('',(-4.452469377,-22.8742356128,3.64629187045));
#92520=CARTESIAN_POINT('Origin',(-4.452469377,-22.8742356128,3.94629187045));
#92521=CARTESIAN_POINT('',(-4.452469377,-23.1742356128,3.34629187045));
#92522=CARTESIAN_POINT('Origin',(-4.452469377,-22.8742356128,3.34629187045));
#92523=CARTESIAN_POINT('Origin',(-4.452469377,-23.1742356128,3.94629187045));
#92524=CARTESIAN_POINT('Origin',(-5.98564848014,-22.8742356128,3.94629187045));
#92525=CARTESIAN_POINT('',(-5.98564848014,-23.1742356128,3.34629187045));
#92526=CARTESIAN_POINT('',(-5.98564848014,-22.8742356128,3.64629187045));
#92527=CARTESIAN_POINT('Origin',(-5.98564848014,-22.8742356128,3.34629187045));
#92528=CARTESIAN_POINT('Origin',(-5.98564848014,-22.8742356128,3.94629187045));
#92529=CARTESIAN_POINT('Origin',(-5.98564848014,-23.1742356128,3.94629187045));
#92530=CARTESIAN_POINT('Origin',(-6.6707290414,-22.8742356128,3.34629187045));
#92531=CARTESIAN_POINT('',(-5.21905892857,-22.8742356128,3.64629187045));
#92532=CARTESIAN_POINT('',(-5.21905892857,-23.1742356128,3.34629187045));
#92533=CARTESIAN_POINT('Origin',(-4.1372329486,-21.0742356128,5.87450964899));
#92534=CARTESIAN_POINT('',(-3.31206782846,-20.7742356128,5.11154620667));
#92535=CARTESIAN_POINT('',(-3.10840045127,-21.0742356128,5.33181785593));
#92536=CARTESIAN_POINT('Ctrl Pts',(-3.31206782846,-20.7742356128,5.11154620667));
#92537=CARTESIAN_POINT('Ctrl Pts',(-3.29933521826663,-20.7742356127999,
5.12531686098549));
#92538=CARTESIAN_POINT('Ctrl Pts',(-3.28660287019773,-20.775999501442,5.13908723180644));
#92539=CARTESIAN_POINT('Ctrl Pts',(-3.27409353932531,-20.7794964191287,
5.15261640363735));
#92540=CARTESIAN_POINT('Ctrl Pts',(-3.26210247220447,-20.7828484589079,
5.16558505952856));
#92541=CARTESIAN_POINT('Ctrl Pts',(-3.25031672255145,-20.7877924035019,
5.1783316591539));
#92542=CARTESIAN_POINT('Ctrl Pts',(-3.23892583382867,-20.7942487422808,
5.19065120625108));
#92543=CARTESIAN_POINT('Ctrl Pts',(-3.22753797140324,-20.800703365759,5.20296748032772));
#92544=CARTESIAN_POINT('Ctrl Pts',(-3.21654515523054,-20.8086693535063,
5.21485650144502));
#92545=CARTESIAN_POINT('Ctrl Pts',(-3.2061240830046,-20.8180186608397,5.22612716637859));
#92546=CARTESIAN_POINT('Ctrl Pts',(-3.19570270992945,-20.8273682380811,
5.23739815668853));
#92547=CARTESIAN_POINT('Ctrl Pts',(-3.18585347586854,-20.8381008902533,
5.24805036353882));
#92548=CARTESIAN_POINT('Ctrl Pts',(-3.17673470576069,-20.8500440916057,
5.25791255432522));
#92549=CARTESIAN_POINT('Ctrl Pts',(-3.17554748033519,-20.8515990460721,
5.25919656998899));
#92550=CARTESIAN_POINT('Ctrl Pts',(-3.17437260707132,-20.8531744629905,
5.26046722646361));
#92551=CARTESIAN_POINT('Ctrl Pts',(-3.17321040762789,-20.8547699110405,
5.26172417586659));
#92552=CARTESIAN_POINT('Ctrl Pts',(-3.16700069378047,-20.8632945028438,
5.26844014545107));
#92553=CARTESIAN_POINT('Ctrl Pts',(-3.16115327543625,-20.8723916371716,
5.2747642828771));
#92554=CARTESIAN_POINT('Ctrl Pts',(-3.15571375996958,-20.8819903575583,
5.28064726256438));
#92555=CARTESIAN_POINT('Ctrl Pts',(-3.15299400223624,-20.8867897177517,
5.28358875240802));
#92556=CARTESIAN_POINT('Ctrl Pts',(-3.15037611880697,-20.8917143566616,
5.28642006250033));
#92557=CARTESIAN_POINT('Ctrl Pts',(-3.14786523424292,-20.896754634957,5.28913565049302));
#92558=CARTESIAN_POINT('Ctrl Pts',(-3.14680766159051,-20.8988775762351,
5.29027944325729));
#92559=CARTESIAN_POINT('Ctrl Pts',(-3.14562334882535,-20.9013206204291,
5.29156030880195));
#92560=CARTESIAN_POINT('Ctrl Pts',(-3.14450250481394,-20.9037103020532,
5.2927725312126));
#92561=CARTESIAN_POINT('Ctrl Pts',(-3.14326498842998,-20.9063487335674,
5.2941109378766));
#92562=CARTESIAN_POINT('Ctrl Pts',(-3.14210503148785,-20.9089219096235,
5.29536546195516));
#92563=CARTESIAN_POINT('Ctrl Pts',(-3.14123879647682,-20.910887453468,5.29630231800518));
#92564=CARTESIAN_POINT('Ctrl Pts',(-3.14102688301432,-20.911368298962,5.29653150801353));
#92565=CARTESIAN_POINT('Ctrl Pts',(-3.14083239185809,-20.9118126387024,
5.29674185533738));
#92566=CARTESIAN_POINT('Ctrl Pts',(-3.14065826128173,-20.9122123369602,
5.29693018215616));
#92567=CARTESIAN_POINT('Ctrl Pts',(-3.1375970523511,-20.9192390171794,5.30024096049042));
#92568=CARTESIAN_POINT('Ctrl Pts',(-3.13478628520643,-20.9264540360834,
5.30338356310924));
#92569=CARTESIAN_POINT('Ctrl Pts',(-3.13223592512423,-20.9338322706568,
5.30634721230281));
#92570=CARTESIAN_POINT('Ctrl Pts',(-3.13096074508313,-20.9375213879435,
5.30782903689959));
#92571=CARTESIAN_POINT('Ctrl Pts',(-3.129750643895,-20.9412512918604,5.3092661479207));
#92572=CARTESIAN_POINT('Ctrl Pts',(-3.12860673216448,-20.9450187312842,
5.31065734421785));
#92573=CARTESIAN_POINT('Ctrl Pts',(-3.12803477629922,-20.9469024509962,
5.31135294236643));
#92574=CARTESIAN_POINT('Ctrl Pts',(-3.12747936638829,-20.948795553409,5.31203706335906));
#92575=CARTESIAN_POINT('Ctrl Pts',(-3.12694063242266,-20.950697626295,5.31270956660706));
#92576=CARTESIAN_POINT('Ctrl Pts',(-3.12663283447761,-20.9517843484305,
5.31309379171811));
#92577=CARTESIAN_POINT('Ctrl Pts',(-3.12619161680522,-20.9533813143145,
5.31365170209757));
#92578=CARTESIAN_POINT('Ctrl Pts',(-3.12585743559154,-20.9546204589871,
5.31407645693962));
#92579=CARTESIAN_POINT('Ctrl Pts',(-3.12560670461402,-20.9555501700011,
5.31439514390465));
#92580=CARTESIAN_POINT('Ctrl Pts',(-3.12541480694582,-20.9562775177554,
5.31464041022965));
#92581=CARTESIAN_POINT('Ctrl Pts',(-3.12537458248023,-20.9564303402735,
5.3146920888797));
#92582=CARTESIAN_POINT('Ctrl Pts',(-3.12522435030849,-20.957001108796,5.31488510066286));
#92583=CARTESIAN_POINT('Ctrl Pts',(-3.12479964436627,-20.9584280758291,
5.31532581148723));
#92584=CARTESIAN_POINT('Ctrl Pts',(-3.12412770189941,-20.9607278021972,
5.31598476355186));
#92585=CARTESIAN_POINT('Ctrl Pts',(-3.12396023830268,-20.9613009471733,
5.31614898964004));
#92586=CARTESIAN_POINT('Ctrl Pts',(-3.12377757874227,-20.9619283916087,
5.31632659765268));
#92587=CARTESIAN_POINT('Ctrl Pts',(-3.1235804670171,-20.9626105622649,5.31651678315158));
#92588=CARTESIAN_POINT('Ctrl Pts',(-3.12311253766171,-20.9642299873657,
5.31696827013355));
#92589=CARTESIAN_POINT('Ctrl Pts',(-3.12243241818589,-20.9666119834499,
5.31761216570488));
#92590=CARTESIAN_POINT('Ctrl Pts',(-3.12174493077351,-20.969121675404,5.31825518911771));
#92591=CARTESIAN_POINT('Ctrl Pts',(-3.12109418479046,-20.9714972417466,
5.31886384739328));
#92592=CARTESIAN_POINT('Ctrl Pts',(-3.1204372075556,-20.9739871819659,5.31947132386135));
#92593=CARTESIAN_POINT('Ctrl Pts',(-3.11991259420517,-20.9760333492218,
5.31995167406521));
#92594=CARTESIAN_POINT('Ctrl Pts',(-3.11982119675865,-20.9763898297845,
5.32003536004467));
#92595=CARTESIAN_POINT('Ctrl Pts',(-3.11973373269842,-20.9767327986748,
5.32011527847067));
#92596=CARTESIAN_POINT('Ctrl Pts',(-3.11965084049907,-20.9770592586797,
5.32019086546073));
#92597=CARTESIAN_POINT('Ctrl Pts',(-3.11873221172192,-20.980677157076,5.32102853637301));
#92598=CARTESIAN_POINT('Ctrl Pts',(-3.11800394114676,-20.9837595200313,
5.32169404058884));
#92599=CARTESIAN_POINT('Ctrl Pts',(-3.11737165618863,-20.9865959563919,
5.32228942746157));
#92600=CARTESIAN_POINT('Ctrl Pts',(-3.11667947524101,-20.9897010867334,
5.32294121498944));
#92601=CARTESIAN_POINT('Ctrl Pts',(-3.11610269286778,-20.9925119721021,
5.32350857546106));
#92602=CARTESIAN_POINT('Ctrl Pts',(-3.11555570510201,-20.9954279844329,
5.32408406940618));
#92603=CARTESIAN_POINT('Ctrl Pts',(-3.11544778770807,-20.9960032961146,
5.32419761089772));
#92604=CARTESIAN_POINT('Ctrl Pts',(-3.11534113468803,-20.9965827453735,
5.32431135583329));
#92605=CARTESIAN_POINT('Ctrl Pts',(-3.11523524285449,-20.9971694629971,
5.32442584825116));
#92606=CARTESIAN_POINT('Ctrl Pts',(-3.11209966050602,-21.0145428652934,
5.32781610406697));
#92607=CARTESIAN_POINT('Ctrl Pts',(-3.110027452273,-21.0323321591983,5.3300569564894));
#92608=CARTESIAN_POINT('Ctrl Pts',(-3.10905193709402,-21.0502512911575,
5.33111237020608));
#92609=CARTESIAN_POINT('Ctrl Pts',(-3.10861763232592,-21.0582289880891,
5.33158224624629));
#92610=CARTESIAN_POINT('Ctrl Pts',(-3.1084002383703,-21.066232297709,5.33181765908384));
#92611=CARTESIAN_POINT('Ctrl Pts',(-3.10840045126752,-21.0742356128,5.33181785593268));
#92612=CARTESIAN_POINT('',(-4.71627105755,-21.0742356128,6.81848575139));
#92613=CARTESIAN_POINT('',(-3.91233575441,-21.0742356128,6.07515180366));
#92614=CARTESIAN_POINT('',(-4.91993843473,-20.7742356128,6.59821410213));
#92615=CARTESIAN_POINT('Ctrl Pts',(-4.91993843473,-20.7742356128,6.59821410213));
#92616=CARTESIAN_POINT('Ctrl Pts',(-4.91101807800614,-20.7742356128001,
6.60786170359966));
#92617=CARTESIAN_POINT('Ctrl Pts',(-4.90252339602707,-20.7750985628785,
6.61712968289017));
#92618=CARTESIAN_POINT('Ctrl Pts',(-4.8944934572549,-20.7766036070835,6.62592256231193));
#92619=CARTESIAN_POINT('Ctrl Pts',(-4.88605462232259,-20.7781852903283,
6.63516318794124));
#92620=CARTESIAN_POINT('Ctrl Pts',(-4.87812882597999,-20.7804752394698,
6.64387935631824));
#92621=CARTESIAN_POINT('Ctrl Pts',(-4.87072223708168,-20.7832292456085,
6.65200261974273));
#92622=CARTESIAN_POINT('Ctrl Pts',(-4.86531045478571,-20.7852415189868,
6.65793805558096));
#92623=CARTESIAN_POINT('Ctrl Pts',(-4.86017499035168,-20.7875018067851,
6.66355789937889));
#92624=CARTESIAN_POINT('Ctrl Pts',(-4.85530752896798,-20.7899222629677,
6.66884704557737));
#92625=CARTESIAN_POINT('Ctrl Pts',(-4.84828146203815,-20.7934161349884,
6.67648180469773));
#92626=CARTESIAN_POINT('Ctrl Pts',(-4.84182598167012,-20.7972434179056,
6.68344575129118));
#92627=CARTESIAN_POINT('Ctrl Pts',(-4.8359312132666,-20.8011818445937,6.68978189067321));
#92628=CARTESIAN_POINT('Ctrl Pts',(-4.83433051190638,-20.8022513089942,
6.69150244460053));
#92629=CARTESIAN_POINT('Ctrl Pts',(-4.8327710384092,-20.8033292152502,6.69317683282407));
#92630=CARTESIAN_POINT('Ctrl Pts',(-4.83125236393977,-20.8044116620105,
6.69480616639989));
#92631=CARTESIAN_POINT('Ctrl Pts',(-4.82769667927255,-20.8069460032574,
6.69862093811689));
#92632=CARTESIAN_POINT('Ctrl Pts',(-4.82436526487051,-20.8095049076771,
6.70218957148497));
#92633=CARTESIAN_POINT('Ctrl Pts',(-4.82125350553739,-20.812044273078,6.70553206549793));
#92634=CARTESIAN_POINT('Ctrl Pts',(-4.81969762587084,-20.8133139557784,
6.70720331250441));
#92635=CARTESIAN_POINT('Ctrl Pts',(-4.81843122123371,-20.8143803798034,
6.7085628667989));
#92636=CARTESIAN_POINT('Ctrl Pts',(-4.81709937825491,-20.8155303534285,
6.70999899677484));
#92637=CARTESIAN_POINT('Ctrl Pts',(-4.81587928901512,-20.8165838338074,
6.71131462238422));
#92638=CARTESIAN_POINT('Ctrl Pts',(-4.81460418147319,-20.8177075259004,
6.71269462123414));
#92639=CARTESIAN_POINT('Ctrl Pts',(-4.81301644753763,-20.8191595577754,
6.71442100155403));
#92640=CARTESIAN_POINT('Ctrl Pts',(-4.81287101948364,-20.8192925562364,
6.71457912888554));
#92641=CARTESIAN_POINT('Ctrl Pts',(-4.81272298219209,-20.8194283405095,
6.7147401475396));
#92642=CARTESIAN_POINT('Ctrl Pts',(-4.81257214682211,-20.8195671295471,
6.71490426436397));
#92643=CARTESIAN_POINT('Ctrl Pts',(-4.80473608843389,-20.8267773681179,
6.72343030847733));
#92644=CARTESIAN_POINT('Ctrl Pts',(-4.79752989742272,-20.8344866681735,
6.73123516492522));
#92645=CARTESIAN_POINT('Ctrl Pts',(-4.79092681315199,-20.8424631101107,
6.7383485989656));
#92646=CARTESIAN_POINT('Ctrl Pts',(-4.78541183125531,-20.8491251381994,
6.74428983163013));
#92647=CARTESIAN_POINT('Ctrl Pts',(-4.78031680760064,-20.8559741803587,
6.74974956049137));
#92648=CARTESIAN_POINT('Ctrl Pts',(-4.77561385480444,-20.8628961108439,
6.75475842594953));
#92649=CARTESIAN_POINT('Ctrl Pts',(-4.77223310973378,-20.8678719809795,
6.75835907812297));
#92650=CARTESIAN_POINT('Ctrl Pts',(-4.76896166073005,-20.8730320642035,
6.76182963192853));
#92651=CARTESIAN_POINT('Ctrl Pts',(-4.76589273431812,-20.8782133062045,
6.76508294196168));
#92652=CARTESIAN_POINT('Ctrl Pts',(-4.76261503962766,-20.88374700989,6.76855756324314));
#92653=CARTESIAN_POINT('Ctrl Pts',(-4.75956871210815,-20.8893043149753,
6.77178399636243));
#92654=CARTESIAN_POINT('Ctrl Pts',(-4.75683198223358,-20.8946499026989,
6.77469430090779));
#92655=CARTESIAN_POINT('Ctrl Pts',(-4.75429868506137,-20.899598130286,6.77738827021165));
#92656=CARTESIAN_POINT('Ctrl Pts',(-4.75202989571111,-20.9043638139079,
6.77981219865064));
#92657=CARTESIAN_POINT('Ctrl Pts',(-4.75006304874771,-20.9087436757408,
6.78193882013059));
#92658=CARTESIAN_POINT('Ctrl Pts',(-4.74555434167549,-20.9187838641179,
6.78681378675738));
#92659=CARTESIAN_POINT('Ctrl Pts',(-4.74160660860021,-20.9288814156251,
6.7910825342297));
#92660=CARTESIAN_POINT('Ctrl Pts',(-4.73813954370417,-20.9389926751171,
6.79483177943904));
#92661=CARTESIAN_POINT('Ctrl Pts',(-4.73453775139493,-20.9494968501952,
6.79872671736649));
#92662=CARTESIAN_POINT('Ctrl Pts',(-4.73145429815306,-20.9600166233867,
6.80206143894353));
#92663=CARTESIAN_POINT('Ctrl Pts',(-4.72882070162607,-20.9705491771698,
6.80490985719644));
#92664=CARTESIAN_POINT('Ctrl Pts',(-4.72607730103734,-20.9815208708038,
6.80787703619746));
#92665=CARTESIAN_POINT('Ctrl Pts',(-4.72382167411467,-20.9925073236551,
6.8103169231494));
#92666=CARTESIAN_POINT('Ctrl Pts',(-4.72200555539,-21.0035411667321,6.81228154610962));
#92667=CARTESIAN_POINT('Ctrl Pts',(-4.72009746998151,-21.0151337540938,
6.81434565587991));
#92668=CARTESIAN_POINT('Ctrl Pts',(-4.7186740823484,-21.0267797209318,6.81588563580126));
#92669=CARTESIAN_POINT('Ctrl Pts',(-4.71771751058766,-21.0385403140574,
6.81692062577603));
#92670=CARTESIAN_POINT('Ctrl Pts',(-4.71676093882692,-21.050300907183,6.8179556157508));
#92671=CARTESIAN_POINT('Ctrl Pts',(-4.7162710575463,-21.0621774370813,6.818485751394));
#92672=CARTESIAN_POINT('Ctrl Pts',(-4.7162710575463,-21.0742356128,6.818485751394));
#92673=CARTESIAN_POINT('',(-4.1160031316,-20.7742356128,5.8548801544));
#92674=CARTESIAN_POINT('Origin',(-2.31985562646,-21.0742356128,7.05423263334));
#92675=CARTESIAN_POINT('',(-1.46510738459,-21.0742356128,5.8553296721));
#92676=CARTESIAN_POINT('',(-2.54349379462,-21.0742356128,6.85242635913));
#92677=CARTESIAN_POINT('',(-1.2614400074,-20.7742356128,6.07560132137));
#92678=CARTESIAN_POINT('Origin',(-1.26144000740192,-21.0742356128,6.07560132136512));
#92679=CARTESIAN_POINT('',(-2.33982641743,-20.7742356128,7.0726980084));
#92680=CARTESIAN_POINT('Origin',(-0.00234331738835,-21.0742356128,3.08191746407));
#92681=CARTESIAN_POINT('',(-6.21380646358,-21.0742356128,1.78497474518));
#92682=CARTESIAN_POINT('',(-5.92013962829,-20.7742356128,1.84629187045));
#92683=CARTESIAN_POINT('Ctrl Pts',(-6.21380646358263,-21.0742356128,1.78497474517945));
#92684=CARTESIAN_POINT('Ctrl Pts',(-6.21380646358263,-21.0638291242201,
1.78497474517945));
#92685=CARTESIAN_POINT('Ctrl Pts',(-6.21327417566471,-21.0536166921391,
1.78505315888558));
#92686=CARTESIAN_POINT('Ctrl Pts',(-6.21224803590314,-21.0435122709929,
1.7852283036963));
#92687=CARTESIAN_POINT('Ctrl Pts',(-6.2112178215814,-21.0333677275616,1.78540414396596));
#92688=CARTESIAN_POINT('Ctrl Pts',(-6.20968970505262,-21.0233311229344,
1.78567751866417));
#92689=CARTESIAN_POINT('Ctrl Pts',(-6.20765173862219,-21.0133172081608,
1.78607754692084));
#92690=CARTESIAN_POINT('Ctrl Pts',(-6.20633833173915,-21.0068635471027,
1.78633535286792));
#92691=CARTESIAN_POINT('Ctrl Pts',(-6.20481214385547,-21.0004193812891,
1.78664597516925));
#92692=CARTESIAN_POINT('Ctrl Pts',(-6.20305914183912,-20.9939650457512,
1.78701943793744));
#92693=CARTESIAN_POINT('Ctrl Pts',(-6.20017203893198,-20.9833350916946,
1.78763451164169));
#92694=CARTESIAN_POINT('Ctrl Pts',(-6.1966691290526,-20.9726827259468,1.78840119577086));
#92695=CARTESIAN_POINT('Ctrl Pts',(-6.19245514538327,-20.9619932754936,
1.7893188173187));
#92696=CARTESIAN_POINT('Ctrl Pts',(-6.19142746403405,-20.9593863957033,
1.78954260142048));
#92697=CARTESIAN_POINT('Ctrl Pts',(-6.19035731493665,-20.956777469529,1.78977539984786));
#92698=CARTESIAN_POINT('Ctrl Pts',(-6.18924298052752,-20.9541666224691,
1.79001727404038));
#92699=CARTESIAN_POINT('Ctrl Pts',(-6.18640116205152,-20.947508339864,1.79063411091049));
#92700=CARTESIAN_POINT('Ctrl Pts',(-6.18327258049845,-20.9408382928993,
1.79130942869506));
#92701=CARTESIAN_POINT('Ctrl Pts',(-6.17982938053887,-20.934169877643,1.79204407797328));
#92702=CARTESIAN_POINT('Ctrl Pts',(-6.17831560267499,-20.9312381572896,
1.79236706119474));
#92703=CARTESIAN_POINT('Ctrl Pts',(-6.17688544243804,-20.9285769855239,
1.79267133246466));
#92704=CARTESIAN_POINT('Ctrl Pts',(-6.17535411987191,-20.9258272802483,
1.79299524597198));
#92705=CARTESIAN_POINT('Ctrl Pts',(-6.17391712939085,-20.9232469615133,
1.7932992058541));
#92706=CARTESIAN_POINT('Ctrl Pts',(-6.17239097810791,-20.9205884555348,
1.79362047868821));
#92707=CARTESIAN_POINT('Ctrl Pts',(-6.17058626019263,-20.9175771306239,
1.79399842408086));
#92708=CARTESIAN_POINT('Ctrl Pts',(-6.16993973029997,-20.9164983406618,
1.79413382086064));
#92709=CARTESIAN_POINT('Ctrl Pts',(-6.16925708304517,-20.9153745097185,
1.79427656745455));
#92710=CARTESIAN_POINT('Ctrl Pts',(-6.16852821746026,-20.9141939713519,
1.79442876434852));
#92711=CARTESIAN_POINT('Ctrl Pts',(-6.16226859189097,-20.9040553006583,
1.79573585798662));
#92712=CARTESIAN_POINT('Ctrl Pts',(-6.15517323883986,-20.8939067913336,
1.79721736722423));
#92713=CARTESIAN_POINT('Ctrl Pts',(-6.14713178957169,-20.8839003131641,
1.79888899627398));
#92714=CARTESIAN_POINT('Ctrl Pts',(-6.14250264364114,-20.8781399774145,
1.79985128734304));
#92715=CARTESIAN_POINT('Ctrl Pts',(-6.13756008361075,-20.872427578217,1.8008765606857));
#92716=CARTESIAN_POINT('Ctrl Pts',(-6.13228512614383,-20.8667997672481,
1.8019674021234));
#92717=CARTESIAN_POINT('Ctrl Pts',(-6.12756782361308,-20.86176691398,1.80294292260997));
#92718=CARTESIAN_POINT('Ctrl Pts',(-6.12271663472741,-20.8569369691441,
1.80394169722641));
#92719=CARTESIAN_POINT('Ctrl Pts',(-6.11760803373886,-20.8521972192353,
1.80499799326209));
#92720=CARTESIAN_POINT('Ctrl Pts',(-6.11234437566273,-20.8473136076668,
1.80608635016675));
#92721=CARTESIAN_POINT('Ctrl Pts',(-6.10680731541783,-20.8425247796987,
1.80723580224648));
#92722=CARTESIAN_POINT('Ctrl Pts',(-6.1008263123872,-20.837754257854,1.80849112969859));
#92723=CARTESIAN_POINT('Ctrl Pts',(-6.09543622633937,-20.8334550586889,
1.80962243208224));
#92724=CARTESIAN_POINT('Ctrl Pts',(-6.08968498885813,-20.8291706338078,
1.81083984845462));
#92725=CARTESIAN_POINT('Ctrl Pts',(-6.08342555190955,-20.8248881944549,
1.81218069347538));
#92726=CARTESIAN_POINT('Ctrl Pts',(-6.08273932768923,-20.8244187091593,
1.81232769077506));
#92727=CARTESIAN_POINT('Ctrl Pts',(-6.08204697635262,-20.8239492959192,
1.81247617541911));
#92728=CARTESIAN_POINT('Ctrl Pts',(-6.08134829036222,-20.823479974991,1.81262619935616));
#92729=CARTESIAN_POINT('Ctrl Pts',(-6.07084476035318,-20.8164245502068,
1.81488154860675));
#92730=CARTESIAN_POINT('Ctrl Pts',(-6.05949429674607,-20.8097986564887,
1.81725014952178));
#92731=CARTESIAN_POINT('Ctrl Pts',(-6.04732674889071,-20.8038283905592,
1.81977071506763));
#92732=CARTESIAN_POINT('Ctrl Pts',(-6.04124297496303,-20.8008432575944,
1.82103099784056));
#92733=CARTESIAN_POINT('Ctrl Pts',(-6.03495585748087,-20.7980223837757,
1.82232960162766));
#92734=CARTESIAN_POINT('Ctrl Pts',(-6.02847522956622,-20.7953955144343,
1.82367335937379));
#92735=CARTESIAN_POINT('Ctrl Pts',(-6.02583793509647,-20.7943265087641,
1.82422020219816));
#92736=CARTESIAN_POINT('Ctrl Pts',(-6.0228510692185,-20.7931653163342,1.82484135358158));
#92737=CARTESIAN_POINT('Ctrl Pts',(-6.01989947204153,-20.7920763253463,
1.82545656126346));
#92738=CARTESIAN_POINT('Ctrl Pts',(-6.0167298538359,-20.7909068955583,1.82611721153239));
#92739=CARTESIAN_POINT('Ctrl Pts',(-6.01360113456556,-20.7898210851413,
1.82677095962912));
#92740=CARTESIAN_POINT('Ctrl Pts',(-6.01101145633295,-20.788960047348,1.82731391901932));
#92741=CARTESIAN_POINT('Ctrl Pts',(-6.01008678157446,-20.7886526037809,
1.82750778899));
#92742=CARTESIAN_POINT('Ctrl Pts',(-6.00923099123423,-20.7883732746121,
1.82768750069863));
#92743=CARTESIAN_POINT('Ctrl Pts',(-6.00846713791962,-20.7881270953015,
1.82784824664587));
#92744=CARTESIAN_POINT('Ctrl Pts',(-6.0026023396212,-20.7862369522931,1.82908243983431));
#92745=CARTESIAN_POINT('Ctrl Pts',(-5.99587512952763,-20.7842726880881,
1.83049099473282));
#92746=CARTESIAN_POINT('Ctrl Pts',(-5.98825586153528,-20.7824167003156,
1.8320826743304));
#92747=CARTESIAN_POINT('Ctrl Pts',(-5.98084399712823,-20.7806112342623,
1.83363102692392));
#92748=CARTESIAN_POINT('Ctrl Pts',(-5.97258700545796,-20.7789084592162,
1.83535287478211));
#92749=CARTESIAN_POINT('Ctrl Pts',(-5.96347756599724,-20.7775200828796,
1.83725209508735));
#92750=CARTESIAN_POINT('Ctrl Pts',(-5.95480118246376,-20.7761977089138,
1.83906102788216));
#92751=CARTESIAN_POINT('Ctrl Pts',(-5.94535068955056,-20.7751610722981,
1.8410310343364));
#92752=CARTESIAN_POINT('Ctrl Pts',(-5.93515058418323,-20.7746277752809,
1.84315899601206));
#92753=CARTESIAN_POINT('Ctrl Pts',(-5.93031300926584,-20.7743748500236,
1.84416821833444));
#92754=CARTESIAN_POINT('Ctrl Pts',(-5.92530735504451,-20.7742356127999,
1.84521285807765));
#92755=CARTESIAN_POINT('Ctrl Pts',(-5.92013962829,-20.7742356128,1.84629187045));
#92756=CARTESIAN_POINT('',(-5.76218263052,-21.0742356128,0.419477620705));
#92757=CARTESIAN_POINT('Origin',(-0.00234331738835,-21.0742356128,3.08191746407));
#92758=CARTESIAN_POINT('',(-5.48986775992,-20.7742356128,0.545353000555));
#92759=CARTESIAN_POINT('Ctrl Pts',(-5.76218263051847,-21.0742356128,0.419477620705708));
#92760=CARTESIAN_POINT('Ctrl Pts',(-5.76218263051847,-21.0700542173555,
0.419477620705718));
#92761=CARTESIAN_POINT('Ctrl Pts',(-5.76208822882541,-21.0658728234983,
0.419481774388309));
#92762=CARTESIAN_POINT('Ctrl Pts',(-5.76189949703241,-21.0616950856527,
0.419490058448013));
#92763=CARTESIAN_POINT('Ctrl Pts',(-5.76180351272392,-21.0595703918119,
0.419494271515295));
#92764=CARTESIAN_POINT('Ctrl Pts',(-5.76170596844914,-21.0578162530132,
0.419502972865373));
#92765=CARTESIAN_POINT('Ctrl Pts',(-5.76157699842966,-21.0558688871039,
0.419508645330075));
#92766=CARTESIAN_POINT('Ctrl Pts',(-5.76145237759245,-21.0539871911022,
0.419514126505492));
#92767=CARTESIAN_POINT('Ctrl Pts',(-5.7612993086323,-21.0519248572092,0.41951636520272));
#92768=CARTESIAN_POINT('Ctrl Pts',(-5.76105052573855,-21.0491764894493,
0.419527231998826));
#92769=CARTESIAN_POINT('Ctrl Pts',(-5.76054427759769,-21.0435838377684,
0.419549344834819));
#92770=CARTESIAN_POINT('Ctrl Pts',(-5.75995086462676,-21.0380043491261,
0.4197570049967));
#92771=CARTESIAN_POINT('Ctrl Pts',(-5.75927114796157,-21.0324468066016,
0.420149699187728));
#92772=CARTESIAN_POINT('Ctrl Pts',(-5.75893128962897,-21.0296680353393,
0.42034604628324));
#92773=CARTESIAN_POINT('Ctrl Pts',(-5.75856986164284,-21.0268947495701,
0.420588648987048));
#92774=CARTESIAN_POINT('Ctrl Pts',(-5.75818700380084,-21.0241280412191,
0.420877413809454));
#92775=CARTESIAN_POINT('Ctrl Pts',(-5.75800935278482,-21.0228442525758,
0.421011404441123));
#92776=CARTESIAN_POINT('Ctrl Pts',(-5.75774710432639,-21.0209676723318,
0.421231939899458));
#92777=CARTESIAN_POINT('Ctrl Pts',(-5.75750471561971,-21.0193269715218,
0.421435552712598));
#92778=CARTESIAN_POINT('Ctrl Pts',(-5.75722472950835,-21.0174317782761,
0.421670748322804));
#92779=CARTESIAN_POINT('Ctrl Pts',(-5.75697461782143,-21.0158507644803,
0.42188180568687));
#92780=CARTESIAN_POINT('Ctrl Pts',(-5.75697430408476,-21.0158487352453,
0.42188208656193));
#92781=CARTESIAN_POINT('Ctrl Pts',(-5.75697391849401,-21.0158462412614,
0.421882431764879));
#92782=CARTESIAN_POINT('Ctrl Pts',(-5.75681273469604,-21.0149286495503,
0.421957097869057));
#92783=CARTESIAN_POINT('Ctrl Pts',(-5.75646751532521,-21.0131012056486,
0.422116826131579));
#92784=CARTESIAN_POINT('Ctrl Pts',(-5.75611606673489,-21.0112407869194,
0.422279436568426));
#92785=CARTESIAN_POINT('Ctrl Pts',(-5.75557395522215,-21.0084370054318,
0.422530172355905));
#92786=CARTESIAN_POINT('Ctrl Pts',(-5.75476782901722,-21.0047090998318,
0.422902939748514));
#92787=CARTESIAN_POINT('Ctrl Pts',(-5.75396170281228,-21.0009811942318,
0.423275707141123));
#92788=CARTESIAN_POINT('Ctrl Pts',(-5.75289137553641,-20.9963284789036,
0.423770592291697));
#92789=CARTESIAN_POINT('Ctrl Pts',(-5.75143609421341,-20.9907917516533,
0.424443412285836));
#92790=CARTESIAN_POINT('Ctrl Pts',(-5.75003801615353,-20.98547265852,0.42508978550398));
#92791=CARTESIAN_POINT('Ctrl Pts',(-5.748284064558,-20.9793370244532,0.42590065187824));
#92792=CARTESIAN_POINT('Ctrl Pts',(-5.74602953787445,-20.9724505880868,
0.426942898528165));
#92793=CARTESIAN_POINT('Ctrl Pts',(-5.74383550469501,-20.9657489287159,
0.427957179595572));
#92794=CARTESIAN_POINT('Ctrl Pts',(-5.74116676451505,-20.9583354833729,
0.429190883969123));
#92795=CARTESIAN_POINT('Ctrl Pts',(-5.73786227189959,-20.9503096563882,
0.430718453591819));
#92796=CARTESIAN_POINT('Ctrl Pts',(-5.73474618032658,-20.9427414107469,
0.432158930960783));
#92797=CARTESIAN_POINT('Ctrl Pts',(-5.73106397875205,-20.9346282631776,
0.433861082610605));
#92798=CARTESIAN_POINT('Ctrl Pts',(-5.7266659725094,-20.926095961081,0.435894103682038));
#92799=CARTESIAN_POINT('Ctrl Pts',(-5.72244512364354,-20.9179073511426,
0.437845232036613));
#92800=CARTESIAN_POINT('Ctrl Pts',(-5.71756421491754,-20.9093323848096,
0.440101462659826));
#92801=CARTESIAN_POINT('Ctrl Pts',(-5.71188791964413,-20.9005271966043,
0.442725349212077));
#92802=CARTESIAN_POINT('Ctrl Pts',(-5.70643988023259,-20.8920760836763,
0.445243723725645));
#92803=CARTESIAN_POINT('Ctrl Pts',(-5.70025837439386,-20.8834128049173,
0.448101132492726));
#92804=CARTESIAN_POINT('Ctrl Pts',(-5.69323182479467,-20.8747203666876,
0.451349151232407));
#92805=CARTESIAN_POINT('Ctrl Pts',(-5.68647772309588,-20.8663649696347,
0.454471231077957));
#92806=CARTESIAN_POINT('Ctrl Pts',(-5.67894210952565,-20.8579827361327,
0.457954554149233));
#92807=CARTESIAN_POINT('Ctrl Pts',(-5.67054418362936,-20.8497784476017,
0.461836469810334));
#92808=CARTESIAN_POINT('Ctrl Pts',(-5.6624554326642,-20.8418762051202,0.465575470301429));
#92809=CARTESIAN_POINT('Ctrl Pts',(-5.6535660256726,-20.8341393286479,0.469684563567774));
#92810=CARTESIAN_POINT('Ctrl Pts',(-5.64383110675435,-20.8267879818355,
0.474184483903669));
#92811=CARTESIAN_POINT('Ctrl Pts',(-5.63418816478761,-20.8195060916333,
0.478641888327719));
#92812=CARTESIAN_POINT('Ctrl Pts',(-5.62371480691348,-20.8126028174762,
0.48348314188324));
#92813=CARTESIAN_POINT('Ctrl Pts',(-5.61240580309607,-20.8063250428812,
0.488710662141486));
#92814=CARTESIAN_POINT('Ctrl Pts',(-5.6019057715892,-20.8004963393009,0.4935642397245));
#92815=CARTESIAN_POINT('Ctrl Pts',(-5.5906851835362,-20.7952075582835,0.498750885402041));
#92816=CARTESIAN_POINT('Ctrl Pts',(-5.57877932195408,-20.7906767474455,
0.504254289919316));
#92817=CARTESIAN_POINT('Ctrl Pts',(-5.5671865239154,-20.7862650738648,0.509612982917204));
#92818=CARTESIAN_POINT('Ctrl Pts',(-5.55494366255547,-20.7825726642816,
0.515272159292754));
#92819=CARTESIAN_POINT('Ctrl Pts',(-5.54212646457403,-20.7798115878137,
0.521196815032388));
#92820=CARTESIAN_POINT('Ctrl Pts',(-5.52976210381069,-20.7771480613867,
0.526912150089981));
#92821=CARTESIAN_POINT('Ctrl Pts',(-5.51686313783045,-20.7753519171367,
0.532874599206211));
#92822=CARTESIAN_POINT('Ctrl Pts',(-5.5035416480442,-20.7746140611604,0.539032353698168));
#92823=CARTESIAN_POINT('Ctrl Pts',(-5.49902989564469,-20.7743641624234,
0.54111787596711));
#92824=CARTESIAN_POINT('Ctrl Pts',(-5.49447006936149,-20.7742356128,0.543225619674669));
#92825=CARTESIAN_POINT('Ctrl Pts',(-5.48986775992,-20.7742356128,0.545353000555));
#92826=CARTESIAN_POINT('Origin',(-0.00234331738835,-20.7742356128,3.08191746407));
#92827=CARTESIAN_POINT('Origin',(-5.48986775992,-21.0742356128,0.545353000555));
#92828=CARTESIAN_POINT('',(-5.1900363009,-21.0742356128,0.55540766038));
#92829=CARTESIAN_POINT('Origin',(-5.48986775992,-21.0742356128,0.545353000555));
#92830=CARTESIAN_POINT('Origin',(-5.48986775992,-21.0742356128,0.545353000555));
#92831=CARTESIAN_POINT('Origin',(1.47842115491E-15,-21.0742356128,0.729452270839));
#92832=CARTESIAN_POINT('',(-5.08448267152,-21.0742356128,1.78529520144));
#92833=CARTESIAN_POINT('',(-5.3782162351,-20.7742356128,1.84629187045));
#92834=CARTESIAN_POINT('Ctrl Pts',(-5.08448267152607,-21.0742356128,1.78529520144126));
#92835=CARTESIAN_POINT('Ctrl Pts',(-5.08448267152607,-21.0614130940682,
1.78529520144126));
#92836=CARTESIAN_POINT('Ctrl Pts',(-5.08528146803515,-21.0485906280905,
1.78549730909642));
#92837=CARTESIAN_POINT('Ctrl Pts',(-5.08687246330687,-21.0358733936431,
1.7859002586259));
#92838=CARTESIAN_POINT('Ctrl Pts',(-5.08766796094273,-21.0295147764195,
1.78610173339064));
#92839=CARTESIAN_POINT('Ctrl Pts',(-5.08866130593276,-21.0231824345426,
1.78635337671675));
#92840=CARTESIAN_POINT('Ctrl Pts',(-5.08985043859178,-21.0168894102148,
1.78665479764093));
#92841=CARTESIAN_POINT('Ctrl Pts',(-5.0903951219712,-21.0140068842564,1.78679286379055));
#92842=CARTESIAN_POINT('Ctrl Pts',(-5.09092718216906,-21.0113881381866,
1.78693799787711));
#92843=CARTESIAN_POINT('Ctrl Pts',(-5.0915147214932,-21.0086827022826,1.78708833999566));
#92844=CARTESIAN_POINT('Ctrl Pts',(-5.09207204900295,-21.00611638239,1.78723095138369));
#92845=CARTESIAN_POINT('Ctrl Pts',(-5.09267924627531,-21.0034718705681,
1.78737821109546));
#92846=CARTESIAN_POINT('Ctrl Pts',(-5.09342319728476,-21.0004534336218,
1.78756269841702));
#92847=CARTESIAN_POINT('Ctrl Pts',(-5.0936071767023,-20.9997069728143,1.7876083222142));
#92848=CARTESIAN_POINT('Ctrl Pts',(-5.09379967401835,-20.9989376697526,
1.78765640532237));
#92849=CARTESIAN_POINT('Ctrl Pts',(-5.09400233909841,-20.9981411165267,
1.78770783716017));
#92850=CARTESIAN_POINT('Ctrl Pts',(-5.09709097517254,-20.9860015657566,
1.7884916635083));
#92851=CARTESIAN_POINT('Ctrl Pts',(-5.10094234956947,-20.974063720211,1.78935051102611));
#92852=CARTESIAN_POINT('Ctrl Pts',(-5.1055271132446,-20.9624169074904,1.79028097896789));
#92853=CARTESIAN_POINT('Ctrl Pts',(-5.10654181896996,-20.9598392200921,
1.7904869113157));
#92854=CARTESIAN_POINT('Ctrl Pts',(-5.1075923771993,-20.9572759311037,1.79069622721775));
#92855=CARTESIAN_POINT('Ctrl Pts',(-5.10867832162472,-20.9547282358368,
1.79090865953936));
#92856=CARTESIAN_POINT('Ctrl Pts',(-5.11167461524405,-20.9476987388446,
1.79149479414705));
#92857=CARTESIAN_POINT('Ctrl Pts',(-5.11494087661384,-20.9407862593262,
1.79210608868242));
#92858=CARTESIAN_POINT('Ctrl Pts',(-5.11846765793979,-20.9340111008953,
1.79274037257807));
#92859=CARTESIAN_POINT('Ctrl Pts',(-5.11985187154921,-20.9313519435392,
1.79298932036345));
#92860=CARTESIAN_POINT('Ctrl Pts',(-5.1211267858793,-20.928986911576,1.79323158599076));
#92861=CARTESIAN_POINT('Ctrl Pts',(-5.12245944386044,-20.9265929771404,
1.79347032304439));
#92862=CARTESIAN_POINT('Ctrl Pts',(-5.12371441533186,-20.9243385956984,
1.79369514306253));
#92863=CARTESIAN_POINT('Ctrl Pts',(-5.12502075047096,-20.922058421466,1.79391703398184));
#92864=CARTESIAN_POINT('Ctrl Pts',(-5.12654632236385,-20.9194925254243,
1.79416863251517));
#92865=CARTESIAN_POINT('Ctrl Pts',(-5.12752829683552,-20.9178409189536,
1.79433058052822));
#92866=CARTESIAN_POINT('Ctrl Pts',(-5.12860157962051,-20.9160710796194,
1.79450533697522));
#92867=CARTESIAN_POINT('Ctrl Pts',(-5.12981865714979,-20.914117158484,1.7947096656124));
#92868=CARTESIAN_POINT('Ctrl Pts',(-5.13493442695431,-20.9059041971033,
1.79556852484454));
#92869=CARTESIAN_POINT('Ctrl Pts',(-5.14041852996597,-20.897943240988,1.79661719636324));
#92870=CARTESIAN_POINT('Ctrl Pts',(-5.14624478500792,-20.8902716071521,
1.79785127829691));
#92871=CARTESIAN_POINT('Ctrl Pts',(-5.1491579125289,-20.8864357902341,1.79846831926374));
#92872=CARTESIAN_POINT('Ctrl Pts',(-5.15215653588352,-20.8826722651419,
1.79913170401791));
#92873=CARTESIAN_POINT('Ctrl Pts',(-5.15523710145265,-20.8789854927669,
1.79984085770605));
#92874=CARTESIAN_POINT('Ctrl Pts',(-5.15677738423722,-20.8771421065794,
1.80019543455013));
#92875=CARTESIAN_POINT('Ctrl Pts',(-5.15833814960495,-20.8753179065473,
1.80056145300697));
#92876=CARTESIAN_POINT('Ctrl Pts',(-5.15991893697881,-20.8735134363296,
1.80093883851198));
#92877=CARTESIAN_POINT('Ctrl Pts',(-5.16070933066575,-20.8726112012207,
1.80112753126449));
#92878=CARTESIAN_POINT('Ctrl Pts',(-5.1615047296844,-20.871713898423,1.80131906574349));
#92879=CARTESIAN_POINT('Ctrl Pts',(-5.16230507536263,-20.8708215951015,
1.80151343250699));
#92880=CARTESIAN_POINT('Ctrl Pts',(-5.16286595087811,-20.8701962764435,
1.80164964309903));
#92881=CARTESIAN_POINT('Ctrl Pts',(-5.16381117101369,-20.8691535012779,
1.80187989131107));
#92882=CARTESIAN_POINT('Ctrl Pts',(-5.16433869641073,-20.8685768123516,
1.80201031399209));
#92883=CARTESIAN_POINT('Ctrl Pts',(-5.16456392748109,-20.8683305905301,
1.80206599896994));
#92884=CARTESIAN_POINT('Ctrl Pts',(-5.16471247623231,-20.8681689155371,
1.80210294211167));
#92885=CARTESIAN_POINT('Ctrl Pts',(-5.1647208930014,-20.8681597501726,1.80210502009182));
#92886=CARTESIAN_POINT('Ctrl Pts',(-5.16478496730456,-20.8680899770403,
1.80212083912267));
#92887=CARTESIAN_POINT('Ctrl Pts',(-5.16543415713941,-20.8673822152715,
1.80225950119297));
#92888=CARTESIAN_POINT('Ctrl Pts',(-5.1666860085911,-20.8660564184847,1.8025153204794));
#92889=CARTESIAN_POINT('Ctrl Pts',(-5.1676325256999,-20.8650539917672,1.80270874385327));
#92890=CARTESIAN_POINT('Ctrl Pts',(-5.16892428264733,-20.8636986921275,
1.80296985397145));
#92891=CARTESIAN_POINT('Ctrl Pts',(-5.17058106734596,-20.8620092639083,
1.80330799035701));
#92892=CARTESIAN_POINT('Ctrl Pts',(-5.1725050808472,-20.8600473416948,1.80370066598446));
#92893=CARTESIAN_POINT('Ctrl Pts',(-5.17492098970874,-20.8576352118099,
1.8041932137294));
#92894=CARTESIAN_POINT('Ctrl Pts',(-5.17787468853171,-20.8548243854623,
1.80479514724455));
#92895=CARTESIAN_POINT('Ctrl Pts',(-5.1792155093237,-20.8535484211087,1.80506839276513));
#92896=CARTESIAN_POINT('Ctrl Pts',(-5.18096220677253,-20.851916394557,1.80541625744203));
#92897=CARTESIAN_POINT('Ctrl Pts',(-5.18272412749508,-20.8503133827491,
1.80577433408361));
#92898=CARTESIAN_POINT('Ctrl Pts',(-5.18455593116523,-20.8486467907875,
1.80614661309585));
#92899=CARTESIAN_POINT('Ctrl Pts',(-5.18640420676291,-20.8470119466033,
1.80652993493292));
#92900=CARTESIAN_POINT('Ctrl Pts',(-5.1877915946851,-20.8458061052139,1.80681508756679));
#92901=CARTESIAN_POINT('Ctrl Pts',(-5.18800943258993,-20.8456167724702,
1.8068598602301));
#92902=CARTESIAN_POINT('Ctrl Pts',(-5.18821584645905,-20.8454379528746,
1.80690215364221));
#92903=CARTESIAN_POINT('Ctrl Pts',(-5.18840893352295,-20.8452711264075,
1.80694149257333));
#92904=CARTESIAN_POINT('Ctrl Pts',(-5.1936202871629,-20.8407685372677,1.80800323683386));
#92905=CARTESIAN_POINT('Ctrl Pts',(-5.19865361893382,-20.8367359737122,
1.80903280841691));
#92906=CARTESIAN_POINT('Ctrl Pts',(-5.2034457792482,-20.8331144155368,1.81001714106857));
#92907=CARTESIAN_POINT('Ctrl Pts',(-5.20584185940539,-20.8313036364491,
1.8105093073944));
#92908=CARTESIAN_POINT('Ctrl Pts',(-5.20817788729427,-20.8295956268,1.81099021388227));
#92909=CARTESIAN_POINT('Ctrl Pts',(-5.21044732529831,-20.8279832426908,
1.81145850828711));
#92910=CARTESIAN_POINT('Ctrl Pts',(-5.21158204430033,-20.8271770506363,
1.81169265548952));
#92911=CARTESIAN_POINT('Ctrl Pts',(-5.21270012169541,-20.8263947736905,
1.81192365088883));
#92912=CARTESIAN_POINT('Ctrl Pts',(-5.21380082865156,-20.8256355352479,
1.81215134374786));
#92913=CARTESIAN_POINT('Ctrl Pts',(-5.2145476908534,-20.8251203695249,1.81230584008232));
#92914=CARTESIAN_POINT('Ctrl Pts',(-5.21576632620745,-20.8242901399562,
1.81255684264991));
#92915=CARTESIAN_POINT('Ctrl Pts',(-5.21648082540202,-20.8238087349836,
1.81270562152336));
#92916=CARTESIAN_POINT('Ctrl Pts',(-5.2168193373676,-20.8235806572688,1.81277610925697));
#92917=CARTESIAN_POINT('Ctrl Pts',(-5.21704411632927,-20.8234301284241,
1.81282312096779));
#92918=CARTESIAN_POINT('Ctrl Pts',(-5.21705013203587,-20.8234260963392,
1.8128243686639));
#92919=CARTESIAN_POINT('Ctrl Pts',(-5.21712543227981,-20.8233756256304,
1.81283998641723));
#92920=CARTESIAN_POINT('Ctrl Pts',(-5.21794283507666,-20.8228205263349,
1.81302715496386));
#92921=CARTESIAN_POINT('Ctrl Pts',(-5.21951437433468,-20.8217883955223,
1.81336586433952));
#92922=CARTESIAN_POINT('Ctrl Pts',(-5.22109550447098,-20.8207499657638,
1.81370664080983));
#92923=CARTESIAN_POINT('Ctrl Pts',(-5.22344024804095,-20.8192284429785,
1.81420110808858));
#92924=CARTESIAN_POINT('Ctrl Pts',(-5.22658729860372,-20.8172915736929,
1.81485262134387));
#92925=CARTESIAN_POINT('Ctrl Pts',(-5.22971685572864,-20.8153654708383,
1.81550051304735));
#92926=CARTESIAN_POINT('Ctrl Pts',(-5.23364039011882,-20.8130282348166,
1.81630427268963));
#92927=CARTESIAN_POINT('Ctrl Pts',(-5.23841592276139,-20.8103901583995,
1.81728413247834));
#92928=CARTESIAN_POINT('Ctrl Pts',(-5.2430438977556,-20.8078335950578,1.81823371589435));
#92929=CARTESIAN_POINT('Ctrl Pts',(-5.24847286282806,-20.8049942587288,
1.8193494472573));
#92930=CARTESIAN_POINT('Ctrl Pts',(-5.25476408162235,-20.8020181237148,
1.8206558715834));
#92931=CARTESIAN_POINT('Ctrl Pts',(-5.26085974723718,-20.7991344974314,
1.82192168765233));
#92932=CARTESIAN_POINT('Ctrl Pts',(-5.26775980090195,-20.7961293482283,
1.82332050551907));
#92933=CARTESIAN_POINT('Ctrl Pts',(-5.27551754699974,-20.7931746130028,
1.82489808968304));
#92934=CARTESIAN_POINT('Ctrl Pts',(-5.28273403840939,-20.7904260284135,
1.82636560646225));
#92935=CARTESIAN_POINT('Ctrl Pts',(-5.2906934607079,-20.7877214605548,1.82798843561937));
#92936=CARTESIAN_POINT('Ctrl Pts',(-5.29942286128885,-20.7852385908721,
1.82978958090487));
#92937=CARTESIAN_POINT('Ctrl Pts',(-5.30778785157575,-20.7828593690015,
1.83151553707779));
#92938=CARTESIAN_POINT('Ctrl Pts',(-5.31686057569694,-20.7806841633692,
1.83340582143119));
#92939=CARTESIAN_POINT('Ctrl Pts',(-5.3266394453264,-20.7789010890687,1.83545887229495));
#92940=CARTESIAN_POINT('Ctrl Pts',(-5.33583825993341,-20.7772237817169,
1.83739014196007));
#92941=CARTESIAN_POINT('Ctrl Pts',(-5.34566235646555,-20.7758941532551,
1.8394657905466));
#92942=CARTESIAN_POINT('Ctrl Pts',(-5.35607973455985,-20.7750893176935,
1.84165835473634));
#92943=CARTESIAN_POINT('Ctrl Pts',(-5.36318972295453,-20.7745400075454,
1.84315480670367));
#92944=CARTESIAN_POINT('Ctrl Pts',(-5.37057545291419,-20.7742356128,1.84470518673479));
#92945=CARTESIAN_POINT('Ctrl Pts',(-5.3782162351,-20.7742356128,1.84629187045));
#92946=CARTESIAN_POINT('Origin',(1.126325016E-16,-20.7742356128,0.729452270839));
#92947=CARTESIAN_POINT('Origin',(2.57175827821E-16,-21.0742356128,0.729452270839));
#92948=CARTESIAN_POINT('Origin',(-5.92013962829,-21.0742356128,1.84629187045));
#92949=CARTESIAN_POINT('',(-5.92013962829,-21.0742356128,2.14629187045));
#92950=CARTESIAN_POINT('Origin',(-5.92013962829,-21.0742356128,1.84629187045));
#92951=CARTESIAN_POINT('Origin',(-5.92013962829,-21.0742356128,1.84629187045));
#92952=CARTESIAN_POINT('Origin',(-5.3782162351,-21.0742356128,1.84629187045));
#92953=CARTESIAN_POINT('',(-5.3782162351,-21.0742356128,2.14629187045));
#92954=CARTESIAN_POINT('Origin',(-5.3782162351,-21.0742356128,1.84629187045));
#92955=CARTESIAN_POINT('Origin',(-5.3782162351,-21.0742356128,1.84629187045));
#92956=CARTESIAN_POINT('Origin',(-3.31206782846,-21.0742356128,5.11154620667));
#92957=CARTESIAN_POINT('',(-3.13117783752,-21.0742356128,4.87221628548));
#92958=CARTESIAN_POINT('Origin',(-3.31206782846,-21.0742356128,5.11154620667));
#92959=CARTESIAN_POINT('Origin',(-3.31206782846,-21.0742356128,5.11154620667));
#92960=CARTESIAN_POINT('Origin',(-5.60029074364,-21.0742356128,1.84629187045));
#92961=CARTESIAN_POINT('',(-5.6491779317,-20.7742356128,1.84629187045));
#92962=CARTESIAN_POINT('',(-5.6491779317,-21.0742356128,2.14629187045));
#92963=CARTESIAN_POINT('Origin',(1.47842115491E-15,-21.0742356128,0.729452270839));
#92964=CARTESIAN_POINT('',(-4.2092958712,-21.0742356128,3.77060280966));
#92965=CARTESIAN_POINT('',(-4.452469377,-20.7742356128,3.94629187045));
#92966=CARTESIAN_POINT('Ctrl Pts',(-4.20929587120239,-21.0742356128,3.77060280966173));
#92967=CARTESIAN_POINT('Ctrl Pts',(-4.20929587120239,-21.0567670633141,
3.77060280966173));
#92968=CARTESIAN_POINT('Ctrl Pts',(-4.21053420664878,-21.039288104426,3.7714875497586));
#92969=CARTESIAN_POINT('Ctrl Pts',(-4.21302952672439,-21.0219367655753,
3.77327918596831));
#92970=CARTESIAN_POINT('Ctrl Pts',(-4.21552484680001,-21.0045854267246,
3.77507082217803));
#92971=CARTESIAN_POINT('Ctrl Pts',(-4.21927769717971,-20.9873595047338,
3.77776973840221));
#92972=CARTESIAN_POINT('Ctrl Pts',(-4.22434041182606,-20.9704316655761,
3.78142247514592));
#92973=CARTESIAN_POINT('Ctrl Pts',(-4.2290076878942,-20.9548260262887,3.78478990388288));
#92974=CARTESIAN_POINT('Ctrl Pts',(-4.23478878393056,-20.9394753388172,
3.78897006104767));
#92975=CARTESIAN_POINT('Ctrl Pts',(-4.24173245519993,-20.9245813330018,
3.79399759136516));
#92976=CARTESIAN_POINT('Ctrl Pts',(-4.24232076312392,-20.9233194268283,
3.79442355276356));
#92977=CARTESIAN_POINT('Ctrl Pts',(-4.24291741501226,-20.9220608303557,
3.79485559592467));
#92978=CARTESIAN_POINT('Ctrl Pts',(-4.24352243904187,-20.9208056843632,
3.79529374087375));
#92979=CARTESIAN_POINT('Ctrl Pts',(-4.24637370724739,-20.9148906170492,
3.79735856590814));
#92980=CARTESIAN_POINT('Ctrl Pts',(-4.2494837284245,-20.9089093610656,3.79961172647346));
#92981=CARTESIAN_POINT('Ctrl Pts',(-4.25278436811486,-20.9030443905848,
3.8020023595835));
#92982=CARTESIAN_POINT('Ctrl Pts',(-4.25609549745106,-20.8971607808496,
3.80440059027976));
#92983=CARTESIAN_POINT('Ctrl Pts',(-4.25959825927427,-20.8913947792768,
3.80693702485545));
#92984=CARTESIAN_POINT('Ctrl Pts',(-4.26318787729757,-20.8859011249233,
3.80953429455957));
#92985=CARTESIAN_POINT('Ctrl Pts',(-4.26574097359176,-20.8819937931457,
3.81138158850939));
#92986=CARTESIAN_POINT('Ctrl Pts',(-4.26833719887337,-20.8782235763595,
3.81325907226093));
#92987=CARTESIAN_POINT('Ctrl Pts',(-4.27092931133313,-20.8746352746839,
3.81513200774992));
#92988=CARTESIAN_POINT('Ctrl Pts',(-4.27772396722458,-20.8652293266398,
3.82004149850395));
#92989=CARTESIAN_POINT('Ctrl Pts',(-4.28525987940435,-20.8559988435105,
3.82547188896741));
#92990=CARTESIAN_POINT('Ctrl Pts',(-4.29358234259888,-20.8471407335453,
3.83147537999488));
#92991=CARTESIAN_POINT('Ctrl Pts',(-4.29734859711526,-20.8431320769874,
3.83419220489007));
#92992=CARTESIAN_POINT('Ctrl Pts',(-4.30127563429279,-20.8392002484946,
3.83702618686642));
#92993=CARTESIAN_POINT('Ctrl Pts',(-4.30536586453391,-20.8353663275283,
3.83998090287142));
#92994=CARTESIAN_POINT('Ctrl Pts',(-4.31193016316833,-20.8292133726383,
3.84472284576788));
#92995=CARTESIAN_POINT('Ctrl Pts',(-4.31891569582986,-20.8233125443284,
3.84977500785908));
#92996=CARTESIAN_POINT('Ctrl Pts',(-4.32632635631929,-20.8177620044615,
3.85513691010998));
#92997=CARTESIAN_POINT('Ctrl Pts',(-4.330031686564,-20.8149867345281,3.85781786123542));
#92998=CARTESIAN_POINT('Ctrl Pts',(-4.33384315336668,-20.8122992204208,
3.86057600867429));
#92999=CARTESIAN_POINT('Ctrl Pts',(-4.3377602566725,-20.8097127162401,3.86340969540574));
#93000=CARTESIAN_POINT('Ctrl Pts',(-4.33948117149357,-20.8085763782291,
3.8646546289992));
#93001=CARTESIAN_POINT('Ctrl Pts',(-4.3414979467098,-20.8072824582389,3.86611317481211));
#93002=CARTESIAN_POINT('Ctrl Pts',(-4.34345078725751,-20.8060737953689,
3.86752521019504));
#93003=CARTESIAN_POINT('Ctrl Pts',(-4.34561904450574,-20.8047318056033,
3.86909300637654));
#93004=CARTESIAN_POINT('Ctrl Pts',(-4.34770824252956,-20.8034950021666,
3.87060329056719));
#93005=CARTESIAN_POINT('Ctrl Pts',(-4.34920034244517,-20.8026314786707,
3.87168154390545));
#93006=CARTESIAN_POINT('Ctrl Pts',(-4.34942324250476,-20.8025024796428,
3.87184262074142));
#93007=CARTESIAN_POINT('Ctrl Pts',(-4.34963278664701,-20.8023817233861,
3.87199403392379));
#93008=CARTESIAN_POINT('Ctrl Pts',(-4.34982722465402,-20.8022700347198,
3.87213451813516));
#93009=CARTESIAN_POINT('Ctrl Pts',(-4.35516377370196,-20.7992046255698,
3.87599025033482));
#93010=CARTESIAN_POINT('Ctrl Pts',(-4.36125806845615,-20.7959906141422,
3.88039336313273));
#93011=CARTESIAN_POINT('Ctrl Pts',(-4.36815945129353,-20.7928434952946,
3.8853795348017));
#93012=CARTESIAN_POINT('Ctrl Pts',(-4.37448994688551,-20.789956708333,3.88995324684102));
#93013=CARTESIAN_POINT('Ctrl Pts',(-4.38150021419207,-20.7871267873611,
3.89501804152803));
#93014=CARTESIAN_POINT('Ctrl Pts',(-4.38921284910019,-20.7845634272244,
3.90059026672928));
#93015=CARTESIAN_POINT('Ctrl Pts',(-4.39666085655732,-20.7820880182831,
3.9059713038646));
#93016=CARTESIAN_POINT('Ctrl Pts',(-4.40476457688503,-20.7798615624639,
3.91182606547739));
#93017=CARTESIAN_POINT('Ctrl Pts',(-4.41351920705256,-20.7781089820743,
3.91815110222087));
#93018=CARTESIAN_POINT('Ctrl Pts',(-4.42183641148545,-20.7764439694917,
3.9241601080423));
#93019=CARTESIAN_POINT('Ctrl Pts',(-4.43074160378321,-20.7752072573721,
3.93059392855731));
#93020=CARTESIAN_POINT('Ctrl Pts',(-4.44019906484498,-20.7746177736591,
3.93742677551188));
#93021=CARTESIAN_POINT('Ctrl Pts',(-4.44419274238802,-20.7743688476681,
3.94031213631424));
#93022=CARTESIAN_POINT('Ctrl Pts',(-4.44828445852957,-20.7742356127999,
3.94326833220267));
#93023=CARTESIAN_POINT('Ctrl Pts',(-4.452469377,-20.7742356128,3.94629187045));
#93024=CARTESIAN_POINT('Origin',(2.57175827821E-16,-21.0742356128,0.729452270839));
#93025=CARTESIAN_POINT('Origin',(1.126325016E-16,-20.7742356128,0.729452270839));
#93026=CARTESIAN_POINT('Origin',(-1.05,-22.8742356128,-4.99584562937));
#93027=CARTESIAN_POINT('',(-0.972828518105,-23.1742356128,-4.40082919062));
#93028=CARTESIAN_POINT('Origin',(-1.05,-23.1742356128,-4.99584562937));
#93029=CARTESIAN_POINT('',(-1.01141425905,-22.8742356128,-4.69833741));
#93030=CARTESIAN_POINT('Origin',(-0.972828518105,-22.8742356128,-4.40082919062));
#93031=CARTESIAN_POINT('Origin',(-1.05,-22.8742356128,-4.99584562937));
#93032=CARTESIAN_POINT('Origin',(-0.00234331738835,-22.8742356128,3.08191746407));
#93033=CARTESIAN_POINT('',(-4.23842172091,-23.1742356128,-3.16219806837));
#93034=CARTESIAN_POINT('Origin',(-0.00234331738835,-23.1742356128,3.08191746407));
#93035=CARTESIAN_POINT('',(-4.40684492179,-22.8742356128,-3.41045927235));
#93036=CARTESIAN_POINT('Origin',(-4.23842172091,-22.8742356128,-3.16219806837));
#93037=CARTESIAN_POINT('Origin',(-0.00234331738835,-22.8742356128,3.08191746407));
#93038=CARTESIAN_POINT('Origin',(-6.34552156645,-22.8742356128,-5.5301356238));
#93039=CARTESIAN_POINT('',(-6.56346233154,-22.8742356128,-5.32397592135));
#93040=CARTESIAN_POINT('',(-6.78140309663,-23.1742356128,-5.11781621891));
#93041=CARTESIAN_POINT('Origin',(-6.78140309663,-22.8742356128,-5.11781621891));
#93042=CARTESIAN_POINT('Origin',(-6.34552156645,-23.1742356128,-5.5301356238));
#93043=CARTESIAN_POINT('Origin',(-6.34552156645,-22.8742356128,-5.5301356238));
#93044=CARTESIAN_POINT('Origin',(-4.57526812267,-22.8742356128,-3.65872047634));
#93045=CARTESIAN_POINT('',(-5.01114965285,-23.1742356128,-3.24640107146));
#93046=CARTESIAN_POINT('Origin',(-4.57526812267,-23.1742356128,-3.65872047634));
#93047=CARTESIAN_POINT('',(-4.79320888776,-22.8742356128,-3.4525607739));
#93048=CARTESIAN_POINT('Origin',(-5.01114965285,-22.8742356128,-3.24640107146));
#93049=CARTESIAN_POINT('Origin',(-4.57526812267,-22.8742356128,-3.65872047634));
#93050=CARTESIAN_POINT('Origin',(-1.2614400074,-21.0742356128,6.07560132137));
#93051=CARTESIAN_POINT('',(-1.19254592572,-21.0742356128,5.78361912069));
#93052=CARTESIAN_POINT('Origin',(-1.2614400074,-21.0742356128,6.07560132137));
#93053=CARTESIAN_POINT('Origin',(-1.2614400074,-21.0742356128,6.07560132137));
#93054=CARTESIAN_POINT('Origin',(-1.71825752818E-13,-21.9742356128,-5.63016324424));
#93055=CARTESIAN_POINT('',(-0.246933912590001,-21.0742356137361,-6.5991955009251));
#93056=CARTESIAN_POINT('Origin',(-1.72570291390173E-13,-21.0742355071906,
-5.63016324424002));
#93057=CARTESIAN_POINT('',(-0.246934184763,-21.3732856128,-6.59919549778));
#93058=CARTESIAN_POINT('Origin',(2.84607155346,-21.3642356128,5.53854202767));
#93059=CARTESIAN_POINT('',(-0.530881033960364,-21.0742356128,-6.52327988866722));
#93060=CARTESIAN_POINT('',(-0.530881036642,-22.1242356128,-6.52327988851));
#93061=CARTESIAN_POINT('Origin',(2.84607155346,-21.0742356128,5.53854202767));
#93062=CARTESIAN_POINT('Origin',(-0.45,-22.8742356128,-6.23438845923));
#93063=CARTESIAN_POINT('Origin',(-0.45,-22.8742356128,-6.23438845923));
#93064=CARTESIAN_POINT('Ctrl Pts',(7.715616340275E-16,-20.7742356128,-6.9673210071));
#93065=CARTESIAN_POINT('Ctrl Pts',(7.715616340275E-16,-20.7742356128,-6.9673210071));
#93066=CARTESIAN_POINT('Ctrl Pts',(7.715616340275E-16,-20.7742356128,-6.9673210071));
#93067=CARTESIAN_POINT('Ctrl Pts',(7.715616340275E-16,-20.7742356128,-6.9673210071));
#93068=CARTESIAN_POINT('Ctrl Pts',(7.715616340275E-16,-20.7742356128,-6.9673210071));
#93069=CARTESIAN_POINT('Ctrl Pts',(7.715616340275E-16,-20.7742356128,-6.9673210071));
#93070=CARTESIAN_POINT('Ctrl Pts',(0.0620789114664,-20.7727817153,-6.86712083978));
#93071=CARTESIAN_POINT('Ctrl Pts',(0.0372447941938,-20.7727814769555,-6.86710441347656));
#93072=CARTESIAN_POINT('Ctrl Pts',(0.0124139553071,-20.7727812105989,-6.8670860566289));
#93073=CARTESIAN_POINT('Ctrl Pts',(-0.0124139554138,-20.7727812105989,-6.8670860566289));
#93074=CARTESIAN_POINT('Ctrl Pts',(-0.0372447942657,-20.7727814769555,-6.86710441347656));
#93075=CARTESIAN_POINT('Ctrl Pts',(-0.0620789114664,-20.7727817153,-6.86712083978));
#93076=CARTESIAN_POINT('Ctrl Pts',(0.126706651057,-20.809097628,-6.7683471563));
#93077=CARTESIAN_POINT('Ctrl Pts',(0.0760530156428,-20.8106930399,-6.76865483887));
#93078=CARTESIAN_POINT('Ctrl Pts',(0.0253584233265,-20.8114382347,-6.76885772281));
#93079=CARTESIAN_POINT('Ctrl Pts',(-0.0253584229554,-20.8114382347,-6.76885772281));
#93080=CARTESIAN_POINT('Ctrl Pts',(-0.0760530153923,-20.8106930399,-6.76865483887));
#93081=CARTESIAN_POINT('Ctrl Pts',(-0.126706651057,-20.809097628,-6.7683471563));
#93082=CARTESIAN_POINT('Ctrl Pts',(0.185538258403,-20.8478771982,-6.68330934255));
#93083=CARTESIAN_POINT('Ctrl Pts',(0.111595913132,-20.8641740172,-6.68722155122));
#93084=CARTESIAN_POINT('Ctrl Pts',(0.0372374622574,-20.8723993359,-6.68904882319));
#93085=CARTESIAN_POINT('Ctrl Pts',(-0.0372374612746,-20.8723993359,-6.68904882319));
#93086=CARTESIAN_POINT('Ctrl Pts',(-0.111595912483,-20.8641740172,-6.68722155122));
#93087=CARTESIAN_POINT('Ctrl Pts',(-0.185538258404,-20.8478771982,-6.68330934255));
#93088=CARTESIAN_POINT('Ctrl Pts',(0.248193078621,-20.9544277624,-6.59756027965));
#93089=CARTESIAN_POINT('Ctrl Pts',(0.151037451012,-20.9653225623,-6.62292642142));
#93090=CARTESIAN_POINT('Ctrl Pts',(0.0507127937414,-20.9709039046,-6.63587730141));
#93091=CARTESIAN_POINT('Ctrl Pts',(-0.0507127941925,-20.9709039046,-6.63587730141));
#93092=CARTESIAN_POINT('Ctrl Pts',(-0.15103745131,-20.9653225623,-6.62292642142));
#93093=CARTESIAN_POINT('Ctrl Pts',(-0.248193078621,-20.9544277624,-6.59756027965));
#93094=CARTESIAN_POINT('Ctrl Pts',(0.246933661348,-21.0742356173,-6.5991953663));
#93095=CARTESIAN_POINT('Ctrl Pts',(0.15021854742,-21.0742356301,-6.62384075504));
#93096=CARTESIAN_POINT('Ctrl Pts',(0.0504287451839,-21.0742356366,-6.63642024334));
#93097=CARTESIAN_POINT('Ctrl Pts',(-0.0504287451839,-21.0742356366,-6.63642024334));
#93098=CARTESIAN_POINT('Ctrl Pts',(-0.15021854742,-21.0742356301,-6.62384075504));
#93099=CARTESIAN_POINT('Ctrl Pts',(-0.246933661348,-21.0742356173,-6.5991953663));
#93100=CARTESIAN_POINT('Ctrl Pts',(-6.57550091203307E-15,-20.7742356128,
-6.96732100709999));
#93101=CARTESIAN_POINT('Ctrl Pts',(-0.000739046140776542,-20.7742183042276,
-6.96612812943488));
#93102=CARTESIAN_POINT('Ctrl Pts',(-0.00213178760716483,-20.7741874385235,
-6.96388034917257));
#93103=CARTESIAN_POINT('Ctrl Pts',(-0.00418474029193665,-20.7742053701667,
-6.9605765338024));
#93104=CARTESIAN_POINT('Ctrl Pts',(-0.00641465514642071,-20.774224847497,
-6.95698793333194));
#93105=CARTESIAN_POINT('Ctrl Pts',(-0.00942378940812995,-20.7743021658575,
-6.95215281744824));
#93106=CARTESIAN_POINT('Ctrl Pts',(-0.0132219688318108,-20.7745826669425,
-6.94607879927397));
#93107=CARTESIAN_POINT('Ctrl Pts',(-0.0170201482554917,-20.7748631680274,
-6.94000478109969));
#93108=CARTESIAN_POINT('Ctrl Pts',(-0.0216078184058048,-20.7753481037327,
-6.93269120520879));
#93109=CARTESIAN_POINT('Ctrl Pts',(-0.0269904576317545,-20.7762314335538,
-6.9241638748923));
#93110=CARTESIAN_POINT('Ctrl Pts',(-0.0323089928856136,-20.777104243452,
-6.91573809991356));
#93111=CARTESIAN_POINT('Ctrl Pts',(-0.0383968143842043,-20.7783663975252,
-6.9061281889125));
#93112=CARTESIAN_POINT('Ctrl Pts',(-0.0452340558275931,-20.7802380903564,
-6.8953994038545));
#93113=CARTESIAN_POINT('Ctrl Pts',(-0.0485017240992391,-20.7811326135833,
-6.89027188118068));
#93114=CARTESIAN_POINT('Ctrl Pts',(-0.051940429322601,-20.7821668181412,
-6.88488924067781));
#93115=CARTESIAN_POINT('Ctrl Pts',(-0.0555471514172319,-20.7833679719454,
-6.87926140234126));
#93116=CARTESIAN_POINT('Ctrl Pts',(-0.0595526878616734,-20.7847019436826,
-6.87301126413569));
#93117=CARTESIAN_POINT('Ctrl Pts',(-0.063127261239606,-20.7860232276961,
-6.86746021183157));
#93118=CARTESIAN_POINT('Ctrl Pts',(-0.0664331293085701,-20.7873256017318,
-6.86234415039677));
#93119=CARTESIAN_POINT('Ctrl Pts',(-0.0700590269614373,-20.7887540540658,
-6.85673282085748));
#93120=CARTESIAN_POINT('Ctrl Pts',(-0.0733617729652654,-20.7901604262365,
-6.85164463855104));
#93121=CARTESIAN_POINT('Ctrl Pts',(-0.0765514209480796,-20.7915988864223,
-6.84674347698261));
#93122=CARTESIAN_POINT('Ctrl Pts',(-0.0785513039528601,-20.7925007891069,
-6.84367048906131));
#93123=CARTESIAN_POINT('Ctrl Pts',(-0.0805066452710636,-20.7934164265047,
-6.84067126660403));
#93124=CARTESIAN_POINT('Ctrl Pts',(-0.0824682378119286,-20.7943690054015,
-6.83766549654366));
#93125=CARTESIAN_POINT('Ctrl Pts',(-0.0920786456764894,-20.7990359642781,
-6.82293936171931));
#93126=CARTESIAN_POINT('Ctrl Pts',(-0.100960528456615,-20.8041428102936,
-6.80948841419464));
#93127=CARTESIAN_POINT('Ctrl Pts',(-0.109114333331388,-20.8094053876005,
-6.797269946806));
#93128=CARTESIAN_POINT('Ctrl Pts',(-0.114438108000665,-20.8128414246644,
-6.78929227648152));
#93129=CARTESIAN_POINT('Ctrl Pts',(-0.119451716877995,-20.8163450388597,
-6.78183955514836));
#93130=CARTESIAN_POINT('Ctrl Pts',(-0.12415772521919,-20.8198442769267,
-6.77489576919354));
#93131=CARTESIAN_POINT('Ctrl Pts',(-0.130114551502564,-20.824273583417,
-6.76610638258755));
#93132=CARTESIAN_POINT('Ctrl Pts',(-0.135577437715922,-20.82869661386,-6.7581295295839));
#93133=CARTESIAN_POINT('Ctrl Pts',(-0.140483820768466,-20.8329959479912,
-6.75092075220541));
#93134=CARTESIAN_POINT('Ctrl Pts',(-0.142937012294739,-20.8351456150569,
-6.74731636351616));
#93135=CARTESIAN_POINT('Ctrl Pts',(-0.145262555217202,-20.8372633999559,
-6.74390296005163));
#93136=CARTESIAN_POINT('Ctrl Pts',(-0.147467464851545,-20.8393348214145,
-6.74067276188158));
#93137=CARTESIAN_POINT('Ctrl Pts',(-0.148569919668717,-20.8403705321438,
-6.73905766279656));
#93138=CARTESIAN_POINT('Ctrl Pts',(-0.149642232430758,-20.84139465963,-6.73748836687227));
#93139=CARTESIAN_POINT('Ctrl Pts',(-0.150684903317464,-20.8424055801115,
-6.73596387258709));
#93140=CARTESIAN_POINT('Ctrl Pts',(-0.15131977036796,-20.8430211148047,
-6.73503563031748));
#93141=CARTESIAN_POINT('Ctrl Pts',(-0.151588988504639,-20.8432845686164,
-6.73464223535714));
#93142=CARTESIAN_POINT('Ctrl Pts',(-0.152141066761498,-20.8438275612463,
-6.73383575971623));
#93143=CARTESIAN_POINT('Ctrl Pts',(-0.152495691609109,-20.8441763499845,
-6.73331772391659));
#93144=CARTESIAN_POINT('Ctrl Pts',(-0.152967046458675,-20.844640439587,
-6.73262921807131));
#93145=CARTESIAN_POINT('Ctrl Pts',(-0.153724483183895,-20.8453971487028,
-6.73152382693266));
#93146=CARTESIAN_POINT('Ctrl Pts',(-0.165819652379691,-20.8574806990291,
-6.71387232892058));
#93147=CARTESIAN_POINT('Ctrl Pts',(-0.176794399150034,-20.8706467710759,
-6.69801435723457));
#93148=CARTESIAN_POINT('Ctrl Pts',(-0.186589072833805,-20.8845898753631,
-6.68394159693474));
#93149=CARTESIAN_POINT('Ctrl Pts',(-0.196711292295833,-20.8989992539839,
-6.66939822644683));
#93150=CARTESIAN_POINT('Ctrl Pts',(-0.205572200092412,-20.9142354112887,
-6.65676360713048));
#93151=CARTESIAN_POINT('Ctrl Pts',(-0.213142751347805,-20.9299280505707,
-6.64602128475438));
#93152=CARTESIAN_POINT('Ctrl Pts',(-0.220146036668008,-20.9444448310021,
-6.63608389102129));
#93153=CARTESIAN_POINT('Ctrl Pts',(-0.226045896532328,-20.9593494493265,
-6.62776573152344));
#93154=CARTESIAN_POINT('Ctrl Pts',(-0.230849786453082,-20.9743672314828,
-6.62103443567695));
#93155=CARTESIAN_POINT('Ctrl Pts',(-0.235484211608852,-20.9888552377771,
-6.61454059686787));
#93156=CARTESIAN_POINT('Ctrl Pts',(-0.239099720633237,-21.0034475477172,
-6.60952261522757));
#93157=CARTESIAN_POINT('Ctrl Pts',(-0.241718744711677,-21.0179417593159,
-6.60594163792155));
#93158=CARTESIAN_POINT('Ctrl Pts',(-0.244248413806021,-21.0319414622701,
-6.60248283519685));
#93159=CARTESIAN_POINT('Ctrl Pts',(-0.245849619786232,-21.0458498424135,
-6.60036330646126));
#93160=CARTESIAN_POINT('Ctrl Pts',(-0.246540851867042,-21.0595316198178,
-6.59955630271868));
#93161=CARTESIAN_POINT('Ctrl Pts',(-0.24679002646896,-21.0644636123177,
-6.59926539487183));
#93162=CARTESIAN_POINT('Ctrl Pts',(-0.246920851074132,-21.0693665923741,
-6.59914522303046));
#93163=CARTESIAN_POINT('Ctrl Pts',(-0.246933661366624,-21.0742356155283,
-6.59919536627582));
#93164=CARTESIAN_POINT('Origin',(2.84607155346,-21.0742356128,5.53854202767));
#93165=CARTESIAN_POINT('',(-1.05,-20.7742356128,-6.68100624476));
#93166=CARTESIAN_POINT('Ctrl Pts',(-1.05,-20.7742356128,-6.68100624476));
#93167=CARTESIAN_POINT('Ctrl Pts',(-1.03625292470594,-20.7740159455194,
-6.67687310983531));
#93168=CARTESIAN_POINT('Ctrl Pts',(-1.02237382634443,-20.7742867438727,
-6.67269596024792));
#93169=CARTESIAN_POINT('Ctrl Pts',(-1.00846284537523,-20.7749590260321,
-6.6685054782835));
#93170=CARTESIAN_POINT('Ctrl Pts',(-0.993968393349887,-20.7756595058564,
-6.66413923409621));
#93171=CARTESIAN_POINT('Ctrl Pts',(-0.979438879191048,-20.7767959613459,
-6.65975837854857));
#93172=CARTESIAN_POINT('Ctrl Pts',(-0.96494582937768,-20.7783083760812,
-6.65538485104873));
#93173=CARTESIAN_POINT('Ctrl Pts',(-0.949182506410178,-20.7799533495161,
-6.65062799673753));
#93174=CARTESIAN_POINT('Ctrl Pts',(-0.933461830247863,-20.782042980466,
-6.64587966075301));
#93175=CARTESIAN_POINT('Ctrl Pts',(-0.917834461394271,-20.7845474988965,
-6.64115542515622));
#93176=CARTESIAN_POINT('Ctrl Pts',(-0.908284964982968,-20.7860779478152,
-6.63826856228761));
#93177=CARTESIAN_POINT('Ctrl Pts',(-0.898769536443018,-20.7877642505962,
-6.63539046214858));
#93178=CARTESIAN_POINT('Ctrl Pts',(-0.889294615397127,-20.7896072434251,
-6.63252311810195));
#93179=CARTESIAN_POINT('Ctrl Pts',(-0.871011378197203,-20.7931635659407,
-6.62699016103724));
#93180=CARTESIAN_POINT('Ctrl Pts',(-0.852879229238803,-20.797300044157,
-6.62149721776252));
#93181=CARTESIAN_POINT('Ctrl Pts',(-0.834927156599105,-20.8020715544452,
-6.61605309569464));
#93182=CARTESIAN_POINT('Ctrl Pts',(-0.817519370509437,-20.8066983979351,
-6.61077403325401));
#93183=CARTESIAN_POINT('Ctrl Pts',(-0.800278528149882,-20.811923828354,
-6.60554014165193));
#93184=CARTESIAN_POINT('Ctrl Pts',(-0.783241385589988,-20.8178396330701,
-6.60036265094451));
#93185=CARTESIAN_POINT('Ctrl Pts',(-0.766995111590773,-20.8234808246023,
-6.5954255006938));
#93186=CARTESIAN_POINT('Ctrl Pts',(-0.75093240170514,-20.8297509634394,
-6.59053912116687));
#93187=CARTESIAN_POINT('Ctrl Pts',(-0.735123129947809,-20.8367492310671,
-6.58572501216975));
#93188=CARTESIAN_POINT('Ctrl Pts',(-0.721365830513912,-20.8428391550528,
-6.58153575285423));
#93189=CARTESIAN_POINT('Ctrl Pts',(-0.707800285523294,-20.8494811269749,
-6.57740117455926));
#93190=CARTESIAN_POINT('Ctrl Pts',(-0.694511943633331,-20.8567437051301,
-6.57334766925701));
#93191=CARTESIAN_POINT('Ctrl Pts',(-0.681861691477839,-20.8636575432691,
-6.56948880826353));
#93192=CARTESIAN_POINT('Ctrl Pts',(-0.669462246162125,-20.8711341867228,
-6.56570329210059));
#93193=CARTESIAN_POINT('Ctrl Pts',(-0.657430144764881,-20.8792291148818,
-6.56202717171159));
#93194=CARTESIAN_POINT('Ctrl Pts',(-0.646106591108891,-20.8868473480003,
-6.55856753111379));
#93195=CARTESIAN_POINT('Ctrl Pts',(-0.635108251855433,-20.8950134147344,
-6.55520473747399));
#93196=CARTESIAN_POINT('Ctrl Pts',(-0.624574744850416,-20.9037661637504,
-6.55198202898773));
#93197=CARTESIAN_POINT('Ctrl Pts',(-0.615767147388661,-20.9110847794763,
-6.5492873595799));
#93198=CARTESIAN_POINT('Ctrl Pts',(-0.607285106257906,-20.9188135257316,
-6.54669080698833));
#93199=CARTESIAN_POINT('Ctrl Pts',(-0.599236493259071,-20.9269691201472,
-6.54422580515893));
#93200=CARTESIAN_POINT('Ctrl Pts',(-0.590128979800226,-20.9361976898294,
-6.54143650005251));
#93201=CARTESIAN_POINT('Ctrl Pts',(-0.581575283606785,-20.9459732020675,
-6.53881527683606));
#93202=CARTESIAN_POINT('Ctrl Pts',(-0.573774149863334,-20.9563085906836,
-6.53642377787523));
#93203=CARTESIAN_POINT('Ctrl Pts',(-0.56627503412483,-20.9662438485556,
-6.53412486491134));
#93204=CARTESIAN_POINT('Ctrl Pts',(-0.559471283802019,-20.9766965655441,
-6.53203821531165));
#93205=CARTESIAN_POINT('Ctrl Pts',(-0.553583731234507,-20.9876651913132,
-6.53023237010088));
#93206=CARTESIAN_POINT('Ctrl Pts',(-0.547811914458446,-20.9984181990356,
-6.52846202366864));
#93207=CARTESIAN_POINT('Ctrl Pts',(-0.542920470100945,-21.0096671438262,
-6.52696149994591));
#93208=CARTESIAN_POINT('Ctrl Pts',(-0.539162633367657,-21.0213962266405,
-6.52580944852247));
#93209=CARTESIAN_POINT('Ctrl Pts',(-0.535502136482079,-21.0328214891412,
-6.52468723887186));
#93210=CARTESIAN_POINT('Ctrl Pts',(-0.532917204308461,-21.0447024126547,
-6.5238956579284));
#93211=CARTESIAN_POINT('Ctrl Pts',(-0.531686808004321,-21.0570093207758,
-6.52352140235709));
#93212=CARTESIAN_POINT('Ctrl Pts',(-0.53112156681897,-21.062663085592,-6.52334947022267));
#93213=CARTESIAN_POINT('Ctrl Pts',(-0.530842835073694,-21.068406533619,
-6.52326581257046));
#93214=CARTESIAN_POINT('Ctrl Pts',(-0.530881032646531,-21.0742356128,-6.52327988721974));
#93215=CARTESIAN_POINT('Origin',(2.84607155346,-20.7742356128,5.53854202767));
#93216=CARTESIAN_POINT('Origin',(-2.45,-20.1742356128,10.7304528845));
#93217=CARTESIAN_POINT('',(-2.45,-19.6742356128,10.4304528845));
#93218=CARTESIAN_POINT('',(-2.75,-19.6742356128,10.7304528845));
#93219=CARTESIAN_POINT('Origin',(-2.45,-19.6742356128,10.7304528845));
#93220=CARTESIAN_POINT('',(-2.75,-20.6742356128,10.7304528845));
#93221=CARTESIAN_POINT('',(-2.75,-20.1742356128,10.7304528845));
#93222=CARTESIAN_POINT('',(-2.45,-20.6742356128,10.4304528845));
#93223=CARTESIAN_POINT('Origin',(-2.45,-20.6742356128,10.7304528845));
#93224=CARTESIAN_POINT('',(-2.45,-20.1742356128,10.4304528845));
#93225=CARTESIAN_POINT('Origin',(1.47842115491E-15,-21.0742356128,0.729452270839));
#93226=CARTESIAN_POINT('',(-0.992653804111,-21.0742356128,5.82664824081));
#93227=CARTESIAN_POINT('Origin',(2.57175827821E-16,-21.0742356128,0.729452270839));
#93228=CARTESIAN_POINT('',(-1.05,-20.7742356128,6.12111625914));
#93229=CARTESIAN_POINT('Origin',(-1.04999999999979,-21.0742356128,6.12111625913628));
#93230=CARTESIAN_POINT('Origin',(1.126325016E-16,-20.7742356128,0.729452270839));
#93231=CARTESIAN_POINT('Origin',(9.79717439318E-17,-22.3742356128,0.729452270839));
#93232=CARTESIAN_POINT('',(-10.7000575594,-22.3742356128,-2.76302312605));
#93233=CARTESIAN_POINT('',(-10.9449284019,-22.3742356128,-2.34954507713));
#93234=CARTESIAN_POINT('Origin',(-11.0821857629,-22.3742356128,-2.71007990903));
#93235=CARTESIAN_POINT('Origin',(2.84607155346,-22.3742356128,5.53854202767));
#93236=CARTESIAN_POINT('Origin',(2.84607155346,-19.6742356128,5.53854202767));
#93237=CARTESIAN_POINT('',(-11.2744572343,-19.3742356128,-1.7432341771));
#93238=CARTESIAN_POINT('Origin',(-11.2744572343,-19.6742356128,-1.7432341771));
#93239=CARTESIAN_POINT('',(-12.6801076867,-19.3742356128,8.90771939699));
#93240=CARTESIAN_POINT('Origin',(-12.6801076867,-19.6742356128,8.90771939699));
#93241=CARTESIAN_POINT('Origin',(2.84607155346,-19.3742356128,5.53854202767));
#93242=CARTESIAN_POINT('Origin',(-8.94493678676E-16,-19.6742356128,0.580061096523));
#93243=CARTESIAN_POINT('',(-12.1784262599,-19.3742356128,9.98548517727));
#93244=CARTESIAN_POINT('Origin',(-12.1784262599,-19.6742356128,9.98548517727));
#93245=CARTESIAN_POINT('',(-3.05,-19.3742356128,15.662287998));
#93246=CARTESIAN_POINT('Origin',(-3.05,-19.6742356128,15.662287998));
#93247=CARTESIAN_POINT('Origin',(1.21374489213E-15,-19.3742356128,0.580061096523));
#93248=CARTESIAN_POINT('Origin',(-1.01908995768E-15,-19.4742356128,-4.23765442876));
#93249=CARTESIAN_POINT('',(3.35920145722,-19.3742356128,-2.84622762644));
#93250=CARTESIAN_POINT('Origin',(3.35920145722,-19.4742356128,-2.84622762644));
#93251=CARTESIAN_POINT('',(0.153073372946,-19.3742356128,-4.17424936164));
#93252=CARTESIAN_POINT('',(1.75613741508,-19.3742356128,-3.51023849404));
#93253=CARTESIAN_POINT('Origin',(0.153073372946,-19.4742356128,-4.17424936164));
#93254=CARTESIAN_POINT('Origin',(-1.62738508975E-15,-19.4742356128,5.69655897044));
#93255=CARTESIAN_POINT('',(0.153073372946,-19.3742356128,5.63315390332));
#93256=CARTESIAN_POINT('Origin',(0.153073372946,-19.4742356128,5.63315390332));
#93257=CARTESIAN_POINT('',(3.35920145722,-19.3742356128,4.30513216811));
#93258=CARTESIAN_POINT('',(1.75613741508,-19.3742356128,4.96914303572));
#93259=CARTESIAN_POINT('Origin',(3.35920145722,-19.4742356128,4.30513216811));
#93260=CARTESIAN_POINT('Origin',(3.20612808427,-19.4742356128,3.93558035511));
#93261=CARTESIAN_POINT('',(3.57567989727,-19.3742356128,4.08865372805));
#93262=CARTESIAN_POINT('Origin',(3.20612808427,-19.3742356128,3.93558035511));
#93263=CARTESIAN_POINT('Origin',(3.57567989727,-19.4742356128,4.08865372805));
#93264=CARTESIAN_POINT('Origin',(4.11560885829,-19.4742356128,2.78514990766));
#93265=CARTESIAN_POINT('',(4.90370163248,-19.3742356128,0.882525643785));
#93266=CARTESIAN_POINT('',(4.23969076488,-19.3742356128,2.48558968592));
#93267=CARTESIAN_POINT('Origin',(4.90370163248,-19.4742356128,0.882525643785));
#93268=CARTESIAN_POINT('Origin',(4.53414981948,-19.4742356128,0.729452270839));
#93269=CARTESIAN_POINT('',(4.90370163248,-19.3742356128,0.576378897893));
#93270=CARTESIAN_POINT('Origin',(4.53414981948,-19.3742356128,0.729452270839));
#93271=CARTESIAN_POINT('Origin',(4.90370163248,-19.4742356128,0.576378897893));
#93272=CARTESIAN_POINT('Origin',(5.81860454091,-19.4742356128,2.78514990766));
#93273=CARTESIAN_POINT('',(3.57567989727,-19.3742356128,-2.62974918638));
#93274=CARTESIAN_POINT('',(4.23969076488,-19.3742356128,-1.02668514424));
#93275=CARTESIAN_POINT('Origin',(3.57567989727,-19.4742356128,-2.62974918638));
#93276=CARTESIAN_POINT('Origin',(3.20612808427,-19.4742356128,-2.47667581343));
#93277=CARTESIAN_POINT('Origin',(3.20612808427,-19.3742356128,-2.47667581343));
#93278=CARTESIAN_POINT('Origin',(1.61893433855E-15,-19.4742356128,-3.80469754864));
#93279=CARTESIAN_POINT('',(-0.153073372946,-19.3742356128,-4.17424936164));
#93280=CARTESIAN_POINT('Origin',(1.57762160836E-15,-19.3742356128,-3.80469754864));
#93281=CARTESIAN_POINT('Origin',(-0.153073372946,-19.4742356128,-4.17424936164));
#93282=CARTESIAN_POINT('Origin',(-1.01908995768E-15,-19.4742356128,-4.23765442876));
#93283=CARTESIAN_POINT('',(-3.35920145722,-19.3742356128,-2.84622762644));
#93284=CARTESIAN_POINT('',(-1.75613741508,-19.3742356128,-3.51023849404));
#93285=CARTESIAN_POINT('Origin',(-3.35920145722,-19.4742356128,-2.84622762644));
#93286=CARTESIAN_POINT('Origin',(3.14260590599E-16,-19.4742356128,5.26360209032));
#93287=CARTESIAN_POINT('',(-0.153073372946,-19.3742356128,5.63315390332));
#93288=CARTESIAN_POINT('Origin',(-0.153073372946,-19.4742356128,5.63315390332));
#93289=CARTESIAN_POINT('Origin',(1.87729180512E-16,-19.3742356128,5.26360209032));
#93290=CARTESIAN_POINT('Origin',(-1.62738508975E-15,-19.4742356128,5.69655897044));
#93291=CARTESIAN_POINT('',(-3.35920145722,-19.3742356128,4.30513216811));
#93292=CARTESIAN_POINT('Origin',(-3.35920145722,-19.4742356128,4.30513216811));
#93293=CARTESIAN_POINT('',(-1.75613741508,-19.3742356128,4.96914303572));
#93294=CARTESIAN_POINT('Origin',(-3.20612808427,-19.4742356128,3.93558035511));
#93295=CARTESIAN_POINT('',(-3.57567989727,-19.3742356128,4.08865372805));
#93296=CARTESIAN_POINT('Origin',(-3.57567989727,-19.4742356128,4.08865372805));
#93297=CARTESIAN_POINT('Origin',(-3.20612808427,-19.3742356128,3.93558035511));
#93298=CARTESIAN_POINT('Origin',(-4.11560885829,-19.4742356128,2.78514990766));
#93299=CARTESIAN_POINT('',(-4.90370163248,-19.3742356128,0.882525643785));
#93300=CARTESIAN_POINT('Origin',(-4.90370163248,-19.4742356128,0.882525643785));
#93301=CARTESIAN_POINT('',(-4.23969076488,-19.3742356128,2.48558968592));
#93302=CARTESIAN_POINT('Origin',(-4.53414981948,-19.4742356128,0.729452270839));
#93303=CARTESIAN_POINT('',(-4.90370163248,-19.3742356128,0.576378897893));
#93304=CARTESIAN_POINT('Origin',(-4.90370163248,-19.4742356128,0.576378897893));
#93305=CARTESIAN_POINT('Origin',(-4.53414981948,-19.3742356128,0.729452270839));
#93306=CARTESIAN_POINT('Origin',(-5.81860454091,-19.4742356128,2.78514990766));
#93307=CARTESIAN_POINT('',(-3.57567989727,-19.3742356128,-2.62974918638));
#93308=CARTESIAN_POINT('Origin',(-3.57567989727,-19.4742356128,-2.62974918638));
#93309=CARTESIAN_POINT('',(-4.23969076488,-19.3742356128,-1.02668514424));
#93310=CARTESIAN_POINT('Origin',(-3.20612808427,-19.4742356128,-2.47667581343));
#93311=CARTESIAN_POINT('Origin',(-3.20612808427,-19.3742356128,-2.47667581343));
#93312=CARTESIAN_POINT('Origin',(4.65365783676E-16,-19.3742356128,0.729452270839));
#93313=CARTESIAN_POINT('Origin',(-10.0415172382,-19.3742356128,8.33514586886));
#93314=CARTESIAN_POINT('',(-3.05,-19.3742356128,10.7304528845));
#93315=CARTESIAN_POINT('',(-3.05,-19.3742356128,2.96634320571));
#93316=CARTESIAN_POINT('',(-2.45,-19.3742356128,10.1304528845));
#93317=CARTESIAN_POINT('Origin',(-2.45,-19.3742356128,10.7304528845));
#93318=CARTESIAN_POINT('',(-6.6707290414,-19.3742356128,10.1304528845));
#93319=CARTESIAN_POINT('',(-10.3267865236,-19.3742356128,-3.3434289261));
#93320=CARTESIAN_POINT('Origin',(2.84607155346,-19.3742356128,5.53854202767));
#93321=CARTESIAN_POINT('Origin',(-11.0821857629,-19.3742356128,-2.71007990903));
#93322=CARTESIAN_POINT('Ctrl Pts',(1.13381424745833E-15,-19.3742356128,
-10.0919881826));
#93323=CARTESIAN_POINT('Ctrl Pts',(1.13381424745833E-15,-19.3742356128,
-10.0919881826));
#93324=CARTESIAN_POINT('Ctrl Pts',(1.13381424745833E-15,-19.3742356128,
-10.0919881826));
#93325=CARTESIAN_POINT('Ctrl Pts',(1.13381424745833E-15,-19.3742356128,
-10.0919881826));
#93326=CARTESIAN_POINT('Ctrl Pts',(1.13381424745833E-15,-19.3742356128,
-10.0919881826));
#93327=CARTESIAN_POINT('Ctrl Pts',(1.13381424745833E-15,-19.3742356128,
-10.0919881826));
#93328=CARTESIAN_POINT('Ctrl Pts',(-0.0415097842719,-19.3742356128,-10.1079379349));
#93329=CARTESIAN_POINT('Ctrl Pts',(-0.0249058705631,-19.3742356128,-10.1079379349));
#93330=CARTESIAN_POINT('Ctrl Pts',(-0.0083019552457,-19.3742356128,-10.1079379261));
#93331=CARTESIAN_POINT('Ctrl Pts',(0.0083019552457,-19.3742356128,-10.1079379261));
#93332=CARTESIAN_POINT('Ctrl Pts',(0.0249058705631,-19.3742356128,-10.1079379349));
#93333=CARTESIAN_POINT('Ctrl Pts',(0.0415097842719,-19.3742356128,-10.1079379349));
#93334=CARTESIAN_POINT('Ctrl Pts',(-0.0833222863185,-19.3764713196,-10.1232737584));
#93335=CARTESIAN_POINT('Ctrl Pts',(-0.0499933690234,-19.3759012652,-10.1232736299));
#93336=CARTESIAN_POINT('Ctrl Pts',(-0.0166644595934,-19.3756162324,-10.1232735872));
#93337=CARTESIAN_POINT('Ctrl Pts',(0.0166644595551,-19.3756162324,-10.1232735872));
#93338=CARTESIAN_POINT('Ctrl Pts',(0.0499933689979,-19.3759012652,-10.1232736299));
#93339=CARTESIAN_POINT('Ctrl Pts',(0.0833222863185,-19.3764713196,-10.1232737584));
#93340=CARTESIAN_POINT('Ctrl Pts',(-0.125363533497,-19.3807247797,-10.1376350659));
#93341=CARTESIAN_POINT('Ctrl Pts',(-0.0752314126451,-19.3789864318,-10.1378539929));
#93342=CARTESIAN_POINT('Ctrl Pts',(-0.025079356408,-19.378117295,-10.1379634778));
#93343=CARTESIAN_POINT('Ctrl Pts',(0.0250793561827,-19.378117295,-10.1379634778));
#93344=CARTESIAN_POINT('Ctrl Pts',(0.0752314124954,-19.3789864318,-10.1378539929));
#93345=CARTESIAN_POINT('Ctrl Pts',(0.125363533497,-19.3807247797,-10.1376350659));
#93346=CARTESIAN_POINT('Ctrl Pts',(-0.214270880278,-19.3937598094,-10.1664794265));
#93347=CARTESIAN_POINT('Ctrl Pts',(-0.128662254182,-19.3884633982,-10.1680588961));
#93348=CARTESIAN_POINT('Ctrl Pts',(-0.0429040381187,-19.3858130556,-10.1688486495));
#93349=CARTESIAN_POINT('Ctrl Pts',(0.0429040383692,-19.3858130556,-10.1688486495));
#93350=CARTESIAN_POINT('Ctrl Pts',(0.128662254349,-19.3884633982,-10.1680588961));
#93351=CARTESIAN_POINT('Ctrl Pts',(0.214270880278,-19.3937598094,-10.1664794265));
#93352=CARTESIAN_POINT('Ctrl Pts',(-0.302878944992,-19.4154221962,-10.1917028607));
#93353=CARTESIAN_POINT('Ctrl Pts',(-0.182097857803,-19.4049779364,-10.197316357));
#93354=CARTESIAN_POINT('Ctrl Pts',(-0.0607613296063,-19.3997406668,-10.2001306891));
#93355=CARTESIAN_POINT('Ctrl Pts',(0.0607613293279,-19.3997406668,-10.2001306891));
#93356=CARTESIAN_POINT('Ctrl Pts',(0.182097857618,-19.4049779364,-10.197316357));
#93357=CARTESIAN_POINT('Ctrl Pts',(0.302878944991,-19.4154221962,-10.1917028607));
#93358=CARTESIAN_POINT('Ctrl Pts',(-0.349011853831,-19.4292028661,-10.2039820431));
#93359=CARTESIAN_POINT('Ctrl Pts',(-0.209987919386,-19.4158427429,-10.2126719835));
#93360=CARTESIAN_POINT('Ctrl Pts',(-0.070093390793,-19.4091363298,-10.2170325701));
#93361=CARTESIAN_POINT('Ctrl Pts',(0.070093395411,-19.4091363298,-10.2170325701));
#93362=CARTESIAN_POINT('Ctrl Pts',(0.209987922457,-19.4158427429,-10.2126719835));
#93363=CARTESIAN_POINT('Ctrl Pts',(0.349011853831,-19.4292028661,-10.2039820431));
#93364=CARTESIAN_POINT('Ctrl Pts',(-0.414201204383,-19.4525352086,-10.2201075969));
#93365=CARTESIAN_POINT('Ctrl Pts',(-0.249526732723,-19.4351881568,-10.2348601694));
#93366=CARTESIAN_POINT('Ctrl Pts',(-0.0833448932135,-19.4264619682,-10.24227702));
#93367=CARTESIAN_POINT('Ctrl Pts',(0.0833448912668,-19.4264619682,-10.24227702));
#93368=CARTESIAN_POINT('Ctrl Pts',(0.249526731429,-19.4351881568,-10.2348601694));
#93369=CARTESIAN_POINT('Ctrl Pts',(0.414201204383,-19.4525352086,-10.2201075969));
#93370=CARTESIAN_POINT('Ctrl Pts',(-0.476889168989,-19.4827229707,-10.2341511354));
#93371=CARTESIAN_POINT('Ctrl Pts',(-0.287745576237,-19.4629708985,-10.2572820885));
#93372=CARTESIAN_POINT('Ctrl Pts',(-0.0961879175727,-19.453011347,-10.2689444929));
#93373=CARTESIAN_POINT('Ctrl Pts',(0.0961879183933,-19.453011347,-10.2689444929));
#93374=CARTESIAN_POINT('Ctrl Pts',(0.287745576783,-19.4629708985,-10.2572820885));
#93375=CARTESIAN_POINT('Ctrl Pts',(0.476889168989,-19.4827229707,-10.2341511354));
#93376=CARTESIAN_POINT('Ctrl Pts',(-0.495216410211,-19.492424266,-10.2381345523));
#93377=CARTESIAN_POINT('Ctrl Pts',(-0.298936557215,-19.4721609989,-10.2639381086));
#93378=CARTESIAN_POINT('Ctrl Pts',(-0.0999515182904,-19.4619368311,-10.2769563707));
#93379=CARTESIAN_POINT('Ctrl Pts',(0.09995152576,-19.4619368311,-10.2769563707));
#93380=CARTESIAN_POINT('Ctrl Pts',(0.298936562175,-19.4721609989,-10.2639381086));
#93381=CARTESIAN_POINT('Ctrl Pts',(0.495216410211,-19.492424266,-10.2381345523));
#93382=CARTESIAN_POINT('Ctrl Pts',(-0.548607288051,-19.5230709178,-10.2493705418));
#93383=CARTESIAN_POINT('Ctrl Pts',(-0.331601042239,-19.50197069,-10.2837483093));
#93384=CARTESIAN_POINT('Ctrl Pts',(-0.110947746796,-19.4913020672,-10.3011245839));
#93385=CARTESIAN_POINT('Ctrl Pts',(0.110947732078,-19.4913020672,-10.3011245839));
#93386=CARTESIAN_POINT('Ctrl Pts',(0.331601032464,-19.50197069,-10.2837483093));
#93387=CARTESIAN_POINT('Ctrl Pts',(0.548607288052,-19.5230709178,-10.2493705418));
#93388=CARTESIAN_POINT('Ctrl Pts',(-0.596976385661,-19.562200797,-10.2586626864));
#93389=CARTESIAN_POINT('Ctrl Pts',(-0.361343872845,-19.5433606575,-10.3026842693));
#93390=CARTESIAN_POINT('Ctrl Pts',(-0.120986572931,-19.5338129691,-10.3249810452));
#93391=CARTESIAN_POINT('Ctrl Pts',(0.120986601929,-19.5338129691,-10.3249810452));
#93392=CARTESIAN_POINT('Ctrl Pts',(0.36134389211,-19.5433606575,-10.3026842693));
#93393=CARTESIAN_POINT('Ctrl Pts',(0.596976385661,-19.562200797,-10.2586626864));
#93394=CARTESIAN_POINT('Ctrl Pts',(-0.628284771894,-19.5926160239,-10.2642394886));
#93395=CARTESIAN_POINT('Ctrl Pts',(-0.380691753868,-19.576871863,-10.3156638409));
#93396=CARTESIAN_POINT('Ctrl Pts',(-0.127533759232,-19.5688752663,-10.3417537086));
#93397=CARTESIAN_POINT('Ctrl Pts',(0.127533760988,-19.5688752663,-10.3417537086));
#93398=CARTESIAN_POINT('Ctrl Pts',(0.380691755013,-19.576871863,-10.3156638409));
#93399=CARTESIAN_POINT('Ctrl Pts',(0.628284771894,-19.5926160239,-10.2642394886));
#93400=CARTESIAN_POINT('Ctrl Pts',(-0.647446102181,-19.633156143,-10.2675153591));
#93401=CARTESIAN_POINT('Ctrl Pts',(-0.392565377877,-19.6252559631,-10.3238501103));
#93402=CARTESIAN_POINT('Ctrl Pts',(-0.131557494297,-19.6212431604,-10.3524631664));
#93403=CARTESIAN_POINT('Ctrl Pts',(0.131557494286,-19.6212431604,-10.3524631664));
#93404=CARTESIAN_POINT('Ctrl Pts',(0.392565377877,-19.6252559631,-10.3238501103));
#93405=CARTESIAN_POINT('Ctrl Pts',(0.647446102181,-19.633156143,-10.2675153591));
#93406=CARTESIAN_POINT('Ctrl Pts',(-0.647446102181,-19.6742356128,-10.2675153591));
#93407=CARTESIAN_POINT('Ctrl Pts',(-0.392565377877,-19.6742356128,-10.3238501103));
#93408=CARTESIAN_POINT('Ctrl Pts',(-0.131557494527,-19.6742356128,-10.3524631675));
#93409=CARTESIAN_POINT('Ctrl Pts',(0.131557494527,-19.6742356128,-10.3524631675));
#93410=CARTESIAN_POINT('Ctrl Pts',(0.392565377877,-19.6742356128,-10.3238501103));
#93411=CARTESIAN_POINT('Ctrl Pts',(0.647446102181,-19.6742356128,-10.2675153591));
#93412=CARTESIAN_POINT('Ctrl Pts',(-0.647446102181,-19.6742356128,-10.2675153591));
#93413=CARTESIAN_POINT('Ctrl Pts',(-0.647445941636813,-19.6661001011575,
-10.2675153945841));
#93414=CARTESIAN_POINT('Ctrl Pts',(-0.646542770743725,-19.6579947206812,
-10.2673610476357));
#93415=CARTESIAN_POINT('Ctrl Pts',(-0.6448617348847,-19.6500513204232,-10.2670699532246));
#93416=CARTESIAN_POINT('Ctrl Pts',(-0.643110060949621,-19.6417741340008,
-10.266766626862));
#93417=CARTESIAN_POINT('Ctrl Pts',(-0.640514331113089,-19.633672486467,
-10.266314905712));
#93418=CARTESIAN_POINT('Ctrl Pts',(-0.637226684371121,-19.6258364904321,
-10.2657366368423));
#93419=CARTESIAN_POINT('Ctrl Pts',(-0.633683129499015,-19.6173905459294,
-10.265113355927));
#93420=CARTESIAN_POINT('Ctrl Pts',(-0.629336605338115,-19.6092529554109,
-10.2643431920501));
#93421=CARTESIAN_POINT('Ctrl Pts',(-0.624378482864707,-19.6014736015796,
-10.2634539338467));
#93422=CARTESIAN_POINT('Ctrl Pts',(-0.620736150240958,-19.5957587378579,
-10.2628006675785));
#93423=CARTESIAN_POINT('Ctrl Pts',(-0.616763848379759,-19.5902357668082,
-10.2620831507));
#93424=CARTESIAN_POINT('Ctrl Pts',(-0.612533267931434,-19.5849072924126,
-10.2613118426351));
#93425=CARTESIAN_POINT('Ctrl Pts',(-0.606480198733363,-19.5772833683127,
-10.2602082633161));
#93426=CARTESIAN_POINT('Ctrl Pts',(-0.59990047287895,-19.5700585023242,
-10.2589948789287));
#93427=CARTESIAN_POINT('Ctrl Pts',(-0.592977788625539,-19.5632046643295,
-10.2576984743346));
#93428=CARTESIAN_POINT('Ctrl Pts',(-0.586303368636261,-19.556596621605,
-10.2564485619567));
#93429=CARTESIAN_POINT('Ctrl Pts',(-0.579310981101092,-19.550332062835,
-10.2551216113969));
#93430=CARTESIAN_POINT('Ctrl Pts',(-0.572123283687863,-19.544366280316,
-10.2537352999208));
#93431=CARTESIAN_POINT('Ctrl Pts',(-0.565452398298276,-19.5388294513213,
-10.2524486674376));
#93432=CARTESIAN_POINT('Ctrl Pts',(-0.558613515362534,-19.5335490260034,
-10.2511109441));
#93433=CARTESIAN_POINT('Ctrl Pts',(-0.551661093300188,-19.5284883850772,
-10.2497295965832));
#93434=CARTESIAN_POINT('Ctrl Pts',(-0.547611964544735,-19.5255410400353,
-10.2489250922103));
#93435=CARTESIAN_POINT('Ctrl Pts',(-0.543523480221757,-19.5226682993563,
-10.2481056613876));
#93436=CARTESIAN_POINT('Ctrl Pts',(-0.539398338224439,-19.5198645633611,
-10.247271538349));
#93437=CARTESIAN_POINT('Ctrl Pts',(-0.536480092791513,-19.5178811189686,
-10.2466814554502));
#93438=CARTESIAN_POINT('Ctrl Pts',(-0.533543376246939,-19.5159322357429,
-10.246084000407));
#93439=CARTESIAN_POINT('Ctrl Pts',(-0.530587106428603,-19.5140165822185,
-10.2454789413881));
#93440=CARTESIAN_POINT('Ctrl Pts',(-0.522248905685559,-19.5086134544183,
-10.2437723638863));
#93441=CARTESIAN_POINT('Ctrl Pts',(-0.513755279272081,-19.503470639622,
-10.2420051344035));
#93442=CARTESIAN_POINT('Ctrl Pts',(-0.505148889126634,-19.4985340614123,
-10.2401816464316));
#93443=CARTESIAN_POINT('Ctrl Pts',(-0.493851874114429,-19.4920541555282,
-10.2377880794837));
#93444=CARTESIAN_POINT('Ctrl Pts',(-0.482361393685303,-19.4859314445867,
-10.235297811603));
#93445=CARTESIAN_POINT('Ctrl Pts',(-0.470738754303351,-19.4801299566937,
-10.2327185873485));
#93446=CARTESIAN_POINT('Ctrl Pts',(-0.460415430607163,-19.4749770275293,
-10.2304276991958));
#93447=CARTESIAN_POINT('Ctrl Pts',(-0.44998689248508,-19.4700825616961,
-10.2280666991948));
#93448=CARTESIAN_POINT('Ctrl Pts',(-0.439477083766254,-19.4654176369213,
-10.2256374783638));
#93449=CARTESIAN_POINT('Ctrl Pts',(-0.422732203090843,-19.4579851887387,
-10.2217670927042));
#93450=CARTESIAN_POINT('Ctrl Pts',(-0.405782552671417,-19.4511239727718,
-10.2177231721969));
#93451=CARTESIAN_POINT('Ctrl Pts',(-0.388710157357095,-19.4447597442073,
-10.2135127613696));
#93452=CARTESIAN_POINT('Ctrl Pts',(-0.381260998107146,-19.4419828548953,
-10.2116756424309));
#93453=CARTESIAN_POINT('Ctrl Pts',(-0.373787812289178,-19.4393009012942,
-10.2098067387429));
#93454=CARTESIAN_POINT('Ctrl Pts',(-0.366294824663843,-19.436709133715,
-10.2079062805535));
#93455=CARTESIAN_POINT('Ctrl Pts',(-0.345601093381887,-19.4295513290432,
-10.2026576970711));
#93456=CARTESIAN_POINT('Ctrl Pts',(-0.324759283924013,-19.4230782905106,
-10.197168887497));
#93457=CARTESIAN_POINT('Ctrl Pts',(-0.303821610594384,-19.4172207371684,
-10.1914391367788));
#93458=CARTESIAN_POINT('Ctrl Pts',(-0.282246141989557,-19.4111847533106,
-10.185534848619));
#93459=CARTESIAN_POINT('Ctrl Pts',(-0.260564896862457,-19.4058026301278,
-10.1793742687788));
#93460=CARTESIAN_POINT('Ctrl Pts',(-0.238824865074793,-19.4010423842632,
-10.1729531784551));
#93461=CARTESIAN_POINT('Ctrl Pts',(-0.229060950242532,-19.3989044556871,
-10.1700693289897));
#93462=CARTESIAN_POINT('Ctrl Pts',(-0.219285416886937,-19.3968925139675,
-10.1671329286478));
#93463=CARTESIAN_POINT('Ctrl Pts',(-0.209505275647252,-19.3950061365628,
-10.1641437615851));
#93464=CARTESIAN_POINT('Ctrl Pts',(-0.186799713516908,-19.3906267254363,
-10.1572041155416));
#93465=CARTESIAN_POINT('Ctrl Pts',(-0.164070264338569,-19.3869226098162,
-10.1499848160957));
#93466=CARTESIAN_POINT('Ctrl Pts',(-0.141363992467237,-19.383901171999,
-10.1424921906684));
#93467=CARTESIAN_POINT('Ctrl Pts',(-0.1176844998854,-19.3807502313785,-10.1346784214494));
#93468=CARTESIAN_POINT('Ctrl Pts',(-0.0940309082477135,-19.3783415049,-10.126561853247));
#93469=CARTESIAN_POINT('Ctrl Pts',(-0.0704547890620564,-19.376712860041,
-10.118136804536));
#93470=CARTESIAN_POINT('Ctrl Pts',(-0.0515376158941429,-19.3754060564664,
-10.111376654396));
#93471=CARTESIAN_POINT('Ctrl Pts',(-0.0326704350502771,-19.3746020563644,
-10.1044164174881));
#93472=CARTESIAN_POINT('Ctrl Pts',(-0.0138743237156372,-19.3743346947001,
-10.0972858826397));
#93473=CARTESIAN_POINT('Ctrl Pts',(-0.00924519296368537,-19.3742688485216,
-10.0955297652409));
#93474=CARTESIAN_POINT('Ctrl Pts',(-0.00462033833946646,-19.3742356128,
-10.09376354789));
#93475=CARTESIAN_POINT('Ctrl Pts',(-1.46021229138484E-14,-19.3742356128,
-10.0919881826));
#93476=CARTESIAN_POINT('Origin',(2.84607155346,-19.6742356128,5.53854202767));
#93477=CARTESIAN_POINT('Ctrl Pts',(-10.3267865236,-19.3742356128,-3.3434289261));
#93478=CARTESIAN_POINT('Ctrl Pts',(-10.3387312196063,-19.3742356127965,
-3.3514827927929));
#93479=CARTESIAN_POINT('Ctrl Pts',(-10.3502659022817,-19.3752737080098,
-3.35929500283175));
#93480=CARTESIAN_POINT('Ctrl Pts',(-10.3612964278539,-19.3771435879029,
-3.366782731296));
#93481=CARTESIAN_POINT('Ctrl Pts',(-10.3726225546623,-19.3790635777208,
-3.37447111944563));
#93482=CARTESIAN_POINT('Ctrl Pts',(-10.3834174120365,-19.3818597256152,
-3.38181758261816));
#93483=CARTESIAN_POINT('Ctrl Pts',(-10.3936260273276,-19.3853112756837,
-3.38876386993635));
#93484=CARTESIAN_POINT('Ctrl Pts',(-10.404292680099,-19.3889176889978,-3.39602182145676));
#93485=CARTESIAN_POINT('Ctrl Pts',(-10.4143196241775,-19.393238865228,-3.40284309446403));
#93486=CARTESIAN_POINT('Ctrl Pts',(-10.4236902973134,-19.3980382520255,
-3.40919213448965));
#93487=CARTESIAN_POINT('Ctrl Pts',(-10.4288958013969,-19.4007043601279,
-3.4127190906966));
#93488=CARTESIAN_POINT('Ctrl Pts',(-10.4338995668108,-19.4035183843968,
-3.41610084279332));
#93489=CARTESIAN_POINT('Ctrl Pts',(-10.4387038417048,-19.4064428549585,
-3.41933470452082));
#93490=CARTESIAN_POINT('Ctrl Pts',(-10.4479416835707,-19.4120661378027,
-3.42555289642579));
#93491=CARTESIAN_POINT('Ctrl Pts',(-10.4564343914218,-19.4180968666509,
-3.43123772413905));
#93492=CARTESIAN_POINT('Ctrl Pts',(-10.4642110658934,-19.4243032304506,
-3.43642557350015));
#93493=CARTESIAN_POINT('Ctrl Pts',(-10.468973720738,-19.4281041827376,-3.43960275881023));
#93494=CARTESIAN_POINT('Ctrl Pts',(-10.4734684907843,-19.4319718023247,
-3.44259400325187));
#93495=CARTESIAN_POINT('Ctrl Pts',(-10.477706871939,-19.4358603802918,-3.44541093680795));
#93496=CARTESIAN_POINT('Ctrl Pts',(-10.4832863710631,-19.4409793907275,
-3.44911921073018));
#93497=CARTESIAN_POINT('Ctrl Pts',(-10.4884211141688,-19.4461343216654,
-3.45252637078225));
#93498=CARTESIAN_POINT('Ctrl Pts',(-10.4931417652086,-19.4512367616961,
-3.45566728613861));
#93499=CARTESIAN_POINT('Ctrl Pts',(-10.4955020907286,-19.4537879817114,
-3.45723774381679));
#93500=CARTESIAN_POINT('Ctrl Pts',(-10.497758968688,-19.4563263498715,-3.45874172903051));
#93501=CARTESIAN_POINT('Ctrl Pts',(-10.4999165611424,-19.4588423794387,
-3.460183992036));
#93502=CARTESIAN_POINT('Ctrl Pts',(-10.5010151617041,-19.4601234886168,
-3.46091836193272));
#93503=CARTESIAN_POINT('Ctrl Pts',(-10.5018334456779,-19.4610958633222,
-3.46146508757472));
#93504=CARTESIAN_POINT('Ctrl Pts',(-10.5027639399852,-19.4622174177238,
-3.46208908760247));
#93505=CARTESIAN_POINT('Ctrl Pts',(-10.5036608864843,-19.4632985358844,
-3.46269059008983));
#93506=CARTESIAN_POINT('Ctrl Pts',(-10.5046628965481,-19.4645174989002,
-3.4633644336224));
#93507=CARTESIAN_POINT('Ctrl Pts',(-10.5060957679725,-19.4663149543736,
-3.46433051713108));
#93508=CARTESIAN_POINT('Ctrl Pts',(-10.5163491930108,-19.4791772912472,
-3.47124367393553));
#93509=CARTESIAN_POINT('Ctrl Pts',(-10.5254908828199,-19.4929441876984,
-3.47740738103718));
#93510=CARTESIAN_POINT('Ctrl Pts',(-10.5334831428677,-19.5073425987759,
-3.48279617293412));
#93511=CARTESIAN_POINT('Ctrl Pts',(-10.5419680711657,-19.5226285735648,
-3.48851714704963));
#93512=CARTESIAN_POINT('Ctrl Pts',(-10.549157878795,-19.5386258135561,-3.49336498501857));
#93513=CARTESIAN_POINT('Ctrl Pts',(-10.5550496559692,-19.5550381187943,
-3.49733766485271));
#93514=CARTESIAN_POINT('Ctrl Pts',(-10.5611683702378,-19.5720825865791,
-3.5014633627647));
#93515=CARTESIAN_POINT('Ctrl Pts',(-10.5658877319341,-19.5895745010765,
-3.50464558914306));
#93516=CARTESIAN_POINT('Ctrl Pts',(-10.5692405803808,-19.607219645542,-3.506906418514));
#93517=CARTESIAN_POINT('Ctrl Pts',(-10.572797265971,-19.6259375303653,-3.50930469549345));
#93518=CARTESIAN_POINT('Ctrl Pts',(-10.5748167551615,-19.6448277038803,
-3.51066648913781));
#93519=CARTESIAN_POINT('Ctrl Pts',(-10.5753692578738,-19.663583483134,-3.51103905824762));
#93520=CARTESIAN_POINT('Ctrl Pts',(-10.5754740112682,-19.6671395408632,
-3.51110969659566));
#93521=CARTESIAN_POINT('Ctrl Pts',(-10.5755261020433,-19.6706908911756,
-3.51114482325917));
#93522=CARTESIAN_POINT('Ctrl Pts',(-10.5755261020433,-19.6742356128,-3.51114482325917));
#93523=CARTESIAN_POINT('Origin',(-11.0821857629,-19.6742356128,-2.71007990903));
#93524=CARTESIAN_POINT('',(-10.5566756949,-19.6742356128,-3.15068305993));
#93525=CARTESIAN_POINT('Origin',(-10.3267865236,-19.6742356128,-3.3434289261));
#93526=CARTESIAN_POINT('',(-11.2159436339,-19.6742356128,-2.03747244546));
#93527=CARTESIAN_POINT('Origin',(-11.0821857629,-19.6742356128,-2.71007990903));
#93528=CARTESIAN_POINT('Origin',(-11.2744572342983,-19.6742356128,-1.74323417709617));
#93529=CARTESIAN_POINT('Origin',(-12.5441720511,-22.5760378048,9.34841724773));
#93530=CARTESIAN_POINT('',(-12.8222448081,-25.4742356128,9.46100295649));
#93531=CARTESIAN_POINT('Origin',(-12.5441720511,-25.4742356128,9.34841724773));
#93532=CARTESIAN_POINT('',(-12.8222448231109,-23.4742356815,9.46100293550673));
#93533=CARTESIAN_POINT('',(-12.8222448081,-21.2742356128,9.46100295649));
#93534=CARTESIAN_POINT('Origin',(-12.5441720511,-23.47423564715,9.34841724773));
#93535=CARTESIAN_POINT('Origin',(-12.5441720511,-25.4742356128,9.34841724773));
#93536=CARTESIAN_POINT('Origin',(-12.5441720511,-25.4742356128,9.34841724773));
#93537=CARTESIAN_POINT('Origin',(-10.0415172382,-25.4742356128,8.33514586886));
#93538=CARTESIAN_POINT('Origin',(-10.0415172382,-25.4742356128,8.33514586886));
#93539=CARTESIAN_POINT('Origin',(-10.0415172382,-19.6742356128,8.33514586886));
#93540=CARTESIAN_POINT('Origin',(-10.0415172382,-19.6742356128,8.33514586886));
#93541=CARTESIAN_POINT('Origin',(-10.0415172382,-21.2742356128,8.33514586886));
#93542=CARTESIAN_POINT('Ctrl Pts',(-12.822244843051,-23.4742356815,9.46100291845212));
#93543=CARTESIAN_POINT('Ctrl Pts',(-12.8222448374688,-23.4526557884998,
9.46100292804296));
#93544=CARTESIAN_POINT('Ctrl Pts',(-12.8227658011016,-23.4310761714824,
9.459718249267));
#93545=CARTESIAN_POINT('Ctrl Pts',(-12.8237956782946,-23.4096767931088,
9.45716500907838));
#93546=CARTESIAN_POINT('Ctrl Pts',(-12.8249218353694,-23.3862768561876,
9.45437307473734));
#93547=CARTESIAN_POINT('Ctrl Pts',(-12.8266564446377,-23.3630965146334,
9.45006425351064));
#93548=CARTESIAN_POINT('Ctrl Pts',(-12.8289489787169,-23.3403539792507,
9.4443040829754));
#93549=CARTESIAN_POINT('Ctrl Pts',(-12.8312709606729,-23.3173193132581,
9.43846992235491));
#93550=CARTESIAN_POINT('Ctrl Pts',(-12.8341646949754,-23.2947342337854,
9.43114748157285));
#93551=CARTESIAN_POINT('Ctrl Pts',(-12.8375494613154,-23.2727938554516,
9.42244323588751));
#93552=CARTESIAN_POINT('Ctrl Pts',(-12.8410023873676,-23.250411659361,9.41356371107774));
#93553=CARTESIAN_POINT('Ctrl Pts',(-12.8449656668396,-23.2287009550523,
9.40324680779877));
#93554=CARTESIAN_POINT('Ctrl Pts',(-12.8493339497345,-23.2078282931751,
9.39163588847771));
#93555=CARTESIAN_POINT('Ctrl Pts',(-12.8533668576591,-23.1885581301571,
9.38091639762304));
#93556=CARTESIAN_POINT('Ctrl Pts',(-12.8577443119826,-23.1700021065795,
9.36909474059184));
#93557=CARTESIAN_POINT('Ctrl Pts',(-12.8623765483007,-23.1522553698924,
9.35629852758267));
#93558=CARTESIAN_POINT('Ctrl Pts',(-12.8676258737502,-23.1321444795705,
9.34179765111725));
#93559=CARTESIAN_POINT('Ctrl Pts',(-12.8732011777363,-23.1130741318264,
9.3260463447321));
#93560=CARTESIAN_POINT('Ctrl Pts',(-12.8789692176796,-23.0951288263937,
9.30924271806145));
#93561=CARTESIAN_POINT('Ctrl Pts',(-12.8847323055415,-23.0771989276877,
9.29245351794285));
#93562=CARTESIAN_POINT('Ctrl Pts',(-12.8906877245128,-23.0603914552665,
9.27461404125843));
#93563=CARTESIAN_POINT('Ctrl Pts',(-12.8967175034202,-23.0447417766193,
9.25591265355548));
#93564=CARTESIAN_POINT('Ctrl Pts',(-12.9032960762988,-23.0276677589662,
9.23550917876373));
#93565=CARTESIAN_POINT('Ctrl Pts',(-12.909961941791,-23.0119710592708,9.21408281923307));
#93566=CARTESIAN_POINT('Ctrl Pts',(-12.9165837263722,-22.997646095339,9.1918614547601));
#93567=CARTESIAN_POINT('Ctrl Pts',(-12.9229613039847,-22.9838494264575,
9.17045959928658));
#93568=CARTESIAN_POINT('Ctrl Pts',(-12.9292980187867,-22.9713240464602,
9.14832050002835));
#93569=CARTESIAN_POINT('Ctrl Pts',(-12.9354980002173,-22.9600302011921,
9.12562740036042));
#93570=CARTESIAN_POINT('Ctrl Pts',(-12.9422358704374,-22.9477565412539,
9.10096552642308));
#93571=CARTESIAN_POINT('Ctrl Pts',(-12.9488130289529,-22.9369364542937,
9.07564536621217));
#93572=CARTESIAN_POINT('Ctrl Pts',(-12.9551362385969,-22.9274915788356,
9.04986970620133));
#93573=CARTESIAN_POINT('Ctrl Pts',(-12.9614594482409,-22.9180467033774,
9.02409404619048));
#93574=CARTESIAN_POINT('Ctrl Pts',(-12.9675285501681,-22.9099757205391,
8.99786337398523));
#93575=CARTESIAN_POINT('Ctrl Pts',(-12.9732844031999,-22.9031898545,8.97133867789998));
#93576=CARTESIAN_POINT('Ctrl Pts',(-10.5755260924,-22.0742355256,-3.51114484425));
#93577=CARTESIAN_POINT('Ctrl Pts',(-10.6188297183,-22.0742355492,-3.44692120094));
#93578=CARTESIAN_POINT('Ctrl Pts',(-10.6414054613,-22.0742355727,-3.36872151284));
#93579=CARTESIAN_POINT('Ctrl Pts',(-10.6370511822,-22.0742355929,-3.28545797344));
#93580=CARTESIAN_POINT('Ctrl Pts',(-10.6064419603,-22.0742356067,-3.21003960317));
#93581=CARTESIAN_POINT('Ctrl Pts',(-10.5566756907,-22.0742356132,-3.15068306769));
#93582=CARTESIAN_POINT('Ctrl Pts',(-10.5755260601,-22.166010044,-3.51114490853));
#93583=CARTESIAN_POINT('Ctrl Pts',(-10.6188296919,-22.1536827124,-3.44692125214));
#93584=CARTESIAN_POINT('Ctrl Pts',(-10.6414054404,-22.1413553808,-3.36872155059));
#93585=CARTESIAN_POINT('Ctrl Pts',(-10.6370511655,-22.1307558548,-3.28545799936));
#93586=CARTESIAN_POINT('Ctrl Pts',(-10.6064419458,-22.1235274771,-3.21003962102));
#93587=CARTESIAN_POINT('Ctrl Pts',(-10.5566756767,-22.1201229434,-3.15068308186));
#93588=CARTESIAN_POINT('Ctrl Pts',(-10.5859201877,-22.2577874429,-3.49572587157));
#93589=CARTESIAN_POINT('Ctrl Pts',(-10.6278514281,-22.233131778,-3.43337939424));
#93590=CARTESIAN_POINT('Ctrl Pts',(-10.6489702842,-22.208476113,-3.35703447733));
#93591=CARTESIAN_POINT('Ctrl Pts',(-10.6432450252,-22.1872763848,-3.27537017178));
#93592=CARTESIAN_POINT('Ctrl Pts',(-10.6115652008,-22.1728195852,-3.20109406558));
#93593=CARTESIAN_POINT('Ctrl Pts',(-10.5611420569,-22.1660113751,-3.14236541304));
#93594=CARTESIAN_POINT('Ctrl Pts',(-10.6066865316,-22.3446142249,-3.46495847428));
#93595=CARTESIAN_POINT('Ctrl Pts',(-10.6458822742,-22.3082051755,-3.40634319147));
#93596=CARTESIAN_POINT('Ctrl Pts',(-10.6640744247,-22.271796126,-3.33367204908));
#93597=CARTESIAN_POINT('Ctrl Pts',(-10.6555763229,-22.2405343767,-3.25514874825));
#93598=CARTESIAN_POINT('Ctrl Pts',(-10.6217403852,-22.2193079256,-3.18308999607));
#93599=CARTESIAN_POINT('Ctrl Pts',(-10.5700204128,-22.2094250148,-3.125562098));
#93600=CARTESIAN_POINT('Ctrl Pts',(-10.674845259,-22.520870984,-3.36284445229));
#93601=CARTESIAN_POINT('Ctrl Pts',(-10.7051567944,-22.4603981097,-3.31661379633));
#93602=CARTESIAN_POINT('Ctrl Pts',(-10.7138373508,-22.3999252353,-3.25613169144));
#93603=CARTESIAN_POINT('Ctrl Pts',(-10.6962772721,-22.3481414788,-3.18810636174));
#93604=CARTESIAN_POINT('Ctrl Pts',(-10.6552160972,-22.313296938,-3.12357064819));
#93605=CARTESIAN_POINT('Ctrl Pts',(-10.5989042983,-22.2975531745,-3.07021211854));
#93606=CARTESIAN_POINT('Ctrl Pts',(-10.7768953898,-22.6311647495,-3.20613583022));
#93607=CARTESIAN_POINT('Ctrl Pts',(-10.7945590475,-22.5536945709,-3.178366012));
#93608=CARTESIAN_POINT('Ctrl Pts',(-10.7886824067,-22.4762243923,-3.13547322182));
#93609=CARTESIAN_POINT('Ctrl Pts',(-10.7562408317,-22.4108351721,-3.08179482002));
#93610=CARTESIAN_POINT('Ctrl Pts',(-10.7028434694,-22.368886031,-3.02683000685));
#93611=CARTESIAN_POINT('Ctrl Pts',(-10.6386344625,-22.3527003413,-2.97820952919));
#93612=CARTESIAN_POINT('Ctrl Pts',(-10.8408451958,-22.6662436275,-3.10591749488));
#93613=CARTESIAN_POINT('Ctrl Pts',(-10.8508648422,-22.5823049863,-3.08975078999));
#93614=CARTESIAN_POINT('Ctrl Pts',(-10.835946736,-22.4983663451,-3.05779148046));
#93615=CARTESIAN_POINT('Ctrl Pts',(-10.7939944577,-22.4282060593,-3.01294781655));
#93616=CARTESIAN_POINT('Ctrl Pts',(-10.7324020912,-22.3847322352,-2.96381562098));
#93617=CARTESIAN_POINT('Ctrl Pts',(-10.6626475871,-22.3702395434,-2.91797567427));
#93618=CARTESIAN_POINT('Ctrl Pts',(-10.9022658531,-22.6742356128,-3.00720831272));
#93619=CARTESIAN_POINT('Ctrl Pts',(-10.9055923018,-22.5849236589,-3.00178035997));
#93620=CARTESIAN_POINT('Ctrl Pts',(-10.8807899278,-22.495611705,-2.97883906106));
#93621=CARTESIAN_POINT('Ctrl Pts',(-10.8268747327,-22.422876423,-2.93934282537));
#93622=CARTESIAN_POINT('Ctrl Pts',(-10.7549391582,-22.3819887897,-2.89162579979));
#93623=CARTESIAN_POINT('Ctrl Pts',(-10.6791013717,-22.3742356128,-2.84444941082));
#93624=CARTESIAN_POINT('Ctrl Pts',(-10.9558455155,-22.6742356128,-2.9197793747));
#93625=CARTESIAN_POINT('Ctrl Pts',(-10.9558455155,-22.5799878332,-2.9197793747));
#93626=CARTESIAN_POINT('Ctrl Pts',(-10.9242889413,-22.4857400536,-2.90044034768));
#93627=CARTESIAN_POINT('Ctrl Pts',(-10.8607738721,-22.4112466293,-2.86151598188));
#93628=CARTESIAN_POINT('Ctrl Pts',(-10.7804157158,-22.3742356128,-2.81226955396));
#93629=CARTESIAN_POINT('Ctrl Pts',(-10.7000575594,-22.3742356128,-2.76302312605));
#93630=CARTESIAN_POINT('',(-10.5566756928877,-22.0742356130312,-3.15068306070111));
#93631=CARTESIAN_POINT('Origin',(-10.3289416669918,-22.0742354221932,-3.34331619631364));
#93632=CARTESIAN_POINT('Origin',(-10.7018663106063,-22.6721142716748,-2.76413150657896));
#93633=CARTESIAN_POINT('Ctrl Pts',(-10.5566756907,-22.0742356132,-3.15068306769));
#93634=CARTESIAN_POINT('Ctrl Pts',(-10.5566756859512,-22.0898005735048,
-3.15068307249646));
#93635=CARTESIAN_POINT('Ctrl Pts',(-10.5573215621371,-22.1049828544198,
-3.14956730460941));
#93636=CARTESIAN_POINT('Ctrl Pts',(-10.5584978473689,-22.1196224072354,
-3.14747917537089));
#93637=CARTESIAN_POINT('Ctrl Pts',(-10.5597026713832,-22.1346171417708,
-3.14534038438448));
#93638=CARTESIAN_POINT('Ctrl Pts',(-10.5614636623284,-22.1490426809088,
-3.14218291907421));
#93639=CARTESIAN_POINT('Ctrl Pts',(-10.5636517974364,-22.1627817175157,
-3.13816526443253));
#93640=CARTESIAN_POINT('Ctrl Pts',(-10.5658925822785,-22.1768513354569,
-3.13405093913847));
#93641=CARTESIAN_POINT('Ctrl Pts',(-10.5685810564944,-22.1902013580508,
-3.12903543901091));
#93642=CARTESIAN_POINT('Ctrl Pts',(-10.5715778051455,-22.2027583291733,
-3.12327540451024));
#93643=CARTESIAN_POINT('Ctrl Pts',(-10.5722285509149,-22.2054850829943,
-3.12202460955891));
#93644=CARTESIAN_POINT('Ctrl Pts',(-10.5728938380069,-22.2081746216534,
-3.12073863082624));
#93645=CARTESIAN_POINT('Ctrl Pts',(-10.5735722505496,-22.2108264835374,
-3.11941893786222));
#93646=CARTESIAN_POINT('Ctrl Pts',(-10.5767098864281,-22.2230912582412,
-3.11331540095486));
#93647=CARTESIAN_POINT('Ctrl Pts',(-10.5801400974471,-22.2345491177178,
-3.10650592289017));
#93648=CARTESIAN_POINT('Ctrl Pts',(-10.5837599834052,-22.2451819019482,
-3.09916288252606));
#93649=CARTESIAN_POINT('Ctrl Pts',(-10.5858115691318,-22.2512080775278,
-3.09500118324169));
#93650=CARTESIAN_POINT('Ctrl Pts',(-10.5879242114495,-22.2569701262268,
-3.09066763613829));
#93651=CARTESIAN_POINT('Ctrl Pts',(-10.5900806129031,-22.2624708648471,
-3.0861898087817));
#93652=CARTESIAN_POINT('Ctrl Pts',(-10.5925134060449,-22.2686766477117,
-3.08113804642784));
#93653=CARTESIAN_POINT('Ctrl Pts',(-10.5950025653009,-22.2745494339731,
-3.0759040953588));
#93654=CARTESIAN_POINT('Ctrl Pts',(-10.5975255802534,-22.2800979399819,
-3.07052547791864));
#93655=CARTESIAN_POINT('Ctrl Pts',(-10.5980937173012,-22.2813473625509,
-3.06931431116335));
#93656=CARTESIAN_POINT('Ctrl Pts',(-10.598663581943,-22.2825803644228,-3.06809579402851));
#93657=CARTESIAN_POINT('Ctrl Pts',(-10.5992350299983,-22.2837970686739,
-3.06687046288606));
#93658=CARTESIAN_POINT('Ctrl Pts',(-10.6007896133565,-22.2871070251309,
-3.06353703759118));
#93659=CARTESIAN_POINT('Ctrl Pts',(-10.6023553288436,-22.2902961983313,
-3.06015269099193));
#93660=CARTESIAN_POINT('Ctrl Pts',(-10.6039279613649,-22.2933677297212,
-3.05672524457382));
#93661=CARTESIAN_POINT('Ctrl Pts',(-10.6047142776256,-22.2949034954161,
-3.05501152136476));
#93662=CARTESIAN_POINT('Ctrl Pts',(-10.6055023240052,-22.2964098493286,
-3.05328702260517));
#93663=CARTESIAN_POINT('Ctrl Pts',(-10.6062915890173,-22.2978872035116,
-3.05155269432272));
#93664=CARTESIAN_POINT('Ctrl Pts',(-10.6067749132123,-22.2987918945979,
-3.05049063936261));
#93665=CARTESIAN_POINT('Ctrl Pts',(-10.6071177353671,-22.2994259157237,
-3.04973510754653));
#93666=CARTESIAN_POINT('Ctrl Pts',(-10.6075784274124,-22.300268624085,-3.04871832870286));
#93667=CARTESIAN_POINT('Ctrl Pts',(-10.6078700422379,-22.3008020525526,
-3.04807471484389));
#93668=CARTESIAN_POINT('Ctrl Pts',(-10.6082089738345,-22.3014187874837,
-3.04732610967217));
#93669=CARTESIAN_POINT('Ctrl Pts',(-10.6086625394533,-22.3022326923837,
-3.04632115024142));
#93670=CARTESIAN_POINT('Ctrl Pts',(-10.6133661861168,-22.3106731934043,
-3.03589934162453));
#93671=CARTESIAN_POINT('Ctrl Pts',(-10.618088525891,-22.318158006891,-3.02504352114557));
#93672=CARTESIAN_POINT('Ctrl Pts',(-10.6227349108549,-22.3247632918189,
-3.01388705341523));
#93673=CARTESIAN_POINT('Ctrl Pts',(-10.6275370085389,-22.3315899374155,
-3.00235670277379));
#93674=CARTESIAN_POINT('Ctrl Pts',(-10.6322563565154,-22.3374778766665,
-2.99050341653969));
#93675=CARTESIAN_POINT('Ctrl Pts',(-10.6368193302651,-22.3425438840508,
-2.9784373250117));
#93676=CARTESIAN_POINT('Ctrl Pts',(-10.6415727814018,-22.3478213675254,
-2.96586754494355));
#93677=CARTESIAN_POINT('Ctrl Pts',(-10.646155819192,-22.3522078165756,-2.95306559830315));
#93678=CARTESIAN_POINT('Ctrl Pts',(-10.6505367312537,-22.3558567328289,
-2.94014022159176));
#93679=CARTESIAN_POINT('Ctrl Pts',(-10.6540771116143,-22.3588055597533,
-2.92969473690327));
#93680=CARTESIAN_POINT('Ctrl Pts',(-10.6574866958116,-22.361273330863,-2.91916829324453));
#93681=CARTESIAN_POINT('Ctrl Pts',(-10.6607733565153,-22.3633442036669,
-2.9086173822976));
#93682=CARTESIAN_POINT('Ctrl Pts',(-10.6651828350991,-22.3661225462162,
-2.89446197653664));
#93683=CARTESIAN_POINT('Ctrl Pts',(-10.6693355569454,-22.3681818404446,
-2.88025185841365));
#93684=CARTESIAN_POINT('Ctrl Pts',(-10.6732963279558,-22.3697259156136,
-2.86602304448339));
#93685=CARTESIAN_POINT('Ctrl Pts',(-10.6774323877848,-22.3713383257386,
-2.8511645167987));
#93686=CARTESIAN_POINT('Ctrl Pts',(-10.6813598786535,-22.3723889750259,
-2.83628552145626));
#93687=CARTESIAN_POINT('Ctrl Pts',(-10.6851919722119,-22.3730728664481,
-2.82140498507979));
#93688=CARTESIAN_POINT('Ctrl Pts',(-10.6892557863458,-22.3737981116921,
-2.80562464644122));
#93689=CARTESIAN_POINT('Ctrl Pts',(-10.6932123001532,-22.374110482048,-2.78984241926712));
#93690=CARTESIAN_POINT('Ctrl Pts',(-10.697233260058,-22.3742040322445,-2.77405800409609));
#93691=CARTESIAN_POINT('Ctrl Pts',(-10.6981702131669,-22.3742258310561,
-2.77037996272886));
#93692=CARTESIAN_POINT('Ctrl Pts',(-10.6991108225775,-22.3742356128,-2.76670171793979));
#93693=CARTESIAN_POINT('Ctrl Pts',(-10.7000575594,-22.3742356128,-2.76302312605));
#93694=CARTESIAN_POINT('Origin',(2.84607155346,-22.6742356128,5.53854202767));
#93695=CARTESIAN_POINT('Origin',(-10.9467697490204,-22.6721143269662,-2.35059830462873));
#93696=CARTESIAN_POINT('Ctrl Pts',(-11.2053401891,-22.6742356128,-2.49849372966));
#93697=CARTESIAN_POINT('Ctrl Pts',(-11.2053401891,-22.5799878332,-2.49849372966));
#93698=CARTESIAN_POINT('Ctrl Pts',(-11.1732131726,-22.4857400536,-2.48011792621));
#93699=CARTESIAN_POINT('Ctrl Pts',(-11.1085499535,-22.4112466293,-2.44313227564));
#93700=CARTESIAN_POINT('Ctrl Pts',(-11.0267391777,-22.3742356128,-2.39633867638));
#93701=CARTESIAN_POINT('Ctrl Pts',(-10.9449284019,-22.3742356128,-2.34954507713));
#93702=CARTESIAN_POINT('Ctrl Pts',(-11.2476948874,-22.6742356128,-2.42444362923));
#93703=CARTESIAN_POINT('Ctrl Pts',(-11.2450653313,-22.5840941242,-2.429040968));
#93704=CARTESIAN_POINT('Ctrl Pts',(-11.2130113811,-22.4939526355,-2.41703302845));
#93705=CARTESIAN_POINT('Ctrl Pts',(-11.1517699452,-22.4209218727,-2.38727936284));
#93706=CARTESIAN_POINT('Ctrl Pts',(-11.0744430753,-22.3806857596,-2.34601859644));
#93707=CARTESIAN_POINT('Ctrl Pts',(-10.9959501219,-22.3742356128,-2.30169489009));
#93708=CARTESIAN_POINT('Ctrl Pts',(-11.2941946283,-22.6686213022,-2.34203463014));
#93709=CARTESIAN_POINT('Ctrl Pts',(-11.2868586676,-22.5829413188,-2.35499473105));
#93710=CARTESIAN_POINT('Ctrl Pts',(-11.2526857413,-22.4972613355,-2.35302785728));
#93711=CARTESIAN_POINT('Ctrl Pts',(-11.1928402247,-22.426280398,-2.33351209766));
#93712=CARTESIAN_POINT('Ctrl Pts',(-11.1189291588,-22.3836825181,-2.2998966476));
#93713=CARTESIAN_POINT('Ctrl Pts',(-11.043868081,-22.3714284849,-2.25918468729));
#93714=CARTESIAN_POINT('Ctrl Pts',(-11.3417981924,-22.6467118109,-2.25595171063));
#93715=CARTESIAN_POINT('Ctrl Pts',(-11.3291442479,-22.5660000486,-2.27877967267));
#93716=CARTESIAN_POINT('Ctrl Pts',(-11.2910933501,-22.4852882864,-2.28766776945));
#93717=CARTESIAN_POINT('Ctrl Pts',(-11.229550879,-22.4176465288,-2.27867532762));
#93718=CARTESIAN_POINT('Ctrl Pts',(-11.1557537306,-22.375311083,-2.25331234023));
#93719=CARTESIAN_POINT('Ctrl Pts',(-11.0817600114,-22.3604736068,-2.21745676256));
#93720=CARTESIAN_POINT('Ctrl Pts',(-11.4353537652,-22.5603047021,-2.08352845036));
#93721=CARTESIAN_POINT('Ctrl Pts',(-11.4121163918,-22.4942390833,-2.12677174602));
#93722=CARTESIAN_POINT('Ctrl Pts',(-11.3657157526,-22.4281734646,-2.15766880717));
#93723=CARTESIAN_POINT('Ctrl Pts',(-11.2994862528,-22.3717132431,-2.16962607727));
#93724=CARTESIAN_POINT('Ctrl Pts',(-11.2242843437,-22.3339703351,-2.16051799049));
#93725=CARTESIAN_POINT('Ctrl Pts',(-11.1508960681,-22.3172702763,-2.13427099913));
#93726=CARTESIAN_POINT('Ctrl Pts',(-11.5032693058,-22.4004263802,-1.95414386857));
#93727=CARTESIAN_POINT('Ctrl Pts',(-11.4721201637,-22.3564749274,-2.01366537708));
#93728=CARTESIAN_POINT('Ctrl Pts',(-11.418463566,-22.3125234745,-2.06143417372));
#93729=CARTESIAN_POINT('Ctrl Pts',(-11.3465841747,-22.2747985542,-2.0888955933));
#93730=CARTESIAN_POINT('Ctrl Pts',(-11.2678343078,-22.2492105131,-2.09172776553));
#93731=CARTESIAN_POINT('Ctrl Pts',(-11.1928782665,-22.237330862,-2.07277075552));
#93732=CARTESIAN_POINT('Ctrl Pts',(-11.5284593408,-22.2976444921,-1.90521795022));
#93733=CARTESIAN_POINT('Ctrl Pts',(-11.4944206426,-22.2676340437,-1.97094002685));
#93734=CARTESIAN_POINT('Ctrl Pts',(-11.4380739731,-22.2376235953,-2.02511044406));
#93735=CARTESIAN_POINT('Ctrl Pts',(-11.3640715597,-22.2118199507,-2.05839415541));
#93736=CARTESIAN_POINT('Ctrl Pts',(-11.283947635,-22.1942244807,-2.0655995494));
#93737=CARTESIAN_POINT('Ctrl Pts',(-11.208324537,-22.1859402315,-2.04918926595));
#93738=CARTESIAN_POINT('Ctrl Pts',(-11.5410916547,-22.1859264501,-1.88073379583));
#93739=CARTESIAN_POINT('Ctrl Pts',(-11.5055896574,-22.1709238273,-1.9495777849));
#93740=CARTESIAN_POINT('Ctrl Pts',(-11.4478685938,-22.1559212045,-2.00696368603));
#93741=CARTESIAN_POINT('Ctrl Pts',(-11.3727622471,-22.1430213573,-2.04316893107));
#93742=CARTESIAN_POINT('Ctrl Pts',(-11.2919149591,-22.1342242685,-2.05258032919));
#93743=CARTESIAN_POINT('Ctrl Pts',(-11.2159437174,-22.1300808784,-2.0374723572));
#93744=CARTESIAN_POINT('Ctrl Pts',(-11.5410916367,-22.0742358827,-1.88073379256));
#93745=CARTESIAN_POINT('Ctrl Pts',(-11.5055896399,-22.0742358104,-1.94957779219));
#93746=CARTESIAN_POINT('Ctrl Pts',(-11.4478685736,-22.0742357381,-2.00696370221));
#93747=CARTESIAN_POINT('Ctrl Pts',(-11.3727622216,-22.074235676,-2.04316895153));
#93748=CARTESIAN_POINT('Ctrl Pts',(-11.2919149284,-22.0742356336,-2.05258034776));
#93749=CARTESIAN_POINT('Ctrl Pts',(-11.2159436836,-22.0742356136,-2.03747236903));
#93750=CARTESIAN_POINT('',(-11.2159436600663,-22.0742356133472,-2.03747240750538));
#93751=CARTESIAN_POINT('Origin',(-11.2753946067519,-22.074235881436,-1.74517806931961));
#93752=CARTESIAN_POINT('Ctrl Pts',(-10.9449284019,-22.3742356128,-2.34954507713));
#93753=CARTESIAN_POINT('Ctrl Pts',(-10.9565768825276,-22.3742356128,-2.33862067127606));
#93754=CARTESIAN_POINT('Ctrl Pts',(-10.968280766592,-22.3740622680576,-2.32779191576226));
#93755=CARTESIAN_POINT('Ctrl Pts',(-10.979949755164,-22.37354310181,-2.31690595964475));
#93756=CARTESIAN_POINT('Ctrl Pts',(-10.9911689868806,-22.373043945744,-2.30643958002794));
#93757=CARTESIAN_POINT('Ctrl Pts',(-11.0023563344253,-22.372225707338,-2.29592034716022));
#93758=CARTESIAN_POINT('Ctrl Pts',(-11.0134389745054,-22.3709040042025,
-2.28524712449359));
#93759=CARTESIAN_POINT('Ctrl Pts',(-11.0238481066063,-22.3696626228676,
-2.27522252892091));
#93760=CARTESIAN_POINT('Ctrl Pts',(-11.0341647801129,-22.3679770644684,
-2.26506174680759));
#93761=CARTESIAN_POINT('Ctrl Pts',(-11.0443340519157,-22.3656632096047,
-2.25471467683243));
#93762=CARTESIAN_POINT('Ctrl Pts',(-11.0474655616257,-22.3649506847441,
-2.25152841623034));
#93763=CARTESIAN_POINT('Ctrl Pts',(-11.0505831413501,-22.3641783511552,
-2.24832476821515));
#93764=CARTESIAN_POINT('Ctrl Pts',(-11.0536853244324,-22.3633402225444,
-2.24510308453649));
#93765=CARTESIAN_POINT('Ctrl Pts',(-11.0633642697261,-22.3607252250548,
-2.23505129221736));
#93766=CARTESIAN_POINT('Ctrl Pts',(-11.0728793857902,-22.3574725336843,
-2.22483316903463));
#93767=CARTESIAN_POINT('Ctrl Pts',(-11.0821562752923,-22.3534133609767,
-2.2145039537747));
#93768=CARTESIAN_POINT('Ctrl Pts',(-11.0896802081132,-22.3501212076366,
-2.20612654217665));
#93769=CARTESIAN_POINT('Ctrl Pts',(-11.0970483562335,-22.3462982180438,
-2.19767660347488));
#93770=CARTESIAN_POINT('Ctrl Pts',(-11.1042297129877,-22.3418596791366,
-2.18920695368937));
#93771=CARTESIAN_POINT('Ctrl Pts',(-11.1122476406949,-22.3369040857435,
-2.17975065705759));
#93772=CARTESIAN_POINT('Ctrl Pts',(-11.1200316088684,-22.331181788504,-2.17027399083279));
#93773=CARTESIAN_POINT('Ctrl Pts',(-11.1276410948107,-22.3246179799789,
-2.16092525729618));
#93774=CARTESIAN_POINT('Ctrl Pts',(-11.1314458377819,-22.3213360757163,
-2.15625089052788));
#93775=CARTESIAN_POINT('Ctrl Pts',(-11.1351832582712,-22.317839173301,-2.15159900315221));
#93776=CARTESIAN_POINT('Ctrl Pts',(-11.1388218124651,-22.3141117280667,
-2.14697715269855));
#93777=CARTESIAN_POINT('Ctrl Pts',(-11.139525886561,-22.3133904532158,-2.14608280703086));
#93778=CARTESIAN_POINT('Ctrl Pts',(-11.1402262722922,-22.312660544195,-2.145189591596));
#93779=CARTESIAN_POINT('Ctrl Pts',(-11.1409228190846,-22.3119219228704,
-2.144297623045));
#93780=CARTESIAN_POINT('Ctrl Pts',(-11.1420260993752,-22.3107519995309,
-2.14288480866867));
#93781=CARTESIAN_POINT('Ctrl Pts',(-11.1431197477329,-22.3095602176583,
-2.1414751213253));
#93782=CARTESIAN_POINT('Ctrl Pts',(-11.1442033086172,-22.308346245778,-2.14006904278067));
#93783=CARTESIAN_POINT('Ctrl Pts',(-11.1452339612863,-22.3071915498336,
-2.13873162037472));
#93784=CARTESIAN_POINT('Ctrl Pts',(-11.1464488402109,-22.3057917228803,
-2.13714291255623));
#93785=CARTESIAN_POINT('Ctrl Pts',(-11.1475069745288,-22.3045370649081,
-2.13575056520196));
#93786=CARTESIAN_POINT('Ctrl Pts',(-11.1482636315973,-22.3036398765197,
-2.13475491706011));
#93787=CARTESIAN_POINT('Ctrl Pts',(-11.1489410725372,-22.3028181867498,
-2.13385890924935));
#93788=CARTESIAN_POINT('Ctrl Pts',(-11.1494233819929,-22.3022264767122,
-2.13321857299617));
#93789=CARTESIAN_POINT('Ctrl Pts',(-11.1557486448315,-22.29446647643,-2.12482086264944));
#93790=CARTESIAN_POINT('Ctrl Pts',(-11.1618495924945,-22.2858526143557,
-2.1165696985762));
#93791=CARTESIAN_POINT('Ctrl Pts',(-11.1676296764402,-22.2763188870647,
-2.10861659005254));
#93792=CARTESIAN_POINT('Ctrl Pts',(-11.1731962959871,-22.2671372500517,
-2.10095719794287));
#93793=CARTESIAN_POINT('Ctrl Pts',(-11.1784653901721,-22.2571017817321,
-2.09357457146205));
#93794=CARTESIAN_POINT('Ctrl Pts',(-11.1833374488865,-22.2461885091507,
-2.08663413877296));
#93795=CARTESIAN_POINT('Ctrl Pts',(-11.1882095076009,-22.2352752365692,
-2.07969370608386));
#93796=CARTESIAN_POINT('Ctrl Pts',(-11.1926845419211,-22.2234833193454,
-2.07319587467472));
#93797=CARTESIAN_POINT('Ctrl Pts',(-11.1966487080552,-22.2108358475213,
-2.06733170400025));
#93798=CARTESIAN_POINT('Ctrl Pts',(-11.2004710745941,-22.1986407801437,
-2.06167729674131));
#93799=CARTESIAN_POINT('Ctrl Pts',(-11.2038037915588,-22.1856447995889,
-2.05660690044393));
#93800=CARTESIAN_POINT('Ctrl Pts',(-11.2065790246433,-22.1719101123269,
-2.05231577287415));
#93801=CARTESIAN_POINT('Ctrl Pts',(-11.2092944749749,-22.1584712911741,
-2.04811708273626));
#93802=CARTESIAN_POINT('Ctrl Pts',(-11.2114758661764,-22.1443248656484,
-2.04466512644328));
#93803=CARTESIAN_POINT('Ctrl Pts',(-11.2130487391782,-22.1295766664627,
-2.04215055378544));
#93804=CARTESIAN_POINT('Ctrl Pts',(-11.2145585009443,-22.1154202360173,
-2.03973687788627));
#93805=CARTESIAN_POINT('Ctrl Pts',(-11.2155070568181,-22.1007092604967,
-2.0381878039234));
#93806=CARTESIAN_POINT('Ctrl Pts',(-11.2158247434131,-22.0855848206322,
-2.03766750097925));
#93807=CARTESIAN_POINT('Ctrl Pts',(-11.2159036934711,-22.0818261621817,
-2.03753819760833));
#93808=CARTESIAN_POINT('Ctrl Pts',(-11.2159436859039,-22.0780422089381,
-2.03747236822363));
#93809=CARTESIAN_POINT('Ctrl Pts',(-11.2159436836,-22.0742356136,-2.03747236903));
#93810=CARTESIAN_POINT('Origin',(-11.2744572343,-19.6742356128,-1.7432341771));
#93811=CARTESIAN_POINT('Origin',(-11.2744572343,-19.6742356128,-1.7432341771));
#93812=CARTESIAN_POINT('Origin',(-11.2744572343,-21.2742356128,-1.7432341771));
#93813=CARTESIAN_POINT('',(-11.2159436339,-20.8742356128,-2.03747244546));
#93814=CARTESIAN_POINT('Origin',(-10.3267865236,-21.2742356128,-3.3434289261));
#93815=CARTESIAN_POINT('Origin',(-10.3267865236,-19.6742356128,-3.3434289261));
#93816=CARTESIAN_POINT('',(-10.5566756949,-20.8742356128,-3.15068305993));
#93817=CARTESIAN_POINT('Origin',(-6.6707290414,-19.6742356128,10.1304528845));
#93818=CARTESIAN_POINT('Origin',(-2.45,-19.6742356128,10.1304528845));
#93819=CARTESIAN_POINT('',(-2.88657986403E-14,-19.6742356128,10.4304528845));
#93820=CARTESIAN_POINT('Origin',(-2.75,-19.3742356128,10.4304528845));
#93821=CARTESIAN_POINT('',(-1.375,-20.6742356128,10.4304528845));
#93822=CARTESIAN_POINT('Origin',(-1.375,-20.6742356128,10.7304528845));
#93823=CARTESIAN_POINT('',(-2.45,-20.9304376384,10.5743743079));
#93824=CARTESIAN_POINT('Origin',(-2.45,-20.6742356128,10.7304528845));
#93825=CARTESIAN_POINT('',(-1.82443078508723,-20.9742355917829,10.7304528845));
#93826=CARTESIAN_POINT('Ctrl Pts',(-2.45000000001651,-20.9304376384374,
10.5743743079454));
#93827=CARTESIAN_POINT('Ctrl Pts',(-2.44729189173785,-20.9308368579965,
10.5750296244019));
#93828=CARTESIAN_POINT('Ctrl Pts',(-2.44457723791173,-20.9312343514944,
10.5756877663935));
#93829=CARTESIAN_POINT('Ctrl Pts',(-2.33821087635373,-20.9467017934165,
10.6015224622014));
#93830=CARTESIAN_POINT('Ctrl Pts',(-2.23664227464802,-20.957470549854,10.6278009815082));
#93831=CARTESIAN_POINT('Ctrl Pts',(-2.0775138014278,-20.9680551199903,10.6682233822152));
#93832=CARTESIAN_POINT('Ctrl Pts',(-2.02332178583692,-20.9705889581146,
10.6818849323202));
#93833=CARTESIAN_POINT('Ctrl Pts',(-1.93823023557501,-20.9730684400875,
10.7029370878533));
#93834=CARTESIAN_POINT('Ctrl Pts',(-1.90756560839508,-20.973660008163,10.710444942518));
#93835=CARTESIAN_POINT('Ctrl Pts',(-1.85938817655537,-20.9741488490342,
10.722093182511));
#93836=CARTESIAN_POINT('Ctrl Pts',(-1.84191849476494,-20.9742356126494,
10.7262868288948));
#93837=CARTESIAN_POINT('Ctrl Pts',(-1.82443078250423,-20.9742356128,10.7304528736574));
#93838=CARTESIAN_POINT('',(-4.4408920985E-16,-20.9742356128,10.7304528845));
#93839=CARTESIAN_POINT('Origin',(-1.97861558624E-15,-21.2742356128,0.580061096523));
#93840=CARTESIAN_POINT('',(-2.45,-20.9742356128,15.7712943679));
#93841=CARTESIAN_POINT('Origin',(2.78569866985E-16,-20.9742356128,0.580061096523));
#93842=CARTESIAN_POINT('Origin',(-2.45000000000807,-21.2742356128,15.7712943679849));
#93843=CARTESIAN_POINT('Origin',(2.69422295812E-16,-20.9742356128,0.729452270839));
#93844=CARTESIAN_POINT('',(-1.01362101456,-20.9742356128,10.8791871183));
#93845=CARTESIAN_POINT('Origin',(-0.00234352656470205,-20.9742355812827,
3.0819174256968));
#93846=CARTESIAN_POINT('',(-0.767157287525,-20.9742356128,11.1596805575));
#93847=CARTESIAN_POINT('Origin',(-1.05,-20.9742356128,11.1596805575));
#93848=CARTESIAN_POINT('',(-0.767157287525,-20.9742356128,14.92922515));
#93849=CARTESIAN_POINT('',(-0.767157287525,-20.9742356128,12.1167294155));
#93850=CARTESIAN_POINT('',(-1.07064182355,-20.9742356128,15.2113136381));
#93851=CARTESIAN_POINT('Origin',(-1.05,-20.9742356128,14.92922515));
#93852=CARTESIAN_POINT('',(-2.45000000041083,-20.9742356123072,15.0444077749624));
#93853=CARTESIAN_POINT('Origin',(5.40116187885964E-9,-20.9742356120504,
0.58006109717732));
#93854=CARTESIAN_POINT('',(-2.45,-20.9742356128,13.3490218086));
#93855=CARTESIAN_POINT('Origin',(-3.05,-19.6742356128,15.662287998));
#93856=CARTESIAN_POINT('',(-2.75,-19.6742356128,15.662287998));
#93857=CARTESIAN_POINT('Origin',(-3.05,-19.6742356128,15.662287998));
#93858=CARTESIAN_POINT('Origin',(-3.05,-19.6742356128,15.662287998));
#93859=CARTESIAN_POINT('',(-2.97246042119851,-19.3848539651149,15.6779684221767));
#93860=CARTESIAN_POINT('Origin',(-3.05,-19.6742356128,15.662287998));
#93861=CARTESIAN_POINT('Origin',(-3.05,-19.6742356128,2.96634320571));
#93862=CARTESIAN_POINT('',(-2.75,-19.6742356128,13.1963704412));
#93863=CARTESIAN_POINT('Origin',(-3.05,-19.6742356128,10.7304528845));
#93864=CARTESIAN_POINT('Origin',(-3.05,-22.4223864096,15.662287998));
#93865=CARTESIAN_POINT('',(-2.750000005455,-20.6742356128438,15.6622879962));
#93866=CARTESIAN_POINT('Ctrl Pts',(-2.75,-20.6742356128,15.6622879962));
#93867=CARTESIAN_POINT('Ctrl Pts',(-2.75000002192,-20.6742356209121,15.7685078015738));
#93868=CARTESIAN_POINT('Ctrl Pts',(-2.79701105507061,-20.6742356114132,
15.8747276069476));
#93869=CARTESIAN_POINT('Ctrl Pts',(-2.89192095826334,-20.6742355819167,
15.9523655950137));
#93870=CARTESIAN_POINT('Ctrl Pts',(-3.00535144290051,-20.6742355416214,
15.9773898040232));
#93871=CARTESIAN_POINT('Ctrl Pts',(-3.10946375772823,-20.6742355012,15.9563357177875));
#93872=CARTESIAN_POINT('',(-2.75,-20.1742356128,15.662287998));
#93873=CARTESIAN_POINT('Origin',(-2.75,-19.3742356128,10.4304528845));
#93874=CARTESIAN_POINT('',(-2.75,-20.6742356128,13.3490218086));
#93875=CARTESIAN_POINT('Ctrl Pts',(-3.1094637805,-20.6742355012,15.9563357204));
#93876=CARTESIAN_POINT('Ctrl Pts',(-3.00535146138,-20.6742355416,15.9773898081));
#93877=CARTESIAN_POINT('Ctrl Pts',(-2.89192096986,-20.6742355819,15.9523656045));
#93878=CARTESIAN_POINT('Ctrl Pts',(-2.7970110589,-20.6742356114,15.8747276156));
#93879=CARTESIAN_POINT('Ctrl Pts',(-2.75000002192,-20.6742356209,15.7685078059));
#93880=CARTESIAN_POINT('Ctrl Pts',(-2.75000002182,-20.6742356129,15.6622879962));
#93881=CARTESIAN_POINT('Ctrl Pts',(-3.10946380353,-20.7613039297,15.9563357159));
#93882=CARTESIAN_POINT('Ctrl Pts',(-3.00535147528,-20.7455779654,15.9773898056));
#93883=CARTESIAN_POINT('Ctrl Pts',(-2.89192097435,-20.7298520012,15.9523656029));
#93884=CARTESIAN_POINT('Ctrl Pts',(-2.79701105681,-20.7183575883,15.8747276131));
#93885=CARTESIAN_POINT('Ctrl Pts',(-2.75000001886,-20.7146527462,15.7685078017));
#93886=CARTESIAN_POINT('Ctrl Pts',(-2.75000002231,-20.7177698279,15.6622879905));
#93887=CARTESIAN_POINT('Ctrl Pts',(-3.09336559174,-20.8484128662,15.9595900965));
#93888=CARTESIAN_POINT('Ctrl Pts',(-2.99245619263,-20.8169453132,15.9798833716));
#93889=CARTESIAN_POINT('Ctrl Pts',(-2.88234381849,-20.7854777603,15.9544199132));
#93890=CARTESIAN_POINT('Ctrl Pts',(-2.78979771265,-20.7624813454,15.8769278231));
#93891=CARTESIAN_POINT('Ctrl Pts',(-2.74323291398,-20.755077053,15.7712039881));
#93892=CARTESIAN_POINT('Ctrl Pts',(-2.74210499444,-20.7613240613,15.6654801511));
#93893=CARTESIAN_POINT('Ctrl Pts',(-3.0611129676,-20.9309303248,15.9661188953));
#93894=CARTESIAN_POINT('Ctrl Pts',(-2.96663575098,-20.8849847431,15.9848817048));
#93895=CARTESIAN_POINT('Ctrl Pts',(-2.86318716199,-20.8390391614,15.9585340485));
#93896=CARTESIAN_POINT('Ctrl Pts',(-2.77538294467,-20.80528071,15.8813354034));
#93897=CARTESIAN_POINT('Ctrl Pts',(-2.72969914456,-20.7940068531,15.7766097304));
#93898=CARTESIAN_POINT('Ctrl Pts',(-2.72628672053,-20.8025832991,15.6718840609));
#93899=CARTESIAN_POINT('Ctrl Pts',(-2.95857415151,-21.0968055424,15.9864129862));
#93900=CARTESIAN_POINT('Ctrl Pts',(-2.883615269,-21.0232686806,16.0006863819));
#93901=CARTESIAN_POINT('Ctrl Pts',(-2.80037813885,-20.9497318188,15.9717891925));
#93902=CARTESIAN_POINT('Ctrl Pts',(-2.72731697454,-20.8948262684,15.8954574233));
#93903=CARTESIAN_POINT('Ctrl Pts',(-2.68525006547,-20.8745215131,15.7936237677));
#93904=CARTESIAN_POINT('Ctrl Pts',(-2.67599823713,-20.8855201685,15.6917901077));
#93905=CARTESIAN_POINT('Ctrl Pts',(-2.802073414,-21.210145586,16.0157241263));
#93906=CARTESIAN_POINT('Ctrl Pts',(-2.75443180074,-21.1206683319,16.0242286253));
#93907=CARTESIAN_POINT('Ctrl Pts',(-2.69943877243,-21.0311910779,15.9921593039));
#93908=CARTESIAN_POINT('Ctrl Pts',(-2.64793358485,-20.9628100879,15.9169517332));
#93909=CARTESIAN_POINT('Ctrl Pts',(-2.61350648776,-20.9339674316,15.8187461919));
#93910=CARTESIAN_POINT('Ctrl Pts',(-2.59924369788,-20.942191106,15.7205406559));
#93911=CARTESIAN_POINT('Ctrl Pts',(-2.70443397686,-21.2527626391,16.0332525536));
#93912=CARTESIAN_POINT('Ctrl Pts',(-2.67281955818,-21.1584143796,16.038616685));
#93913=CARTESIAN_POINT('Ctrl Pts',(-2.63437509944,-21.0640661201,16.0048673446));
#93914=CARTESIAN_POINT('Ctrl Pts',(-2.59591773658,-20.9910117695,15.9302754357));
#93915=CARTESIAN_POINT('Ctrl Pts',(-2.56711899741,-20.9580670061,15.8340046748));
#93916=CARTESIAN_POINT('Ctrl Pts',(-2.55135784288,-20.9634991119,15.7377339138));
#93917=CARTESIAN_POINT('Ctrl Pts',(-2.60121936463,-21.2742356128,16.0507826341));
#93918=CARTESIAN_POINT('Ctrl Pts',(-2.58568379068,-21.1783721495,16.0532881684));
#93919=CARTESIAN_POINT('Ctrl Pts',(-2.56380921231,-21.0825086862,16.0180414277));
#93920=CARTESIAN_POINT('Ctrl Pts',(-2.53876678585,-21.0074397583,15.9440093758));
#93921=CARTESIAN_POINT('Ctrl Pts',(-2.51662240651,-20.9716977028,15.8494690665));
#93922=CARTESIAN_POINT('Ctrl Pts',(-2.50073751227,-20.9742356128,15.7549287572));
#93923=CARTESIAN_POINT('Ctrl Pts',(-2.49776595187,-21.2742356128,16.0674673138));
#93924=CARTESIAN_POINT('Ctrl Pts',(-2.49776595187,-21.1799878332,16.0674673138));
#93925=CARTESIAN_POINT('Ctrl Pts',(-2.49187306376,-21.0857400536,16.0309284411));
#93926=CARTESIAN_POINT('Ctrl Pts',(-2.4800122327,-21.0112466293,15.9573853181));
#93927=CARTESIAN_POINT('Ctrl Pts',(-2.46500611635,-20.9742356128,15.864339843));
#93928=CARTESIAN_POINT('Ctrl Pts',(-2.45,-20.9742356128,15.7712943679));
#93929=CARTESIAN_POINT('Ctrl Pts',(-2.75000002182,-20.6742356129,15.6622879962));
#93930=CARTESIAN_POINT('Ctrl Pts',(-2.75000002198767,-20.6891327288188,
15.662287996202));
#93931=CARTESIAN_POINT('Ctrl Pts',(-2.7488884673052,-20.7043898896441,15.6627908269653));
#93932=CARTESIAN_POINT('Ctrl Pts',(-2.74651746486329,-20.7198130389006,
15.6638118403573));
#93933=CARTESIAN_POINT('Ctrl Pts',(-2.74423092920776,-20.7346867396071,
15.6647964802227));
#93934=CARTESIAN_POINT('Ctrl Pts',(-2.74077278856836,-20.7497146973984,
15.6662631994214));
#93935=CARTESIAN_POINT('Ctrl Pts',(-2.73603745825241,-20.7646874654371,
15.6682067376741));
#93936=CARTESIAN_POINT('Ctrl Pts',(-2.7338400705365,-20.7716354446415,15.6691086192318));
#93937=CARTESIAN_POINT('Ctrl Pts',(-2.73136807582815,-20.778571039602,15.6701128877873));
#93938=CARTESIAN_POINT('Ctrl Pts',(-2.72861328945327,-20.7854707230258,
15.6712174187728));
#93939=CARTESIAN_POINT('Ctrl Pts',(-2.72296675191468,-20.799613134144,15.6734813967454));
#93940=CARTESIAN_POINT('Ctrl Pts',(-2.71613031669946,-20.8136044725922,
15.6761744654426));
#93941=CARTESIAN_POINT('Ctrl Pts',(-2.70806242614445,-20.8272155055718,
15.6793002985697));
#93942=CARTESIAN_POINT('Ctrl Pts',(-2.70552338278455,-20.8314990295826,
15.6802840285536));
#93943=CARTESIAN_POINT('Ctrl Pts',(-2.70286266137133,-20.8357446890429,
15.6813104484459));
#93944=CARTESIAN_POINT('Ctrl Pts',(-2.70007978559827,-20.8399448481202,
15.6823791917623));
#93945=CARTESIAN_POINT('Ctrl Pts',(-2.69426700983312,-20.8487179967928,
15.6846115462601));
#93946=CARTESIAN_POINT('Ctrl Pts',(-2.68792075017705,-20.857292667102,15.687029930608));
#93947=CARTESIAN_POINT('Ctrl Pts',(-2.68104398035804,-20.8655956668358,
15.6896343447235));
#93948=CARTESIAN_POINT('Ctrl Pts',(-2.67941833810201,-20.8675584644246,
15.6902500183246));
#93949=CARTESIAN_POINT('Ctrl Pts',(-2.67776307577371,-20.8695060866975,
15.6908760803931));
#93950=CARTESIAN_POINT('Ctrl Pts',(-2.67607832738159,-20.8714375297582,
15.6915125453967));
#93951=CARTESIAN_POINT('Ctrl Pts',(-2.67419967587668,-20.8735912688148,
15.6922222632052));
#93952=CARTESIAN_POINT('Ctrl Pts',(-2.67228435995548,-20.8757248910275,
15.6929449165403));
#93953=CARTESIAN_POINT('Ctrl Pts',(-2.67033263730239,-20.8778369880354,
15.6936804881095));
#93954=CARTESIAN_POINT('Ctrl Pts',(-2.66859870637496,-20.879713397226,15.6943339776262));
#93955=CARTESIAN_POINT('Ctrl Pts',(-2.66660548636659,-20.8818162220527,
15.6950847913152));
#93956=CARTESIAN_POINT('Ctrl Pts',(-2.66467211375905,-20.8837967669163,
15.6958131945261));
#93957=CARTESIAN_POINT('Ctrl Pts',(-2.66247767151406,-20.8860447512417,
15.696639956409));
#93958=CARTESIAN_POINT('Ctrl Pts',(-2.66036059309485,-20.8881350146166,
15.6974377084262));
#93959=CARTESIAN_POINT('Ctrl Pts',(-2.65883635900915,-20.889613008879,15.6980158102704));
#93960=CARTESIAN_POINT('Ctrl Pts',(-2.65162649322279,-20.8966041530638,
15.7007503224732));
#93961=CARTESIAN_POINT('Ctrl Pts',(-2.643585031057,-20.9037016639627,15.7037798378816));
#93962=CARTESIAN_POINT('Ctrl Pts',(-2.63461960904651,-20.9107022452566,
15.7071214036503));
#93963=CARTESIAN_POINT('Ctrl Pts',(-2.62932398864371,-20.9148372899971,
15.7090951717385));
#93964=CARTESIAN_POINT('Ctrl Pts',(-2.62370631841184,-20.9189376969414,
15.7111775798599));
#93965=CARTESIAN_POINT('Ctrl Pts',(-2.61775168794802,-20.9229543962997,
15.7133695690179));
#93966=CARTESIAN_POINT('Ctrl Pts',(-2.61173828221312,-20.9270107425505,
15.7155831942383));
#93967=CARTESIAN_POINT('Ctrl Pts',(-2.60538119420661,-20.9309816775041,
15.7179085866684));
#93968=CARTESIAN_POINT('Ctrl Pts',(-2.59867000660302,-20.9348109629388,
15.7203441452));
#93969=CARTESIAN_POINT('Ctrl Pts',(-2.59692526996035,-20.9358064789351,
15.7209773279489));
#93970=CARTESIAN_POINT('Ctrl Pts',(-2.59515662848469,-20.9367923932735,
15.7216179421837));
#93971=CARTESIAN_POINT('Ctrl Pts',(-2.59336396019278,-20.937767659153,15.7222659288205));
#93972=CARTESIAN_POINT('Ctrl Pts',(-2.59239613536374,-20.938294185191,15.7226157635105));
#93973=CARTESIAN_POINT('Ctrl Pts',(-2.59142541592154,-20.938815485287,15.7229662682405));
#93974=CARTESIAN_POINT('Ctrl Pts',(-2.59042809853723,-20.9393437769894,
15.7233259661923));
#93975=CARTESIAN_POINT('Ctrl Pts',(-2.58679089344647,-20.9412704507842,
15.7246377805071));
#93976=CARTESIAN_POINT('Ctrl Pts',(-2.58285965075778,-20.9432522129818,
15.726049979423));
#93977=CARTESIAN_POINT('Ctrl Pts',(-2.57890122778666,-20.9451356436071,
15.7274652287701));
#93978=CARTESIAN_POINT('Ctrl Pts',(-2.57595883428822,-20.9465356440787,
15.7285172185418));
#93979=CARTESIAN_POINT('Ctrl Pts',(-2.57300196178022,-20.9478822490868,
15.7295707596454));
#93980=CARTESIAN_POINT('Ctrl Pts',(-2.57014764205019,-20.9491296563122,
15.730584465258));
#93981=CARTESIAN_POINT('Ctrl Pts',(-2.56747171730329,-20.9502991005859,
15.7315348142698));
#93982=CARTESIAN_POINT('Ctrl Pts',(-2.56488607804088,-20.9513816261541,
15.7324501148568));
#93983=CARTESIAN_POINT('Ctrl Pts',(-2.56249084795086,-20.9523502970827,
15.7332957897429));
#93984=CARTESIAN_POINT('Ctrl Pts',(-2.56198673178439,-20.9525541700539,
15.7334737761432));
#93985=CARTESIAN_POINT('Ctrl Pts',(-2.56148899337878,-20.9527538885307,
15.7336494084665));
#93986=CARTESIAN_POINT('Ctrl Pts',(-2.56098799203385,-20.9529533606897,
15.7338260904627));
#93987=CARTESIAN_POINT('Ctrl Pts',(-2.54305852071686,-20.960091925069,15.7401490570897));
#93988=CARTESIAN_POINT('Ctrl Pts',(-2.52444947588824,-20.9654910132208,
15.7465790967645));
#93989=CARTESIAN_POINT('Ctrl Pts',(-2.50548871504351,-20.9690589576089,
15.7529798707704));
#93990=CARTESIAN_POINT('Ctrl Pts',(-2.48721902877561,-20.9724968589213,
15.7591473518076));
#93991=CARTESIAN_POINT('Ctrl Pts',(-2.46862329501776,-20.9742356128,15.7652873410953));
#93992=CARTESIAN_POINT('Ctrl Pts',(-2.45,-20.9742356128,15.7712943679));
#93993=CARTESIAN_POINT('Origin',(-2.45,-20.6742356128,13.3490218086));
#93994=CARTESIAN_POINT('',(-2.7328425359048,-20.7742356128,14.7056612864094));
#93995=CARTESIAN_POINT('Ctrl Pts',(-2.45000000049961,-20.9742356128,15.0444077754865));
#93996=CARTESIAN_POINT('Ctrl Pts',(-2.4505642246363,-20.9742356127991,15.0443122060722));
#93997=CARTESIAN_POINT('Ctrl Pts',(-2.45112837604849,-20.9742340210488,
15.0442160442459));
#93998=CARTESIAN_POINT('Ctrl Pts',(-2.45271374680238,-20.9742250770619,
15.0439441126589));
#93999=CARTESIAN_POINT('Ctrl Pts',(-2.45373475694185,-20.9742141013729,
15.0437670015517));
#94000=CARTESIAN_POINT('Ctrl Pts',(-2.45684314513659,-20.9741648228718,
15.0432217654727));
#94001=CARTESIAN_POINT('Ctrl Pts',(-2.4589292490415,-20.9741099489642,15.0428475546937));
#94002=CARTESIAN_POINT('Ctrl Pts',(-2.47343386336903,-20.9735771126508,
15.0401878296793));
#94003=CARTESIAN_POINT('Ctrl Pts',(-2.48577021911375,-20.9723499449582,
15.0376330465997));
#94004=CARTESIAN_POINT('Ctrl Pts',(-2.4979272248846,-20.9703825039113,15.0347954601426));
#94005=CARTESIAN_POINT('Ctrl Pts',(-2.52673836491087,-20.9657198245833,
15.0280706051666));
#94006=CARTESIAN_POINT('Ctrl Pts',(-2.55429827846532,-20.9569165134737,
15.0198723368218));
#94007=CARTESIAN_POINT('Ctrl Pts',(-2.5945651553735,-20.9376298024471,15.0033035455715));
#94008=CARTESIAN_POINT('Ctrl Pts',(-2.60860989911875,-20.929371510587,14.9964054063729));
#94009=CARTESIAN_POINT('Ctrl Pts',(-2.64141722292707,-20.906490382548,14.9765328685671));
#94010=CARTESIAN_POINT('Ctrl Pts',(-2.65833205103465,-20.8911324882057,
14.962552890661));
#94011=CARTESIAN_POINT('Ctrl Pts',(-2.69268191586262,-20.8531499395656,
14.9219853022821));
#94012=CARTESIAN_POINT('Ctrl Pts',(-2.70622600372626,-20.8315298749212,
14.8938483721785));
#94013=CARTESIAN_POINT('Ctrl Pts',(-2.72505121860894,-20.795769394928,14.826784031487));
#94014=CARTESIAN_POINT('Ctrl Pts',(-2.72971376844571,-20.7828404745285,
14.7890007210827));
#94015=CARTESIAN_POINT('Ctrl Pts',(-2.73248325800256,-20.7752696738283,
14.7349347464044));
#94016=CARTESIAN_POINT('Ctrl Pts',(-2.73284271189799,-20.7742356144309,
14.7202906426028));
#94017=CARTESIAN_POINT('Ctrl Pts',(-2.73284271247462,-20.7742356128,14.7056612864095));
#94018=CARTESIAN_POINT('',(-2.73284184833111,-20.7742356128,10.7560440517756));
#94019=CARTESIAN_POINT('',(-2.73284210357,-20.7742356128,12.7308526862));
#94020=CARTESIAN_POINT('',(-2.73249401778459,-20.7752152053705,10.7304528485382));
#94021=CARTESIAN_POINT('Origin',(-2.61837242878611,-21.0942392376549,10.8006651608268));
#94022=CARTESIAN_POINT('Origin',(-2.45,-20.6742356128,10.7304528845));
#94023=CARTESIAN_POINT('Origin',(-6.51383560964,-21.0742356128,10.9320666897));
#94024=CARTESIAN_POINT('',(-4.98919124473,-20.7742356128,9.52235136777));
#94025=CARTESIAN_POINT('',(-8.14487887576,-20.7742356128,12.4401604693));
#94026=CARTESIAN_POINT('',(-6.56703506025,-20.7742356128,10.9812559186));
#94027=CARTESIAN_POINT('Origin',(-8.14487887576,-21.0742356128,12.4401604693));
#94028=CARTESIAN_POINT('Origin',(-4.98919124473,-21.0742356128,9.52235136777));
#94029=CARTESIAN_POINT('Origin',(-4.98919124473,-21.0742356128,9.52235136777));
#94030=CARTESIAN_POINT('Origin',(-4.98919124473,-21.0742356128,9.52235136777));
#94031=CARTESIAN_POINT('Origin',(-0.00234331738803,-21.0742356128,3.08191746407));
#94032=CARTESIAN_POINT('Ctrl Pts',(-2.73249449536286,-20.7752151161147,
10.7304528285094));
#94033=CARTESIAN_POINT('Ctrl Pts',(-2.73245710700268,-20.7753197109045,
10.7290952012981));
#94034=CARTESIAN_POINT('Ctrl Pts',(-2.73240712664869,-20.7754319433538,
10.727752397751));
#94035=CARTESIAN_POINT('Ctrl Pts',(-2.73152298709635,-20.7771409318656,
10.7087546905869));
#94036=CARTESIAN_POINT('Ctrl Pts',(-2.72772545244807,-20.7809744979902,
10.6881339522637));
#94037=CARTESIAN_POINT('Ctrl Pts',(-2.71679996433014,-20.790736326335,10.6559122059645));
#94038=CARTESIAN_POINT('Ctrl Pts',(-2.70771619875055,-20.7984214920223,
10.6384138803735));
#94039=CARTESIAN_POINT('Ctrl Pts',(-2.68765731828287,-20.8146185581327,
10.6112737349406));
#94040=CARTESIAN_POINT('Ctrl Pts',(-2.67249689114102,-20.8263682945712,
10.5972506978324));
#94041=CARTESIAN_POINT('Ctrl Pts',(-2.63942576926425,-20.8502432000307,
10.5761069546454));
#94042=CARTESIAN_POINT('Ctrl Pts',(-2.61427989630385,-20.8668329470141,
10.5673521750875));
#94043=CARTESIAN_POINT('Ctrl Pts',(-2.57563645957668,-20.8884881384831,
10.5611700175102));
#94044=CARTESIAN_POINT('Ctrl Pts',(-2.55565602930818,-20.8983536598198,
10.5602963146483));
#94045=CARTESIAN_POINT('Ctrl Pts',(-2.51151087548645,-20.9166072793448,
10.562148593287));
#94046=CARTESIAN_POINT('Ctrl Pts',(-2.48028974593003,-20.925972433295,10.5670447011082));
#94047=CARTESIAN_POINT('Ctrl Pts',(-2.45000000001651,-20.9304376384374,
10.5743743079454));
#94048=CARTESIAN_POINT('Origin',(-0.00234331738835,-20.7742356128,3.08191746407));
#94049=CARTESIAN_POINT('Origin',(-1.05,-21.0742356128,11.1596805575));
#94050=CARTESIAN_POINT('Origin',(-1.05,-21.0742356128,11.1596805575));
#94051=CARTESIAN_POINT('Origin',(-1.05,-21.0742356128,11.1596805575));
#94052=CARTESIAN_POINT('Origin',(-1.05,-21.0742356128,12.1167294155));
#94053=CARTESIAN_POINT('Origin',(-1.05,-21.0742356128,14.92922515));
#94054=CARTESIAN_POINT('Origin',(-8.14487887576,-21.0742356128,12.4401604693));
#94055=CARTESIAN_POINT('Origin',(-8.14487887576,-21.0742356128,12.4401604693));
#94056=CARTESIAN_POINT('Origin',(-1.05,-21.0742356128,14.92922515));
#94057=CARTESIAN_POINT('Origin',(-1.05,-21.0742356128,14.92922515));
#94058=CARTESIAN_POINT('Origin',(-1.51003344041E-15,-21.0742356128,0.580061096523));
#94059=CARTESIAN_POINT('Origin',(-5.42499920527E-16,-20.7742356128,0.580061096523));
#94060=CARTESIAN_POINT('Origin',(2.93915231795E-16,-20.7742356128,0.729452270839));
#94061=CARTESIAN_POINT('Origin',(-2.45,-20.6742356128,10.7304528845));
#94062=CARTESIAN_POINT('Origin',(-0.75,-23.1742356128,-8.70195642562));
#94063=CARTESIAN_POINT('',(-0.75,-21.0742356128,-4.99584562937));
#94064=CARTESIAN_POINT('',(-0.75,-22.1242356128,-4.99584562937));
#94065=CARTESIAN_POINT('',(-0.75,-21.0742356128,-6.2343884565225));
#94066=CARTESIAN_POINT('',(-0.75,-21.0742356128,-6.03615517446));
#94067=CARTESIAN_POINT('',(-0.75,-22.1242356128,-6.23438845923));
#94068=CARTESIAN_POINT('Origin',(2.32682891838E-16,-21.2742356128,0.729452270839));
#94069=CARTESIAN_POINT('',(-0.992653804111,-22.1242356128,5.82664824081));
#94070=CARTESIAN_POINT('',(-1.19254592572,-22.1242356128,5.7836191207));
#94071=CARTESIAN_POINT('Origin',(-1.05,-22.1242356128,6.12111625914));
#94072=CARTESIAN_POINT('',(-0.75,-21.0742356128,6.12111625914));
#94073=CARTESIAN_POINT('',(-0.75,-21.9742356128,6.12111625914));
#94074=CARTESIAN_POINT('Origin',(-1.05,-21.0742356128,6.12111625914));
#94075=CARTESIAN_POINT('Origin',(-0.75,-23.1742356128,-8.70195642562));
#94076=CARTESIAN_POINT('',(-0.75,-21.0742356128,9.0358656718));
#94077=CARTESIAN_POINT('',(-0.75,-22.1242356128,9.0358656718));
#94078=CARTESIAN_POINT('',(-0.75,-21.0742356128,7.56406439184));
#94079=CARTESIAN_POINT('Origin',(-1.05,-22.1242356128,9.0358656718));
#94080=CARTESIAN_POINT('',(-1.10198928897,-21.0742356128,9.33132652171));
#94081=CARTESIAN_POINT('',(-1.10198928897,-21.2742356128,9.33132652171));
#94082=CARTESIAN_POINT('Origin',(-1.05,-21.0742356128,9.0358656718));
#94083=CARTESIAN_POINT('Origin',(-0.00234331738835,-21.2742356128,3.08191746407));
#94084=CARTESIAN_POINT('',(-3.58772315463,-22.1242356128,8.31731489457));
#94085=CARTESIAN_POINT('Origin',(-0.00234331738835,-21.0742356128,3.08191746407));
#94086=CARTESIAN_POINT('Origin',(-1.2614400074,-22.1242356128,6.07560132137));
#94087=CARTESIAN_POINT('',(-1.46510738459,-21.9742356128,5.8553296721));
#94088=CARTESIAN_POINT('Origin',(-3.41821282746,-22.1242356128,8.06979469543));
#94089=CARTESIAN_POINT('',(-3.62188020465,-21.9742356128,7.84952304616));
#94090=CARTESIAN_POINT('Origin',(-3.88971125292,-23.1742356128,8.09716475273));
#94091=CARTESIAN_POINT('Origin',(-0.00234331738835,-21.2742356128,3.08191746407));
#94092=CARTESIAN_POINT('',(-5.76218263052,-22.1242356128,0.419477620705));
#94093=CARTESIAN_POINT('',(-6.21380646358,-22.1242356128,1.78497474518));
#94094=CARTESIAN_POINT('Origin',(-5.48986775992,-22.1242356128,0.545353000555));
#94095=CARTESIAN_POINT('',(-5.1900363009,-21.9742356128,0.55540766038));
#94096=CARTESIAN_POINT('Origin',(2.32682891838E-16,-21.2742356128,0.729452270839));
#94097=CARTESIAN_POINT('',(-5.08448267152,-22.1242356128,1.78529520144));
#94098=CARTESIAN_POINT('Origin',(-5.92013962829,-22.1242356128,1.84629187045));
#94099=CARTESIAN_POINT('',(-5.92013962829,-21.9742356128,2.14629187045));
#94100=CARTESIAN_POINT('Origin',(-5.3782162351,-22.1242356128,1.84629187045));
#94101=CARTESIAN_POINT('',(-5.3782162351,-21.9742356128,2.14629187045));
#94102=CARTESIAN_POINT('Origin',(-11.4443506127,-23.1742356128,2.14629187045));
#94103=CARTESIAN_POINT('Origin',(2.32682891838E-16,-21.2742356128,0.729452270839));
#94104=CARTESIAN_POINT('',(-3.13117783752,-22.1242356128,4.87221628548));
#94105=CARTESIAN_POINT('',(-4.2092958712,-22.1242356128,3.77060280966));
#94106=CARTESIAN_POINT('Origin',(-3.31206782846,-22.1242356128,5.11154620667));
#94107=CARTESIAN_POINT('',(-3.10840045127,-21.9742356128,5.33181785593));
#94108=CARTESIAN_POINT('Origin',(-9.80058174751,-23.1742356128,11.519536597));
#94109=CARTESIAN_POINT('',(-4.71627105755,-22.1242356128,6.81848575139));
#94110=CARTESIAN_POINT('Origin',(-4.91993843473,-22.1242356128,6.59821410213));
#94111=CARTESIAN_POINT('',(-5.16397092918,-21.0742356128,6.77270806092));
#94112=CARTESIAN_POINT('',(-5.16397092918,-21.2742356128,6.77270806092));
#94113=CARTESIAN_POINT('Origin',(-4.91993843473,-21.0742356128,6.59821410213));
#94114=CARTESIAN_POINT('Origin',(-0.00234331738835,-21.2742356128,3.08191746407));
#94115=CARTESIAN_POINT('',(-6.28256615006,-21.0742356128,3.98918589435));
#94116=CARTESIAN_POINT('',(-6.28256615006,-22.1242356128,3.98918589435));
#94117=CARTESIAN_POINT('Origin',(-0.00234331738835,-21.0742356128,3.08191746407));
#94118=CARTESIAN_POINT('Origin',(-4.452469377,-22.1242356128,3.94629187045));
#94119=CARTESIAN_POINT('',(-4.452469377,-21.0742356128,3.64629187045));
#94120=CARTESIAN_POINT('Origin',(-4.452469377,-21.0742356128,3.94629187045));
#94121=CARTESIAN_POINT('',(-4.452469377,-21.9742356128,3.64629187045));
#94122=CARTESIAN_POINT('Origin',(-5.98564848014,-22.1242356128,3.94629187045));
#94123=CARTESIAN_POINT('',(-5.98564848014,-21.0742356128,3.64629187045));
#94124=CARTESIAN_POINT('',(-5.98564848014,-21.9742356128,3.64629187045));
#94125=CARTESIAN_POINT('Origin',(-5.98564848014,-21.0742356128,3.94629187045));
#94126=CARTESIAN_POINT('Origin',(-11.7190551593,-23.1742356128,3.64629187045));
#94127=CARTESIAN_POINT('',(-4.57919858809,-21.0742356128,3.64629187045));
#94128=CARTESIAN_POINT('Origin',(-4.91993843473,-21.0742356128,6.59821410213));
#94129=CARTESIAN_POINT('Origin',(-4.91993843473,-21.0742356128,6.59821410213));
#94130=CARTESIAN_POINT('Origin',(-0.00234331738835,-21.0742356128,3.08191746407));
#94131=CARTESIAN_POINT('',(-5.98564848014,-20.7742356128,3.94629187045));
#94132=CARTESIAN_POINT('Ctrl Pts',(-5.98564848014,-20.7742356128,3.94629187045));
#94133=CARTESIAN_POINT('Ctrl Pts',(-5.99753462039329,-20.7742356128,3.94800899420363));
#94134=CARTESIAN_POINT('Ctrl Pts',(-6.00894948786785,-20.7749568618164,
3.94963477641195));
#94135=CARTESIAN_POINT('Ctrl Pts',(-6.01980989987418,-20.7762266979977,
3.95115850173577));
#94136=CARTESIAN_POINT('Ctrl Pts',(-6.03099450509648,-20.7775344399486,
3.95272771165195));
#94137=CARTESIAN_POINT('Ctrl Pts',(-6.04159134724835,-20.7794231116068,
3.95418902876826));
#94138=CARTESIAN_POINT('Ctrl Pts',(-6.05155400424851,-20.7817112682625,
3.9555638575554));
#94139=CARTESIAN_POINT('Ctrl Pts',(-6.06195399546318,-20.7840998689256,
3.95699903767931));
#94140=CARTESIAN_POINT('Ctrl Pts',(-6.07166333777175,-20.7869229649579,
3.95834038822613));
#94141=CARTESIAN_POINT('Ctrl Pts',(-6.08067142144271,-20.789995541024,3.95964186007419));
#94142=CARTESIAN_POINT('Ctrl Pts',(-6.08133300126666,-20.790221199933,3.95973744394614));
#94143=CARTESIAN_POINT('Ctrl Pts',(-6.08199081474964,-20.790448216819,3.95983282365959));
#94144=CARTESIAN_POINT('Ctrl Pts',(-6.08264486504496,-20.7906765244433,
3.95992802554191));
#94145=CARTESIAN_POINT('Ctrl Pts',(-6.09230022220808,-20.7940468946914,
3.96133343454936));
#94146=CARTESIAN_POINT('Ctrl Pts',(-6.10113662242138,-20.7976945475709,
3.96265857234215));
#94147=CARTESIAN_POINT('Ctrl Pts',(-6.10919527072438,-20.8014229304912,
3.96388251875472));
#94148=CARTESIAN_POINT('Ctrl Pts',(-6.11214308238635,-20.8027867535841,
3.96433023199061));
#94149=CARTESIAN_POINT('Ctrl Pts',(-6.11498709011435,-20.8041617700191,
3.9647646361173));
#94150=CARTESIAN_POINT('Ctrl Pts',(-6.11773006477687,-20.8055397069305,
3.96518539232357));
#94151=CARTESIAN_POINT('Ctrl Pts',(-6.12285088731743,-20.8081121588352,
3.96597089643143));
#94152=CARTESIAN_POINT('Ctrl Pts',(-6.12761988753479,-20.8106943410743,
3.96670660222514));
#94153=CARTESIAN_POINT('Ctrl Pts',(-6.13205927382818,-20.813239401917,3.96738351325775));
#94154=CARTESIAN_POINT('Ctrl Pts',(-6.13427896697488,-20.8145119323384,
3.96772196877405));
#94155=CARTESIAN_POINT('Ctrl Pts',(-6.1360941609467,-20.8155850054129,3.96799380562841));
#94156=CARTESIAN_POINT('Ctrl Pts',(-6.13799483590152,-20.8167338355379,
3.96827874364878));
#94157=CARTESIAN_POINT('Ctrl Pts',(-6.13974121001297,-20.8177894011852,
3.96854054979343));
#94158=CARTESIAN_POINT('Ctrl Pts',(-6.14155986098848,-20.8189091200391,
3.96881351450609));
#94159=CARTESIAN_POINT('Ctrl Pts',(-6.14380738476804,-20.8203385235072,
3.96913982299513));
#94160=CARTESIAN_POINT('Ctrl Pts',(-6.14400596467851,-20.8204648184169,
3.96916865397398));
#94161=CARTESIAN_POINT('Ctrl Pts',(-6.14420787354382,-20.8205935547799,
3.9691978853907));
#94162=CARTESIAN_POINT('Ctrl Pts',(-6.14441334507419,-20.820724916961,3.96922753607458));
#94163=CARTESIAN_POINT('Ctrl Pts',(-6.15508617823865,-20.8275482790126,
3.97076768522153));
#94164=CARTESIAN_POINT('Ctrl Pts',(-6.16499012109537,-20.834842585959,3.97218466576068));
#94165=CARTESIAN_POINT('Ctrl Pts',(-6.17413375640074,-20.8424304525795,
3.97348871453297));
#94166=CARTESIAN_POINT('Ctrl Pts',(-6.1823369609858,-20.8492379006211,3.97465864077245));
#94167=CARTESIAN_POINT('Ctrl Pts',(-6.18992916790955,-20.8562816337656,
3.97573831638601));
#94168=CARTESIAN_POINT('Ctrl Pts',(-6.19693925316656,-20.8634552142654,
3.97675221889574));
#94169=CARTESIAN_POINT('Ctrl Pts',(-6.20435116306778,-20.8710399911097,
3.97782423924575));
#94170=CARTESIAN_POINT('Ctrl Pts',(-6.21111336229814,-20.8787689847565,
3.978813861966));
#94171=CARTESIAN_POINT('Ctrl Pts',(-6.21728147452881,-20.8865425448021,
3.97972042315571));
#94172=CARTESIAN_POINT('Ctrl Pts',(-6.21977879971208,-20.8896898784658,
3.98008746869649));
#94173=CARTESIAN_POINT('Ctrl Pts',(-6.22230837615001,-20.8930158375082,
3.98047141698488));
#94174=CARTESIAN_POINT('Ctrl Pts',(-6.22470980772358,-20.8963114866291,
3.98082717094525));
#94175=CARTESIAN_POINT('Ctrl Pts',(-6.22724267464651,-20.8997875134873,
3.98120239606049));
#94176=CARTESIAN_POINT('Ctrl Pts',(-6.22963286905179,-20.9032293675739,
3.98154610338506));
#94177=CARTESIAN_POINT('Ctrl Pts',(-6.23173340912521,-20.9063721333557,
3.98184549185762));
#94178=CARTESIAN_POINT('Ctrl Pts',(-6.2325602073125,-20.9076091642909,3.98196333481122));
#94179=CARTESIAN_POINT('Ctrl Pts',(-6.23334256305448,-20.9087996933672,
3.98207473695029));
#94180=CARTESIAN_POINT('Ctrl Pts',(-6.23407297039883,-20.9099270947014,
3.98218035773893));
#94181=CARTESIAN_POINT('Ctrl Pts',(-6.24080352615489,-20.9203158696751,
3.98315363191598));
#94182=CARTESIAN_POINT('Ctrl Pts',(-6.24683001815921,-20.9310048591711,
3.98394041908957));
#94183=CARTESIAN_POINT('Ctrl Pts',(-6.25215756345662,-20.9419326633264,
3.98461729373962));
#94184=CARTESIAN_POINT('Ctrl Pts',(-6.2537092163496,-20.9451153972095,3.98481443415801));
#94185=CARTESIAN_POINT('Ctrl Pts',(-6.25520166000752,-20.9483187118516,
3.9850022549043));
#94186=CARTESIAN_POINT('Ctrl Pts',(-6.25663514487,-20.9515419369133,3.98518260759789));
#94187=CARTESIAN_POINT('Ctrl Pts',(-6.25875058534709,-20.956298555515,3.98544875996417));
#94188=CARTESIAN_POINT('Ctrl Pts',(-6.26080955526559,-20.9612759828185,
3.9857313059189));
#94189=CARTESIAN_POINT('Ctrl Pts',(-6.26272853899919,-20.9662974014104,
3.98599052917547));
#94190=CARTESIAN_POINT('Ctrl Pts',(-6.2646990064388,-20.9714535377876,3.98625670703708));
#94191=CARTESIAN_POINT('Ctrl Pts',(-6.26652172448506,-20.9766556017273,
3.98649806712921));
#94192=CARTESIAN_POINT('Ctrl Pts',(-6.2681448066767,-20.9817049057232,3.98671332194709));
#94193=CARTESIAN_POINT('Ctrl Pts',(-6.26968978634078,-20.9865112377941,
3.98691821872799));
#94194=CARTESIAN_POINT('Ctrl Pts',(-6.27105457364326,-20.9911787935128,
3.98710015778145));
#94195=CARTESIAN_POINT('Ctrl Pts',(-6.27222390388891,-20.9955360949015,
3.98729080196867));
#94196=CARTESIAN_POINT('Ctrl Pts',(-6.274855029626,-21.0053405174507,3.98771977302239));
#94197=CARTESIAN_POINT('Ctrl Pts',(-6.27692564331862,-21.0150164297704,
3.98807174964736));
#94198=CARTESIAN_POINT('Ctrl Pts',(-6.27851136625063,-21.0246215233591,
3.98836052942438));
#94199=CARTESIAN_POINT('Ctrl Pts',(-6.28014978966751,-21.0345458360744,
3.98865890661213));
#94200=CARTESIAN_POINT('Ctrl Pts',(-6.2812705008667,-21.0443956961073,3.98888987925294));
#94201=CARTESIAN_POINT('Ctrl Pts',(-6.28191433142828,-21.0542422738849,
3.98903308895698));
#94202=CARTESIAN_POINT('Ctrl Pts',(-6.2823497481363,-21.0609014241911,3.98912994036729));
#94203=CARTESIAN_POINT('Ctrl Pts',(-6.28256615006486,-21.0675591942924,
3.9891858943507));
#94204=CARTESIAN_POINT('Ctrl Pts',(-6.28256615006486,-21.0742356128,3.9891858943507));
#94205=CARTESIAN_POINT('Origin',(-0.00234331738835,-20.7742356128,3.08191746407));
#94206=CARTESIAN_POINT('Origin',(-4.452469377,-21.0742356128,3.94629187045));
#94207=CARTESIAN_POINT('Origin',(-4.452469377,-21.0742356128,3.94629187045));
#94208=CARTESIAN_POINT('Origin',(-5.98564848014,-21.0742356128,3.94629187045));
#94209=CARTESIAN_POINT('Origin',(-5.98564848014,-21.0742356128,3.94629187045));
#94210=CARTESIAN_POINT('Origin',(-4.57919858809,-21.0742356128,3.94629187045));
#94211=CARTESIAN_POINT('',(-5.21905892857,-20.7742356128,3.94629187045));
#94212=CARTESIAN_POINT('Origin',(2.93915231795E-16,-20.7742356128,0.729452270839));
#94213=CARTESIAN_POINT('',(-1.05,-20.7742356128,9.0358656718));
#94214=CARTESIAN_POINT('Origin',(-0.00234331738835,-20.7742356128,3.08191746407));
#94215=CARTESIAN_POINT('',(-1.05,-20.7742356128,7.56406439184));
#94216=CARTESIAN_POINT('Origin',(-10.3267865236,-19.6742356128,-3.3434289261));
#94217=CARTESIAN_POINT('Origin',(-1.05,-21.0742356128,-4.99584562937));
#94218=CARTESIAN_POINT('',(-1.01141425905,-21.0742356128,-4.69833741));
#94219=CARTESIAN_POINT('',(-1.05,-20.7742356128,-4.99584562937));
#94220=CARTESIAN_POINT('Origin',(-1.05,-21.0742356128,-4.99584562937));
#94221=CARTESIAN_POINT('Origin',(-1.05,-21.0742356128,-4.99584562937));
#94222=CARTESIAN_POINT('Origin',(-1.05,-21.0742356128,-4.99584562937));
#94223=CARTESIAN_POINT('Origin',(2.93915231795E-16,-20.7742356128,0.729452270839));
#94224=CARTESIAN_POINT('Origin',(2.93915231795E-16,-20.7742356128,0.729452270839));
#94225=CARTESIAN_POINT('Origin',(-1.05,-22.1242356128,-4.99584562937));
#94226=CARTESIAN_POINT('',(-1.01141425905,-21.2742356128,-4.69833741));
#94227=CARTESIAN_POINT('Origin',(-11.0821857629,-20.8742356128,-2.71007990903));
#94228=CARTESIAN_POINT('Origin',(-11.0821857629,-22.0742356128,-2.71007990903));
#94229=CARTESIAN_POINT('Origin',(-1.05,-21.0742356128,6.12111625914));
#94230=CARTESIAN_POINT('Origin',(-1.05,-21.0742356128,6.12111625914));
#94231=CARTESIAN_POINT('Origin',(-0.00234331738835,-21.0742356128,3.08191746407));
#94232=CARTESIAN_POINT('Ctrl Pts',(-1.05,-20.7742356128,9.0358656718));
#94233=CARTESIAN_POINT('Ctrl Pts',(-1.0523959262998,-20.7742356127999,9.0494810158149));
#94234=CARTESIAN_POINT('Ctrl Pts',(-1.05479609358863,-20.7751955471885,
9.06312046382714));
#94235=CARTESIAN_POINT('Ctrl Pts',(-1.05716675141005,-20.7770995761648,
9.07659420488324));
#94236=CARTESIAN_POINT('Ctrl Pts',(-1.05765242878117,-20.777489655146,9.07935457421036));
#94237=CARTESIAN_POINT('Ctrl Pts',(-1.05813687069917,-20.7779191854724,
9.08210800638467));
#94238=CARTESIAN_POINT('Ctrl Pts',(-1.05861979407081,-20.778387763992,9.08485290999588));
#94239=CARTESIAN_POINT('Ctrl Pts',(-1.06123562797834,-20.7809258966483,
9.09972113207978));
#94240=CARTESIAN_POINT('Ctrl Pts',(-1.06382481858908,-20.7846312659766,
9.11444090215554));
#94241=CARTESIAN_POINT('Ctrl Pts',(-1.06635220403382,-20.7894619264883,
9.12879872839508));
#94242=CARTESIAN_POINT('Ctrl Pts',(-1.06656892432023,-20.7898761498636,
9.1300298948645));
#94243=CARTESIAN_POINT('Ctrl Pts',(-1.06678519130229,-20.7902986162517,
9.13125840625777));
#94244=CARTESIAN_POINT('Ctrl Pts',(-1.06700098355357,-20.7907292818386,
9.13248413206188));
#94245=CARTESIAN_POINT('Ctrl Pts',(-1.06973333853196,-20.7961823565126,
9.14800423523072));
#94246=CARTESIAN_POINT('Ctrl Pts',(-1.0723842253386,-20.8029406104611,9.16304733867516));
#94247=CARTESIAN_POINT('Ctrl Pts',(-1.07491156867559,-20.8109185406861,
9.17744085776139));
#94248=CARTESIAN_POINT('Ctrl Pts',(-1.07743891201258,-20.818896470911,9.19183437684762));
#94249=CARTESIAN_POINT('Ctrl Pts',(-1.0798437756864,-20.8281006365983,9.20558435730489));
#94250=CARTESIAN_POINT('Ctrl Pts',(-1.08213257646722,-20.8383966814998,
9.21847863961296));
#94251=CARTESIAN_POINT('Ctrl Pts',(-1.08442137724805,-20.8486927264013,
9.23137292192103));
#94252=CARTESIAN_POINT('Ctrl Pts',(-1.08659398041548,-20.8600780828836,
9.24341074044898));
#94253=CARTESIAN_POINT('Ctrl Pts',(-1.08846412215442,-20.8724030816455,
9.25446151045095));
#94254=CARTESIAN_POINT('Ctrl Pts',(-1.09033426389336,-20.8847280804074,
9.26551228045291));
#94255=CARTESIAN_POINT('Ctrl Pts',(-1.09190173768304,-20.8979944937689,
9.27557482824863));
#94256=CARTESIAN_POINT('Ctrl Pts',(-1.09373094217068,-20.9119964096905,
9.28439342814165));
#94257=CARTESIAN_POINT('Ctrl Pts',(-1.09481843980888,-20.920320820984,9.28963625726252));
#94258=CARTESIAN_POINT('Ctrl Pts',(-1.09599868490452,-20.9289044572172,
9.29444075987992));
#94259=CARTESIAN_POINT('Ctrl Pts',(-1.0969443005408,-20.9377134971514,9.29884544678996));
#94260=CARTESIAN_POINT('Ctrl Pts',(-1.09780280437058,-20.9457110325453,
9.30284436605073));
#94261=CARTESIAN_POINT('Ctrl Pts',(-1.09846784732843,-20.9538940657016,
9.30651334732055));
#94262=CARTESIAN_POINT('Ctrl Pts',(-1.09896829273513,-20.962228930443,9.30983126609625));
#94263=CARTESIAN_POINT('Ctrl Pts',(-1.09986705170843,-20.9771976650487,
9.31578997654175));
#94264=CARTESIAN_POINT('Ctrl Pts',(-1.1002349936443,-20.9926630556998,9.32061678088581));
#94265=CARTESIAN_POINT('Ctrl Pts',(-1.10081734141703,-21.0084193812886,
9.32411179976513));
#94266=CARTESIAN_POINT('Ctrl Pts',(-1.10121648140339,-21.019218735,9.32650727864078));
#94267=CARTESIAN_POINT('Ctrl Pts',(-1.10171607543104,-21.0301449616615,
9.32827562220263));
#94268=CARTESIAN_POINT('Ctrl Pts',(-1.10194569498976,-21.0411252195446,
9.32947326775938));
#94269=CARTESIAN_POINT('Ctrl Pts',(-1.10217531916459,-21.0521056981675,
9.33067093739279));
#94270=CARTESIAN_POINT('Ctrl Pts',(-1.10213545468708,-21.0631759320558,
9.33130080239825));
#94271=CARTESIAN_POINT('Ctrl Pts',(-1.10198928897115,-21.0742356128,9.33132652171654));
#94272=CARTESIAN_POINT('Origin',(-0.45,-22.1242356128,-6.23438845923));
#94273=CARTESIAN_POINT('Origin',(-0.45,-21.0742356128,-6.23438845923));
#94274=CARTESIAN_POINT('Ctrl Pts',(-0.530881089940139,-21.0742435944873,
-6.52327990521127));
#94275=CARTESIAN_POINT('Ctrl Pts',(-0.605869334571474,-21.074241803815,
-6.50228543550801));
#94276=CARTESIAN_POINT('Ctrl Pts',(-0.674045596111476,-21.0742407617281,
-6.45695987785349));
#94277=CARTESIAN_POINT('Ctrl Pts',(-0.724740690411004,-21.0742407618033,
-6.390119097022));
#94278=CARTESIAN_POINT('Ctrl Pts',(-0.750003689199869,-21.0742418040299,
-6.31224618327166));
#94279=CARTESIAN_POINT('Ctrl Pts',(-0.750000029081184,-21.0742435948102,
-6.23437446321454));
#94280=CARTESIAN_POINT('Ctrl Pts',(-0.529863965484531,-20.9334730733702,
-6.5229624048105));
#94281=CARTESIAN_POINT('Ctrl Pts',(-0.604729632930939,-20.9650040286309,
-6.5017257304758));
#94282=CARTESIAN_POINT('Ctrl Pts',(-0.672745476661423,-20.9833541286166,
-6.45604164489109));
#94283=CARTESIAN_POINT('Ctrl Pts',(-0.723524938742467,-20.9833528049852,
-6.38909475830119));
#94284=CARTESIAN_POINT('Ctrl Pts',(-0.749174751443758,-20.9650002442128,
-6.31129794540516));
#94285=CARTESIAN_POINT('Ctrl Pts',(-0.749435926165564,-20.9334673875941,
-6.23350231178913));
#94286=CARTESIAN_POINT('Ctrl Pts',(-0.68296904973928,-20.8341940751783,
-6.57017290017678));
#94287=CARTESIAN_POINT('Ctrl Pts',(-0.709063502037876,-20.8613416651734,
-6.52452364681565));
#94288=CARTESIAN_POINT('Ctrl Pts',(-0.735145295108947,-20.874961887123,
-6.4799295145159));
#94289=CARTESIAN_POINT('Ctrl Pts',(-0.764898754103171,-20.8749609046628,
-6.43990412638473));
#94290=CARTESIAN_POINT('Ctrl Pts',(-0.799929343938473,-20.8613387211769,
-6.40244473945582));
#94291=CARTESIAN_POINT('Ctrl Pts',(-0.835971167587679,-20.8341891797982,
-6.36498507291063));
#94292=CARTESIAN_POINT('Ctrl Pts',(-0.784928027206935,-20.8055941305548,
-6.60113592908881));
#94293=CARTESIAN_POINT('Ctrl Pts',(-0.811295647961892,-20.8073540418052,
-6.57624029892075));
#94294=CARTESIAN_POINT('Ctrl Pts',(-0.837074174388714,-20.8079529197238,
-6.54898974260409));
#94295=CARTESIAN_POINT('Ctrl Pts',(-0.85992459713757,-20.8079528765283,
-6.51819337189669));
#94296=CARTESIAN_POINT('Ctrl Pts',(-0.878603960261464,-20.8073538919411,
-6.48545637104955));
#94297=CARTESIAN_POINT('Ctrl Pts',(-0.89485605580427,-20.8055938131957,
-6.45271958057142));
#94298=CARTESIAN_POINT('Ctrl Pts',(-0.922335918992876,-20.7721966680782,
-6.64273052609052));
#94299=CARTESIAN_POINT('Ctrl Pts',(-0.931743355474937,-20.7721716130412,
-6.62722231169815));
#94300=CARTESIAN_POINT('Ctrl Pts',(-0.941283625175912,-20.7721536510732,
-6.61227372299854));
#94301=CARTESIAN_POINT('Ctrl Pts',(-0.951544288548907,-20.7721534830166,
-6.59819859894796));
#94302=CARTESIAN_POINT('Ctrl Pts',(-0.962831436656691,-20.7721713423069,
-6.58460198829503));
#94303=CARTESIAN_POINT('Ctrl Pts',(-0.97469324757036,-20.7721966726456,
-6.57099919715921));
#94304=CARTESIAN_POINT('Ctrl Pts',(-1.05,-20.7742356128,-6.68100624476));
#94305=CARTESIAN_POINT('Ctrl Pts',(-1.05,-20.7742356128,-6.68100624476));
#94306=CARTESIAN_POINT('Ctrl Pts',(-1.05,-20.7742356128,-6.68100624476));
#94307=CARTESIAN_POINT('Ctrl Pts',(-1.05,-20.7742356128,-6.68100624476));
#94308=CARTESIAN_POINT('Ctrl Pts',(-1.05,-20.7742356128,-6.68100624476));
#94309=CARTESIAN_POINT('Ctrl Pts',(-1.05,-20.7742356128,-6.68100624476));
#94310=CARTESIAN_POINT('Ctrl Pts',(-1.05,-20.7742356128,-6.68100624476));
#94311=CARTESIAN_POINT('Ctrl Pts',(-1.00503272302771,-20.7742356128,-6.61525813211032));
#94312=CARTESIAN_POINT('Ctrl Pts',(-0.966555030638054,-20.784200008547,
-6.55977739297378));
#94313=CARTESIAN_POINT('Ctrl Pts',(-0.920872678369823,-20.8029478256253,
-6.49195734453869));
#94314=CARTESIAN_POINT('Ctrl Pts',(-0.907564542264599,-20.8098627882809,
-6.47191750510528));
#94315=CARTESIAN_POINT('Ctrl Pts',(-0.89025216397347,-20.8202162407514,
-6.44570801102259));
#94316=CARTESIAN_POINT('Ctrl Pts',(-0.882255155685331,-20.8253927093966,
-6.4335658302481));
#94317=CARTESIAN_POINT('Ctrl Pts',(-0.874005385604677,-20.8312552684653,
-6.42108444364487));
#94318=CARTESIAN_POINT('Ctrl Pts',(-0.870692640879228,-20.8337138929026,
-6.41609624030784));
#94319=CARTESIAN_POINT('Ctrl Pts',(-0.868532729530181,-20.8353392827204,
-6.41285098527206));
#94320=CARTESIAN_POINT('Ctrl Pts',(-0.868536031383549,-20.835325974443,
-6.41285141739827));
#94321=CARTESIAN_POINT('Ctrl Pts',(-0.84971875761109,-20.84988186283,-6.38472311999057));
#94322=CARTESIAN_POINT('Ctrl Pts',(-0.834869826129459,-20.8642005359298,
-6.36250843958396));
#94323=CARTESIAN_POINT('Ctrl Pts',(-0.815482968411093,-20.8868838228403,
-6.33336879490777));
#94324=CARTESIAN_POINT('Ctrl Pts',(-0.806507337791894,-20.898528185668,
-6.31984456655309));
#94325=CARTESIAN_POINT('Ctrl Pts',(-0.797271494820506,-20.9124718813195,
-6.3058960896103));
#94326=CARTESIAN_POINT('Ctrl Pts',(-0.793573962211397,-20.9185076218975,
-6.30031026866431));
#94327=CARTESIAN_POINT('Ctrl Pts',(-0.791166377172266,-20.9225429112605,
-6.29667352086561));
#94328=CARTESIAN_POINT('Ctrl Pts',(-0.790466771165988,-20.9237252585396,
-6.29561659938596));
#94329=CARTESIAN_POINT('Ctrl Pts',(-0.762891354789432,-20.9725020900793,
-6.25398143917688));
#94330=CARTESIAN_POINT('Ctrl Pts',(-0.75,-21.0240629896735,-6.23438843361193));
#94331=CARTESIAN_POINT('Ctrl Pts',(-0.75,-21.0742356128,-6.23438845562));
#94332=CARTESIAN_POINT('Origin',(-1.05,-21.0742356128,7.56406439184));
#94333=CARTESIAN_POINT('Ctrl Pts',(-1.05,-20.7742356128,9.0358656718));
#94334=CARTESIAN_POINT('Ctrl Pts',(-1.03689721887064,-20.7742356128,9.0358656718));
#94335=CARTESIAN_POINT('Ctrl Pts',(-1.02436620890084,-20.7750936657409,
9.03591396069315));
#94336=CARTESIAN_POINT('Ctrl Pts',(-1.01250197740514,-20.776588361968,9.03597690865791));
#94337=CARTESIAN_POINT('Ctrl Pts',(-0.999990657744915,-20.7781645805625,
9.03604328987352));
#94338=CARTESIAN_POINT('Ctrl Pts',(-0.988220470098179,-20.780447884538,
9.03612571051123));
#94339=CARTESIAN_POINT('Ctrl Pts',(-0.9772443658479,-20.783191773756,9.03618418968654));
#94340=CARTESIAN_POINT('Ctrl Pts',(-0.967775256719244,-20.785558932982,
9.03623463979891));
#94341=CARTESIAN_POINT('Ctrl Pts',(-0.958895821169001,-20.7882689318648,
9.03626719339298));
#94342=CARTESIAN_POINT('Ctrl Pts',(-0.950612352771678,-20.7911774179081,
9.03625795098188));
#94343=CARTESIAN_POINT('Ctrl Pts',(-0.940691041670133,-20.7946609822179,
9.03624688112183));
#94344=CARTESIAN_POINT('Ctrl Pts',(-0.931618460909888,-20.7984298272103,
9.03619870448758));
#94345=CARTESIAN_POINT('Ctrl Pts',(-0.923353302993488,-20.8022787377616,
9.03613447787256));
#94346=CARTESIAN_POINT('Ctrl Pts',(-0.920375997747112,-20.8036652063196,
9.03611134192769));
#94347=CARTESIAN_POINT('Ctrl Pts',(-0.917503214531104,-20.8050624512225,
9.03608633983968));
#94348=CARTESIAN_POINT('Ctrl Pts',(-0.914732311286345,-20.8064621746117,
9.03606109662758));
#94349=CARTESIAN_POINT('Ctrl Pts',(-0.909500772179841,-20.8091048896405,
9.03601343677098));
#94350=CARTESIAN_POINT('Ctrl Pts',(-0.904632123230069,-20.8117561091739,
9.03596471449331));
#94351=CARTESIAN_POINT('Ctrl Pts',(-0.900104656732014,-20.8143676035612,
9.035927646362));
#94352=CARTESIAN_POINT('Ctrl Pts',(-0.897840923482987,-20.8156733507549,
9.03590911229635));
#94353=CARTESIAN_POINT('Ctrl Pts',(-0.895976722356037,-20.8167827050556,
9.03589341635984));
#94354=CARTESIAN_POINT('Ctrl Pts',(-0.89403431412729,-20.8179648486727,
9.03588251977217));
#94355=CARTESIAN_POINT('Ctrl Pts',(-0.892198750878441,-20.8190819667667,
9.0358722225671));
#94356=CARTESIAN_POINT('Ctrl Pts',(-0.890293122601369,-20.8202640633863,
9.03586615670055));
#94357=CARTESIAN_POINT('Ctrl Pts',(-0.887937645634305,-20.8217761243718,
9.03586587241935));
#94358=CARTESIAN_POINT('Ctrl Pts',(-0.887800537371023,-20.8218641388414,
9.03586585587183));
#94359=CARTESIAN_POINT('Ctrl Pts',(-0.887661913346612,-20.8219532839679,
9.03586585902197));
#94360=CARTESIAN_POINT('Ctrl Pts',(-0.88752170207832,-20.8220436170816,
9.03586588222689));
#94361=CARTESIAN_POINT('Ctrl Pts',(-0.875790229627156,-20.8296017858925,
9.03586782378187));
#94362=CARTESIAN_POINT('Ctrl Pts',(-0.865002652397592,-20.837709857829,
9.03588740175503));
#94363=CARTESIAN_POINT('Ctrl Pts',(-0.85513457659743,-20.8461403144017,
9.03590580540881));
#94364=CARTESIAN_POINT('Ctrl Pts',(-0.847849685717023,-20.8523639143666,
9.03591939150323));
#94365=CARTESIAN_POINT('Ctrl Pts',(-0.841064842089272,-20.8587638439859,
9.03593188650693));
#94366=CARTESIAN_POINT('Ctrl Pts',(-0.83475747530647,-20.865260371867,9.03593079134057));
#94367=CARTESIAN_POINT('Ctrl Pts',(-0.827331828577942,-20.8729087174712,
9.03592950200402));
#94368=CARTESIAN_POINT('Ctrl Pts',(-0.820566291017425,-20.8806916527784,
9.03591648427122));
#94369=CARTESIAN_POINT('Ctrl Pts',(-0.814403529620822,-20.8885091959321,
9.03590063301748));
#94370=CARTESIAN_POINT('Ctrl Pts',(-0.811809679859459,-20.8917995281612,
9.03589396137013));
#94371=CARTESIAN_POINT('Ctrl Pts',(-0.809174848559519,-20.8952906291691,
9.03588689130171));
#94372=CARTESIAN_POINT('Ctrl Pts',(-0.806688716921365,-20.8987374096837,
9.03588082404002));
#94373=CARTESIAN_POINT('Ctrl Pts',(-0.804046067395552,-20.902401187077,
9.03587437480541));
#94374=CARTESIAN_POINT('Ctrl Pts',(-0.801571639184609,-20.9060145063025,
9.03586906588609));
#94375=CARTESIAN_POINT('Ctrl Pts',(-0.799442290801424,-20.9092482364348,
9.03586681334286));
#94376=CARTESIAN_POINT('Ctrl Pts',(-0.798815366061185,-20.9102003142814,
9.03586615014697));
#94377=CARTESIAN_POINT('Ctrl Pts',(-0.798218038451281,-20.9111193010546,
9.03586575284659));
#94378=CARTESIAN_POINT('Ctrl Pts',(-0.797654124306548,-20.9119964097062,
9.03586567179813));
#94379=CARTESIAN_POINT('Ctrl Pts',(-0.790082400390862,-20.9237734233107,
9.03586458355345));
#94380=CARTESIAN_POINT('Ctrl Pts',(-0.783434264015833,-20.9359220630882,
9.0359759557514));
#94381=CARTESIAN_POINT('Ctrl Pts',(-0.777682618896556,-20.9483658587849,
9.03608697054653));
#94382=CARTESIAN_POINT('Ctrl Pts',(-0.776930171717263,-20.9499937928416,
9.03610149382948));
#94383=CARTESIAN_POINT('Ctrl Pts',(-0.776193089454086,-20.9516268154847,
9.03611595308919));
#94384=CARTESIAN_POINT('Ctrl Pts',(-0.775471332291151,-20.9532647869322,
9.0361300481624));
#94385=CARTESIAN_POINT('Ctrl Pts',(-0.773245359604993,-20.9583164578959,
9.03617351880543));
#94386=CARTESIAN_POINT('Ctrl Pts',(-0.771079574482088,-20.9636200439308,
9.03621337543365));
#94387=CARTESIAN_POINT('Ctrl Pts',(-0.769078220880423,-20.9689606816328,
9.03624367184624));
#94388=CARTESIAN_POINT('Ctrl Pts',(-0.767021713500409,-20.9744484978983,
9.03627480317457));
#94389=CARTESIAN_POINT('Ctrl Pts',(-0.765139169078809,-20.9799749931927,
9.03629581098497));
#94390=CARTESIAN_POINT('Ctrl Pts',(-0.763489899487749,-20.9852874610062,
9.03629994928468));
#94391=CARTESIAN_POINT('Ctrl Pts',(-0.762245712563468,-20.9892951156826,
9.03630307116263));
#94392=CARTESIAN_POINT('Ctrl Pts',(-0.761132979627602,-20.9931804778751,
9.03629658488695));
#94393=CARTESIAN_POINT('Ctrl Pts',(-0.760158087745634,-20.9968308572201,
9.03627763582184));
#94394=CARTESIAN_POINT('Ctrl Pts',(-0.757461543130412,-21.0069277827854,
9.03622522283076));
#94395=CARTESIAN_POINT('Ctrl Pts',(-0.755364431579379,-21.0168797090857,
9.03615294405315));
#94396=CARTESIAN_POINT('Ctrl Pts',(-0.753782303417459,-21.0267484683918,
9.03608326612259));
#94397=CARTESIAN_POINT('Ctrl Pts',(-0.752161163936008,-21.0368605665955,
9.03601187010871));
#94398=CARTESIAN_POINT('Ctrl Pts',(-0.751080542463713,-21.0468862667509,
9.03594335399294));
#94399=CARTESIAN_POINT('Ctrl Pts',(-0.750500652262316,-21.0569110834329,
9.0359029130572));
#94400=CARTESIAN_POINT('Ctrl Pts',(-0.750166935726296,-21.062680187807,
9.03587964001525));
#94401=CARTESIAN_POINT('Ctrl Pts',(-0.75,-21.0684492707566,9.0358656718));
#94402=CARTESIAN_POINT('Ctrl Pts',(-0.75,-21.0742356128,9.0358656718));
#94403=CARTESIAN_POINT('Origin',(-1.05,-21.0742356128,-6.03615517446));
#94404=CARTESIAN_POINT('',(-1.05,-20.7742356128,-5.83842593707));
#94405=CARTESIAN_POINT('Origin',(-1.05,-21.0742356128,9.0358656718));
#94406=CARTESIAN_POINT('Origin',(-11.0821857629,-22.0742356128,-2.71007990903));
#94407=CARTESIAN_POINT('Origin',(-2.45,-19.6742356128,10.7304528845));
#94408=CARTESIAN_POINT('Origin',(-4.57526812267,-21.0742356128,-3.65872047634));
#94409=CARTESIAN_POINT('',(-4.79320888776,-21.0742356128,-3.4525607739));
#94410=CARTESIAN_POINT('',(-4.57526812267,-20.7742356128,-3.65872047634));
#94411=CARTESIAN_POINT('Origin',(-4.57526812267,-21.0742356128,-3.65872047634));
#94412=CARTESIAN_POINT('',(-4.40684492179,-21.0742356128,-3.41045927235));
#94413=CARTESIAN_POINT('Origin',(-4.57526812267,-21.0742356128,-3.65872047634));
#94414=CARTESIAN_POINT('Origin',(-4.57526812267,-21.0742356128,-3.65872047634));
#94415=CARTESIAN_POINT('Origin',(-4.57526812267,-22.1242356128,-3.65872047634));
#94416=CARTESIAN_POINT('',(-4.79320888776,-21.9742356128,-3.4525607739));
#94417=CARTESIAN_POINT('',(-4.40684492179,-21.2742356128,-3.41045927235));
#94418=CARTESIAN_POINT('Origin',(-0.00234331738835,-21.2742356128,3.08191746407));
#94419=CARTESIAN_POINT('Origin',(-0.00234331738835,-21.0742356128,3.08191746407));
#94420=CARTESIAN_POINT('Origin',(-0.00234331738835,-21.0742356128,3.08191746407));
#94421=CARTESIAN_POINT('Origin',(-0.00234331738835,-20.7742356128,3.08191746407));
#94422=CARTESIAN_POINT('Origin',(-3.69394702409,-21.0742356128,-6.14889144395));
#94423=CARTESIAN_POINT('',(-3.69394702409,-20.7742356128,-7.0794205347));
#94424=CARTESIAN_POINT('',(-3.69394702409,-20.7742356128,-7.27665075431));
#94425=CARTESIAN_POINT('',(-3.69394702409,-20.7742356128,-7.17803564451));
#94426=CARTESIAN_POINT('Origin',(-3.69394702409,-21.0742356128,-7.27665075431));
#94427=CARTESIAN_POINT('Origin',(-3.69394702409,-21.0742356128,-7.0794205347));
#94428=CARTESIAN_POINT('Origin',(-3.09394702409,-21.0742356128,-7.0794205347));
#94429=CARTESIAN_POINT('',(-2.83839294143,-20.7742356128,-6.53656501909));
#94430=CARTESIAN_POINT('Origin',(-3.09394702409,-20.7742356128,-7.0794205347));
#94431=CARTESIAN_POINT('Origin',(-2.83839294143,-21.0742356128,-6.53656501909));
#94432=CARTESIAN_POINT('Origin',(2.84607155346,-21.0742356128,5.53854202767));
#94433=CARTESIAN_POINT('',(-2.48410064475,-20.7742356128,-6.69708673107));
#94434=CARTESIAN_POINT('Origin',(2.84607155346,-20.7742356128,5.53854202767));
#94435=CARTESIAN_POINT('Origin',(-2.48410064475,-21.0742356128,-6.69708673107));
#94436=CARTESIAN_POINT('Origin',(-2.72372695744,-21.0742356128,-7.24715875387));
#94437=CARTESIAN_POINT('',(-2.12372695744,-20.7742356128,-7.24715875387));
#94438=CARTESIAN_POINT('Origin',(-2.72372695744,-20.7742356128,-7.24715875387));
#94439=CARTESIAN_POINT('Origin',(-2.12372695744,-21.0742356128,-7.24715875387));
#94440=CARTESIAN_POINT('Origin',(-2.12372695744,-21.0742356128,-6.11170048962));
#94441=CARTESIAN_POINT('',(-2.12372695744,-20.7742356128,-7.96338790087));
#94442=CARTESIAN_POINT('',(-2.12372695744,-20.7742356128,-7.60527332737));
#94443=CARTESIAN_POINT('Origin',(-2.12372695744,-21.0742356128,-7.96338790087));
#94444=CARTESIAN_POINT('Origin',(2.93915231795E-16,-20.7742356128,0.729452270839));
#94445=CARTESIAN_POINT('Origin',(2.84607155346,-20.7742356128,5.53854202767));
#94446=CARTESIAN_POINT('',(-6.34552156645,-20.7742356128,-5.5301356238));
#94447=CARTESIAN_POINT('',(-5.6152263525,-20.7742356128,-4.75810745444));
#94448=CARTESIAN_POINT('Origin',(2.84607155346,-20.7742356128,5.53854202767));
#94449=CARTESIAN_POINT('Origin',(-3.69394702409,-21.0742356128,-7.27665075431));
#94450=CARTESIAN_POINT('',(-3.83031550589,-21.0742356128,-7.54386534443));
#94451=CARTESIAN_POINT('Origin',(-3.69394702409,-21.0742356128,-7.27665075431));
#94452=CARTESIAN_POINT('Origin',(-3.69394702409,-21.0742356128,-7.27665075431));
#94453=CARTESIAN_POINT('',(-3.69394702409,-20.7869530199367,-7.36307246360657));
#94454=CARTESIAN_POINT('Origin',(-3.69394702409,-21.0742356128,-7.27665075431));
#94455=CARTESIAN_POINT('Origin',(2.84607155346,-21.0742356128,5.53854202767));
#94456=CARTESIAN_POINT('',(-6.53717906469,-21.0742356128,-5.76093294477));
#94457=CARTESIAN_POINT('Ctrl Pts',(-6.34552156645,-20.7742356128,-5.5301356238));
#94458=CARTESIAN_POINT('Ctrl Pts',(-6.35462138301445,-20.7742356127979,
-5.54109378251365));
#94459=CARTESIAN_POINT('Ctrl Pts',(-6.36368064291087,-20.7752517639833,
-5.55208549333866));
#94460=CARTESIAN_POINT('Ctrl Pts',(-6.37260695645825,-20.777273789321,-5.56300022566799));
#94461=CARTESIAN_POINT('Ctrl Pts',(-6.37610580132191,-20.7780663620813,
-5.56727847053874));
#94462=CARTESIAN_POINT('Ctrl Pts',(-6.37970394101495,-20.7790449225188,
-5.5716935505611));
#94463=CARTESIAN_POINT('Ctrl Pts',(-6.38325357036565,-20.7801826608097,
-5.57606224502158));
#94464=CARTESIAN_POINT('Ctrl Pts',(-6.38688094104391,-20.7813453169938,
-5.58052661936114));
#94465=CARTESIAN_POINT('Ctrl Pts',(-6.39045731242105,-20.7826741723983,
-5.58494214445669));
#94466=CARTESIAN_POINT('Ctrl Pts',(-6.39383252904759,-20.7840858569653,
-5.58912237105533));
#94467=CARTESIAN_POINT('Ctrl Pts',(-6.39558079613565,-20.7848170697852,
-5.59128761062115));
#94468=CARTESIAN_POINT('Ctrl Pts',(-6.3972752542099,-20.7855696092156,-5.5933899123615));
#94469=CARTESIAN_POINT('Ctrl Pts',(-6.39889617916021,-20.7863267818342,
-5.59540473642287));
#94470=CARTESIAN_POINT('Ctrl Pts',(-6.4067087739043,-20.7899762307613,-5.6051158608454));
#94471=CARTESIAN_POINT('Ctrl Pts',(-6.41448410644142,-20.7944359352525,
-5.61454942787996));
#94472=CARTESIAN_POINT('Ctrl Pts',(-6.42215737836493,-20.7996683893748,
-5.62362561625228));
#94473=CARTESIAN_POINT('Ctrl Pts',(-6.42599401432668,-20.8022846164359,
-5.62816371043844));
#94474=CARTESIAN_POINT('Ctrl Pts',(-6.42980518073347,-20.8050938211416,
-5.63261251725625));
#94475=CARTESIAN_POINT('Ctrl Pts',(-6.43358309418349,-20.8080900855734,
-5.63696245862029));
#94476=CARTESIAN_POINT('Ctrl Pts',(-6.4354720509085,-20.8095882177892,-5.63913742930231));
#94477=CARTESIAN_POINT('Ctrl Pts',(-6.43735269856414,-20.8111331027077,
-5.64128768864255));
#94478=CARTESIAN_POINT('Ctrl Pts',(-6.4392240870303,-20.8127239260744,-5.64341206858515));
#94479=CARTESIAN_POINT('Ctrl Pts',(-6.44015978126338,-20.8135193377577,
-5.64447425855645));
#94480=CARTESIAN_POINT('Ctrl Pts',(-6.44109316094471,-20.8143262332724,
-5.64552997897415));
#94481=CARTESIAN_POINT('Ctrl Pts',(-6.44202410895548,-20.8151445063426,
-5.64657908588352));
#94482=CARTESIAN_POINT('Ctrl Pts',(-6.44261778414038,-20.8156663275514,
-5.64724811222139));
#94483=CARTESIAN_POINT('Ctrl Pts',(-6.44354427447535,-20.8164900898511,
-5.6482879742904));
#94484=CARTESIAN_POINT('Ctrl Pts',(-6.44416414274481,-20.8170490495453,
-5.64898306931919));
#94485=CARTESIAN_POINT('Ctrl Pts',(-6.44451629612468,-20.8173666001529,
-5.6493779597754));
#94486=CARTESIAN_POINT('Ctrl Pts',(-6.44476996974886,-20.8175974114304,
-5.64966216020775));
#94487=CARTESIAN_POINT('Ctrl Pts',(-6.44480954196002,-20.8176333489548,
-5.64970642349396));
#94488=CARTESIAN_POINT('Ctrl Pts',(-6.44518816390414,-20.817977194673,-5.65012992905467));
#94489=CARTESIAN_POINT('Ctrl Pts',(-6.44607338207147,-20.8188020664663,
-5.65117043428081));
#94490=CARTESIAN_POINT('Ctrl Pts',(-6.44745013086571,-20.8201458282837,
-5.65280979040693));
#94491=CARTESIAN_POINT('Ctrl Pts',(-6.4488238952052,-20.8214866771541,-5.65444559280981));
#94492=CARTESIAN_POINT('Ctrl Pts',(-6.45068728558032,-20.8233444260723,
-5.65667792254751));
#94493=CARTESIAN_POINT('Ctrl Pts',(-6.45300569216522,-20.8257983946515,
-5.65946510923294));
#94494=CARTESIAN_POINT('Ctrl Pts',(-6.45372613691793,-20.8265609652885,
-5.66033122738298));
#94495=CARTESIAN_POINT('Ctrl Pts',(-6.45449036269108,-20.8273813968179,
-5.66125073558712));
#94496=CARTESIAN_POINT('Ctrl Pts',(-6.45529687830475,-20.8282628146959,
-5.66222183861902));
#94497=CARTESIAN_POINT('Ctrl Pts',(-6.45785966141141,-20.8310636071537,
-5.66530761452068));
#94498=CARTESIAN_POINT('Ctrl Pts',(-6.46085151790742,-20.8344780402339,
-5.66891683889509));
#94499=CARTESIAN_POINT('Ctrl Pts',(-6.46420753902736,-20.8386266302964,
-5.67297137007079));
#94500=CARTESIAN_POINT('Ctrl Pts',(-6.46478199801265,-20.8393367553977,
-5.67366539486438));
#94501=CARTESIAN_POINT('Ctrl Pts',(-6.46536705973206,-20.8400684559734,
-5.6743723861403));
#94502=CARTESIAN_POINT('Ctrl Pts',(-6.46596231189143,-20.8408224112228,
-5.67509184754763));
#94503=CARTESIAN_POINT('Ctrl Pts',(-6.46799868596679,-20.8434017129518,
-5.67755314489032));
#94504=CARTESIAN_POINT('Ctrl Pts',(-6.47015463099074,-20.8462413196276,
-5.68016075620037));
#94505=CARTESIAN_POINT('Ctrl Pts',(-6.47241108890313,-20.8493698313455,
-5.6828917376211));
#94506=CARTESIAN_POINT('Ctrl Pts',(-6.47353931785933,-20.8509340872045,
-5.68425722833147));
#94507=CARTESIAN_POINT('Ctrl Pts',(-6.47469263688536,-20.8525706359401,
-5.68565351562601));
#94508=CARTESIAN_POINT('Ctrl Pts',(-6.47586823453987,-20.8542831556721,
-5.68707721476377));
#94509=CARTESIAN_POINT('Ctrl Pts',(-6.47645603336713,-20.8551394155382,
-5.68778906433264));
#94510=CARTESIAN_POINT('Ctrl Pts',(-6.47704939965348,-20.8560146721983,
-5.68850776421543));
#94511=CARTESIAN_POINT('Ctrl Pts',(-6.47764795866675,-20.8569093949851,
-5.68923286325865));
#94512=CARTESIAN_POINT('Ctrl Pts',(-6.47806170308007,-20.857527857904,-5.68973407645831));
#94513=CARTESIAN_POINT('Ctrl Pts',(-6.4787652989644,-20.8585915532641,-5.69058656106244));
#94514=CARTESIAN_POINT('Ctrl Pts',(-6.4791619845149,-20.8591977964133,-5.69106721237673));
#94515=CARTESIAN_POINT('Ctrl Pts',(-6.47933917912821,-20.8594685978585,
-5.69128191347602));
#94516=CARTESIAN_POINT('Ctrl Pts',(-6.47945556311053,-20.8596474323066,
-5.69142293700902));
#94517=CARTESIAN_POINT('Ctrl Pts',(-6.47945882540606,-20.8596524399293,
-5.69142689015969));
#94518=CARTESIAN_POINT('Ctrl Pts',(-6.47953375728477,-20.859767460343,-5.69151769033493));
#94519=CARTESIAN_POINT('Ctrl Pts',(-6.48003658343336,-20.8605308716777,
-5.69212361565121));
#94520=CARTESIAN_POINT('Ctrl Pts',(-6.48095350691224,-20.8619644430849,
-5.69322805168281));
#94521=CARTESIAN_POINT('Ctrl Pts',(-6.48186934924366,-20.8633963241633,
-5.69433118547028));
#94522=CARTESIAN_POINT('Ctrl Pts',(-6.48319846339372,-20.8654970458354,
-5.69593183623601));
#94523=CARTESIAN_POINT('Ctrl Pts',(-6.484902500209,-20.8683231621742,-5.69798382309152));
#94524=CARTESIAN_POINT('Ctrl Pts',(-6.48534133346799,-20.8690509597383,
-5.69851226242518));
#94525=CARTESIAN_POINT('Ctrl Pts',(-6.48580489668337,-20.8698270318595,
-5.69907047190041));
#94526=CARTESIAN_POINT('Ctrl Pts',(-6.48629224595167,-20.8706526761846,
-5.69965731484674));
#94527=CARTESIAN_POINT('Ctrl Pts',(-6.48816837764793,-20.8738311307117,
-5.70191646392924));
#94528=CARTESIAN_POINT('Ctrl Pts',(-6.49039934096965,-20.8777425180432,
-5.70460275764763));
#94529=CARTESIAN_POINT('Ctrl Pts',(-6.492913072037,-20.8824761327407,-5.70762941498989));
#94530=CARTESIAN_POINT('Ctrl Pts',(-6.4932628924439,-20.8831348806239,-5.70805061617435));
#94531=CARTESIAN_POINT('Ctrl Pts',(-6.49361814054776,-20.8838095846428,
-5.70847835057653));
#94532=CARTESIAN_POINT('Ctrl Pts',(-6.49397857387117,-20.8845005141774,
-5.70891232619948));
#94533=CARTESIAN_POINT('Ctrl Pts',(-6.49545378708667,-20.8873284113619,
-5.7106885398085));
#94534=CARTESIAN_POINT('Ctrl Pts',(-6.49701614826464,-20.8904280304556,
-5.71256964974964));
#94535=CARTESIAN_POINT('Ctrl Pts',(-6.49864678920395,-20.8938186014525,
-5.71453293450427));
#94536=CARTESIAN_POINT('Ctrl Pts',(-6.4994621096736,-20.895513886951,-5.71551457688158));
#94537=CARTESIAN_POINT('Ctrl Pts',(-6.50029445787025,-20.8972819591972,
-5.71651671212822));
#94538=CARTESIAN_POINT('Ctrl Pts',(-6.50114109704214,-20.8991252361538,
-5.71753604458659));
#94539=CARTESIAN_POINT('Ctrl Pts',(-6.50164636287223,-20.9002252854929,
-5.718144372051));
#94540=CARTESIAN_POINT('Ctrl Pts',(-6.50233258152216,-20.9017422885018,
-5.71897055637223));
#94541=CARTESIAN_POINT('Ctrl Pts',(-6.50288249303833,-20.9029801780563,
-5.71963262872614));
#94542=CARTESIAN_POINT('Ctrl Pts',(-6.50325403039707,-20.903816534819,-5.72007994544244));
#94543=CARTESIAN_POINT('Ctrl Pts',(-6.50356421322428,-20.9045245122334,
-5.72045339232661));
#94544=CARTESIAN_POINT('Ctrl Pts',(-6.50372095659478,-20.9048832171215,
-5.72064210415655));
#94545=CARTESIAN_POINT('Ctrl Pts',(-6.50683086732657,-20.9120002018932,
-5.72438629405919));
#94546=CARTESIAN_POINT('Ctrl Pts',(-6.50969750337871,-20.9193271435348,
-5.72793343384607));
#94547=CARTESIAN_POINT('Ctrl Pts',(-6.51230992256894,-20.9268368343399,
-5.73127059607242));
#94548=CARTESIAN_POINT('Ctrl Pts',(-6.51361613216405,-20.9305916797424,
-5.73293917718559));
#94549=CARTESIAN_POINT('Ctrl Pts',(-6.51485881169394,-20.9343921918088,
-5.73455529299171));
#94550=CARTESIAN_POINT('Ctrl Pts',(-6.51603673967929,-20.9382348374568,
-5.73611749502398));
#94551=CARTESIAN_POINT('Ctrl Pts',(-6.51662570367197,-20.9401561602808,
-5.73689859604012));
#94552=CARTESIAN_POINT('Ctrl Pts',(-6.51719848126221,-20.9420880150999,
-5.7376662203995));
#94553=CARTESIAN_POINT('Ctrl Pts',(-6.5177549292471,-20.9440299532835,-5.73842019816372));
#94554=CARTESIAN_POINT('Ctrl Pts',(-6.518068227445,-20.9451233272374,-5.73884471201084));
#94555=CARTESIAN_POINT('Ctrl Pts',(-6.51851504736597,-20.9467195697101,
-5.73945651069025));
#94556=CARTESIAN_POINT('Ctrl Pts',(-6.51885870560263,-20.9479763409979,
-5.73992904768629));
#94557=CARTESIAN_POINT('Ctrl Pts',(-6.51912541772417,-20.9489517174058,
-5.74029578222449));
#94558=CARTESIAN_POINT('Ctrl Pts',(-6.51933137464634,-20.9497215873646,
-5.74058029811398));
#94559=CARTESIAN_POINT('Ctrl Pts',(-6.51937514746328,-20.94988556466,-5.74064102913961));
#94560=CARTESIAN_POINT('Ctrl Pts',(-6.51953189131393,-20.9504727426052,
-5.74085849777596));
#94561=CARTESIAN_POINT('Ctrl Pts',(-6.51995825601406,-20.9519071351304,
-5.7413568825184));
#94562=CARTESIAN_POINT('Ctrl Pts',(-6.52062847809654,-20.9542065208781,
-5.74210513476412));
#94563=CARTESIAN_POINT('Ctrl Pts',(-6.52081492568855,-20.9548461818904,
-5.74231328939388));
#94564=CARTESIAN_POINT('Ctrl Pts',(-6.52102006186129,-20.9555529011717,
-5.74254056006038));
#94565=CARTESIAN_POINT('Ctrl Pts',(-6.52124290425209,-20.9563273184521,
-5.74278576272304));
#94566=CARTESIAN_POINT('Ctrl Pts',(-6.5217203956944,-20.9579866868641,-5.74331116622743));
#94567=CARTESIAN_POINT('Ctrl Pts',(-6.52240651959259,-20.9604015063807,
-5.74405486018587));
#94568=CARTESIAN_POINT('Ctrl Pts',(-6.52310449530053,-20.9629612481078,
-5.74480417864417));
#94569=CARTESIAN_POINT('Ctrl Pts',(-6.52376236227997,-20.9653738959107,
-5.74551043799561));
#94570=CARTESIAN_POINT('Ctrl Pts',(-6.52443037325414,-20.9679152808702,
-5.74622123045526));
#94571=CARTESIAN_POINT('Ctrl Pts',(-6.52497603397311,-20.9700535545329,
-5.74679738364521));
#94572=CARTESIAN_POINT('Ctrl Pts',(-6.52509285049939,-20.9705113219565,
-5.74692072808235));
#94573=CARTESIAN_POINT('Ctrl Pts',(-6.52520417807828,-20.9709505462195,
-5.74703804466427));
#94574=CARTESIAN_POINT('Ctrl Pts',(-6.52530888899692,-20.9713659136585,
-5.74714817548923));
#94575=CARTESIAN_POINT('Ctrl Pts',(-6.52622696913516,-20.9750077554146,
-5.74811377606193));
#94576=CARTESIAN_POINT('Ctrl Pts',(-6.52695772118715,-20.9781122602895,
-5.74888261750753));
#94577=CARTESIAN_POINT('Ctrl Pts',(-6.52759396873366,-20.9809631998065,
-5.74956650069956));
#94578=CARTESIAN_POINT('Ctrl Pts',(-6.52829065852984,-20.9840849728992,
-5.75031535143271));
#94579=CARTESIAN_POINT('Ctrl Pts',(-6.5288736745872,-20.9869032273788,-5.75096189958322));
#94580=CARTESIAN_POINT('Ctrl Pts',(-6.52942882700837,-20.9898113882429,
-5.75160948203996));
#94581=CARTESIAN_POINT('Ctrl Pts',(-6.52959567907912,-20.9906854412845,
-5.75180411412616));
#94582=CARTESIAN_POINT('Ctrl Pts',(-6.5297597991612,-20.9915677238951,-5.75199858061829));
#94583=CARTESIAN_POINT('Ctrl Pts',(-6.52992296280191,-20.9924691784577,
-5.75219501960245));
#94584=CARTESIAN_POINT('Ctrl Pts',(-6.5330537311515,-21.0097662024811,-5.75596427206302));
#94585=CARTESIAN_POINT('Ctrl Pts',(-6.53518820255804,-21.027504551347,-5.75853433457631));
#94586=CARTESIAN_POINT('Ctrl Pts',(-6.53629205249415,-21.0453989597899,
-5.7598638744019));
#94587=CARTESIAN_POINT('Ctrl Pts',(-6.53688316709687,-21.0549814635267,
-5.76057584654602));
#94588=CARTESIAN_POINT('Ctrl Pts',(-6.53717929485058,-21.0646085312747,
-5.76093275370235));
#94589=CARTESIAN_POINT('Ctrl Pts',(-6.53717906472003,-21.0742356128,-5.76093294480616));
#94590=CARTESIAN_POINT('Origin',(2.84607155346,-21.0742356128,5.53854202767));
#94591=CARTESIAN_POINT('Origin',(-2.12372695744,-21.0742356128,-7.96338790087));
#94592=CARTESIAN_POINT('Origin',(-2.12372695744,-21.0742356128,-7.96338790086));
#94593=CARTESIAN_POINT('Ctrl Pts',(4.9961481711E-16,-20.7742356128,-8.56468050289));
#94594=CARTESIAN_POINT('Ctrl Pts',(4.9961481711E-16,-20.7742356128,-8.56468050289));
#94595=CARTESIAN_POINT('Ctrl Pts',(4.9961481711E-16,-20.7742356128,-8.56468050289));
#94596=CARTESIAN_POINT('Ctrl Pts',(4.9961481711E-16,-20.7742356128,-8.56468050289));
#94597=CARTESIAN_POINT('Ctrl Pts',(4.9961481711E-16,-20.7742356128,-8.56468050289));
#94598=CARTESIAN_POINT('Ctrl Pts',(4.9961481711E-16,-20.7742356128,-8.56468050289));
#94599=CARTESIAN_POINT('Ctrl Pts',(-0.0739219411499,-20.7751437694,-8.66437291113));
#94600=CARTESIAN_POINT('Ctrl Pts',(-0.0443506287058,-20.7751432313524,-8.66431384724197));
#94601=CARTESIAN_POINT('Ctrl Pts',(-0.0147838746951,-20.7751431251168,-8.66430218528719));
#94602=CARTESIAN_POINT('Ctrl Pts',(0.0147838753332,-20.7751431251168,-8.66430218528719));
#94603=CARTESIAN_POINT('Ctrl Pts',(0.0443506291288,-20.7751432313524,-8.66431384724197));
#94604=CARTESIAN_POINT('Ctrl Pts',(0.0739219411508,-20.7751437694,-8.66437291113));
#94605=CARTESIAN_POINT('Ctrl Pts',(-0.152819706761,-20.8273615349,-8.76362621195));
#94606=CARTESIAN_POINT('Ctrl Pts',(-0.0916409326323,-20.8166811403,-8.76306421395));
#94607=CARTESIAN_POINT('Ctrl Pts',(-0.0305356341741,-20.8113350481,-8.76271543885));
#94608=CARTESIAN_POINT('Ctrl Pts',(0.0305356341745,-20.8113350481,-8.76271543885));
#94609=CARTESIAN_POINT('Ctrl Pts',(0.0916409326401,-20.8166811403,-8.76306421395));
#94610=CARTESIAN_POINT('Ctrl Pts',(0.15281970676,-20.8273615349,-8.76362621195));
#94611=CARTESIAN_POINT('Ctrl Pts',(-0.208944325295,-20.9488183216,-8.82888814763));
#94612=CARTESIAN_POINT('Ctrl Pts',(-0.12665670177,-20.9401545709,-8.84731068645));
#94613=CARTESIAN_POINT('Ctrl Pts',(-0.042439220578,-20.9357432811,-8.85664858235));
#94614=CARTESIAN_POINT('Ctrl Pts',(0.0424392246749,-20.9357432811,-8.85664858234));
#94615=CARTESIAN_POINT('Ctrl Pts',(0.126656704487,-20.9401545709,-8.84731068645));
#94616=CARTESIAN_POINT('Ctrl Pts',(0.208944325295,-20.9488183216,-8.82888814763));
#94617=CARTESIAN_POINT('Ctrl Pts',(-0.207931718075,-21.0742356128,-8.82796731988));
#94618=CARTESIAN_POINT('Ctrl Pts',(-0.125978962059,-21.0742356128,-8.8453886697));
#94619=CARTESIAN_POINT('Ctrl Pts',(-0.0422016682077,-21.0742356128,-8.85422710799));
#94620=CARTESIAN_POINT('Ctrl Pts',(0.0422016682077,-21.0742356128,-8.85422710799));
#94621=CARTESIAN_POINT('Ctrl Pts',(0.125978962059,-21.0742356128,-8.8453886697));
#94622=CARTESIAN_POINT('Ctrl Pts',(0.207931718075,-21.0742356128,-8.82796731988));
#94623=CARTESIAN_POINT('',(-0.207931718075,-21.0742356128,-8.82796731988));
#94624=CARTESIAN_POINT('Ctrl Pts',(-0.207931718084929,-21.0742356128,-8.82796731992671));
#94625=CARTESIAN_POINT('Ctrl Pts',(-0.20793171808493,-21.058807737806,-8.82796731992671));
#94626=CARTESIAN_POINT('Ctrl Pts',(-0.206991629534422,-21.0430697565,-8.82694819743859));
#94627=CARTESIAN_POINT('Ctrl Pts',(-0.205085678166485,-21.0272270718591,
-8.82478346590272));
#94628=CARTESIAN_POINT('Ctrl Pts',(-0.203232437820272,-21.0118225327598,
-8.82267860221707));
#94629=CARTESIAN_POINT('Ctrl Pts',(-0.200465888764402,-20.9963193501386,
-8.81949003333179));
#94630=CARTESIAN_POINT('Ctrl Pts',(-0.19677085228483,-20.980944658764,-8.81513107578119));
#94631=CARTESIAN_POINT('Ctrl Pts',(-0.195150931677628,-20.9742043249338,
-8.81322008919115));
#94632=CARTESIAN_POINT('Ctrl Pts',(-0.193352680913129,-20.9674891605202,
-8.81108459728923));
#94633=CARTESIAN_POINT('Ctrl Pts',(-0.191375454563993,-20.9608204182865,
-8.80871960777743));
#94634=CARTESIAN_POINT('Ctrl Pts',(-0.187012508935183,-20.9461051785314,
-8.80350102435265));
#94635=CARTESIAN_POINT('Ctrl Pts',(-0.181777358262892,-20.9316143647805,
-8.79716206443024));
#94636=CARTESIAN_POINT('Ctrl Pts',(-0.175670860520978,-20.9175956542866,
-8.78967869242846));
#94637=CARTESIAN_POINT('Ctrl Pts',(-0.173991508311643,-20.9137403589218,
-8.78762068506718));
#94638=CARTESIAN_POINT('Ctrl Pts',(-0.172246322135771,-20.9099209095847,
-8.78547638336927));
#94639=CARTESIAN_POINT('Ctrl Pts',(-0.170435476972045,-20.9061427547366,
-8.78324590276991));
#94640=CARTESIAN_POINT('Ctrl Pts',(-0.166237736720972,-20.8973845720942,
-8.77807540096295));
#94641=CARTESIAN_POINT('Ctrl Pts',(-0.161687020782996,-20.888848122063,
-8.77244120058218));
#94642=CARTESIAN_POINT('Ctrl Pts',(-0.156787037910526,-20.8806033711716,
-8.76635090530234));
#94643=CARTESIAN_POINT('Ctrl Pts',(-0.154337046474292,-20.8764809957259,
-8.76330575766242));
#94644=CARTESIAN_POINT('Ctrl Pts',(-0.151799750460363,-20.8724314930626,
-8.7601466442437));
#94645=CARTESIAN_POINT('Ctrl Pts',(-0.149175845791688,-20.868463921362,
-8.75687546171829));
#94646=CARTESIAN_POINT('Ctrl Pts',(-0.147863893457352,-20.8664801355117,
-8.75523987045558));
#94647=CARTESIAN_POINT('Ctrl Pts',(-0.146530289983459,-20.8645168283287,
-8.7535762667923));
#94648=CARTESIAN_POINT('Ctrl Pts',(-0.145175132487716,-20.8625751257222,
-8.75188493254781));
#94649=CARTESIAN_POINT('Ctrl Pts',(-0.144417055132561,-20.8614889340574,
-8.75093879736075));
#94650=CARTESIAN_POINT('Ctrl Pts',(-0.143420664491045,-20.8600877544966,
-8.74969906130205));
#94651=CARTESIAN_POINT('Ctrl Pts',(-0.142574027140396,-20.8589148254055,
-8.74864098373894));
#94652=CARTESIAN_POINT('Ctrl Pts',(-0.141907194996003,-20.8579909979599,
-8.74780761614677));
#94653=CARTESIAN_POINT('Ctrl Pts',(-0.141333533377844,-20.8572073668546,
-8.74708833579977));
#94654=CARTESIAN_POINT('Ctrl Pts',(-0.141045101226366,-20.8568159508745,
-8.74672804704856));
#94655=CARTESIAN_POINT('Ctrl Pts',(-0.137764128976178,-20.8523635173909,
-8.74262969189393));
#94656=CARTESIAN_POINT('Ctrl Pts',(-0.133874809386624,-20.8474708462403,
-8.73788048463094));
#94657=CARTESIAN_POINT('Ctrl Pts',(-0.129357595883939,-20.8422910728369,
-8.7323721476904));
#94658=CARTESIAN_POINT('Ctrl Pts',(-0.124987989632303,-20.8372805569,-8.72704380456091));
#94659=CARTESIAN_POINT('Ctrl Pts',(-0.120030647505103,-20.832001217571,
-8.72100417194565));
#94660=CARTESIAN_POINT('Ctrl Pts',(-0.114469013595954,-20.8266392802401,
-8.7141550459496));
#94661=CARTESIAN_POINT('Ctrl Pts',(-0.109120501929856,-20.821482812764,
-8.7075683789933));
#94662=CARTESIAN_POINT('Ctrl Pts',(-0.103212926652253,-20.8162500078874,
-8.700232109932));
#94663=CARTESIAN_POINT('Ctrl Pts',(-0.0967355344333589,-20.8111521065984,
-8.69207251981437));
#94664=CARTESIAN_POINT('Ctrl Pts',(-0.0906551254465784,-20.8063666429791,
-8.68441301064724));
#94665=CARTESIAN_POINT('Ctrl Pts',(-0.0840724678907984,-20.8017004470412,
-8.67602728380219));
#94666=CARTESIAN_POINT('Ctrl Pts',(-0.0769845460691857,-20.7973657450748,
-8.66687829516898));
#94667=CARTESIAN_POINT('Ctrl Pts',(-0.070136880226554,-20.7931779744784,
-8.65803942553482));
#94668=CARTESIAN_POINT('Ctrl Pts',(-0.0628174889399522,-20.7892999888431,
-8.64848743646407));
#94669=CARTESIAN_POINT('Ctrl Pts',(-0.0550312825271058,-20.7859539936799,
-8.63822244714815));
#94670=CARTESIAN_POINT('Ctrl Pts',(-0.047498167146639,-20.7827167602583,
-8.62829112182797));
#94671=CARTESIAN_POINT('Ctrl Pts',(-0.0395279866114865,-20.7799780356088,
-8.61769177993309));
#94672=CARTESIAN_POINT('Ctrl Pts',(-0.0311341756824106,-20.7779617380583,
-8.60646612885158));
#94673=CARTESIAN_POINT('Ctrl Pts',(-0.0230959746664929,-20.776030862422,
-8.59571606065369));
#94674=CARTESIAN_POINT('Ctrl Pts',(-0.0146692297076344,-20.7747631710937,
-8.58439126306306));
#94675=CARTESIAN_POINT('Ctrl Pts',(-0.00587517811084473,-20.7743676687153,
-8.5725740159694));
#94676=CARTESIAN_POINT('Ctrl Pts',(-0.00393453439359006,-20.7742803904912,
-8.56996622295441));
#94677=CARTESIAN_POINT('Ctrl Pts',(-0.00197604276587682,-20.7742356127995,
-8.56733464308287));
#94678=CARTESIAN_POINT('Ctrl Pts',(2.94663555151017E-14,-20.7742356128,
-8.56468050289));
#94679=CARTESIAN_POINT('Origin',(1.59370492737E-14,-21.0742356128,-7.84982397628));
#94680=CARTESIAN_POINT('Origin',(2.84607155346,-21.0742356128,5.53854202767));
#94681=CARTESIAN_POINT('Origin',(2.84607155346,-21.0742356128,5.53854202767));
#94682=CARTESIAN_POINT('Origin',(-3.69394702409,-23.1223803511,-7.27665075431));
#94683=CARTESIAN_POINT('',(-3.83031550589,-22.5742356128,-7.54386534443));
#94684=CARTESIAN_POINT('Origin',(2.84607155346,-21.2742356128,5.53854202767));
#94685=CARTESIAN_POINT('',(-6.53717906469,-22.1242356128,-5.76093294477));
#94686=CARTESIAN_POINT('Origin',(1.56676269779E-14,-23.2742356128,-7.84982397628));
#94687=CARTESIAN_POINT('',(-0.207931718075,-22.6642356128,-8.82796731988));
#94688=CARTESIAN_POINT('Origin',(2.84607155346,-22.6642356128,5.53854202767));
#94689=CARTESIAN_POINT('Origin',(-6.34552156645,-22.1242356128,-5.5301356238));
#94690=CARTESIAN_POINT('',(-6.56346233154,-21.0742356128,-5.32397592135));
#94691=CARTESIAN_POINT('Origin',(-6.34552156645,-21.0742356128,-5.5301356238));
#94692=CARTESIAN_POINT('',(-6.56346233154,-21.9742356128,-5.32397592135));
#94693=CARTESIAN_POINT('Origin',(-6.34552156645,-21.0742356128,-5.5301356238));
#94694=CARTESIAN_POINT('Origin',(-6.34552156645,-21.0742356128,-5.5301356238));
#94695=CARTESIAN_POINT('Origin',(-5.6152263525,-21.0742356128,-4.75810745444));
#94696=CARTESIAN_POINT('',(-5.67833560965,-21.0742356128,-4.38826834763));
#94697=CARTESIAN_POINT('Origin',(-6.78099426296,-23.1742356128,-5.55393878512));
#94698=CARTESIAN_POINT('',(-6.4527882763,-22.8742356128,-5.20697736155));
#94699=CARTESIAN_POINT('Origin',(-6.6707290414,-22.8742356128,-5.00081765911));
#94700=CARTESIAN_POINT('',(-5.89627637474,-23.1742356128,-4.18210864518));
#94701=CARTESIAN_POINT('Ctrl Pts',(-8.01224741424,-22.8742356128,11.9089404858));
#94702=CARTESIAN_POINT('Ctrl Pts',(-8.01224741424,-22.8742356128,11.9089404858));
#94703=CARTESIAN_POINT('Ctrl Pts',(-8.01224741424,-22.8742356128,11.9089404858));
#94704=CARTESIAN_POINT('Ctrl Pts',(-8.01224741424,-22.8742356128,11.9089404858));
#94705=CARTESIAN_POINT('Ctrl Pts',(-8.01224741424,-22.8742356128,11.9089404858));
#94706=CARTESIAN_POINT('Ctrl Pts',(-8.01224741424,-22.8742356128,11.9089404858));
#94707=CARTESIAN_POINT('Ctrl Pts',(-7.9829584197,-22.9540055384,11.8818593216));
#94708=CARTESIAN_POINT('Ctrl Pts',(-7.97710218322187,-22.9460296098,11.8764445334088));
#94709=CARTESIAN_POINT('Ctrl Pts',(-7.97124593377672,-22.9380536813,11.871029733228));
#94710=CARTESIAN_POINT('Ctrl Pts',(-7.96538971029938,-22.9300777704,11.8656149570576));
#94711=CARTESIAN_POINT('Ctrl Pts',(-7.95953347384813,-22.9221018241,11.8602001688912));
#94712=CARTESIAN_POINT('Ctrl Pts',(-7.95367723737,-22.9141258956,11.8547853807));
#94713=CARTESIAN_POINT('Ctrl Pts',(-7.95813278234,-23.0338190575,11.8499462819));
#94714=CARTESIAN_POINT('Ctrl Pts',(-7.94826431478,-23.0178581995,11.8371231287));
#94715=CARTESIAN_POINT('Ctrl Pts',(-7.9374729589,-23.0018973414,11.825280653));
#94716=CARTESIAN_POINT('Ctrl Pts',(-7.92575194148,-22.985933847,11.8144431763));
#94717=CARTESIAN_POINT('Ctrl Pts',(-7.91310342567,-22.9699706625,11.8046126985));
#94718=CARTESIAN_POINT('Ctrl Pts',(-7.8995407209,-22.9540193262,11.7957709419));
#94719=CARTESIAN_POINT('Ctrl Pts',(-7.93828028322,-23.1128615217,11.8131880532));
#94720=CARTESIAN_POINT('Ctrl Pts',(-7.92684545497,-23.0884116462,11.7921000842));
#94721=CARTESIAN_POINT('Ctrl Pts',(-7.91214424925,-23.0639617707,11.7733048715));
#94722=CARTESIAN_POINT('Ctrl Pts',(-7.89441627707,-23.0398170763,11.7569132495));
#94723=CARTESIAN_POINT('Ctrl Pts',(-7.87387109886,-23.0162629748,11.743118982));
#94724=CARTESIAN_POINT('Ctrl Pts',(-7.85067760242,-22.993550642,11.7321889401));
#94725=CARTESIAN_POINT('Ctrl Pts',(-7.91959338184,-23.2114810387,11.7607695014));
#94726=CARTESIAN_POINT('Ctrl Pts',(-7.91104746367,-23.1749621125,11.7286518091));
#94727=CARTESIAN_POINT('Ctrl Pts',(-7.89353608553,-23.1384431864,11.699923838));
#94728=CARTESIAN_POINT('Ctrl Pts',(-7.86773087157,-23.1032976549,11.6760638439));
#94729=CARTESIAN_POINT('Ctrl Pts',(-7.83466815185,-23.0709369526,11.6580300375));
#94730=CARTESIAN_POINT('Ctrl Pts',(-7.79578364279,-23.0428577871,11.6462926502));
#94731=CARTESIAN_POINT('Ctrl Pts',(-7.9155846643,-23.3039994083,11.6969647216));
#94732=CARTESIAN_POINT('Ctrl Pts',(-7.91452330598,-23.2518708228,11.6602860726));
#94733=CARTESIAN_POINT('Ctrl Pts',(-7.89660201748,-23.1997422373,11.6241805214));
#94734=CARTESIAN_POINT('Ctrl Pts',(-7.86189143973,-23.152468004,11.5920864577));
#94735=CARTESIAN_POINT('Ctrl Pts',(-7.813878937,-23.1147977551,11.5672283653));
#94736=CARTESIAN_POINT('Ctrl Pts',(-7.7578101336,-23.0891176504,11.5510833748));
#94737=CARTESIAN_POINT('Ctrl Pts',(-7.91547477954,-23.3227166577,11.6832984902));
#94738=CARTESIAN_POINT('Ctrl Pts',(-7.91611333971,-23.2672089627,11.6460479894));
#94739=CARTESIAN_POINT('Ctrl Pts',(-7.8981958921,-23.2117012676,11.6085883389));
#94740=CARTESIAN_POINT('Ctrl Pts',(-7.86161748026,-23.161883129,11.5747672402));
#94741=CARTESIAN_POINT('Ctrl Pts',(-7.81044715471,-23.1232964092,11.5483470151));
#94742=CARTESIAN_POINT('Ctrl Pts',(-7.75082874056,-23.0984762171,11.5310636155));
#94743=CARTESIAN_POINT('Ctrl Pts',(-7.91677660432,-23.3563766548,11.6571003353));
#94744=CARTESIAN_POINT('Ctrl Pts',(-7.92076615745,-23.2943123864,11.6196720445));
#94745=CARTESIAN_POINT('Ctrl Pts',(-7.90299820073,-23.232248118,11.5801462658));
#94746=CARTESIAN_POINT('Ctrl Pts',(-7.86292199155,-23.177666138,11.5430910367));
#94747=CARTESIAN_POINT('Ctrl Pts',(-7.80583878281,-23.1377865125,11.5134079972));
#94748=CARTESIAN_POINT('Ctrl Pts',(-7.73977321638,-23.1153060651,11.4934396195));
#94749=CARTESIAN_POINT('Ctrl Pts',(-7.92150726931,-23.3879026248,11.6287650914));
#94750=CARTESIAN_POINT('Ctrl Pts',(-7.92877089289,-23.3187255874,11.5933170483));
#94751=CARTESIAN_POINT('Ctrl Pts',(-7.91117889789,-23.2495485499,11.5529211001));
#94752=CARTESIAN_POINT('Ctrl Pts',(-7.86756066908,-23.1901424998,11.512590852));
#94753=CARTESIAN_POINT('Ctrl Pts',(-7.80474013232,-23.1498013146,11.4786358364));
#94754=CARTESIAN_POINT('Ctrl Pts',(-7.73293017851,-23.1310691765,11.4544031088));
#94755=CARTESIAN_POINT('Ctrl Pts',(-7.92449811306,-23.4017307742,11.6153459759));
#94756=CARTESIAN_POINT('Ctrl Pts',(-7.93315539553,-23.3292061538,11.5813393505));
#94757=CARTESIAN_POINT('Ctrl Pts',(-7.91560788059,-23.2566815335,11.5408618336));
#94758=CARTESIAN_POINT('Ctrl Pts',(-7.8703758173,-23.195077514,11.4990394033));
#94759=CARTESIAN_POINT('Ctrl Pts',(-7.80503619115,-23.1547136059,11.4628778853));
#94760=CARTESIAN_POINT('Ctrl Pts',(-7.73084447823,-23.1379833031,11.4362901237));
#94761=CARTESIAN_POINT('Ctrl Pts',(-7.93181038161,-23.4257772831,11.589727728));
#94762=CARTESIAN_POINT('Ctrl Pts',(-7.94259323556,-23.3469662924,11.5595945247));
#94763=CARTESIAN_POINT('Ctrl Pts',(-7.92493476604,-23.2681553018,11.519738107));
#94764=CARTESIAN_POINT('Ctrl Pts',(-7.87677950673,-23.2025700218,11.4752128338));
#94765=CARTESIAN_POINT('Ctrl Pts',(-7.80718493183,-23.1625463217,11.4343934188));
#94766=CARTESIAN_POINT('Ctrl Pts',(-7.7293286586,-23.1500063561,11.4025092567));
#94767=CARTESIAN_POINT('Ctrl Pts',(-7.9432480685,-23.4460266432,11.5624437668));
#94768=CARTESIAN_POINT('Ctrl Pts',(-7.95448793125,-23.3612017167,11.5386017188));
#94769=CARTESIAN_POINT('Ctrl Pts',(-7.93590497166,-23.2763767903,11.501049282));
#94770=CARTESIAN_POINT('Ctrl Pts',(-7.88511487967,-23.2072029876,11.4540877922));
#94771=CARTESIAN_POINT('Ctrl Pts',(-7.81267918242,-23.1680646299,11.4074826391));
#94772=CARTESIAN_POINT('Ctrl Pts',(-7.73333253621,-23.160131205,11.3683518533));
#94773=CARTESIAN_POINT('Ctrl Pts',(-7.94999449773,-23.4537301075,11.5494738265));
#94774=CARTESIAN_POINT('Ctrl Pts',(-7.96070319611,-23.3664896798,11.5290641468));
#94775=CARTESIAN_POINT('Ctrl Pts',(-7.94047144087,-23.2792492521,11.4940040546));
#94776=CARTESIAN_POINT('Ctrl Pts',(-7.88862227931,-23.2086330447,11.4460633288));
#94777=CARTESIAN_POINT('Ctrl Pts',(-7.81641530283,-23.1699761106,11.3956528028));
#94778=CARTESIAN_POINT('Ctrl Pts',(-7.73725084228,-23.1639828938,11.3527669762));
#94779=CARTESIAN_POINT('Ctrl Pts',(-7.96049908281,-23.4651088112,11.5297325584));
#94780=CARTESIAN_POINT('Ctrl Pts',(-7.97007721933,-23.3740670261,11.5152608651));
#94781=CARTESIAN_POINT('Ctrl Pts',(-7.94978862977,-23.283025241,11.4814426691));
#94782=CARTESIAN_POINT('Ctrl Pts',(-7.89640547391,-23.2103198029,11.4320835828));
#94783=CARTESIAN_POINT('Ctrl Pts',(-7.82205263778,-23.1724642569,11.3783945077));
#94784=CARTESIAN_POINT('Ctrl Pts',(-7.74357804624,-23.1696721938,11.3291632218));
#94785=CARTESIAN_POINT('Ctrl Pts',(-7.97506561416,-23.4709827428,11.5096523074));
#94786=CARTESIAN_POINT('Ctrl Pts',(-7.9810664946,-23.3778924556,11.5016653458));
#94787=CARTESIAN_POINT('Ctrl Pts',(-7.95750099919,-23.2848021685,11.4721994645));
#94788=CARTESIAN_POINT('Ctrl Pts',(-7.90326281492,-23.2109322204,11.4220498027));
#94789=CARTESIAN_POINT('Ctrl Pts',(-7.83108568197,-23.1736253884,11.3629902197));
#94790=CARTESIAN_POINT('Ctrl Pts',(-7.75598816389,-23.1726091877,11.3070891094));
#94791=CARTESIAN_POINT('Ctrl Pts',(-7.97859188254,-23.4732430341,11.5041738872));
#94792=CARTESIAN_POINT('Ctrl Pts',(-7.98384179584,-23.3793507423,11.4980345926));
#94793=CARTESIAN_POINT('Ctrl Pts',(-7.96094423,-23.2854584504,11.4680769659));
#94794=CARTESIAN_POINT('Ctrl Pts',(-7.90642284084,-23.2112027901,11.4176654474));
#94795=CARTESIAN_POINT('Ctrl Pts',(-7.83310388244,-23.1740525381,11.3586594366));
#94796=CARTESIAN_POINT('Ctrl Pts',(-7.75868462277,-23.1737393161,11.3008434315));
#94797=CARTESIAN_POINT('Ctrl Pts',(-7.98964252128,-23.4742356128,11.4914912894));
#94798=CARTESIAN_POINT('Ctrl Pts',(-7.99152767193,-23.3799878332,11.4894524491));
#94799=CARTESIAN_POINT('Ctrl Pts',(-7.96481831906,-23.2857400536,11.4638652708));
#94800=CARTESIAN_POINT('Ctrl Pts',(-7.91010101675,-23.2112175685,11.4132726072));
#94801=CARTESIAN_POINT('Ctrl Pts',(-7.84045640218,-23.1742356128,11.3497690655));
#94802=CARTESIAN_POINT('Ctrl Pts',(-7.76937087202,-23.1742356128,11.2878239122));
#94803=CARTESIAN_POINT('Ctrl Pts',(-7.99564314217,-23.4742356128,11.4850014593));
#94804=CARTESIAN_POINT('Ctrl Pts',(-7.99564314217,-23.3799878332,11.4850014593));
#94805=CARTESIAN_POINT('Ctrl Pts',(-7.96846821668,-23.2857400536,11.4598750038));
#94806=CARTESIAN_POINT('Ctrl Pts',(-7.91377225193,-23.2112466293,11.4093020693));
#94807=CARTESIAN_POINT('Ctrl Pts',(-7.84457187242,-23.1742356128,11.3453180757));
#94808=CARTESIAN_POINT('Ctrl Pts',(-7.77537149291,-23.1742356128,11.2813340821));
#94809=CARTESIAN_POINT('',(-7.77537149291,-23.1742356128,11.2813340821));
#94810=CARTESIAN_POINT('Ctrl Pts',(-7.77537149291,-23.1742356128,11.2813340821));
#94811=CARTESIAN_POINT('Ctrl Pts',(-7.76937087202,-23.1742356128,11.2878239122));
#94812=CARTESIAN_POINT('Ctrl Pts',(-7.75868462277,-23.1737393161,11.3008434315));
#94813=CARTESIAN_POINT('Ctrl Pts',(-7.75598816389,-23.1726091877,11.3070891094));
#94814=CARTESIAN_POINT('Ctrl Pts',(-7.74357804624,-23.1696721938,11.3291632218));
#94815=CARTESIAN_POINT('Ctrl Pts',(-7.73725084228,-23.1639828938,11.3527669762));
#94816=CARTESIAN_POINT('Ctrl Pts',(-7.73333253621,-23.160131205,11.3683518533));
#94817=CARTESIAN_POINT('Ctrl Pts',(-7.7293286586,-23.1500063561,11.4025092567));
#94818=CARTESIAN_POINT('Ctrl Pts',(-7.73084447823,-23.1379833031,11.4362901237));
#94819=CARTESIAN_POINT('Ctrl Pts',(-7.73293017851,-23.1310691765,11.4544031088));
#94820=CARTESIAN_POINT('Ctrl Pts',(-7.73977321638,-23.1153060651,11.4934396195));
#94821=CARTESIAN_POINT('Ctrl Pts',(-7.75082874056,-23.0984762171,11.5310636155));
#94822=CARTESIAN_POINT('Ctrl Pts',(-7.7578101336,-23.0891176504,11.5510833748));
#94823=CARTESIAN_POINT('Ctrl Pts',(-7.79578364279,-23.0428577871,11.6462926502));
#94824=CARTESIAN_POINT('Ctrl Pts',(-7.85067760242,-22.993550642,11.7321889401));
#94825=CARTESIAN_POINT('Ctrl Pts',(-7.8995407209,-22.9540193262,11.7957709419));
#94826=CARTESIAN_POINT('Ctrl Pts',(-7.95367723737,-22.9141258956,11.8547853807));
#94827=CARTESIAN_POINT('Ctrl Pts',(-8.01224741424,-22.8742356128,11.9089404858));
#94828=CARTESIAN_POINT('Origin',(-7.77692939202971,-23.472114284594,11.2827738681602));
#94829=CARTESIAN_POINT('Origin',(-6.6707290414,-22.8742356128,10.2599605573));
#94830=CARTESIAN_POINT('',(-5.39652599911,-23.1742356128,9.08180806924));
#94831=CARTESIAN_POINT('',(-6.58594874601,-23.1742356128,10.1815710757));
#94832=CARTESIAN_POINT('Origin',(-5.39652599911,-22.8742356128,9.08180806924));
#94833=CARTESIAN_POINT('Origin',(-4.98919124473,-22.8742356128,9.52235136777));
#94834=CARTESIAN_POINT('',(-4.62185483489,-23.1742356128,9.04794230167));
#94835=CARTESIAN_POINT('Origin',(-4.98919124473,-23.1742356128,9.52235136777));
#94836=CARTESIAN_POINT('Origin',(-4.62185483489,-22.8742356128,9.04794230167));
#94837=CARTESIAN_POINT('Origin',(-0.00234331738803,-22.8742356128,3.08191746407));
#94838=CARTESIAN_POINT('',(-0.972828518105,-23.1742356128,10.5646641188));
#94839=CARTESIAN_POINT('Origin',(-0.00234331738835,-23.1742356128,3.08191746407));
#94840=CARTESIAN_POINT('Origin',(-0.972828518105,-22.8742356128,10.5646641188));
#94841=CARTESIAN_POINT('Origin',(-1.05,-22.8742356128,11.1596805575));
#94842=CARTESIAN_POINT('',(-0.45,-23.1742356128,11.1596805575));
#94843=CARTESIAN_POINT('Origin',(-1.05,-23.1742356128,11.1596805575));
#94844=CARTESIAN_POINT('Origin',(-0.45,-22.8742356128,11.1596805575));
#94845=CARTESIAN_POINT('Origin',(-0.45,-22.8742356128,2.93538176615));
#94846=CARTESIAN_POINT('',(-0.45,-23.1742356128,14.92922515));
#94847=CARTESIAN_POINT('',(-0.45,-23.1742356128,13.0444528538));
#94848=CARTESIAN_POINT('Origin',(-0.45,-22.8742356128,14.92922515));
#94849=CARTESIAN_POINT('Ctrl Pts',(-8.78908955148,-23.4742356128,12.6272235745));
#94850=CARTESIAN_POINT('Ctrl Pts',(-8.78908955148,-23.3799878332,12.6272235745));
#94851=CARTESIAN_POINT('Ctrl Pts',(-8.76403540825,-23.2856521198,12.6543202923));
#94852=CARTESIAN_POINT('Ctrl Pts',(-8.71344985896,-23.2111401141,12.7090299003));
#94853=CARTESIAN_POINT('Ctrl Pts',(-8.64940616788,-23.1742356128,12.7782948442));
#94854=CARTESIAN_POINT('Ctrl Pts',(-8.58542217429,-23.1742356128,12.8474952237));
#94855=CARTESIAN_POINT('Ctrl Pts',(-8.71988917196,-23.4742356128,12.5632395809));
#94856=CARTESIAN_POINT('Ctrl Pts',(-8.72947215345,-23.3790967554,12.5721001887));
#94857=CARTESIAN_POINT('Ctrl Pts',(-8.71152123069,-23.285897088,12.6066774531));
#94858=CARTESIAN_POINT('Ctrl Pts',(-8.66821560358,-23.2117943285,12.6661101146));
#94859=CARTESIAN_POINT('Ctrl Pts',(-8.60980196734,-23.1742356128,12.7407571089));
#94860=CARTESIAN_POINT('Ctrl Pts',(-8.55126681507,-23.1742356128,12.8159145257));
#94861=CARTESIAN_POINT('Ctrl Pts',(-8.65068769611,-23.4557342571,12.4992545736));
#94862=CARTESIAN_POINT('Ctrl Pts',(-8.67114447119,-23.3616092561,12.5181692988));
#94863=CARTESIAN_POINT('Ctrl Pts',(-8.6616791149,-23.2705882254,12.5620766304));
#94864=CARTESIAN_POINT('Ctrl Pts',(-8.62409294795,-23.1983198307,12.6285650769));
#94865=CARTESIAN_POINT('Ctrl Pts',(-8.568611422,-23.16211697,12.707808508));
#94866=CARTESIAN_POINT('Ctrl Pts',(-8.51298776904,-23.1652660131,12.7860692819));
#94867=CARTESIAN_POINT('Ctrl Pts',(-8.58504814405,-23.4187037356,12.4385629891));
#94868=CARTESIAN_POINT('Ctrl Pts',(-8.61720687318,-23.3287980114,12.4682975647));
#94869=CARTESIAN_POINT('Ctrl Pts',(-8.61787660959,-23.2418003868,12.5228744536));
#94870=CARTESIAN_POINT('Ctrl Pts',(-8.58556282332,-23.1726965799,12.5981338043));
#94871=CARTESIAN_POINT('Ctrl Pts',(-8.53069999004,-23.1387145708,12.6814672949));
#94872=CARTESIAN_POINT('Ctrl Pts',(-8.47363957019,-23.1456118409,12.7605886079));
#94873=CARTESIAN_POINT('Ctrl Pts',(-8.46797276655,-23.3115821157,12.3303128573));
#94874=CARTESIAN_POINT('Ctrl Pts',(-8.52237213304,-23.2378310806,12.3806115513));
#94875=CARTESIAN_POINT('Ctrl Pts',(-8.54446981637,-23.1647358306,12.4578324878));
#94876=CARTESIAN_POINT('Ctrl Pts',(-8.52245288296,-23.1060736658,12.5529815994));
#94877=CARTESIAN_POINT('Ctrl Pts',(-8.46636077569,-23.0779179681,12.6438102103));
#94878=CARTESIAN_POINT('Ctrl Pts',(-8.40034769996,-23.089880852,12.7198837328));
#94879=CARTESIAN_POINT('Ctrl Pts',(-8.38931991359,-23.1521307593,12.2575889261));
#94880=CARTESIAN_POINT('Ctrl Pts',(-8.45970633708,-23.1061611813,12.3226695586));
#94881=CARTESIAN_POINT('Ctrl Pts',(-8.4993062219,-23.0588540528,12.4194802488));
#94882=CARTESIAN_POINT('Ctrl Pts',(-8.48540796624,-23.0202466991,12.5332516118));
#94883=CARTESIAN_POINT('Ctrl Pts',(-8.42613724507,-23.0015045278,12.6297956016));
#94884=CARTESIAN_POINT('Ctrl Pts',(-8.34720486119,-23.0113292253,12.6980018322));
#94885=CARTESIAN_POINT('Ctrl Pts',(-8.36213066678,-23.0627326652,12.2324492288));
#94886=CARTESIAN_POINT('Ctrl Pts',(-8.43792182062,-23.0327194928,12.3025271783));
#94887=CARTESIAN_POINT('Ctrl Pts',(-8.48363550117,-23.0005841899,12.4073998633));
#94888=CARTESIAN_POINT('Ctrl Pts',(-8.47259449573,-22.9739829087,12.5290848856));
#94889=CARTESIAN_POINT('Ctrl Pts',(-8.41152527253,-22.9610560938,12.6277894396));
#94890=CARTESIAN_POINT('Ctrl Pts',(-8.32640121972,-22.9690248134,12.6908033837));
#94891=CARTESIAN_POINT('Ctrl Pts',(-8.34854625295,-22.9684833924,12.2198888201));
#94892=CARTESIAN_POINT('Ctrl Pts',(-8.42693586094,-22.9542535279,12.29236935));
#94893=CARTESIAN_POINT('Ctrl Pts',(-8.47477476029,-22.9392158893,12.4011922791));
#94894=CARTESIAN_POINT('Ctrl Pts',(-8.46499990031,-22.9265127562,12.5267357874));
#94895=CARTESIAN_POINT('Ctrl Pts',(-8.40290084109,-22.9193127846,12.6268959398));
#94896=CARTESIAN_POINT('Ctrl Pts',(-8.31471092647,-22.9207536636,12.6874600337));
#94897=CARTESIAN_POINT('Ctrl Pts',(-8.34854625295,-22.8742356128,12.2198888201));
#94898=CARTESIAN_POINT('Ctrl Pts',(-8.4275605919,-22.8742356128,12.2929469882));
#94899=CARTESIAN_POINT('Ctrl Pts',(-8.47411942559,-22.8742356128,12.4014233916));
#94900=CARTESIAN_POINT('Ctrl Pts',(-8.4651120838,-22.8742356128,12.5258960706));
#94901=CARTESIAN_POINT('Ctrl Pts',(-8.40342053421,-22.8742356128,12.6265390425));
#94902=CARTESIAN_POINT('Ctrl Pts',(-8.31471092647,-22.8742356128,12.6874600337));
#94903=CARTESIAN_POINT('',(-8.58542217429,-23.1742356128,12.8474952237));
#94904=CARTESIAN_POINT('Ctrl Pts',(-8.31471092647,-22.8742356128,12.6874600337));
#94905=CARTESIAN_POINT('Ctrl Pts',(-8.31471092647,-22.9207536636,12.6874600337));
#94906=CARTESIAN_POINT('Ctrl Pts',(-8.32640121972,-22.9690248134,12.6908033837));
#94907=CARTESIAN_POINT('Ctrl Pts',(-8.34720486119,-23.0113292253,12.6980018322));
#94908=CARTESIAN_POINT('Ctrl Pts',(-8.40034769996,-23.089880852,12.7198837328));
#94909=CARTESIAN_POINT('Ctrl Pts',(-8.47363957019,-23.1456118409,12.7605886079));
#94910=CARTESIAN_POINT('Ctrl Pts',(-8.51298776904,-23.1652660131,12.7860692819));
#94911=CARTESIAN_POINT('Ctrl Pts',(-8.55126681507,-23.1742356128,12.8159145257));
#94912=CARTESIAN_POINT('Ctrl Pts',(-8.58542217429,-23.1742356128,12.8474952237));
#94913=CARTESIAN_POINT('Origin',(-8.58542217429,-23.4742356128,12.8474952237));
#94914=CARTESIAN_POINT('Origin',(-8.14487887576,-22.8742356128,12.4401604693));
#94915=CARTESIAN_POINT('',(-8.48454297717,-23.1742356128,12.9347595981));
#94916=CARTESIAN_POINT('Origin',(-8.48454297717,-22.8742356128,12.9347595981));
#94917=CARTESIAN_POINT('Origin',(-8.14487887576,-23.1742356128,12.4401604693));
#94918=CARTESIAN_POINT('Origin',(-1.05,-22.8742356128,14.92922515));
#94919=CARTESIAN_POINT('',(-1.09378792023,-23.1742356128,15.5276251985));
#94920=CARTESIAN_POINT('Origin',(-1.05,-23.1742356128,14.92922515));
#94921=CARTESIAN_POINT('Origin',(-1.09378792023,-22.8742356128,15.5276251985));
#94922=CARTESIAN_POINT('Origin',(2.71042223425E-15,-22.8742356128,0.580061096523));
#94923=CARTESIAN_POINT('Origin',(-3.80460715967E-16,-23.1742356128,0.580061096523));
#94924=CARTESIAN_POINT('Origin',(-8.21591479143,-23.4742356128,11.6886688365));
#94925=CARTESIAN_POINT('',(-7.85913400544,-23.1742356128,11.2062712093));
#94926=CARTESIAN_POINT('Origin',(-8.21591479143,-23.1742356128,11.6886688365));
#94927=CARTESIAN_POINT('Origin',(-7.85913400544,-23.4742356128,11.2062712093));
#94928=CARTESIAN_POINT('Origin',(-2.3120230745E-14,-23.4742356128,0.580061096523));
#94929=CARTESIAN_POINT('',(-8.48602987721,-23.1742356128,10.7126632105));
#94930=CARTESIAN_POINT('Origin',(8.85900795181E-16,-23.1742356128,0.580061096523));
#94931=CARTESIAN_POINT('Origin',(-8.48739188241962,-23.4721143216659,10.7142894999642));
#94932=CARTESIAN_POINT('Ctrl Pts',(-12.9732843937,-22.9031898545,8.97133867634));
#94933=CARTESIAN_POINT('Ctrl Pts',(-12.9781011914,-22.9849535816,8.94914145692));
#94934=CARTESIAN_POINT('Ctrl Pts',(-12.9535953066,-23.0667173088,8.92058122207));
#94935=CARTESIAN_POINT('Ctrl Pts',(-12.8986935104,-23.1346740075,8.88934991896));
#94936=CARTESIAN_POINT('Ctrl Pts',(-12.8237786321,-23.1759719524,8.86135389883));
#94937=CARTESIAN_POINT('Ctrl Pts',(-12.7426122303,-23.1887127298,8.84011906693));
#94938=CARTESIAN_POINT('Ctrl Pts',(-12.9823757633,-22.8915014019,8.92944287783));
#94939=CARTESIAN_POINT('Ctrl Pts',(-12.9862583246,-22.9763016188,8.91126726307));
#94940=CARTESIAN_POINT('Ctrl Pts',(-12.9595430587,-23.0611018356,8.88653324147));
#94941=CARTESIAN_POINT('Ctrl Pts',(-12.9012478152,-23.1309752745,8.85841244838));
#94942=CARTESIAN_POINT('Ctrl Pts',(-12.822883741,-23.172105454,8.83249977476));
#94943=CARTESIAN_POINT('Ctrl Pts',(-12.7392305459,-23.1828685028,8.81230742555));
#94944=CARTESIAN_POINT('Ctrl Pts',(-12.9914751666,-22.882822481,8.8868408148));
#94945=CARTESIAN_POINT('Ctrl Pts',(-12.9944056315,-22.9704026765,8.87289342313));
#94946=CARTESIAN_POINT('Ctrl Pts',(-12.9654027633,-23.0579828719,8.85218917069));
#94947=CARTESIAN_POINT('Ctrl Pts',(-12.9035898329,-23.1294730391,8.82727742946));
#94948=CARTESIAN_POINT('Ctrl Pts',(-12.8217308477,-23.1700741969,8.8033687928));
#94949=CARTESIAN_POINT('Ctrl Pts',(-12.7356821525,-23.1785290452,8.78399143876));
#94950=CARTESIAN_POINT('Ctrl Pts',(-13.000513389,-22.8770866751,8.84380834125));
#94951=CARTESIAN_POINT('Ctrl Pts',(-13.0024779758,-22.9671810863,8.834295766));
#94952=CARTESIAN_POINT('Ctrl Pts',(-12.9711165232,-23.0572754975,8.81782605389));
#94953=CARTESIAN_POINT('Ctrl Pts',(-12.9056733165,-23.1300795876,8.79620887499));
#94954=CARTESIAN_POINT('Ctrl Pts',(-12.820300204,-23.1698045819,8.77418794581));
#94955=CARTESIAN_POINT('Ctrl Pts',(-12.731982211,-23.1756611501,8.75535198255));
#94956=CARTESIAN_POINT('Ctrl Pts',(-13.0094376369,-22.8742356128,8.80057964365));
#94957=CARTESIAN_POINT('Ctrl Pts',(-13.0104250706,-22.9665621944,8.79571296462));
#94958=CARTESIAN_POINT('Ctrl Pts',(-12.97663939,-23.0588887759,8.78368803172));
#94959=CARTESIAN_POINT('Ctrl Pts',(-12.9074626588,-23.1326978759,8.76544020738));
#94960=CARTESIAN_POINT('Ctrl Pts',(-12.8185800084,-23.171217802,8.7451543519));
#94961=CARTESIAN_POINT('Ctrl Pts',(-12.728148167,-23.1742356128,8.7265439874));
#94962=CARTESIAN_POINT('Ctrl Pts',(-13.018207968,-22.8742356128,8.75735407375));
#94963=CARTESIAN_POINT('Ctrl Pts',(-13.018207968,-22.9684833924,8.75735407375));
#94964=CARTESIAN_POINT('Ctrl Pts',(-12.9819360276,-23.0627311721,8.74999461196));
#94965=CARTESIAN_POINT('Ctrl Pts',(-12.9089301686,-23.1372245963,8.73518195451));
#94966=CARTESIAN_POINT('Ctrl Pts',(-12.8165644307,-23.1742356128,8.71644123897));
#94967=CARTESIAN_POINT('Ctrl Pts',(-12.7241986928,-23.1742356128,8.69770052342));
#94968=CARTESIAN_POINT('',(-12.7426122126818,-23.1887126399569,8.84011909764617));
#94969=CARTESIAN_POINT('Origin',(-12.6820772987135,-22.9047704876882,8.9076975331626));
#94970=CARTESIAN_POINT('',(-12.7241986928,-23.1742356128,8.69770052342));
#94971=CARTESIAN_POINT('Origin',(-12.726277687684,-22.8763569532575,8.69812226440674));
#94972=CARTESIAN_POINT('Origin',(-12.6973454005032,-23.4896761342038,8.67085289361702));
#94973=CARTESIAN_POINT('Ctrl Pts',(-12.8222448424,-23.4742356815,9.46100292006));
#94974=CARTESIAN_POINT('Ctrl Pts',(-12.8494736832,-23.4742356636,9.39375104048));
#94975=CARTESIAN_POINT('Ctrl Pts',(-12.8563714436,-23.4742356458,9.31826754191));
#94976=CARTESIAN_POINT('Ctrl Pts',(-12.8394938336,-23.4742356301,9.24276446755));
#94977=CARTESIAN_POINT('Ctrl Pts',(-12.8011121316,-23.4742356188,9.17740252767));
#94978=CARTESIAN_POINT('Ctrl Pts',(-12.7478394439,-23.4742356125,9.1281455822));
#94979=CARTESIAN_POINT('Ctrl Pts',(-12.8222448265,-23.4046541603,9.4610029458));
#94980=CARTESIAN_POINT('Ctrl Pts',(-12.8494736715,-23.4136498524,9.39375106135));
#94981=CARTESIAN_POINT('Ctrl Pts',(-12.8563714358,-23.4226455445,9.31826755752));
#94982=CARTESIAN_POINT('Ctrl Pts',(-12.8394938286,-23.4305372305,9.24276447831));
#94983=CARTESIAN_POINT('Ctrl Pts',(-12.801112128,-23.4362628909,9.17740253498));
#94984=CARTESIAN_POINT('Ctrl Pts',(-12.7478394405,-23.4394448584,9.12814558784));
#94985=CARTESIAN_POINT('Ctrl Pts',(-12.8267376752,-23.3350444003,9.44989804488));
#94986=CARTESIAN_POINT('Ctrl Pts',(-12.8532287465,-23.3530402345,9.38369795688));
#94987=CARTESIAN_POINT('Ctrl Pts',(-12.8592761475,-23.3710360687,9.30931517965));
#94988=CARTESIAN_POINT('Ctrl Pts',(-12.8415116196,-23.3868230014,9.23486539817));
#94989=CARTESIAN_POINT('Ctrl Pts',(-12.8023354301,-23.3982761819,9.17041054742));
#94990=CARTESIAN_POINT('Ctrl Pts',(-12.7484601992,-23.4046400789,9.12185309334));
#94991=CARTESIAN_POINT('Ctrl Pts',(-12.8357660159,-23.2683909506,9.42765504858));
#94992=CARTESIAN_POINT('Ctrl Pts',(-12.8607726482,-23.2950473443,9.36356310571));
#94993=CARTESIAN_POINT('Ctrl Pts',(-12.8651123819,-23.3217037379,9.29138732719));
#94994=CARTESIAN_POINT('Ctrl Pts',(-12.8455698325,-23.3450683354,9.21904951484));
#94995=CARTESIAN_POINT('Ctrl Pts',(-12.8048034097,-23.3619761005,9.15641249749));
#94996=CARTESIAN_POINT('Ctrl Pts',(-12.7497239393,-23.3713130963,9.10925542748));
#94997=CARTESIAN_POINT('Ctrl Pts',(-12.8654176334,-23.1205674467,9.35093873948));
#94998=CARTESIAN_POINT('Ctrl Pts',(-12.8856609251,-23.1667016048,9.29404448239));
#94999=CARTESIAN_POINT('Ctrl Pts',(-12.88434645,-23.2128357629,9.22937157743));
#95000=CARTESIAN_POINT('Ctrl Pts',(-12.8587400955,-23.2531200257,9.16420855068));
#95001=CARTESIAN_POINT('Ctrl Pts',(-12.8124201304,-23.2819402616,9.10778516284));
#95002=CARTESIAN_POINT('Ctrl Pts',(-12.7530521925,-23.2974017916,9.06547349059));
#95003=CARTESIAN_POINT('Ctrl Pts',(-12.9068680488,-23.010101918,9.22909905079));
#95004=CARTESIAN_POINT('Ctrl Pts',(-12.9207907755,-23.0719215919,9.18344085273));
#95005=CARTESIAN_POINT('Ctrl Pts',(-12.9112658476,-23.1337412658,9.13042485238));
#95006=CARTESIAN_POINT('Ctrl Pts',(-12.8761980932,-23.187134812,9.07635129743));
#95007=CARTESIAN_POINT('Ctrl Pts',(-12.8208608743,-23.2240649689,9.02951363011));
#95008=CARTESIAN_POINT('Ctrl Pts',(-12.7544308643,-23.2421683956,8.99467312589));
#95009=CARTESIAN_POINT('Ctrl Pts',(-12.9314667335,-22.9612266295,9.14763068363));
#95010=CARTESIAN_POINT('Ctrl Pts',(-12.9418297489,-23.0307478118,9.10939417332));
#95011=CARTESIAN_POINT('Ctrl Pts',(-12.9272163182,-23.1002689941,9.06405821655));
#95012=CARTESIAN_POINT('Ctrl Pts',(-12.8858996435,-23.1597742276,9.01725069446));
#95013=CARTESIAN_POINT('Ctrl Pts',(-12.8244369644,-23.1997556874,8.97665312932));
#95014=CARTESIAN_POINT('Ctrl Pts',(-12.7531935733,-23.2177311451,8.94663366293));
#95015=CARTESIAN_POINT('Ctrl Pts',(-12.9538489501,-22.9261034781,9.0609030715));
#95016=CARTESIAN_POINT('Ctrl Pts',(-12.9611499959,-23.0022194475,9.03052977793));
#95017=CARTESIAN_POINT('Ctrl Pts',(-12.941507993,-23.078335417,8.99337186849));
#95018=CARTESIAN_POINT('Ctrl Pts',(-12.8935474744,-23.1426522193,8.95421942683));
#95019=CARTESIAN_POINT('Ctrl Pts',(-12.8254935651,-23.1840524297,8.91999612505));
#95020=CARTESIAN_POINT('Ctrl Pts',(-12.7492414901,-23.2001695455,8.89463935599));
#95021=CARTESIAN_POINT('Ctrl Pts',(-12.9732844032,-22.9031895891,8.9713386779));
#95022=CARTESIAN_POINT('Ctrl Pts',(-12.9781011912,-22.9849533577,8.94914147504));
#95023=CARTESIAN_POINT('Ctrl Pts',(-12.9535952945,-23.0667171263,8.92058125628));
#95024=CARTESIAN_POINT('Ctrl Pts',(-12.8986934857,-23.1346738584,8.88934996626));
#95025=CARTESIAN_POINT('Ctrl Pts',(-12.8237785974,-23.1759718213,8.86135395422));
#95026=CARTESIAN_POINT('Ctrl Pts',(-12.7426121901,-23.188712601,8.84011912524));
#95027=CARTESIAN_POINT('Ctrl Pts',(-12.7478394439013,-23.4742356125,9.12814558220122));
#95028=CARTESIAN_POINT('Ctrl Pts',(-12.7478394423705,-23.4585747866676,
9.12814558473974));
#95029=CARTESIAN_POINT('Ctrl Pts',(-12.7479941055707,-23.4430020566137,
9.12661399498703));
#95030=CARTESIAN_POINT('Ctrl Pts',(-12.7482793501886,-23.4277199381803,
9.12361011238638));
#95031=CARTESIAN_POINT('Ctrl Pts',(-12.7485863803035,-23.4112706512066,
9.12037680889192));
#95032=CARTESIAN_POINT('Ctrl Pts',(-12.7490439774559,-23.3951575737632,
9.11543863325741));
#95033=CARTESIAN_POINT('Ctrl Pts',(-12.7495774547234,-23.3795881719316,
9.10888164768596));
#95034=CARTESIAN_POINT('Ctrl Pts',(-12.7501402959479,-23.3631617902941,
9.10196374881271));
#95035=CARTESIAN_POINT('Ctrl Pts',(-12.7507868072288,-23.347340616678,9.09324434020817));
#95036=CARTESIAN_POINT('Ctrl Pts',(-12.7513935053284,-23.3323249264688,
9.0828266307671));
#95037=CARTESIAN_POINT('Ctrl Pts',(-12.7516567580278,-23.3258094602383,
9.07830627684944));
#95038=CARTESIAN_POINT('Ctrl Pts',(-12.7519121450063,-23.3194451133931,
9.07346616307184));
#95039=CARTESIAN_POINT('Ctrl Pts',(-12.7521482626982,-23.3132454913329,
9.06831467777211));
#95040=CARTESIAN_POINT('Ctrl Pts',(-12.7524122220315,-23.3063148454626,
9.06255575892657));
#95041=CARTESIAN_POINT('Ctrl Pts',(-12.7526520218503,-23.2995900663332,
9.05640783074764));
#95042=CARTESIAN_POINT('Ctrl Pts',(-12.7528502599117,-23.2930878600365,
9.04988322236555));
#95043=CARTESIAN_POINT('Ctrl Pts',(-12.7532355027692,-23.280451898429,9.03720372601321));
#95044=CARTESIAN_POINT('Ctrl Pts',(-12.7534629873913,-23.2686667930293,
9.02310682296249));
#95045=CARTESIAN_POINT('Ctrl Pts',(-12.7534091553356,-23.2578545455587,
9.00772645227283));
#95046=CARTESIAN_POINT('Ctrl Pts',(-12.7533534964837,-23.2466753834094,
8.99182414719493));
#95047=CARTESIAN_POINT('Ctrl Pts',(-12.7529967102063,-23.2365359417805,
8.97455013960297));
#95048=CARTESIAN_POINT('Ctrl Pts',(-12.7522140218396,-23.2275144867261,
8.95606210733663));
#95049=CARTESIAN_POINT('Ctrl Pts',(-12.7513879506109,-23.2179929903313,
8.93654932015219));
#95050=CARTESIAN_POINT('Ctrl Pts',(-12.7500865167735,-23.2097159112915,
8.91568541081658));
#95051=CARTESIAN_POINT('Ctrl Pts',(-12.7481861664673,-23.2027216494298,
8.89365486866089));
#95052=CARTESIAN_POINT('Ctrl Pts',(-12.7467056778765,-23.197272693596,8.87649173499866));
#95053=CARTESIAN_POINT('Ctrl Pts',(-12.7448619117108,-23.1926006117108,
8.85862103845975));
#95054=CARTESIAN_POINT('Ctrl Pts',(-12.7426122052017,-23.1887125986295,
8.84011912919091));
#95055=CARTESIAN_POINT('Origin',(-6.6707290414,-23.4742356128,3.1005467775));
#95056=CARTESIAN_POINT('',(-11.9421544921,-23.1742356128,7.97460750747));
#95057=CARTESIAN_POINT('',(-12.3331765925,-23.1742356128,8.33615401544));
#95058=CARTESIAN_POINT('Origin',(-11.9407143760008,-23.4721143158025,7.97616506106996));
#95059=CARTESIAN_POINT('Ctrl Pts',(-3.81744045688,-22.8742356128,-9.21387212773));
#95060=CARTESIAN_POINT('Ctrl Pts',(-3.81744045688,-22.9684833924,-9.21387212773));
#95061=CARTESIAN_POINT('Ctrl Pts',(-3.80220506528,-23.0627311721,-9.18014234586));
#95062=CARTESIAN_POINT('Ctrl Pts',(-3.77154023633,-23.1372245963,-9.11225318231));
#95063=CARTESIAN_POINT('Ctrl Pts',(-3.73274363021,-23.1742356128,-9.02636099807));
#95064=CARTESIAN_POINT('Ctrl Pts',(-3.69394702409,-23.1742356128,-8.94046881382));
#95065=CARTESIAN_POINT('Ctrl Pts',(-3.71160470889,-22.8742356128,-9.26167703413));
#95066=CARTESIAN_POINT('Ctrl Pts',(-3.72515638761,-22.9642074605,-9.25555588183));
#95067=CARTESIAN_POINT('Ctrl Pts',(-3.7250970863,-23.0541793081,-9.21865622161));
#95068=CARTESIAN_POINT('Ctrl Pts',(-3.70844285493,-23.1271496569,-9.15193510136));
#95069=CARTESIAN_POINT('Ctrl Pts',(-3.67843010495,-23.1675189946,-9.06966143177));
#95070=CARTESIAN_POINT('Ctrl Pts',(-3.64200986566,-23.1742356128,-8.98738776219));
#95071=CARTESIAN_POINT('Ctrl Pts',(-3.60518947181,-22.8967702026,-9.30860522068));
#95072=CARTESIAN_POINT('Ctrl Pts',(-3.63104913481,-22.9796757788,-9.29721692608));
#95073=CARTESIAN_POINT('Ctrl Pts',(-3.64474315,-23.0625813551,-9.25775017492));
#95074=CARTESIAN_POINT('Ctrl Pts',(-3.64141126432,-23.131420749,-9.19204052568));
#95075=CARTESIAN_POINT('Ctrl Pts',(-3.62129881914,-23.1730680404,-9.11274337915));
#95076=CARTESIAN_POINT('Ctrl Pts',(-3.58978817426,-23.1855028319,-9.03344623294));
#95077=CARTESIAN_POINT('Ctrl Pts',(-3.50276689342,-22.9419634255,-9.35255588844));
#95078=CARTESIAN_POINT('Ctrl Pts',(-3.53957219131,-23.0156863099,-9.33675316789));
#95079=CARTESIAN_POINT('Ctrl Pts',(-3.56543990858,-23.0894091943,-9.29523917398));
#95080=CARTESIAN_POINT('Ctrl Pts',(-3.57431565494,-23.1517903264,-9.2303724476));
#95081=CARTESIAN_POINT('Ctrl Pts',(-3.56438630978,-23.1921341626,-9.15347743429));
#95082=CARTESIAN_POINT('Ctrl Pts',(-3.53952573637,-23.2081001313,-9.07658241785));
#95083=CARTESIAN_POINT('Ctrl Pts',(-3.34853990601,-23.0590627588,-9.41717252271));
#95084=CARTESIAN_POINT('Ctrl Pts',(-3.40101481294,-23.1138397009,-9.39536923091));
#95085=CARTESIAN_POINT('Ctrl Pts',(-3.44422712818,-23.1686166429,-9.35116723508));
#95086=CARTESIAN_POINT('Ctrl Pts',(-3.47088045966,-23.2161685094,-9.28743732801));
#95087=CARTESIAN_POINT('Ctrl Pts',(-3.47682492232,-23.2495777226,-9.21371939274));
#95088=CARTESIAN_POINT('Ctrl Pts',(-3.4638420321,-23.2666487717,-9.14000145959));
#95089=CARTESIAN_POINT('Ctrl Pts',(-3.24903060406,-23.2324009559,-9.45772855228));
#95090=CARTESIAN_POINT('Ctrl Pts',(-3.31106586193,-23.2635682408,-9.43250094395));
#95091=CARTESIAN_POINT('Ctrl Pts',(-3.36479660614,-23.2947355258,-9.38683384758));
#95092=CARTESIAN_POINT('Ctrl Pts',(-3.40250113652,-23.322122922,-9.32374506153));
#95093=CARTESIAN_POINT('Ctrl Pts',(-3.41904507547,-23.3420909713,-9.25177549042));
#95094=CARTESIAN_POINT('Ctrl Pts',(-3.41500902577,-23.3533185645,-9.17980591789));
#95095=CARTESIAN_POINT('Ctrl Pts',(-3.22037852073,-23.3101536719,-9.46927274181));
#95096=CARTESIAN_POINT('Ctrl Pts',(-3.28511942878,-23.331162522,-9.44310189027));
#95097=CARTESIAN_POINT('Ctrl Pts',(-3.34181908965,-23.3521713721,-9.39703707137));
#95098=CARTESIAN_POINT('Ctrl Pts',(-3.38266593906,-23.3706950509,-9.33412380265));
#95099=CARTESIAN_POINT('Ctrl Pts',(-3.40228901679,-23.384336583,-9.2626299648));
#95100=CARTESIAN_POINT('Ctrl Pts',(-3.40094883361,-23.3921942807,-9.19113612813));
#95101=CARTESIAN_POINT('Ctrl Pts',(-3.2061108834,-23.3922234913,-9.47502541989));
#95102=CARTESIAN_POINT('Ctrl Pts',(-3.27219964976,-23.4027249383,-9.44838409371));
#95103=CARTESIAN_POINT('Ctrl Pts',(-3.33037855145,-23.4132263854,-9.4021208728));
#95104=CARTESIAN_POINT('Ctrl Pts',(-3.37279084839,-23.422485337,-9.33929519246));
#95105=CARTESIAN_POINT('Ctrl Pts',(-3.393947035,-23.4293033961,-9.26803870195));
#95106=CARTESIAN_POINT('Ctrl Pts',(-3.39394702816,-23.4332296702,-9.19678221123));
#95107=CARTESIAN_POINT('Ctrl Pts',(-3.20611087388,-23.4742356128,-9.47502544833));
#95108=CARTESIAN_POINT('Ctrl Pts',(-3.27219964627,-23.4742356465,-9.44838411889));
#95109=CARTESIAN_POINT('Ctrl Pts',(-3.33037855462,-23.4742356801,-9.40212089616));
#95110=CARTESIAN_POINT('Ctrl Pts',(-3.37279085872,-23.4742357098,-9.33929521563));
#95111=CARTESIAN_POINT('Ctrl Pts',(-3.39394705252,-23.4742357316,-9.26803872592));
#95112=CARTESIAN_POINT('Ctrl Pts',(-3.39394705213,-23.4742357442,-9.19678223621));
#95113=CARTESIAN_POINT('',(-3.69394702409,-23.1742356128,-8.94046881382));
#95114=CARTESIAN_POINT('Origin',(-3.69482026935181,-22.8763568962883,-8.94240201772957));
#95115=CARTESIAN_POINT('Ctrl Pts',(-3.69394702409,-23.1742356128,-8.94046881382));
#95116=CARTESIAN_POINT('Ctrl Pts',(-3.67899884906695,-23.1742356128,-8.95397268413816));
#95117=CARTESIAN_POINT('Ctrl Pts',(-3.66455031612627,-23.175353499792,-8.96691364760397));
#95118=CARTESIAN_POINT('Ctrl Pts',(-3.65070330540787,-23.1773700763482,
-8.97922431578443));
#95119=CARTESIAN_POINT('Ctrl Pts',(-3.63641423969004,-23.1794510305355,
-8.99192799242906));
#95120=CARTESIAN_POINT('Ctrl Pts',(-3.62276587287881,-23.1824896811564,
-9.0039606699122));
#95121=CARTESIAN_POINT('Ctrl Pts',(-3.60983308751173,-23.1862642542778,
-9.01528450778334));
#95122=CARTESIAN_POINT('Ctrl Pts',(-3.59620581883196,-23.1902415198566,
-9.02721642939002));
#95123=CARTESIAN_POINT('Ctrl Pts',(-3.58337317073403,-23.1950359774261,
-9.03836150991428));
#95124=CARTESIAN_POINT('Ctrl Pts',(-3.5713794826881,-23.2004026426052,-9.04871270075273));
#95125=CARTESIAN_POINT('Ctrl Pts',(-3.55873745080754,-23.2060594140692,
-9.05962344681185));
#95126=CARTESIAN_POINT('Ctrl Pts',(-3.54702870580604,-23.2123510615671,
-9.0696513765444));
#95127=CARTESIAN_POINT('Ctrl Pts',(-3.53625798419655,-23.2190072933907,
-9.07882473415894));
#95128=CARTESIAN_POINT('Ctrl Pts',(-3.52548726258705,-23.2256635252143,
-9.08799809177348));
#95129=CARTESIAN_POINT('Ctrl Pts',(-3.51565445515374,-23.2326833770868,
-9.09631707780529));
#95130=CARTESIAN_POINT('Ctrl Pts',(-3.50671897808822,-23.2398231608574,
-9.1038423601356));
#95131=CARTESIAN_POINT('Ctrl Pts',(-3.50370542903012,-23.242231100411,-9.10638031164196));
#95132=CARTESIAN_POINT('Ctrl Pts',(-3.50079412602067,-23.2446525516423,
-9.1088296778814));
#95133=CARTESIAN_POINT('Ctrl Pts',(-3.49798326952153,-23.2470782891206,
-9.11119791470152));
#95134=CARTESIAN_POINT('Ctrl Pts',(-3.49657784127196,-23.2482911578598,
-9.11238203311158));
#95135=CARTESIAN_POINT('Ctrl Pts',(-3.49553564848842,-23.249208117903,-9.11325991246051));
#95136=CARTESIAN_POINT('Ctrl Pts',(-3.49434510622956,-23.2502694936275,
-9.11426032900786));
#95137=CARTESIAN_POINT('Ctrl Pts',(-3.4932901731775,-23.2512099729124,-9.11514679269596));
#95138=CARTESIAN_POINT('Ctrl Pts',(-3.49211846283781,-23.2522635690391,
-9.11612972241234));
#95139=CARTESIAN_POINT('Ctrl Pts',(-3.49049264692078,-23.2537643261086,
-9.11749010669963));
#95140=CARTESIAN_POINT('Ctrl Pts',(-3.4902836520405,-23.253957244963,-9.11766498095708));
#95141=CARTESIAN_POINT('Ctrl Pts',(-3.49006718960407,-23.2541576045751,
-9.11784605897054));
#95142=CARTESIAN_POINT('Ctrl Pts',(-3.489842580416,-23.2543661668826,-9.11803390325523));
#95143=CARTESIAN_POINT('Ctrl Pts',(-3.47856184707405,-23.264840964448,-9.12746816239441));
#95144=CARTESIAN_POINT('Ctrl Pts',(-3.46818823610973,-23.2760891770451,
-9.13608324636035));
#95145=CARTESIAN_POINT('Ctrl Pts',(-3.4587908077671,-23.2879520814553,-9.14385003815369));
#95146=CARTESIAN_POINT('Ctrl Pts',(-3.44763144110507,-23.3020391800917,
-9.15307303770734));
#95147=CARTESIAN_POINT('Ctrl Pts',(-3.43785049160989,-23.3169954292007,
-9.16109877651924));
#95148=CARTESIAN_POINT('Ctrl Pts',(-3.42952044756393,-23.3325442547886,
-9.16790677016603));
#95149=CARTESIAN_POINT('Ctrl Pts',(-3.42150473969357,-23.3475063417778,
-9.17445786256781));
#95150=CARTESIAN_POINT('Ctrl Pts',(-3.41483311376225,-23.363015262272,-9.17988102525593));
#95151=CARTESIAN_POINT('Ctrl Pts',(-3.40953111081634,-23.3788158559842,
-9.18418102289095));
#95152=CARTESIAN_POINT('Ctrl Pts',(-3.40427986614197,-23.3944651840644,
-9.18843985486654));
#95153=CARTESIAN_POINT('Ctrl Pts',(-3.40037230162103,-23.4104000145971,
-9.19159685104193));
#95154=CARTESIAN_POINT('Ctrl Pts',(-3.3977890626441,-23.4263809625103,-9.19368246110308));
#95155=CARTESIAN_POINT('Ctrl Pts',(-3.39520582366718,-23.4423619104235,
-9.19576807116422));
#95156=CARTESIAN_POINT('Ctrl Pts',(-3.3939470498033,-23.4583889758006,-9.19678222096313));
#95157=CARTESIAN_POINT('Ctrl Pts',(-3.39394705212995,-23.4742356127999,
-9.1967822362099));
#95158=CARTESIAN_POINT('Origin',(-3.69394702409,-23.4742356128,3.39628270998));
#95159=CARTESIAN_POINT('',(-3.69394702409,-23.1742356128,-8.44362980932));
#95160=CARTESIAN_POINT('Ctrl Pts',(-9.06991786197,-22.8742351711,13.3798726472));
#95161=CARTESIAN_POINT('Ctrl Pts',(-9.06991791346,-22.9684830268,13.3798726085));
#95162=CARTESIAN_POINT('Ctrl Pts',(-9.04851963512,-23.0627308825,13.3496744364));
#95163=CARTESIAN_POINT('Ctrl Pts',(-9.00545047601,-23.1372243637,13.2888935201));
#95164=CARTESIAN_POINT('Ctrl Pts',(-8.95096009845,-23.1742354012,13.2119945921));
#95165=CARTESIAN_POINT('Ctrl Pts',(-8.89646970336,-23.1742353894,13.1350956831));
#95166=CARTESIAN_POINT('Ctrl Pts',(-9.22406041417,-22.8742363569,13.2706476151));
#95167=CARTESIAN_POINT('Ctrl Pts',(-9.20132424908,-22.9647386701,13.2867584141));
#95168=CARTESIAN_POINT('Ctrl Pts',(-9.15852680885,-23.0552409834,13.275328887));
#95169=CARTESIAN_POINT('Ctrl Pts',(-9.10021479707,-23.128400233,13.232683254));
#95170=CARTESIAN_POINT('Ctrl Pts',(-9.0393710411,-23.168352818,13.1677082076));
#95171=CARTESIAN_POINT('Ctrl Pts',(-8.986120014,-23.1742360128,13.0945214235));
#95172=CARTESIAN_POINT('Ctrl Pts',(-9.3768173424,-22.9427255764,13.1589191215));
#95173=CARTESIAN_POINT('Ctrl Pts',(-9.33383370545,-23.019699187,13.1904054535));
#95174=CARTESIAN_POINT('Ctrl Pts',(-9.27188264132,-23.0966727976,13.1965141601));
#95175=CARTESIAN_POINT('Ctrl Pts',(-9.19881019143,-23.1602830893,13.1710975036));
#95176=CARTESIAN_POINT('Ctrl Pts',(-9.1296041316,-23.1981089887,13.1188723071));
#95177=CARTESIAN_POINT('Ctrl Pts',(-9.07411181992,-23.2084805514,13.051815332));
#95178=CARTESIAN_POINT('Ctrl Pts',(-9.5056235281,-23.0835945845,13.0599834668));
#95179=CARTESIAN_POINT('Ctrl Pts',(-9.44694848687,-23.1391655975,13.1046059873));
#95180=CARTESIAN_POINT('Ctrl Pts',(-9.36995382261,-23.1947366105,13.1251829804));
#95181=CARTESIAN_POINT('Ctrl Pts',(-9.2844923694,-23.2410848235,13.113878162));
#95182=CARTESIAN_POINT('Ctrl Pts',(-9.20688851793,-23.2696054116,13.0728111063));
#95183=CARTESIAN_POINT('Ctrl Pts',(-9.14715364651,-23.2789180606,13.0124182766));
#95184=CARTESIAN_POINT('Ctrl Pts',(-9.57074430825,-23.2789184576,13.0098414435));
#95185=CARTESIAN_POINT('Ctrl Pts',(-9.50407307406,-23.3067030636,13.0611772932));
#95186=CARTESIAN_POINT('Ctrl Pts',(-9.41940322383,-23.3344876695,13.0891378612));
#95187=CARTESIAN_POINT('Ctrl Pts',(-9.32764499777,-23.3576610293,13.0850021715));
#95188=CARTESIAN_POINT('Ctrl Pts',(-9.2458338001,-23.3719208617,13.049538037));
#95189=CARTESIAN_POINT('Ctrl Pts',(-9.18405109086,-23.3765770352,12.9924125631));
#95190=CARTESIAN_POINT('Ctrl Pts',(-9.57074430825,-23.4742356128,13.0098414435));
#95191=CARTESIAN_POINT('Ctrl Pts',(-9.50407307406,-23.4742356128,13.0611772932));
#95192=CARTESIAN_POINT('Ctrl Pts',(-9.41940322382,-23.4742356128,13.0891378611));
#95193=CARTESIAN_POINT('Ctrl Pts',(-9.32764499778,-23.4742356128,13.0850021715));
#95194=CARTESIAN_POINT('Ctrl Pts',(-9.2458338001,-23.4742356128,13.049538037));
#95195=CARTESIAN_POINT('Ctrl Pts',(-9.18405109086,-23.4742356128,12.9924125631));
#95196=CARTESIAN_POINT('',(-8.89646969686788,-23.17423555695,13.1350956958597));
#95197=CARTESIAN_POINT('Origin',(-8.89769520903801,-22.8763558982741,13.1368257591445));
#95198=CARTESIAN_POINT('Ctrl Pts',(-8.89646970862946,-23.1742353894,13.1350956905365));
#95199=CARTESIAN_POINT('Ctrl Pts',(-8.91309680047625,-23.1742355049141,
13.1275705378248));
#95200=CARTESIAN_POINT('Ctrl Pts',(-8.92916239855924,-23.1756511702746,
13.120179101675));
#95201=CARTESIAN_POINT('Ctrl Pts',(-8.94451183302731,-23.1782464117074,
13.1130138149001));
#95202=CARTESIAN_POINT('Ctrl Pts',(-8.95958315050042,-23.1807946298606,
13.1059783562325));
#95203=CARTESIAN_POINT('Ctrl Pts',(-8.97396381020449,-23.1844790085148,
13.0991617725664));
#95204=CARTESIAN_POINT('Ctrl Pts',(-8.98755390972639,-23.189062385306,13.0926394475502));
#95205=CARTESIAN_POINT('Ctrl Pts',(-8.99701199211221,-23.1922522041315,
13.0881002101994));
#95206=CARTESIAN_POINT('Ctrl Pts',(-9.00608818080905,-23.1958771858743,
13.0837031896146));
#95207=CARTESIAN_POINT('Ctrl Pts',(-9.01476254474212,-23.1998570495597,
13.079467854496));
#95208=CARTESIAN_POINT('Ctrl Pts',(-9.027482024044,-23.2056928427269,13.0732574559246));
#95209=CARTESIAN_POINT('Ctrl Pts',(-9.03934274711023,-23.212293430192,13.0673924478358));
#95210=CARTESIAN_POINT('Ctrl Pts',(-9.05033294399465,-23.2194260101855,
13.0619070683858));
#95211=CARTESIAN_POINT('Ctrl Pts',(-9.05395907702327,-23.2217793514555,
13.0600972085801));
#95212=CARTESIAN_POINT('Ctrl Pts',(-9.05749078373108,-23.2241907687581,
13.0583284758369));
#95213=CARTESIAN_POINT('Ctrl Pts',(-9.06092859580915,-23.2266524199078,
13.0566015206519));
#95214=CARTESIAN_POINT('Ctrl Pts',(-9.06785721579022,-23.2316136699572,
13.0531209882874));
#95215=CARTESIAN_POINT('Ctrl Pts',(-9.07440401191121,-23.2367786623744,
13.0498105322997));
#95216=CARTESIAN_POINT('Ctrl Pts',(-9.08059335916827,-23.2420847942466,
13.0466889651196));
#95217=CARTESIAN_POINT('Ctrl Pts',(-9.0836880327968,-23.2447378601827,13.0451281815295));
#95218=CARTESIAN_POINT('Ctrl Pts',(-9.08668953155372,-23.247426726068,13.0436101398472));
#95219=CARTESIAN_POINT('Ctrl Pts',(-9.08959773920902,-23.2501447149073,
13.0421324470578));
#95220=CARTESIAN_POINT('Ctrl Pts',(-9.09117417163362,-23.2516180367067,
13.0413314441367));
#95221=CARTESIAN_POINT('Ctrl Pts',(-9.09249083656084,-23.2528771175428,
13.0406611989853));
#95222=CARTESIAN_POINT('Ctrl Pts',(-9.09392855283527,-23.2542797644668,
13.0399269440846));
#95223=CARTESIAN_POINT('Ctrl Pts',(-9.09514314021191,-23.2554647251424,
13.0393066431604));
#95224=CARTESIAN_POINT('Ctrl Pts',(-9.09644407818803,-23.2567523375043,
13.0386406609476));
#95225=CARTESIAN_POINT('Ctrl Pts',(-9.09804347097728,-23.2583792358661,
13.037819360047));
#95226=CARTESIAN_POINT('Ctrl Pts',(-9.11048146896409,-23.2710311364403,
13.0314323492911));
#95227=CARTESIAN_POINT('Ctrl Pts',(-9.12170996655921,-23.284815934694,13.0255917484038));
#95228=CARTESIAN_POINT('Ctrl Pts',(-9.13160827419955,-23.2994894912599,
13.0204003640024));
#95229=CARTESIAN_POINT('Ctrl Pts',(-9.14140778591686,-23.3140165897021,
13.0152607952883));
#95230=CARTESIAN_POINT('Ctrl Pts',(-9.14990355505978,-23.3294146670775,
13.0107577262315));
#95231=CARTESIAN_POINT('Ctrl Pts',(-9.15701840945915,-23.3454289145785,
13.0069645198718));
#95232=CARTESIAN_POINT('Ctrl Pts',(-9.16410040151333,-23.3613691948975,
13.0031888337099));
#95233=CARTESIAN_POINT('Ctrl Pts',(-9.16981423379896,-23.377919961051,13.0001165870717));
#95234=CARTESIAN_POINT('Ctrl Pts',(-9.17412316825768,-23.3948130306609,
12.9977916560662));
#95235=CARTESIAN_POINT('Ctrl Pts',(-9.17839082006171,-23.4115442526573,
12.9954889995522));
#95236=CARTESIAN_POINT('Ctrl Pts',(-9.18128041821572,-23.4286113244906,
12.9939194681916));
#95237=CARTESIAN_POINT('Ctrl Pts',(-9.18279429024485,-23.4457365917114,
12.9930964360048));
#95238=CARTESIAN_POINT('Ctrl Pts',(-9.18363397469894,-23.4552352946272,
12.9926399328664));
#95239=CARTESIAN_POINT('Ctrl Pts',(-9.18405109086,-23.4647515930551,12.9924125631));
#95240=CARTESIAN_POINT('Ctrl Pts',(-9.18405109086,-23.4742356128,12.9924125631));
#95241=CARTESIAN_POINT('Origin',(-6.6707290414,-23.4742356128,11.0771333555));
#95242=CARTESIAN_POINT('',(-8.74094594938,-23.1742356128,12.9912954789));
#95243=CARTESIAN_POINT('Origin',(2.84607155346,-22.8742356128,5.53854202767));
#95244=CARTESIAN_POINT('Origin',(2.84607155346,-23.1742356128,5.53854202767));
#95245=CARTESIAN_POINT('Origin',(4.58869751468E-17,-22.8742356128,0.580061096523));
#95246=CARTESIAN_POINT('Origin',(-7.30083966106E-16,-23.1742356128,0.580061096523));
#95247=CARTESIAN_POINT('Origin',(-3.23631964477E-15,-23.0742356128,-4.23765442876));
#95248=CARTESIAN_POINT('',(0.153073372946,-23.1742356128,-4.17424936164));
#95249=CARTESIAN_POINT('Origin',(0.153073372946,-23.0742356128,-4.17424936164));
#95250=CARTESIAN_POINT('',(3.35920145722,-23.1742356128,-2.84622762644));
#95251=CARTESIAN_POINT('',(1.75613741508,-23.1742356128,-3.51023849404));
#95252=CARTESIAN_POINT('Origin',(3.35920145722,-23.0742356128,-2.84622762644));
#95253=CARTESIAN_POINT('Origin',(-2.06825793744E-15,-23.0742356128,5.69655897044));
#95254=CARTESIAN_POINT('',(0.153073372946,-23.1742356128,5.63315390332));
#95255=CARTESIAN_POINT('',(1.7388152851,-23.1742356128,4.97631809688));
#95256=CARTESIAN_POINT('Origin',(0.153073372946,-23.0742356128,5.63315390332));
#95257=CARTESIAN_POINT('Origin',(3.81389112164,-23.0742356128,3.51356095948));
#95258=CARTESIAN_POINT('',(4.23969076488,-23.1742356128,2.48558968592));
#95259=CARTESIAN_POINT('Origin',(6.12032227755,-23.0742356128,3.51356095948));
#95260=CARTESIAN_POINT('',(3.57567989727,-23.1742356128,-2.62974918638));
#95261=CARTESIAN_POINT('Origin',(3.57567989727,-23.0742356128,-2.62974918638));
#95262=CARTESIAN_POINT('',(4.23277615087,-23.1742356128,-1.04337849916));
#95263=CARTESIAN_POINT('Origin',(3.20612808427,-23.0742356128,-2.47667581343));
#95264=CARTESIAN_POINT('Origin',(3.20612808427,-23.1742356128,-2.47667581343));
#95265=CARTESIAN_POINT('Origin',(1.12255033962E-15,-23.0742356128,-3.80469754864));
#95266=CARTESIAN_POINT('',(-0.153073372946,-23.1742356128,-4.17424936164));
#95267=CARTESIAN_POINT('Origin',(-0.153073372946,-23.0742356128,-4.17424936164));
#95268=CARTESIAN_POINT('Origin',(1.11225582468E-15,-23.1742356128,-3.80469754864));
#95269=CARTESIAN_POINT('Origin',(-1.45996280537E-15,-23.0742356128,-4.23765442876));
#95270=CARTESIAN_POINT('',(-3.35920145722,-23.1742356128,-2.84622762644));
#95271=CARTESIAN_POINT('Origin',(-3.35920145722,-23.0742356128,-2.84622762644));
#95272=CARTESIAN_POINT('',(-1.75613741508,-23.1742356128,-3.51023849404));
#95273=CARTESIAN_POINT('Origin',(-1.5436783271E-16,-23.0742356128,5.26360209032));
#95274=CARTESIAN_POINT('',(-0.153073372946,-23.1742356128,5.63315390332));
#95275=CARTESIAN_POINT('Origin',(-2.77636603164E-16,-23.1742356128,5.26360209032));
#95276=CARTESIAN_POINT('Origin',(-0.153073372946,-23.0742356128,5.63315390332));
#95277=CARTESIAN_POINT('Origin',(-2.06825793744E-15,-23.0742356128,5.69655897044));
#95278=CARTESIAN_POINT('',(-1.7388152851,-23.1742356128,4.97631809688));
#95279=CARTESIAN_POINT('Origin',(-3.81389112164,-23.0742356128,3.51356095948));
#95280=CARTESIAN_POINT('',(-4.23969076488,-23.1742356128,2.48558968592));
#95281=CARTESIAN_POINT('Origin',(-6.12032227755,-23.0742356128,3.51356095948));
#95282=CARTESIAN_POINT('',(-3.57567989727,-23.1742356128,-2.62974918638));
#95283=CARTESIAN_POINT('',(-4.23277615087,-23.1742356128,-1.04337849916));
#95284=CARTESIAN_POINT('Origin',(-3.57567989727,-23.0742356128,-2.62974918638));
#95285=CARTESIAN_POINT('Origin',(-3.20612808427,-23.0742356128,-2.47667581343));
#95286=CARTESIAN_POINT('Origin',(-3.20612808427,-23.1742356128,-2.47667581343));
#95287=CARTESIAN_POINT('Origin',(0.,-23.1742356128,0.729452270839));
#95288=CARTESIAN_POINT('',(-6.06355150788,-23.1742356128,8.47279340685));
#95289=CARTESIAN_POINT('',(-6.6707290414,-23.1742356128,9.03420135995));
#95290=CARTESIAN_POINT('',(-5.99440665492,-23.1742356128,7.66760345225));
#95291=CARTESIAN_POINT('Origin',(-6.47088626226,-23.1742356128,8.03225010833));
#95292=CARTESIAN_POINT('',(-7.50515696478,-23.1742356128,3.88262115182));
#95293=CARTESIAN_POINT('Origin',(-0.00234331738835,-23.1742356128,3.08191746407));
#95294=CARTESIAN_POINT('',(-8.10176909975,-23.1742356128,3.34629187045));
#95295=CARTESIAN_POINT('Origin',(-8.10176909975,-23.1742356128,3.94629187045));
#95296=CARTESIAN_POINT('',(-11.4530804658,-23.1742356128,3.34629187045));
#95297=CARTESIAN_POINT('',(-6.6707290414,-23.1742356128,3.34629187045));
#95298=CARTESIAN_POINT('',(-12.0493948734,-23.1742356128,3.87989061057));
#95299=CARTESIAN_POINT('Origin',(-11.4530804658,-23.1742356128,3.94629187045));
#95300=CARTESIAN_POINT('Origin',(2.84607155346,-23.1742356128,5.53854202767));
#95301=CARTESIAN_POINT('Origin',(-10.1862176145,-22.8742356128,9.72278707155));
#95302=CARTESIAN_POINT('',(-10.9304145503,-22.8742356128,10.3907473403));
#95303=CARTESIAN_POINT('',(-11.1383462684,-22.8742356128,10.0284846777));
#95304=CARTESIAN_POINT('Origin',(-10.1862176145,-22.8742356128,9.72278707155));
#95305=CARTESIAN_POINT('Ctrl Pts',(-10.9304145503437,-22.8742356128,10.3907473403392));
#95306=CARTESIAN_POINT('Ctrl Pts',(-10.9481405479233,-22.8882672659973,
10.3709982119854));
#95307=CARTESIAN_POINT('Ctrl Pts',(-10.9645717766644,-22.9013026990597,
10.3525880372788));
#95308=CARTESIAN_POINT('Ctrl Pts',(-10.9810103536057,-22.9142753573368,
10.3340804995609));
#95309=CARTESIAN_POINT('Ctrl Pts',(-10.992000443497,-22.9229482905903,10.3217071959644));
#95310=CARTESIAN_POINT('Ctrl Pts',(-11.002992272732,-22.9315950772944,10.3092917362859));
#95311=CARTESIAN_POINT('Ctrl Pts',(-11.0143770648586,-22.9404798718002,
10.2963873039649));
#95312=CARTESIAN_POINT('Ctrl Pts',(-11.0200212309283,-22.944884629931,10.2899897555297));
#95313=CARTESIAN_POINT('Ctrl Pts',(-11.0257621179678,-22.9493475068719,
10.2834716325873));
#95314=CARTESIAN_POINT('Ctrl Pts',(-11.031648508022,-22.9538972342928,10.2767748704144));
#95315=CARTESIAN_POINT('Ctrl Pts',(-11.138346268408,-22.8742356128,10.0284846777026));
#95316=CARTESIAN_POINT('Ctrl Pts',(-11.1304025349713,-22.8879754443996,
10.0532263049571));
#95317=CARTESIAN_POINT('Ctrl Pts',(-11.1227115500163,-22.9011602400043,
10.0769601464436));
#95318=CARTESIAN_POINT('Ctrl Pts',(-11.1149362788915,-22.9142785484054,
10.1007522253721));
#95319=CARTESIAN_POINT('Ctrl Pts',(-11.1089402979403,-22.9243948679554,
10.1190997337428));
#95320=CARTESIAN_POINT('Ctrl Pts',(-11.1028949842124,-22.9344737618983,
10.1374798306995));
#95321=CARTESIAN_POINT('Ctrl Pts',(-11.0966317645807,-22.9447233863069,
10.1563922783035));
#95322=CARTESIAN_POINT('Ctrl Pts',(-11.0947731720942,-22.947764932993,10.1620044929607));
#95323=CARTESIAN_POINT('Ctrl Pts',(-11.0928952369663,-22.9508212969781,
10.1676637551768));
#95324=CARTESIAN_POINT('Ctrl Pts',(-11.090993057621,-22.9538972342935,10.1733836478105));
#95325=CARTESIAN_POINT('Ctrl Pts',(-11.9005548436,-23.1693861532,7.89557218486));
#95326=CARTESIAN_POINT('Ctrl Pts',(-11.8339499555,-23.1595472711,7.96980237474));
#95327=CARTESIAN_POINT('Ctrl Pts',(-11.7599452826,-23.1908783468,8.04284981847));
#95328=CARTESIAN_POINT('Ctrl Pts',(-11.6942870876,-23.2663663442,8.09701806802));
#95329=CARTESIAN_POINT('Ctrl Pts',(-11.6548578916,-23.3654515188,8.11755397837));
#95330=CARTESIAN_POINT('Ctrl Pts',(-11.6438378503,-23.4645366935,8.10736463748));
#95331=CARTESIAN_POINT('Ctrl Pts',(-11.8668157199,-23.1614761236,7.83132058431));
#95332=CARTESIAN_POINT('Ctrl Pts',(-11.8129234492,-23.1460753827,7.92069454621));
#95333=CARTESIAN_POINT('Ctrl Pts',(-11.7451516804,-23.1734640687,8.00787961054));
#95334=CARTESIAN_POINT('Ctrl Pts',(-11.6772007057,-23.2482114783,8.07033400293));
#95335=CARTESIAN_POINT('Ctrl Pts',(-11.6288782137,-23.3484640563,8.08997448939));
#95336=CARTESIAN_POINT('Ctrl Pts',(-11.6054955414,-23.4487166343,8.07191260584));
#95337=CARTESIAN_POINT('Ctrl Pts',(-11.8201190291,-23.1436931675,7.77911937176));
#95338=CARTESIAN_POINT('Ctrl Pts',(-11.7896480761,-23.1271929291,7.88233980762));
#95339=CARTESIAN_POINT('Ctrl Pts',(-11.7361184989,-23.1516755686,7.98200912796));
#95340=CARTESIAN_POINT('Ctrl Pts',(-11.6667987778,-23.2222222498,8.05091722103));
#95341=CARTESIAN_POINT('Ctrl Pts',(-11.6024958012,-23.3176864267,8.06826984747));
#95342=CARTESIAN_POINT('Ctrl Pts',(-11.5554237252,-23.4131506081,8.04186749464));
#95343=CARTESIAN_POINT('Ctrl Pts',(-11.7752729456,-23.1083028984,7.76843597189));
#95344=CARTESIAN_POINT('Ctrl Pts',(-11.7595402729,-23.1052304081,7.86585583205));
#95345=CARTESIAN_POINT('Ctrl Pts',(-11.7167014673,-23.1327309513,7.95914759566));
#95346=CARTESIAN_POINT('Ctrl Pts',(-11.6496136328,-23.1915820263,8.02617572742));
#95347=CARTESIAN_POINT('Ctrl Pts',(-11.5756983226,-23.2669761984,8.04953640203));
#95348=CARTESIAN_POINT('Ctrl Pts',(-11.5102889752,-23.3423703627,8.03319245204));
#95349=CARTESIAN_POINT('Ctrl Pts',(-11.717675025,-23.0445100599,7.76252036052));
#95350=CARTESIAN_POINT('Ctrl Pts',(-11.7084114695,-23.0501289834,7.8515782493));
#95351=CARTESIAN_POINT('Ctrl Pts',(-11.6708968566,-23.0738598269,7.93631728547));
#95352=CARTESIAN_POINT('Ctrl Pts',(-11.6066799831,-23.1148476696,8.0001560579));
#95353=CARTESIAN_POINT('Ctrl Pts',(-11.5292674801,-23.1648160129,8.02969505599));
#95354=CARTESIAN_POINT('Ctrl Pts',(-11.4529027709,-23.2147843626,8.02583184946));
#95355=CARTESIAN_POINT('Ctrl Pts',(-11.6840057838,-22.9724912879,7.77196745159));
#95356=CARTESIAN_POINT('Ctrl Pts',(-11.6739934323,-22.9791841994,7.85280062059));
#95357=CARTESIAN_POINT('Ctrl Pts',(-11.6374046012,-22.9945001244,7.92955173236));
#95358=CARTESIAN_POINT('Ctrl Pts',(-11.575491188,-23.017355905,7.98966707089));
#95359=CARTESIAN_POINT('Ctrl Pts',(-11.4989860406,-23.044051495,8.02274251311));
#95360=CARTESIAN_POINT('Ctrl Pts',(-11.4203500465,-23.0707470797,8.02802946276));
#95361=CARTESIAN_POINT('Ctrl Pts',(-11.674734675,-22.9402340389,7.77528500471));
#95362=CARTESIAN_POINT('Ctrl Pts',(-11.6632751245,-22.9448939304,7.85395206414));
#95363=CARTESIAN_POINT('Ctrl Pts',(-11.6261291027,-22.9551888401,7.92866239052));
#95364=CARTESIAN_POINT('Ctrl Pts',(-11.5648099781,-22.9704904338,7.98774399745));
#95365=CARTESIAN_POINT('Ctrl Pts',(-11.4893943947,-22.9883613924,8.02148806052));
#95366=CARTESIAN_POINT('Ctrl Pts',(-11.4114432261,-23.0062323557,8.02896986926));
#95367=CARTESIAN_POINT('Ctrl Pts',(-11.6698654776,-22.907226316,7.77708988832));
#95368=CARTESIAN_POINT('Ctrl Pts',(-11.6579204713,-22.9095613324,7.85454768026));
#95369=CARTESIAN_POINT('Ctrl Pts',(-11.6206811584,-22.914710848,7.92810475864));
#95370=CARTESIAN_POINT('Ctrl Pts',(-11.5596933648,-22.9223583919,7.98661599137));
#95371=CARTESIAN_POINT('Ctrl Pts',(-11.4846565636,-22.931287768,8.02077577683));
#95372=CARTESIAN_POINT('Ctrl Pts',(-11.4067703651,-22.9402171391,8.02950137053));
#95373=CARTESIAN_POINT('Ctrl Pts',(-11.6698655273,-22.8742356121,7.77708987718));
#95374=CARTESIAN_POINT('Ctrl Pts',(-11.6579205194,-22.8742356226,7.85454767439));
#95375=CARTESIAN_POINT('Ctrl Pts',(-11.6206812044,-22.8742356357,7.92810475784));
#95376=CARTESIAN_POINT('Ctrl Pts',(-11.5596934089,-22.87423565,7.98661599254));
#95377=CARTESIAN_POINT('Ctrl Pts',(-11.4846566078,-22.8742356631,8.02077577467));
#95378=CARTESIAN_POINT('Ctrl Pts',(-11.4067704135,-22.8742356736,8.02950136067));
#95379=CARTESIAN_POINT('',(-11.9005548348204,-23.1693861585525,7.895572186247));
#95380=CARTESIAN_POINT('Ctrl Pts',(-11.6438378503,-23.4645366935,8.10736463748));
#95381=CARTESIAN_POINT('Ctrl Pts',(-11.6457407548972,-23.4474269895683,
8.10912409945425));
#95382=CARTESIAN_POINT('Ctrl Pts',(-11.6486630325428,-23.4303180321677,
8.10978091601121));
#95383=CARTESIAN_POINT('Ctrl Pts',(-11.65256298317,-23.4134680180269,8.10932257821117));
#95384=CARTESIAN_POINT('Ctrl Pts',(-11.6565377789634,-23.3962946300209,
8.10885544430778));
#95385=CARTESIAN_POINT('Ctrl Pts',(-11.6615279369715,-23.37939060852,8.10723006852047));
#95386=CARTESIAN_POINT('Ctrl Pts',(-11.6674552116862,-23.3630165572466,
8.10447292972245));
#95387=CARTESIAN_POINT('Ctrl Pts',(-11.6735237627704,-23.3462522310777,
8.10165007462501));
#95388=CARTESIAN_POINT('Ctrl Pts',(-11.6805744213503,-23.3300439067293,
8.09764098964143));
#95389=CARTESIAN_POINT('Ctrl Pts',(-11.6884909237533,-23.3146514397464,
8.09251343822578));
#95390=CARTESIAN_POINT('Ctrl Pts',(-11.6964815336893,-23.2991148816364,
8.0873378870539));
#95391=CARTESIAN_POINT('Ctrl Pts',(-11.7053539547591,-23.2844099860543,
8.08102307394607));
#95392=CARTESIAN_POINT('Ctrl Pts',(-11.7149602963441,-23.2707770127254,
8.073675339938));
#95393=CARTESIAN_POINT('Ctrl Pts',(-11.7245993021421,-23.2570976835241,
8.06630262160609));
#95394=CARTESIAN_POINT('Ctrl Pts',(-11.7349768686908,-23.2444980259262,
8.05789023480772));
#95395=CARTESIAN_POINT('Ctrl Pts',(-11.745920364852,-23.2331869359498,8.04857827595082));
#95396=CARTESIAN_POINT('Ctrl Pts',(-11.756829296706,-23.2219115713012,8.03929572829864));
#95397=CARTESIAN_POINT('Ctrl Pts',(-11.7683002094792,-23.2119170519958,
8.02911960219298));
#95398=CARTESIAN_POINT('Ctrl Pts',(-11.7801446348235,-23.2033704216458,
8.01821646048037));
#95399=CARTESIAN_POINT('Ctrl Pts',(-11.7918096503827,-23.1949532487468,
8.00747847074888));
#95400=CARTESIAN_POINT('Ctrl Pts',(-11.8038365705567,-23.1879407235758,
7.99603566767177));
#95401=CARTESIAN_POINT('Ctrl Pts',(-11.8160340495087,-23.1824486649995,
7.98406915540297));
#95402=CARTESIAN_POINT('Ctrl Pts',(-11.8280723255703,-23.1770282893999,
7.97225883142102));
#95403=CARTESIAN_POINT('Ctrl Pts',(-11.840276398251,-23.1730892198954,7.95993868610934));
#95404=CARTESIAN_POINT('Ctrl Pts',(-11.8524564888357,-23.1706957080467,
7.94729963439745));
#95405=CARTESIAN_POINT('Ctrl Pts',(-11.8643709607006,-23.1683543929817,
7.93493621025267));
#95406=CARTESIAN_POINT('Ctrl Pts',(-11.8762621855935,-23.1674921212114,
7.92226792528629));
#95407=CARTESIAN_POINT('Ctrl Pts',(-11.8879515998144,-23.1681206308898,
7.90948528184542));
#95408=CARTESIAN_POINT('Ctrl Pts',(-11.892181889249,-23.1683480826509,7.90485936300359));
#95409=CARTESIAN_POINT('Ctrl Pts',(-11.8963857612096,-23.1687702957837,
7.90021856034556));
#95410=CARTESIAN_POINT('Ctrl Pts',(-11.9005548359276,-23.1693861518639,
7.89557218635399));
#95411=CARTESIAN_POINT('',(-11.6698655452447,-22.8742356128,7.77708987356263));
#95412=CARTESIAN_POINT('Ctrl Pts',(-11.6698655273,-22.8742356128,7.77708987718));
#95413=CARTESIAN_POINT('Ctrl Pts',(-11.6698655124336,-22.8841203453796,
7.77708988050861));
#95414=CARTESIAN_POINT('Ctrl Pts',(-11.6703872773143,-22.8945390468658,
7.77689324751285));
#95415=CARTESIAN_POINT('Ctrl Pts',(-11.6715891474942,-22.9054209100778,
7.7764658141757));
#95416=CARTESIAN_POINT('Ctrl Pts',(-11.6718882682496,-22.908129181902,7.7763594348139));
#95417=CARTESIAN_POINT('Ctrl Pts',(-11.6722296873662,-22.910866176731,7.77623891315925));
#95418=CARTESIAN_POINT('Ctrl Pts',(-11.6726162016286,-22.9136308753537,
7.77610410993981));
#95419=CARTESIAN_POINT('Ctrl Pts',(-11.6728244048813,-22.9151201328075,
7.77603149562384));
#95420=CARTESIAN_POINT('Ctrl Pts',(-11.6730453375116,-22.9166151485335,
7.77595486411559));
#95421=CARTESIAN_POINT('Ctrl Pts',(-11.6732805949692,-22.9181230332283,
7.77587382906681));
#95422=CARTESIAN_POINT('Ctrl Pts',(-11.674145482278,-22.9236665358625,7.77557591636307));
#95423=CARTESIAN_POINT('Ctrl Pts',(-11.6752247585291,-22.9294892000468,
7.77521098652493));
#95424=CARTESIAN_POINT('Ctrl Pts',(-11.6765188200825,-22.9353811920076,
7.77479159710103));
#95425=CARTESIAN_POINT('Ctrl Pts',(-11.6777949650932,-22.9411916081532,
7.77437801420816));
#95426=CARTESIAN_POINT('Ctrl Pts',(-11.6792803566587,-22.9470693851126,
7.77391183617433));
#95427=CARTESIAN_POINT('Ctrl Pts',(-11.6809271617018,-22.9528173364117,
7.77342261518714));
#95428=CARTESIAN_POINT('Ctrl Pts',(-11.6822016511858,-22.9572657703755,
7.77304399902602));
#95429=CARTESIAN_POINT('Ctrl Pts',(-11.6835717755419,-22.9616365225724,
7.77265209353309));
#95430=CARTESIAN_POINT('Ctrl Pts',(-11.6849943332863,-22.9658401362469,
7.7722646214258));
#95431=CARTESIAN_POINT('Ctrl Pts',(-11.6869904334254,-22.9717385497725,
7.77172092952276));
#95432=CARTESIAN_POINT('Ctrl Pts',(-11.6891111912027,-22.9774017432891,
7.77119600464548));
#95433=CARTESIAN_POINT('Ctrl Pts',(-11.6914115443287,-22.9830234104527,
7.77067661915821));
#95434=CARTESIAN_POINT('Ctrl Pts',(-11.6936439591363,-22.9884790480577,
7.77017257313175));
#95435=CARTESIAN_POINT('Ctrl Pts',(-11.6960457876511,-22.993895771449,7.76967272729939));
#95436=CARTESIAN_POINT('Ctrl Pts',(-11.6987131473567,-22.9994417956824,
7.76916948557355));
#95437=CARTESIAN_POINT('Ctrl Pts',(-11.700426214222,-23.0030036363776,7.76884628704733));
#95438=CARTESIAN_POINT('Ctrl Pts',(-11.7022496933578,-23.0066186583115,
7.76852175128625));
#95439=CARTESIAN_POINT('Ctrl Pts',(-11.7042191449779,-23.0103284488021,
7.76819851840486));
#95440=CARTESIAN_POINT('Ctrl Pts',(-11.7083171006155,-23.0180476314926,
7.76752594843917));
#95441=CARTESIAN_POINT('Ctrl Pts',(-11.7126643864249,-23.025476754061,7.76701456578987));
#95442=CARTESIAN_POINT('Ctrl Pts',(-11.7172052293534,-23.032615071251,7.76669876886871));
#95443=CARTESIAN_POINT('Ctrl Pts',(-11.7177627166421,-23.0334914550323,
7.76665999792417));
#95444=CARTESIAN_POINT('Ctrl Pts',(-11.7183231854258,-23.0343635452706,
7.76662416222729));
#95445=CARTESIAN_POINT('Ctrl Pts',(-11.7188864419448,-23.0352312083239,
7.76659140543157));
#95446=CARTESIAN_POINT('Ctrl Pts',(-11.7198925864243,-23.0367811138495,
7.76653289200462));
#95447=CARTESIAN_POINT('Ctrl Pts',(-11.7209076421493,-23.0383169059184,
7.7664841882737));
#95448=CARTESIAN_POINT('Ctrl Pts',(-11.7219315119051,-23.0398385808136,
7.76644546906638));
#95449=CARTESIAN_POINT('Ctrl Pts',(-11.7223273569165,-23.0404268855398,
7.76643049957931));
#95450=CARTESIAN_POINT('Ctrl Pts',(-11.72272451719,-23.041013078508,7.76641702418818));
#95451=CARTESIAN_POINT('Ctrl Pts',(-11.7231229790036,-23.0415971536289,
7.76640505882331));
#95452=CARTESIAN_POINT('Ctrl Pts',(-11.7234037527934,-23.0420087187517,
7.76639662749884));
#95453=CARTESIAN_POINT('Ctrl Pts',(-11.7236851727353,-23.0424192322473,
7.76638894600219));
#95454=CARTESIAN_POINT('Ctrl Pts',(-11.7239672327341,-23.042828691091,7.76638202072213));
#95455=CARTESIAN_POINT('Ctrl Pts',(-11.7241736706056,-23.0431283713454,
7.76637695215487));
#95456=CARTESIAN_POINT('Ctrl Pts',(-11.7243799312776,-23.0434267115443,
7.76637230938042));
#95457=CARTESIAN_POINT('Ctrl Pts',(-11.7245799519957,-23.043715051258,7.76636818977289));
#95458=CARTESIAN_POINT('Ctrl Pts',(-11.7257206878381,-23.045359478142,7.7663446952869));
#95459=CARTESIAN_POINT('Ctrl Pts',(-11.7267188556241,-23.0467712679517,
7.76633475147523));
#95460=CARTESIAN_POINT('Ctrl Pts',(-11.7278501756133,-23.0483433079471,
7.76633514799306));
#95461=CARTESIAN_POINT('Ctrl Pts',(-11.7288494912053,-23.0497319195634,
7.76633549824449));
#95462=CARTESIAN_POINT('Ctrl Pts',(-11.7299524098615,-23.0512456217772,
7.76634351678061));
#95463=CARTESIAN_POINT('Ctrl Pts',(-11.7313750775217,-23.0531480387012,
7.76637596130601));
#95464=CARTESIAN_POINT('Ctrl Pts',(-11.7373284520788,-23.0611089988252,
7.76651173047928));
#95465=CARTESIAN_POINT('Ctrl Pts',(-11.7434317507374,-23.0685194797057,
7.76705223096266));
#95466=CARTESIAN_POINT('Ctrl Pts',(-11.7495966028089,-23.0754143832906,
7.76800907885379));
#95467=CARTESIAN_POINT('Ctrl Pts',(-11.7555268124262,-23.0820468576914,
7.76892950784386));
#95468=CARTESIAN_POINT('Ctrl Pts',(-11.7615104447489,-23.088199390884,7.77023684976931));
#95469=CARTESIAN_POINT('Ctrl Pts',(-11.7674655798331,-23.0938978810723,
7.77190303623388));
#95470=CARTESIAN_POINT('Ctrl Pts',(-11.7687515475446,-23.0951284282023,
7.77226283697134));
#95471=CARTESIAN_POINT('Ctrl Pts',(-11.770036266467,-23.0963378510776,7.77263919924583));
#95472=CARTESIAN_POINT('Ctrl Pts',(-11.7713190725072,-23.0975265031653,
7.7730315672446));
#95473=CARTESIAN_POINT('Ctrl Pts',(-11.7780184940438,-23.1037342081074,
7.77508069902199));
#95474=CARTESIAN_POINT('Ctrl Pts',(-11.7846643103656,-23.1093783289844,
7.77758924145152));
#95475=CARTESIAN_POINT('Ctrl Pts',(-11.791166992,-23.1145134944792,7.78054542587794));
#95476=CARTESIAN_POINT('Ctrl Pts',(-11.7944183328172,-23.1170810772266,
7.78202351809116));
#95477=CARTESIAN_POINT('Ctrl Pts',(-11.7976341986518,-23.1195214885636,
7.7836135664346));
#95478=CARTESIAN_POINT('Ctrl Pts',(-11.8008050898331,-23.1218418377442,
7.78531434295865));
#95479=CARTESIAN_POINT('Ctrl Pts',(-11.8022440127623,-23.122894792087,7.78608614060103));
#95480=CARTESIAN_POINT('Ctrl Pts',(-11.8034616587886,-23.1237701018227,
7.78676260102076));
#95481=CARTESIAN_POINT('Ctrl Pts',(-11.8047441929008,-23.1246798089907,
7.78749652651521));
#95482=CARTESIAN_POINT('Ctrl Pts',(-11.8059201430297,-23.1255139156638,
7.78816945971175));
#95483=CARTESIAN_POINT('Ctrl Pts',(-11.8071508091656,-23.1263770130773,
7.78889062389471));
#95484=CARTESIAN_POINT('Ctrl Pts',(-11.8086641746866,-23.1274176790227,
7.78981460459052));
#95485=CARTESIAN_POINT('Ctrl Pts',(-11.8091374815276,-23.1277431485171,
7.79010358063638));
#95486=CARTESIAN_POINT('Ctrl Pts',(-11.8096384931628,-23.1280858563205,
7.79041271122205));
#95487=CARTESIAN_POINT('Ctrl Pts',(-11.8101743388709,-23.1284499143557,
7.7907477664464));
#95488=CARTESIAN_POINT('Ctrl Pts',(-11.8201336553098,-23.1352163568592,
7.79697515793818));
#95489=CARTESIAN_POINT('Ctrl Pts',(-11.8299458768997,-23.141070908697,7.8045010798013));
#95490=CARTESIAN_POINT('Ctrl Pts',(-11.8395088976496,-23.1461218781324,
7.81333714787196));
#95491=CARTESIAN_POINT('Ctrl Pts',(-11.8490941108826,-23.1511845691311,
7.82219372141846));
#95492=CARTESIAN_POINT('Ctrl Pts',(-11.8584352736138,-23.1554412136267,
7.8323669370134));
#95493=CARTESIAN_POINT('Ctrl Pts',(-11.8674423905467,-23.1589852725995,
7.84387767342908));
#95494=CARTESIAN_POINT('Ctrl Pts',(-11.8733075965803,-23.1612930738889,
7.85137317295236));
#95495=CARTESIAN_POINT('Ctrl Pts',(-11.8790314091254,-23.1632979472643,
7.8594372001096));
#95496=CARTESIAN_POINT('Ctrl Pts',(-11.8845698557022,-23.1650229769109,
7.86806183689275));
#95497=CARTESIAN_POINT('Ctrl Pts',(-11.8894630610363,-23.1665470367987,
7.87568168446672));
#95498=CARTESIAN_POINT('Ctrl Pts',(-11.8942119030766,-23.1678521919875,
7.88374041620657));
#95499=CARTESIAN_POINT('Ctrl Pts',(-11.8987644056655,-23.1689586903633,
7.89220348632107));
#95500=CARTESIAN_POINT('Ctrl Pts',(-11.8993647202297,-23.1691045984824,
7.89331946685021));
#95501=CARTESIAN_POINT('Ctrl Pts',(-11.8999615824553,-23.1692470654513,
7.89444241478444));
#95502=CARTESIAN_POINT('Ctrl Pts',(-11.9005548359869,-23.1693861518727,
7.89557218628791));
#95503=CARTESIAN_POINT('Origin',(-11.3748953755427,-22.8742356445387,7.7329560039236));
#95504=CARTESIAN_POINT('Ctrl Pts',(-11.9421544921,-23.1742356128,7.97460750747));
#95505=CARTESIAN_POINT('Ctrl Pts',(-11.8781704985,-23.1742356128,8.04380788698));
#95506=CARTESIAN_POINT('Ctrl Pts',(-11.8141865049,-23.2112466293,8.11300826649));
#95507=CARTESIAN_POINT('Ctrl Pts',(-11.7636135705,-23.2857400536,8.16770423124));
#95508=CARTESIAN_POINT('Ctrl Pts',(-11.7384871149,-23.3799878332,8.19487915673));
#95509=CARTESIAN_POINT('Ctrl Pts',(-11.7384871149,-23.4742356128,8.19487915673));
#95510=CARTESIAN_POINT('Ctrl Pts',(-11.9338050766,-23.1742356128,7.95878179633));
#95511=CARTESIAN_POINT('Ctrl Pts',(-11.8690129979,-23.1723658919,8.02885614127));
#95512=CARTESIAN_POINT('Ctrl Pts',(-11.8029049395,-23.2084420454,8.09871370492));
#95513=CARTESIAN_POINT('Ctrl Pts',(-11.7493954495,-23.283359451,8.15328464759));
#95514=CARTESIAN_POINT('Ctrl Pts',(-11.7215525483,-23.3787975319,8.17922113275));
#95515=CARTESIAN_POINT('Ctrl Pts',(-11.7194707712,-23.4742356128,8.17729628178));
#95516=CARTESIAN_POINT('Ctrl Pts',(-11.925456866,-23.1737486504,7.94293960289));
#95517=CARTESIAN_POINT('Ctrl Pts',(-11.8599896787,-23.169946111,8.01395123592));
#95518=CARTESIAN_POINT('Ctrl Pts',(-11.7918088017,-23.204981018,8.08451905773));
#95519=CARTESIAN_POINT('Ctrl Pts',(-11.7353200262,-23.2802129884,8.13897414048));
#95520=CARTESIAN_POINT('Ctrl Pts',(-11.704689803,-23.37673734,8.16362951651));
#95521=CARTESIAN_POINT('Ctrl Pts',(-11.7004667677,-23.4732616915,8.15972481694));
#95522=CARTESIAN_POINT('Ctrl Pts',(-11.9171250584,-23.1727778426,7.92710974195));
#95523=CARTESIAN_POINT('Ctrl Pts',(-11.8511250917,-23.166992891,7.99912450114));
#95524=CARTESIAN_POINT('Ctrl Pts',(-11.7809316294,-23.2008856654,8.07045852272));
#95525=CARTESIAN_POINT('Ctrl Pts',(-11.721423774,-23.276320039,8.12480753543));
#95526=CARTESIAN_POINT('Ctrl Pts',(-11.6879347422,-23.3738200593,8.14813746342));
#95527=CARTESIAN_POINT('Ctrl Pts',(-11.6815098074,-23.471320079,8.14219684908));
#95528=CARTESIAN_POINT('Ctrl Pts',(-11.9088198181,-23.171323915,7.91131175397));
#95529=CARTESIAN_POINT('Ctrl Pts',(-11.8424378979,-23.1635210449,7.98439851249));
#95530=CARTESIAN_POINT('Ctrl Pts',(-11.7703001202,-23.1961765665,8.0565580465));
#95531=CARTESIAN_POINT('Ctrl Pts',(-11.7077347865,-23.2716977713,8.11081129139));
#95532=CARTESIAN_POINT('Ctrl Pts',(-11.6713131361,-23.3700549965,8.13276881012));
#95533=CARTESIAN_POINT('Ctrl Pts',(-11.6626231066,-23.4684122213,8.12473384452));
#95534=CARTESIAN_POINT('Ctrl Pts',(-11.9005548343,-23.1693861722,7.89557218484));
#95535=CARTESIAN_POINT('Ctrl Pts',(-11.8339499495,-23.1595472906,7.96980237485));
#95536=CARTESIAN_POINT('Ctrl Pts',(-11.7599452801,-23.1908783692,8.04284981853));
#95537=CARTESIAN_POINT('Ctrl Pts',(-11.6942870876,-23.2663663719,8.09701806797));
#95538=CARTESIAN_POINT('Ctrl Pts',(-11.6548578924,-23.3654515527,8.11755397832));
#95539=CARTESIAN_POINT('Ctrl Pts',(-11.6438378503,-23.4645367334,8.10736463748));
#95540=CARTESIAN_POINT('Origin',(-11.9551818975745,-22.3491879643317,7.96775954099132));
#95541=CARTESIAN_POINT('Origin',(2.84607155346,-22.8742356128,5.53854202767));
#95542=CARTESIAN_POINT('',(-11.7512376696,-22.8742356128,3.91309124051));
#95543=CARTESIAN_POINT('Origin',(-12.0493948734,-22.8742356128,3.87989061057));
#95544=CARTESIAN_POINT('Origin',(2.84607155346,-22.8742356128,5.53854202767));
#95545=CARTESIAN_POINT('Origin',(-11.4530804658,-22.8742356128,3.94629187045));
#95546=CARTESIAN_POINT('',(-11.4530804658,-22.8742356128,3.64629187045));
#95547=CARTESIAN_POINT('Origin',(-11.4530804658,-22.8742356128,3.34629187045));
#95548=CARTESIAN_POINT('Origin',(-11.4530804658,-22.8742356128,3.94629187045));
#95549=CARTESIAN_POINT('Origin',(-6.6707290414,-22.8742356128,3.34629187045));
#95550=CARTESIAN_POINT('',(-8.10176909975,-22.8742356128,3.64629187045));
#95551=CARTESIAN_POINT('Origin',(-8.10176909975,-22.8742356128,3.34629187045));
#95552=CARTESIAN_POINT('',(-9.77742478279,-22.8742356128,3.64629187045));
#95553=CARTESIAN_POINT('Origin',(-8.10176909975,-22.8742356128,3.94629187045));
#95554=CARTESIAN_POINT('',(-7.80346303227,-22.8742356128,3.91445651114));
#95555=CARTESIAN_POINT('Origin',(-7.50515696478,-22.8742356128,3.88262115182));
#95556=CARTESIAN_POINT('Origin',(-8.10176909975,-22.8742356128,3.94629187045));
#95557=CARTESIAN_POINT('Origin',(-0.00234331738835,-22.8742356128,3.08191746407));
#95558=CARTESIAN_POINT('',(-6.23264645859,-22.8742356128,7.84992678029));
#95559=CARTESIAN_POINT('Origin',(-5.99440665492,-22.8742356128,7.66760345225));
#95560=CARTESIAN_POINT('Origin',(-0.00234331738835,-22.8742356128,3.08191746407));
#95561=CARTESIAN_POINT('Origin',(-6.47088626226,-22.8742356128,8.03225010833));
#95562=CARTESIAN_POINT('',(-6.26721888507,-22.8742356128,8.25252175759));
#95563=CARTESIAN_POINT('Origin',(-6.06355150788,-22.8742356128,8.47279340685));
#95564=CARTESIAN_POINT('Origin',(-6.47088626226,-22.8742356128,8.03225010833));
#95565=CARTESIAN_POINT('Ctrl Pts',(-8.73611662316,-23.4697910609,10.8942571942));
#95566=CARTESIAN_POINT('Ctrl Pts',(-8.72752432309,-23.3771104598,10.9015348722));
#95567=CARTESIAN_POINT('Ctrl Pts',(-8.69545860941,-23.2844298587,10.881098933));
#95568=CARTESIAN_POINT('Ctrl Pts',(-8.6413960311,-23.2107990757,10.8311116668));
#95569=CARTESIAN_POINT('Ctrl Pts',(-8.57793853593,-23.1733813929,10.7632250691));
#95570=CARTESIAN_POINT('Ctrl Pts',(-8.51747666777,-23.1720133445,10.6920986219));
#95571=CARTESIAN_POINT('Ctrl Pts',(-8.72470175689,-23.4715681133,10.9039255852));
#95572=CARTESIAN_POINT('Ctrl Pts',(-8.7177987489,-23.3784476295,10.9097561006));
#95573=CARTESIAN_POINT('Ctrl Pts',(-8.68736831632,-23.2853271458,10.8877470417));
#95574=CARTESIAN_POINT('Ctrl Pts',(-8.63454393537,-23.211417996,10.8363489167));
#95575=CARTESIAN_POINT('Ctrl Pts',(-8.57168882428,-23.1740163051,10.7675887259));
#95576=CARTESIAN_POINT('Ctrl Pts',(-8.51124350946,-23.1729018671,10.696222277));
#95577=CARTESIAN_POINT('Ctrl Pts',(-8.71323427675,-23.4729019084,10.9136114204));
#95578=CARTESIAN_POINT('Ctrl Pts',(-8.70803661002,-23.3794040149,10.9179891886));
#95579=CARTESIAN_POINT('Ctrl Pts',(-8.67925545718,-23.2859061213,10.8943982297));
#95580=CARTESIAN_POINT('Ctrl Pts',(-8.62767478659,-23.2117711836,10.8415808992));
#95581=CARTESIAN_POINT('Ctrl Pts',(-8.5654164258,-23.1744185718,10.771945772));
#95582=CARTESIAN_POINT('Ctrl Pts',(-8.50497501432,-23.1735687617,10.7003455662));
#95583=CARTESIAN_POINT('Ctrl Pts',(-8.70172748022,-23.4737911951,10.9233030613));
#95584=CARTESIAN_POINT('Ctrl Pts',(-8.69824977302,-23.3799791247,10.9262239001));
#95585=CARTESIAN_POINT('Ctrl Pts',(-8.67113050266,-23.2861670544,10.9010437414));
#95586=CARTESIAN_POINT('Ctrl Pts',(-8.62079773014,-23.2118592846,10.8468003207));
#95587=CARTESIAN_POINT('Ctrl Pts',(-8.55912932234,-23.1745884938,10.7762902146));
#95588=CARTESIAN_POINT('Ctrl Pts',(-8.49867834935,-23.1740134037,10.7044634205));
#95589=CARTESIAN_POINT('Ctrl Pts',(-8.69019480669,-23.4742356128,10.9329890024));
#95590=CARTESIAN_POINT('Ctrl Pts',(-8.68845018412,-23.3801733377,10.9344501196));
#95591=CARTESIAN_POINT('Ctrl Pts',(-8.66300395829,-23.2861110626,10.9076749542));
#95592=CARTESIAN_POINT('Ctrl Pts',(-8.61392194556,-23.2116837148,10.8520000359));
#95593=CARTESIAN_POINT('Ctrl Pts',(-8.55283556198,-23.1745270026,10.7806162216));
#95594=CARTESIAN_POINT('Ctrl Pts',(-8.49236081888,-23.1742356128,10.7085709021));
#95595=CARTESIAN_POINT('Ctrl Pts',(-8.67864985337,-23.4742356128,10.942657873));
#95596=CARTESIAN_POINT('Ctrl Pts',(-8.67864985337,-23.3799878332,10.942657873));
#95597=CARTESIAN_POINT('Ctrl Pts',(-8.65488631632,-23.2857400536,10.9142834188));
#95598=CARTESIAN_POINT('Ctrl Pts',(-8.60705657762,-23.2112466293,10.8571731189));
#95599=CARTESIAN_POINT('Ctrl Pts',(-8.54654322741,-23.1742356128,10.7849181647));
#95600=CARTESIAN_POINT('Ctrl Pts',(-8.48602987721,-23.1742356128,10.7126632105));
#95601=CARTESIAN_POINT('',(-8.51747674095254,-23.1720132750395,10.6920985878956));
#95602=CARTESIAN_POINT('Origin',(-8.46564327939413,-22.8727019153709,10.6937226627841));
#95603=CARTESIAN_POINT('Origin',(-8.54339070302529,-23.4677320541598,10.6671045573098));
#95604=CARTESIAN_POINT('Ctrl Pts',(-8.73611663424,-23.4697908757,10.8942572059));
#95605=CARTESIAN_POINT('Ctrl Pts',(-8.72752435034,-23.3771103023,10.9015348641));
#95606=CARTESIAN_POINT('Ctrl Pts',(-8.69545865342,-23.2844297289,10.881098906));
#95607=CARTESIAN_POINT('Ctrl Pts',(-8.64139608915,-23.2107989673,10.8311116257));
#95608=CARTESIAN_POINT('Ctrl Pts',(-8.57793860163,-23.1733812942,10.7632250217));
#95609=CARTESIAN_POINT('Ctrl Pts',(-8.51747673428,-23.1720132443,10.6920985753));
#95610=CARTESIAN_POINT('Ctrl Pts',(-8.85271909481,-23.4283765706,10.7986501186));
#95611=CARTESIAN_POINT('Ctrl Pts',(-8.80174479507,-23.3522217493,10.8290472717));
#95612=CARTESIAN_POINT('Ctrl Pts',(-8.74702097884,-23.2760669279,10.8249995844));
#95613=CARTESIAN_POINT('Ctrl Pts',(-8.69926483364,-23.2110252232,10.7808433397));
#95614=CARTESIAN_POINT('Ctrl Pts',(-8.66655321101,-23.1680969408,10.704046549));
#95615=CARTESIAN_POINT('Ctrl Pts',(-8.64928312709,-23.1513060056,10.6105493344));
#95616=CARTESIAN_POINT('Ctrl Pts',(-8.95374236957,-23.2551805764,10.8169485727));
#95617=CARTESIAN_POINT('Ctrl Pts',(-8.90906105284,-23.2232432649,10.7961844516));
#95618=CARTESIAN_POINT('Ctrl Pts',(-8.87369407635,-23.1913059533,10.770178964));
#95619=CARTESIAN_POINT('Ctrl Pts',(-8.84720879161,-23.1552341963,10.7456901634));
#95620=CARTESIAN_POINT('Ctrl Pts',(-8.82709666423,-23.1116114836,10.7203986113));
#95621=CARTESIAN_POINT('Ctrl Pts',(-8.81389010608,-23.0647081339,10.6876384968));
#95622=CARTESIAN_POINT('Ctrl Pts',(-9.01791018836,-23.1549008445,10.8214049608));
#95623=CARTESIAN_POINT('Ctrl Pts',(-8.99622746462,-23.1216722312,10.8155316644));
#95624=CARTESIAN_POINT('Ctrl Pts',(-8.97425273896,-23.0884436179,10.8039507789));
#95625=CARTESIAN_POINT('Ctrl Pts',(-8.95224692858,-23.0584727018,10.783603786));
#95626=CARTESIAN_POINT('Ctrl Pts',(-8.93220449355,-23.0344758471,10.7563348016));
#95627=CARTESIAN_POINT('Ctrl Pts',(-8.91487253124,-23.0145682268,10.7261343735));
#95628=CARTESIAN_POINT('Ctrl Pts',(-9.08532173979,-23.0061361581,10.858062108));
#95629=CARTESIAN_POINT('Ctrl Pts',(-9.07401122054583,-22.994360504385,10.847601774363));
#95630=CARTESIAN_POINT('Ctrl Pts',(-9.06350105813443,-22.9825848532249,
10.8378821902984));
#95631=CARTESIAN_POINT('Ctrl Pts',(-9.05419277619886,-22.9699073952249,
10.8292755748936));
#95632=CARTESIAN_POINT('Ctrl Pts',(-9.04554579428692,-22.955591884285,10.8212820971294));
#95633=CARTESIAN_POINT('Ctrl Pts',(-9.03689844897,-22.9401858313,10.8132890077));
#95634=CARTESIAN_POINT('Ctrl Pts',(-9.1336794452,-22.8742356128,10.9029059811));
#95635=CARTESIAN_POINT('Ctrl Pts',(-9.1336794452,-22.8742356128,10.9029059811));
#95636=CARTESIAN_POINT('Ctrl Pts',(-9.1336794452,-22.8742356128,10.9029059811));
#95637=CARTESIAN_POINT('Ctrl Pts',(-9.1336794452,-22.8742356128,10.9029059811));
#95638=CARTESIAN_POINT('Ctrl Pts',(-9.1336794452,-22.8742356128,10.9029059811));
#95639=CARTESIAN_POINT('Ctrl Pts',(-9.1336794452,-22.8742356128,10.9029059811));
#95640=CARTESIAN_POINT('Ctrl Pts',(-9.1336794452,-22.8742356128,10.9029059811));
#95641=CARTESIAN_POINT('Ctrl Pts',(-9.12359832874988,-22.8811058500385,
10.8935710990721));
#95642=CARTESIAN_POINT('Ctrl Pts',(-9.113191622868,-22.8880836120972,10.8842714443679));
#95643=CARTESIAN_POINT('Ctrl Pts',(-9.10255323648157,-22.8951026557958,
10.8751006061354));
#95644=CARTESIAN_POINT('Ctrl Pts',(-9.09148992869508,-22.9024020560981,
10.865563463721));
#95645=CARTESIAN_POINT('Ctrl Pts',(-9.08017585698654,-22.9097463028922,
10.8561652636545));
#95646=CARTESIAN_POINT('Ctrl Pts',(-9.068677710726,-22.9170878993633,10.8469738134868));
#95647=CARTESIAN_POINT('Ctrl Pts',(-9.05606690031054,-22.9251399348085,
10.8368929158462));
#95648=CARTESIAN_POINT('Ctrl Pts',(-9.04323465488263,-22.9331888946587,
10.8270603983741));
#95649=CARTESIAN_POINT('Ctrl Pts',(-9.03022424765914,-22.9412018306295,
10.8175265503564));
#95650=CARTESIAN_POINT('Ctrl Pts',(-9.02087653152683,-22.9469589640962,
10.8106766721483));
#95651=CARTESIAN_POINT('Ctrl Pts',(-9.01143583423362,-22.9526981799119,
10.8039800671005));
#95652=CARTESIAN_POINT('Ctrl Pts',(-9.0019065535912,-22.9584144908771,10.7974466868649));
#95653=CARTESIAN_POINT('Ctrl Pts',(-8.9847535490042,-22.9687040302333,10.7856863971478));
#95654=CARTESIAN_POINT('Ctrl Pts',(-8.96731630136919,-22.9789182402692,
10.7744552003213));
#95655=CARTESIAN_POINT('Ctrl Pts',(-8.94956526595337,-22.9890573569769,
10.7637843427106));
#95656=CARTESIAN_POINT('Ctrl Pts',(-8.93276576605315,-22.9986529713243,
10.7536854911695));
#95657=CARTESIAN_POINT('Ctrl Pts',(-8.91568265292127,-23.0081832742568,
10.744085552575));
#95658=CARTESIAN_POINT('Ctrl Pts',(-8.89826151733235,-23.0176556306316,
10.7350216727571));
#95659=CARTESIAN_POINT('Ctrl Pts',(-8.88417397090941,-23.0253154217791,
10.7276921948907));
#95660=CARTESIAN_POINT('Ctrl Pts',(-8.86986440346832,-23.0329378192506,
10.7207128487755));
#95661=CARTESIAN_POINT('Ctrl Pts',(-8.85530486807876,-23.0405181524084,
10.7141276263695));
#95662=CARTESIAN_POINT('Ctrl Pts',(-8.84127764671044,-23.047821339523,10.707783167568));
#95663=CARTESIAN_POINT('Ctrl Pts',(-8.82701783103774,-23.055085911662,10.7018038913073));
#95664=CARTESIAN_POINT('Ctrl Pts',(-8.81251122931992,-23.0622926242237,
10.6962618555677));
#95665=CARTESIAN_POINT('Ctrl Pts',(-8.79876011359606,-23.0691240200497,
10.6910084422402));
#95666=CARTESIAN_POINT('Ctrl Pts',(-8.78478689488389,-23.0759036692302,
10.6861475775762));
#95667=CARTESIAN_POINT('Ctrl Pts',(-8.77059576001363,-23.0825967640568,
10.681777295819));
#95668=CARTESIAN_POINT('Ctrl Pts',(-8.75729431827173,-23.0888702447702,
10.6776810026951));
#95669=CARTESIAN_POINT('Ctrl Pts',(-8.7438012610872,-23.0950677771167,10.6740156131765));
#95670=CARTESIAN_POINT('Ctrl Pts',(-8.73013818703274,-23.1011418674376,
10.6708977038454));
#95671=CARTESIAN_POINT('Ctrl Pts',(-8.71719988970545,-23.1068937492069,
10.6679451883422));
#95672=CARTESIAN_POINT('Ctrl Pts',(-8.70410903249947,-23.1125349926791,
10.6654835591288));
#95673=CARTESIAN_POINT('Ctrl Pts',(-8.69090263710776,-23.1180067844081,
10.6636460594846));
#95674=CARTESIAN_POINT('Ctrl Pts',(-8.67775361963559,-23.1234548028049,
10.6618165432381));
#95675=CARTESIAN_POINT('Ctrl Pts',(-8.66448983074481,-23.1287350304218,
10.6606054381024));
#95676=CARTESIAN_POINT('Ctrl Pts',(-8.6511695285881,-23.1337685681875,10.6601821897177));
#95677=CARTESIAN_POINT('Ctrl Pts',(-8.63836928290993,-23.1386055845909,
10.6597754659631));
#95678=CARTESIAN_POINT('Ctrl Pts',(-8.62551678329554,-23.1432148356153,
10.6600962419175));
#95679=CARTESIAN_POINT('Ctrl Pts',(-8.61268579786253,-23.1475055628669,
10.6613321230521));
#95680=CARTESIAN_POINT('Ctrl Pts',(-8.6001045595605,-23.1517127737878,10.662543948531));
#95681=CARTESIAN_POINT('Ctrl Pts',(-8.58754389183535,-23.1556138260663,
10.6646354720753));
#95682=CARTESIAN_POINT('Ctrl Pts',(-8.57509640895897,-23.1591018128687,
10.6678214861139));
#95683=CARTESIAN_POINT('Ctrl Pts',(-8.56297826588685,-23.1624975133107,
10.6709232034919));
#95684=CARTESIAN_POINT('Ctrl Pts',(-8.55096733469553,-23.1655017591573,
10.675062205123));
#95685=CARTESIAN_POINT('Ctrl Pts',(-8.53917239193139,-23.1679945890078,
10.6804742569932));
#95686=CARTESIAN_POINT('Ctrl Pts',(-8.5318464032349,-23.1695429172763,10.6838357511198));
#95687=CARTESIAN_POINT('Ctrl Pts',(-8.52460420271352,-23.1708935277647,
10.6876891087437));
#95688=CARTESIAN_POINT('Ctrl Pts',(-8.51747674491568,-23.1720132445407,
10.6920985878117));
#95689=CARTESIAN_POINT('Origin',(-6.6707290414,-22.8742356128,9.03420135995));
#95690=CARTESIAN_POINT('',(-7.70044916513,-22.8742356128,9.57771386935));
#95691=CARTESIAN_POINT('Origin',(7.16045579301E-17,-22.6642356128,0.580061096523));
#95692=CARTESIAN_POINT('',(-10.9304145503,-21.0742356128,10.3907473403));
#95693=CARTESIAN_POINT('',(-10.9304145503,-21.9742356128,10.3907473403));
#95694=CARTESIAN_POINT('',(-10.0062431967,-21.0742356128,11.3317411468));
#95695=CARTESIAN_POINT('Origin',(2.04268023839E-15,-21.0742356128,0.580061096523));
#95696=CARTESIAN_POINT('',(-10.0062431967,-23.2742356128,11.3317411468));
#95697=CARTESIAN_POINT('Origin',(-10.1862176145,-21.9742356128,9.72278707155));
#95698=CARTESIAN_POINT('',(-11.1383462684,-21.0742356128,10.0284846777));
#95699=CARTESIAN_POINT('',(-11.1383462684,-22.6642356128,10.0284846777));
#95700=CARTESIAN_POINT('Origin',(-10.1862176145,-21.0742356128,9.72278707155));
#95701=CARTESIAN_POINT('Origin',(2.84607155346,-22.6642356128,5.53854202767));
#95702=CARTESIAN_POINT('Origin',(2.84607155346,-21.0742356128,5.53854202767));
#95703=CARTESIAN_POINT('Origin',(-11.3733704264,-23.1237854196,7.73136642019));
#95704=CARTESIAN_POINT('',(-11.669865565,-21.0742356128,7.77708985809));
#95705=CARTESIAN_POINT('',(-11.669865565,-22.5742356128,7.77708985809));
#95706=CARTESIAN_POINT('Origin',(-11.3733704264,-21.0742356128,7.73136642019));
#95707=CARTESIAN_POINT('Origin',(2.84607155346,-21.2742356128,5.53854202767));
#95708=CARTESIAN_POINT('',(-11.7512376696,-21.0742356128,3.91309124051));
#95709=CARTESIAN_POINT('',(-11.7512376696,-22.1242356128,3.91309124051));
#95710=CARTESIAN_POINT('Origin',(2.84607155346,-21.0742356128,5.53854202767));
#95711=CARTESIAN_POINT('Origin',(-11.4530804658,-22.1242356128,3.94629187045));
#95712=CARTESIAN_POINT('',(-11.4530804658,-21.0742356128,3.64629187045));
#95713=CARTESIAN_POINT('',(-11.4530804658,-21.9742356128,3.64629187045));
#95714=CARTESIAN_POINT('Origin',(-11.4530804658,-21.0742356128,3.94629187045));
#95715=CARTESIAN_POINT('Origin',(-11.7190551593,-23.1742356128,3.64629187045));
#95716=CARTESIAN_POINT('',(-8.10176909975,-21.0742356128,3.64629187045));
#95717=CARTESIAN_POINT('',(-8.10176909975,-22.1242356128,3.64629187045));
#95718=CARTESIAN_POINT('',(-8.95225019493,-21.0742356128,3.64629187045));
#95719=CARTESIAN_POINT('Origin',(-8.10176909975,-22.1242356128,3.94629187045));
#95720=CARTESIAN_POINT('',(-7.80346303227,-21.0742356128,3.91445651114));
#95721=CARTESIAN_POINT('',(-7.80346303227,-21.2742356128,3.91445651114));
#95722=CARTESIAN_POINT('Origin',(-8.10176909975,-21.0742356128,3.94629187045));
#95723=CARTESIAN_POINT('Origin',(-0.00234331738835,-21.2742356128,3.08191746407));
#95724=CARTESIAN_POINT('',(-6.23264645859,-21.0742356128,7.84992678029));
#95725=CARTESIAN_POINT('',(-6.23264645859,-22.1242356128,7.84992678029));
#95726=CARTESIAN_POINT('Origin',(-0.00234331738835,-21.0742356128,3.08191746407));
#95727=CARTESIAN_POINT('Origin',(-6.47088626226,-22.1242356128,8.03225010833));
#95728=CARTESIAN_POINT('',(-6.26721888507,-21.0742356128,8.25252175759));
#95729=CARTESIAN_POINT('',(-6.26721888507,-21.9742356128,8.25252175759));
#95730=CARTESIAN_POINT('Origin',(-6.47088626226,-21.0742356128,8.03225010833));
#95731=CARTESIAN_POINT('Origin',(-9.80058174751,-23.1742356128,11.519536597));
#95732=CARTESIAN_POINT('',(-9.59819339216,-21.0742356128,11.3324044552));
#95733=CARTESIAN_POINT('',(-9.59819339216,-23.2742356128,11.3324044552));
#95734=CARTESIAN_POINT('',(-8.22276378328,-21.0742356128,10.0606559488));
#95735=CARTESIAN_POINT('Origin',(-9.80186076935,-23.2742356128,11.1121328059));
#95736=CARTESIAN_POINT('Origin',(-9.80186076935,-21.0742356128,11.1121328059));
#95737=CARTESIAN_POINT('Origin',(-9.80186076935,-21.0742356128,11.1121328059));
#95738=CARTESIAN_POINT('',(-9.80186076935,-20.7742356128,11.1121328059));
#95739=CARTESIAN_POINT('Origin',(-9.80186076935,-21.0742356128,11.1121328059));
#95740=CARTESIAN_POINT('Origin',(-9.80186076935,-21.0742356128,11.1121328059));
#95741=CARTESIAN_POINT('Origin',(2.04268023839E-15,-21.0742356128,0.580061096523));
#95742=CARTESIAN_POINT('',(-10.7071554695,-20.7742356128,10.1903592597));
#95743=CARTESIAN_POINT('Origin',(-10.7071554695,-21.0742356128,10.1903592597));
#95744=CARTESIAN_POINT('Origin',(-5.42499920527E-16,-20.7742356128,0.580061096523));
#95745=CARTESIAN_POINT('Origin',(-10.1862176145,-21.0742356128,9.72278707155));
#95746=CARTESIAN_POINT('',(-10.8527076722,-20.7742356128,9.93677539585));
#95747=CARTESIAN_POINT('Origin',(-10.8527076722,-21.0742356128,9.93677539585));
#95748=CARTESIAN_POINT('Origin',(-10.1862176145,-20.7742356128,9.72278707155));
#95749=CARTESIAN_POINT('Origin',(-10.8795671881,-21.0742356128,9.85222376962));
#95750=CARTESIAN_POINT('',(-10.8795671881,-20.7742356128,9.85222376962));
#95751=CARTESIAN_POINT('Origin',(-10.8795671881,-21.0742356128,9.85222376962));
#95752=CARTESIAN_POINT('Origin',(-10.8795671881,-21.0742356128,9.85222376962));
#95753=CARTESIAN_POINT('Origin',(2.84607155346,-21.0742356128,5.53854202767));
#95754=CARTESIAN_POINT('Origin',(2.84607155346,-20.7742356128,5.53854202767));
#95755=CARTESIAN_POINT('Origin',(-11.3733704264,-21.0742356128,7.73136642019));
#95756=CARTESIAN_POINT('',(-11.3733704264,-20.7742356128,7.73136642019));
#95757=CARTESIAN_POINT('Origin',(-11.3733704264,-21.0742356128,7.73136642019));
#95758=CARTESIAN_POINT('Origin',(-11.3733704264,-21.0742356128,7.73136642019));
#95759=CARTESIAN_POINT('Origin',(2.84607155346,-21.0742356128,5.53854202767));
#95760=CARTESIAN_POINT('',(-11.4530804658,-20.7742356128,3.94629187045));
#95761=CARTESIAN_POINT('Origin',(-11.4530804658806,-21.0742356128,3.9462918704403));
#95762=CARTESIAN_POINT('Origin',(2.84607155346,-20.7742356128,5.53854202767));
#95763=CARTESIAN_POINT('Origin',(-11.4530804658,-21.0742356128,3.94629187045));
#95764=CARTESIAN_POINT('Origin',(-11.4530804658,-21.0742356128,3.94629187045));
#95765=CARTESIAN_POINT('Origin',(-8.95225019493,-21.0742356128,3.94629187045));
#95766=CARTESIAN_POINT('',(-8.10176909975,-20.7742356128,3.94629187045));
#95767=CARTESIAN_POINT('Origin',(-8.10176909975,-21.0742356128,3.94629187045));
#95768=CARTESIAN_POINT('',(-9.77742478279,-20.7742356128,3.94629187045));
#95769=CARTESIAN_POINT('Origin',(-8.10176909975,-21.0742356128,3.94629187045));
#95770=CARTESIAN_POINT('Origin',(-8.10176909975,-21.0742356128,3.94629187045));
#95771=CARTESIAN_POINT('Origin',(-0.00234331738835,-21.0742356128,3.08191746407));
#95772=CARTESIAN_POINT('',(-6.47088626226,-20.7742356128,8.03225010833));
#95773=CARTESIAN_POINT('Origin',(-6.47088626225866,-21.0742356128,8.0322501083283));
#95774=CARTESIAN_POINT('Origin',(-0.00234331738835,-20.7742356128,3.08191746407));
#95775=CARTESIAN_POINT('Origin',(-6.47088626226,-21.0742356128,8.03225010833));
#95776=CARTESIAN_POINT('Origin',(-6.47088626226,-21.0742356128,8.03225010833));
#95777=CARTESIAN_POINT('Origin',(-8.42643116047,-21.0742356128,9.84038429957));
#95778=CARTESIAN_POINT('',(-8.1363735158,-20.7742356128,9.57219145714));
#95779=CARTESIAN_POINT('Origin',(-9.00617217252,-21.0742356128,8.1200469301));
#95780=CARTESIAN_POINT('',(-10.5002881066,-20.7742356128,9.5015350813));
#95781=CARTESIAN_POINT('Origin',(-10.5002881066,-21.0742356128,9.5015350813));
#95782=CARTESIAN_POINT('',(-10.6899276473,-20.7742356128,9.67687942546));
#95783=CARTESIAN_POINT('Origin',(-10.9076228609,-21.0742356128,9.06099178277));
#95784=CARTESIAN_POINT('',(-10.4339531167,-20.7742356128,8.69270253038));
#95785=CARTESIAN_POINT('Origin',(-10.4339531167,-21.0742356128,8.69270253038));
#95786=CARTESIAN_POINT('Origin',(-10.9076228609,-20.7742356128,9.06099178277));
#95787=CARTESIAN_POINT('Origin',(5.59539391719E-15,-21.0742356128,0.580061096523));
#95788=CARTESIAN_POINT('',(-10.9433745451,-20.7742356128,7.99119341506));
#95789=CARTESIAN_POINT('Origin',(-10.9433745451,-21.0742356128,7.99119341506));
#95790=CARTESIAN_POINT('Origin',(8.04064645258E-16,-20.7742356128,0.580061096523));
#95791=CARTESIAN_POINT('Origin',(-11.4401704731,-21.0742356128,8.32763628675));
#95792=CARTESIAN_POINT('Origin',(-11.4401704731,-20.7742356128,8.32763628675));
#95793=CARTESIAN_POINT('Origin',(2.93915231795E-16,-20.7742356128,0.729452270839));
#95794=CARTESIAN_POINT('',(0.,0.,0.));
#95795=CARTESIAN_POINT('Origin',(-3.54162636048E-14,-23.4742356128,0.580061096522));
#95796=CARTESIAN_POINT('',(7.55300678542,-23.1742356128,11.1813685383));
#95797=CARTESIAN_POINT('',(10.9011091428,-23.1742356128,7.69353074443));
#95798=CARTESIAN_POINT('Origin',(-3.36841676743E-14,-23.1742356128,0.580061096522));
#95799=CARTESIAN_POINT('',(7.72708272879,-23.4742356128,11.4256993917));
#95800=CARTESIAN_POINT('Origin',(7.55300678542,-23.4742356128,11.1813685383));
#95801=CARTESIAN_POINT('',(11.1523495973,-23.4742356128,7.85747657088));
#95802=CARTESIAN_POINT('Origin',(-3.54162636048E-14,-23.4742356128,0.580061096522));
#95803=CARTESIAN_POINT('Origin',(10.9011091428,-23.4742356128,7.69353074443));
#95804=CARTESIAN_POINT('Origin',(-15.6588697715,-28.8242356128,14.965390674));
#95805=CARTESIAN_POINT('',(3.78111690148,-25.6742356128,-1.85483293631));
#95806=CARTESIAN_POINT('',(8.81393818057,-25.6742356128,7.09680280277));
#95807=CARTESIAN_POINT('Origin',(-15.6588697715,-25.6742356128,14.965390674));
#95808=CARTESIAN_POINT('',(3.78111690148,-32.4742356128,-1.85483293631));
#95809=CARTESIAN_POINT('',(3.78111690148,-28.8242356128,-1.85483293631));
#95810=CARTESIAN_POINT('',(8.81393818057,-32.4742356128,7.09680280277));
#95811=CARTESIAN_POINT('Origin',(-15.6588697715,-32.4742356128,14.965390674));
#95812=CARTESIAN_POINT('',(8.81393818057,-28.8242356128,7.09680280277));
#95813=CARTESIAN_POINT('Origin',(8.52833752869,-28.8242356128,7.18863018236));
#95814=CARTESIAN_POINT('',(8.74359670241,-25.6742356128,7.39758828372));
#95815=CARTESIAN_POINT('Origin',(8.52833113701624,-25.6742356128,7.18862868760432));
#95816=CARTESIAN_POINT('',(8.74359670241,-32.4742356128,7.39758828372));
#95817=CARTESIAN_POINT('Origin',(8.52833752869,-32.4742356128,7.18863018236));
#95818=CARTESIAN_POINT('',(8.74359670241,-28.8242356128,7.39758828372));
#95819=CARTESIAN_POINT('Origin',(-0.0657457778947,-28.8242356128,-1.15388688513));
#95820=CARTESIAN_POINT('',(0.0451717833072,-25.6742356128,11.1229180654));
#95821=CARTESIAN_POINT('Origin',(-0.0657457778946,-25.6742356128,-1.15388688513));
#95822=CARTESIAN_POINT('',(0.0451717833072,-32.4742356128,11.1229180654));
#95823=CARTESIAN_POINT('Origin',(-0.0657457778947,-32.4742356128,-1.15388688513));
#95824=CARTESIAN_POINT('',(0.0451717833071,-28.8242356128,11.1229180654));
#95825=CARTESIAN_POINT('Origin',(-15.6588697715,-25.6742356128,14.965390674));
#95826=CARTESIAN_POINT('',(8.30073298506,-25.1742356128,7.13507985462));
#95827=CARTESIAN_POINT('Ctrl Pts',(8.81393818057,-25.6742356128,7.09680280277));
#95828=CARTESIAN_POINT('Ctrl Pts',(8.81409597531014,-25.6430987071103,7.09679428198758));
#95829=CARTESIAN_POINT('Ctrl Pts',(8.81109093290262,-25.6115059429941,7.09701288121902));
#95830=CARTESIAN_POINT('Ctrl Pts',(8.80487037092342,-25.5800824415237,7.09746532919756));
#95831=CARTESIAN_POINT('Ctrl Pts',(8.79926072489547,-25.5517450146485,7.09787334265587));
#95832=CARTESIAN_POINT('Ctrl Pts',(8.79103561354454,-25.5235452886408,7.09847156569394));
#95833=CARTESIAN_POINT('Ctrl Pts',(8.78018861926916,-25.4959592212314,7.09926271867066));
#95834=CARTESIAN_POINT('Ctrl Pts',(8.77037287022121,-25.4709958158829,7.09997865516707));
#95835=CARTESIAN_POINT('Ctrl Pts',(8.75840870206946,-25.4465334581682,7.10085268219171));
#95836=CARTESIAN_POINT('Ctrl Pts',(8.74432821981368,-25.4229440144713,7.10188423921424));
#95837=CARTESIAN_POINT('Ctrl Pts',(8.73123668297153,-25.4010113799469,7.10284334462838));
#95838=CARTESIAN_POINT('Ctrl Pts',(8.71631480657571,-25.3798332969455,7.10393869376322));
#95839=CARTESIAN_POINT('Ctrl Pts',(8.69963101268627,-25.359720545253,7.10516680982952));
#95840=CARTESIAN_POINT('Ctrl Pts',(8.69317933739034,-25.3519428812463,7.10564172615479));
#95841=CARTESIAN_POINT('Ctrl Pts',(8.68646461977483,-25.3443245121491,7.10613646555696));
#95842=CARTESIAN_POINT('Ctrl Pts',(8.67949292808951,-25.3368836314267,7.10665067565743));
#95843=CARTESIAN_POINT('Ctrl Pts',(8.67647070290223,-25.3336580130044,7.10687358550303));
#95844=CARTESIAN_POINT('Ctrl Pts',(8.67316612602285,-25.3302224683051,7.10711784043832));
#95845=CARTESIAN_POINT('Ctrl Pts',(8.66993041923766,-25.3269524229621,7.10735706822193));
#95846=CARTESIAN_POINT('Ctrl Pts',(8.66677232332068,-25.3237608121235,7.10759055794669));
#95847=CARTESIAN_POINT('Ctrl Pts',(8.66368055276476,-25.3207264237881,7.1078192059096));
#95848=CARTESIAN_POINT('Ctrl Pts',(8.66101580561167,-25.3181635759878,7.10801593081068));
#95849=CARTESIAN_POINT('Ctrl Pts',(8.64724802689458,-25.3049222741409,7.10903233677742));
#95850=CARTESIAN_POINT('Ctrl Pts',(8.63225657618394,-25.2920046393027,7.11014168728378));
#95851=CARTESIAN_POINT('Ctrl Pts',(8.61600070173619,-25.2796661628299,7.11134761798622));
#95852=CARTESIAN_POINT('Ctrl Pts',(8.60677675522023,-25.2726650354873,7.11203189002197));
#95853=CARTESIAN_POINT('Ctrl Pts',(8.59714641349781,-25.2658508967218,7.11274721153374));
#95854=CARTESIAN_POINT('Ctrl Pts',(8.58710884486889,-25.259274077119,7.11349381184021));
#95855=CARTESIAN_POINT('Ctrl Pts',(8.5698814614288,-25.2479863442725,7.11477519483558));
#95856=CARTESIAN_POINT('Ctrl Pts',(8.55145176627244,-25.2373969109191,7.11614891068513));
#95857=CARTESIAN_POINT('Ctrl Pts',(8.53185116100626,-25.2277728047567,7.11761393892338));
#95858=CARTESIAN_POINT('Ctrl Pts',(8.52384812727395,-25.2238432298677,7.11821211792093));
#95859=CARTESIAN_POINT('Ctrl Pts',(8.51565041966796,-25.2200747426444,7.11882548312532));
#95860=CARTESIAN_POINT('Ctrl Pts',(8.50726250968196,-25.2164861229366,7.11945380371546));
#95861=CARTESIAN_POINT('Ctrl Pts',(8.50488129707811,-25.2154673630199,7.11963217531351));
#95862=CARTESIAN_POINT('Ctrl Pts',(8.50197597208091,-25.2142508838615,7.11984987911369));
#95863=CARTESIAN_POINT('Ctrl Pts',(8.49942431172375,-25.2132081626979,7.1200411607002));
#95864=CARTESIAN_POINT('Ctrl Pts',(8.49754711050464,-25.2124410553381,7.12018188241748));
#95865=CARTESIAN_POINT('Ctrl Pts',(8.49586208380619,-25.2117662483067,7.12030824103353));
#95866=CARTESIAN_POINT('Ctrl Pts',(8.49472562376124,-25.2113146890593,7.12039348309374));
#95867=CARTESIAN_POINT('Ctrl Pts',(8.48470395294944,-25.2073326941365,7.12114517504327));
#95868=CARTESIAN_POINT('Ctrl Pts',(8.47355138450343,-25.2032580976879,7.12198258088398));
#95869=CARTESIAN_POINT('Ctrl Pts',(8.4612079575769,-25.1993036718151,7.12291109578253));
#95870=CARTESIAN_POINT('Ctrl Pts',(8.44960457064268,-25.1955863302876,7.12378394233529));
#95871=CARTESIAN_POINT('Ctrl Pts',(8.43694804343264,-25.1919755178591,7.12473735944721));
#95872=CARTESIAN_POINT('Ctrl Pts',(8.42320929947104,-25.1886882300447,7.12577452498151));
#95873=CARTESIAN_POINT('Ctrl Pts',(8.41004691756789,-25.185538849158,7.12676817977974));
#95874=CARTESIAN_POINT('Ctrl Pts',(8.39589040114202,-25.182686711434,7.12783876345823));
#95875=CARTESIAN_POINT('Ctrl Pts',(8.38074527934273,-25.1803564605959,7.1289869922473));
#95876=CARTESIAN_POINT('Ctrl Pts',(8.36665346776027,-25.1781882736254,7.13005536422632));
#95877=CARTESIAN_POINT('Ctrl Pts',(8.35170527003246,-25.1764723672986,7.1311909953895));
#95878=CARTESIAN_POINT('Ctrl Pts',(8.33594155628545,-25.1754140609642,7.1323919600745));
#95879=CARTESIAN_POINT('Ctrl Pts',(8.32461548857318,-25.1746536786458,7.13325484096417));
#95880=CARTESIAN_POINT('Ctrl Pts',(8.3128690940841,-25.1742332866394,7.13415140342761));
#95881=CARTESIAN_POINT('Ctrl Pts',(8.30073298506,-25.1742356128,7.13507985462));
#95882=CARTESIAN_POINT('',(3.40300521133,-25.1742356128,-1.52767616996));
#95883=CARTESIAN_POINT('Origin',(-15.6588697715,-25.1742356128,14.965390674));
#95884=CARTESIAN_POINT('Origin',(3.40300521133,-25.6742356128,-1.52767616996));
#95885=CARTESIAN_POINT('Ctrl Pts',(8.30073298506,-25.1742356128,7.13507985462));
#95886=CARTESIAN_POINT('Ctrl Pts',(8.30073298506,-25.1742356128,7.13507985462));
#95887=CARTESIAN_POINT('Ctrl Pts',(8.30073298506,-25.1742356128,7.13507985462));
#95888=CARTESIAN_POINT('Ctrl Pts',(8.30073298506,-25.1742356128,7.13507985462));
#95889=CARTESIAN_POINT('Ctrl Pts',(8.30073298506,-25.1742356128,7.13507985462));
#95890=CARTESIAN_POINT('Ctrl Pts',(8.30073298506,-25.1742356128,7.13507985462));
#95891=CARTESIAN_POINT('Ctrl Pts',(8.4984544281,-25.174197715,7.11995353125));
#95892=CARTESIAN_POINT('Ctrl Pts',(8.49276880815,-25.1768387338,7.14348907236));
#95893=CARTESIAN_POINT('Ctrl Pts',(8.48739621864,-25.1782703109,7.1669182153));
#95894=CARTESIAN_POINT('Ctrl Pts',(8.48185217011,-25.1782703109,7.1903276789));
#95895=CARTESIAN_POINT('Ctrl Pts',(8.47614313121,-25.1768387338,7.21368444167));
#95896=CARTESIAN_POINT('Ctrl Pts',(8.47066320143,-25.174197715,7.23727979168));
#95897=CARTESIAN_POINT('Ctrl Pts',(8.70134899424,-25.2739717972,7.10492272115));
#95898=CARTESIAN_POINT('Ctrl Pts',(8.68923886464,-25.2513427762,7.15177407669));
#95899=CARTESIAN_POINT('Ctrl Pts',(8.6767502882,-25.2399151794,7.19877329204));
#95900=CARTESIAN_POINT('Ctrl Pts',(8.66568269835,-25.2399151794,7.24586328974));
#95901=CARTESIAN_POINT('Ctrl Pts',(8.65593998646,-25.2513427762,7.29347796257));
#95902=CARTESIAN_POINT('Ctrl Pts',(8.64594321094,-25.2739717972,7.34077222156));
#95903=CARTESIAN_POINT('Ctrl Pts',(8.81494578451,-25.4754097912,7.09674839301));
#95904=CARTESIAN_POINT('Ctrl Pts',(8.83671968197,-25.4572913208,7.15869208185));
#95905=CARTESIAN_POINT('Ctrl Pts',(8.84072845773,-25.4471049231,7.22634784813));
#95906=CARTESIAN_POINT('Ctrl Pts',(8.82507001711,-25.4471049231,7.29331987756));
#95907=CARTESIAN_POINT('Ctrl Pts',(8.79148126327,-25.4572913208,7.35218191877));
#95908=CARTESIAN_POINT('Ctrl Pts',(8.74450298325,-25.4754097912,7.39804592883));
#95909=CARTESIAN_POINT('Ctrl Pts',(8.81393818057,-25.6742356128,7.09680280277));
#95910=CARTESIAN_POINT('Ctrl Pts',(8.83380283672,-25.6742356128,7.15858566939));
#95911=CARTESIAN_POINT('Ctrl Pts',(8.83696093696,-25.6742356128,7.22574008976));
#95912=CARTESIAN_POINT('Ctrl Pts',(8.82141102617,-25.6742356128,7.29223268441));
#95913=CARTESIAN_POINT('Ctrl Pts',(8.78879978729,-25.6742356128,7.35102211263));
#95914=CARTESIAN_POINT('Ctrl Pts',(8.74359670241,-25.6742356128,7.39758828372));
#95915=CARTESIAN_POINT('Ctrl Pts',(8.74359670241,-25.6742356128,7.39758828372));
#95916=CARTESIAN_POINT('Ctrl Pts',(8.74372026636865,-25.6475507397519,7.39764771721947));
#95917=CARTESIAN_POINT('Ctrl Pts',(8.74182618313521,-25.6208162503538,7.39653602596286));
#95918=CARTESIAN_POINT('Ctrl Pts',(8.73801919658173,-25.5944358816126,7.39430757850375));
#95919=CARTESIAN_POINT('Ctrl Pts',(8.73421219462006,-25.5680554061009,7.39207912202535));
#95920=CARTESIAN_POINT('Ctrl Pts',(8.72849227567299,-25.5420290554374,7.38873390121572));
#95921=CARTESIAN_POINT('Ctrl Pts',(8.72098866821749,-25.5167170035454,7.38434111159174));
#95922=CARTESIAN_POINT('Ctrl Pts',(8.71348504486413,-25.4914048980248,7.37994831266077));
#95923=CARTESIAN_POINT('Ctrl Pts',(8.70419772727086,-25.466807095613,7.37450794139217));
#95924=CARTESIAN_POINT('Ctrl Pts',(8.69328040076856,-25.4432401846987,7.36810400637077));
#95925=CARTESIAN_POINT('Ctrl Pts',(8.68236303758426,-25.4196731946,7.36170004983228));
#95926=CARTESIAN_POINT('Ctrl Pts',(8.66981565635879,-25.3971371042455,7.35433252397831));
#95927=CARTESIAN_POINT('Ctrl Pts',(8.65581637278916,-25.3759048974086,7.34610023724638));
#95928=CARTESIAN_POINT('Ctrl Pts',(8.64227591227988,-25.3553685709052,7.33813776167824));
#95929=CARTESIAN_POINT('Ctrl Pts',(8.6273772855856,-25.3360518414704,7.32936635610616));
#95930=CARTESIAN_POINT('Ctrl Pts',(8.6113033813004,-25.3181628924002,7.31988858811994));
#95931=CARTESIAN_POINT('Ctrl Pts',(8.59486613553566,-25.2998695737937,7.3101965805699));
#95932=CARTESIAN_POINT('Ctrl Pts',(8.57720378186642,-25.2830667777551,7.29975760222087));
#95933=CARTESIAN_POINT('Ctrl Pts',(8.55853027393535,-25.2679387521626,7.28870277438831));
#95934=CARTESIAN_POINT('Ctrl Pts',(8.53975404846916,-25.2527275117021,7.27758713716363));
#95935=CARTESIAN_POINT('Ctrl Pts',(8.5199555841994,-25.2392096737772,7.26584898160584));
#95936=CARTESIAN_POINT('Ctrl Pts',(8.49937968702385,-25.2275283404032,7.25363349339433));
#95937=CARTESIAN_POINT('Ctrl Pts',(8.47873372599749,-25.2158072304309,7.24137640971136));
#95938=CARTESIAN_POINT('Ctrl Pts',(8.45730513048159,-25.2059351634624,7.22863884304467));
#95939=CARTESIAN_POINT('Ctrl Pts',(8.4353672412806,-25.1980110304246,7.21557761615551));
#95940=CARTESIAN_POINT('Ctrl Pts',(8.41288483366739,-25.1898902131798,7.20219219770616));
#95941=CARTESIAN_POINT('Ctrl Pts',(8.38986748854582,-25.1838151952435,7.18846686114024));
#95942=CARTESIAN_POINT('Ctrl Pts',(8.36663630941895,-25.179844349708,7.17458014983943));
#95943=CARTESIAN_POINT('Ctrl Pts',(8.34476122003766,-25.1761052970954,7.16150405717714));
#95944=CARTESIAN_POINT('Ctrl Pts',(8.3226966840604,-25.1742311488963,7.14828490547556));
#95945=CARTESIAN_POINT('Ctrl Pts',(8.30073298506,-25.1742356128,7.13507985462));
#95946=CARTESIAN_POINT('Origin',(-0.0657457778946,-25.6742356128,-1.15388688513));
#95947=CARTESIAN_POINT('',(0.0406546049764,-25.1742356128,10.6229384707));
#95948=CARTESIAN_POINT('Origin',(0.0406546049764,-25.6742356128,10.6229384707));
#95949=CARTESIAN_POINT('Origin',(-0.0657457778947,-25.1742356128,-1.15388688513));
#95950=CARTESIAN_POINT('Origin',(-1.33907057367E-16,-25.1742356128,0.729452270839));
#95951=CARTESIAN_POINT('',(-8.30073298506,-25.1742356128,7.13507985462));
#95952=CARTESIAN_POINT('',(-3.40300521133,-25.1742356128,-1.52767616996));
#95953=CARTESIAN_POINT('Origin',(15.6588697715,-25.1742356128,14.965390674));
#95954=CARTESIAN_POINT('Origin',(2.80638175951E-15,-25.1742356128,1.41673472726));
#95955=CARTESIAN_POINT('',(-0.0406546049764,-25.1742356128,10.6229384707));
#95956=CARTESIAN_POINT('Origin',(-5.68076154778E-15,-25.1742356128,6.12312211857));
#95957=CARTESIAN_POINT('Origin',(0.0657457778947,-25.1742356128,-1.15388688513));
#95958=CARTESIAN_POINT('Origin',(2.74514941955E-15,-25.6742356128,1.41673472726));
#95959=CARTESIAN_POINT('',(-3.78111690148,-25.6742356128,-1.85483293631));
#95960=CARTESIAN_POINT('Origin',(4.0774170491E-15,-25.6742356128,1.41673472726));
#95961=CARTESIAN_POINT('Origin',(-3.40300521133,-25.6742356128,-1.52767616996));
#95962=CARTESIAN_POINT('Origin',(3.69165330737E-15,-28.8242356128,1.41673472726));
#95963=CARTESIAN_POINT('',(-3.78111690148,-32.4742356128,-1.85483293631));
#95964=CARTESIAN_POINT('',(-3.78111690148,-28.8242356128,-1.85483293631));
#95965=CARTESIAN_POINT('Origin',(3.24465722568E-15,-32.4742356128,1.41673472726));
#95966=CARTESIAN_POINT('Origin',(15.6588697715,-25.6742356128,14.965390674));
#95967=CARTESIAN_POINT('',(-8.81393818057,-25.6742356128,7.09680280277));
#95968=CARTESIAN_POINT('Ctrl Pts',(-8.81393818057,-25.6742356128,7.09680280277));
#95969=CARTESIAN_POINT('Ctrl Pts',(-8.81494581646,-25.4754098599,7.09674839068));
#95970=CARTESIAN_POINT('Ctrl Pts',(-8.70134895175,-25.2739717119,7.10492272423));
#95971=CARTESIAN_POINT('Ctrl Pts',(-8.49845441271,-25.1741977344,7.11995353245));
#95972=CARTESIAN_POINT('Ctrl Pts',(-8.30073298506,-25.1742356128,7.13507985462));
#95973=CARTESIAN_POINT('Origin',(15.6588697715,-25.6742356128,14.965390674));
#95974=CARTESIAN_POINT('Origin',(15.6588697715,-28.8242356128,14.965390674));
#95975=CARTESIAN_POINT('',(-8.81393818057,-32.4742356128,7.09680280277));
#95976=CARTESIAN_POINT('',(-8.81393818057,-28.8242356128,7.09680280277));
#95977=CARTESIAN_POINT('Origin',(15.6588697715,-32.4742356128,14.965390674));
#95978=CARTESIAN_POINT('Origin',(-5.74199388774E-15,-25.6742356128,6.12312211857));
#95979=CARTESIAN_POINT('',(-0.0451717833072,-25.6742356128,11.1229180654));
#95980=CARTESIAN_POINT('Origin',(-5.76281056945E-15,-25.6742356128,6.12312211857));
#95981=CARTESIAN_POINT('Origin',(-0.0406546049764,-25.6742356128,10.6229384707));
#95982=CARTESIAN_POINT('Origin',(-6.14857431118E-15,-28.8242356128,6.12312211857));
#95983=CARTESIAN_POINT('',(-0.0451717833072,-32.4742356128,11.1229180654));
#95984=CARTESIAN_POINT('Origin',(-6.59557039287E-15,-32.4742356128,6.12312211857));
#95985=CARTESIAN_POINT('',(-0.0451717833072,-28.8242356128,11.1229180654));
#95986=CARTESIAN_POINT('Origin',(-8.52833752869,-28.8242356128,7.18863018236));
#95987=CARTESIAN_POINT('',(-8.74359670241,-25.6742356128,7.39758828372));
#95988=CARTESIAN_POINT('Origin',(-8.52833113701624,-25.6742356128,7.18862868760432));
#95989=CARTESIAN_POINT('',(-8.74359670241,-32.4742356128,7.39758828372));
#95990=CARTESIAN_POINT('',(-8.74359670241,-28.8242356128,7.39758828372));
#95991=CARTESIAN_POINT('Origin',(-8.52833752869,-32.4742356128,7.18863018236));
#95992=CARTESIAN_POINT('Origin',(0.0657457778947,-25.6742356128,-1.15388688513));
#95993=CARTESIAN_POINT('Ctrl Pts',(-8.74359670241,-25.6742356128,7.39758828372));
#95994=CARTESIAN_POINT('Ctrl Pts',(-8.74374103998485,-25.6425708684088,
7.39766117029625));
#95995=CARTESIAN_POINT('Ctrl Pts',(-8.74104638015217,-25.6104477310781,
7.39608617488609));
#95996=CARTESIAN_POINT('Ctrl Pts',(-8.7354771414879,-25.5785226691775,7.39283088384102));
#95997=CARTESIAN_POINT('Ctrl Pts',(-8.73040906011818,-25.5494704375891,
7.38986852562778));
#95998=CARTESIAN_POINT('Ctrl Pts',(-8.72295992326411,-25.5205822157641,
7.38551435667961));
#95999=CARTESIAN_POINT('Ctrl Pts',(-8.71313383437791,-25.4923697627127,
7.37976148770456));
#96000=CARTESIAN_POINT('Ctrl Pts',(-8.70468153488379,-25.4681017039341,
7.37481292962711));
#96001=CARTESIAN_POINT('Ctrl Pts',(-8.69446951826318,-25.4443321822236,
7.36882887446864));
#96002=CARTESIAN_POINT('Ctrl Pts',(-8.68253023474047,-25.4214038181183,
7.3618220078867));
#96003=CARTESIAN_POINT('Ctrl Pts',(-8.67075128078371,-25.3987833531141,
7.35490923471293));
#96004=CARTESIAN_POINT('Ctrl Pts',(-8.65728988089475,-25.3769813332839,
7.34700019558017));
#96005=CARTESIAN_POINT('Ctrl Pts',(-8.64221836816086,-25.3563387689072,
7.33813082388733));
#96006=CARTESIAN_POINT('Ctrl Pts',(-8.63738810977467,-25.3497230481463,
7.33528828526789));
#96007=CARTESIAN_POINT('Ctrl Pts',(-8.63239278338873,-25.3432263804671,
7.33234727894179));
#96008=CARTESIAN_POINT('Ctrl Pts',(-8.62723614053898,-25.3368600324647,
7.32930928634434));
#96009=CARTESIAN_POINT('Ctrl Pts',(-8.62461032881768,-25.333618227342,7.32776231153843));
#96010=CARTESIAN_POINT('Ctrl Pts',(-8.62174269443592,-25.3301699453249,
7.32607232011319));
#96011=CARTESIAN_POINT('Ctrl Pts',(-8.61893519950626,-25.3268883248504,
7.32441745480467));
#96012=CARTESIAN_POINT('Ctrl Pts',(-8.61622925699588,-25.3237254068158,
7.32282244911472));
#96013=CARTESIAN_POINT('Ctrl Pts',(-8.61357983367571,-25.3207168303973,
7.32126046002638));
#96014=CARTESIAN_POINT('Ctrl Pts',(-8.61128536912057,-25.3181634673016,
7.31990782820919));
#96015=CARTESIAN_POINT('Ctrl Pts',(-8.59929941137436,-25.3048250602617,
7.31284187124298));
#96016=CARTESIAN_POINT('Ctrl Pts',(-8.58625654488145,-25.2918288567523,
7.3051443219223));
#96017=CARTESIAN_POINT('Ctrl Pts',(-8.57212647692136,-25.2794305292251,
7.29679382196662));
#96018=CARTESIAN_POINT('Ctrl Pts',(-8.56421120807483,-25.2724853329314,
7.2921161054589));
#96019=CARTESIAN_POINT('Ctrl Pts',(-8.55595540779658,-25.2657282394864,
7.28723384786007));
#96020=CARTESIAN_POINT('Ctrl Pts',(-8.54735934678809,-25.259207553683,7.28214644639095));
#96021=CARTESIAN_POINT('Ctrl Pts',(-8.53238762194693,-25.2478505014786,
7.27328573973973));
#96022=CARTESIAN_POINT('Ctrl Pts',(-8.51638126776519,-25.2372098719035,
7.26380132803334));
#96023=CARTESIAN_POINT('Ctrl Pts',(-8.4993730392377,-25.2275526372549,7.25370744627357));
#96024=CARTESIAN_POINT('Ctrl Pts',(-8.49258297210632,-25.2236972521123,
7.2496777417894));
#96025=CARTESIAN_POINT('Ctrl Pts',(-8.4856336790979,-25.2199987375441,7.24555115737597));
#96026=CARTESIAN_POINT('Ctrl Pts',(-8.4785291407219,-25.2164745981546,7.24132967662755));
#96027=CARTESIAN_POINT('Ctrl Pts',(-8.47646322137075,-25.215449818306,7.24010211780429));
#96028=CARTESIAN_POINT('Ctrl Pts',(-8.47395268214777,-25.2142311697352,
7.23861008609302));
#96029=CARTESIAN_POINT('Ctrl Pts',(-8.47174800998708,-25.2131866536585,
7.23729953917551));
#96030=CARTESIAN_POINT('Ctrl Pts',(-8.47015655922779,-25.2124326658626,
7.2363535160324));
#96031=CARTESIAN_POINT('Ctrl Pts',(-8.46872511422753,-25.2117677253727,
7.2355024531919));
#96032=CARTESIAN_POINT('Ctrl Pts',(-8.46774142009499,-25.2113143951645,
7.23491753911709));
#96033=CARTESIAN_POINT('Ctrl Pts',(-8.45887145042537,-25.2072267168266,
7.22964336909694));
#96034=CARTESIAN_POINT('Ctrl Pts',(-8.44903341435114,-25.2030683007582,
7.22378969990896));
#96035=CARTESIAN_POINT('Ctrl Pts',(-8.43817822310785,-25.1990544953082,
7.21732358184192));
#96036=CARTESIAN_POINT('Ctrl Pts',(-8.42798831593375,-25.1952866846789,
7.21125375392244));
#96037=CARTESIAN_POINT('Ctrl Pts',(-8.41690143527307,-25.1916466537825,
7.20464384498518));
#96038=CARTESIAN_POINT('Ctrl Pts',(-8.40489619864105,-25.188352056581,7.19747738556042));
#96039=CARTESIAN_POINT('Ctrl Pts',(-8.3933971585147,-25.1851963748913,7.19061309733228));
#96040=CARTESIAN_POINT('Ctrl Pts',(-8.38105487920422,-25.1823579194766,
7.18323779100804));
#96041=CARTESIAN_POINT('Ctrl Pts',(-8.36787853944442,-25.1800609103949,
7.17535300675156));
#96042=CARTESIAN_POINT('Ctrl Pts',(-8.35560155307287,-25.1779206840722,
7.16800639983157));
#96043=CARTESIAN_POINT('Ctrl Pts',(-8.34260004343601,-25.1762509850684,
7.16021723063684));
#96044=CARTESIAN_POINT('Ctrl Pts',(-8.32891385869611,-25.1752566994474,
7.15200547873626));
#96045=CARTESIAN_POINT('Ctrl Pts',(-8.31981484133295,-25.174595666274,7.14654604102258));
#96046=CARTESIAN_POINT('Ctrl Pts',(-8.3104138424029,-25.1742336464764,7.14090019430669));
#96047=CARTESIAN_POINT('Ctrl Pts',(-8.30073298506,-25.1742356128,7.13507985462));
#96048=CARTESIAN_POINT('Origin',(0.0657457778947,-25.6742356128,-1.15388688513));
#96049=CARTESIAN_POINT('Ctrl Pts',(-8.30073298506,-25.1742356128,7.13507985462));
#96050=CARTESIAN_POINT('Ctrl Pts',(-8.30073298506,-25.1742356128,7.13507985462));
#96051=CARTESIAN_POINT('Ctrl Pts',(-8.30073298506,-25.1742356128,7.13507985462));
#96052=CARTESIAN_POINT('Ctrl Pts',(-8.30073298506,-25.1742356128,7.13507985462));
#96053=CARTESIAN_POINT('Ctrl Pts',(-8.30073298506,-25.1742356128,7.13507985462));
#96054=CARTESIAN_POINT('Ctrl Pts',(-8.30073298506,-25.1742356128,7.13507985462));
#96055=CARTESIAN_POINT('Ctrl Pts',(-8.47066318824,-25.1741977344,7.23727978366));
#96056=CARTESIAN_POINT('Ctrl Pts',(-8.47614311863,-25.1768387543,7.2136844367));
#96057=CARTESIAN_POINT('Ctrl Pts',(-8.48185215775,-25.1782703319,7.19032767617));
#96058=CARTESIAN_POINT('Ctrl Pts',(-8.48739620589,-25.1782703319,7.16691821418));
#96059=CARTESIAN_POINT('Ctrl Pts',(-8.49276879436,-25.1768387543,7.14348907246));
#96060=CARTESIAN_POINT('Ctrl Pts',(-8.49845441271,-25.1741977344,7.11995353245));
#96061=CARTESIAN_POINT('Ctrl Pts',(-8.64594317412,-25.2739717119,7.34077220006));
#96062=CARTESIAN_POINT('Ctrl Pts',(-8.65593994326,-25.2513426907,7.29347794093));
#96063=CARTESIAN_POINT('Ctrl Pts',(-8.66568265086,-25.2399150938,7.2458632715));
#96064=CARTESIAN_POINT('Ctrl Pts',(-8.67675023931,-25.2399150938,7.1987732799));
#96065=CARTESIAN_POINT('Ctrl Pts',(-8.68923881751,-25.2513426907,7.15177407204));
#96066=CARTESIAN_POINT('Ctrl Pts',(-8.70134895175,-25.2739717119,7.10492272423));
#96067=CARTESIAN_POINT('Ctrl Pts',(-8.74450301091,-25.4754098599,7.39804594503));
#96068=CARTESIAN_POINT('Ctrl Pts',(-8.79148129659,-25.4572913909,7.35218193136));
#96069=CARTESIAN_POINT('Ctrl Pts',(-8.82507005415,-25.4471049939,7.29331988562));
#96070=CARTESIAN_POINT('Ctrl Pts',(-8.84072849584,-25.4471049939,7.22634785159));
#96071=CARTESIAN_POINT('Ctrl Pts',(-8.83671971824,-25.4572913909,7.15869208165));
#96072=CARTESIAN_POINT('Ctrl Pts',(-8.81494581646,-25.4754098599,7.09674839068));
#96073=CARTESIAN_POINT('Ctrl Pts',(-8.74359670241,-25.6742356128,7.39758828372));
#96074=CARTESIAN_POINT('Ctrl Pts',(-8.78879978729,-25.6742356128,7.35102211263));
#96075=CARTESIAN_POINT('Ctrl Pts',(-8.82141102617,-25.6742356128,7.29223268441));
#96076=CARTESIAN_POINT('Ctrl Pts',(-8.83696093696,-25.6742356128,7.22574008976));
#96077=CARTESIAN_POINT('Ctrl Pts',(-8.83380283672,-25.6742356128,7.15858566939));
#96078=CARTESIAN_POINT('Ctrl Pts',(-8.81393818057,-25.6742356128,7.09680280277));
#96079=CARTESIAN_POINT('Origin',(0.0657457778947,-28.8242356128,-1.15388688513));
#96080=CARTESIAN_POINT('Origin',(0.0657457778947,-32.4742356128,-1.15388688513));
#96081=CARTESIAN_POINT('Origin',(-2.68618205273E-16,-26.2742356128,0.729452270839));
#96082=CARTESIAN_POINT('',(-7.90115867216,-26.2742356128,11.6700302451));
#96083=CARTESIAN_POINT('',(-9.22598000443009,-26.274235669025,12.8949853715999));
#96084=CARTESIAN_POINT('',(-9.09620098718,-26.2742356128,12.7749892117));
#96085=CARTESIAN_POINT('',(-11.4035900518,-26.2742356128,8.02142239733));
#96086=CARTESIAN_POINT('Origin',(-3.57591647086E-14,-26.2742356128,0.580061096522));
#96087=CARTESIAN_POINT('',(-12.6175523599,-26.2742356128,9.14387515104));
#96088=CARTESIAN_POINT('',(-12.1305681918,-26.2742356128,8.69360028097));
#96089=CARTESIAN_POINT('',(-12.1784262599,-26.2742356128,9.98548517727));
#96090=CARTESIAN_POINT('Origin',(-10.0415172382,-26.2742356128,8.33514586886));
#96091=CARTESIAN_POINT('Origin',(-2.00838475998E-15,-26.2742356128,0.580061096523));
#96092=CARTESIAN_POINT('Origin',(-12.1305681918,-25.9742356128,8.69360028097));
#96093=CARTESIAN_POINT('',(-12.6068339548724,-26.2541477093856,8.98696687274956));
#96094=CARTESIAN_POINT('',(-12.5655736216481,-25.9742356128984,8.68722821702829));
#96095=CARTESIAN_POINT('Ctrl Pts',(-12.6068339569,-26.2541477174,8.98696686913));
#96096=CARTESIAN_POINT('Ctrl Pts',(-12.602271199,-26.244718344,8.94944232356));
#96097=CARTESIAN_POINT('Ctrl Pts',(-12.5976340417,-26.2325138521,8.912882128));
#96098=CARTESIAN_POINT('Ctrl Pts',(-12.592997343,-26.2175047318,8.87772639907));
#96099=CARTESIAN_POINT('Ctrl Pts',(-12.5863327646,-26.191160811,8.82889624954));
#96100=CARTESIAN_POINT('Ctrl Pts',(-12.5802806769,-26.1586266769,8.78631135752));
#96101=CARTESIAN_POINT('Ctrl Pts',(-12.5784179469,-26.1475421121,8.77337100062));
#96102=CARTESIAN_POINT('Ctrl Pts',(-12.5749839513,-26.1246988195,8.74977888646));
#96103=CARTESIAN_POINT('Ctrl Pts',(-12.5720318185,-26.0996123734,8.72988564417));
#96104=CARTESIAN_POINT('Ctrl Pts',(-12.5707272399,-26.0868775377,8.72117067463));
#96105=CARTESIAN_POINT('Ctrl Pts',(-12.568480527,-26.061055694,8.7062606411));
#96106=CARTESIAN_POINT('Ctrl Pts',(-12.566907631,-26.033788263,8.69593652529));
#96107=CARTESIAN_POINT('Ctrl Pts',(-12.5663159136,-26.020173083,8.69206958938));
#96108=CARTESIAN_POINT('Ctrl Pts',(-12.5658096281,-26.0027489841,8.68876644826));
#96109=CARTESIAN_POINT('Ctrl Pts',(-12.5656142634,-25.9851944876,8.68749304576));
#96110=CARTESIAN_POINT('Ctrl Pts',(-12.5655871714,-25.981542709,8.68731649095));
#96111=CARTESIAN_POINT('Ctrl Pts',(-12.5655736257,-25.9778891268,8.68722821403));
#96112=CARTESIAN_POINT('Ctrl Pts',(-12.5655736197,-25.9742356128,8.68722821523));
#96113=CARTESIAN_POINT('Ctrl Pts',(-12.6175523599,-26.2742356128,9.14387515104));
#96114=CARTESIAN_POINT('Ctrl Pts',(-12.6172775701366,-26.2742356128,9.1204109896849));
#96115=CARTESIAN_POINT('Ctrl Pts',(-12.6163614798089,-26.2727853712571,
9.09667519636503));
#96116=CARTESIAN_POINT('Ctrl Pts',(-12.6148425376273,-26.2699936097463,
9.07290148779792));
#96117=CARTESIAN_POINT('Ctrl Pts',(-12.6143935062009,-26.2691683060127,
9.06587347685785));
#96118=CARTESIAN_POINT('Ctrl Pts',(-12.6138920543085,-26.2682256034708,
9.05884197806186));
#96119=CARTESIAN_POINT('Ctrl Pts',(-12.6133398078109,-26.2671678572136,
9.05181269741915));
#96120=CARTESIAN_POINT('Ctrl Pts',(-12.6116358448962,-26.2639041689815,
9.03012377121524));
#96121=CARTESIAN_POINT('Ctrl Pts',(-12.6094465737123,-26.2595469161348,
9.00845340393981));
#96122=CARTESIAN_POINT('Ctrl Pts',(-12.6068339507173,-26.2541476931765,
8.9869668790268));
#96123=CARTESIAN_POINT('',(-11.607257429,-25.9742356128,7.80115074806));
#96124=CARTESIAN_POINT('Origin',(-11.4035900518,-25.9742356128,8.02142239733));
#96125=CARTESIAN_POINT('',(-12.3599175224,-25.9742356128,8.49707465678));
#96126=CARTESIAN_POINT('Origin',(-13.1616800929,-23.1742356128,9.23839965433));
#96127=CARTESIAN_POINT('',(-12.5655736249,-23.4742356128,8.68722822002));
#96128=CARTESIAN_POINT('',(-11.607257429,-23.4742356128,7.80115074806));
#96129=CARTESIAN_POINT('',(-3.17376422771,-23.4742356128,0.00338173602688));
#96130=CARTESIAN_POINT('',(-12.5655736249,-27.9742356128,8.68722822002));
#96131=CARTESIAN_POINT('',(-11.607257429,-24.7242356128,7.80115074806));
#96132=CARTESIAN_POINT('Origin',(-3.57224253046E-14,-25.9742356128,0.580061096522));
#96133=CARTESIAN_POINT('',(-7.72708272879,-25.9742356128,11.4256993917));
#96134=CARTESIAN_POINT('Origin',(-7.90115867216,-25.9742356128,11.6700302451));
#96135=CARTESIAN_POINT('',(-11.1523495973,-25.9742356128,7.85747657088));
#96136=CARTESIAN_POINT('Origin',(-3.39552160364E-14,-25.9742356128,0.580061096522));
#96137=CARTESIAN_POINT('Origin',(-11.4035900518,-25.9742356128,8.02142239733));
#96138=CARTESIAN_POINT('Origin',(-11.4035900518,-25.9742356128,8.02142239733));
#96139=CARTESIAN_POINT('Origin',(-11.4035900518,-25.9742356128,8.02142239733));
#96140=CARTESIAN_POINT('Origin',(-11.4035900518,-24.7242356128,8.02142239733));
#96141=CARTESIAN_POINT('',(-11.1523495973,-23.4742356128,7.85747657088));
#96142=CARTESIAN_POINT('Origin',(-11.4035900518,-23.4742356128,8.02142239733));
#96143=CARTESIAN_POINT('',(-11.1523495973,-24.7267356128,7.85747657088));
#96144=CARTESIAN_POINT('Origin',(-3.37715190165E-14,-24.4742356128,0.580061096522));
#96145=CARTESIAN_POINT('',(-7.72708272879,-23.4742356128,11.4256993917));
#96146=CARTESIAN_POINT('',(-7.72708272879,-24.7242356128,11.4256993917));
#96147=CARTESIAN_POINT('Origin',(-3.36399067654E-14,-23.4742356128,0.580061096522));
#96148=CARTESIAN_POINT('Origin',(-9.09620098718,-25.9742356128,12.7749892117));
#96149=CARTESIAN_POINT('',(-8.93233349645,-25.9742356128,13.0320605967));
#96150=CARTESIAN_POINT('Ctrl Pts',(-8.93233349645,-25.9742356128,13.0320605967));
#96151=CARTESIAN_POINT('Ctrl Pts',(-8.93233349645,-25.9890568327864,13.0320605967));
#96152=CARTESIAN_POINT('Ctrl Pts',(-8.93344543935767,-26.0038788180243,
13.0315888128132));
#96153=CARTESIAN_POINT('Ctrl Pts',(-8.93564750676488,-26.018509087112,13.0306516936333));
#96154=CARTESIAN_POINT('Ctrl Pts',(-8.93798761514531,-26.034056483703,13.0296558292747));
#96155=CARTESIAN_POINT('Ctrl Pts',(-8.94155846689529,-26.0493869490561,
13.0281345264418));
#96156=CARTESIAN_POINT('Ctrl Pts',(-8.94628177617279,-26.0642939979475,
13.0261107034094));
#96157=CARTESIAN_POINT('Ctrl Pts',(-8.95118424470664,-26.0797664842551,
13.0240101149975));
#96158=CARTESIAN_POINT('Ctrl Pts',(-8.9573276962761,-26.0947828330173,13.0213682483627));
#96159=CARTESIAN_POINT('Ctrl Pts',(-8.96457850957973,-26.1091429358216,
13.0182248593873));
#96160=CARTESIAN_POINT('Ctrl Pts',(-8.97222041741152,-26.1242775941682,
13.014911922228));
#96161=CARTESIAN_POINT('Ctrl Pts',(-8.98109059226912,-26.1386817706972,
13.0110424603843));
#96162=CARTESIAN_POINT('Ctrl Pts',(-8.99099940321383,-26.1521692986935,
13.0066739274749));
#96163=CARTESIAN_POINT('Ctrl Pts',(-8.99289007084896,-26.1547428095621,
13.0058403820747));
#96164=CARTESIAN_POINT('Ctrl Pts',(-8.99481848775625,-26.1572830840322,
13.0049886908228));
#96165=CARTESIAN_POINT('Ctrl Pts',(-8.9967832607327,-26.1597890245021,13.0041192827899));
#96166=CARTESIAN_POINT('Ctrl Pts',(-9.00694335034053,-26.1727475596766,
12.9996234638704));
#96167=CARTESIAN_POINT('Ctrl Pts',(-9.0180777154112,-26.1847862798302,12.9946527566583));
#96168=CARTESIAN_POINT('Ctrl Pts',(-9.02998776274932,-26.1957776113637,
12.9892701764838));
#96169=CARTESIAN_POINT('Ctrl Pts',(-9.03423770921764,-26.1996997259706,
12.9873494723124));
#96170=CARTESIAN_POINT('Ctrl Pts',(-9.03858641957574,-26.203488948385,12.9853763532502));
#96171=CARTESIAN_POINT('Ctrl Pts',(-9.04302503821336,-26.2071411042599,
12.9833537344883));
#96172=CARTESIAN_POINT('Ctrl Pts',(-9.05733192261861,-26.2189130036273,
12.9768342798594));
#96173=CARTESIAN_POINT('Ctrl Pts',(-9.07257322609965,-26.2292583824396,
12.9697996826004));
#96174=CARTESIAN_POINT('Ctrl Pts',(-9.08845512475273,-26.2380574138996,
12.9623517337336));
#96175=CARTESIAN_POINT('Ctrl Pts',(-9.10541279720069,-26.2474524551738,
12.9543992917712));
#96176=CARTESIAN_POINT('Ctrl Pts',(-9.12310069284028,-26.2550849446076,
12.9459753050102));
#96177=CARTESIAN_POINT('Ctrl Pts',(-9.14117969848556,-26.2608654055676,
12.9372106237479));
#96178=CARTESIAN_POINT('Ctrl Pts',(-9.1469184542949,-26.2627002771621,12.9344284814942));
#96179=CARTESIAN_POINT('Ctrl Pts',(-9.15269675618503,-26.2643489154705,
12.9316120798377));
#96180=CARTESIAN_POINT('Ctrl Pts',(-9.15850413396806,-26.2658094227087,
12.928765815912));
#96181=CARTESIAN_POINT('Ctrl Pts',(-9.17863028160214,-26.2708709815385,
12.9189017550375));
#96182=CARTESIAN_POINT('Ctrl Pts',(-9.19910546511503,-26.2736699194545,
12.9086770906661));
#96183=CARTESIAN_POINT('Ctrl Pts',(-9.21950805504983,-26.2741583270136,
12.8982876942716));
#96184=CARTESIAN_POINT('Ctrl Pts',(-9.22166632400898,-26.274209992752,12.8971886616579));
#96185=CARTESIAN_POINT('Ctrl Pts',(-9.22382380187443,-26.2742358404664,
12.8960878053211));
#96186=CARTESIAN_POINT('Ctrl Pts',(-9.22598000443021,-26.2742358377001,
12.8949853715998));
#96187=CARTESIAN_POINT('',(-7.69749129497,-25.9742356128,11.8903018944));
#96188=CARTESIAN_POINT('',(-8.68674913995,-25.9742356128,12.8049886066));
#96189=CARTESIAN_POINT('Origin',(-7.90115867216,-25.9742356128,11.6700302451));
#96190=CARTESIAN_POINT('Origin',(-7.90115867216,-25.9742356128,11.6700302451));
#96191=CARTESIAN_POINT('Origin',(-7.90115867216,-25.9742356128,11.6700302451));
#96192=CARTESIAN_POINT('Origin',(-7.90115867216,-24.7242356128,11.6700302451));
#96193=CARTESIAN_POINT('',(-7.69749129497,-23.4742356128,11.8903018944));
#96194=CARTESIAN_POINT('Origin',(-7.90115867216,-23.4742356128,11.6700302451));
#96195=CARTESIAN_POINT('',(-7.69749129497,-24.7267356128,11.8903018944));
#96196=CARTESIAN_POINT('Origin',(-9.64366495121,-23.1742356128,13.6897712562));
#96197=CARTESIAN_POINT('',(-8.93233349645,-23.4742356128,13.0320605967));
#96198=CARTESIAN_POINT('',(-8.93233349645,-27.9742356128,13.0320605967));
#96199=CARTESIAN_POINT('',(0.393995566301,-23.4742356128,4.40875848149));
#96200=CARTESIAN_POINT('Origin',(-2.68618205273E-16,-26.2742356128,0.729452270839));
#96201=CARTESIAN_POINT('',(11.4035900518,-26.2742356128,8.02142239733));
#96202=CARTESIAN_POINT('',(12.6175523516746,-26.27423561115,9.1438751395306));
#96203=CARTESIAN_POINT('',(12.1305681918,-26.2742356128,8.69360028097));
#96204=CARTESIAN_POINT('',(7.90115867216,-26.2742356128,11.6700302451));
#96205=CARTESIAN_POINT('Origin',(-4.37527704859E-14,-26.2742356128,0.580061096522));
#96206=CARTESIAN_POINT('',(9.22598003749396,-26.2742356128,12.8949854022109));
#96207=CARTESIAN_POINT('',(9.09620098718,-26.2742356128,12.7749892117));
#96208=CARTESIAN_POINT('',(12.1784262599,-26.2742356128,9.98548517727));
#96209=CARTESIAN_POINT('Origin',(1.54432891882E-15,-26.2742356128,0.580061096523));
#96210=CARTESIAN_POINT('Origin',(10.0415172382,-26.2742356128,8.33514586886));
#96211=CARTESIAN_POINT('Origin',(9.09620098718,-25.9742356128,12.7749892117));
#96212=CARTESIAN_POINT('',(8.93233349645,-25.9742356128,13.0320605967));
#96213=CARTESIAN_POINT('Ctrl Pts',(9.22598003749,-26.2742356128,12.8949854022));
#96214=CARTESIAN_POINT('Ctrl Pts',(9.18809325963,-26.2742357357,12.9143563956));
#96215=CARTESIAN_POINT('Ctrl Pts',(9.14988050464,-26.2675847856,12.9333199946));
#96216=CARTESIAN_POINT('Ctrl Pts',(9.112555303,-26.2543622577,12.9512548511));
#96217=CARTESIAN_POINT('Ctrl Pts',(9.03207275784,-26.2094852035,12.9888169711));
#96218=CARTESIAN_POINT('Ctrl Pts',(8.97065416936,-26.1347652578,13.0157974347));
#96219=CARTESIAN_POINT('Ctrl Pts',(8.9450884596,-26.0844303721,13.0266425468));
#96220=CARTESIAN_POINT('Ctrl Pts',(8.93233349646,-26.0293225561,13.0320605967));
#96221=CARTESIAN_POINT('Ctrl Pts',(8.93233349645,-25.9742356128,13.0320605967));
#96222=CARTESIAN_POINT('',(7.69749129497,-25.9742356128,11.8903018944));
#96223=CARTESIAN_POINT('Origin',(7.90115867216,-25.9742356128,11.6700302451));
#96224=CARTESIAN_POINT('',(8.68674913995,-25.9742356128,12.8049886066));
#96225=CARTESIAN_POINT('Origin',(9.64366495121,-23.1742356128,13.6897712562));
#96226=CARTESIAN_POINT('',(8.93233349645,-23.4742356128,13.0320605967));
#96227=CARTESIAN_POINT('',(7.69749129497,-23.4742356128,11.8903018944));
#96228=CARTESIAN_POINT('',(-0.408787176222,-23.4742356128,4.39508187623));
#96229=CARTESIAN_POINT('',(8.93233349645,-27.9742356128,13.0320605967));
#96230=CARTESIAN_POINT('',(7.69749129497,-24.7242356128,11.8903018944));
#96231=CARTESIAN_POINT('Origin',(7.90115867216,-25.9742356128,11.6700302451));
#96232=CARTESIAN_POINT('',(7.72708272879,-25.9742356128,11.4256993917));
#96233=CARTESIAN_POINT('Origin',(7.90115867216,-25.9742356128,11.6700302451));
#96234=CARTESIAN_POINT('Origin',(7.90115867216,-25.9742356128,11.6700302451));
#96235=CARTESIAN_POINT('Origin',(7.90115867216,-24.7242356128,11.6700302451));
#96236=CARTESIAN_POINT('Origin',(7.90115867216,-23.4742356128,11.6700302451));
#96237=CARTESIAN_POINT('',(7.72708272879,-24.7267356128,11.4256993917));
#96238=CARTESIAN_POINT('Origin',(-3.37715190165E-14,-24.4742356128,0.580061096522));
#96239=CARTESIAN_POINT('',(11.1523495973,-25.9742356128,7.85747657088));
#96240=CARTESIAN_POINT('Origin',(-4.37160310819E-14,-25.9742356128,0.580061096522));
#96241=CARTESIAN_POINT('',(11.1523495973,-24.7242356128,7.85747657088));
#96242=CARTESIAN_POINT('Origin',(-4.37160310819E-14,-25.9742356128,0.580061096522));
#96243=CARTESIAN_POINT('Origin',(11.4035900518,-25.9742356128,8.02142239733));
#96244=CARTESIAN_POINT('Origin',(12.1305681918,-25.9742356128,8.69360028097));
#96245=CARTESIAN_POINT('',(12.6068339233452,-26.2541477670181,8.98696693402157));
#96246=CARTESIAN_POINT('Ctrl Pts',(12.6068339453758,-26.254147742503,8.98696694713534));
#96247=CARTESIAN_POINT('Ctrl Pts',(12.609740724862,-26.2601548567899,9.01087250247576));
#96248=CARTESIAN_POINT('Ctrl Pts',(12.6121229018983,-26.2648728878816,9.03500586221848));
#96249=CARTESIAN_POINT('Ctrl Pts',(12.6138969346234,-26.2682287168868,9.05914080022458));
#96250=CARTESIAN_POINT('Ctrl Pts',(12.6144682432968,-26.2693094264984,9.06691320443121));
#96251=CARTESIAN_POINT('Ctrl Pts',(12.6149767251104,-26.2702485354808,9.07468576079593));
#96252=CARTESIAN_POINT('Ctrl Pts',(12.6154203387632,-26.27104275443,9.0824507415481));
#96253=CARTESIAN_POINT('Ctrl Pts',(12.6165958818517,-26.2731473754007,9.10302736131617));
#96254=CARTESIAN_POINT('Ctrl Pts',(12.6173143352754,-26.2742356003459,9.12355292911173));
#96255=CARTESIAN_POINT('Ctrl Pts',(12.6175523434,-26.2742356062,9.14387513582));
#96256=CARTESIAN_POINT('',(12.5655736249,-25.9742356128,8.68722822002));
#96257=CARTESIAN_POINT('Ctrl Pts',(12.5655736249,-25.9742356128,8.68722822002));
#96258=CARTESIAN_POINT('Ctrl Pts',(12.5655736249,-26.0013830382,8.68722822002));
#96259=CARTESIAN_POINT('Ctrl Pts',(12.566321511,-26.0285303094,8.69210196752));
#96260=CARTESIAN_POINT('Ctrl Pts',(12.5678174566,-26.0548464782,8.70184791871));
#96261=CARTESIAN_POINT('Ctrl Pts',(12.5710356589,-26.0928453409,8.7230882249));
#96262=CARTESIAN_POINT('Ctrl Pts',(12.5753569082,-26.1268141304,8.75236686589));
#96263=CARTESIAN_POINT('Ctrl Pts',(12.5769602275,-26.1380192113,8.76332897983));
#96264=CARTESIAN_POINT('Ctrl Pts',(12.5804314507,-26.1598522682,8.78731738945));
#96265=CARTESIAN_POINT('Ctrl Pts',(12.5842177446,-26.179372288,8.81410290281));
#96266=CARTESIAN_POINT('Ctrl Pts',(12.5862189463,-26.1887463534,8.82844547636));
#96267=CARTESIAN_POINT('Ctrl Pts',(12.5914446459,-26.2110918433,8.86644043173));
#96268=CARTESIAN_POINT('Ctrl Pts',(12.5968838275,-26.2294331381,8.90752664916));
#96269=CARTESIAN_POINT('Ctrl Pts',(12.6002199949,-26.2391192104,8.93339289159));
#96270=CARTESIAN_POINT('Ctrl Pts',(12.6035463933,-26.2473540241,8.95993044556));
#96271=CARTESIAN_POINT('Ctrl Pts',(12.6068338975,-26.2541477512,8.98696693379));
#96272=CARTESIAN_POINT('',(11.607257429,-25.9742356128,7.80115074806));
#96273=CARTESIAN_POINT('',(12.3599175224,-25.9742356128,8.49707465678));
#96274=CARTESIAN_POINT('Origin',(11.4035900518,-25.9742356128,8.02142239733));
#96275=CARTESIAN_POINT('Origin',(11.4035900518,-25.9742356128,8.02142239733));
#96276=CARTESIAN_POINT('Origin',(11.4035900518,-25.9742356128,8.02142239733));
#96277=CARTESIAN_POINT('Origin',(11.4035900518,-24.7242356128,8.02142239733));
#96278=CARTESIAN_POINT('',(11.607257429,-23.4742356128,7.80115074806));
#96279=CARTESIAN_POINT('Origin',(11.4035900518,-23.4742356128,8.02142239733));
#96280=CARTESIAN_POINT('',(11.607257429,-24.7267356128,7.80115074806));
#96281=CARTESIAN_POINT('Origin',(13.1616800929,-23.1742356128,9.23839965433));
#96282=CARTESIAN_POINT('',(12.5655736249,-23.4742356128,8.68722822002));
#96283=CARTESIAN_POINT('',(12.5655736249,-27.9742356128,8.68722822002));
#96284=CARTESIAN_POINT('',(3.26251388724,-23.4742356128,0.0854413675889));
#96285=CARTESIAN_POINT('Origin',(3.59394702409,-23.1742356128,-9.19678210318));
#96286=CARTESIAN_POINT('',(3.59394702409,-23.4742356128,-6.76017690617));
#96287=CARTESIAN_POINT('',(3.59394702409,-23.4742356128,-8.84845722572));
#96288=CARTESIAN_POINT('',(3.59394702409,-23.4742356128,3.49118372723));
#96289=CARTESIAN_POINT('',(3.59394702409,-25.9742356128,-8.84845722572));
#96290=CARTESIAN_POINT('',(3.59394702409,-27.9742356128,-8.84845722572));
#96291=CARTESIAN_POINT('',(3.59394702409,-25.9742356128,-6.76017690617));
#96292=CARTESIAN_POINT('',(3.59394702409,-25.9742356128,-8.53006468251));
#96293=CARTESIAN_POINT('',(3.59394702409,-24.7242356128,-6.76017690617));
#96294=CARTESIAN_POINT('Origin',(3.29394702409,-25.9742356128,-8.53006468251));
#96295=CARTESIAN_POINT('',(3.29394702904934,-26.2742356235235,-9.11457262156164));
#96296=CARTESIAN_POINT('Ctrl Pts',(3.59394702409,-25.9742356128,-8.84845722572));
#96297=CARTESIAN_POINT('Ctrl Pts',(3.59394702409,-25.9891777812359,-8.84845722572));
#96298=CARTESIAN_POINT('Ctrl Pts',(3.59282636130367,-26.0041057621838,-8.84954173138075));
#96299=CARTESIAN_POINT('Ctrl Pts',(3.59061714062251,-26.0188096181909,-8.85162544826636));
#96300=CARTESIAN_POINT('Ctrl Pts',(3.58839889516404,-26.0335735401874,-8.85371767723999));
#96301=CARTESIAN_POINT('Ctrl Pts',(3.58508344995202,-26.0481106067043,-8.85681729776892));
#96302=CARTESIAN_POINT('Ctrl Pts',(3.58075367323913,-26.0622239415934,-8.86083796584521));
#96303=CARTESIAN_POINT('Ctrl Pts',(3.57642912096537,-26.076320246907,-8.86485378246217));
#96304=CARTESIAN_POINT('Ctrl Pts',(3.57109322753218,-26.089993101306,-8.86978842524));
#96305=CARTESIAN_POINT('Ctrl Pts',(3.56487248323579,-26.1030742544672,-8.87555586234964));
#96306=CARTESIAN_POINT('Ctrl Pts',(3.55765481797495,-26.1182517606055,-8.88224757454468));
#96307=CARTESIAN_POINT('Ctrl Pts',(3.54924347424757,-26.1326432914629,-8.89002062963786));
#96308=CARTESIAN_POINT('Ctrl Pts',(3.53984316918362,-26.146093361616,-8.89865624715161));
#96309=CARTESIAN_POINT('Ctrl Pts',(3.53668269397923,-26.1506154077546,-8.90155962686548));
#96310=CARTESIAN_POINT('Ctrl Pts',(3.53341058644801,-26.1550314449506,-8.90456050810524));
#96311=CARTESIAN_POINT('Ctrl Pts',(3.53003502635557,-26.1593368153522,-8.90765057629916));
#96312=CARTESIAN_POINT('Ctrl Pts',(3.51871962783149,-26.1737690815695,-8.91800896190725));
#96313=CARTESIAN_POINT('Ctrl Pts',(3.50623880909602,-26.1869592376811,-8.92936841135558));
#96314=CARTESIAN_POINT('Ctrl Pts',(3.49286605549448,-26.1988045753596,-8.94144488155553));
#96315=CARTESIAN_POINT('Ctrl Pts',(3.48991429740156,-26.2014191880563,-8.9441105119641));
#96316=CARTESIAN_POINT('Ctrl Pts',(3.48691903007162,-26.2039684749351,-8.94681107663402));
#96317=CARTESIAN_POINT('Ctrl Pts',(3.48388309834292,-26.206451649493,-8.9495435208975));
#96318=CARTESIAN_POINT('Ctrl Pts',(3.46840744838,-26.2191096219669,-8.96347214470841));
#96319=CARTESIAN_POINT('Ctrl Pts',(3.45187175831933,-26.2300517991658,-8.97823314593818));
#96320=CARTESIAN_POINT('Ctrl Pts',(3.43460513144561,-26.2392173043093,-8.99349336029075));
#96321=CARTESIAN_POINT('Ctrl Pts',(3.43258777506472,-26.240288161427,-8.99527629629922));
#96322=CARTESIAN_POINT('Ctrl Pts',(3.43056040052516,-26.2413348070526,-8.99706604684286));
#96323=CARTESIAN_POINT('Ctrl Pts',(3.42852350169025,-26.2423571741797,-8.99886208056783));
#96324=CARTESIAN_POINT('Ctrl Pts',(3.40860261656626,-26.2523559319703,-9.01642730319981));
#96325=CARTESIAN_POINT('Ctrl Pts',(3.38776498003673,-26.2600351445809,-9.03460259281844));
#96326=CARTESIAN_POINT('Ctrl Pts',(3.36643491858791,-26.2653464252946,-9.05297755580061));
#96327=CARTESIAN_POINT('Ctrl Pts',(3.34271095817104,-26.2712537975596,-9.07341476342406));
#96328=CARTESIAN_POINT('Ctrl Pts',(3.31836689102333,-26.2742356128,-9.09410743824334));
#96329=CARTESIAN_POINT('Ctrl Pts',(3.29394702409,-26.2742356128,-9.11457260736));
#96330=CARTESIAN_POINT('',(3.29394702409,-26.2742356128,-6.76017690617));
#96331=CARTESIAN_POINT('',(3.29394702409,-26.2742356128,-8.43254284669));
#96332=CARTESIAN_POINT('Origin',(3.29394702409,-25.9742356128,-6.76017690617));
#96333=CARTESIAN_POINT('Origin',(-2.68618205273E-16,-26.2742356128,0.729452270839));
#96334=CARTESIAN_POINT('',(-3.29394702409,-26.2742356128,-9.11457265181));
#96335=CARTESIAN_POINT('',(-3.29394702409,-26.2742356128,-6.76017690617));
#96336=CARTESIAN_POINT('',(-3.29394702409,-26.2742356128,-8.53006468251));
#96337=CARTESIAN_POINT('',(-0.728014505146,-26.2742356128,-7.7348985358));
#96338=CARTESIAN_POINT('Origin',(2.84607155346,-26.2742356128,5.53854202767));
#96339=CARTESIAN_POINT('',(0.728014505146,-26.2742356128,-7.7348985358));
#96340=CARTESIAN_POINT('Origin',(1.52421666678E-14,-26.2742356128,-5.03119831567));
#96341=CARTESIAN_POINT('Origin',(-2.84607155346,-26.2742356128,5.53854202767));
#96342=CARTESIAN_POINT('',(0.582701491963,-26.2742356128,-9.97458510214));
#96343=CARTESIAN_POINT('Origin',(-2.84607155346,-26.2742356128,5.53854202767));
#96344=CARTESIAN_POINT('',(-0.582701491963,-26.2742356128,-9.97458510214));
#96345=CARTESIAN_POINT('Origin',(2.04045674064E-15,-26.2742356128,-7.33821278943));
#96346=CARTESIAN_POINT('Origin',(2.84607155346,-26.2742356128,5.53854202767));
#96347=CARTESIAN_POINT('Origin',(3.29394702409,-24.7242356128,-6.76017690617));
#96348=CARTESIAN_POINT('',(3.15994605614,-23.4742356128,-6.49176725547));
#96349=CARTESIAN_POINT('Origin',(3.29394702409,-23.4742356128,-6.76017690617));
#96350=CARTESIAN_POINT('',(3.15994605614,-25.9742356128,-6.49176725547));
#96351=CARTESIAN_POINT('Origin',(3.29394702409,-25.9742356128,-6.76017690617));
#96352=CARTESIAN_POINT('',(3.15994605614,-24.7267356128,-6.49176725547));
#96353=CARTESIAN_POINT('Origin',(3.29394702409,-25.9742356128,-6.76017690617));
#96354=CARTESIAN_POINT('Origin',(3.29394702409,-25.9742356128,-6.76017690617));
#96355=CARTESIAN_POINT('Origin',(-2.84607155346,-25.9742356128,5.53854202767));
#96356=CARTESIAN_POINT('',(0.650012951023,-25.9742356128,-7.44521636936));
#96357=CARTESIAN_POINT('Origin',(-2.84607155346,-25.9742356128,5.53854202767));
#96358=CARTESIAN_POINT('Origin',(0.728014505146,-25.9742356128,-7.7348985358));
#96359=CARTESIAN_POINT('Origin',(-2.84607155346,-24.4742356128,5.53854202767));
#96360=CARTESIAN_POINT('',(0.650012951023,-23.4742356128,-7.44521636936));
#96361=CARTESIAN_POINT('',(0.650012951023,-24.7267356128,-7.44521636936));
#96362=CARTESIAN_POINT('Origin',(-2.84607155346,-23.4742356128,5.53854202767));
#96363=CARTESIAN_POINT('Origin',(1.52789060718E-14,-25.9742356128,-5.03119831567));
#96364=CARTESIAN_POINT('',(-0.650012951023,-25.9742356128,-7.44521636936));
#96365=CARTESIAN_POINT('Origin',(1.55009506767E-14,-25.9742356128,-5.03119831567));
#96366=CARTESIAN_POINT('Origin',(-0.728014505146,-25.9742356128,-7.7348985358));
#96367=CARTESIAN_POINT('Origin',(1.56846476966E-14,-24.4742356128,-5.03119831567));
#96368=CARTESIAN_POINT('',(-0.650012951023,-23.4742356128,-7.44521636936));
#96369=CARTESIAN_POINT('',(-0.650012951023,-24.7267356128,-7.44521636936));
#96370=CARTESIAN_POINT('Origin',(1.60291569814E-14,-23.4742356128,-5.03119831567));
#96371=CARTESIAN_POINT('Origin',(2.84607155346,-25.9742356128,5.53854202767));
#96372=CARTESIAN_POINT('',(-3.15994605614,-25.9742356128,-6.49176725547));
#96373=CARTESIAN_POINT('Origin',(2.84607155346,-25.9742356128,5.53854202767));
#96374=CARTESIAN_POINT('Origin',(-3.29394702409,-25.9742356128,-6.76017690617));
#96375=CARTESIAN_POINT('Origin',(2.84607155346,-24.4742356128,5.53854202767));
#96376=CARTESIAN_POINT('',(-3.15994605614,-23.4742356128,-6.49176725547));
#96377=CARTESIAN_POINT('',(-3.15994605614,-24.7242356128,-6.49176725547));
#96378=CARTESIAN_POINT('Origin',(2.84607155346,-23.4742356128,5.53854202767));
#96379=CARTESIAN_POINT('Origin',(-3.29394702409,-25.9742356128,-8.53006468251));
#96380=CARTESIAN_POINT('',(-3.59394702409,-25.9742356128,-8.84845722568));
#96381=CARTESIAN_POINT('Ctrl Pts',(-3.29394702409,-26.2742356128,-9.11457265181));
#96382=CARTESIAN_POINT('Ctrl Pts',(-3.30720704925,-26.2742356128,-9.1034600928));
#96383=CARTESIAN_POINT('Ctrl Pts',(-3.32044878803,-26.2735029951,-9.09229236737));
#96384=CARTESIAN_POINT('Ctrl Pts',(-3.33363103946,-26.2720418371,-9.0811040513));
#96385=CARTESIAN_POINT('Ctrl Pts',(-3.37291095474,-26.2654802717,-9.04755646576));
#96386=CARTESIAN_POINT('Ctrl Pts',(-3.41093514101,-26.2524263623,-9.01447547571));
#96387=CARTESIAN_POINT('Ctrl Pts',(-3.43541561624,-26.240866543,-8.99291668586));
#96388=CARTESIAN_POINT('Ctrl Pts',(-3.46997146608,-26.219486164,-8.96214399258));
#96389=CARTESIAN_POINT('Ctrl Pts',(-3.50089098302,-26.1920639406,-8.9342126496));
#96390=CARTESIAN_POINT('Ctrl Pts',(-3.51056331552,-26.1824628447,-8.9254339626));
#96391=CARTESIAN_POINT('Ctrl Pts',(-3.52866003196,-26.1623189549,-8.90893921363));
#96392=CARTESIAN_POINT('Ctrl Pts',(-3.54462619729,-26.1398775942,-8.89427266222));
#96393=CARTESIAN_POINT('Ctrl Pts',(-3.55192119026,-26.1282916208,-8.88754705425));
#96394=CARTESIAN_POINT('Ctrl Pts',(-3.56506382466,-26.1044831752,-8.87539313986));
#96395=CARTESIAN_POINT('Ctrl Pts',(-3.57557442716,-26.0789471162,-8.86562061849));
#96396=CARTESIAN_POINT('Ctrl Pts',(-3.58006361288,-26.0660011409,-8.8614367189));
#96397=CARTESIAN_POINT('Ctrl Pts',(-3.58736522612,-26.0402449423,-8.8546203727));
#96398=CARTESIAN_POINT('Ctrl Pts',(-3.59178640039,-26.0136034223,-8.85048167902));
#96399=CARTESIAN_POINT('Ctrl Pts',(-3.59322678156,-26.0005307527,-8.8491320671));
#96400=CARTESIAN_POINT('Ctrl Pts',(-3.59394702493,-25.9873832723,-8.84845722511));
#96401=CARTESIAN_POINT('Ctrl Pts',(-3.59394702409,-25.9742356128,-8.84845722568));
#96402=CARTESIAN_POINT('',(-3.59394702409,-25.9742356128,-6.76017690617));
#96403=CARTESIAN_POINT('',(-3.59394702409,-25.9742356128,-7.89543489424));
#96404=CARTESIAN_POINT('Origin',(-3.29394702409,-25.9742356128,-6.76017690617));
#96405=CARTESIAN_POINT('Origin',(-3.29394702409,-25.9742356128,-6.76017690617));
#96406=CARTESIAN_POINT('Origin',(-3.29394702409,-25.9742356128,-6.76017690617));
#96407=CARTESIAN_POINT('Origin',(-3.29394702409,-24.7242356128,-6.76017690617));
#96408=CARTESIAN_POINT('',(-3.59394702409,-23.4742356128,-6.76017690617));
#96409=CARTESIAN_POINT('Origin',(-3.29394702409,-23.4742356128,-6.76017690617));
#96410=CARTESIAN_POINT('',(-3.59394702409,-24.7267356128,-6.76017690617));
#96411=CARTESIAN_POINT('Origin',(-3.59394702409,-23.1742356128,-9.19678210318));
#96412=CARTESIAN_POINT('',(-3.59394702409,-23.4742356128,-8.84845722572));
#96413=CARTESIAN_POINT('',(-3.59394702409,-27.9742356128,-8.84845722572));
#96414=CARTESIAN_POINT('',(-3.59394702409,-23.4742356128,3.49118372723));
#96415=CARTESIAN_POINT('Origin',(-1.02789922074E-15,-32.4742356128,0.729452270839));
#96416=CARTESIAN_POINT('',(12.4158605957,-32.4742356128,10.1688562115));
#96417=CARTESIAN_POINT('',(-12.4158605957,-32.4742356128,10.1688562115));
#96418=CARTESIAN_POINT('Origin',(-9.91308936055E-16,-32.4742356128,0.580061096523));
#96419=CARTESIAN_POINT('',(-12.9732844032,-32.4742356128,8.9713386779));
#96420=CARTESIAN_POINT('Origin',(-10.0415172382,-32.4742356128,8.33514586886));
#96421=CARTESIAN_POINT('',(-0.647446102181,-32.4742356128,-10.2675153591));
#96422=CARTESIAN_POINT('Origin',(2.84607155346,-32.4742356128,5.53854202767));
#96423=CARTESIAN_POINT('',(0.647446102181,-32.4742356128,-10.2675153591));
#96424=CARTESIAN_POINT('Origin',(9.48108817785E-16,-32.4742356128,-7.33821278943));
#96425=CARTESIAN_POINT('',(12.9732844032,-32.4742356128,8.9713386779));
#96426=CARTESIAN_POINT('Origin',(-2.84607155346,-32.4742356128,5.53854202767));
#96427=CARTESIAN_POINT('Origin',(10.0415172382,-32.4742356128,8.33514586886));
#96428=CARTESIAN_POINT('Origin',(-3.3774316049,-23.4742356128,-0.216889913236));
#96429=CARTESIAN_POINT('',(-12.7692410021,-23.1742356128,8.46695657076));
#96430=CARTESIAN_POINT('Origin',(-12.7692410021,-23.4742356128,8.46695657076));
#96431=CARTESIAN_POINT('',(-11.8109248062,-23.1742356128,7.5808790988));
#96432=CARTESIAN_POINT('Origin',(-11.8109248062,-23.4742356128,7.5808790988));
#96433=CARTESIAN_POINT('',(-12.2900829041,-23.1742356128,8.02391783478));
#96434=CARTESIAN_POINT('Origin',(-11.4035900518,-23.4742356128,8.02142239733));
#96435=CARTESIAN_POINT('',(-10.9011091428,-23.1742356128,7.69353074443));
#96436=CARTESIAN_POINT('Origin',(-10.9011091428,-23.4742356128,7.69353074443));
#96437=CARTESIAN_POINT('Origin',(-11.4035900518,-23.1742356128,8.02142239733));
#96438=CARTESIAN_POINT('Origin',(-3.36399067654E-14,-23.4742356128,0.580061096522));
#96439=CARTESIAN_POINT('',(-7.55300678542,-23.1742356128,11.1813685383));
#96440=CARTESIAN_POINT('Origin',(-7.55300678542,-23.4742356128,11.1813685383));
#96441=CARTESIAN_POINT('Origin',(-3.36841676743E-14,-23.1742356128,0.580061096522));
#96442=CARTESIAN_POINT('Origin',(-7.90115867216,-23.4742356128,11.6700302451));
#96443=CARTESIAN_POINT('',(-7.49382391778,-23.1742356128,12.1105735437));
#96444=CARTESIAN_POINT('Origin',(-7.49382391778,-23.4742356128,12.1105735437));
#96445=CARTESIAN_POINT('Origin',(-7.90115867216,-23.1742356128,11.6700302451));
#96446=CARTESIAN_POINT('Origin',(0.59766294349,-23.4742356128,4.62903013076));
#96447=CARTESIAN_POINT('',(-8.72866611926,-23.1742356128,13.252332246));
#96448=CARTESIAN_POINT('Origin',(-8.72866611926,-23.4742356128,13.252332246));
#96449=CARTESIAN_POINT('',(-8.11124501852,-23.1742356128,12.6814528948));
#96450=CARTESIAN_POINT('Origin',(-0.612454553411,-23.4742356128,4.61535352549));
#96451=CARTESIAN_POINT('',(8.72866611926,-23.1742356128,13.252332246));
#96452=CARTESIAN_POINT('Origin',(8.72866611926,-23.4742356128,13.252332246));
#96453=CARTESIAN_POINT('',(7.49382391778,-23.1742356128,12.1105735437));
#96454=CARTESIAN_POINT('Origin',(7.49382391778,-23.4742356128,12.1105735437));
#96455=CARTESIAN_POINT('',(8.11124501852,-23.1742356128,12.6814528948));
#96456=CARTESIAN_POINT('Origin',(7.90115867216,-23.4742356128,11.6700302451));
#96457=CARTESIAN_POINT('Origin',(7.90115867216,-23.1742356128,11.6700302451));
#96458=CARTESIAN_POINT('Origin',(11.4035900518,-23.4742356128,8.02142239733));
#96459=CARTESIAN_POINT('',(11.8109248062,-23.1742356128,7.5808790988));
#96460=CARTESIAN_POINT('Origin',(11.8109248062,-23.4742356128,7.5808790988));
#96461=CARTESIAN_POINT('Origin',(11.4035900518,-23.1742356128,8.02142239733));
#96462=CARTESIAN_POINT('Origin',(3.46618126442,-23.4742356128,-0.134830281674));
#96463=CARTESIAN_POINT('',(12.7692410021,-23.1742356128,8.46695657076));
#96464=CARTESIAN_POINT('Origin',(12.7692410021,-23.4742356128,8.46695657076));
#96465=CARTESIAN_POINT('',(12.2900829041,-23.1742356128,8.02391783478));
#96466=CARTESIAN_POINT('Origin',(3.89394702409,-23.4742356128,3.49118372723));
#96467=CARTESIAN_POINT('',(3.89394702409,-23.1742356128,-6.76017690617));
#96468=CARTESIAN_POINT('Origin',(3.89394702409,-23.4742356128,-6.76017690617));
#96469=CARTESIAN_POINT('',(3.89394702409,-23.1742356128,-8.84845722572));
#96470=CARTESIAN_POINT('',(3.89394702409,-23.1742356128,-7.80431706594));
#96471=CARTESIAN_POINT('Origin',(3.89394702409,-23.4742356128,-8.84845722572));
#96472=CARTESIAN_POINT('Origin',(3.29394702409,-23.4742356128,-6.76017690617));
#96473=CARTESIAN_POINT('',(3.02594508819,-23.1742356128,-6.22335760477));
#96474=CARTESIAN_POINT('Origin',(3.02594508819,-23.4742356128,-6.22335760477));
#96475=CARTESIAN_POINT('Origin',(3.29394702409,-23.1742356128,-6.76017690617));
#96476=CARTESIAN_POINT('Origin',(-2.84607155346,-23.4742356128,5.53854202767));
#96477=CARTESIAN_POINT('',(0.572011396901,-23.1742356128,-7.15553420291));
#96478=CARTESIAN_POINT('Origin',(0.572011396901,-23.4742356128,-7.15553420291));
#96479=CARTESIAN_POINT('Origin',(-2.84607155346,-23.1742356128,5.53854202767));
#96480=CARTESIAN_POINT('Origin',(1.60291569814E-14,-23.4742356128,-5.03119831567));
#96481=CARTESIAN_POINT('',(-0.572011396901,-23.1742356128,-7.15553420291));
#96482=CARTESIAN_POINT('Origin',(-0.572011396901,-23.4742356128,-7.15553420291));
#96483=CARTESIAN_POINT('Origin',(1.6213480319E-14,-23.1742356128,-5.03119831567));
#96484=CARTESIAN_POINT('Origin',(2.84607155346,-23.4742356128,5.53854202767));
#96485=CARTESIAN_POINT('',(-3.02594508819,-23.1742356128,-6.22335760477));
#96486=CARTESIAN_POINT('Origin',(-3.02594508819,-23.4742356128,-6.22335760477));
#96487=CARTESIAN_POINT('Origin',(2.84607155346,-23.1742356128,5.53854202767));
#96488=CARTESIAN_POINT('Origin',(-3.29394702409,-23.4742356128,-6.76017690617));
#96489=CARTESIAN_POINT('',(-3.89394702409,-23.1742356128,-6.76017690617));
#96490=CARTESIAN_POINT('Origin',(-3.89394702409,-23.4742356128,-6.76017690617));
#96491=CARTESIAN_POINT('Origin',(-3.29394702409,-23.1742356128,-6.76017690617));
#96492=CARTESIAN_POINT('Origin',(-3.89394702409,-23.4742356128,3.49118372723));
#96493=CARTESIAN_POINT('',(-3.89394702409,-23.1742356128,-8.84845722572));
#96494=CARTESIAN_POINT('Origin',(-3.89394702409,-23.4742356128,-8.84845722572));
#96495=CARTESIAN_POINT('',(-3.89394702409,-23.1742356128,-7.80431706594));
#96496=CARTESIAN_POINT('Origin',(1.11022302463E-16,-23.1742356128,0.729452270839));
#96497=CARTESIAN_POINT('Origin',(-2.84607155346,-23.1742356128,5.53854202767));
#96498=CARTESIAN_POINT('Origin',(2.84607155346,-23.1742356128,5.53854202767));
#96499=CARTESIAN_POINT('Origin',(5.47668310535E-15,-23.1742356128,0.580061096523));
#96500=CARTESIAN_POINT('Origin',(12.7692410021,-23.4742356128,8.46695657076));
#96501=CARTESIAN_POINT('',(13.0641007993,-23.4742356128,8.52225304435));
#96502=CARTESIAN_POINT('Origin',(12.7692410021,-23.4742356128,8.46695657076));
#96503=CARTESIAN_POINT('Origin',(12.7692410021,-23.4742356128,8.46695657076));
#96504=CARTESIAN_POINT('',(12.8356936926466,-23.1882133320383,8.52839999861852));
#96505=CARTESIAN_POINT('Origin',(12.7692410021,-23.4742356128,8.46695657076));
#96506=CARTESIAN_POINT('Origin',(3.89394702409,-23.4742356128,-8.84845722572));
#96507=CARTESIAN_POINT('',(4.02121700373,-23.4742356128,-9.12012310927));
#96508=CARTESIAN_POINT('Origin',(3.89394702409,-23.4742356128,-8.84845722572));
#96509=CARTESIAN_POINT('',(3.89394702409,-23.4742356128,-9.14845722572));
#96510=CARTESIAN_POINT('Origin',(3.89394702409,-23.4742356128,-8.84845722572));
#96511=CARTESIAN_POINT('',(3.89394702409,-23.4034955956937,-9.13999770314947));
#96512=CARTESIAN_POINT('Origin',(3.89394702409,-23.4742356128,-8.84845722572));
#96513=CARTESIAN_POINT('Origin',(3.89394702409,-23.4742356128,-8.84845722572));
#96514=CARTESIAN_POINT('Origin',(-2.84607155346,-23.4742356128,5.53854202767));
#96515=CARTESIAN_POINT('Origin',(-2.84607155346,-23.4742356128,5.53854202767));
#96516=CARTESIAN_POINT('Ctrl Pts',(12.5655736249,-25.9742356128,8.68722822002));
#96517=CARTESIAN_POINT('Ctrl Pts',(12.6125281896,-25.9742356128,8.73064330802));
#96518=CARTESIAN_POINT('Ctrl Pts',(12.6710473074,-25.9742356128,8.76156013382));
#96519=CARTESIAN_POINT('Ctrl Pts',(12.7367182007,-25.9742356128,8.77578329688));
#96520=CARTESIAN_POINT('Ctrl Pts',(12.8688414275,-25.9742356128,8.7679322687));
#96521=CARTESIAN_POINT('Ctrl Pts',(12.9795662208,-25.9742356128,8.69541878151));
#96522=CARTESIAN_POINT('Ctrl Pts',(13.0237889047,-25.9742356128,8.64482907085));
#96523=CARTESIAN_POINT('Ctrl Pts',(13.0523134365,-25.9742356128,8.58510731301));
#96524=CARTESIAN_POINT('Ctrl Pts',(13.0641007993,-25.9742356128,8.52225304435));
#96525=CARTESIAN_POINT('Ctrl Pts',(12.5655736249,-26.0156901503,8.68722822002));
#96526=CARTESIAN_POINT('Ctrl Pts',(12.6125281896,-26.0101392553,8.73064330802));
#96527=CARTESIAN_POINT('Ctrl Pts',(12.6710473074,-26.0069407531,8.76156013382));
#96528=CARTESIAN_POINT('Ctrl Pts',(12.7367182007,-26.0066348021,8.77578329688));
#96529=CARTESIAN_POINT('Ctrl Pts',(12.8688414275,-26.0118680127,8.7679322687));
#96530=CARTESIAN_POINT('Ctrl Pts',(12.9795662208,-26.0268285906,8.69541878151));
#96531=CARTESIAN_POINT('Ctrl Pts',(13.0237889047,-26.0362726342,8.64482907085));
#96532=CARTESIAN_POINT('Ctrl Pts',(13.0523134365,-26.0467091655,8.58510731301));
#96533=CARTESIAN_POINT('Ctrl Pts',(13.0641007993,-26.0571446878,8.52225304435));
#96534=CARTESIAN_POINT('Ctrl Pts',(12.5673190764,-26.0571611787,8.69860099886));
#96535=CARTESIAN_POINT('Ctrl Pts',(12.6147839704,-26.0460087182,8.73985554978));
#96536=CARTESIAN_POINT('Ctrl Pts',(12.6733623751,-26.039567434,8.7690990864));
#96537=CARTESIAN_POINT('Ctrl Pts',(12.7386568777,-26.038925371,8.78241060374));
#96538=CARTESIAN_POINT('Ctrl Pts',(12.8694529589,-26.0493679679,8.77449484918));
#96539=CARTESIAN_POINT('Ctrl Pts',(12.9783519251,-26.079330936,8.70501235676));
#96540=CARTESIAN_POINT('Ctrl Pts',(13.0216997747,-26.0982548482,8.65661829968));
#96541=CARTESIAN_POINT('Ctrl Pts',(13.0495520754,-26.1191713964,8.59946132904));
#96542=CARTESIAN_POINT('Ctrl Pts',(13.0609230524,-26.1400859332,8.53920080258));
#96543=CARTESIAN_POINT('Ctrl Pts',(12.5708020939,-26.0955898119,8.72129739555));
#96544=CARTESIAN_POINT('Ctrl Pts',(12.6192645611,-26.0807374464,8.75832152472));
#96545=CARTESIAN_POINT('Ctrl Pts',(12.6779437588,-26.072572542,8.78430344011));
#96546=CARTESIAN_POINT('Ctrl Pts',(12.7424767707,-26.0724883755,8.79585386213));
#96547=CARTESIAN_POINT('Ctrl Pts',(12.8706190688,-26.0884772207,8.78786373285));
#96548=CARTESIAN_POINT('Ctrl Pts',(12.9758918612,-26.1312493712,8.7243679619));
#96549=CARTESIAN_POINT('Ctrl Pts',(13.0175064499,-26.1580067779,8.68029613171));
#96550=CARTESIAN_POINT('Ctrl Pts',(13.0440297261,-26.1874767751,8.62818300551));
#96551=CARTESIAN_POINT('Ctrl Pts',(13.0545801486,-26.2169441965,8.57302387625));
#96552=CARTESIAN_POINT('Ctrl Pts',(12.5794459662,-26.1608028821,8.77948305254));
#96553=CARTESIAN_POINT('Ctrl Pts',(12.6296141113,-26.142770098,8.80804311593));
#96554=CARTESIAN_POINT('Ctrl Pts',(12.6879356315,-26.1342515256,8.82779050493));
#96555=CARTESIAN_POINT('Ctrl Pts',(12.7502196423,-26.1368008678,8.83632815809));
#96556=CARTESIAN_POINT('Ctrl Pts',(12.8715106952,-26.1635294701,8.82947566206));
#96557=CARTESIAN_POINT('Ctrl Pts',(12.9681422326,-26.2258042788,8.77959930959));
#96558=CARTESIAN_POINT('Ctrl Pts',(13.0057211957,-26.2639659335,8.74503645745));
#96559=CARTESIAN_POINT('Ctrl Pts',(13.0291938131,-26.3056693816,8.70391024913));
#96560=CARTESIAN_POINT('Ctrl Pts',(13.037895068,-26.3473699802,8.65987870015));
#96561=CARTESIAN_POINT('Ctrl Pts',(12.5904350881,-26.208935598,8.85843870903));
#96562=CARTESIAN_POINT('Ctrl Pts',(12.6413857281,-26.193073841,8.8794045658));
#96563=CARTESIAN_POINT('Ctrl Pts',(12.6981640128,-26.1879369487,8.89407137053));
#96564=CARTESIAN_POINT('Ctrl Pts',(12.7569188608,-26.1947558682,8.90085098743));
#96565=CARTESIAN_POINT('Ctrl Pts',(12.8688909488,-26.2311660085,8.89755364806));
#96566=CARTESIAN_POINT('Ctrl Pts',(12.9549222972,-26.3046245246,8.86341292137));
#96567=CARTESIAN_POINT('Ctrl Pts',(12.9876969697,-26.3485480349,8.83930386397));
#96568=CARTESIAN_POINT('Ctrl Pts',(13.0075899899,-26.3960930753,8.81007138323));
#96569=CARTESIAN_POINT('Ctrl Pts',(13.0141520182,-26.4436357412,8.77811343457));
#96570=CARTESIAN_POINT('Ctrl Pts',(12.5959177038,-26.2279044079,8.8994052873));
#96571=CARTESIAN_POINT('Ctrl Pts',(12.646874483,-26.2139581927,8.91740539891));
#96572=CARTESIAN_POINT('Ctrl Pts',(12.7025812771,-26.2109800213,8.93027129181));
#96573=CARTESIAN_POINT('Ctrl Pts',(12.7593862349,-26.2199914752,8.93670805691));
#96574=CARTESIAN_POINT('Ctrl Pts',(12.8665236815,-26.2605801567,8.93574094902));
#96575=CARTESIAN_POINT('Ctrl Pts',(12.9473429566,-26.3377051372,8.90908651151));
#96576=CARTESIAN_POINT('Ctrl Pts',(12.9777936856,-26.3833026499,8.88980176083));
#96577=CARTESIAN_POINT('Ctrl Pts',(12.9959671442,-26.4324389347,8.86600393028));
#96578=CARTESIAN_POINT('Ctrl Pts',(13.0015068071,-26.4815731476,8.83957127532));
#96579=CARTESIAN_POINT('Ctrl Pts',(12.6014286433,-26.242977575,8.94251399615));
#96580=CARTESIAN_POINT('Ctrl Pts',(12.6520390535,-26.231349296,8.95817349548));
#96581=CARTESIAN_POINT('Ctrl Pts',(12.7063906649,-26.2306858466,8.96978929718));
#96582=CARTESIAN_POINT('Ctrl Pts',(12.7610505563,-26.2417976368,8.97629178839));
#96583=CARTESIAN_POINT('Ctrl Pts',(12.8631123569,-26.2859464251,8.9781294015));
#96584=CARTESIAN_POINT('Ctrl Pts',(12.9386865297,-26.365438177,8.95883155382));
#96585=CARTESIAN_POINT('Ctrl Pts',(12.9668261506,-26.4119362845,8.94417302517));
#96586=CARTESIAN_POINT('Ctrl Pts',(12.9832936343,-26.4618287729,8.92554423077));
#96587=CARTESIAN_POINT('Ctrl Pts',(12.9878157168,-26.5117194744,8.90437404317));
#96588=CARTESIAN_POINT('Ctrl Pts',(12.606833891,-26.2541478224,8.98696694086));
#96589=CARTESIAN_POINT('Ctrl Pts',(12.6567634559,-26.2450231646,9.00090329165));
#96590=CARTESIAN_POINT('Ctrl Pts',(12.7095130326,-26.2466650943,9.01179180097));
#96591=CARTESIAN_POINT('Ctrl Pts',(12.7618789354,-26.2596853008,9.01872934487));
#96592=CARTESIAN_POINT('Ctrl Pts',(12.8587193341,-26.3067070888,9.02376000338));
#96593=CARTESIAN_POINT('Ctrl Pts',(12.9290963448,-26.3874138436,9.01159791107));
#96594=CARTESIAN_POINT('Ctrl Pts',(12.954969534,-26.4341563453,9.00132365176));
#96595=CARTESIAN_POINT('Ctrl Pts',(12.969765568,-26.4841089383,8.98755447916));
#96596=CARTESIAN_POINT('Ctrl Pts',(12.9732844047,-26.5340600059,8.97133867828));
#96597=CARTESIAN_POINT('',(13.0641007993,-25.9742356128,8.52225304435));
#96598=CARTESIAN_POINT('Origin',(12.7692410021,-25.9742356128,8.46695657076));
#96599=CARTESIAN_POINT('',(12.9732844000412,-26.5340599311358,8.97133869610266));
#96600=CARTESIAN_POINT('Origin',(12.6801075664532,-26.5340600708344,8.90771940054616));
#96601=CARTESIAN_POINT('Ctrl Pts',(13.0641007993,-25.9742356128,8.52225304435));
#96602=CARTESIAN_POINT('Ctrl Pts',(13.0641007993,-26.0571446878,8.52225304435));
#96603=CARTESIAN_POINT('Ctrl Pts',(13.0609230524,-26.1400859332,8.53920080258));
#96604=CARTESIAN_POINT('Ctrl Pts',(13.0545801486,-26.2169441965,8.57302387625));
#96605=CARTESIAN_POINT('Ctrl Pts',(13.037895068,-26.3473699802,8.65987870015));
#96606=CARTESIAN_POINT('Ctrl Pts',(13.0141520182,-26.4436357412,8.77811343457));
#96607=CARTESIAN_POINT('Ctrl Pts',(13.0015068071,-26.4815731476,8.83957127532));
#96608=CARTESIAN_POINT('Ctrl Pts',(12.9878157168,-26.5117194744,8.90437404317));
#96609=CARTESIAN_POINT('Ctrl Pts',(12.9732844047,-26.5340600059,8.97133867828));
#96610=CARTESIAN_POINT('Origin',(12.7692410021,-27.9742356128,8.46695657076));
#96611=CARTESIAN_POINT('',(13.0641007993,-27.8242356128,8.52225304435));
#96612=CARTESIAN_POINT('Origin',(3.89394702409,-27.9742356128,-8.84845722572));
#96613=CARTESIAN_POINT('',(4.02121700373,-25.9742356128,-9.12012310927));
#96614=CARTESIAN_POINT('',(4.02121700373,-27.8242356128,-9.12012310927));
#96615=CARTESIAN_POINT('Ctrl Pts',(3.59394702409,-25.9742356128,-8.84845722572));
#96616=CARTESIAN_POINT('Ctrl Pts',(3.59394702409,-25.9742356128002,-8.96899190619));
#96617=CARTESIAN_POINT('Ctrl Pts',(3.65448289574,-25.9742356128002,-9.08952658665));
#96618=CARTESIAN_POINT('Ctrl Pts',(3.77723460344,-25.9742356128002,-9.1675743146));
#96619=CARTESIAN_POINT('Ctrl Pts',(3.91206646884,-25.9742356128003,-9.17125793036));
#96620=CARTESIAN_POINT('Ctrl Pts',(4.02121700373,-25.9742356128,-9.12012310927));
#96621=CARTESIAN_POINT('Ctrl Pts',(4.02121700311545,-25.9742087333861,-9.12012310955797));
#96622=CARTESIAN_POINT('Ctrl Pts',(3.91205553437643,-25.9742146970064,-9.1712630529297));
#96623=CARTESIAN_POINT('Ctrl Pts',(3.77720758969876,-25.9742206606268,-9.1675735762));
#96624=CARTESIAN_POINT('Ctrl Pts',(3.65444600647237,-25.9742245217385,-9.089503129595));
#96625=CARTESIAN_POINT('Ctrl Pts',(3.5939227712474,-25.9742247028758,-8.96894360624986));
#96626=CARTESIAN_POINT('Ctrl Pts',(3.59394702986297,-25.9742221718257,-8.84839685399463));
#96627=CARTESIAN_POINT('Ctrl Pts',(4.02122205614958,-26.0847136525922,-9.12012074183368));
#96628=CARTESIAN_POINT('Ctrl Pts',(3.91205926363719,-26.0602023764211,-9.17126135222328));
#96629=CARTESIAN_POINT('Ctrl Pts',(3.77720986797824,-26.0356911001499,-9.16757232040782));
#96630=CARTESIAN_POINT('Ctrl Pts',(3.65444734645218,-26.0198214098812,-9.08950176074631));
#96631=CARTESIAN_POINT('Ctrl Pts',(3.5939243024794,-26.0190768988899,-8.96894175972539));
#96632=CARTESIAN_POINT('Ctrl Pts',(3.59394951005266,-26.029479841544,-8.84839452991358));
#96633=CARTESIAN_POINT('Ctrl Pts',(3.99525994980673,-26.1953560420414,-9.1322859303989));
#96634=CARTESIAN_POINT('Ctrl Pts',(3.89289863013481,-26.146162866449,-9.17999943960044));
#96635=CARTESIAN_POINT('Ctrl Pts',(3.76550434421357,-26.0969696909566,-9.17402461392749));
#96636=CARTESIAN_POINT('Ctrl Pts',(3.64756279207107,-26.065177481353,-9.09653482858758));
#96637=CARTESIAN_POINT('Ctrl Pts',(3.58605698027632,-26.0638115296301,-8.97842905062067));
#96638=CARTESIAN_POINT('Ctrl Pts',(3.58120648340124,-26.0848066822428,-8.86033548279754));
#96639=CARTESIAN_POINT('Ctrl Pts',(3.94360062276572,-26.293916292257,-9.15648299770932));
#96640=CARTESIAN_POINT('Ctrl Pts',(3.85442237244048,-26.2261168661153,-9.19756876089837));
#96641=CARTESIAN_POINT('Ctrl Pts',(3.7414986999235,-26.1583174399736,-9.18721517340115));
#96642=CARTESIAN_POINT('Ctrl Pts',(3.6330764351228,-26.1131686986625,-9.11086249079868));
#96643=CARTESIAN_POINT('Ctrl Pts',(3.56996718935291,-26.108201380164,-8.9974689177855));
#96644=CARTESIAN_POINT('Ctrl Pts',(3.55585088691963,-26.1340888379853,-8.88408647848547));
#96645=CARTESIAN_POINT('Ctrl Pts',(3.81878709152418,-26.4439556743499,-9.21381749055382));
#96646=CARTESIAN_POINT('Ctrl Pts',(3.75615830652382,-26.3530421884608,-9.24190779271982));
#96647=CARTESIAN_POINT('Ctrl Pts',(3.6725256492406,-26.2621287025717,-9.22341791384639));
#96648=CARTESIAN_POINT('Ctrl Pts',(3.58523528668288,-26.1982144741315,-9.14939448447646));
#96649=CARTESIAN_POINT('Ctrl Pts',(3.5232681863945,-26.1833159073178,-9.0448740837474));
#96650=CARTESIAN_POINT('Ctrl Pts',(3.49459357993615,-26.2091086215099,-8.94036284953103));
#96651=CARTESIAN_POINT('Ctrl Pts',(3.65518574680024,-26.5331576706117,-9.28645512724112));
#96652=CARTESIAN_POINT('Ctrl Pts',(3.62051284919576,-26.434977950602,-9.30153534977169));
#96653=CARTESIAN_POINT('Ctrl Pts',(3.56782721193058,-26.3367982306924,-9.27548347767736));
#96654=CARTESIAN_POINT('Ctrl Pts',(3.50535217434315,-26.263852978627,-9.20388490272889));
#96655=CARTESIAN_POINT('Ctrl Pts',(3.45109619805268,-26.2377244615336,-9.10776802330137));
#96656=CARTESIAN_POINT('Ctrl Pts',(3.41430468871176,-26.2537045861121,-9.01165851362097));
#96657=CARTESIAN_POINT('Ctrl Pts',(3.5753967783082,-26.560421829436,-9.32123386752726));
#96658=CARTESIAN_POINT('Ctrl Pts',(3.55290435767089,-26.46163192706,-9.33083686690438));
#96659=CARTESIAN_POINT('Ctrl Pts',(3.51371779768073,-26.3628420247839,-9.30175173243743));
#96660=CARTESIAN_POINT('Ctrl Pts',(3.46268894387028,-26.2877149808645,-9.23119412114871));
#96661=CARTESIAN_POINT('Ctrl Pts',(3.41348702446829,-26.2568846180366,-9.13849094265645));
#96662=CARTESIAN_POINT('Ctrl Pts',(3.37514906929817,-26.2673339290873,-9.04579442022087));
#96663=CARTESIAN_POINT('Ctrl Pts',(3.49280842183818,-26.5742388712317,-9.35651769670719));
#96664=CARTESIAN_POINT('Ctrl Pts',(3.48193300696612,-26.4768356794767,-9.36107471062541));
#96665=CARTESIAN_POINT('Ctrl Pts',(3.45560668553042,-26.3794324877216,-9.32929021973307));
#96666=CARTESIAN_POINT('Ctrl Pts',(3.41589189003752,-26.3038151487329,-9.25969681792774));
#96667=CARTESIAN_POINT('Ctrl Pts',(3.37274412802113,-26.2692830090117,-9.17005833196199));
#96668=CARTESIAN_POINT('Ctrl Pts',(3.33461993282405,-26.274239735331,-9.08042587139392));
#96669=CARTESIAN_POINT('Ctrl Pts',(3.40986370467272,-26.5742356882418,-9.39127343593685));
#96670=CARTESIAN_POINT('Ctrl Pts',(3.40986677190155,-26.4799793512239,-9.39127214064104));
#96671=CARTESIAN_POINT('Ctrl Pts',(3.39556373278484,-26.3857230142061,-9.35712926318368));
#96672=CARTESIAN_POINT('Ctrl Pts',(3.36677172202495,-26.3112263962281,-9.28841020083968));
#96673=CARTESIAN_POINT('Ctrl Pts',(3.33034394782978,-26.274222231551,-9.20147178423216));
#96674=CARTESIAN_POINT('Ctrl Pts',(3.29391705058738,-26.2742356584786,-9.11453884399441));
#96675=CARTESIAN_POINT('',(3.40988747183743,-26.5742356512186,-9.39126347679935));
#96676=CARTESIAN_POINT('Ctrl Pts',(4.02121700373,-25.9742356128,-9.12012310927));
#96677=CARTESIAN_POINT('Ctrl Pts',(4.02121700373,-26.0847351827,-9.12012310927));
#96678=CARTESIAN_POINT('Ctrl Pts',(3.99525241027,-26.1953704263,-9.13228946189));
#96679=CARTESIAN_POINT('Ctrl Pts',(3.94359404173,-26.2939242033,-9.15648602078));
#96680=CARTESIAN_POINT('Ctrl Pts',(3.81878605501,-26.4439540873,-9.2138179004));
#96681=CARTESIAN_POINT('Ctrl Pts',(3.65519433633,-26.5331529872,-9.28645131356));
#96682=CARTESIAN_POINT('Ctrl Pts',(3.57541049572,-26.560417142,-9.32122788832));
#96683=CARTESIAN_POINT('Ctrl Pts',(3.49282735343,-26.5742357037,-9.35650960864));
#96684=CARTESIAN_POINT('Ctrl Pts',(3.4098874718,-26.5742356887,-9.39126347671));
#96685=CARTESIAN_POINT('Origin',(3.29476705670924,-26.5721143469785,-9.11652908600206));
#96686=CARTESIAN_POINT('Origin',(-2.84607155346,-26.5742356128,5.53854202767));
#96687=CARTESIAN_POINT('',(0.647446102181,-26.5742356128,-10.2675153591));
#96688=CARTESIAN_POINT('Origin',(-2.84607155346,-26.5742356128,5.53854202767));
#96689=CARTESIAN_POINT('Origin',(0.582701491963,-26.5742356128,-9.97458510214));
#96690=CARTESIAN_POINT('Origin',(-2.84607155346,-27.8242356128,5.53854202767));
#96691=CARTESIAN_POINT('',(12.9732844032,-27.8242356128,8.9713386779));
#96692=CARTESIAN_POINT('',(0.647446102181,-27.8242356128,-10.2675153591));
#96693=CARTESIAN_POINT('Origin',(2.00371733667E-15,-26.5742356128,-7.33821278943));
#96694=CARTESIAN_POINT('',(-0.647446102181,-26.5742356128,-10.2675153591));
#96695=CARTESIAN_POINT('Origin',(1.67065042928E-15,-26.5742356128,-7.33821278943));
#96696=CARTESIAN_POINT('Origin',(-0.582701491963,-26.5742356128,-9.97458510214));
#96697=CARTESIAN_POINT('Origin',(1.51756957939E-15,-27.8242356128,-7.33821278943));
#96698=CARTESIAN_POINT('',(-0.647446102181,-27.8242356128,-10.2675153591));
#96699=CARTESIAN_POINT('Origin',(-12.7692410021,-23.4742356128,8.46695657076));
#96700=CARTESIAN_POINT('',(-13.0641007993,-23.4742356128,8.52225304435));
#96701=CARTESIAN_POINT('',(-12.9895126513631,-23.4742356128,8.67062394794872));
#96702=CARTESIAN_POINT('Origin',(-12.7692410021,-23.4742356128,8.46695657076));
#96703=CARTESIAN_POINT('',(-12.9840525338676,-23.4078536953505,8.66557541894761));
#96704=CARTESIAN_POINT('Origin',(-12.7692410021,-23.4742356128,8.46695657076));
#96705=CARTESIAN_POINT('Origin',(-12.7692410021,-23.4742356128,8.46695657076));
#96706=CARTESIAN_POINT('Origin',(-12.7692410021,-23.4742356128,8.46695657076));
#96707=CARTESIAN_POINT('Origin',(-3.89394702409,-23.4742356128,-8.84845722572));
#96708=CARTESIAN_POINT('',(-4.02121700373,-23.4742356128,-9.12012310927));
#96709=CARTESIAN_POINT('Origin',(-3.89394702409,-23.4742356128,-8.84845722572));
#96710=CARTESIAN_POINT('Origin',(-3.89394702409,-23.4742356128,-8.84845722572));
#96711=CARTESIAN_POINT('',(-3.89394702409,-23.1865648064703,-8.93357777074639));
#96712=CARTESIAN_POINT('Origin',(-3.89394702409,-23.4742356128,-8.84845722572));
#96713=CARTESIAN_POINT('Origin',(2.84607155346,-23.4742356128,5.53854202767));
#96714=CARTESIAN_POINT('Origin',(2.84607155346,-23.4742356128,5.53854202767));
#96715=CARTESIAN_POINT('Ctrl Pts',(-12.6068339386,-26.2541477285,8.98696689141));
#96716=CARTESIAN_POINT('Ctrl Pts',(-12.656763501,-26.2450230638,9.00090325616));
#96717=CARTESIAN_POINT('Ctrl Pts',(-12.7095130758,-26.2466649863,9.01179177872));
#96718=CARTESIAN_POINT('Ctrl Pts',(-12.7618789767,-26.2596851856,9.018729334));
#96719=CARTESIAN_POINT('Ctrl Pts',(-12.8587193698,-26.30670696,9.02376000973));
#96720=CARTESIAN_POINT('Ctrl Pts',(-12.9290963696,-26.3874137021,9.01159792233));
#96721=CARTESIAN_POINT('Ctrl Pts',(-12.9549695516,-26.4341561975,9.00132366206));
#96722=CARTESIAN_POINT('Ctrl Pts',(-12.9697655766,-26.4841087839,8.98755448534));
#96723=CARTESIAN_POINT('Ctrl Pts',(-12.9732844032,-26.5340598441,8.9713386779));
#96724=CARTESIAN_POINT('Ctrl Pts',(-12.602271199,-26.244718344,8.94944232356));
#96725=CARTESIAN_POINT('Ctrl Pts',(-12.6527754898,-26.2334802622,8.96483328464));
#96726=CARTESIAN_POINT('Ctrl Pts',(-12.7068774073,-26.2331761106,8.97633576006));
#96727=CARTESIAN_POINT('Ctrl Pts',(-12.761179757,-26.2445853283,8.98290608319));
#96728=CARTESIAN_POINT('Ctrl Pts',(-12.8624277437,-26.2891818679,8.98524139971));
#96729=CARTESIAN_POINT('Ctrl Pts',(-12.9371918658,-26.3688629587,8.96705573637));
#96730=CARTESIAN_POINT('Ctrl Pts',(-12.964978225,-26.4153991423,8.95308053464));
#96731=CARTESIAN_POINT('Ctrl Pts',(-12.9811851756,-26.4653009826,8.93520914846));
#96732=CARTESIAN_POINT('Ctrl Pts',(-12.9855508674,-26.5152010752,8.91481113395));
#96733=CARTESIAN_POINT('Ctrl Pts',(-12.5976340417,-26.2325138521,8.912882128));
#96734=CARTESIAN_POINT('Ctrl Pts',(-12.6484748874,-26.2192934199,8.93016638754));
#96735=CARTESIAN_POINT('Ctrl Pts',(-12.7037532053,-26.2170356489,8.94265428589));
#96736=CARTESIAN_POINT('Ctrl Pts',(-12.7598856352,-26.2266967758,8.94911991702));
#96737=CARTESIAN_POINT('Ctrl Pts',(-12.8654365701,-26.2683789496,8.94903642348));
#96738=CARTESIAN_POINT('Ctrl Pts',(-12.9446209623,-26.3462161918,8.92467166475));
#96739=CARTESIAN_POINT('Ctrl Pts',(-12.9743518533,-26.3920801662,8.90682449267));
#96740=CARTESIAN_POINT('Ctrl Pts',(-12.9919939688,-26.4414371519,8.88463204637));
#96741=CARTESIAN_POINT('Ctrl Pts',(-12.9972165276,-26.4907921504,8.8598339424));
#96742=CARTESIAN_POINT('Ctrl Pts',(-12.5930010467,-26.2175177033,8.87774657721));
#96743=CARTESIAN_POINT('Ctrl Pts',(-12.6439314611,-26.2025806566,8.89736399926));
#96744=CARTESIAN_POINT('Ctrl Pts',(-12.7001900362,-26.1984644898,8.91122227553));
#96745=CARTESIAN_POINT('Ctrl Pts',(-12.7580199858,-26.2063019338,8.91786661014));
#96746=CARTESIAN_POINT('Ctrl Pts',(-12.8677144157,-26.2446206613,8.91568901553));
#96747=CARTESIAN_POINT('Ctrl Pts',(-12.9513046343,-26.319697988,8.88504420709));
#96748=CARTESIAN_POINT('Ctrl Pts',(-12.982992513,-26.3643472171,8.86318110532));
#96749=CARTESIAN_POINT('Ctrl Pts',(-13.002081513,-26.4125746646,8.83647618314));
#96750=CARTESIAN_POINT('Ctrl Pts',(-13.0081651461,-26.4607998779,8.80708839192));
#96751=CARTESIAN_POINT('Ctrl Pts',(-12.5818292035,-26.1733614649,8.79590968998));
#96752=CARTESIAN_POINT('Ctrl Pts',(-12.6323244128,-26.1554842052,8.82249979162));
#96753=CARTESIAN_POINT('Ctrl Pts',(-12.6904347476,-26.1475299818,8.84085890335));
#96754=CARTESIAN_POINT('Ctrl Pts',(-12.7520318679,-26.1509983382,8.84880669813));
#96755=CARTESIAN_POINT('Ctrl Pts',(-12.8713824144,-26.1801158283,8.84250417641));
#96756=CARTESIAN_POINT('Ctrl Pts',(-12.9656920029,-26.2455948371,8.79617037266));
#96757=CARTESIAN_POINT('Ctrl Pts',(-13.0022038566,-26.2854891551,8.76401868675));
#96758=CARTESIAN_POINT('Ctrl Pts',(-13.0248773755,-26.3289895549,8.72565667529));
#96759=CARTESIAN_POINT('Ctrl Pts',(-13.0330999298,-26.3724871935,8.68442780782));
#96760=CARTESIAN_POINT('Ctrl Pts',(-12.5723981851,-26.1119182248,8.73171604256));
#96761=CARTESIAN_POINT('Ctrl Pts',(-12.6212992155,-26.0956425018,8.76686070247));
#96762=CARTESIAN_POINT('Ctrl Pts',(-12.6800096167,-26.086872764,8.79140324302));
#96763=CARTESIAN_POINT('Ctrl Pts',(-12.7441850222,-26.0871118638,8.8021873834));
#96764=CARTESIAN_POINT('Ctrl Pts',(-12.8711063426,-26.1055282096,8.79420158155));
#96765=CARTESIAN_POINT('Ctrl Pts',(-12.9747302188,-26.1536338998,8.73340720985));
#96766=CARTESIAN_POINT('Ctrl Pts',(-13.0155596279,-26.1836251588,8.69127581187));
#96767=CARTESIAN_POINT('Ctrl Pts',(-13.0414826419,-26.2166144707,8.64142369403));
#96768=CARTESIAN_POINT('Ctrl Pts',(-13.0516641058,-26.249601018,8.58855181802));
#96769=CARTESIAN_POINT('Ctrl Pts',(-12.5678634067,-26.0691543106,8.70214065489));
#96770=CARTESIAN_POINT('Ctrl Pts',(-12.6154947189,-26.0563582708,8.74269816246));
#96771=CARTESIAN_POINT('Ctrl Pts',(-12.6740974841,-26.0489588063,8.77139810866));
#96772=CARTESIAN_POINT('Ctrl Pts',(-12.7392779978,-26.0482057465,8.7844092739));
#96773=CARTESIAN_POINT('Ctrl Pts',(-12.8696620869,-26.0601436152,8.77645823375));
#96774=CARTESIAN_POINT('Ctrl Pts',(-12.9779865573,-26.0944629325,8.70793763124));
#96775=CARTESIAN_POINT('Ctrl Pts',(-13.0210579562,-26.1161437068,8.66024422424));
#96776=CARTESIAN_POINT('Ctrl Pts',(-13.0486971014,-26.140109634,8.6039070082));
#96777=CARTESIAN_POINT('Ctrl Pts',(-13.0599353737,-26.1640732171,8.54447530783));
#96778=CARTESIAN_POINT('Ctrl Pts',(-12.5655736321,-26.0216427322,8.68722826989));
#96779=CARTESIAN_POINT('Ctrl Pts',(-12.6125281998,-26.0152947619,8.73064336108));
#96780=CARTESIAN_POINT('Ctrl Pts',(-12.6710473198,-26.011636969,8.76156019108));
#96781=CARTESIAN_POINT('Ctrl Pts',(-12.7367182138,-26.0112870749,8.77578335878));
#96782=CARTESIAN_POINT('Ctrl Pts',(-12.8688414379,-26.0172717145,8.76793233964));
#96783=CARTESIAN_POINT('Ctrl Pts',(-12.9795662207,-26.0343805031,8.69541885992));
#96784=CARTESIAN_POINT('Ctrl Pts',(-13.0237888974,-26.0451806345,8.64482915231));
#96785=CARTESIAN_POINT('Ctrl Pts',(-13.0523134203,-26.0571157701,8.58510739684));
#96786=CARTESIAN_POINT('Ctrl Pts',(-13.0641007736,-26.0690497547,8.52225313007));
#96787=CARTESIAN_POINT('Ctrl Pts',(-12.5655736251,-25.9742356164,8.68722820936));
#96788=CARTESIAN_POINT('Ctrl Pts',(-12.6125281889,-25.9742356185,8.7306432957));
#96789=CARTESIAN_POINT('Ctrl Pts',(-12.6710473059,-25.974235622,8.76156011981));
#96790=CARTESIAN_POINT('Ctrl Pts',(-12.7367181986,-25.9742356268,8.7757832814));
#96791=CARTESIAN_POINT('Ctrl Pts',(-12.8688414249,-25.9742356378,8.76793225111));
#96792=CARTESIAN_POINT('Ctrl Pts',(-12.97956622,-25.9742356495,8.6954187635));
#96793=CARTESIAN_POINT('Ctrl Pts',(-13.0237889055,-25.9742356551,8.64482905307));
#96794=CARTESIAN_POINT('Ctrl Pts',(-13.0523134395,-25.9742356597,8.58510729574));
#96795=CARTESIAN_POINT('Ctrl Pts',(-13.0641008049,-25.9742356631,8.52225302769));
#96796=CARTESIAN_POINT('',(-12.973284400749,-26.5340597893858,8.9713386775021));
#96797=CARTESIAN_POINT('Origin',(-12.6801076948398,-26.5340598313603,8.90771935941597));
#96798=CARTESIAN_POINT('',(-13.06410080176,-25.9742356388815,8.52225303564387));
#96799=CARTESIAN_POINT('Origin',(-12.7692410021,-25.9742356128,8.46695657076));
#96800=CARTESIAN_POINT('Ctrl Pts',(-12.9732844032,-26.5340597894,8.9713386779));
#96801=CARTESIAN_POINT('Ctrl Pts',(-12.979891943676,-26.5239011923188,8.94088915075278));
#96802=CARTESIAN_POINT('Ctrl Pts',(-12.9862906228497,-26.5118121653252,
8.91097621606126));
#96803=CARTESIAN_POINT('Ctrl Pts',(-12.9924394245919,-26.4977670410124,
8.88184770694584));
#96804=CARTESIAN_POINT('Ctrl Pts',(-12.9980298766749,-26.4849973018402,
8.85536424865845));
#96805=CARTESIAN_POINT('Ctrl Pts',(-13.0034139204697,-26.4706087797295,
8.82952839709536));
#96806=CARTESIAN_POINT('Ctrl Pts',(-13.0085558742,-26.4545791221706,8.80456712582049));
#96807=CARTESIAN_POINT('Ctrl Pts',(-13.0131702409556,-26.4401941776882,
8.78216699031034));
#96808=CARTESIAN_POINT('Ctrl Pts',(-13.0175896851213,-26.4244868111922,
8.76047103867062));
#96809=CARTESIAN_POINT('Ctrl Pts',(-13.0217832115077,-26.4074544672131,
8.73968323166975));
#96810=CARTESIAN_POINT('Ctrl Pts',(-13.02367954228,-26.3997523675871,8.73028289541987));
#96811=CARTESIAN_POINT('Ctrl Pts',(-13.0255295972387,-26.3917795864622,
8.7210688510905));
#96812=CARTESIAN_POINT('Ctrl Pts',(-13.0273300783176,-26.383537525235,8.71206315735746));
#96813=CARTESIAN_POINT('Ctrl Pts',(-13.0306453306873,-26.3683612963176,
8.69548084064264));
#96814=CARTESIAN_POINT('Ctrl Pts',(-13.0337930017314,-26.3522696202503,
8.67960169725163));
#96815=CARTESIAN_POINT('Ctrl Pts',(-13.0367521637379,-26.3352719026803,
8.66456608725168));
#96816=CARTESIAN_POINT('Ctrl Pts',(-13.039820293027,-26.3176482663235,8.64897681051787));
#96817=CARTESIAN_POINT('Ctrl Pts',(-13.0426855701156,-26.299049974877,8.63429569933343));
#96818=CARTESIAN_POINT('Ctrl Pts',(-13.0453189403406,-26.2795297324795,
8.62071705815884));
#96819=CARTESIAN_POINT('Ctrl Pts',(-13.0479416652738,-26.2600883998665,
8.60719330808789));
#96820=CARTESIAN_POINT('Ctrl Pts',(-13.050334105218,-26.2397321641038,8.59476479434834));
#96821=CARTESIAN_POINT('Ctrl Pts',(-13.0524654801459,-26.2185617555089,
8.5836369832028));
#96822=CARTESIAN_POINT('Ctrl Pts',(-13.0544533237903,-26.1988170068846,
8.57325854233227));
#96823=CARTESIAN_POINT('Ctrl Pts',(-13.0562139011086,-26.178364235337,8.56401270697199));
#96824=CARTESIAN_POINT('Ctrl Pts',(-13.0577234588786,-26.157328093979,8.5560577868111));
#96825=CARTESIAN_POINT('Ctrl Pts',(-13.0591678057951,-26.1372006854713,
8.5484465084402));
#96826=CARTESIAN_POINT('Ctrl Pts',(-13.060382227609,-26.1165392613583,8.54201785128485));
#96827=CARTESIAN_POINT('Ctrl Pts',(-13.0613491801184,-26.0954923757779,
8.53688852111132));
#96828=CARTESIAN_POINT('Ctrl Pts',(-13.0622572570709,-26.0757269875808,
8.53207150428079));
#96829=CARTESIAN_POINT('Ctrl Pts',(-13.0629470166407,-26.0556218219351,
8.52840084562135));
#96830=CARTESIAN_POINT('Ctrl Pts',(-13.0634081609753,-26.0353336900326,
8.5259448160036));
#96831=CARTESIAN_POINT('Ctrl Pts',(-13.063868376796,-26.0150864082753,8.52349373160047));
#96832=CARTESIAN_POINT('Ctrl Pts',(-13.0641007978549,-25.9946567351865,
8.52225305135991));
#96833=CARTESIAN_POINT('Ctrl Pts',(-13.0641008048946,-25.9742356631,8.52225302771906));
#96834=CARTESIAN_POINT('Origin',(-12.7692410021,-27.9742356128,8.46695657076));
#96835=CARTESIAN_POINT('',(-13.0641007993,-27.8242356128,8.52225304435));
#96836=CARTESIAN_POINT('Origin',(2.84607155346,-26.5742356128,5.53854202767));
#96837=CARTESIAN_POINT('',(-3.40988736318,-26.5742356128,-9.39126352223));
#96838=CARTESIAN_POINT('Origin',(2.84607155346,-26.5742356128,5.53854202767));
#96839=CARTESIAN_POINT('Origin',(-3.29476681586543,-26.5721143161574,-9.11652914022926));
#96840=CARTESIAN_POINT('Ctrl Pts',(-3.40988736318,-26.5742356128,-9.39126352223));
#96841=CARTESIAN_POINT('Ctrl Pts',(-3.40988736318,-26.4799878332,-9.39126352223));
#96842=CARTESIAN_POINT('Ctrl Pts',(-3.39558379717,-26.3857400536,-9.35712815432));
#96843=CARTESIAN_POINT('Ctrl Pts',(-3.3667944876,-26.3112466293,-9.28842265298));
#96844=CARTESIAN_POINT('Ctrl Pts',(-3.33037075585,-26.2742356128,-9.20149765239));
#96845=CARTESIAN_POINT('Ctrl Pts',(-3.29394702409,-26.2742356128,-9.11457265181));
#96846=CARTESIAN_POINT('Ctrl Pts',(-3.4910113153,-26.5742356128,-9.3572705737));
#96847=CARTESIAN_POINT('Ctrl Pts',(-3.48037253295,-26.4769107573,-9.36172848744));
#96848=CARTESIAN_POINT('Ctrl Pts',(-3.45431071589,-26.3795859018,-9.32989979882));
#96849=CARTESIAN_POINT('Ctrl Pts',(-3.41483915768,-26.303996431,-9.26033984988));
#96850=CARTESIAN_POINT('Ctrl Pts',(-3.37184251989,-26.2694021533,-9.17077476858));
#96851=CARTESIAN_POINT('Ctrl Pts',(-3.33375727379,-26.2742356128,-9.08120968728));
#96852=CARTESIAN_POINT('Ctrl Pts',(-3.5717957464,-26.5610173226,-9.32277198251));
#96853=CARTESIAN_POINT('Ctrl Pts',(-3.54981186007,-26.4622981571,-9.33215415735));
#96854=CARTESIAN_POINT('Ctrl Pts',(-3.51119131997,-26.3635789917,-9.30295815815));
#96855=CARTESIAN_POINT('Ctrl Pts',(-3.46066295418,-26.2884340565,-9.23245787906));
#96856=CARTESIAN_POINT('Ctrl Pts',(-3.41172937916,-26.2574332304,-9.13990415856));
#96857=CARTESIAN_POINT('Ctrl Pts',(-3.37340074696,-26.2676265362,-9.04735043987));
#96858=CARTESIAN_POINT('Ctrl Pts',(-3.64994177161,-26.5349267151,-9.2887404003));
#96859=CARTESIAN_POINT('Ctrl Pts',(-3.61607413424,-26.4367209398,-9.30345845196));
#96860=CARTESIAN_POINT('Ctrl Pts',(-3.56428404035,-26.3385151645,-9.27721330878));
#96861=CARTESIAN_POINT('Ctrl Pts',(-3.50256972223,-26.2654317018,-9.20569945623));
#96862=CARTESIAN_POINT('Ctrl Pts',(-3.44864766071,-26.2389835875,-9.10982452003));
#96863=CARTESIAN_POINT('Ctrl Pts',(-3.41175001833,-26.2545810833,-9.01394958175));
#96864=CARTESIAN_POINT('Ctrl Pts',(-3.81424885473,-26.4476638797,-9.21588066878));
#96865=CARTESIAN_POINT('Ctrl Pts',(-3.75250256194,-26.3563393693,-9.24354676394));
#96866=CARTESIAN_POINT('Ctrl Pts',(-3.66984966637,-26.2650148589,-9.22480841607));
#96867=CARTESIAN_POINT('Ctrl Pts',(-3.58330407322,-26.2006837329,-9.15088080098));
#96868=CARTESIAN_POINT('Ctrl Pts',(-3.52146064047,-26.1853980321,-9.04666045675));
#96869=CARTESIAN_POINT('Ctrl Pts',(-3.4923805164,-26.2109498456,-8.94244011508));
#96870=CARTESIAN_POINT('Ctrl Pts',(-3.94071289979,-26.2993639395,-9.1578343834));
#96871=CARTESIAN_POINT('Ctrl Pts',(-3.85226553394,-26.2305560501,-9.19855372868));
#96872=CARTESIAN_POINT('Ctrl Pts',(-3.74014873645,-26.1617481608,-9.18796857302));
#96873=CARTESIAN_POINT('Ctrl Pts',(-3.63226461004,-26.1158647884,-9.11169933207));
#96874=CARTESIAN_POINT('Ctrl Pts',(-3.56907345668,-26.1106751416,-8.99858447989));
#96875=CARTESIAN_POINT('Ctrl Pts',(-3.55444130117,-26.1367996538,-8.88546962456));
#96876=CARTESIAN_POINT('Ctrl Pts',(-3.99426364762,-26.1995473566,-9.13275311113));
#96877=CARTESIAN_POINT('Ctrl Pts',(-3.89218061974,-26.1494194207,-9.18032667121));
#96878=CARTESIAN_POINT('Ctrl Pts',(-3.76509502836,-26.0992914848,-9.17426692037));
#96879=CARTESIAN_POINT('Ctrl Pts',(-3.64735025537,-26.0668944366,-9.09682188935));
#96880=CARTESIAN_POINT('Ctrl Pts',(-3.58578912303,-26.065499903,-8.97883752401));
#96881=CARTESIAN_POINT('Ctrl Pts',(-3.58072010307,-26.08689148,-8.86085315859));
#96882=CARTESIAN_POINT('Ctrl Pts',(-4.02121701032,-26.0867730682,-9.12012310673));
#96883=CARTESIAN_POINT('Ctrl Pts',(-3.9120664741,-26.0618073391,-9.17125792781));
#96884=CARTESIAN_POINT('Ctrl Pts',(-3.77723460736,-26.0368416101,-9.16757431204));
#96885=CARTESIAN_POINT('Ctrl Pts',(-3.65448289879,-26.0206759356,-9.08952658412));
#96886=CARTESIAN_POINT('Ctrl Pts',(-3.59394702701,-26.0199130168,-8.96899190369));
#96887=CARTESIAN_POINT('Ctrl Pts',(-3.59394702751,-26.0305043095,-8.84845722325));
#96888=CARTESIAN_POINT('Ctrl Pts',(-4.02121700383,-25.9742356142,-9.12012310922));
#96889=CARTESIAN_POINT('Ctrl Pts',(-3.91206646892,-25.9742356136,-9.17125793032));
#96890=CARTESIAN_POINT('Ctrl Pts',(-3.7772346035,-25.974235613,-9.16757431456));
#96891=CARTESIAN_POINT('Ctrl Pts',(-3.65448289578,-25.9742356126,-9.08952658662));
#96892=CARTESIAN_POINT('Ctrl Pts',(-3.59394702413,-25.9742356126,-8.96899190615));
#96893=CARTESIAN_POINT('Ctrl Pts',(-3.59394702414,-25.9742356128,-8.84845722568));
#96894=CARTESIAN_POINT('',(-4.02121700383,-25.9742356142,-9.12012310922));
#96895=CARTESIAN_POINT('Ctrl Pts',(-3.40988736318,-26.5742356128,-9.39126352223));
#96896=CARTESIAN_POINT('Ctrl Pts',(-3.4910113153,-26.5742356128,-9.3572705737));
#96897=CARTESIAN_POINT('Ctrl Pts',(-3.5717957464,-26.5610173226,-9.32277198251));
#96898=CARTESIAN_POINT('Ctrl Pts',(-3.64994177161,-26.5349267151,-9.2887404003));
#96899=CARTESIAN_POINT('Ctrl Pts',(-3.81424885473,-26.4476638797,-9.21588066878));
#96900=CARTESIAN_POINT('Ctrl Pts',(-3.94071289979,-26.2993639395,-9.1578343834));
#96901=CARTESIAN_POINT('Ctrl Pts',(-3.99426364762,-26.1995473566,-9.13275311113));
#96902=CARTESIAN_POINT('Ctrl Pts',(-4.02121701032,-26.0867730682,-9.12012310673));
#96903=CARTESIAN_POINT('Ctrl Pts',(-4.02121700383,-25.9742356142,-9.12012310922));
#96904=CARTESIAN_POINT('Ctrl Pts',(-3.59394702414,-25.9742356128,-8.84845722568));
#96905=CARTESIAN_POINT('Ctrl Pts',(-3.59394702413859,-25.9742356128,-8.86547082365358));
#96906=CARTESIAN_POINT('Ctrl Pts',(-3.59539869159477,-25.974235612795,-8.88248672119199));
#96907=CARTESIAN_POINT('Ctrl Pts',(-3.59828751216145,-25.9742356127898,
-8.89925093236573));
#96908=CARTESIAN_POINT('Ctrl Pts',(-3.60122870276565,-25.9742356127845,
-8.9163190538544));
#96909=CARTESIAN_POINT('Ctrl Pts',(-3.60565938344924,-25.9742356127791,
-8.93312594622168));
#96910=CARTESIAN_POINT('Ctrl Pts',(-3.61151215671489,-25.9742356127769,
-8.94941892221616));
#96911=CARTESIAN_POINT('Ctrl Pts',(-3.61752207494251,-25.9742356127746,
-8.9661493590479));
#96912=CARTESIAN_POINT('Ctrl Pts',(-3.62503123537727,-25.9742356127756,
-8.98233749575522));
#96913=CARTESIAN_POINT('Ctrl Pts',(-3.63391585030532,-25.9742356127818,
-8.99773161493334));
#96914=CARTESIAN_POINT('Ctrl Pts',(-3.64291284694615,-25.9742356127882,
-9.01332045470364));
#96915=CARTESIAN_POINT('Ctrl Pts',(-3.65331989483763,-25.9742356127999,
-9.02809466264263));
#96916=CARTESIAN_POINT('Ctrl Pts',(-3.66496225633728,-25.9742356128182,
-9.04182116714993));
#96917=CARTESIAN_POINT('Ctrl Pts',(-3.67676344198006,-25.9742356128368,
-9.05573492750878));
#96918=CARTESIAN_POINT('Ctrl Pts',(-3.68983340448778,-25.9742356128621,
-9.06857177135196));
#96919=CARTESIAN_POINT('Ctrl Pts',(-3.70394976533629,-25.9742356128952,
-9.08012422995346));
#96920=CARTESIAN_POINT('Ctrl Pts',(-3.71326866162606,-25.9742356129171,
-9.08775056968468));
#96921=CARTESIAN_POINT('Ctrl Pts',(-3.72304275512652,-25.9742356129423,
-9.09481791747569));
#96922=CARTESIAN_POINT('Ctrl Pts',(-3.73320020269621,-25.9742356129715,
-9.10127620403795));
#96923=CARTESIAN_POINT('Ctrl Pts',(-3.74860166909693,-25.9742356130157,
-9.11106873142366));
#96924=CARTESIAN_POINT('Ctrl Pts',(-3.76489842790395,-25.9742356130674,
-9.11946694152528));
#96925=CARTESIAN_POINT('Ctrl Pts',(-3.78182194867813,-25.9742356131258,
-9.12632585130464));
#96926=CARTESIAN_POINT('Ctrl Pts',(-3.79860151107297,-25.9742356131837,
-9.1331264163962));
#96927=CARTESIAN_POINT('Ctrl Pts',(-3.81599663952131,-25.9742356132481,
-9.13841346048746));
#96928=CARTESIAN_POINT('Ctrl Pts',(-3.83372562740725,-25.9742356133179,
-9.1420926721867));
#96929=CARTESIAN_POINT('Ctrl Pts',(-3.85107739541277,-25.9742356133862,
-9.14569360125604));
#96930=CARTESIAN_POINT('Ctrl Pts',(-3.86874841653982,-25.9742356134597,
-9.14775424225408));
#96931=CARTESIAN_POINT('Ctrl Pts',(-3.88646372344271,-25.9742356135371,
-9.14823449310598));
#96932=CARTESIAN_POINT('Ctrl Pts',(-3.90391680093427,-25.9742356136134,
-9.14870763508312));
#96933=CARTESIAN_POINT('Ctrl Pts',(-3.92141238189434,-25.9742356136936,
-9.14764666810675));
#96934=CARTESIAN_POINT('Ctrl Pts',(-3.93868441830445,-25.9742356137763,
-9.145062978613));
#96935=CARTESIAN_POINT('Ctrl Pts',(-3.95554177681329,-25.9742356138571,
-9.14254131995981));
#96936=CARTESIAN_POINT('Ctrl Pts',(-3.97218578514195,-25.9742356139402,
-9.13856913641943));
#96937=CARTESIAN_POINT('Ctrl Pts',(-3.98837262606647,-25.9742356140244,
-9.1332060827271));
#96938=CARTESIAN_POINT('Ctrl Pts',(-3.99956528614096,-25.9742356140826,
-9.12949771015339));
#96939=CARTESIAN_POINT('Ctrl Pts',(-4.0105394337227,-25.9742356141413,-9.12512533516117));
#96940=CARTESIAN_POINT('Ctrl Pts',(-4.02121700383,-25.9742356142,-9.12012310922));
#96941=CARTESIAN_POINT('Origin',(-3.89394702409,-27.9742356128,-8.84845722572));
#96942=CARTESIAN_POINT('',(-4.02121700373,-27.8242356128,-9.12012310927));
#96943=CARTESIAN_POINT('Origin',(2.84607155346,-27.8242356128,5.53854202767));
#96944=CARTESIAN_POINT('',(-12.9732844032,-27.8242356128,8.9713386779));
#96945=CARTESIAN_POINT('Origin',(10.0415172382,-26.5742356128,8.33514586886));
#96946=CARTESIAN_POINT('',(12.9037784987484,-26.5742355987284,9.23373391245544));
#96947=CARTESIAN_POINT('Origin',(12.6175523690299,-26.5742356128,9.14387512190451));
#96948=CARTESIAN_POINT('',(12.4158605957,-26.5742356128,10.1688562115));
#96949=CARTESIAN_POINT('Origin',(12.1784262599,-26.5742356128,9.98548517727));
#96950=CARTESIAN_POINT('Origin',(10.0415172382,-26.5742356128,8.33514586886));
#96951=CARTESIAN_POINT('Ctrl Pts',(12.6068339386,-26.2541477285,8.98696689141));
#96952=CARTESIAN_POINT('Ctrl Pts',(12.7066930633,-26.2358983992,9.01483962091));
#96953=CARTESIAN_POINT('Ctrl Pts',(12.8178300069,-26.2607313227,9.03051509132));
#96954=CARTESIAN_POINT('Ctrl Pts',(12.9140852431,-26.3342556033,9.02641004159));
#96955=CARTESIAN_POINT('Ctrl Pts',(12.9662467501,-26.4341577237,9.00377029278));
#96956=CARTESIAN_POINT('Ctrl Pts',(12.9732844032,-26.5340598441,8.9713386779));
#96957=CARTESIAN_POINT('Ctrl Pts',(12.6106280003,-26.2619885586,9.01816975155));
#96958=CARTESIAN_POINT('Ctrl Pts',(12.708974138,-26.2477664531,9.04491835482));
#96959=CARTESIAN_POINT('Ctrl Pts',(12.8159524428,-26.2758436136,9.06233104132));
#96960=CARTESIAN_POINT('Ctrl Pts',(12.9070210129,-26.3504586067,9.06354827381));
#96961=CARTESIAN_POINT('Ctrl Pts',(12.9560253652,-26.4501000555,9.04813737607));
#96962=CARTESIAN_POINT('Ctrl Pts',(12.9621611611,-26.5497415044,9.02259791155));
#96963=CARTESIAN_POINT('Ctrl Pts',(12.6136807588,-26.2679937272,9.04969534782));
#96964=CARTESIAN_POINT('Ctrl Pts',(12.7102354837,-26.2577528513,9.0760062137));
#96965=CARTESIAN_POINT('Ctrl Pts',(12.8129790795,-26.2887376058,9.09562365218));
#96966=CARTESIAN_POINT('Ctrl Pts',(12.8989313579,-26.3639769508,9.10215295496));
#96967=CARTESIAN_POINT('Ctrl Pts',(12.9446683244,-26.4628643491,9.09369562263));
#96968=CARTESIAN_POINT('Ctrl Pts',(12.949656063,-26.5617517538,9.07481948836));
#96969=CARTESIAN_POINT('Ctrl Pts',(12.6158914118,-26.2721121063,9.08130970942));
#96970=CARTESIAN_POINT('Ctrl Pts',(12.7104096761,-26.2656378329,9.10778259443));
#96971=CARTESIAN_POINT('Ctrl Pts',(12.8088747795,-26.2991108653,9.12998686861));
#96972=CARTESIAN_POINT('Ctrl Pts',(12.8897865248,-26.3745377171,9.1418082035));
#96973=CARTESIAN_POINT('Ctrl Pts',(12.9321497434,-26.4722631499,9.14006801201));
#96974=CARTESIAN_POINT('Ctrl Pts',(12.9357345368,-26.5699885837,9.12765954366));
#96975=CARTESIAN_POINT('Ctrl Pts',(12.6171883094,-26.2742355975,9.11279216515));
#96976=CARTESIAN_POINT('Ctrl Pts',(12.7094740156,-26.2712015816,9.13993707984));
#96977=CARTESIAN_POINT('Ctrl Pts',(12.8036505085,-26.3066955811,9.16503705887));
#96978=CARTESIAN_POINT('Ctrl Pts',(12.8795985938,-26.3818769922,9.18212527582));
#96979=CARTESIAN_POINT('Ctrl Pts',(12.9184829148,-26.4780562725,9.18689609473));
#96980=CARTESIAN_POINT('Ctrl Pts',(12.9204030457,-26.5742355538,9.18077993753));
#96981=CARTESIAN_POINT('Ctrl Pts',(12.6175523411,-26.2742356062,9.14387513829));
#96982=CARTESIAN_POINT('Ctrl Pts',(12.7074729361,-26.2742356042,9.17210511002));
#96983=CARTESIAN_POINT('Ctrl Pts',(12.7973935329,-26.311246617,9.20033507989));
#96984=CARTESIAN_POINT('Ctrl Pts',(12.8684667546,-26.3857400362,9.22264803953));
#96985=CARTESIAN_POINT('Ctrl Pts',(12.9037784934,-26.4799878104,9.23373391858));
#96986=CARTESIAN_POINT('Ctrl Pts',(12.9037784969,-26.574235585,9.23373391359));
#96987=CARTESIAN_POINT('Ctrl Pts',(12.9732843928317,-26.5340598587174,8.97133872568045));
#96988=CARTESIAN_POINT('Ctrl Pts',(12.9674428625711,-26.54229530553,8.99825824592988));
#96989=CARTESIAN_POINT('Ctrl Pts',(12.9612109795608,-26.5492260544689,9.02518736608815));
#96990=CARTESIAN_POINT('Ctrl Pts',(12.9545858707363,-26.5549069523633,9.05210598814747));
#96991=CARTESIAN_POINT('Ctrl Pts',(12.9478040477681,-26.5607222294918,9.07966135881259));
#96992=CARTESIAN_POINT('Ctrl Pts',(12.9406099943118,-26.5652277143943,9.10720670287461));
#96993=CARTESIAN_POINT('Ctrl Pts',(12.9329983321515,-26.5684286387089,9.13473197822653));
#96994=CARTESIAN_POINT('Ctrl Pts',(12.9254138081857,-26.571618150627,9.16215911650105));
#96995=CARTESIAN_POINT('Ctrl Pts',(12.9174143717085,-26.5735122847671,9.18956733401115));
#96996=CARTESIAN_POINT('Ctrl Pts',(12.9089958566211,-26.574065542159,9.21694310775132));
#96997=CARTESIAN_POINT('Ctrl Pts',(12.9072742542534,-26.5741786843492,9.22254150561577));
#96998=CARTESIAN_POINT('Ctrl Pts',(12.905535138156,-26.5742355816927,9.22813850523854));
#96999=CARTESIAN_POINT('Ctrl Pts',(12.9037784973901,-26.574235585,9.23373391202899));
#97000=CARTESIAN_POINT('Origin',(10.0415172382,-27.8242356128,8.33514586886));
#97001=CARTESIAN_POINT('',(12.4158605957,-27.8242356128,10.1688562115));
#97002=CARTESIAN_POINT('Origin',(-10.0415172382,-26.5742356128,8.33514586886));
#97003=CARTESIAN_POINT('',(-12.4158605957,-26.5742356128,10.1688562115));
#97004=CARTESIAN_POINT('Origin',(-12.1784262599,-26.5742356128,9.98548517727));
#97005=CARTESIAN_POINT('',(-12.9037784845,-26.5742356128,9.23373396017));
#97006=CARTESIAN_POINT('Origin',(-12.6195762561711,-26.5721143167766,9.14451056062222));
#97007=CARTESIAN_POINT('Origin',(-10.0415172382,-26.5742356128,8.33514586886));
#97008=CARTESIAN_POINT('Ctrl Pts',(-12.6175523599,-26.2742356128,9.14387515104));
#97009=CARTESIAN_POINT('Ctrl Pts',(-12.7074729489,-26.2742356128,9.1721051285));
#97010=CARTESIAN_POINT('Ctrl Pts',(-12.7973935379,-26.3112466293,9.20033510596));
#97011=CARTESIAN_POINT('Ctrl Pts',(-12.8684667518,-26.3857400536,9.22264807394));
#97012=CARTESIAN_POINT('Ctrl Pts',(-12.9037784845,-26.4799878332,9.23373396017));
#97013=CARTESIAN_POINT('Ctrl Pts',(-12.9037784845,-26.5742356128,9.23373396017));
#97014=CARTESIAN_POINT('Ctrl Pts',(-12.6171883574,-26.2742356128,9.11279315844));
#97015=CARTESIAN_POINT('Ctrl Pts',(-12.7094739788,-26.2712016953,9.13993811731));
#97016=CARTESIAN_POINT('Ctrl Pts',(-12.8036503248,-26.3066957496,9.1650382076));
#97017=CARTESIAN_POINT('Ctrl Pts',(-12.8795982434,-26.3818771498,9.18212660258));
#97018=CARTESIAN_POINT('Ctrl Pts',(-12.9184824419,-26.4780563813,9.18689763116));
#97019=CARTESIAN_POINT('Ctrl Pts',(-12.9204025066,-26.5742356128,9.18078167336));
#97020=CARTESIAN_POINT('Ctrl Pts',(-12.6158916105,-26.2721122483,9.0813123221));
#97021=CARTESIAN_POINT('Ctrl Pts',(-12.7104096521,-26.2656382627,9.10778530133));
#97022=CARTESIAN_POINT('Ctrl Pts',(-12.8088743595,-26.2991114721,9.12998985719));
#97023=CARTESIAN_POINT('Ctrl Pts',(-12.8897856562,-26.3745383201,9.14181166467));
#97024=CARTESIAN_POINT('Ctrl Pts',(-12.9321485573,-26.4722636434,9.1400720384));
#97025=CARTESIAN_POINT('Ctrl Pts',(-12.9357331951,-26.5699889642,9.12766410551));
#97026=CARTESIAN_POINT('Ctrl Pts',(-12.6136812731,-26.2679944507,9.04969907596));
#97027=CARTESIAN_POINT('Ctrl Pts',(-12.7102357572,-26.257754074,9.07600987399));
#97028=CARTESIAN_POINT('Ctrl Pts',(-12.8129788034,-26.28873921,9.09562757859));
#97029=CARTESIAN_POINT('Ctrl Pts',(-12.8989304246,-26.363978659,9.10215754682));
#97030=CARTESIAN_POINT('Ctrl Pts',(-12.944666986,-26.4628659856,9.09370108211));
#97031=CARTESIAN_POINT('Ctrl Pts',(-12.9496546007,-26.5617533112,9.074825766));
#97032=CARTESIAN_POINT('Ctrl Pts',(-12.6106281314,-26.26198871,9.01817066751));
#97033=CARTESIAN_POINT('Ctrl Pts',(-12.708974212,-26.2477667318,9.04491924544));
#97034=CARTESIAN_POINT('Ctrl Pts',(-12.8159523793,-26.2758439872,9.06233199343));
#97035=CARTESIAN_POINT('Ctrl Pts',(-12.9070207823,-26.350459,9.06354939385));
#97036=CARTESIAN_POINT('Ctrl Pts',(-12.9560250323,-26.4501004207,9.04813871743));
#97037=CARTESIAN_POINT('Ctrl Pts',(-12.9621607982,-26.5497418392,9.02259946049));
#97038=CARTESIAN_POINT('Ctrl Pts',(-12.6068339484,-26.2541476936,8.98696687838));
#97039=CARTESIAN_POINT('Ctrl Pts',(-12.7066930674,-26.2358983672,9.01483961189));
#97040=CARTESIAN_POINT('Ctrl Pts',(-12.8178300052,-26.2607312902,9.0305150864));
#97041=CARTESIAN_POINT('Ctrl Pts',(-12.9140852366,-26.3342555659,9.02641003965));
#97042=CARTESIAN_POINT('Ctrl Pts',(-12.9662467409,-26.4341576782,9.00377029183));
#97043=CARTESIAN_POINT('Ctrl Pts',(-12.9732843934,-26.5340597894,8.97133867629));
#97044=CARTESIAN_POINT('Ctrl Pts',(-12.9037784845,-26.5742356128,9.23373396017));
#97045=CARTESIAN_POINT('Ctrl Pts',(-12.9123899316053,-26.5742356128,9.20630402689466));
#97046=CARTESIAN_POINT('Ctrl Pts',(-12.9205796598355,-26.5728724678115,
9.17883767519317));
#97047=CARTESIAN_POINT('Ctrl Pts',(-12.9283513177015,-26.5702022988638,
9.15135033698744));
#97048=CARTESIAN_POINT('Ctrl Pts',(-12.9361496963363,-26.5675229492537,
9.1237684909151));
#97049=CARTESIAN_POINT('Ctrl Pts',(-12.9435274399562,-26.5635275942613,
9.09616440770698));
#97050=CARTESIAN_POINT('Ctrl Pts',(-12.9504901127122,-26.5582212495112,
9.06854732983508));
#97051=CARTESIAN_POINT('Ctrl Pts',(-12.9572170081428,-26.5530945937709,
9.04186545041132));
#97052=CARTESIAN_POINT('Ctrl Pts',(-12.9635566560319,-26.5467441560851,
9.01517048220121));
#97053=CARTESIAN_POINT('Ctrl Pts',(-12.9695122335975,-26.5391272012899,
8.9884798091082));
#97054=CARTESIAN_POINT('Ctrl Pts',(-12.9707872326892,-26.537496526458,8.98276573963696));
#97055=CARTESIAN_POINT('Ctrl Pts',(-12.9720446165679,-26.5358076273671,
8.97705193099787));
#97056=CARTESIAN_POINT('Ctrl Pts',(-12.9732843934,-26.5340597894,8.97133867629));
#97057=CARTESIAN_POINT('Origin',(-10.0415172382,-27.8242356128,8.33514586886));
#97058=CARTESIAN_POINT('',(-12.4158605957,-27.8242356128,10.1688562115));
#97059=CARTESIAN_POINT('Origin',(-8.72866611926,-23.4742356128,13.252332246));
#97060=CARTESIAN_POINT('',(-8.89884287263,-23.4742356128,13.4993947332));
#97061=CARTESIAN_POINT('Origin',(-8.72866611926,-23.4742356128,13.252332246));
#97062=CARTESIAN_POINT('Origin',(-8.72866611926,-23.4742356128,13.252332246));
#97063=CARTESIAN_POINT('',(-8.78700378468238,-23.1849482466887,13.3062723665177));
#97064=CARTESIAN_POINT('Origin',(-8.72866611926,-23.4742356128,13.252332246));
#97065=CARTESIAN_POINT('Origin',(8.72866611926,-23.4742356128,13.252332246));
#97066=CARTESIAN_POINT('',(8.89884287263,-23.4742356128,13.4993947332));
#97067=CARTESIAN_POINT('',(8.94893776852305,-23.4742356128,13.4559996231887));
#97068=CARTESIAN_POINT('Origin',(8.72866611926,-23.4742356128,13.252332246));
#97069=CARTESIAN_POINT('',(8.94177659881935,-23.3983621101791,13.4493782688019));
#97070=CARTESIAN_POINT('Origin',(8.72866611926,-23.4742356128,13.252332246));
#97071=CARTESIAN_POINT('Origin',(8.72866611926,-23.4742356128,13.252332246));
#97072=CARTESIAN_POINT('Origin',(8.72866611926,-23.4742356128,13.252332246));
#97073=CARTESIAN_POINT('Origin',(5.43994370138E-15,-23.4742356128,0.580061096523));
#97074=CARTESIAN_POINT('Origin',(1.10873183178E-16,-23.4742356128,0.580061096523));
#97075=CARTESIAN_POINT('Origin',(-2.04512416396E-15,-26.5742356128,0.580061096523));
#97076=CARTESIAN_POINT('',(-9.40585242867367,-26.5742358357554,13.1350810502009));
#97077=CARTESIAN_POINT('Origin',(-9.22597996127761,-26.5742356128,12.8949854593485));
#97078=CARTESIAN_POINT('Origin',(-2.68767324558E-16,-26.5742356128,0.580061096523));
#97079=CARTESIAN_POINT('Ctrl Pts',(-8.93233349645,-25.9742356128,13.0320605967));
#97080=CARTESIAN_POINT('Ctrl Pts',(-9.0112864001,-25.9742356128,13.1050619605));
#97081=CARTESIAN_POINT('Ctrl Pts',(-9.05753156728,-25.9742356128,13.2134376055));
#97082=CARTESIAN_POINT('Ctrl Pts',(-9.04862484094,-25.9742356128,13.3377236529));
#97083=CARTESIAN_POINT('Ctrl Pts',(-8.98739853023,-25.9742356128,13.4383975561));
#97084=CARTESIAN_POINT('Ctrl Pts',(-8.89884287263,-25.9742356128,13.4993947332));
#97085=CARTESIAN_POINT('Ctrl Pts',(-8.93233349645,-26.0285372111,13.0320605967));
#97086=CARTESIAN_POINT('Ctrl Pts',(-9.0112864001,-26.0241566749,13.1050619605));
#97087=CARTESIAN_POINT('Ctrl Pts',(-9.05753156726,-26.0284966165,13.2134376055));
#97088=CARTESIAN_POINT('Ctrl Pts',(-9.04862484095,-26.0429379832,13.3377236529));
#97089=CARTESIAN_POINT('Ctrl Pts',(-8.98739853023,-26.0628883963,13.4383975561));
#97090=CARTESIAN_POINT('Ctrl Pts',(-8.89884287263,-26.0828388094,13.4993947332));
#97091=CARTESIAN_POINT('Ctrl Pts',(-8.94472655074,-26.08285904,13.0267961436));
#97092=CARTESIAN_POINT('Ctrl Pts',(-9.02169065378,-26.074050391,13.1006602186));
#97093=CARTESIAN_POINT('Ctrl Pts',(-9.06768131823,-26.0827027622,13.2080228858));
#97094=CARTESIAN_POINT('Ctrl Pts',(-9.06113122668,-26.1115995645,13.3293879943));
#97095=CARTESIAN_POINT('Ctrl Pts',(-9.00408533535,-26.1515406257,13.4266880848));
#97096=CARTESIAN_POINT('Ctrl Pts',(-8.91997599276,-26.1914817452,13.4848363629));
#97097=CARTESIAN_POINT('Ctrl Pts',(-8.9695742685,-26.1326166293,13.016255239));
#97098=CARTESIAN_POINT('Ctrl Pts',(-9.04255123506,-26.1212616413,13.0918512663));
#97099=CARTESIAN_POINT('Ctrl Pts',(-9.08803799129,-26.134748461,13.1971786824));
#97100=CARTESIAN_POINT('Ctrl Pts',(-9.08621282797,-26.1765733467,13.3126866711));
#97101=CARTESIAN_POINT('Ctrl Pts',(-9.03754117443,-26.2337854443,13.4032271249));
#97102=CARTESIAN_POINT('Ctrl Pts',(-8.96233987903,-26.290997548,13.4556696979));
#97103=CARTESIAN_POINT('Ctrl Pts',(-9.03028791925,-26.2079395652,12.989613417));
#97104=CARTESIAN_POINT('Ctrl Pts',(-9.09589435053,-26.1961913738,13.0677079223));
#97105=CARTESIAN_POINT('Ctrl Pts',(-9.14175144084,-26.2188939721,13.1671618616));
#97106=CARTESIAN_POINT('Ctrl Pts',(-9.15122220031,-26.2795381045,13.2688142601));
#97107=CARTESIAN_POINT('Ctrl Pts',(-9.12142423198,-26.3605908527,13.3437756344));
#97108=CARTESIAN_POINT('Ctrl Pts',(-9.06630530821,-26.4416435958,13.3830106592));
#97109=CARTESIAN_POINT('Ctrl Pts',(-9.1104960852,-26.2536276545,12.9522433826));
#97110=CARTESIAN_POINT('Ctrl Pts',(-9.1703946836,-26.2462276286,13.0306868925));
#97111=CARTESIAN_POINT('Ctrl Pts',(-9.21936149245,-26.2769167679,13.1209534215));
#97112=CARTESIAN_POINT('Ctrl Pts',(-9.24339400518,-26.3479556515,13.2050413138));
#97113=CARTESIAN_POINT('Ctrl Pts',(-9.23603570877,-26.4404876405,13.260825769));
#97114=CARTESIAN_POINT('Ctrl Pts',(-9.20475552832,-26.5330196335,13.28361302));
#97115=CARTESIAN_POINT('Ctrl Pts',(-9.14847854779,-26.2673388385,12.9340159562));
#97116=CARTESIAN_POINT('Ctrl Pts',(-9.2065559864,-26.2624721802,13.0119783221));
#97117=CARTESIAN_POINT('Ctrl Pts',(-9.2575613966,-26.2961769579,13.0975892735));
#97118=CARTESIAN_POINT('Ctrl Pts',(-9.28841654251,-26.3700572474,13.1735175604));
#97119=CARTESIAN_POINT('Ctrl Pts',(-9.29115586865,-26.4652497721,13.2205120876));
#97120=CARTESIAN_POINT('Ctrl Pts',(-9.27058953184,-26.5604422808,13.2357088969));
#97121=CARTESIAN_POINT('Ctrl Pts',(-9.18739830238,-26.274235893,12.9147116237));
#97122=CARTESIAN_POINT('Ctrl Pts',(-9.24438226141,-26.2719282776,12.9916193734));
#97123=CARTESIAN_POINT('Ctrl Pts',(-9.2979593505,-26.307785511,13.072211743));
#97124=CARTESIAN_POINT('Ctrl Pts',(-9.33575986597,-26.382802277,13.1399052833));
#97125=CARTESIAN_POINT('Ctrl Pts',(-9.34842419719,-26.4785192081,13.1781045816));
#97126=CARTESIAN_POINT('Ctrl Pts',(-9.33836508495,-26.5742361412,13.1856405721));
#97127=CARTESIAN_POINT('Ctrl Pts',(-9.22598003346,-26.2742358377,12.8949853402));
#97128=CARTESIAN_POINT('Ctrl Pts',(-9.28248863171,-26.2742358325,12.9704136123));
#97129=CARTESIAN_POINT('Ctrl Pts',(-9.33899722271,-26.3112468736,13.0458418922));
#97130=CARTESIAN_POINT('Ctrl Pts',(-9.38366159094,-26.3857403537,13.1054603965));
#97131=CARTESIAN_POINT('Ctrl Pts',(-9.40585244492,-26.4799882059,13.1350810267));
#97132=CARTESIAN_POINT('Ctrl Pts',(-9.40585242353,-26.5742360581,13.1350810427));
#97133=CARTESIAN_POINT('',(-8.89884287263,-25.9742356128,13.4993947332));
#97134=CARTESIAN_POINT('Ctrl Pts',(-8.89884287263,-25.9742356128,13.4993947332));
#97135=CARTESIAN_POINT('Ctrl Pts',(-8.98739853023,-25.9742356128002,13.4383975561));
#97136=CARTESIAN_POINT('Ctrl Pts',(-9.04862484094,-25.9742356128001,13.3377236529));
#97137=CARTESIAN_POINT('Ctrl Pts',(-9.05753156728,-25.9742356128001,13.2134376055));
#97138=CARTESIAN_POINT('Ctrl Pts',(-9.0112864001,-25.9742356128001,13.1050619605));
#97139=CARTESIAN_POINT('Ctrl Pts',(-8.93233349645,-25.9742356128,13.0320605967));
#97140=CARTESIAN_POINT('Ctrl Pts',(-8.89884287263,-25.9742356128,13.4993947332));
#97141=CARTESIAN_POINT('Ctrl Pts',(-8.89895609808286,-26.0010432829593,
13.4993167434567));
#97142=CARTESIAN_POINT('Ctrl Pts',(-8.90059919950406,-26.0277666642535,
13.4981851695452));
#97143=CARTESIAN_POINT('Ctrl Pts',(-8.90372878865397,-26.0541518085826,
13.496027640683));
#97144=CARTESIAN_POINT('Ctrl Pts',(-8.90702142789706,-26.081911606272,13.4937577056022));
#97145=CARTESIAN_POINT('Ctrl Pts',(-8.91195898935124,-26.1092969617299,
13.4903524012086));
#97146=CARTESIAN_POINT('Ctrl Pts',(-8.91844967243714,-26.1360470459536,
13.4858669737749));
#97147=CARTESIAN_POINT('Ctrl Pts',(-8.92544355331223,-26.1648709617083,
13.4810338083391));
#97148=CARTESIAN_POINT('Ctrl Pts',(-8.93424021215507,-26.1929569983882,
13.4749468232508));
#97149=CARTESIAN_POINT('Ctrl Pts',(-8.94468577595512,-26.2200211365478,
13.4676969887184));
#97150=CARTESIAN_POINT('Ctrl Pts',(-8.95549613608157,-26.2480304508958,
13.4601939641185));
#97151=CARTESIAN_POINT('Ctrl Pts',(-8.96807170222389,-26.2749450857715,
13.451445930878));
#97152=CARTESIAN_POINT('Ctrl Pts',(-8.98221286723584,-26.3004968966248,
13.4415701314541));
#97153=CARTESIAN_POINT('Ctrl Pts',(-8.99656295183038,-26.3264262063373,
13.4315484283587));
#97154=CARTESIAN_POINT('Ctrl Pts',(-9.01252419020305,-26.3509519159204,
13.4203659558918));
#97155=CARTESIAN_POINT('Ctrl Pts',(-9.02987348408223,-26.3738436039025,
13.4081537502609));
#97156=CARTESIAN_POINT('Ctrl Pts',(-9.03813067124657,-26.3847386266909,
13.4023414982877));
#97157=CARTESIAN_POINT('Ctrl Pts',(-9.04670216437771,-26.3952642555391,
13.3962960646772));
#97158=CARTESIAN_POINT('Ctrl Pts',(-9.05556386016477,-26.4053998182991,
13.3900316588417));
#97159=CARTESIAN_POINT('Ctrl Pts',(-9.06617082519398,-26.417531532401,13.3825335077853));
#97160=CARTESIAN_POINT('Ctrl Pts',(-9.07717152666241,-26.4290529763397,
13.3747371662871));
#97161=CARTESIAN_POINT('Ctrl Pts',(-9.08851925551041,-26.4399493747432,
13.3666713990996));
#97162=CARTESIAN_POINT('Ctrl Pts',(-9.10945377975007,-26.4600512752697,
13.3517915054257));
#97163=CARTESIAN_POINT('Ctrl Pts',(-9.13156720191249,-26.4780257582573,
13.3359958573705));
#97164=CARTESIAN_POINT('Ctrl Pts',(-9.1545917526907,-26.493783803096,13.319450281518));
#97165=CARTESIAN_POINT('Ctrl Pts',(-9.17536032095728,-26.5079978493604,
13.3045258677949));
#97166=CARTESIAN_POINT('Ctrl Pts',(-9.19687135475279,-26.520409644557,13.2889905507415));
#97167=CARTESIAN_POINT('Ctrl Pts',(-9.21895271273267,-26.5309615712851,
13.2729526717885));
#97168=CARTESIAN_POINT('Ctrl Pts',(-9.2368976785699,-26.5395368574983,13.2599190897881));
#97169=CARTESIAN_POINT('Ctrl Pts',(-9.25507229474382,-26.5468177853716,
13.2466605914074));
#97170=CARTESIAN_POINT('Ctrl Pts',(-9.27346468079951,-26.5528426061672,
13.2331808449775));
#97171=CARTESIAN_POINT('Ctrl Pts',(-9.29181826304442,-26.5588547159418,
13.2197295377903));
#97172=CARTESIAN_POINT('Ctrl Pts',(-9.31038957007988,-26.5636163178449,
13.2060573013725));
#97173=CARTESIAN_POINT('Ctrl Pts',(-9.32918002295672,-26.5671165247323,
13.1921579856977));
#97174=CARTESIAN_POINT('Ctrl Pts',(-9.34748417167067,-26.5705261449163,
13.1786183896698));
#97175=CARTESIAN_POINT('Ctrl Pts',(-9.36599704153926,-26.5727388942514,
13.1648627383229));
#97176=CARTESIAN_POINT('Ctrl Pts',(-9.38472045559965,-26.5736958247132,
13.1508847837228));
#97177=CARTESIAN_POINT('Ctrl Pts',(-9.39173501954148,-26.5740543303731,
13.1456480648209));
#97178=CARTESIAN_POINT('Ctrl Pts',(-9.39877908188713,-26.5742360668045,
13.1403801822461));
#97179=CARTESIAN_POINT('Ctrl Pts',(-9.40585242322525,-26.5742360581,13.1350810429283));
#97180=CARTESIAN_POINT('Origin',(-8.72866611926,-27.9742356128,13.252332246));
#97181=CARTESIAN_POINT('',(-8.89884287263,-27.8242356128,13.4993947332));
#97182=CARTESIAN_POINT('Origin',(1.50758951484E-15,-26.5742356128,0.580061096523));
#97183=CARTESIAN_POINT('',(9.40585256108342,-26.5742356128,13.1350809262965));
#97184=CARTESIAN_POINT('Origin',(9.22725087823104,-26.5721145657866,12.8966831494532));
#97185=CARTESIAN_POINT('Origin',(-2.68767324558E-16,-26.5742356128,0.580061096523));
#97186=CARTESIAN_POINT('Ctrl Pts',(9.22598017922,-26.2742358667,12.8949853208));
#97187=CARTESIAN_POINT('Ctrl Pts',(9.28248884108,-26.2742358731,12.9704135146));
#97188=CARTESIAN_POINT('Ctrl Pts',(9.33899753074,-26.3112469248,13.0458416783));
#97189=CARTESIAN_POINT('Ctrl Pts',(9.38366202162,-26.385740412,13.105460047));
#97190=CARTESIAN_POINT('Ctrl Pts',(9.40585299479,-26.4799882688,13.1350805566));
#97191=CARTESIAN_POINT('Ctrl Pts',(9.40585306927,-26.5742361254,13.1350804849));
#97192=CARTESIAN_POINT('Ctrl Pts',(9.18809325963,-26.2742357357,12.9143563956));
#97193=CARTESIAN_POINT('Ctrl Pts',(9.2450687066,-26.2719697063,12.9912374316));
#97194=CARTESIAN_POINT('Ctrl Pts',(9.29869866779,-26.3078477237,13.071736699));
#97195=CARTESIAN_POINT('Ctrl Pts',(9.3366228955,-26.3828550411,13.1392846998));
#97196=CARTESIAN_POINT('Ctrl Pts',(9.34945889077,-26.478545471,13.1773294073));
#97197=CARTESIAN_POINT('Ctrl Pts',(9.33958101525,-26.5742358983,13.1847296173));
#97198=CARTESIAN_POINT('Ctrl Pts',(9.14988050464,-26.2675847856,12.9333199946));
#97199=CARTESIAN_POINT('Ctrl Pts',(9.20791871134,-26.2628099114,13.0112443559));
#97200=CARTESIAN_POINT('Ctrl Pts',(9.25901673093,-26.2965916112,13.096674713));
#97201=CARTESIAN_POINT('Ctrl Pts',(9.29012180691,-26.3705121727,13.1723066998));
#97202=CARTESIAN_POINT('Ctrl Pts',(9.29321828466,-26.4657229441,13.218984685));
#97203=CARTESIAN_POINT('Ctrl Pts',(9.2730301115,-26.5609337322,13.2339056769));
#97204=CARTESIAN_POINT('Ctrl Pts',(9.112555303,-26.2543622577,12.9512548511));
#97205=CARTESIAN_POINT('Ctrl Pts',(9.17235549832,-26.2470995345,13.0296719809));
#97206=CARTESIAN_POINT('Ctrl Pts',(9.22143309124,-26.2779511011,13.1196858885));
#97207=CARTESIAN_POINT('Ctrl Pts',(9.24583568971,-26.3491419477,13.2033312194));
#97208=CARTESIAN_POINT('Ctrl Pts',(9.23902495122,-26.4418155436,13.2586389408));
#97209=CARTESIAN_POINT('Ctrl Pts',(9.20832565648,-26.534489123,13.281014498));
#97210=CARTESIAN_POINT('Ctrl Pts',(9.03207275784,-26.2094852035,12.9888169711));
#97211=CARTESIAN_POINT('Ctrl Pts',(9.09749481749,-26.197804545,13.0669613638));
#97212=CARTESIAN_POINT('Ctrl Pts',(9.14338431009,-26.2207373383,13.1662307438));
#97213=CARTESIAN_POINT('Ctrl Pts',(9.15318354628,-26.2817510699,13.2674823288));
#97214=CARTESIAN_POINT('Ctrl Pts',(9.12391877788,-26.3632427792,13.341998513));
#97215=CARTESIAN_POINT('Ctrl Pts',(9.06936730061,-26.4447345097,13.3808551065));
#97216=CARTESIAN_POINT('Ctrl Pts',(8.97065416936,-26.1347652578,13.0157974347));
#97217=CARTESIAN_POINT('Ctrl Pts',(9.04345996357,-26.1233054476,13.0914671212));
#97218=CARTESIAN_POINT('Ctrl Pts',(9.08892654614,-26.1370041575,13.1967048874));
#97219=CARTESIAN_POINT('Ctrl Pts',(9.08730678255,-26.1793863705,13.3119583562));
#97220=CARTESIAN_POINT('Ctrl Pts',(9.03899779297,-26.2373408339,13.4022057303));
#97221=CARTESIAN_POINT('Ctrl Pts',(8.96418223747,-26.2952952698,13.4544010418));
#97222=CARTESIAN_POINT('Ctrl Pts',(8.9450884596,-26.0844303721,13.0266425468));
#97223=CARTESIAN_POINT('Ctrl Pts',(9.02199368194,-26.0754916974,13.1005323275));
#97224=CARTESIAN_POINT('Ctrl Pts',(9.0679762798,-26.0842677714,13.2078657435));
#97225=CARTESIAN_POINT('Ctrl Pts',(9.06149508662,-26.113583452,13.3291454014));
#97226=CARTESIAN_POINT('Ctrl Pts',(9.00457191343,-26.1541045198,13.4263466133));
#97227=CARTESIAN_POINT('Ctrl Pts',(8.92059308555,-26.1946255531,13.4844114062));
#97228=CARTESIAN_POINT('Ctrl Pts',(8.93233349646,-26.0293225561,13.0320605967));
#97229=CARTESIAN_POINT('Ctrl Pts',(9.0112864001,-26.0248786653,13.1050619605));
#97230=CARTESIAN_POINT('Ctrl Pts',(9.05753156729,-26.0292813737,13.2134376054));
#97231=CARTESIAN_POINT('Ctrl Pts',(9.04862484094,-26.0439316,13.3377236529));
#97232=CARTESIAN_POINT('Ctrl Pts',(8.98739853023,-26.0641705484,13.4383975561));
#97233=CARTESIAN_POINT('Ctrl Pts',(8.89884287263,-26.0844094969,13.4993947332));
#97234=CARTESIAN_POINT('Ctrl Pts',(8.93233349645,-25.9742356128,13.0320605967));
#97235=CARTESIAN_POINT('Ctrl Pts',(9.0112864001,-25.9742356128,13.1050619605));
#97236=CARTESIAN_POINT('Ctrl Pts',(9.05753156728,-25.9742356128,13.2134376055));
#97237=CARTESIAN_POINT('Ctrl Pts',(9.04862484094,-25.9742356128,13.3377236529));
#97238=CARTESIAN_POINT('Ctrl Pts',(8.98739853023,-25.9742356128,13.4383975561));
#97239=CARTESIAN_POINT('Ctrl Pts',(8.89884287263,-25.9742356128,13.4993947332));
#97240=CARTESIAN_POINT('',(8.89884287263,-25.9742356128,13.4993947332));
#97241=CARTESIAN_POINT('Ctrl Pts',(8.89884287263,-25.9742356128,13.4993947332));
#97242=CARTESIAN_POINT('Ctrl Pts',(8.91298306467026,-25.9742356128,13.4896549625125));
#97243=CARTESIAN_POINT('Ctrl Pts',(8.92628553401168,-25.9742356128,13.4786970415768));
#97244=CARTESIAN_POINT('Ctrl Pts',(8.93854791254593,-25.9742356128,13.4666811475669));
#97245=CARTESIAN_POINT('Ctrl Pts',(8.95104535408271,-25.9742356128,13.4544349155262));
#97246=CARTESIAN_POINT('Ctrl Pts',(8.96246226321512,-25.9742356128,13.4410901641476));
#97247=CARTESIAN_POINT('Ctrl Pts',(8.97262533430588,-25.9742356128,13.4268518558005));
#97248=CARTESIAN_POINT('Ctrl Pts',(8.98311909131686,-25.9742356128,13.4121502614983));
#97249=CARTESIAN_POINT('Ctrl Pts',(8.99227578537047,-25.9742356128,13.3964964516728));
#97250=CARTESIAN_POINT('Ctrl Pts',(8.99995175024907,-25.9742356128,13.3801470495469));
#97251=CARTESIAN_POINT('Ctrl Pts',(9.00766424539377,-25.9742356128,13.3637198398725));
#97252=CARTESIAN_POINT('Ctrl Pts',(9.01388179530927,-25.9742356128,13.3465910269051));
#97253=CARTESIAN_POINT('Ctrl Pts',(9.0185081506613,-25.9742356128,13.3290433912322));
#97254=CARTESIAN_POINT('Ctrl Pts',(9.02324515897379,-25.9742356128,13.3110760519938));
#97255=CARTESIAN_POINT('Ctrl Pts',(9.02631368963526,-25.9742356128,13.2926702667125));
#97256=CARTESIAN_POINT('Ctrl Pts',(9.02766503882281,-25.9742356128,13.274143441584));
#97257=CARTESIAN_POINT('Ctrl Pts',(9.0289486472493,-25.9742356128,13.2565453336559));
#97258=CARTESIAN_POINT('Ctrl Pts',(9.02868389097897,-25.9742356128,13.2388306328017));
#97259=CARTESIAN_POINT('Ctrl Pts',(9.02687144828272,-25.9742356128,13.2212742225973));
#97260=CARTESIAN_POINT('Ctrl Pts',(9.02502174785923,-25.9742356128,13.2033569116351));
#97261=CARTESIAN_POINT('Ctrl Pts',(9.02155985184751,-25.9742356128,13.1856052086565));
#97262=CARTESIAN_POINT('Ctrl Pts',(9.01653597905922,-25.9742356128,13.168306927222));
#97263=CARTESIAN_POINT('Ctrl Pts',(9.01158677833036,-25.9742356128,13.151265757851));
#97264=CARTESIAN_POINT('Ctrl Pts',(9.0051217696928,-25.9742356128,13.1346651906981));
#97265=CARTESIAN_POINT('Ctrl Pts',(8.9972370966015,-25.9742356128,13.1187670484391));
#97266=CARTESIAN_POINT('Ctrl Pts',(8.98917398112835,-25.9742356128,13.1025091065614));
#97267=CARTESIAN_POINT('Ctrl Pts',(8.97962599034423,-25.9742356128,13.086986455719));
#97268=CARTESIAN_POINT('Ctrl Pts',(8.96874817699059,-25.9742356128,13.0724552782259));
#97269=CARTESIAN_POINT('Ctrl Pts',(8.95848641872981,-25.9742356128,13.05874706079));
#97270=CARTESIAN_POINT('Ctrl Pts',(8.94704161419982,-25.9742356128,13.0459214436467));
#97271=CARTESIAN_POINT('Ctrl Pts',(8.9345873676507,-25.9742356128,13.0341661661072));
#97272=CARTESIAN_POINT('Ctrl Pts',(8.93383968856693,-25.9742356128,13.0334604489765));
#97273=CARTESIAN_POINT('Ctrl Pts',(8.93308838402742,-25.9742356128,13.0327585801828));
#97274=CARTESIAN_POINT('Ctrl Pts',(8.93233349645,-25.9742356128,13.0320605967));
#97275=CARTESIAN_POINT('Ctrl Pts',(9.40585253196699,-26.5742356128001,13.1350808874316));
#97276=CARTESIAN_POINT('Ctrl Pts',(9.38966886904336,-26.5742356625068,13.1472052249601));
#97277=CARTESIAN_POINT('Ctrl Pts',(9.37371043414577,-26.5732883695804,13.1591121368475));
#97278=CARTESIAN_POINT('Ctrl Pts',(9.35792283466795,-26.5714573040172,13.1708460778927));
#97279=CARTESIAN_POINT('Ctrl Pts',(9.34201605619545,-26.569612415925,13.1826685972742));
#97280=CARTESIAN_POINT('Ctrl Pts',(9.32628204370353,-26.5668701774511,13.1943160189337));
#97281=CARTESIAN_POINT('Ctrl Pts',(9.31066243960798,-26.5632416337301,13.2058344298026));
#97282=CARTESIAN_POINT('Ctrl Pts',(9.29515443644995,-26.5596390156906,13.2172705424618));
#97283=CARTESIAN_POINT('Ctrl Pts',(9.27975857422437,-26.5551624841021,13.2285799346777));
#97284=CARTESIAN_POINT('Ctrl Pts',(9.2644247047449,-26.5497730925338,13.2398012826113));
#97285=CARTESIAN_POINT('Ctrl Pts',(9.24921727962928,-26.5444281423369,13.2509300983759));
#97286=CARTESIAN_POINT('Ctrl Pts',(9.23407016532093,-26.5381851359198,13.2619727680672));
#97287=CARTESIAN_POINT('Ctrl Pts',(9.2189509255191,-26.5309600288552,13.2729539975724));
#97288=CARTESIAN_POINT('Ctrl Pts',(9.20382905634151,-26.5237336652776,13.2839371368152));
#97289=CARTESIAN_POINT('Ctrl Pts',(9.18918039767918,-26.5157377018366,13.2945354690637));
#97290=CARTESIAN_POINT('Ctrl Pts',(9.17494003359809,-26.5069897570663,13.3048032283136));
#97291=CARTESIAN_POINT('Ctrl Pts',(9.16059836413125,-26.4981795797635,13.3151440319958));
#97292=CARTESIAN_POINT('Ctrl Pts',(9.1466701415747,-26.4886063214309,13.3251499910549));
#97293=CARTESIAN_POINT('Ctrl Pts',(9.13310430195239,-26.4782388663181,13.3348638296197));
#97294=CARTESIAN_POINT('Ctrl Pts',(9.11953846233007,-26.4678714112053,13.3445776681844));
#97295=CARTESIAN_POINT('Ctrl Pts',(9.10633428546738,-26.4567093462435,13.3539998486706));
#97296=CARTESIAN_POINT('Ctrl Pts',(9.09346630996625,-26.4446784843961,13.3631536894615));
#97297=CARTESIAN_POINT('Ctrl Pts',(9.08047306334464,-26.4325305008194,13.3723966438733));
#97298=CARTESIAN_POINT('Ctrl Pts',(9.06782160736129,-26.4194959284248,13.3813666470324));
#97299=CARTESIAN_POINT('Ctrl Pts',(9.0555219142915,-26.4054564922348,13.3900613629745));
#97300=CARTESIAN_POINT('Ctrl Pts',(9.04333267047346,-26.3915431279079,13.3986780017756));
#97301=CARTESIAN_POINT('Ctrl Pts',(9.03188529279735,-26.3770877111105,13.4067442529712));
#97302=CARTESIAN_POINT('Ctrl Pts',(9.0211058886148,-26.3620851591429,13.4143208599837));
#97303=CARTESIAN_POINT('Ctrl Pts',(9.01063047203914,-26.3475056908441,13.4216838007681));
#97304=CARTESIAN_POINT('Ctrl Pts',(9.00078546904118,-26.3324087757691,13.4285845585318));
#97305=CARTESIAN_POINT('Ctrl Pts',(8.9915296376939,-26.316749732984,13.4350584629122));
#97306=CARTESIAN_POINT('Ctrl Pts',(8.98237304571567,-26.3012585836562,13.4414629552472));
#97307=CARTESIAN_POINT('Ctrl Pts',(8.97379258055418,-26.2852166573475,13.4474499888569));
#97308=CARTESIAN_POINT('Ctrl Pts',(8.96578137748102,-26.2685508639815,13.4530295650986));
#97309=CARTESIAN_POINT('Ctrl Pts',(8.95797597478179,-26.2523131993841,13.4584658072035));
#97310=CARTESIAN_POINT('Ctrl Pts',(8.95071060864188,-26.2354825818213,13.4635154704097));
#97311=CARTESIAN_POINT('Ctrl Pts',(8.9440164384977,-26.2179729998285,13.4681611210768));
#97312=CARTESIAN_POINT('Ctrl Pts',(8.94308638265781,-26.2155403026254,13.468806565462));
#97313=CARTESIAN_POINT('Ctrl Pts',(8.94216741815707,-26.2130944800201,13.4694441650684));
#97314=CARTESIAN_POINT('Ctrl Pts',(8.94125969379736,-26.2106352851941,13.4700738273255));
#97315=CARTESIAN_POINT('Ctrl Pts',(8.93349674327698,-26.1896040023491,13.4754587626243));
#97316=CARTESIAN_POINT('Ctrl Pts',(8.92683498762293,-26.1683122326554,13.4800697405241));
#97317=CARTESIAN_POINT('Ctrl Pts',(8.92122702740422,-26.1467792344255,13.4839469960848));
#97318=CARTESIAN_POINT('Ctrl Pts',(8.9155694983306,-26.1250559056613,13.4878585227728));
#97319=CARTESIAN_POINT('Ctrl Pts',(8.9109841011639,-26.1030857806081,13.4910235212305));
#97320=CARTESIAN_POINT('Ctrl Pts',(8.90746043306424,-26.0808653513723,13.4934542237138));
#97321=CARTESIAN_POINT('Ctrl Pts',(8.9039681996182,-26.0588431506521,13.4958632418931));
#97322=CARTESIAN_POINT('Ctrl Pts',(8.90151881605978,-26.0365736279148,13.4975510147087));
#97323=CARTESIAN_POINT('Ctrl Pts',(8.90014240237732,-26.014051170286,13.4984994019142));
#97324=CARTESIAN_POINT('Ctrl Pts',(8.89933657923613,-26.0008653688186,13.4990546364101));
#97325=CARTESIAN_POINT('Ctrl Pts',(8.89889929429057,-25.9875929284109,13.4993558699346));
#97326=CARTESIAN_POINT('Ctrl Pts',(8.89884287263,-25.9742356128,13.4993947332));
#97327=CARTESIAN_POINT('Origin',(8.72866611926,-27.9742356128,13.252332246));
#97328=CARTESIAN_POINT('',(8.89884287263,-27.8242356128,13.4993947332));
#97329=CARTESIAN_POINT('Origin',(-4.21848174452E-16,-27.8242356128,0.580061096523));
#97330=CARTESIAN_POINT('',(0.,0.,0.));
#97331=CARTESIAN_POINT('Origin',(1.33226762955E-14,-19.0742356128,-4.4019615652));
#97332=CARTESIAN_POINT('',(-4.33093462721,-19.3742356128,-6.08690818754));
#97333=CARTESIAN_POINT('',(-3.63173186089,-19.3742356128,-7.3013690143));
#97334=CARTESIAN_POINT('Origin',(8.59173843182E-14,-19.3742356128,-4.4019615652));
#97335=CARTESIAN_POINT('',(3.63173186095,-19.3742356128,-7.3013690143));
#97336=CARTESIAN_POINT('Origin',(1.33226762955E-14,-19.3742356128,-4.4019615652));
#97337=CARTESIAN_POINT('',(4.33093462721,-19.3742356128,-6.08690818754));
#97338=CARTESIAN_POINT('Origin',(7.66166644017E-14,-19.3742356128,-4.4019615652));
#97339=CARTESIAN_POINT('',(4.05968610969081,-19.146953327667,-5.98137915983575));
#97340=CARTESIAN_POINT('Origin',(4.33093462721,-19.0742356128,-6.08690818754));
#97341=CARTESIAN_POINT('',(-4.0596861374133,-19.1469533408308,-5.98137909746699));
#97342=CARTESIAN_POINT('Origin',(1.33226762955E-14,-19.146953353,-4.4019615652));
#97343=CARTESIAN_POINT('Origin',(-4.33093462721,-19.0742356128,-6.08690818754));
#97344=CARTESIAN_POINT('Origin',(0.,-3.07423561284,0.473661560394));
#97345=CARTESIAN_POINT('',(5.42382962926,-3.07423561284,7.46684196367));
#97346=CARTESIAN_POINT('',(6.97990993744,-3.07423561284,5.91455829396));
#97347=CARTESIAN_POINT('Origin',(0.,-3.07423561284,0.473661560394));
#97348=CARTESIAN_POINT('',(5.65920103905,-3.07423561284,5.05609743232));
#97349=CARTESIAN_POINT('',(6.31955548824,-3.07423561284,5.48532786314));
#97350=CARTESIAN_POINT('',(4.5,-3.07423561284,6.1986309857));
#97351=CARTESIAN_POINT('Origin',(0.,-3.07423561284,0.473661560394));
#97352=CARTESIAN_POINT('',(4.5,-3.07423561284,6.27570807841));
#97353=CARTESIAN_POINT('',(4.5,-3.07423561284,6.23716953205));
#97354=CARTESIAN_POINT('',(4.96191481463,-3.07423561284,6.87127502104));
#97355=CARTESIAN_POINT('Origin',(5.42382962926,-4.67423561284,7.46684196367));
#97356=CARTESIAN_POINT('',(4.5,-4.67423561284,6.27570807841));
#97357=CARTESIAN_POINT('',(4.5,-3.87423561284,6.27570807841));
#97358=CARTESIAN_POINT('',(5.42382962926,-4.67423561284,7.46684196367));
#97359=CARTESIAN_POINT('',(4.96191481463,-4.67423561284,6.87127502104));
#97360=CARTESIAN_POINT('',(5.42382962926,-12.0242356128,7.46684196367));
#97361=CARTESIAN_POINT('Origin',(4.5,-4.67423561284,6.27570807841));
#97362=CARTESIAN_POINT('',(4.5,-4.67423561284,6.1986309857));
#97363=CARTESIAN_POINT('',(4.5,-3.87423561284,6.1986309857));
#97364=CARTESIAN_POINT('',(4.5,-4.67423561284,6.23716953205));
#97365=CARTESIAN_POINT('Origin',(0.,-3.87423561284,0.473661560394));
#97366=CARTESIAN_POINT('',(5.65920103905,-4.67423561284,5.05609743232));
#97367=CARTESIAN_POINT('',(5.65920103905,-3.87423561284,5.05609743232));
#97368=CARTESIAN_POINT('Origin',(0.,-4.67423561284,0.473661560394));
#97369=CARTESIAN_POINT('Origin',(5.65920103905,-4.67423561284,5.05609743232));
#97370=CARTESIAN_POINT('',(6.97990993744,-4.67423561284,5.91455829396));
#97371=CARTESIAN_POINT('',(6.97990993744,-12.0242356128,5.91455829396));
#97372=CARTESIAN_POINT('',(6.31955548824,-4.67423561284,5.48532786314));
#97373=CARTESIAN_POINT('Origin',(0.,-1.97423561284,0.473661560394));
#97374=CARTESIAN_POINT('',(-4.68330338854,-1.97423561284,-4.73359921144));
#97375=CARTESIAN_POINT('',(-6.87681426213,-1.97423561284,-0.852355399956));
#97376=CARTESIAN_POINT('',(-5.78005882534,-1.97423561284,-2.7929773057));
#97377=CARTESIAN_POINT('',(-5.81927285325,-1.97423561284,-6.19406394831));
#97378=CARTESIAN_POINT('',(-5.2512881209,-1.97423561284,-5.46383157987));
#97379=CARTESIAN_POINT('',(-8.68139919901,-1.97423561284,-1.24558477082));
#97380=CARTESIAN_POINT('Origin',(0.,-1.97423561284,0.473661560394));
#97381=CARTESIAN_POINT('',(-7.77910673057,-1.97423561284,-1.04897008539));
#97382=CARTESIAN_POINT('Origin',(-5.81927285325,-4.67423561284,-6.19406394831));
#97383=CARTESIAN_POINT('',(-4.68330338854,-4.67423561284,-4.73359921144));
#97384=CARTESIAN_POINT('',(-5.81927285325,-4.67423561284,-6.19406394831));
#97385=CARTESIAN_POINT('',(-5.2512881209,-4.67423561284,-5.46383157987));
#97386=CARTESIAN_POINT('',(-5.81927285325,-12.0242356128,-6.19406394831));
#97387=CARTESIAN_POINT('',(-4.68330338854,-3.32423561284,-4.73359921144));
#97388=CARTESIAN_POINT('Origin',(-4.68330338854,-4.67423561284,-4.73359921144));
#97389=CARTESIAN_POINT('',(-6.87681426213,-4.67423561284,-0.852355399956));
#97390=CARTESIAN_POINT('',(-6.87681426213,-3.32423561284,-0.852355399956));
#97391=CARTESIAN_POINT('',(-5.78005882534,-4.67423561284,-2.7929773057));
#97392=CARTESIAN_POINT('Origin',(-6.87681426213,-4.67423561284,-0.852355399956));
#97393=CARTESIAN_POINT('',(-8.68139919901,-4.67423561284,-1.24558477082));
#97394=CARTESIAN_POINT('',(-8.68139919901,-12.0242356128,-1.24558477082));
#97395=CARTESIAN_POINT('',(-7.77910673057,-4.67423561284,-1.04897008539));
#97396=CARTESIAN_POINT('Origin',(0.,-18.3742356128,0.473661560394));
#97397=CARTESIAN_POINT('',(-1.2046272227,-18.3742356128,-11.8721618652));
#97398=CARTESIAN_POINT('Origin',(0.,-18.3742356128,-11.8721618652));
#97399=CARTESIAN_POINT('Origin',(0.,-18.8742356128,-11.8721618652));
#97400=CARTESIAN_POINT('',(-1.2046272227,-19.3742356128,-11.8721618652));
#97401=CARTESIAN_POINT('',(-1.2046272227,-18.8742356128,-11.8721618652));
#97402=CARTESIAN_POINT('Origin',(-4.16333634234434E-16,-19.3742356128,-11.8721618652));
#97403=CARTESIAN_POINT('Origin',(0.,-19.3742356128,0.473661560394));
#97404=CARTESIAN_POINT('',(-4.2,-19.3742356128,-7.3013690143));
#97405=CARTESIAN_POINT('',(-3.91586593048,-19.3742356128,-7.3013690143));
#97406=CARTESIAN_POINT('',(-6.,-19.3742356128,-5.5013690143));
#97407=CARTESIAN_POINT('Origin',(-4.2,-19.3742356128,-5.5013690143));
#97408=CARTESIAN_POINT('',(-6.,-19.3742356128,-3.77162994903));
#97409=CARTESIAN_POINT('',(-6.,-19.3742356128,-4.63649948183));
#97410=CARTESIAN_POINT('',(-6.,-19.3742356128,4.71895306982));
#97411=CARTESIAN_POINT('Origin',(0.,-19.3742356128,0.473661560394));
#97412=CARTESIAN_POINT('',(-6.,-19.3742356128,6.1986309857));
#97413=CARTESIAN_POINT('',(-6.,-19.3742356128,5.45879202751));
#97414=CARTESIAN_POINT('',(-5.60798767447,-19.3742356128,7.32004558724));
#97415=CARTESIAN_POINT('Origin',(-4.2,-19.3742356128,6.1986309857));
#97416=CARTESIAN_POINT('',(-7.62360441819,-19.3742356128,4.96845362177));
#97417=CARTESIAN_POINT('Origin',(0.,-19.3742356128,0.473661560394));
#97418=CARTESIAN_POINT('',(-9.82022628685,-19.3742356128,4.96845362177));
#97419=CARTESIAN_POINT('',(-8.72191535252,-19.3742356128,4.96845362177));
#97420=CARTESIAN_POINT('',(-5.98285024331,-19.3742356128,-8.51775117433));
#97421=CARTESIAN_POINT('Origin',(0.,-19.3742356128,0.473661560394));
#97422=CARTESIAN_POINT('',(-5.17999195052,-19.3742356128,-10.0163199637));
#97423=CARTESIAN_POINT('Origin',(-6.97999195052,-19.3742356128,-10.0163199635));
#97424=CARTESIAN_POINT('',(-5.17999195052,-19.3742356128,-12.4003392757));
#97425=CARTESIAN_POINT('',(-5.17999195052,-19.3742356128,-11.2083296197));
#97426=CARTESIAN_POINT('',(-4.10871050222,-19.3742356128,-12.4074193595));
#97427=CARTESIAN_POINT('Origin',(-4.65570820166,-19.3742356128,-14.1222935581));
#97428=CARTESIAN_POINT('',(-3.03907448041,-19.3742356128,-12.7008507251));
#97429=CARTESIAN_POINT('Origin',(0.,-19.3742356128,0.473661560394));
#97430=CARTESIAN_POINT('',(-1.95746548311,-19.3742356128,-13.4393118415));
#97431=CARTESIAN_POINT('Origin',(-3.4436702163,-19.3742356128,-14.4547898034));
#97432=CARTESIAN_POINT('',(1.95746548311,-19.3742356128,-13.4393118415));
#97433=CARTESIAN_POINT('Origin',(0.,-19.3742356128,0.473661560394));
#97434=CARTESIAN_POINT('',(3.03907448041,-19.3742356128,-12.7008507251));
#97435=CARTESIAN_POINT('Origin',(3.4436702163,-19.3742356128,-14.4547898034));
#97436=CARTESIAN_POINT('',(4.16144704355,-19.3742356128,-12.3904787591));
#97437=CARTESIAN_POINT('Origin',(0.,-19.3742356128,0.473661560394));
#97438=CARTESIAN_POINT('',(5.17999195052,-19.3742356128,-12.3640705239));
#97439=CARTESIAN_POINT('Origin',(4.71546562382,-19.3742356128,-14.1030976346));
#97440=CARTESIAN_POINT('',(5.17999195052,-19.3742356128,-10.0163199635));
#97441=CARTESIAN_POINT('',(5.17999195052,-19.3742356128,-11.1901952438));
#97442=CARTESIAN_POINT('',(5.98285024331,-19.3742356128,-8.51775117433));
#97443=CARTESIAN_POINT('Origin',(6.97999195052,-19.3742356128,-10.0163199635));
#97444=CARTESIAN_POINT('',(9.82022628685,-19.3742356128,4.96845362177));
#97445=CARTESIAN_POINT('Origin',(0.,-19.3742356128,0.473661560394));
#97446=CARTESIAN_POINT('',(7.62360441819,-19.3742356128,4.96845362177));
#97447=CARTESIAN_POINT('',(8.72191535252,-19.3742356128,4.96845362177));
#97448=CARTESIAN_POINT('',(5.60798767447,-19.3742356128,7.32004558724));
#97449=CARTESIAN_POINT('Origin',(0.,-19.3742356128,0.473661560394));
#97450=CARTESIAN_POINT('',(6.,-19.3742356128,6.1986309857));
#97451=CARTESIAN_POINT('Origin',(4.2,-19.3742356128,6.1986309857));
#97452=CARTESIAN_POINT('',(6.,-19.3742356128,4.71895306982));
#97453=CARTESIAN_POINT('',(6.,-19.3742356128,5.45879202751));
#97454=CARTESIAN_POINT('',(6.,-19.3742356128,-3.77162994903));
#97455=CARTESIAN_POINT('Origin',(0.,-19.3742356128,0.473661560394));
#97456=CARTESIAN_POINT('',(6.,-19.3742356128,-5.5013690143));
#97457=CARTESIAN_POINT('',(6.,-19.3742356128,-4.63649948183));
#97458=CARTESIAN_POINT('',(4.20000000006,-19.3742356128,-7.3013690143));
#97459=CARTESIAN_POINT('Origin',(4.2,-19.3742356128,-5.5013690143));
#97460=CARTESIAN_POINT('',(3.91586593048,-19.3742356128,-7.3013690143));
#97461=CARTESIAN_POINT('Origin',(0.,-20.2352955315,-4.4019615652));
#97462=CARTESIAN_POINT('',(3.93695199971652,-18.7782619834169,-5.99493429549677));
#97463=CARTESIAN_POINT('',(-3.93695210731,-18.7782622649,-5.99493430976));
#97464=CARTESIAN_POINT('Origin',(-1.50990331349E-14,-20.2352955315,-5.99493430976));
#97465=CARTESIAN_POINT('Ctrl Pts',(-3.9369521072875,-18.7782622649083,-5.9949343097509));
#97466=CARTESIAN_POINT('Ctrl Pts',(-3.9705399999975,-18.8690178544819,-5.9949343023535));
#97467=CARTESIAN_POINT('Ctrl Pts',(-4.0019605374177,-18.9602724232578,-5.99192992634488));
#97468=CARTESIAN_POINT('Ctrl Pts',(-4.03081052657067,-19.0520074442237,
-5.98704698577112));
#97469=CARTESIAN_POINT('Ctrl Pts',(-4.04074578399551,-19.0835988269218,
-5.98536541593297));
#97470=CARTESIAN_POINT('Ctrl Pts',(-4.05037639795643,-19.1152474735558,
-5.98346074163699));
#97471=CARTESIAN_POINT('Ctrl Pts',(-4.05968616233678,-19.1469533287217,
-5.9813790244995));
#97472=CARTESIAN_POINT('Ctrl Pts',(4.05968610441,-19.1469533038,-5.98137915695));
#97473=CARTESIAN_POINT('Ctrl Pts',(4.03788343644,-19.0727011908,-5.98625455018));
#97474=CARTESIAN_POINT('Ctrl Pts',(4.01461432289,-18.9987108858,-5.9903211697));
#97475=CARTESIAN_POINT('Ctrl Pts',(3.98996106595,-18.9249385271,-5.99330264064));
#97476=CARTESIAN_POINT('Ctrl Pts',(3.96404157784,-18.8514591938,-5.99493417698));
#97477=CARTESIAN_POINT('Ctrl Pts',(3.93695201003,-18.7782619796,-5.99493428923));
#97478=CARTESIAN_POINT('Origin',(0.,-4.67423561284,0.473661560394));
#97479=CARTESIAN_POINT('',(4.2,-4.67423561284,6.4986309857));
#97480=CARTESIAN_POINT('Origin',(4.2,-4.67423561284,6.1986309857));
#97481=CARTESIAN_POINT('',(-4.2,-4.67423561284,6.4986309857));
#97482=CARTESIAN_POINT('',(0.,-4.67423561284,6.4986309857));
#97483=CARTESIAN_POINT('',(-4.5,-4.67423561284,6.1986309857));
#97484=CARTESIAN_POINT('Origin',(-4.2,-4.67423561284,6.1986309857));
#97485=CARTESIAN_POINT('',(-4.5,-4.67423561284,3.49012794495));
#97486=CARTESIAN_POINT('',(-4.5,-4.67423561284,4.84437946532));
#97487=CARTESIAN_POINT('',(-5.44794311523,-4.67423561284,3.49012794495));
#97488=CARTESIAN_POINT('',(-4.97448577881,-4.67423561284,3.49012794495));
#97489=CARTESIAN_POINT('',(-5.44794311523,-4.67423561284,-2.54280482416));
#97490=CARTESIAN_POINT('',(-5.44794311523,-4.67423561284,1.98189475267));
#97491=CARTESIAN_POINT('',(-4.5,-4.67423561284,-2.54280482416));
#97492=CARTESIAN_POINT('',(-4.97448577881,-4.67423561284,-2.54280482416));
#97493=CARTESIAN_POINT('',(-4.5,-4.67423561284,-5.5013690143));
#97494=CARTESIAN_POINT('',(-4.5,-4.67423561284,-4.02208691923));
#97495=CARTESIAN_POINT('',(-4.2,-4.67423561284,-5.8013690143));
#97496=CARTESIAN_POINT('Origin',(-4.2,-4.67423561284,-5.5013690143));
#97497=CARTESIAN_POINT('',(4.2,-4.67423561284,-5.8013690143));
#97498=CARTESIAN_POINT('',(0.,-4.67423561284,-5.8013690143));
#97499=CARTESIAN_POINT('',(4.5,-4.67423561284,-5.5013690143));
#97500=CARTESIAN_POINT('Origin',(4.2,-4.67423561284,-5.5013690143));
#97501=CARTESIAN_POINT('',(4.5,-4.67423561284,0.348630985699));
#97502=CARTESIAN_POINT('Origin',(0.,-4.67423561284,0.473661560394));
#97503=CARTESIAN_POINT('',(-8.40228522294909E-15,-4.67423561284,9.323661560394));
#97504=CARTESIAN_POINT('Origin',(0.,-4.67423561284,0.473661560394));
#97505=CARTESIAN_POINT('Origin',(0.,-4.67423561284,0.473661560394));
#97506=CARTESIAN_POINT('Origin',(-4.5,-4.67423561284,6.4986309857));
#97507=CARTESIAN_POINT('',(-4.5,-19.0742356128,-5.5013690143));
#97508=CARTESIAN_POINT('',(-4.5,-19.0742356128,6.1986309857));
#97509=CARTESIAN_POINT('',(-4.5,-19.0742356128,-2.12633843961));
#97510=CARTESIAN_POINT('',(-4.5,-13.6742356128,-5.5013690143));
#97511=CARTESIAN_POINT('',(-4.5,-14.0742356128,-2.54280482416));
#97512=CARTESIAN_POINT('',(-4.5,-9.37423561284,-2.54280482416));
#97513=CARTESIAN_POINT('',(-4.5,-14.0742356128,3.49012794495));
#97514=CARTESIAN_POINT('',(-4.5,-14.0742356128,1.98189475267));
#97515=CARTESIAN_POINT('',(-4.5,-9.37423561284,3.49012794495));
#97516=CARTESIAN_POINT('',(-4.5,-13.6742356128,6.1986309857));
#97517=CARTESIAN_POINT('Origin',(7.85,-9.17423561284,0.473661560394));
#97518=CARTESIAN_POINT('',(-8.85,-7.67423561284,0.473661560394));
#97519=CARTESIAN_POINT('',(-8.78621078736448,-10.2348957846198,1.53432173217382));
#97520=CARTESIAN_POINT('Ctrl Pts',(-8.85,-7.67423561284,0.473661560394));
#97521=CARTESIAN_POINT('Ctrl Pts',(-8.85,-7.67423561284,0.662394292391));
#97522=CARTESIAN_POINT('Ctrl Pts',(-8.84334932535928,-7.71202837241176,
0.863460154972133));
#97523=CARTESIAN_POINT('Ctrl Pts',(-8.81931354586398,-7.86522295898186,
1.23292358106269));
#97524=CARTESIAN_POINT('Ctrl Pts',(-8.80226283219622,-7.98060481275496,
1.4013511038686));
#97525=CARTESIAN_POINT('Ctrl Pts',(-8.77015828355848,-8.24654987137926,
1.66729616249291));
#97526=CARTESIAN_POINT('Ctrl Pts',(-8.75299937723619,-8.41497576333756,
1.78267503425714));
#97527=CARTESIAN_POINT('Ctrl Pts',(-8.72871516126698,-8.78443358162711,
1.93586745610213));
#97528=CARTESIAN_POINT('Ctrl Pts',(-8.72195505606398,-8.98549748442973,
1.973661560394));
#97529=CARTESIAN_POINT('Ctrl Pts',(-8.72195505606398,-9.36297374125027,
1.973661560394));
#97530=CARTESIAN_POINT('Ctrl Pts',(-8.72871516126698,-9.5640376440529,1.93586745610213));
#97531=CARTESIAN_POINT('Ctrl Pts',(-8.75299937723619,-9.93349546234244,
1.78267503425714));
#97532=CARTESIAN_POINT('Ctrl Pts',(-8.77015828355847,-10.1019213543007,
1.6672961624929));
#97533=CARTESIAN_POINT('Ctrl Pts',(-8.78621078736448,-10.2348957846198,
1.53432173217382));
#97534=CARTESIAN_POINT('Ctrl Pts',(-8.78621078736448,-10.2348957846198,
1.53432173217382));
#97535=CARTESIAN_POINT('Ctrl Pts',(-8.80226283219622,-10.367866412925,1.4013511038686));
#97536=CARTESIAN_POINT('Ctrl Pts',(-8.81931354586398,-10.4832482666981,
1.23292358106269));
#97537=CARTESIAN_POINT('Ctrl Pts',(-8.84334932535928,-10.6364428532682,
0.863460154972134));
#97538=CARTESIAN_POINT('Ctrl Pts',(-8.85,-10.67423561284,0.662394292390999));
#97539=CARTESIAN_POINT('Ctrl Pts',(-8.85,-10.67423561284,0.284928828397001));
#97540=CARTESIAN_POINT('Ctrl Pts',(-8.84334932535928,-10.6364428532682,
0.083862965815866));
#97541=CARTESIAN_POINT('Ctrl Pts',(-8.81931354586398,-10.4832482666981,
-0.285600460274688));
#97542=CARTESIAN_POINT('Ctrl Pts',(-8.80226283219622,-10.367866412925,-0.4540279830806));
#97543=CARTESIAN_POINT('Ctrl Pts',(-8.77015828355847,-10.1019213543007,
-0.719973041704904));
#97544=CARTESIAN_POINT('Ctrl Pts',(-8.75299937723619,-9.93349546234244,
-0.835351913469144));
#97545=CARTESIAN_POINT('Ctrl Pts',(-8.72871516126698,-9.5640376440529,-0.988544335314129));
#97546=CARTESIAN_POINT('Ctrl Pts',(-8.72195505606398,-9.36297374125027,
-1.026338439606));
#97547=CARTESIAN_POINT('Ctrl Pts',(-8.72195505606398,-9.17423561284,-1.026338439606));
#97548=CARTESIAN_POINT('Ctrl Pts',(-8.72195505606398,-8.98549748442973,
-1.026338439606));
#97549=CARTESIAN_POINT('Ctrl Pts',(-8.72871516126698,-8.78443358162711,
-0.988544335314129));
#97550=CARTESIAN_POINT('Ctrl Pts',(-8.75299937723619,-8.41497576333756,
-0.835351913469143));
#97551=CARTESIAN_POINT('Ctrl Pts',(-8.77015828355848,-8.24654987137926,
-0.719973041704905));
#97552=CARTESIAN_POINT('Ctrl Pts',(-8.80226283219622,-7.98060481275496,
-0.4540279830806));
#97553=CARTESIAN_POINT('Ctrl Pts',(-8.81931354586398,-7.86522295898186,
-0.285600460274688));
#97554=CARTESIAN_POINT('Ctrl Pts',(-8.84334932535928,-7.71202837241176,
0.0838629658158672));
#97555=CARTESIAN_POINT('Ctrl Pts',(-8.85,-7.67423561284,0.284928828397001));
#97556=CARTESIAN_POINT('Ctrl Pts',(-8.85,-7.67423561284,0.473661560394));
#97557=CARTESIAN_POINT('',(-5.44794311523,-10.2348957846198,1.53432173217382));
#97558=CARTESIAN_POINT('',(7.85,-10.2348957846198,1.53432173217382));
#97559=CARTESIAN_POINT('Origin',(-5.44794311523,-9.17423561284,0.473661560394));
#97560=CARTESIAN_POINT('Origin',(-6.61089801788,-14.9244482822,0.473661560394));
#97561=CARTESIAN_POINT('',(-6.61089801788,-14.9244482822,-5.41008957278));
#97562=CARTESIAN_POINT('',(-6.61089801788,-9.92423561284,-5.41008957278));
#97563=CARTESIAN_POINT('',(-6.61089801788,-12.0242356128,-5.41008957278));
#97564=CARTESIAN_POINT('',(-6.61089801788,-14.9244482822,-0.276338439606));
#97565=CARTESIAN_POINT('',(-6.61089801788,-14.9244482822,-2.84321400619));
#97566=CARTESIAN_POINT('',(-6.61089801788,-12.6613939106,-0.276338439606));
#97567=CARTESIAN_POINT('',(-6.61089801788,-13.7929210964,-0.276338439606));
#97568=CARTESIAN_POINT('',(-6.61089801788,-10.2242096029,-2.07631242966));
#97569=CARTESIAN_POINT('Origin',(-6.61089801788,-10.2242096029,0.473661560394));
#97570=CARTESIAN_POINT('',(-6.61089801788,-9.92423561284,-2.07631242966));
#97571=CARTESIAN_POINT('',(-6.61089801788,-10.0742226079,-2.07631242966));
#97572=CARTESIAN_POINT('',(-6.61089801788,-9.92423561284,-3.74320100122));
#97573=CARTESIAN_POINT('Origin',(4.,-9.92423561284,10.9094726032));
#97574=CARTESIAN_POINT('',(-8.47467596136,-9.92423561284,-2.07631242966));
#97575=CARTESIAN_POINT('',(-7.54278698962,-9.92423561284,-2.07631242966));
#97576=CARTESIAN_POINT('Origin',(0.,-9.92423561284,0.473661560394));
#97577=CARTESIAN_POINT('Origin',(9.7,-9.17423561284,-2.07631242966));
#97578=CARTESIAN_POINT('',(-8.47467596136,-10.2242096029,-2.07631242966));
#97579=CARTESIAN_POINT('',(-8.47467596136,-9.81495241206,-2.07631242966));
#97580=CARTESIAN_POINT('',(7.23999999989,-10.2242096029,-2.07631242966));
#97581=CARTESIAN_POINT('Origin',(7.23999999989,-10.2242096029,0.473661560394));
#97582=CARTESIAN_POINT('',(-8.81816307332978,-12.6613939105328,-0.276338439790844));
#97583=CARTESIAN_POINT('Ctrl Pts',(-8.81816307399792,-12.6613939105698,
-0.276338439859058));
#97584=CARTESIAN_POINT('Ctrl Pts',(-8.81159014191855,-12.6376118819527,
-0.353620022433216));
#97585=CARTESIAN_POINT('Ctrl Pts',(-8.80407126472156,-12.6100918009648,
-0.429935532759619));
#97586=CARTESIAN_POINT('Ctrl Pts',(-8.76084293562039,-12.4486247941201,
-0.818571700939171));
#97587=CARTESIAN_POINT('Ctrl Pts',(-8.71126631028426,-12.2526596929331,
-1.10409615000023));
#97588=CARTESIAN_POINT('Ctrl Pts',(-8.61746290023769,-11.8019105710455,
-1.55484527188781));
#97589=CARTESIAN_POINT('Ctrl Pts',(-8.56695493619419,-11.516409326613,-1.75076635383017));
#97590=CARTESIAN_POINT('Ctrl Pts',(-8.49497179593289,-10.8887452246525,
-2.01154492600502));
#97591=CARTESIAN_POINT('Ctrl Pts',(-8.47467596136091,-10.5464102971449,
-2.076312429656));
#97592=CARTESIAN_POINT('Ctrl Pts',(-8.47467596136091,-10.2242096029,-2.076312429656));
#97593=CARTESIAN_POINT('',(-7.71453053854,-12.6613939106,-0.276338439606));
#97594=CARTESIAN_POINT('Origin',(4.,-11.2955559564,-0.276338439606));
#97595=CARTESIAN_POINT('',(-8.81816307402,-14.9244482822,-0.276338439606));
#97596=CARTESIAN_POINT('',(-8.81816307402,-9.81495241206,-0.276338439606));
#97597=CARTESIAN_POINT('',(-7.71453054595,-14.9244482822,-0.276338439606));
#97598=CARTESIAN_POINT('Origin',(13.7258691788,-14.9244482822,0.473661560394));
#97599=CARTESIAN_POINT('Origin',(0.,-14.9244482822,0.473661560394));
#97600=CARTESIAN_POINT('Origin',(6.61089801788,-5.78170707891,0.473661560394));
#97601=CARTESIAN_POINT('',(-8.81816307402,-5.78170707891,-0.276338439606));
#97602=CARTESIAN_POINT('',(-6.61089801788,-5.78170707891,-5.41008957278));
#97603=CARTESIAN_POINT('Origin',(0.,-5.78170707891,0.473661560394));
#97604=CARTESIAN_POINT('',(-6.61089801788,-5.78170707891,-0.276338439606));
#97605=CARTESIAN_POINT('',(-6.61089801788,-5.78170707891,-2.84321400619));
#97606=CARTESIAN_POINT('',(-7.71453054595,-5.78170707891,-0.276338439606));
#97607=CARTESIAN_POINT('Origin',(-6.61089801788,-14.9244482822,0.473661560394));
#97608=CARTESIAN_POINT('',(-6.61089801788,-8.42423561284,-5.41008957278));
#97609=CARTESIAN_POINT('',(-6.61089801788,-12.0242356128,-5.41008957278));
#97610=CARTESIAN_POINT('',(-6.61089801788,-8.42423561284,-1.963549961));
#97611=CARTESIAN_POINT('',(-6.61089801788,-8.42423561284,-3.68681976689));
#97612=CARTESIAN_POINT('',(-6.61089801788,-6.73702409145,-0.276338439606));
#97613=CARTESIAN_POINT('Origin',(-6.61089801788,-9.17423561284,0.473661560394));
#97614=CARTESIAN_POINT('',(-6.61089801788,-6.25936558518,-0.276338439606));
#97615=CARTESIAN_POINT('Origin',(4.,-11.2955559564,-0.276338439606));
#97616=CARTESIAN_POINT('',(-8.81816307402,-6.73702409145,-0.276338439606));
#97617=CARTESIAN_POINT('',(-8.81816307402,-9.81495241206,-0.276338439606));
#97618=CARTESIAN_POINT('',(7.85,-6.73702409145,-0.276338439606));
#97619=CARTESIAN_POINT('Origin',(7.85,-9.17423561284,0.473661560394));
#97620=CARTESIAN_POINT('',(-8.50779054749,-8.42423561284,-1.963549961));
#97621=CARTESIAN_POINT('',(-7.55934428269,-8.42423561284,-1.963549961));
#97622=CARTESIAN_POINT('Ctrl Pts',(-8.50779054749224,-8.42423561284108,
-1.96354996099712));
#97623=CARTESIAN_POINT('Ctrl Pts',(-8.51460395755545,-8.34694619186505,
-1.93976578583499));
#97624=CARTESIAN_POINT('Ctrl Pts',(-8.52238203382313,-8.27062509791715,
-1.91224351726085));
#97625=CARTESIAN_POINT('Ctrl Pts',(-8.5669490755189,-7.88202266221689,-1.75078901559462));
#97626=CARTESIAN_POINT('Ctrl Pts',(-8.61745809932542,-7.59651853184558,
-1.55486594266297));
#97627=CARTESIAN_POINT('Ctrl Pts',(-8.71126345553147,-7.14576485501596,
-1.10411226583335));
#97628=CARTESIAN_POINT('Ctrl Pts',(-8.76084110174091,-6.94979776054387,
-0.818584929648812));
#97629=CARTESIAN_POINT('Ctrl Pts',(-8.80407059609266,-6.78832806722135,
-0.429942320036869));
#97630=CARTESIAN_POINT('Ctrl Pts',(-8.811589850943,-6.76080690738505,-0.353623443619236));
#97631=CARTESIAN_POINT('Ctrl Pts',(-8.81816307401943,-6.73702409144926,
-0.276338439606178));
#97632=CARTESIAN_POINT('Origin',(4.,-8.42423561284,10.9094726032));
#97633=CARTESIAN_POINT('Origin',(0.,-8.42423561284,0.473661560394));
#97634=CARTESIAN_POINT('Origin',(-6.61089801788,-14.9244482822,0.473661560394));
#97635=CARTESIAN_POINT('',(-6.61089801788,-8.42423561284,6.35741269357));
#97636=CARTESIAN_POINT('',(-6.61089801788,-5.78170707891,6.35741269357));
#97637=CARTESIAN_POINT('',(-6.61089801788,-12.0242356128,6.35741269357));
#97638=CARTESIAN_POINT('',(-6.61089801788,-5.78170707891,1.22366156039));
#97639=CARTESIAN_POINT('',(-6.61089801788,-5.78170707891,3.79053712698));
#97640=CARTESIAN_POINT('',(-6.61089801788,-6.73702409145,1.22366156039));
#97641=CARTESIAN_POINT('',(-6.61089801788,-6.25936558518,1.22366156039));
#97642=CARTESIAN_POINT('',(-6.61089801788,-8.42423561284,2.91087308178));
#97643=CARTESIAN_POINT('Origin',(-6.61089801788,-9.17423561284,0.473661560394));
#97644=CARTESIAN_POINT('',(-6.61089801788,-8.42423561284,4.63414288768));
#97645=CARTESIAN_POINT('Origin',(4.,-8.42423561284,10.9094726032));
#97646=CARTESIAN_POINT('',(-8.50779054749,-8.42423561284,2.91087308178));
#97647=CARTESIAN_POINT('Origin',(0.,-8.42423561284,0.473661560394));
#97648=CARTESIAN_POINT('',(7.85,-8.42423561284,2.91087308178));
#97649=CARTESIAN_POINT('Origin',(7.85,-9.17423561284,0.473661560394));
#97650=CARTESIAN_POINT('',(-8.81816307402,-6.73702409145,1.22366156039));
#97651=CARTESIAN_POINT('',(-7.71453054595,-6.73702409145,1.22366156039));
#97652=CARTESIAN_POINT('Ctrl Pts',(-8.50779054749244,-8.42423561283885,
2.91087308178444));
#97653=CARTESIAN_POINT('Ctrl Pts',(-8.5146039575556,-8.34694619186358,2.88708890662246));
#97654=CARTESIAN_POINT('Ctrl Pts',(-8.52238203382321,-8.27062509791643,
2.85956663804855));
#97655=CARTESIAN_POINT('Ctrl Pts',(-8.5669490755189,-7.88202266221689,2.69811213638263));
#97656=CARTESIAN_POINT('Ctrl Pts',(-8.61745809932542,-7.59651853184558,
2.50218906345097));
#97657=CARTESIAN_POINT('Ctrl Pts',(-8.71126345553147,-7.14576485501596,
2.05143538662135));
#97658=CARTESIAN_POINT('Ctrl Pts',(-8.76084110174091,-6.94979776054387,
1.76590805043681));
#97659=CARTESIAN_POINT('Ctrl Pts',(-8.80407059609279,-6.78832806722086,
1.3772654408237));
#97660=CARTESIAN_POINT('Ctrl Pts',(-8.81158985094324,-6.76080690738419,
1.30094656440485));
#97661=CARTESIAN_POINT('Ctrl Pts',(-8.81816307401973,-6.73702409144815,
1.22366156039055));
#97662=CARTESIAN_POINT('Origin',(4.,-2.81495241206,1.22366156039));
#97663=CARTESIAN_POINT('',(-8.81816307402,-5.78170707891,1.22366156039));
#97664=CARTESIAN_POINT('',(-7.71453054595,-5.78170707891,1.22366156039));
#97665=CARTESIAN_POINT('',(-8.81816307402,-9.81495241206,1.22366156039));
#97666=CARTESIAN_POINT('Origin',(6.61089801788,-5.78170707891,0.473661560394));
#97667=CARTESIAN_POINT('Origin',(0.,-5.78170707891,0.473661560394));
#97668=CARTESIAN_POINT('Origin',(13.7258691788,-14.9244482822,0.473661560394));
#97669=CARTESIAN_POINT('',(-8.81816307402,-14.9244482822,1.22366156039));
#97670=CARTESIAN_POINT('',(-6.61089801788,-14.9244482822,6.35741269357));
#97671=CARTESIAN_POINT('Origin',(0.,-14.9244482822,0.473661560394));
#97672=CARTESIAN_POINT('',(-6.61089801788,-14.9244482822,1.22366156039));
#97673=CARTESIAN_POINT('',(-6.61089801788,-14.9244482822,3.79053712698));
#97674=CARTESIAN_POINT('',(-7.71453054595,-14.9244482822,1.22366156039));
#97675=CARTESIAN_POINT('Origin',(-6.61089801788,-14.9244482822,0.473661560394));
#97676=CARTESIAN_POINT('',(-6.61089801788,-9.92423561284,6.35741269357));
#97677=CARTESIAN_POINT('',(-6.61089801788,-12.0242356128,6.35741269357));
#97678=CARTESIAN_POINT('',(-6.61089801788,-9.92423561284,3.02363555044));
#97679=CARTESIAN_POINT('',(-6.61089801788,-9.92423561284,4.69052412201));
#97680=CARTESIAN_POINT('',(-6.61089801788,-10.2242096029,3.02363555044));
#97681=CARTESIAN_POINT('',(-6.61089801788,-10.0742226079,3.02363555044));
#97682=CARTESIAN_POINT('',(-6.61089801788,-12.6613939106,1.22366156039));
#97683=CARTESIAN_POINT('Origin',(-6.61089801788,-10.2242096029,0.473661560394));
#97684=CARTESIAN_POINT('',(-6.61089801788,-13.7929210964,1.22366156039));
#97685=CARTESIAN_POINT('Origin',(4.,-2.81495241206,1.22366156039));
#97686=CARTESIAN_POINT('',(-8.81816307334515,-12.6613939101212,1.22366156090261));
#97687=CARTESIAN_POINT('',(7.23999999989,-12.6613939106,1.22366156039));
#97688=CARTESIAN_POINT('',(-8.81816307402,-9.81495241206,1.22366156039));
#97689=CARTESIAN_POINT('Origin',(7.23999999989,-10.2242096029,0.473661560394));
#97690=CARTESIAN_POINT('',(-8.47467596136,-10.2242096029,3.02363555044));
#97691=CARTESIAN_POINT('Ctrl Pts',(-8.47467596136091,-10.2242096029,3.023635550444));
#97692=CARTESIAN_POINT('Ctrl Pts',(-8.47467596136091,-10.5464102971449,
3.023635550444));
#97693=CARTESIAN_POINT('Ctrl Pts',(-8.49497179593289,-10.8887452246525,
2.95886804679302));
#97694=CARTESIAN_POINT('Ctrl Pts',(-8.56695493619419,-11.516409326613,2.69808947461818));
#97695=CARTESIAN_POINT('Ctrl Pts',(-8.61746290023769,-11.8019105710455,
2.50216839267581));
#97696=CARTESIAN_POINT('Ctrl Pts',(-8.71126631028426,-12.2526596929331,
2.05141927078824));
#97697=CARTESIAN_POINT('Ctrl Pts',(-8.76084293562039,-12.4486247941201,
1.76589482172717));
#97698=CARTESIAN_POINT('Ctrl Pts',(-8.80407126470694,-12.6100918009102,
1.37725865367903));
#97699=CARTESIAN_POINT('Ctrl Pts',(-8.81159014189213,-12.637611881856,1.30094314348955));
#97700=CARTESIAN_POINT('Ctrl Pts',(-8.81816307396325,-12.6613939104444,
1.22366156105464));
#97701=CARTESIAN_POINT('',(-7.54278698962,-10.2242096029,3.02363555044));
#97702=CARTESIAN_POINT('Origin',(9.7,-9.17423561284,3.02363555044));
#97703=CARTESIAN_POINT('',(-8.47467596136,-9.92423561284,3.02363555044));
#97704=CARTESIAN_POINT('',(-8.47467596136,-9.81495241206,3.02363555044));
#97705=CARTESIAN_POINT('',(-7.54278698962,-9.92423561284,3.02363555044));
#97706=CARTESIAN_POINT('Origin',(4.,-9.92423561284,10.9094726032));
#97707=CARTESIAN_POINT('Origin',(0.,-9.92423561284,0.473661560394));
#97708=CARTESIAN_POINT('Origin',(13.7258691788,-16.4244482822,0.473661560394));
#97709=CARTESIAN_POINT('',(-6.,-16.4244482822,4.71895306982));
#97710=CARTESIAN_POINT('',(-6.,-16.4244482822,-3.77162994903));
#97711=CARTESIAN_POINT('Origin',(0.,-16.4244482822,0.473661560394));
#97712=CARTESIAN_POINT('',(-6.,-16.4244482822,0.348630985699));
#97713=CARTESIAN_POINT('Origin',(13.7258691788,-16.4244482822,0.473661560394));
#97714=CARTESIAN_POINT('',(6.,-16.4244482822,-3.77162994903));
#97715=CARTESIAN_POINT('',(6.,-16.4244482822,4.71895306982));
#97716=CARTESIAN_POINT('Origin',(0.,-16.4244482822,0.473661560394));
#97717=CARTESIAN_POINT('',(6.,-16.4244482822,0.348630985699));
#97718=CARTESIAN_POINT('Origin',(0.,-12.0242356128,0.473661560394));
#97719=CARTESIAN_POINT('',(6.,-12.7742356128,4.71895306982));
#97720=CARTESIAN_POINT('',(6.,-12.7742356128,-3.77162994903));
#97721=CARTESIAN_POINT('Origin',(0.,-12.0242356128,0.473661560394));
#97722=CARTESIAN_POINT('',(-6.,-12.7742356128,4.71895306982));
#97723=CARTESIAN_POINT('',(-6.,-12.7742356128,-3.77162994903));
#97724=CARTESIAN_POINT('Origin',(0.,-18.1742356128,0.473661560394));
#97725=CARTESIAN_POINT('',(-4.84699160505,-18.1742356128,7.87833389485));
#97726=CARTESIAN_POINT('',(4.84699160505,-18.1742356128,7.87833389485));
#97727=CARTESIAN_POINT('Origin',(0.,-18.1742356128,0.473661560394));
#97728=CARTESIAN_POINT('',(-4.2,-18.1742356128,7.9986309857));
#97729=CARTESIAN_POINT('Origin',(-4.2,-18.1742356128,6.1986309857));
#97730=CARTESIAN_POINT('',(4.2,-18.1742356128,7.9986309857));
#97731=CARTESIAN_POINT('',(0.,-18.1742356128,7.9986309857));
#97732=CARTESIAN_POINT('Origin',(4.2,-18.1742356128,6.1986309857));
#97733=CARTESIAN_POINT('Origin',(-6.,-4.67423561284,6.4986309857));
#97734=CARTESIAN_POINT('',(-6.,-19.3742356128,0.473661560394));
#97735=CARTESIAN_POINT('Origin',(6.,-4.67423561284,6.4986309857));
#97736=CARTESIAN_POINT('',(6.,-19.3742356128,0.473661560394));
#97737=CARTESIAN_POINT('Origin',(0.,-18.0242356128,0.473661560394));
#97738=CARTESIAN_POINT('',(-4.84699160505,-19.3742356128,7.87833389485));
#97739=CARTESIAN_POINT('',(4.84699160505,-19.3742356128,7.87833389485));
#97740=CARTESIAN_POINT('Origin',(0.,-19.3742356128,0.473661560394));
#97741=CARTESIAN_POINT('',(-4.84699160505,-12.7742356128,7.87833389485));
#97742=CARTESIAN_POINT('',(4.84699160505,-12.7742356128,7.87833389485));
#97743=CARTESIAN_POINT('Origin',(4.2,-13.6742356128,6.1986309857));
#97744=CARTESIAN_POINT('',(4.2,-19.3742356128,7.9986309857));
#97745=CARTESIAN_POINT('Origin',(4.2,-19.3742356128,6.1986309857));
#97746=CARTESIAN_POINT('',(4.2,-12.7742356128,7.9986309857));
#97747=CARTESIAN_POINT('Origin',(0.,-4.67423561284,7.9986309857));
#97748=CARTESIAN_POINT('',(-4.2,-19.3742356128,7.9986309857));
#97749=CARTESIAN_POINT('',(-4.2,-12.7742356128,7.9986309857));
#97750=CARTESIAN_POINT('',(0.,-19.3742356128,7.9986309857));
#97751=CARTESIAN_POINT('Origin',(-4.2,-13.6742356128,6.1986309857));
#97752=CARTESIAN_POINT('Origin',(-4.2,-19.3742356128,6.1986309857));
#97753=CARTESIAN_POINT('Origin',(7.85,-9.17423561284,0.473661560394));
#97754=CARTESIAN_POINT('',(4.5,-10.2348957846198,1.53432173217382));
#97755=CARTESIAN_POINT('Origin',(4.5,-9.17423561284,0.473661560394));
#97756=CARTESIAN_POINT('',(8.78621078736448,-10.2348957846198,1.53432173217382));
#97757=CARTESIAN_POINT('',(7.85,-10.2348957846198,1.53432173217382));
#97758=CARTESIAN_POINT('',(8.85,-10.6742356128,0.473661560394));
#97759=CARTESIAN_POINT('Ctrl Pts',(8.78621078736448,-10.2348957846198,1.53432173217382));
#97760=CARTESIAN_POINT('Ctrl Pts',(8.80226283219622,-10.367866412925,1.4013511038686));
#97761=CARTESIAN_POINT('Ctrl Pts',(8.81931354586398,-10.4832482666981,1.23292358106269));
#97762=CARTESIAN_POINT('Ctrl Pts',(8.84334932535928,-10.6364428532682,0.863460154972133));
#97763=CARTESIAN_POINT('Ctrl Pts',(8.85,-10.67423561284,0.662394292390999));
#97764=CARTESIAN_POINT('Ctrl Pts',(8.85,-10.67423561284,0.473661560394));
#97765=CARTESIAN_POINT('Ctrl Pts',(8.85,-10.67423561284,0.473661560394));
#97766=CARTESIAN_POINT('Ctrl Pts',(8.85,-10.67423561284,0.284928828397001));
#97767=CARTESIAN_POINT('Ctrl Pts',(8.84334932535928,-10.6364428532682,0.0838629658158659));
#97768=CARTESIAN_POINT('Ctrl Pts',(8.81931354586398,-10.4832482666981,-0.285600460274688));
#97769=CARTESIAN_POINT('Ctrl Pts',(8.80226283219622,-10.367866412925,-0.454027983080601));
#97770=CARTESIAN_POINT('Ctrl Pts',(8.77015828355848,-10.1019213543007,-0.719973041704905));
#97771=CARTESIAN_POINT('Ctrl Pts',(8.75299937723619,-9.93349546234244,-0.835351913469143));
#97772=CARTESIAN_POINT('Ctrl Pts',(8.72871516126698,-9.5640376440529,-0.988544335314129));
#97773=CARTESIAN_POINT('Ctrl Pts',(8.72195505606398,-9.36297374125027,-1.026338439606));
#97774=CARTESIAN_POINT('Ctrl Pts',(8.72195505606398,-9.17423561284,-1.026338439606));
#97775=CARTESIAN_POINT('Ctrl Pts',(8.72195505606398,-8.98549748442973,-1.026338439606));
#97776=CARTESIAN_POINT('Ctrl Pts',(8.72871516126698,-8.7844335816271,-0.988544335314129));
#97777=CARTESIAN_POINT('Ctrl Pts',(8.75299937723619,-8.41497576333756,-0.835351913469142));
#97778=CARTESIAN_POINT('Ctrl Pts',(8.77015828355848,-8.24654987137926,-0.719973041704905));
#97779=CARTESIAN_POINT('Ctrl Pts',(8.80226283219622,-7.98060481275496,-0.4540279830806));
#97780=CARTESIAN_POINT('Ctrl Pts',(8.81931354586398,-7.86522295898186,-0.285600460274688));
#97781=CARTESIAN_POINT('Ctrl Pts',(8.84334932535928,-7.71202837241176,0.083862965815867));
#97782=CARTESIAN_POINT('Ctrl Pts',(8.85,-7.67423561284,0.284928828397001));
#97783=CARTESIAN_POINT('Ctrl Pts',(8.85,-7.67423561284,0.662394292391));
#97784=CARTESIAN_POINT('Ctrl Pts',(8.84334932535928,-7.71202837241176,0.863460154972134));
#97785=CARTESIAN_POINT('Ctrl Pts',(8.81931354586398,-7.86522295898186,1.23292358106269));
#97786=CARTESIAN_POINT('Ctrl Pts',(8.80226283219622,-7.98060481275496,1.4013511038686));
#97787=CARTESIAN_POINT('Ctrl Pts',(8.77015828355848,-8.24654987137926,1.66729616249291));
#97788=CARTESIAN_POINT('Ctrl Pts',(8.75299937723619,-8.41497576333756,1.78267503425714));
#97789=CARTESIAN_POINT('Ctrl Pts',(8.72871516126698,-8.78443358162711,1.93586745610213));
#97790=CARTESIAN_POINT('Ctrl Pts',(8.72195505606398,-8.98549748442973,1.973661560394));
#97791=CARTESIAN_POINT('Ctrl Pts',(8.72195505606398,-9.36297374125027,1.973661560394));
#97792=CARTESIAN_POINT('Ctrl Pts',(8.72871516126698,-9.5640376440529,1.93586745610213));
#97793=CARTESIAN_POINT('Ctrl Pts',(8.75299937723619,-9.93349546234245,1.78267503425714));
#97794=CARTESIAN_POINT('Ctrl Pts',(8.77015828355847,-10.1019213543007,1.6672961624929));
#97795=CARTESIAN_POINT('Ctrl Pts',(8.78621078736448,-10.2348957846198,1.53432173217382));
#97796=CARTESIAN_POINT('Origin',(4.,-9.92423561284,10.9094726032));
#97797=CARTESIAN_POINT('',(6.61089801788,-9.92423561284,-5.41008957278));
#97798=CARTESIAN_POINT('',(8.47467596136,-9.92423561284,-2.07631242966));
#97799=CARTESIAN_POINT('Origin',(0.,-9.92423561284,0.473661560394));
#97800=CARTESIAN_POINT('',(6.61089801788,-9.92423561284,-2.07631242966));
#97801=CARTESIAN_POINT('',(7.54278698962,-9.92423561284,-2.07631242966));
#97802=CARTESIAN_POINT('',(6.61089801788,-9.92423561284,-3.74320100122));
#97803=CARTESIAN_POINT('Origin',(9.7,-9.17423561284,-2.07631242966));
#97804=CARTESIAN_POINT('',(8.47467596136,-10.2242096029,-2.07631242966));
#97805=CARTESIAN_POINT('',(8.47467596136,-9.81495241206,-2.07631242966));
#97806=CARTESIAN_POINT('',(6.61089801788,-10.2242096029,-2.07631242966));
#97807=CARTESIAN_POINT('',(7.23999999989,-10.2242096029,-2.07631242966));
#97808=CARTESIAN_POINT('',(6.61089801788,-10.0742226079,-2.07631242966));
#97809=CARTESIAN_POINT('Origin',(7.23999999989,-10.2242096029,0.473661560394));
#97810=CARTESIAN_POINT('',(8.81816307332978,-12.6613939105328,-0.276338439790844));
#97811=CARTESIAN_POINT('Ctrl Pts',(8.81816307399792,-12.6613939105698,-0.276338439859058));
#97812=CARTESIAN_POINT('Ctrl Pts',(8.81159014191855,-12.6376118819527,-0.353620022433216));
#97813=CARTESIAN_POINT('Ctrl Pts',(8.80407126472156,-12.6100918009648,-0.429935532759619));
#97814=CARTESIAN_POINT('Ctrl Pts',(8.76084293562039,-12.4486247941201,-0.818571700939171));
#97815=CARTESIAN_POINT('Ctrl Pts',(8.71126631028426,-12.2526596929331,-1.10409615000023));
#97816=CARTESIAN_POINT('Ctrl Pts',(8.61746290023769,-11.8019105710455,-1.55484527188781));
#97817=CARTESIAN_POINT('Ctrl Pts',(8.56695493619419,-11.516409326613,-1.75076635383017));
#97818=CARTESIAN_POINT('Ctrl Pts',(8.49497179593289,-10.8887452246525,-2.01154492600502));
#97819=CARTESIAN_POINT('Ctrl Pts',(8.47467596136091,-10.5464102971449,-2.076312429656));
#97820=CARTESIAN_POINT('Ctrl Pts',(8.47467596136091,-10.2242096029,-2.076312429656));
#97821=CARTESIAN_POINT('',(6.61089801788,-12.6613939106,-0.276338439606));
#97822=CARTESIAN_POINT('',(7.71453053854,-12.6613939106,-0.276338439606));
#97823=CARTESIAN_POINT('Origin',(6.61089801788,-10.2242096029,0.473661560394));
#97824=CARTESIAN_POINT('Origin',(4.,-11.2955559564,-0.276338439606));
#97825=CARTESIAN_POINT('',(8.81816307402,-14.9244482822,-0.276338439606));
#97826=CARTESIAN_POINT('',(6.61089801788,-14.9244482822,-0.276338439606));
#97827=CARTESIAN_POINT('',(7.71453054595,-14.9244482822,-0.276338439606));
#97828=CARTESIAN_POINT('',(6.61089801788,-13.7929210964,-0.276338439606));
#97829=CARTESIAN_POINT('',(8.81816307402,-9.81495241206,-0.276338439606));
#97830=CARTESIAN_POINT('Origin',(4.,-2.81495241206,1.22366156039));
#97831=CARTESIAN_POINT('',(8.81816307334515,-12.6613939101212,1.22366156090261));
#97832=CARTESIAN_POINT('',(8.81816307402,-14.9244482822,1.22366156039));
#97833=CARTESIAN_POINT('',(8.81816307402,-9.81495241206,1.22366156039));
#97834=CARTESIAN_POINT('',(6.61089801788,-12.6613939106,1.22366156039));
#97835=CARTESIAN_POINT('',(7.23999999989,-12.6613939106,1.22366156039));
#97836=CARTESIAN_POINT('',(6.61089801788,-14.9244482822,1.22366156039));
#97837=CARTESIAN_POINT('',(6.61089801788,-13.7929210964,1.22366156039));
#97838=CARTESIAN_POINT('',(7.71453054595,-14.9244482822,1.22366156039));
#97839=CARTESIAN_POINT('Origin',(7.23999999989,-10.2242096029,0.473661560394));
#97840=CARTESIAN_POINT('',(8.47467596136,-10.2242096029,3.02363555044));
#97841=CARTESIAN_POINT('Ctrl Pts',(8.47467596136091,-10.2242096029,3.023635550444));
#97842=CARTESIAN_POINT('Ctrl Pts',(8.47467596136091,-10.5464102971449,3.023635550444));
#97843=CARTESIAN_POINT('Ctrl Pts',(8.49497179593289,-10.8887452246525,2.95886804679302));
#97844=CARTESIAN_POINT('Ctrl Pts',(8.56695493619419,-11.516409326613,2.69808947461818));
#97845=CARTESIAN_POINT('Ctrl Pts',(8.61746290023769,-11.8019105710455,2.50216839267581));
#97846=CARTESIAN_POINT('Ctrl Pts',(8.71126631028426,-12.2526596929331,2.05141927078824));
#97847=CARTESIAN_POINT('Ctrl Pts',(8.76084293562039,-12.4486247941201,1.76589482172717));
#97848=CARTESIAN_POINT('Ctrl Pts',(8.80407126470694,-12.6100918009102,1.37725865367903));
#97849=CARTESIAN_POINT('Ctrl Pts',(8.81159014189213,-12.637611881856,1.30094314348955));
#97850=CARTESIAN_POINT('Ctrl Pts',(8.81816307396325,-12.6613939104444,1.22366156105464));
#97851=CARTESIAN_POINT('',(6.61089801788,-10.2242096029,3.02363555044));
#97852=CARTESIAN_POINT('',(7.54278698962,-10.2242096029,3.02363555044));
#97853=CARTESIAN_POINT('Origin',(6.61089801788,-10.2242096029,0.473661560394));
#97854=CARTESIAN_POINT('Origin',(9.7,-9.17423561284,3.02363555044));
#97855=CARTESIAN_POINT('',(6.61089801788,-9.92423561284,3.02363555044));
#97856=CARTESIAN_POINT('',(6.61089801788,-10.0742226079,3.02363555044));
#97857=CARTESIAN_POINT('',(8.47467596136,-9.92423561284,3.02363555044));
#97858=CARTESIAN_POINT('',(8.47467596136,-9.81495241206,3.02363555044));
#97859=CARTESIAN_POINT('',(7.54278698962,-9.92423561284,3.02363555044));
#97860=CARTESIAN_POINT('Origin',(4.,-9.92423561284,10.9094726032));
#97861=CARTESIAN_POINT('',(6.61089801788,-9.92423561284,6.35741269357));
#97862=CARTESIAN_POINT('Origin',(0.,-9.92423561284,0.473661560394));
#97863=CARTESIAN_POINT('',(6.61089801788,-9.92423561284,4.69052412201));
#97864=CARTESIAN_POINT('Origin',(4.,-8.42423561284,10.9094726032));
#97865=CARTESIAN_POINT('',(6.61089801788,-8.42423561284,6.35741269357));
#97866=CARTESIAN_POINT('',(6.61089801788,-8.42423561284,2.91087308178));
#97867=CARTESIAN_POINT('',(6.61089801788,-8.42423561284,4.63414288768));
#97868=CARTESIAN_POINT('',(8.50779054749,-8.42423561284,2.91087308178));
#97869=CARTESIAN_POINT('Origin',(0.,-8.42423561284,0.473661560394));
#97870=CARTESIAN_POINT('',(7.85,-8.42423561284,2.91087308178));
#97871=CARTESIAN_POINT('Origin',(7.85,-9.17423561284,0.473661560394));
#97872=CARTESIAN_POINT('',(8.81816307402,-6.73702409145,1.22366156039));
#97873=CARTESIAN_POINT('Ctrl Pts',(8.50779054749244,-8.42423561283885,2.91087308178444));
#97874=CARTESIAN_POINT('Ctrl Pts',(8.5146039575556,-8.34694619186358,2.88708890662246));
#97875=CARTESIAN_POINT('Ctrl Pts',(8.52238203382321,-8.27062509791643,2.85956663804855));
#97876=CARTESIAN_POINT('Ctrl Pts',(8.5669490755189,-7.88202266221689,2.69811213638263));
#97877=CARTESIAN_POINT('Ctrl Pts',(8.61745809932542,-7.59651853184558,2.50218906345097));
#97878=CARTESIAN_POINT('Ctrl Pts',(8.71126345553147,-7.14576485501596,2.05143538662135));
#97879=CARTESIAN_POINT('Ctrl Pts',(8.76084110174091,-6.94979776054387,1.76590805043681));
#97880=CARTESIAN_POINT('Ctrl Pts',(8.80407059609279,-6.78832806722086,1.3772654408237));
#97881=CARTESIAN_POINT('Ctrl Pts',(8.81158985094324,-6.76080690738419,1.30094656440485));
#97882=CARTESIAN_POINT('Ctrl Pts',(8.81816307401973,-6.73702409144815,1.22366156039055));
#97883=CARTESIAN_POINT('',(6.61089801788,-6.73702409145,1.22366156039));
#97884=CARTESIAN_POINT('',(7.71453054595,-6.73702409145,1.22366156039));
#97885=CARTESIAN_POINT('Origin',(6.61089801788,-9.17423561284,0.473661560394));
#97886=CARTESIAN_POINT('Origin',(4.,-2.81495241206,1.22366156039));
#97887=CARTESIAN_POINT('',(8.81816307402,-5.78170707891,1.22366156039));
#97888=CARTESIAN_POINT('',(8.81816307402,-9.81495241206,1.22366156039));
#97889=CARTESIAN_POINT('',(6.61089801788,-5.78170707891,1.22366156039));
#97890=CARTESIAN_POINT('',(7.71453054595,-5.78170707891,1.22366156039));
#97891=CARTESIAN_POINT('',(6.61089801788,-6.25936558518,1.22366156039));
#97892=CARTESIAN_POINT('Origin',(4.,-8.42423561284,10.9094726032));
#97893=CARTESIAN_POINT('',(6.61089801788,-8.42423561284,-1.963549961));
#97894=CARTESIAN_POINT('',(6.61089801788,-8.42423561284,-5.41008957278));
#97895=CARTESIAN_POINT('',(6.61089801788,-8.42423561284,-3.68681976689));
#97896=CARTESIAN_POINT('',(8.50779054749,-8.42423561284,-1.963549961));
#97897=CARTESIAN_POINT('',(7.85,-8.42423561284,-1.963549961));
#97898=CARTESIAN_POINT('Origin',(0.,-8.42423561284,0.473661560394));
#97899=CARTESIAN_POINT('Origin',(7.85,-9.17423561284,0.473661560394));
#97900=CARTESIAN_POINT('',(8.81816307402,-6.73702409145,-0.276338439606));
#97901=CARTESIAN_POINT('',(6.61089801788,-6.73702409145,-0.276338439606));
#97902=CARTESIAN_POINT('',(7.71453054595,-6.73702409145,-0.276338439606));
#97903=CARTESIAN_POINT('Ctrl Pts',(8.50779054749224,-8.42423561284108,-1.96354996099712));
#97904=CARTESIAN_POINT('Ctrl Pts',(8.51460395755545,-8.34694619186505,-1.93976578583499));
#97905=CARTESIAN_POINT('Ctrl Pts',(8.52238203382313,-8.27062509791715,-1.91224351726085));
#97906=CARTESIAN_POINT('Ctrl Pts',(8.5669490755189,-7.88202266221689,-1.75078901559463));
#97907=CARTESIAN_POINT('Ctrl Pts',(8.61745809932542,-7.59651853184558,-1.55486594266297));
#97908=CARTESIAN_POINT('Ctrl Pts',(8.71126345553147,-7.14576485501596,-1.10411226583335));
#97909=CARTESIAN_POINT('Ctrl Pts',(8.76084110174091,-6.94979776054387,-0.818584929648813));
#97910=CARTESIAN_POINT('Ctrl Pts',(8.80407059609266,-6.78832806722135,-0.429942320036871));
#97911=CARTESIAN_POINT('Ctrl Pts',(8.811589850943,-6.76080690738505,-0.353623443619237));
#97912=CARTESIAN_POINT('Ctrl Pts',(8.81816307401943,-6.73702409144926,-0.276338439606177));
#97913=CARTESIAN_POINT('Origin',(6.61089801788,-9.17423561284,0.473661560394));
#97914=CARTESIAN_POINT('Origin',(4.,-11.2955559564,-0.276338439606));
#97915=CARTESIAN_POINT('',(6.61089801788,-5.78170707891,-0.276338439606));
#97916=CARTESIAN_POINT('',(6.61089801788,-6.25936558518,-0.276338439606));
#97917=CARTESIAN_POINT('',(8.81816307402,-5.78170707891,-0.276338439606));
#97918=CARTESIAN_POINT('',(7.71453054595,-5.78170707891,-0.276338439606));
#97919=CARTESIAN_POINT('',(8.81816307402,-9.81495241206,-0.276338439606));
#97920=CARTESIAN_POINT('Origin',(-4.8,-19.0742356128,-2.12633843961));
#97921=CARTESIAN_POINT('',(-4.8,-19.3742356128,-5.5013690143));
#97922=CARTESIAN_POINT('Origin',(-4.8,-19.0742356128,-5.5013690143));
#97923=CARTESIAN_POINT('',(-4.8,-19.3742356128,6.1986309857));
#97924=CARTESIAN_POINT('Origin',(-4.8,-19.0742356128,6.1986309857));
#97925=CARTESIAN_POINT('',(-4.8,-19.3742356128,0.348630985699));
#97926=CARTESIAN_POINT('Origin',(0.,-19.3742356128,0.473661560394));
#97927=CARTESIAN_POINT('',(-8.4371184738,-19.3742356128,6.46845362177));
#97928=CARTESIAN_POINT('',(-10.7402266336,-19.3742356128,6.46845362177));
#97929=CARTESIAN_POINT('',(-9.58867255369,-19.3742356128,6.46845362177));
#97930=CARTESIAN_POINT('',(-6.81380166599,-19.3742356128,-9.7665584986));
#97931=CARTESIAN_POINT('Origin',(0.,-19.3742356128,0.473661560394));
#97932=CARTESIAN_POINT('',(-6.67999195052,-19.3742356128,-10.0163199635));
#97933=CARTESIAN_POINT('Origin',(-6.97999195052,-19.3742356128,-10.0163199635));
#97934=CARTESIAN_POINT('',(-6.67999195052,-19.3742356128,-13.3776272862));
#97935=CARTESIAN_POINT('',(-6.67999195052,-19.3742356128,-11.6969736248));
#97936=CARTESIAN_POINT('',(-6.5054999889,-19.3742356128,-13.6501116569));
#97937=CARTESIAN_POINT('Origin',(-6.37999195052,-19.3742356128,-13.3776272862));
#97938=CARTESIAN_POINT('',(-5.2992520131,-19.3742356128,-14.1455185843));
#97939=CARTESIAN_POINT('Origin',(0.,-19.3742356128,0.473661560394));
#97940=CARTESIAN_POINT('',(-4.92636192076,-19.3742356128,-13.9928850408));
#97941=CARTESIAN_POINT('Origin',(-5.19701563986,-19.3742356128,-13.8634765236));
#97942=CARTESIAN_POINT('',(-4.56454191842,-19.3742356128,-13.8364811917));
#97943=CARTESIAN_POINT('Origin',(-4.65570820166,-19.3742356128,-14.1222935581));
#97944=CARTESIAN_POINT('',(-3.37623759365,-19.3742356128,-14.1624666237));
#97945=CARTESIAN_POINT('Origin',(0.,-19.3742356128,0.473661560394));
#97946=CARTESIAN_POINT('',(-3.1436702163,-19.3742356128,-14.4547898034));
#97947=CARTESIAN_POINT('Origin',(-3.4436702163,-19.3742356128,-14.4547898034));
#97948=CARTESIAN_POINT('',(-3.1436702163,-19.3742356128,-14.5088629165));
#97949=CARTESIAN_POINT('',(-3.1436702163,-19.3742356128,-14.48182636));
#97950=CARTESIAN_POINT('',(-2.89961126973,-19.3742356128,-14.8036011029));
#97951=CARTESIAN_POINT('Origin',(-2.8436702163,-19.3742356128,-14.5088629165));
#97952=CARTESIAN_POINT('',(2.89961126973,-19.3742356128,-14.8036011029));
#97953=CARTESIAN_POINT('Origin',(0.,-19.3742356128,0.473661560394));
#97954=CARTESIAN_POINT('',(3.1436702163,-19.3742356128,-14.5088629165));
#97955=CARTESIAN_POINT('Origin',(2.8436702163,-19.3742356128,-14.5088629165));
#97956=CARTESIAN_POINT('',(3.1436702163,-19.3742356128,-14.4547898034));
#97957=CARTESIAN_POINT('',(3.1436702163,-19.3742356128,-14.48182636));
#97958=CARTESIAN_POINT('',(3.37623759365,-19.3742356128,-14.1624666237));
#97959=CARTESIAN_POINT('Origin',(3.4436702163,-19.3742356128,-14.4547898034));
#97960=CARTESIAN_POINT('',(4.62312919377,-19.3742356128,-13.8176611554));
#97961=CARTESIAN_POINT('Origin',(0.,-19.3742356128,0.473661560394));
#97962=CARTESIAN_POINT('',(4.98558691274,-19.3742356128,-13.9725813932));
#97963=CARTESIAN_POINT('Origin',(4.71546562382,-19.3742356128,-14.1030976346));
#97964=CARTESIAN_POINT('',(5.35909918268,-19.3742356128,-14.1236860052));
#97965=CARTESIAN_POINT('Origin',(5.25570820166,-19.3742356128,-13.8420651518));
#97966=CARTESIAN_POINT('',(6.5054999889,-19.3742356128,-13.6501116569));
#97967=CARTESIAN_POINT('Origin',(0.,-19.3742356128,0.473661560394));
#97968=CARTESIAN_POINT('',(6.67999195052,-19.3742356128,-13.3776272862));
#97969=CARTESIAN_POINT('Origin',(6.37999195052,-19.3742356128,-13.3776272862));
#97970=CARTESIAN_POINT('',(6.67999195052,-19.3742356128,-10.0163199635));
#97971=CARTESIAN_POINT('',(6.67999195052,-19.3742356128,-11.6969736248));
#97972=CARTESIAN_POINT('',(6.81380166599,-19.3742356128,-9.7665584986));
#97973=CARTESIAN_POINT('Origin',(6.97999195052,-19.3742356128,-10.0163199635));
#97974=CARTESIAN_POINT('',(10.7402266336,-19.3742356128,6.46845362177));
#97975=CARTESIAN_POINT('Origin',(0.,-19.3742356128,0.473661560394));
#97976=CARTESIAN_POINT('',(8.4371184738,-19.3742356128,6.46845362177));
#97977=CARTESIAN_POINT('',(9.58867255369,-19.3742356128,6.46845362177));
#97978=CARTESIAN_POINT('Origin',(0.,-19.3742356128,0.473661560394));
#97979=CARTESIAN_POINT('Origin',(-4.2,-19.3742356128,-5.5013690143));
#97980=CARTESIAN_POINT('',(-4.2,-19.3742356128,6.7986309857));
#97981=CARTESIAN_POINT('Origin',(-4.2,-19.3742356128,6.1986309857));
#97982=CARTESIAN_POINT('',(4.2,-19.3742356128,6.7986309857));
#97983=CARTESIAN_POINT('',(0.,-19.3742356128,6.7986309857));
#97984=CARTESIAN_POINT('',(4.8,-19.3742356128,6.1986309857));
#97985=CARTESIAN_POINT('Origin',(4.2,-19.3742356128,6.1986309857));
#97986=CARTESIAN_POINT('',(4.8,-19.3742356128,-5.5013690143));
#97987=CARTESIAN_POINT('',(4.8,-19.3742356128,-2.12633843961));
#97988=CARTESIAN_POINT('Origin',(4.2,-19.3742356128,-5.5013690143));
#97989=CARTESIAN_POINT('Origin',(0.,-18.0242356128,0.473661560394));
#97990=CARTESIAN_POINT('',(-6.81380166599,-16.6742356128,-9.7665584986));
#97991=CARTESIAN_POINT('',(-6.81380166599,-18.0242356128,-9.7665584986));
#97992=CARTESIAN_POINT('',(-10.7402266336,-16.6742356128,6.46845362177));
#97993=CARTESIAN_POINT('',(-10.7402266336,-18.0242356128,6.46845362177));
#97994=CARTESIAN_POINT('Origin',(0.,-16.6742356128,0.473661560394));
#97995=CARTESIAN_POINT('Origin',(10.7402266336,-19.3742356128,6.46845362177));
#97996=CARTESIAN_POINT('',(-8.4371184738,-16.6742356128,6.46845362177));
#97997=CARTESIAN_POINT('',(-8.4371184738,-18.0242356128,6.46845362177));
#97998=CARTESIAN_POINT('',(-9.58867255369,-16.6742356128,6.46845362177));
#97999=CARTESIAN_POINT('Origin',(0.,-18.0242356128,0.473661560394));
#98000=CARTESIAN_POINT('',(8.4371184738,-16.6742356128,6.46845362177));
#98001=CARTESIAN_POINT('Origin',(0.,-16.6742356128,0.473661560394));
#98002=CARTESIAN_POINT('',(8.4371184738,-18.0242356128,6.46845362177));
#98003=CARTESIAN_POINT('Origin',(10.7402266336,-19.3742356128,6.46845362177));
#98004=CARTESIAN_POINT('',(10.7402266336,-16.6742356128,6.46845362177));
#98005=CARTESIAN_POINT('',(10.7402266336,-18.0242356128,6.46845362177));
#98006=CARTESIAN_POINT('',(9.58867255369,-16.6742356128,6.46845362177));
#98007=CARTESIAN_POINT('Origin',(0.,-18.0242356128,0.473661560394));
#98008=CARTESIAN_POINT('',(6.81380166599,-16.6742356128,-9.7665584986));
#98009=CARTESIAN_POINT('',(6.81380166599,-18.0242356128,-9.7665584986));
#98010=CARTESIAN_POINT('Origin',(0.,-16.6742356128,0.473661560394));
#98011=CARTESIAN_POINT('Origin',(6.97999195052,-18.0242356128,-10.0163199635));
#98012=CARTESIAN_POINT('',(6.67999195052,-16.6742356128,-10.0163199635));
#98013=CARTESIAN_POINT('',(6.67999195052,-18.0242356128,-10.0163199635));
#98014=CARTESIAN_POINT('Origin',(6.97999195052,-16.6742356128,-10.0163199635));
#98015=CARTESIAN_POINT('Origin',(6.67999195052,-19.3742356128,-9.85434442048));
#98016=CARTESIAN_POINT('',(6.67999195052,-16.6742356128,-13.3776272862));
#98017=CARTESIAN_POINT('',(6.67999195052,-18.0242356128,-13.3776272862));
#98018=CARTESIAN_POINT('',(6.67999195052,-16.6742356128,-11.6969736248));
#98019=CARTESIAN_POINT('Origin',(6.37999195052,-18.0242356128,-13.3776272862));
#98020=CARTESIAN_POINT('',(6.5054999889,-16.6742356128,-13.6501116569));
#98021=CARTESIAN_POINT('Origin',(6.37999195052,-16.6742356128,-13.3776272862));
#98022=CARTESIAN_POINT('',(6.5054999889,-18.0242356128,-13.6501116569));
#98023=CARTESIAN_POINT('Origin',(0.,-18.0242356128,0.473661560394));
#98024=CARTESIAN_POINT('',(5.35909918268,-16.6742356128,-14.1236860052));
#98025=CARTESIAN_POINT('Origin',(0.,-16.6742356128,0.473661560394));
#98026=CARTESIAN_POINT('',(5.35909918268,-18.0242356128,-14.1236860052));
#98027=CARTESIAN_POINT('Origin',(5.25570820166,-18.0242356128,-13.8420651518));
#98028=CARTESIAN_POINT('',(4.98558691274,-16.6742356128,-13.9725813932));
#98029=CARTESIAN_POINT('Origin',(5.25570820166,-16.6742356128,-13.8420651518));
#98030=CARTESIAN_POINT('',(4.98558691274,-18.0242356128,-13.9725813932));
#98031=CARTESIAN_POINT('Origin',(4.71546562382,-18.0242356128,-14.1030976346));
#98032=CARTESIAN_POINT('',(4.62312919377,-16.6742356128,-13.8176611554));
#98033=CARTESIAN_POINT('',(4.62312919377,-18.0242356128,-13.8176611554));
#98034=CARTESIAN_POINT('Origin',(4.71546562382,-16.6742356128,-14.1030976346));
#98035=CARTESIAN_POINT('Origin',(0.,-18.0242356128,0.473661560394));
#98036=CARTESIAN_POINT('',(3.37623759365,-16.6742356128,-14.1624666237));
#98037=CARTESIAN_POINT('',(3.37623759365,-18.0242356128,-14.1624666237));
#98038=CARTESIAN_POINT('Origin',(0.,-16.6742356128,0.473661560394));
#98039=CARTESIAN_POINT('Origin',(3.4436702163,-18.0242356128,-14.4547898034));
#98040=CARTESIAN_POINT('',(3.1436702163,-16.6742356128,-14.4547898034));
#98041=CARTESIAN_POINT('',(3.1436702163,-18.0242356128,-14.4547898034));
#98042=CARTESIAN_POINT('Origin',(3.4436702163,-16.6742356128,-14.4547898034));
#98043=CARTESIAN_POINT('Origin',(3.1436702163,-19.3742356128,-14.2141757917));
#98044=CARTESIAN_POINT('',(3.1436702163,-16.6742356128,-14.5088629165));
#98045=CARTESIAN_POINT('',(3.1436702163,-16.6742356128,-14.48182636));
#98046=CARTESIAN_POINT('',(3.1436702163,-18.0242356128,-14.5088629165));
#98047=CARTESIAN_POINT('Origin',(2.8436702163,-18.0242356128,-14.5088629165));
#98048=CARTESIAN_POINT('',(2.89961126973,-16.6742356128,-14.8036011029));
#98049=CARTESIAN_POINT('Origin',(2.8436702163,-16.6742356128,-14.5088629165));
#98050=CARTESIAN_POINT('',(2.89961126973,-18.0242356128,-14.8036011029));
#98051=CARTESIAN_POINT('Origin',(0.,-18.0242356128,0.473661560394));
#98052=CARTESIAN_POINT('',(-2.89961126973,-16.6742356128,-14.8036011029));
#98053=CARTESIAN_POINT('',(-2.89961126973,-18.0242356128,-14.8036011029));
#98054=CARTESIAN_POINT('Origin',(0.,-16.6742356128,0.473661560394));
#98055=CARTESIAN_POINT('Origin',(-2.8436702163,-18.0242356128,-14.5088629165));
#98056=CARTESIAN_POINT('',(-3.1436702163,-16.6742356128,-14.5088629165));
#98057=CARTESIAN_POINT('Origin',(-2.8436702163,-16.6742356128,-14.5088629165));
#98058=CARTESIAN_POINT('',(-3.1436702163,-18.0242356128,-14.5088629165));
#98059=CARTESIAN_POINT('Origin',(-3.1436702163,-19.3742356128,-14.2141757917));
#98060=CARTESIAN_POINT('',(-3.1436702163,-16.6742356128,-14.4547898034));
#98061=CARTESIAN_POINT('',(-3.1436702163,-18.0242356128,-14.4547898034));
#98062=CARTESIAN_POINT('',(-3.1436702163,-16.6742356128,-14.48182636));
#98063=CARTESIAN_POINT('Origin',(-3.4436702163,-18.0242356128,-14.4547898034));
#98064=CARTESIAN_POINT('',(-3.37623759365,-16.6742356128,-14.1624666237));
#98065=CARTESIAN_POINT('',(-3.37623759365,-18.0242356128,-14.1624666237));
#98066=CARTESIAN_POINT('Origin',(-3.4436702163,-16.6742356128,-14.4547898034));
#98067=CARTESIAN_POINT('Origin',(0.,-18.0242356128,0.473661560394));
#98068=CARTESIAN_POINT('',(-4.56454191842,-16.6742356128,-13.8364811917));
#98069=CARTESIAN_POINT('',(-4.56454191842,-18.0242356128,-13.8364811917));
#98070=CARTESIAN_POINT('Origin',(0.,-16.6742356128,0.473661560394));
#98071=CARTESIAN_POINT('Origin',(-4.65570820166,-18.0242356128,-14.1222935581));
#98072=CARTESIAN_POINT('',(-4.92636192076,-16.6742356128,-13.9928850408));
#98073=CARTESIAN_POINT('',(-4.92636192076,-18.0242356128,-13.9928850408));
#98074=CARTESIAN_POINT('Origin',(-4.65570820166,-16.6742356128,-14.1222935581));
#98075=CARTESIAN_POINT('Origin',(-5.19701563986,-18.0242356128,-13.8634765236));
#98076=CARTESIAN_POINT('',(-5.2992520131,-16.6742356128,-14.1455185843));
#98077=CARTESIAN_POINT('Origin',(-5.19701563986,-16.6742356128,-13.8634765236));
#98078=CARTESIAN_POINT('',(-5.2992520131,-18.0242356128,-14.1455185843));
#98079=CARTESIAN_POINT('Origin',(0.,-18.0242356128,0.473661560394));
#98080=CARTESIAN_POINT('',(-6.5054999889,-16.6742356128,-13.6501116569));
#98081=CARTESIAN_POINT('',(-6.5054999889,-18.0242356128,-13.6501116569));
#98082=CARTESIAN_POINT('Origin',(0.,-16.6742356128,0.473661560394));
#98083=CARTESIAN_POINT('Origin',(-6.37999195052,-18.0242356128,-13.3776272862));
#98084=CARTESIAN_POINT('',(-6.67999195052,-16.6742356128,-13.3776272862));
#98085=CARTESIAN_POINT('Origin',(-6.37999195052,-16.6742356128,-13.3776272862));
#98086=CARTESIAN_POINT('',(-6.67999195052,-18.0242356128,-13.3776272862));
#98087=CARTESIAN_POINT('Origin',(-6.67999195052,-19.3742356128,-9.85434442048));
#98088=CARTESIAN_POINT('',(-6.67999195052,-16.6742356128,-10.0163199635));
#98089=CARTESIAN_POINT('',(-6.67999195052,-18.0242356128,-10.0163199635));
#98090=CARTESIAN_POINT('',(-6.67999195052,-16.6742356128,-11.6969736248));
#98091=CARTESIAN_POINT('Origin',(-6.97999195052,-18.0242356128,-10.0163199635));
#98092=CARTESIAN_POINT('Origin',(-6.97999195052,-16.6742356128,-10.0163199635));
#98093=CARTESIAN_POINT('Origin',(6.61089801788,-5.78170707891,0.473661560394));
#98094=CARTESIAN_POINT('',(6.61089801788,-5.78170707891,6.35741269357));
#98095=CARTESIAN_POINT('Origin',(0.,-5.78170707891,0.473661560394));
#98096=CARTESIAN_POINT('',(6.61089801788,-5.78170707891,3.79053712698));
#98097=CARTESIAN_POINT('Origin',(6.61089801788,-14.9244482822,0.473661560394));
#98098=CARTESIAN_POINT('',(6.61089801788,-12.0242356128,6.35741269357));
#98099=CARTESIAN_POINT('Origin',(6.61089801788,-14.9244482822,0.473661560394));
#98100=CARTESIAN_POINT('',(6.61089801788,-14.9244482822,6.35741269357));
#98101=CARTESIAN_POINT('',(6.61089801788,-12.0242356128,6.35741269357));
#98102=CARTESIAN_POINT('',(6.61089801788,-14.9244482822,3.79053712698));
#98103=CARTESIAN_POINT('Origin',(13.7258691788,-14.9244482822,0.473661560394));
#98104=CARTESIAN_POINT('Origin',(0.,-14.9244482822,0.473661560394));
#98105=CARTESIAN_POINT('Origin',(13.7258691788,-14.9244482822,0.473661560394));
#98106=CARTESIAN_POINT('',(6.61089801788,-14.9244482822,-5.41008957278));
#98107=CARTESIAN_POINT('Origin',(0.,-14.9244482822,0.473661560394));
#98108=CARTESIAN_POINT('',(6.61089801788,-14.9244482822,-2.84321400619));
#98109=CARTESIAN_POINT('Origin',(6.61089801788,-14.9244482822,0.473661560394));
#98110=CARTESIAN_POINT('',(6.61089801788,-12.0242356128,-5.41008957278));
#98111=CARTESIAN_POINT('Origin',(0.,-9.81495241206,0.473661560394));
#98112=CARTESIAN_POINT('',(-8.40228522294909E-15,-16.6742356128,9.323661560394));
#98113=CARTESIAN_POINT('',(-8.40228522294909E-15,-9.81495241206,9.323661560394));
#98114=CARTESIAN_POINT('Origin',(0.,-16.6742356128,0.473661560394));
#98115=CARTESIAN_POINT('',(6.61089801788,-5.78170707891,-5.41008957278));
#98116=CARTESIAN_POINT('Origin',(0.,-5.78170707891,0.473661560394));
#98117=CARTESIAN_POINT('',(6.61089801788,-12.0242356128,-5.41008957278));
#98118=CARTESIAN_POINT('Origin',(6.61089801788,-14.9244482822,0.473661560394));
#98119=CARTESIAN_POINT('',(6.61089801788,-5.78170707891,-2.84321400619));
#98120=CARTESIAN_POINT('Origin',(6.61089801788,-5.78170707891,0.473661560394));
#98121=CARTESIAN_POINT('Origin',(-4.2,-19.0742356128,6.1986309857));
#98122=CARTESIAN_POINT('',(-4.2,-19.0742356128,6.4986309857));
#98123=CARTESIAN_POINT('Origin',(-4.2,-19.0742356128,6.1986309857));
#98124=CARTESIAN_POINT('Origin',(-4.2,-19.0742356128,6.7986309857));
#98125=CARTESIAN_POINT('Origin',(-4.2,-13.6742356128,6.1986309857));
#98126=CARTESIAN_POINT('',(-4.2,-11.8742356128,6.4986309857));
#98127=CARTESIAN_POINT('Origin',(0.,-19.0742356128,6.7986309857));
#98128=CARTESIAN_POINT('',(4.2,-19.0742356128,6.4986309857));
#98129=CARTESIAN_POINT('',(-8.881784197E-16,-19.0742356128,6.4986309857));
#98130=CARTESIAN_POINT('Origin',(4.2,-19.0742356128,6.7986309857));
#98131=CARTESIAN_POINT('Origin',(0.,-4.67423561284,6.4986309857));
#98132=CARTESIAN_POINT('',(4.2,-13.6742356128,6.4986309857));
#98133=CARTESIAN_POINT('Origin',(4.2,-19.0742356128,6.1986309857));
#98134=CARTESIAN_POINT('',(4.5,-19.0742356128,6.1986309857));
#98135=CARTESIAN_POINT('Origin',(4.2,-19.0742356128,6.1986309857));
#98136=CARTESIAN_POINT('Origin',(4.8,-19.0742356128,6.1986309857));
#98137=CARTESIAN_POINT('Origin',(4.2,-13.6742356128,6.1986309857));
#98138=CARTESIAN_POINT('',(4.5,-11.8742356128,6.1986309857));
#98139=CARTESIAN_POINT('Origin',(4.8,-19.0742356128,-2.12633843961));
#98140=CARTESIAN_POINT('',(4.5,-19.0742356128,-5.5013690143));
#98141=CARTESIAN_POINT('',(4.5,-19.0742356128,0.348630985699));
#98142=CARTESIAN_POINT('Origin',(4.8,-19.0742356128,-5.5013690143));
#98143=CARTESIAN_POINT('Origin',(4.5,-4.67423561284,6.4986309857));
#98144=CARTESIAN_POINT('',(4.5,-13.6742356128,-5.5013690143));
#98145=CARTESIAN_POINT('Ctrl Pts',(4.20000000308,-18.6809100802,-5.80136900064));
#98146=CARTESIAN_POINT('Ctrl Pts',(4.13201933245,-18.7060691672,-5.80136900054));
#98147=CARTESIAN_POINT('Ctrl Pts',(4.06403866191,-18.7312282542,-5.8232621298));
#98148=CARTESIAN_POINT('Ctrl Pts',(4.00438515095,-18.7533055279,-5.86715848437));
#98149=CARTESIAN_POINT('Ctrl Pts',(3.96107032752,-18.7693359879,-5.92716273862));
#98150=CARTESIAN_POINT('Ctrl Pts',(3.93695198573,-18.7782619879,-5.99493428879));
#98151=CARTESIAN_POINT('Ctrl Pts',(4.21444980228,-18.7589979661,-5.80136893282));
#98152=CARTESIAN_POINT('Ctrl Pts',(4.14870278107,-18.7823836855,-5.80464328508));
#98153=CARTESIAN_POINT('Ctrl Pts',(4.08401026512,-18.8057694048,-5.82817358597));
#98154=CARTESIAN_POINT('Ctrl Pts',(4.02779990888,-18.8265241376,-5.87164554118));
#98155=CARTESIAN_POINT('Ctrl Pts',(3.98697421869,-18.8420998044,-5.92969663234));
#98156=CARTESIAN_POINT('Ctrl Pts',(3.96404157784,-18.8514591938,-5.99493417698));
#98157=CARTESIAN_POINT('Ctrl Pts',(4.22827546583,-18.8373868265,-5.80049863859));
#98158=CARTESIAN_POINT('Ctrl Pts',(4.16490990067,-18.8591197488,-5.8066369302));
#98159=CARTESIAN_POINT('Ctrl Pts',(4.10341065724,-18.8808526711,-5.83146844409));
#98160=CARTESIAN_POINT('Ctrl Pts',(4.0503920793,-18.9003289652,-5.87438626363));
#98161=CARTESIAN_POINT('Ctrl Pts',(4.01183648058,-18.9153528523,-5.93052115145));
#98162=CARTESIAN_POINT('Ctrl Pts',(3.98996106595,-18.9249385271,-5.99330264064));
#98163=CARTESIAN_POINT('Ctrl Pts',(4.24142568441,-18.9160882934,-5.79890830556));
#98164=CARTESIAN_POINT('Ctrl Pts',(4.18051060715,-18.9362628974,-5.80752351469));
#98165=CARTESIAN_POINT('Ctrl Pts',(4.12207728309,-18.9564375015,-5.83336652821));
#98166=CARTESIAN_POINT('Ctrl Pts',(4.07201635859,-18.9746713345,-5.87563301391));
#98167=CARTESIAN_POINT('Ctrl Pts',(4.03553864585,-18.9890689835,-5.92990313712));
#98168=CARTESIAN_POINT('Ctrl Pts',(4.01461432289,-18.9987108858,-5.9903211697));
#98169=CARTESIAN_POINT('Ctrl Pts',(4.2538376014,-18.9950222816,-5.79673916481));
#98170=CARTESIAN_POINT('Ctrl Pts',(4.19537771422,-19.0137178049,-5.80747373633));
#98171=CARTESIAN_POINT('Ctrl Pts',(4.13985677188,-19.0324133281,-5.83407978878));
#98172=CARTESIAN_POINT('Ctrl Pts',(4.09252688404,-19.0494360536,-5.87562478381));
#98173=CARTESIAN_POINT('Ctrl Pts',(4.05794935095,-19.0631474974,-5.92809450339));
#98174=CARTESIAN_POINT('Ctrl Pts',(4.03788343644,-19.0727011908,-5.98625455018));
#98175=CARTESIAN_POINT('Ctrl Pts',(4.26546731361,-19.0742356128,-5.79413860092));
#98176=CARTESIAN_POINT('Ctrl Pts',(4.20941600096,-19.0915169389,-5.80667244675));
#98177=CARTESIAN_POINT('Ctrl Pts',(4.15663577279,-19.1087982649,-5.83383457041));
#98178=CARTESIAN_POINT('Ctrl Pts',(4.11181833689,-19.1246355845,-5.87461401092));
#98179=CARTESIAN_POINT('Ctrl Pts',(4.07897573734,-19.1376111454,-5.92536020439));
#98180=CARTESIAN_POINT('Ctrl Pts',(4.05968611194,-19.146953353,-5.98137917153));
#98181=CARTESIAN_POINT('',(4.26546731361,-19.0742356128,-5.79413860092));
#98182=CARTESIAN_POINT('Origin',(4.33093462721,-19.0742356128,-6.08690818754));
#98183=CARTESIAN_POINT('',(4.20000000673865,-18.6809100779312,-5.80136900746964));
#98184=CARTESIAN_POINT('Ctrl Pts',(4.26546731361,-19.0742356128,-5.79413860092));
#98185=CARTESIAN_POINT('Ctrl Pts',(4.25718116343965,-19.0177962514537,-5.79599149826871));
#98186=CARTESIAN_POINT('Ctrl Pts',(4.24841774144974,-18.9615220782279,-5.79758138057646));
#98187=CARTESIAN_POINT('Ctrl Pts',(4.23921637206803,-18.9054095339776,-5.79879450761291));
#98188=CARTESIAN_POINT('Ctrl Pts',(4.22817173449333,-18.8380562206902,-5.80025065483338));
#98189=CARTESIAN_POINT('Ctrl Pts',(4.21649704322489,-18.7709427807032,-5.80116455660017));
#98190=CARTESIAN_POINT('Ctrl Pts',(4.20426682708576,-18.7040984271016,-5.80133862753531));
#98191=CARTESIAN_POINT('Ctrl Pts',(4.20285195518481,-18.6963654323146,-5.8013587652068));
#98192=CARTESIAN_POINT('Ctrl Pts',(4.201429643321,-18.6886359881787,-5.80136899394372));
#98193=CARTESIAN_POINT('Ctrl Pts',(4.20000000019741,-18.6809100812668,-5.80136900064));
#98194=CARTESIAN_POINT('Origin',(4.20005977102284,-18.680887963059,-6.10146134989777));
#98195=CARTESIAN_POINT('Origin',(4.33093462721,-19.0742356128,-6.08690818754));
#98196=CARTESIAN_POINT('Origin',(4.33093462721,-19.0742356128,-6.08690818754));
#98197=CARTESIAN_POINT('Origin',(4.2,-19.0742356128,-5.5013690143));
#98198=CARTESIAN_POINT('Origin',(4.2,-19.0742356128,-5.5013690143));
#98199=CARTESIAN_POINT('Origin',(4.2,-13.6742356128,-5.5013690143));
#98200=CARTESIAN_POINT('',(4.2,-11.6775728158,-5.8013690143));
#98201=CARTESIAN_POINT('Origin',(-1.50990331349E-14,-20.2352955315,-6.1013690143));
#98202=CARTESIAN_POINT('',(-4.2,-18.6809100188,-5.8013690143));
#98203=CARTESIAN_POINT('Origin',(4.4408920985E-16,-20.2352955315,-5.8013690143));
#98204=CARTESIAN_POINT('Origin',(-4.20006010219018,-18.6808887946701,-6.10146136541638));
#98205=CARTESIAN_POINT('Origin',(0.,-4.67423561284,-5.8013690143));
#98206=CARTESIAN_POINT('',(-4.2,-13.6742356128,-5.8013690143));
#98207=CARTESIAN_POINT('Ctrl Pts',(-4.26546734067,-19.0742356128,-5.79413853556));
#98208=CARTESIAN_POINT('Ctrl Pts',(-4.20941603025,-19.0915169379,-5.80667236858));
#98209=CARTESIAN_POINT('Ctrl Pts',(-4.15663580604,-19.1087982629,-5.83383447647));
#98210=CARTESIAN_POINT('Ctrl Pts',(-4.11181837608,-19.1246355815,-5.87461389924));
#98211=CARTESIAN_POINT('Ctrl Pts',(-4.0789757843,-19.1376111412,-5.92536007425));
#98212=CARTESIAN_POINT('Ctrl Pts',(-4.05968616788,-19.1469533476,-5.98137902326));
#98213=CARTESIAN_POINT('Ctrl Pts',(-4.25383581433,-18.995009694,-5.79673942591));
#98214=CARTESIAN_POINT('Ctrl Pts',(-4.19537554889,-19.0137054404,-5.80747368304));
#98215=CARTESIAN_POINT('Ctrl Pts',(-4.13985417963,-19.0324011868,-5.83407961226));
#98216=CARTESIAN_POINT('Ctrl Pts',(-4.09252390601,-19.0494240988,-5.87562468998));
#98217=CARTESIAN_POINT('Ctrl Pts',(-4.05794611539,-19.0631356574,-5.92809464302));
#98218=CARTESIAN_POINT('Ctrl Pts',(-4.03788009887,-19.0726893818,-5.98625499045));
#98219=CARTESIAN_POINT('Ctrl Pts',(-4.24142181064,-18.9160629516,-5.7989087319));
#98220=CARTESIAN_POINT('Ctrl Pts',(-4.1805059538,-18.9362380267,-5.80752320608));
#98221=CARTESIAN_POINT('Ctrl Pts',(-4.1220717118,-18.9564131018,-5.8333659072));
#98222=CARTESIAN_POINT('Ctrl Pts',(-4.07200993757,-18.9746473194,-5.87563254882));
#98223=CARTESIAN_POINT('Ctrl Pts',(-4.03553165095,-18.9890451839,-5.92990317159));
#98224=CARTESIAN_POINT('Ctrl Pts',(-4.01460709459,-18.9986871093,-5.99032185261));
#98225=CARTESIAN_POINT('Ctrl Pts',(-4.2282770598,-18.8373949885,-5.80049881029));
#98226=CARTESIAN_POINT('Ctrl Pts',(-4.16491182009,-18.8591277431,-5.80663741972));
#98227=CARTESIAN_POINT('Ctrl Pts',(-4.10341297162,-18.8808604976,-5.83146908674));
#98228=CARTESIAN_POINT('Ctrl Pts',(-4.05039476614,-18.9003366584,-5.8743868734));
#98229=CARTESIAN_POINT('Ctrl Pts',(-4.01183942564,-18.9153604797,-5.93052159234));
#98230=CARTESIAN_POINT('Ctrl Pts',(-3.98996412602,-18.9249461655,-5.99330285525));
#98231=CARTESIAN_POINT('Ctrl Pts',(-4.21445160765,-18.7590074427,-5.8013690143));
#98232=CARTESIAN_POINT('Ctrl Pts',(-4.14870486904,-18.782392944,-5.80464378088));
#98233=CARTESIAN_POINT('Ctrl Pts',(-4.08401276797,-18.8057784452,-5.82817429489));
#98234=CARTESIAN_POINT('Ctrl Pts',(-4.02780284558,-18.8265330161,-5.87164620833));
#98235=CARTESIAN_POINT('Ctrl Pts',(-3.98697746856,-18.8421086289,-5.92969706832));
#98236=CARTESIAN_POINT('Ctrl Pts',(-3.96404497635,-18.8514680746,-5.99493430976));
#98237=CARTESIAN_POINT('Ctrl Pts',(-4.2,-18.6809100188,-5.8013690143));
#98238=CARTESIAN_POINT('Ctrl Pts',(-4.1320193297,-18.7060691067,-5.8013690143));
#98239=CARTESIAN_POINT('Ctrl Pts',(-4.06403865941,-18.7312281946,-5.82326214445));
#98240=CARTESIAN_POINT('Ctrl Pts',(-4.00438514857,-18.7533054691,-5.8671585007));
#98241=CARTESIAN_POINT('Ctrl Pts',(-3.96107032516,-18.7693359296,-5.92716275717));
#98242=CARTESIAN_POINT('Ctrl Pts',(-3.9369519833,-18.7782619299,-5.99493430976));
#98243=CARTESIAN_POINT('',(-4.26546728923319,-19.0742356128,-5.79413859154276));
#98244=CARTESIAN_POINT('Ctrl Pts',(-4.2,-18.6809100188,-5.8013690143));
#98245=CARTESIAN_POINT('Ctrl Pts',(-4.22006430058665,-18.7893389122285,
-5.8013690143));
#98246=CARTESIAN_POINT('Ctrl Pts',(-4.23867827458747,-18.8984340287179,
-5.79935944419928));
#98247=CARTESIAN_POINT('Ctrl Pts',(-4.25554083761466,-19.0081708556049,
-5.79618275354226));
#98248=CARTESIAN_POINT('Ctrl Pts',(-4.2589207689943,-19.0301665002823,-5.79554601780892));
#98249=CARTESIAN_POINT('Ctrl Pts',(-4.2622303821849,-19.0521880859069,-5.79486234132898));
#98250=CARTESIAN_POINT('Ctrl Pts',(-4.26546727976036,-19.0742356128001,
-5.79413854918021));
#98251=CARTESIAN_POINT('Origin',(-4.33093462721,-19.0742356128,-6.08690818754));
#98252=CARTESIAN_POINT('Origin',(-4.33093462721,-19.0742356128,-6.08690818754));
#98253=CARTESIAN_POINT('Origin',(-4.33093462721,-19.0742356128,-6.08690818754));
#98254=CARTESIAN_POINT('Origin',(-4.2,-19.0742356128,-5.5013690143));
#98255=CARTESIAN_POINT('Origin',(-4.2,-19.0742356128,-5.5013690143));
#98256=CARTESIAN_POINT('Origin',(-4.2,-13.6742356128,-5.5013690143));
#98257=CARTESIAN_POINT('Origin',(0.,-16.6742356128,0.473661560394));
#98258=CARTESIAN_POINT('Origin',(-6.54794311523,-4.67423561284,3.49012794495));
#98259=CARTESIAN_POINT('',(-5.44794311523,-14.0742356128,3.49012794495));
#98260=CARTESIAN_POINT('',(-4.97448577881,-14.0742356128,3.49012794495));
#98261=CARTESIAN_POINT('',(-5.44794311523,-9.37423561284,3.49012794495));
#98262=CARTESIAN_POINT('Origin',(-5.44794311523,-4.67423561284,0.473661560394));
#98263=CARTESIAN_POINT('',(-5.44794311523,-14.0742356128,-2.54280482416));
#98264=CARTESIAN_POINT('',(-5.44794311523,-14.0742356128,1.98189475267));
#98265=CARTESIAN_POINT('',(-5.44794311523,-9.37423561284,-2.54280482416));
#98266=CARTESIAN_POINT('Origin',(0.,-14.0742356128,0.473661560394));
#98267=CARTESIAN_POINT('',(-4.97448577881,-14.0742356128,-2.54280482416));
#98268=CARTESIAN_POINT('Origin',(-6.54794311523,-4.67423561284,-2.54280482416));
#98269=CARTESIAN_POINT('',(0.,0.,0.));
#98270=CARTESIAN_POINT('',(0.,0.,0.));
#98271=CARTESIAN_POINT('',(0.,0.,0.));
#98272=CARTESIAN_POINT('',(0.,0.,0.));
#98273=CARTESIAN_POINT('',(0.,0.,0.));
#98274=CARTESIAN_POINT('',(0.,0.,0.));
#98275=CARTESIAN_POINT('',(0.,0.,0.));
#98276=CARTESIAN_POINT('',(0.,0.,0.));
#98277=CARTESIAN_POINT('',(0.,0.,0.));
#98278=CARTESIAN_POINT('',(0.,0.,0.));
#98279=UNCERTAINTY_MEASURE_WITH_UNIT(LENGTH_MEASURE(0.01),#98303,
'DISTANCE_ACCURACY_VALUE',
'Maximum model space distance between geometric entities at asserted c
onnectivities');
#98280=UNCERTAINTY_MEASURE_WITH_UNIT(LENGTH_MEASURE(0.01),#98303,
'DISTANCE_ACCURACY_VALUE',
'Maximum model space distance between geometric entities at asserted c
onnectivities');
#98281=UNCERTAINTY_MEASURE_WITH_UNIT(LENGTH_MEASURE(0.01),#98303,
'DISTANCE_ACCURACY_VALUE',
'Maximum model space distance between geometric entities at asserted c
onnectivities');
#98282=UNCERTAINTY_MEASURE_WITH_UNIT(LENGTH_MEASURE(0.01),#98303,
'DISTANCE_ACCURACY_VALUE',
'Maximum model space distance between geometric entities at asserted c
onnectivities');
#98283=UNCERTAINTY_MEASURE_WITH_UNIT(LENGTH_MEASURE(0.01),#98303,
'DISTANCE_ACCURACY_VALUE',
'Maximum model space distance between geometric entities at asserted c
onnectivities');
#98284=UNCERTAINTY_MEASURE_WITH_UNIT(LENGTH_MEASURE(0.01),#98303,
'DISTANCE_ACCURACY_VALUE',
'Maximum model space distance between geometric entities at asserted c
onnectivities');
#98285=UNCERTAINTY_MEASURE_WITH_UNIT(LENGTH_MEASURE(0.01),#98303,
'DISTANCE_ACCURACY_VALUE',
'Maximum model space distance between geometric entities at asserted c
onnectivities');
#98286=UNCERTAINTY_MEASURE_WITH_UNIT(LENGTH_MEASURE(0.01),#98303,
'DISTANCE_ACCURACY_VALUE',
'Maximum model space distance between geometric entities at asserted c
onnectivities');
#98287=UNCERTAINTY_MEASURE_WITH_UNIT(LENGTH_MEASURE(0.01),#98303,
'DISTANCE_ACCURACY_VALUE',
'Maximum model space distance between geometric entities at asserted c
onnectivities');
#98288=UNCERTAINTY_MEASURE_WITH_UNIT(LENGTH_MEASURE(0.01),#98303,
'DISTANCE_ACCURACY_VALUE',
'Maximum model space distance between geometric entities at asserted c
onnectivities');
#98289=UNCERTAINTY_MEASURE_WITH_UNIT(LENGTH_MEASURE(0.01),#98303,
'DISTANCE_ACCURACY_VALUE',
'Maximum model space distance between geometric entities at asserted c
onnectivities');
#98290=UNCERTAINTY_MEASURE_WITH_UNIT(LENGTH_MEASURE(0.01),#98303,
'DISTANCE_ACCURACY_VALUE',
'Maximum model space distance between geometric entities at asserted c
onnectivities');
#98291=(
GEOMETRIC_REPRESENTATION_CONTEXT(3)
GLOBAL_UNCERTAINTY_ASSIGNED_CONTEXT((#98279))
GLOBAL_UNIT_ASSIGNED_CONTEXT((#98303,#98305,#98306))
REPRESENTATION_CONTEXT('','3D')
);
#98292=(
GEOMETRIC_REPRESENTATION_CONTEXT(3)
GLOBAL_UNCERTAINTY_ASSIGNED_CONTEXT((#98280))
GLOBAL_UNIT_ASSIGNED_CONTEXT((#98303,#98305,#98306))
REPRESENTATION_CONTEXT('','3D')
);
#98293=(
GEOMETRIC_REPRESENTATION_CONTEXT(3)
GLOBAL_UNCERTAINTY_ASSIGNED_CONTEXT((#98281))
GLOBAL_UNIT_ASSIGNED_CONTEXT((#98303,#98305,#98306))
REPRESENTATION_CONTEXT('','3D')
);
#98294=(
GEOMETRIC_REPRESENTATION_CONTEXT(3)
GLOBAL_UNCERTAINTY_ASSIGNED_CONTEXT((#98282))
GLOBAL_UNIT_ASSIGNED_CONTEXT((#98303,#98305,#98306))
REPRESENTATION_CONTEXT('','3D')
);
#98295=(
GEOMETRIC_REPRESENTATION_CONTEXT(3)
GLOBAL_UNCERTAINTY_ASSIGNED_CONTEXT((#98283))
GLOBAL_UNIT_ASSIGNED_CONTEXT((#98303,#98305,#98306))
REPRESENTATION_CONTEXT('','3D')
);
#98296=(
GEOMETRIC_REPRESENTATION_CONTEXT(3)
GLOBAL_UNCERTAINTY_ASSIGNED_CONTEXT((#98284))
GLOBAL_UNIT_ASSIGNED_CONTEXT((#98303,#98305,#98306))
REPRESENTATION_CONTEXT('','3D')
);
#98297=(
GEOMETRIC_REPRESENTATION_CONTEXT(3)
GLOBAL_UNCERTAINTY_ASSIGNED_CONTEXT((#98285))
GLOBAL_UNIT_ASSIGNED_CONTEXT((#98303,#98305,#98306))
REPRESENTATION_CONTEXT('','3D')
);
#98298=(
GEOMETRIC_REPRESENTATION_CONTEXT(3)
GLOBAL_UNCERTAINTY_ASSIGNED_CONTEXT((#98286))
GLOBAL_UNIT_ASSIGNED_CONTEXT((#98303,#98305,#98306))
REPRESENTATION_CONTEXT('','3D')
);
#98299=(
GEOMETRIC_REPRESENTATION_CONTEXT(3)
GLOBAL_UNCERTAINTY_ASSIGNED_CONTEXT((#98287))
GLOBAL_UNIT_ASSIGNED_CONTEXT((#98303,#98305,#98306))
REPRESENTATION_CONTEXT('','3D')
);
#98300=(
GEOMETRIC_REPRESENTATION_CONTEXT(3)
GLOBAL_UNCERTAINTY_ASSIGNED_CONTEXT((#98288))
GLOBAL_UNIT_ASSIGNED_CONTEXT((#98303,#98305,#98306))
REPRESENTATION_CONTEXT('','3D')
);
#98301=(
GEOMETRIC_REPRESENTATION_CONTEXT(3)
GLOBAL_UNCERTAINTY_ASSIGNED_CONTEXT((#98289))
GLOBAL_UNIT_ASSIGNED_CONTEXT((#98303,#98305,#98306))
REPRESENTATION_CONTEXT('','3D')
);
#98302=(
GEOMETRIC_REPRESENTATION_CONTEXT(3)
GLOBAL_UNCERTAINTY_ASSIGNED_CONTEXT((#98290))
GLOBAL_UNIT_ASSIGNED_CONTEXT((#98303,#98305,#98306))
REPRESENTATION_CONTEXT('','3D')
);
#98303=(
LENGTH_UNIT()
NAMED_UNIT(*)
SI_UNIT(.MILLI.,.METRE.)
);
#98304=(
LENGTH_UNIT()
NAMED_UNIT(*)
SI_UNIT($,.METRE.)
);
#98305=(
NAMED_UNIT(*)
PLANE_ANGLE_UNIT()
SI_UNIT($,.RADIAN.)
);
#98306=(
NAMED_UNIT(*)
SI_UNIT($,.STERADIAN.)
SOLID_ANGLE_UNIT()
);
#98307=SHAPE_DEFINITION_REPRESENTATION(#98318,#98339);
#98308=SHAPE_DEFINITION_REPRESENTATION(#98319,#98340);
#98309=SHAPE_DEFINITION_REPRESENTATION(#98320,#98341);
#98310=SHAPE_DEFINITION_REPRESENTATION(#98321,#98342);
#98311=SHAPE_DEFINITION_REPRESENTATION(#98322,#98343);
#98312=SHAPE_DEFINITION_REPRESENTATION(#98323,#98344);
#98313=SHAPE_DEFINITION_REPRESENTATION(#98324,#98345);
#98314=SHAPE_DEFINITION_REPRESENTATION(#98325,#98346);
#98315=SHAPE_DEFINITION_REPRESENTATION(#98326,#98347);
#98316=SHAPE_DEFINITION_REPRESENTATION(#98327,#98348);
#98317=SHAPE_DEFINITION_REPRESENTATION(#98328,#98349);
#98318=PRODUCT_DEFINITION_SHAPE('',$,#98351);
#98319=PRODUCT_DEFINITION_SHAPE('',$,#98352);
#98320=PRODUCT_DEFINITION_SHAPE('',$,#98353);
#98321=PRODUCT_DEFINITION_SHAPE('',$,#98354);
#98322=PRODUCT_DEFINITION_SHAPE('',$,#98355);
#98323=PRODUCT_DEFINITION_SHAPE('',$,#98356);
#98324=PRODUCT_DEFINITION_SHAPE('',$,#98357);
#98325=PRODUCT_DEFINITION_SHAPE('',$,#98358);
#98326=PRODUCT_DEFINITION_SHAPE('',$,#98359);
#98327=PRODUCT_DEFINITION_SHAPE('',$,#98360);
#98328=PRODUCT_DEFINITION_SHAPE('',$,#98361);
#98329=PRODUCT_DEFINITION_SHAPE($,$,#41);
#98330=PRODUCT_DEFINITION_SHAPE($,$,#42);
#98331=PRODUCT_DEFINITION_SHAPE($,$,#43);
#98332=PRODUCT_DEFINITION_SHAPE($,$,#44);
#98333=PRODUCT_DEFINITION_SHAPE($,$,#45);
#98334=PRODUCT_DEFINITION_SHAPE($,$,#46);
#98335=PRODUCT_DEFINITION_SHAPE($,$,#47);
#98336=PRODUCT_DEFINITION_SHAPE($,$,#48);
#98337=PRODUCT_DEFINITION_SHAPE($,$,#49);
#98338=PRODUCT_DEFINITION_SHAPE($,$,#50);
#98339=SHAPE_REPRESENTATION('',(#34290,#38606,#38607,#38608,#38609,#38610,
#38611,#38612,#38613,#38614,#38615),#98291);
#98340=SHAPE_REPRESENTATION('',(#34291),#98292);
#98341=SHAPE_REPRESENTATION('',(#34303),#98293);
#98342=SHAPE_REPRESENTATION('',(#34823),#98294);
#98343=SHAPE_REPRESENTATION('',(#34920),#98295);
#98344=SHAPE_REPRESENTATION('',(#34962),#98296);
#98345=SHAPE_REPRESENTATION('',(#35726),#98297);
#98346=SHAPE_REPRESENTATION('',(#36369),#98298);
#98347=SHAPE_REPRESENTATION('',(#36602),#98299);
#98348=SHAPE_REPRESENTATION('',(#38088),#98300);
#98349=SHAPE_REPRESENTATION('',(#38347),#98301);
#98350=PRODUCT_DEFINITION_CONTEXT('part definition',#98385,'design');
#98351=PRODUCT_DEFINITION('MAS-608','MAS-608',#98362,
#98350);
#98352=PRODUCT_DEFINITION('Pivot Pin','Pivot Pin',#98363,#98350);
#98353=PRODUCT_DEFINITION('Fixed Ceramic Disc','Fixed Ceramic Disc',#98364,
#98350);
#98354=PRODUCT_DEFINITION('Inner Gasket','Inner Gasket',#98365,#98350);
#98355=PRODUCT_DEFINITION('Bottom Gaskets','Bottom Gaskets',#98366,#98350);
#98356=PRODUCT_DEFINITION('Bottom Base','Bottom Base',#98367,#98350);
#98357=PRODUCT_DEFINITION('Control Lever','Control Lever',#98368,#98350);
#98358=PRODUCT_DEFINITION('Main Cartridge Housing',
'Main Cartridge Housing',#98369,#98350);
#98359=PRODUCT_DEFINITION('Disc Carrier','Disc Carrier',#98370,#98350);
#98360=PRODUCT_DEFINITION('Movable Ceramic Disc','Movable Ceramic Disc',
#98371,#98350);
#98361=PRODUCT_DEFINITION('Pivot Adapter','Pivot Adapter',#98372,#98350);
#98362=PRODUCT_DEFINITION_FORMATION('',$,#98387);
#98363=PRODUCT_DEFINITION_FORMATION('',$,#98388);
#98364=PRODUCT_DEFINITION_FORMATION('',$,#98389);
#98365=PRODUCT_DEFINITION_FORMATION('',$,#98390);
#98366=PRODUCT_DEFINITION_FORMATION('',$,#98391);
#98367=PRODUCT_DEFINITION_FORMATION('',$,#98392);
#98368=PRODUCT_DEFINITION_FORMATION('',$,#98393);
#98369=PRODUCT_DEFINITION_FORMATION('',$,#98394);
#98370=PRODUCT_DEFINITION_FORMATION('',$,#98395);
#98371=PRODUCT_DEFINITION_FORMATION('',$,#98396);
#98372=PRODUCT_DEFINITION_FORMATION('',$,#98397);
#98373=PRODUCT_RELATED_PRODUCT_CATEGORY('MAS-608',
'MAS-608',(#98387));
#98374=PRODUCT_RELATED_PRODUCT_CATEGORY('Pivot Pin','Pivot Pin',(#98388));
#98375=PRODUCT_RELATED_PRODUCT_CATEGORY('Fixed Ceramic Disc',
'Fixed Ceramic Disc',(#98389));
#98376=PRODUCT_RELATED_PRODUCT_CATEGORY('Inner Gasket','Inner Gasket',(#98390));
#98377=PRODUCT_RELATED_PRODUCT_CATEGORY('Bottom Gaskets',
'Bottom Gaskets',(#98391));
#98378=PRODUCT_RELATED_PRODUCT_CATEGORY('Bottom Base','Bottom Base',(#98392));
#98379=PRODUCT_RELATED_PRODUCT_CATEGORY('Control Lever','Control Lever',
(#98393));
#98380=PRODUCT_RELATED_PRODUCT_CATEGORY('Main Cartridge Housing',
'Main Cartridge Housing',(#98394));
#98381=PRODUCT_RELATED_PRODUCT_CATEGORY('Disc Carrier','Disc Carrier',(#98395));
#98382=PRODUCT_RELATED_PRODUCT_CATEGORY('Movable Ceramic Disc',
'Movable Ceramic Disc',(#98396));
#98383=PRODUCT_RELATED_PRODUCT_CATEGORY('Pivot Adapter','Pivot Adapter',
(#98397));
#98384=APPLICATION_PROTOCOL_DEFINITION('international standard',
'automotive_design',2009,#98385);
#98385=APPLICATION_CONTEXT(
'Core Data for Automotive Mechanical Design Process');
#98386=PRODUCT_CONTEXT('part definition',#98385,'mechanical');
#98387=PRODUCT('MAS-608','MAS-608','STEP AP214',(#98386));
#98388=PRODUCT('Pivot Pin','Pivot Pin',$,(#98386));
#98389=PRODUCT('Fixed Ceramic Disc','Fixed Ceramic Disc',$,(#98386));
#98390=PRODUCT('Inner Gasket','Inner Gasket',$,(#98386));
#98391=PRODUCT('Bottom Gaskets','Bottom Gaskets',$,(#98386));
#98392=PRODUCT('Bottom Base','Bottom Base',$,(#98386));
#98393=PRODUCT('Control Lever','Control Lever',$,(#98386));
#98394=PRODUCT('Main Cartridge Housing','Main Cartridge Housing',$,(#98386));
#98395=PRODUCT('Disc Carrier','Disc Carrier',$,(#98386));
#98396=PRODUCT('Movable Ceramic Disc','Movable Ceramic Disc',$,(#98386));
#98397=PRODUCT('Pivot Adapter','Pivot Adapter',$,(#98386));
#98398=PRESENTATION_STYLE_ASSIGNMENT((#98400));
#98399=PRESENTATION_STYLE_ASSIGNMENT((#98401));
#98400=SURFACE_STYLE_USAGE(.BOTH.,#98402);
#98401=SURFACE_STYLE_USAGE(.BOTH.,#98403);
#98402=SURFACE_SIDE_STYLE('',(#98404));
#98403=SURFACE_SIDE_STYLE('',(#98405));
#98404=SURFACE_STYLE_FILL_AREA(#98406);
#98405=SURFACE_STYLE_FILL_AREA(#98407);
#98406=FILL_AREA_STYLE('Steel - Satin',(#98408));
#98407=FILL_AREA_STYLE('Opaque(202,209,238)',(#98409));
#98408=FILL_AREA_STYLE_COLOUR('Steel - Satin',#98410);
#98409=FILL_AREA_STYLE_COLOUR('Opaque(202,209,238)',#98411);
#98410=COLOUR_RGB('Steel - Satin', 0.66274510, 0.83137255, 0.94901961);
#98411=COLOUR_RGB('Opaque(202,209,238)', 0.31764706, 0.68627451, 0.89019608);
ENDSEC;
END-ISO-10303-21;
